#45573=CARTESIAN_POINT('Ctrl Pts',(-8.08087814877779,31.3918967161785,21.2950180122802));
#45574=CARTESIAN_POINT('Ctrl Pts',(-8.18714894688558,31.337342542798,21.2892075880416));
#45575=CARTESIAN_POINT('Ctrl Pts',(-8.29568826514029,31.2875147797709,21.283397163803));
#45576=CARTESIAN_POINT('Ctrl Pts',(-8.40833602134445,31.2358009327344,21.2773668029753));
#45577=CARTESIAN_POINT('Ctrl Pts',(-8.52342705878339,31.1891786297618,21.2713364421475));
#45578=CARTESIAN_POINT('Ctrl Pts',(-8.64045761121134,31.1478746784292,21.2653060813198));
#45579=CARTESIAN_POINT('Ctrl Pts',(-8.7530929569649,31.1081219408507,21.2595021970967));
#45580=CARTESIAN_POINT('Ctrl Pts',(-8.86752434410631,31.0732954343172,21.2536983128737));
#45581=CARTESIAN_POINT('Ctrl Pts',(-8.98328254517895,31.0435482288972,21.2478944286506));
#45582=CARTESIAN_POINT('Ctrl Pts',(-9.09902364752437,31.0138054174584,21.2420914017235));
#45583=CARTESIAN_POINT('Ctrl Pts',(-9.21609077866904,30.9891405166922,21.2362883747964));
#45584=CARTESIAN_POINT('Ctrl Pts',(-9.33400102960615,30.9696562961164,21.2304853478693));
#45585=CARTESIAN_POINT('Ctrl Pts',(-9.45192169078268,30.950170355288,21.2246818085957));
#45586=CARTESIAN_POINT('Ctrl Pts',(-9.57068521686028,30.9358660706478,21.2188782693221));
#45587=CARTESIAN_POINT('Ctrl Pts',(-9.68980066115883,30.9267947056179,21.2130747300485));
#45588=CARTESIAN_POINT('Ctrl Pts',(-9.80895473320445,30.9177203988502,21.2072693087549));
#45589=CARTESIAN_POINT('Ctrl Pts',(-9.92846054348736,30.9138824175841,21.2014638874613));
#45590=CARTESIAN_POINT('Ctrl Pts',(-10.0478248515278,30.9152799626442,21.1956584661677));
#45591=CARTESIAN_POINT('Ctrl Pts',(-10.1673213444887,30.9166790553559,21.1898466159075));
#45592=CARTESIAN_POINT('Ctrl Pts',(-10.2866756138682,30.9233252426369,21.1840347656473));
#45593=CARTESIAN_POINT('Ctrl Pts',(-10.4053970920624,30.9351656617093,21.1782229153871));
#45594=CARTESIAN_POINT('Ctrl Pts',(-10.5241965471592,30.9470138576323,21.1724072478726));
#45595=CARTESIAN_POINT('Ctrl Pts',(-10.6423619801288,30.964063021455,21.166591580358));
#45596=CARTESIAN_POINT('Ctrl Pts',(-10.7594122392473,30.9862090175395,21.1607759128434));
#45597=CARTESIAN_POINT('Ctrl Pts',(-10.8766301602221,31.0083867353719,21.1549519150132));
#45598=CARTESIAN_POINT('Ctrl Pts',(-10.992729322997,31.0356757640889,21.1491279171829));
#45599=CARTESIAN_POINT('Ctrl Pts',(-11.1072428327368,31.0679218841237,21.1433039193526));
#45600=CARTESIAN_POINT('Ctrl Pts',(-11.1376238930657,31.0764769561007,21.1417587808808));
#45601=CARTESIAN_POINT('Ctrl Pts',(-11.1678934506043,31.0853806790487,21.1402136424091));
#45602=CARTESIAN_POINT('Ctrl Pts',(-11.1980430315782,31.0946296085407,21.1386685039373));
#45603=CARTESIAN_POINT('Ctrl Pts',(-11.3116761558715,31.129488625502,21.1328449101644));
#45604=CARTESIAN_POINT('Ctrl Pts',(-11.4239698392315,31.1693674834581,21.1270213163916));
#45605=CARTESIAN_POINT('Ctrl Pts',(-11.5344483324783,31.2141456294577,21.1211977226187));
#45606=CARTESIAN_POINT('Ctrl Pts',(-11.6447874407038,31.2588672811781,21.115381476174));
#45607=CARTESIAN_POINT('Ctrl Pts',(-11.7533155387359,31.3084757746901,21.1095652297293));
#45608=CARTESIAN_POINT('Ctrl Pts',(-11.8595713467884,31.3628006095069,21.1037489832845));
#45609=CARTESIAN_POINT('Ctrl Pts',(-11.9657207921956,31.4170710648668,21.0979385589343));
#45610=CARTESIAN_POINT('Ctrl Pts',(-12.0696021111229,31.4760482847061,21.0921281345841));
#45611=CARTESIAN_POINT('Ctrl Pts',(-12.1707739167872,31.539513675479,21.0863177102339));
#45612=CARTESIAN_POINT('Ctrl Pts',(-12.2757752820505,31.6053813609906,21.0802873494479));
#45613=CARTESIAN_POINT('Ctrl Pts',(-12.3778575445559,31.6760835353256,21.0742569886618));
#45614=CARTESIAN_POINT('Ctrl Pts',(-12.4765548627097,31.7513231905915,21.0682266278758));
#45615=CARTESIAN_POINT('Ctrl Pts',(-12.5715455007581,31.8237371426009,21.0624227435409));
#45616=CARTESIAN_POINT('Ctrl Pts',(-12.6634005056374,31.9003536323609,21.056618859206));
#45617=CARTESIAN_POINT('Ctrl Pts',(-12.7517346405485,31.9808641189895,21.0508149748711));
#45618=CARTESIAN_POINT('Ctrl Pts',(-12.8400557275596,32.0613627133548,21.0450119478323));
#45619=CARTESIAN_POINT('Ctrl Pts',(-12.9248566771465,32.1457538857377,21.0392089207934));
#45620=CARTESIAN_POINT('Ctrl Pts',(-13.0057868227125,32.2336900794726,21.0334058937545));
#45621=CARTESIAN_POINT('Ctrl Pts',(-13.0867241135586,32.3216340370481,21.0276023543695));
#45622=CARTESIAN_POINT('Ctrl Pts',(-13.1637896443656,32.413123337798,21.0217988149844));
#45623=CARTESIAN_POINT('Ctrl Pts',(-13.2366714207888,32.5077754688132,21.0159952755993));
#45624=CARTESIAN_POINT('Ctrl Pts',(-13.3095768319158,32.6024582944024,21.0101898541946));
#45625=CARTESIAN_POINT('Ctrl Pts',(-13.3782955414098,32.7003056667091,21.0043844327899));
#45626=CARTESIAN_POINT('Ctrl Pts',(-13.4425578412034,32.8009046155364,20.9985790113851));
#45627=CARTESIAN_POINT('Ctrl Pts',(-13.5068913055313,32.9016149683654,20.9927671610149));
#45628=CARTESIAN_POINT('Ctrl Pts',(-13.5667582894038,33.0050826356966,20.9869553106446));
#45629=CARTESIAN_POINT('Ctrl Pts',(-13.6219340944211,33.1108683434789,20.9811434602744));
#45630=CARTESIAN_POINT('Ctrl Pts',(-13.6771461391971,33.2167235318701,20.9753277926502));
#45631=CARTESIAN_POINT('Ctrl Pts',(-13.7276606964746,33.324899423677,20.9695121250261));
#45632=CARTESIAN_POINT('Ctrl Pts',(-13.7733011124365,33.4349365141039,20.963696457402));
#45633=CARTESIAN_POINT('Ctrl Pts',(-13.8190069033523,33.5451312207478,20.9578724594637));
#45634=CARTESIAN_POINT('Ctrl Pts',(-13.8598244786433,33.6571920648184,20.9520484615254));
#45635=CARTESIAN_POINT('Ctrl Pts',(-13.8956268883525,33.7706440113843,20.9462244635872));
#45636=CARTESIAN_POINT('Ctrl Pts',(-13.9051254566996,33.8007434118807,20.9446793261811));
#45637=CARTESIAN_POINT('Ctrl Pts',(-13.9142713021519,33.8309406722877,20.943134188775));
#45638=CARTESIAN_POINT('Ctrl Pts',(-13.923062660518,33.8612268172943,20.9415890513689));
#45639=CARTESIAN_POINT('Ctrl Pts',(-13.9640196809555,34.0023233587344,20.9343905933279));
#45640=CARTESIAN_POINT('Ctrl Pts',(-13.9973850464633,34.1457148908331,20.927192135287));
#45641=CARTESIAN_POINT('Ctrl Pts',(-14.0229437095927,34.2906700982983,20.9199936772461));
#45642=CARTESIAN_POINT('Ctrl Pts',(-14.0481513699598,34.4336346039029,20.9128940772184));
#45643=CARTESIAN_POINT('Ctrl Pts',(-14.0657652702748,34.5781201849237,20.9057944771907));
#45644=CARTESIAN_POINT('Ctrl Pts',(-14.0756251114016,34.7234047156716,20.898694877163));
#45645=CARTESIAN_POINT('Ctrl Pts',(-14.0817866583163,34.8141949668195,20.8942582419187));
#45646=CARTESIAN_POINT('Ctrl Pts',(-14.0849210219501,34.9052968107325,20.8898216066744));
#45647=CARTESIAN_POINT('Ctrl Pts',(-14.084998525967,34.996529719382,20.8853849714301));
#45648=CARTESIAN_POINT('Ctrl Pts',(-14.0849985259674,34.9965297199084,20.8853849714045));
#45649=CARTESIAN_POINT('Ctrl Pts',(-14.0851010661903,35.1172337115238,20.8795151642127));
#45650=CARTESIAN_POINT('Ctrl Pts',(-14.0798491529871,35.2380430359988,20.8736453570208));
#45651=CARTESIAN_POINT('Ctrl Pts',(-14.0692436282635,35.3584428738826,20.867775549829));
#45652=CARTESIAN_POINT('Ctrl Pts',(-14.0588381189791,35.4765720248277,20.862016444568));
#45653=CARTESIAN_POINT('Ctrl Pts',(-14.0432792039204,35.594306568102,20.8562573393069));
#45654=CARTESIAN_POINT('Ctrl Pts',(-14.0226202175485,35.7111621371884,20.8504982340459));
#45655=CARTESIAN_POINT('Ctrl Pts',(-14.0019643520335,35.8280000534476,20.8447399987861));
#45656=CARTESIAN_POINT('Ctrl Pts',(-13.9762100192018,35.9439588506284,20.8389817635263));
#45657=CARTESIAN_POINT('Ctrl Pts',(-13.9454620141955,36.058562466055,20.8332235282666));
#45658=CARTESIAN_POINT('Ctrl Pts',(-13.9147111095653,36.1731768889268,20.8274647499889));
#45659=CARTESIAN_POINT('Ctrl Pts',(-13.8789657046316,36.2864354749415,20.8217059717112));
#45660=CARTESIAN_POINT('Ctrl Pts',(-13.8383807969595,36.3978761953523,20.8159471934336));
#45661=CARTESIAN_POINT('Ctrl Pts',(-13.79642617796,36.5130779596051,20.8099940605475));
#45662=CARTESIAN_POINT('Ctrl Pts',(-13.7492997768768,36.6263365341239,20.8040409276614));
#45663=CARTESIAN_POINT('Ctrl Pts',(-13.6972267955671,36.7371640746171,20.7980877947753));
#45664=CARTESIAN_POINT('Ctrl Pts',(-13.6467793219885,36.8445320278283,20.7923204946049));
#45665=CARTESIAN_POINT('Ctrl Pts',(-13.5916897459076,36.9496181183724,20.7865531944344));
#45666=CARTESIAN_POINT('Ctrl Pts',(-13.5322089943319,37.0520050244482,20.780785894264));
#45667=CARTESIAN_POINT('Ctrl Pts',(-13.4698533786252,37.1593405640898,20.7747398450201));
#45668=CARTESIAN_POINT('Ctrl Pts',(-13.4026717823633,37.2637090316623,20.7686937957761));
#45669=CARTESIAN_POINT('Ctrl Pts',(-13.3310026043533,37.3646662871939,20.7626477465322));
#45670=CARTESIAN_POINT('Ctrl Pts',(-13.2593334263433,37.4656235427255,20.7566016972883));
#45671=CARTESIAN_POINT('Ctrl Pts',(-13.1831770448823,37.563169225137,20.7505556480444));
#45672=CARTESIAN_POINT('Ctrl Pts',(-13.102917086446,37.6569024360412,20.7445095988004));
#45673=CARTESIAN_POINT('Ctrl Pts',(-13.0256101762298,37.7471868700332,20.7386860051284));
#45674=CARTESIAN_POINT('Ctrl Pts',(-12.9442348728705,37.8342400379334,20.7328624114565));
#45675=CARTESIAN_POINT('Ctrl Pts',(-12.8590915555362,37.9176738126566,20.7270388177845));
#45676=CARTESIAN_POINT('Ctrl Pts',(-12.7740556591683,38.0010023232557,20.7212225714426));
#45677=CARTESIAN_POINT('Ctrl Pts',(-12.6852614933218,38.0807202398707,20.7154063251008));
#45678=CARTESIAN_POINT('Ctrl Pts',(-12.5930494621087,38.1564726336621,20.7095900787589));
#45679=CARTESIAN_POINT('Ctrl Pts',(-12.5009297356738,38.2321491988679,20.7037796545134));
#45680=CARTESIAN_POINT('Ctrl Pts',(-12.4053992638386,38.3038678803899,20.6979692302679));
#45681=CARTESIAN_POINT('Ctrl Pts',(-12.3068346110207,38.3713111807421,20.6921588060223));
#45682=CARTESIAN_POINT('Ctrl Pts',(-12.2045390821698,38.4413073495485,20.6861284451977));
#45683=CARTESIAN_POINT('Ctrl Pts',(-12.0989754539081,38.5066977643392,20.6800980843731));
#45684=CARTESIAN_POINT('Ctrl Pts',(-11.9906019499406,38.567173794041,20.6740677235485));
#45685=CARTESIAN_POINT('Ctrl Pts',(-11.8862985278857,38.6253785822895,20.6682638393222));
#45686=CARTESIAN_POINT('Ctrl Pts',(-11.7793928683705,38.6790312416888,20.6624599550958));
#45687=CARTESIAN_POINT('Ctrl Pts',(-11.6703216060842,38.727901652706,20.6566560708695));
#45688=CARTESIAN_POINT('Ctrl Pts',(-11.5612664548177,38.7767648450285,20.6508530439404));
#45689=CARTESIAN_POINT('Ctrl Pts',(-11.4500467094675,38.820847026836,20.6450500170113));
#45690=CARTESIAN_POINT('Ctrl Pts',(-11.3371209850514,38.8599653458723,20.6392469900822));
#45691=CARTESIAN_POINT('Ctrl Pts',(-11.2241852905032,38.8990871186373,20.6334434508079));
#45692=CARTESIAN_POINT('Ctrl Pts',(-11.1095437032821,38.933244023607,20.6276399115337));
#45693=CARTESIAN_POINT('Ctrl Pts',(-10.9936714595392,38.9623026172287,20.6218363722595));
#45694=CARTESIAN_POINT('Ctrl Pts',(-10.8777616398077,38.9913706342062,20.6160309509666));
#45695=CARTESIAN_POINT('Ctrl Pts',(-10.7606207657281,39.0153369524756,20.6102255296737));
#45696=CARTESIAN_POINT('Ctrl Pts',(-10.6427351272116,39.0341190557851,20.6044201083808));
#45697=CARTESIAN_POINT('Ctrl Pts',(-10.5247189413039,39.0529219585288,20.5986082581232));
#45698=CARTESIAN_POINT('Ctrl Pts',(-10.4059567481628,39.0665291224263,20.5927964078656));
#45699=CARTESIAN_POINT('Ctrl Pts',(-10.2869409963013,39.0749097983442,20.586984557608));
#45700=CARTESIAN_POINT('Ctrl Pts',(-10.1678470742798,39.0832959787333,20.5811688900972));
#45701=CARTESIAN_POINT('Ctrl Pts',(-10.0484996691281,39.0864488239077,20.5753532225864));
#45702=CARTESIAN_POINT('Ctrl Pts',(-9.92939060827338,39.0843897113033,20.5695375550756));
#45703=CARTESIAN_POINT('Ctrl Pts',(-9.81011093658415,39.0823276492429,20.5637135572507));
#45704=CARTESIAN_POINT('Ctrl Pts',(-9.69107069673944,39.0750387534088,20.5578895594258));
#45705=CARTESIAN_POINT('Ctrl Pts',(-9.57275612281357,39.0625961735578,20.5520655616009));
#45706=CARTESIAN_POINT('Ctrl Pts',(-9.54136661965563,39.0592950891135,20.5505204231446));
#45707=CARTESIAN_POINT('Ctrl Pts',(-9.51002813346101,39.0556315303432,20.5489752846882));
#45708=CARTESIAN_POINT('Ctrl Pts',(-9.47874959800879,39.0516074610485,20.5474301462319));
#45709=CARTESIAN_POINT('Ctrl Pts',(-9.36086616727409,39.0364414346629,20.541606784634));
#45710=CARTESIAN_POINT('Ctrl Pts',(-9.2434550920497,39.016101871959,20.5357834230361));
#45711=CARTESIAN_POINT('Ctrl Pts',(-9.12700558900731,38.9906272387152,20.5299600614382));
#45712=CARTESIAN_POINT('Ctrl Pts',(-9.01069687684402,38.9651834050533,20.5241437404559));
#45713=CARTESIAN_POINT('Ctrl Pts',(-8.8953478203895,38.9346169330401,20.5183274194737));
#45714=CARTESIAN_POINT('Ctrl Pts',(-8.78144188777357,38.8990179695825,20.5125110984915));
#45715=CARTESIAN_POINT('Ctrl Pts',(-8.66746502923026,38.8633968396807,20.5066911558545));
#45716=CARTESIAN_POINT('Ctrl Pts',(-8.55493349871637,38.822737008394,20.5008712132176));
#45717=CARTESIAN_POINT('Ctrl Pts',(-8.44432157315873,38.7771801164706,20.4950512705806));
#45718=CARTESIAN_POINT('Ctrl Pts',(-8.33397535865273,38.7317326609357,20.4892453085617));
#45719=CARTESIAN_POINT('Ctrl Pts',(-8.22553992374258,38.6814117788916,20.4834393465427));
#45720=CARTESIAN_POINT('Ctrl Pts',(-8.11947015931623,38.626407660247,20.4776333845238));
#45721=CARTESIAN_POINT('Ctrl Pts',(-8.01301727469707,38.5712048686944,20.4718064515778));
#45722=CARTESIAN_POINT('Ctrl Pts',(-7.90894757308101,38.5112850853853,20.4659795186319));
#45723=CARTESIAN_POINT('Ctrl Pts',(-7.80769890231647,38.4468885820542,20.4601525856859));
#45724=CARTESIAN_POINT('Ctrl Pts',(-7.70645023155192,38.3824920787231,20.45432565274));
#45725=CARTESIAN_POINT('Ctrl Pts',(-7.60802294883767,38.3136190698864,20.448498719794));
#45726=CARTESIAN_POINT('Ctrl Pts',(-7.51282733495086,38.2405550657615,20.4426717868481));
#45727=CARTESIAN_POINT('',(-14.0849985032409,35.0034969300359,20.9896150285484));
#45728=CARTESIAN_POINT('Ctrl Pts',(-14.0849985032409,35.0034969300359,20.9896150285484));
#45729=CARTESIAN_POINT('Ctrl Pts',(-14.0848731076928,35.149979879647,20.982490506098));
#45730=CARTESIAN_POINT('Ctrl Pts',(-14.0768649533832,35.2961228114989,20.9753659836477));
#45731=CARTESIAN_POINT('Ctrl Pts',(-14.0611057921048,35.4411856132435,20.9682414611973));
#45732=CARTESIAN_POINT('Ctrl Pts',(-14.0451084213706,35.5884411288293,20.9610092471899));
#45733=CARTESIAN_POINT('Ctrl Pts',(-14.0211239958759,35.7345836848413,20.9537770331826));
#45734=CARTESIAN_POINT('Ctrl Pts',(-13.9893392113713,35.8788615685165,20.9465448191752));
#45735=CARTESIAN_POINT('Ctrl Pts',(-13.9714671903015,35.9599864657635,20.9424782734007));
#45736=CARTESIAN_POINT('Ctrl Pts',(-13.9511298671922,36.0405222226871,20.9384117276261));
#45737=CARTESIAN_POINT('Ctrl Pts',(-13.9283670284786,36.120338113947,20.9343451818516));
#45738=CARTESIAN_POINT('Ctrl Pts',(-13.8957689635322,36.2346403606827,20.9285215881894));
#45739=CARTESIAN_POINT('Ctrl Pts',(-13.8581254755738,36.3477030066093,20.9226979945273));
#45740=CARTESIAN_POINT('Ctrl Pts',(-13.8155476565826,36.4590480048124,20.9168744008651));
#45741=CARTESIAN_POINT('Ctrl Pts',(-13.7730235558362,36.5702525247569,20.9110581545316));
#45742=CARTESIAN_POINT('Ctrl Pts',(-13.7255776507761,36.6797433291843,20.9052419081981));
#45743=CARTESIAN_POINT('Ctrl Pts',(-13.6733712581126,36.7870558469371,20.8994256618646));
#45744=CARTESIAN_POINT('Ctrl Pts',(-13.6212171243382,36.8942609442635,20.8936152376259));
#45745=CARTESIAN_POINT('Ctrl Pts',(-13.5643121604916,36.9992917276244,20.8878048133873));
#45746=CARTESIAN_POINT('Ctrl Pts',(-13.5028661614887,37.1017025609485,20.8819943891487));
#45747=CARTESIAN_POINT('Ctrl Pts',(-13.439094304187,37.2079898563765,20.875964028321));
#45748=CARTESIAN_POINT('Ctrl Pts',(-13.3704310041989,37.3114545231373,20.8699336674932));
#45749=CARTESIAN_POINT('Ctrl Pts',(-13.29716397028,37.4116249196522,20.8639033066655));
#45750=CARTESIAN_POINT('Ctrl Pts',(-13.2266485576238,37.5080333105528,20.8580994224424));
#45751=CARTESIAN_POINT('Ctrl Pts',(-13.151869234024,37.6013900493696,20.8522955382194));
#45752=CARTESIAN_POINT('Ctrl Pts',(-13.0731268378601,37.6913038547187,20.8464916539963));
#45753=CARTESIAN_POINT('Ctrl Pts',(-12.9943960727923,37.781204378835,20.8406886270691));
#45754=CARTESIAN_POINT('Ctrl Pts',(-12.9117036682631,37.8676626737381,20.834885600142));
#45755=CARTESIAN_POINT('Ctrl Pts',(-12.8253901565136,37.9503212475044,20.8290825732148));
#45756=CARTESIAN_POINT('Ctrl Pts',(-12.7390690241855,38.0329871191566,20.8232790339412));
#45757=CARTESIAN_POINT('Ctrl Pts',(-12.6491264439136,38.1118523202253,20.8174754946676));
#45758=CARTESIAN_POINT('Ctrl Pts',(-12.5559386644293,38.1865973300176,20.811671955394));
#45759=CARTESIAN_POINT('Ctrl Pts',(-12.4627206652368,38.2613665787434,20.8058665341004));
#45760=CARTESIAN_POINT('Ctrl Pts',(-12.3662556922538,38.3320127235715,20.8000611128068));
#45761=CARTESIAN_POINT('Ctrl Pts',(-12.2669512843216,38.3982579175973,20.7942556915132));
#45762=CARTESIAN_POINT('Ctrl Pts',(-12.1675369059512,38.4645764720424,20.7884438412529));
#45763=CARTESIAN_POINT('Ctrl Pts',(-12.0652771560088,38.5264841207323,20.7826319909927));
#45764=CARTESIAN_POINT('Ctrl Pts',(-11.9606067648518,38.5837474957951,20.7768201407325));
#45765=CARTESIAN_POINT('Ctrl Pts',(-11.8558676256214,38.6410484817492,20.7710044732179));
#45766=CARTESIAN_POINT('Ctrl Pts',(-11.7487150575937,38.6936989394978,20.7651888057033));
#45767=CARTESIAN_POINT('Ctrl Pts',(-11.6396049709297,38.74151313499,20.7593731381887));
#45768=CARTESIAN_POINT('Ctrl Pts',(-11.5303385958489,38.7893958191539,20.7535491403584));
#45769=CARTESIAN_POINT('Ctrl Pts',(-11.4191094851098,38.8324282674881,20.7477251425281));
#45770=CARTESIAN_POINT('Ctrl Pts',(-11.3063900619071,38.8704741319573,20.7419011446978));
#45771=CARTESIAN_POINT('Ctrl Pts',(-11.2764849825518,38.8805679078458,20.7403560062263));
#45772=CARTESIAN_POINT('Ctrl Pts',(-11.2464750655801,38.8903109709657,20.7388108677547));
#45773=CARTESIAN_POINT('Ctrl Pts',(-11.2163692495601,38.8997013794295,20.7372657292832));
#45774=CARTESIAN_POINT('Ctrl Pts',(-11.1028985208678,38.9350944240956,20.7314420044528));
#45775=CARTESIAN_POINT('Ctrl Pts',(-10.9876987634882,38.965587897618,20.7256182796223));
#45776=CARTESIAN_POINT('Ctrl Pts',(-10.8712307299976,38.991012655343,20.7197945547919));
#45777=CARTESIAN_POINT('Ctrl Pts',(-10.7549102795949,39.016405195951,20.7139782095253));
#45778=CARTESIAN_POINT('Ctrl Pts',(-10.6373251451083,39.0367417096102,20.7081618642587));
#45779=CARTESIAN_POINT('Ctrl Pts',(-10.5189523331906,39.0519024514265,20.7023455189922));
#45780=CARTESIAN_POINT('Ctrl Pts',(-10.4006986643615,39.0670479338469,20.6965350279191));
#45781=CARTESIAN_POINT('Ctrl Pts',(-10.28165929806,39.0770279566943,20.6907245368459));
#45782=CARTESIAN_POINT('Ctrl Pts',(-10.1623219706014,39.0817737048813,20.6849140457728));
#45783=CARTESIAN_POINT('Ctrl Pts',(-10.0430738621129,39.086515905052,20.6791078987389));
#45784=CARTESIAN_POINT('Ctrl Pts',(-9.92352864238431,39.0860316015774,20.673301751705));
#45785=CARTESIAN_POINT('Ctrl Pts',(-9.80417911357673,39.0803038098211,20.6674956046711));
#45786=CARTESIAN_POINT('Ctrl Pts',(-9.6848774062533,39.074578313101,20.6616917840692));
#45787=CARTESIAN_POINT('Ctrl Pts',(-9.56577164113457,39.0636135255086,20.6558879634673));
#45788=CARTESIAN_POINT('Ctrl Pts',(-9.44735408749383,39.0474445635969,20.6500841428655));
#45789=CARTESIAN_POINT('Ctrl Pts',(-9.32895603525967,39.031278264445,20.6442812780565));
#45790=CARTESIAN_POINT('Ctrl Pts',(-9.21124637345403,39.0099095510758,20.6384784132476));
#45791=CARTESIAN_POINT('Ctrl Pts',(-9.09471107987942,38.9834252812256,20.6326755484387));
#45792=CARTESIAN_POINT('Ctrl Pts',(-8.97816747571492,38.956939122678,20.6268722698047));
#45793=CARTESIAN_POINT('Ctrl Pts',(-8.86279880429894,38.9253367733678,20.6210689911707));
#45794=CARTESIAN_POINT('Ctrl Pts',(-8.74907907106665,38.8887558202536,20.6152657125367));
#45795=CARTESIAN_POINT('Ctrl Pts',(-8.6352596005273,38.8521427840028,20.609457344167));
#45796=CARTESIAN_POINT('Ctrl Pts',(-8.52309234671557,38.810542545988,20.6036489757974));
#45797=CARTESIAN_POINT('Ctrl Pts',(-8.41303458850368,38.7641421044794,20.5978406074277));
#45798=CARTESIAN_POINT('Ctrl Pts',(-8.3029290834294,38.7177215328542,20.5920297191869));
#45799=CARTESIAN_POINT('Ctrl Pts',(-8.1949352672077,38.6664967819516,20.5862188309461));
#45800=CARTESIAN_POINT('Ctrl Pts',(-8.0894874175106,38.6107016869508,20.5804079427053));
#45801=CARTESIAN_POINT('Ctrl Pts',(-7.98388384687261,38.554824196105,20.5745884731896));
#45802=CARTESIAN_POINT('Ctrl Pts',(-7.88083410901292,38.4943630802427,20.568769003674));
#45803=CARTESIAN_POINT('Ctrl Pts',(-7.78074545011815,38.429596804703,20.5629495341583));
#45804=CARTESIAN_POINT('Ctrl Pts',(-7.6888464767986,38.3701299850496,20.5576062387274));
#45805=CARTESIAN_POINT('Ctrl Pts',(-7.59944368418054,38.3070343607522,20.5522629432965));
#45806=CARTESIAN_POINT('Ctrl Pts',(-7.51282733495085,38.2405550657615,20.5469196478657));
#45807=CARTESIAN_POINT('Ctrl Pts',(-7.51282733495087,38.2405550657615,21.796951697066));
#45808=CARTESIAN_POINT('Ctrl Pts',(-7.4180311178499,38.1677976044195,21.7911462584032));
#45809=CARTESIAN_POINT('Ctrl Pts',(-7.32646749484719,38.0909057833876,21.7853408197403));
#45810=CARTESIAN_POINT('Ctrl Pts',(-7.23850323443017,38.0102093969934,21.7795353810774));
#45811=CARTESIAN_POINT('Ctrl Pts',(-7.15044149746005,37.9294235878546,21.7737235091864));
#45812=CARTESIAN_POINT('Ctrl Pts',(-7.06598738566451,37.8448250741453,21.7679116372954));
#45813=CARTESIAN_POINT('Ctrl Pts',(-6.98547092660869,37.7567806343049,21.7620997654045));
#45814=CARTESIAN_POINT('Ctrl Pts',(-6.90490146889063,37.6686782406302,21.7562840679425));
#45815=CARTESIAN_POINT('Ctrl Pts',(-6.82827508719332,37.5771257160173,21.7504683704804));
#45816=CARTESIAN_POINT('Ctrl Pts',(-6.75588057567389,37.4825217341868,21.7446526730184));
#45817=CARTESIAN_POINT('Ctrl Pts',(-6.68338249601108,37.3877824111744,21.738828655575));
#45818=CARTESIAN_POINT('Ctrl Pts',(-6.61512860297032,37.2899832515262,21.7330046381316));
#45819=CARTESIAN_POINT('Ctrl Pts',(-6.55136364389892,37.1895507035412,21.7271806206882));
#45820=CARTESIAN_POINT('Ctrl Pts',(-6.53487637640687,37.1635825494382,21.7256747445006));
#45821=CARTESIAN_POINT('Ctrl Pts',(-6.51868897258072,37.1374384598219,21.724168868313));
#45822=CARTESIAN_POINT('Ctrl Pts',(-6.50280514828385,37.1111260429283,21.7226629921254));
#45823=CARTESIAN_POINT('Ctrl Pts',(-6.44137849223954,37.0093694538341,21.7168393984561));
#45824=CARTESIAN_POINT('Ctrl Pts',(-6.38429762830083,36.9047655862678,21.7110158047867));
#45825=CARTESIAN_POINT('Ctrl Pts',(-6.33183666579976,36.7977215450756,21.7051922111174));
#45826=CARTESIAN_POINT('Ctrl Pts',(-6.27944189059542,36.6908125558416,21.6993759647765));
#45827=CARTESIAN_POINT('Ctrl Pts',(-6.23165560181378,36.5814698797651,21.6935597184356));
#45828=CARTESIAN_POINT('Ctrl Pts',(-6.18870781714492,36.4701281906377,21.6877434720948));
#45829=CARTESIAN_POINT('Ctrl Pts',(-6.14580302344537,36.3588979551552,21.6819330478485));
#45830=CARTESIAN_POINT('Ctrl Pts',(-6.10772724468464,36.2456730661968,21.6761226236023));
#45831=CARTESIAN_POINT('Ctrl Pts',(-6.07466360223744,36.1309107676561,21.6703121993561));
#45832=CARTESIAN_POINT('Ctrl Pts',(-6.04034843251919,36.0118044786872,21.6642818385311));
#45833=CARTESIAN_POINT('Ctrl Pts',(-6.01143253294929,35.8910424947053,21.6582514777062));
#45834=CARTESIAN_POINT('Ctrl Pts',(-5.98806495335441,35.7691567990318,21.6522211168812));
#45835=CARTESIAN_POINT('Ctrl Pts',(-5.9655749679841,35.6518486498751,21.64641723265));
#45836=CARTESIAN_POINT('Ctrl Pts',(-5.94822415578516,35.5335001083631,21.6406133484189));
#45837=CARTESIAN_POINT('Ctrl Pts',(-5.93609381245957,35.4145979967035,21.6348094641877));
#45838=CARTESIAN_POINT('Ctrl Pts',(-5.92396526091538,35.2957134481571,21.6290064372523));
#45839=CARTESIAN_POINT('Ctrl Pts',(-5.91705568616431,35.1762758981931,21.6232034103169));
#45840=CARTESIAN_POINT('Ctrl Pts',(-5.91539460443507,35.0567781870249,21.6174003833815));
#45841=CARTESIAN_POINT('Ctrl Pts',(-5.91373337604967,34.9372699254579,21.6115968440995));
#45842=CARTESIAN_POINT('Ctrl Pts',(-5.91732156768735,34.8177019004437,21.6057933048175));
#45843=CARTESIAN_POINT('Ctrl Pts',(-5.92613656673833,34.6985672095915,21.5999897655354));
#45844=CARTESIAN_POINT('Ctrl Pts',(-5.93495442439076,34.5793938847476,21.5941843442333));
#45845=CARTESIAN_POINT('Ctrl Pts',(-5.94900243029866,34.460654580553,21.5883789229311));
#45846=CARTESIAN_POINT('Ctrl Pts',(-5.96820615034577,34.3428368894328,21.5825735016289));
#45847=CARTESIAN_POINT('Ctrl Pts',(-5.98743113673544,34.2248887261243,21.57676165136));
#45848=CARTESIAN_POINT('Ctrl Pts',(-6.01182316813872,34.1078646163548,21.5709498010911));
#45849=CARTESIAN_POINT('Ctrl Pts',(-6.0412567294953,33.9922417362116,21.5651379508221));
#45850=CARTESIAN_POINT('Ctrl Pts',(-6.07070962297316,33.8765429143393,21.5593222832987));
#45851=CARTESIAN_POINT('Ctrl Pts',(-6.10521052322021,33.7622475449808,21.5535066157753));
#45852=CARTESIAN_POINT('Ctrl Pts',(-6.1445846228837,33.649815838526,21.5476909482518));
#45853=CARTESIAN_POINT('Ctrl Pts',(-6.18401512169361,33.5372230857914,21.5418669504126));
#45854=CARTESIAN_POINT('Ctrl Pts',(-6.22833260108606,33.4264997018816,21.5360429525734));
#45855=CARTESIAN_POINT('Ctrl Pts',(-6.2773148598132,33.3180843222586,21.5302189547342));
#45856=CARTESIAN_POINT('Ctrl Pts',(-6.29031012021587,33.2893211307181,21.5286738163418));
#45857=CARTESIAN_POINT('Ctrl Pts',(-6.30363347546003,33.2607202478935,21.5271286779494));
#45858=CARTESIAN_POINT('Ctrl Pts',(-6.31728025454018,33.2322895383009,21.525583539557));
#45859=CARTESIAN_POINT('Ctrl Pts',(-6.36871467403732,33.1251347997945,21.5197599458878));
#45860=CARTESIAN_POINT('Ctrl Pts',(-6.42491268003554,33.0200539820572,21.5139363522187));
#45861=CARTESIAN_POINT('Ctrl Pts',(-6.48568403854052,32.9174995022735,21.5081127585496));
#45862=CARTESIAN_POINT('Ctrl Pts',(-6.54637872494952,32.8150744101999,21.5022965122089));
#45863=CARTESIAN_POINT('Ctrl Pts',(-6.61163508121126,32.7151696647093,21.4964802658682));
#45864=CARTESIAN_POINT('Ctrl Pts',(-6.68121564602866,32.6182159183009,21.4906640195275));
#45865=CARTESIAN_POINT('Ctrl Pts',(-6.75072656031655,32.521359223128,21.4848535952816));
#45866=CARTESIAN_POINT('Ctrl Pts',(-6.82455283531785,32.4274479803262,21.4790431710356));
#45867=CARTESIAN_POINT('Ctrl Pts',(-6.90241242590131,32.3368859917778,21.4732327467896));
#45868=CARTESIAN_POINT('Ctrl Pts',(-6.98321916307439,32.2428960445964,21.4672023859646));
#45869=CARTESIAN_POINT('Ctrl Pts',(-7.06837035901901,32.1525142994728,21.4611720251395));
#45870=CARTESIAN_POINT('Ctrl Pts',(-7.15750278192142,32.0661570312616,21.4551416643145));
#45871=CARTESIAN_POINT('Ctrl Pts',(-7.24328774218274,31.9830430018149,21.4493377800837));
#45872=CARTESIAN_POINT('Ctrl Pts',(-7.33275996413731,31.9036569233247,21.4435338958528));
#45873=CARTESIAN_POINT('Ctrl Pts',(-7.42555684708045,31.8283336473731,21.437730011622));
#45874=CARTESIAN_POINT('Ctrl Pts',(-7.51834002293136,31.7530214974751,21.431926984687));
#45875=CARTESIAN_POINT('Ctrl Pts',(-7.61444656619753,31.6817712139399,21.4261239577519));
#45876=CARTESIAN_POINT('Ctrl Pts',(-7.71348045926666,31.6148776403438,21.4203209308169));
#45877=CARTESIAN_POINT('Ctrl Pts',(-7.81252309599266,31.5479781607448,21.4145173915353));
#45878=CARTESIAN_POINT('Ctrl Pts',(-7.91449325799753,31.4854363844379,21.4087138522537));
#45879=CARTESIAN_POINT('Ctrl Pts',(-8.01896613726001,31.427503697038,21.4029103129721));
#45880=CARTESIAN_POINT('Ctrl Pts',(-8.12347289585904,31.369552222743,21.3971048916703));
#45881=CARTESIAN_POINT('Ctrl Pts',(-8.2304836288856,31.3162130078463,21.3912994703686));
#45882=CARTESIAN_POINT('Ctrl Pts',(-8.33954972603321,31.2676910782086,21.3854940490669));
#45883=CARTESIAN_POINT('Ctrl Pts',(-8.44873660378823,31.2191154150251,21.3796821987984));
#45884=CARTESIAN_POINT('Ctrl Pts',(-8.55998301570261,31.1753678516908,21.3738703485299));
#45885=CARTESIAN_POINT('Ctrl Pts',(-8.6728210626815,31.1366049815819,21.3680584982614));
#45886=CARTESIAN_POINT('Ctrl Pts',(-8.78573322229546,31.0978166518117,21.3622428307385));
#45887=CARTESIAN_POINT('Ctrl Pts',(-8.90023870816946,31.0640196507947,21.3564271632156));
#45888=CARTESIAN_POINT('Ctrl Pts',(-9.01585679058879,31.0353200452786,21.3506114956926));
#45889=CARTESIAN_POINT('Ctrl Pts',(-9.13164048342669,31.0065793306766,21.344787497854));
#45890=CARTESIAN_POINT('Ctrl Pts',(-9.24853955487536,30.9829506655232,21.3389635000153));
#45891=CARTESIAN_POINT('Ctrl Pts',(-9.36606534026051,30.9644886510901,21.3331395021766));
#45892=CARTESIAN_POINT('Ctrl Pts',(-9.39724557221665,30.9595905779522,21.3315943637806));
#45893=CARTESIAN_POINT('Ctrl Pts',(-9.42846990348814,30.9550558856007,21.3300492253845));
#45894=CARTESIAN_POINT('Ctrl Pts',(-9.45972919594568,30.9508849783827,21.3285040869885));
#45895=CARTESIAN_POINT('Ctrl Pts',(-9.57754480302819,30.9351649179674,21.3226804933035));
#45896=CARTESIAN_POINT('Ctrl Pts',(-9.69623706723345,30.9245658317069,21.3168568996184));
#45897=CARTESIAN_POINT('Ctrl Pts',(-9.81532332053317,30.9191766119984,21.3110333059334));
#45898=CARTESIAN_POINT('Ctrl Pts',(-9.93425932883662,30.913794191591,21.3052170595767));
#45899=CARTESIAN_POINT('Ctrl Pts',(-10.0535879332387,30.9136085824498,21.2994008132201));
#45900=CARTESIAN_POINT('Ctrl Pts',(-10.1728187807789,30.9186572468108,21.2935845668634));
#45901=CARTESIAN_POINT('Ctrl Pts',(-10.2919302775845,30.923700857431,21.2877741426014));
#45902=CARTESIAN_POINT('Ctrl Pts',(-10.4109438065726,30.9339683009686,21.2819637183394));
#45903=CARTESIAN_POINT('Ctrl Pts',(-10.5293670326301,30.9494450324969,21.2761532940774));
#45904=CARTESIAN_POINT('Ctrl Pts',(-10.6522728223415,30.9655075902734,21.2701229332583));
#45905=CARTESIAN_POINT('Ctrl Pts',(-10.7745422900183,30.9871816129408,21.2640925724392));
#45906=CARTESIAN_POINT('Ctrl Pts',(-10.8956281649368,31.0143914906037,21.2580622116202));
#45907=CARTESIAN_POINT('Ctrl Pts',(-11.0121665318834,31.0405794725611,21.2522583273734));
#45908=CARTESIAN_POINT('Ctrl Pts',(-11.1276081707663,31.0718949007598,21.2464544431266));
#45909=CARTESIAN_POINT('Ctrl Pts',(-11.2414742568829,31.1082180598732,21.2406505588797));
#45910=CARTESIAN_POINT('Ctrl Pts',(-11.3553235237601,31.1445358536673,21.2348475319287));
#45911=CARTESIAN_POINT('Ctrl Pts',(-11.4675973117717,31.185859783291,21.2290445049777));
#45912=CARTESIAN_POINT('Ctrl Pts',(-11.5778319398252,31.2320202535487,21.2232414780267));
#45913=CARTESIAN_POINT('Ctrl Pts',(-11.6880763004424,31.2781847992926,21.2174379387292));
#45914=CARTESIAN_POINT('Ctrl Pts',(-11.7962807664794,31.3291865769534,21.2116343994316));
#45915=CARTESIAN_POINT('Ctrl Pts',(-11.9020022219751,31.3848080897964,21.2058308601341));
#45916=CARTESIAN_POINT('Ctrl Pts',(-12.007757961704,31.4404476400463,21.2000254388166));
#45917=CARTESIAN_POINT('Ctrl Pts',(-12.1110287283191,31.5007097148868,21.194220017499));
#45918=CARTESIAN_POINT('Ctrl Pts',(-12.2113971322741,31.5653314973101,21.1884145961814));
#45919=CARTESIAN_POINT('Ctrl Pts',(-12.3118766849435,31.6300248423742,21.1826027458973));
#45920=CARTESIAN_POINT('Ctrl Pts',(-12.4094471158047,31.699087310885,21.1767908956131));
#45921=CARTESIAN_POINT('Ctrl Pts',(-12.5037209694331,31.7722134043247,21.170979045329));
#45922=CARTESIAN_POINT('Ctrl Pts',(-12.5980567426327,31.8453875273736,21.1651633777905));
#45923=CARTESIAN_POINT('Ctrl Pts',(-12.6890913158874,31.9226303271731,21.159347710252));
#45924=CARTESIAN_POINT('Ctrl Pts',(-12.7764724595077,32.0035978771875,21.1535320427135));
#45925=CARTESIAN_POINT('Ctrl Pts',(-12.8639787671778,32.0846814044716,21.1477080448594));
#45926=CARTESIAN_POINT('Ctrl Pts',(-12.9478209141016,32.1695000415701,21.1418840470054));
#45927=CARTESIAN_POINT('Ctrl Pts',(-13.0276853651733,32.2576750138768,21.1360600491513));
#45928=CARTESIAN_POINT('Ctrl Pts',(-13.0488738375526,32.2810683126499,21.1345149109076));
#45929=CARTESIAN_POINT('Ctrl Pts',(-13.0697825624206,32.3046976868828,21.1329697726638));
#45930=CARTESIAN_POINT('Ctrl Pts',(-13.0904061924051,32.3285557153585,21.1314246344201));
#45931=CARTESIAN_POINT('Ctrl Pts',(-13.1692726209863,32.4197907452863,21.125515900844));
#45932=CARTESIAN_POINT('Ctrl Pts',(-13.2442376687111,32.5146859736304,21.119607167268));
#45933=CARTESIAN_POINT('Ctrl Pts',(-13.3149406608934,32.6128692087036,21.113698433692));
#45934=CARTESIAN_POINT('Ctrl Pts',(-13.3839459164557,32.7086948452011,21.1079315819948));
#45935=CARTESIAN_POINT('Ctrl Pts',(-13.4488911827402,32.8076520351367,21.1021647302976));
#45936=CARTESIAN_POINT('Ctrl Pts',(-13.5094788137178,32.9093581234305,21.0963978786004));
#45937=CARTESIAN_POINT('Ctrl Pts',(-13.5700104610616,33.0109702341862,21.0906363555373));
#45938=CARTESIAN_POINT('Ctrl Pts',(-13.6261922654222,33.1153258395129,21.0848748324742));
#45939=CARTESIAN_POINT('Ctrl Pts',(-13.6777687647287,33.2220118354765,21.079113309411));
#45940=CARTESIAN_POINT('Ctrl Pts',(-13.7293102997805,33.3286255078743,21.0733556921454));
#45941=CARTESIAN_POINT('Ctrl Pts',(-13.7762525571435,33.4375660566901,21.0675980748797));
#45942=CARTESIAN_POINT('Ctrl Pts',(-13.8183854556803,33.5483948498821,21.061840457614));
#45943=CARTESIAN_POINT('Ctrl Pts',(-13.8624295242045,33.6642508942395,21.0558216718625));
#45944=CARTESIAN_POINT('Ctrl Pts',(-13.9012174237266,33.7821701041747,21.0498028861109));
#45945=CARTESIAN_POINT('Ctrl Pts',(-13.9345650358086,33.901627122061,21.0437841003594));
#45946=CARTESIAN_POINT('Ctrl Pts',(-13.9664521067653,34.0158522244831,21.0380289222117));
#45947=CARTESIAN_POINT('Ctrl Pts',(-13.9933652579045,34.1314828387702,21.032273744064));
#45948=CARTESIAN_POINT('Ctrl Pts',(-14.0151946311385,34.2480444999362,21.0265185659163));
#45949=CARTESIAN_POINT('Ctrl Pts',(-14.0370247942147,34.364610378599,21.0207631795317));
#45950=CARTESIAN_POINT('Ctrl Pts',(-14.0537707443973,34.4821069611363,21.015007793147));
#45951=CARTESIAN_POINT('Ctrl Pts',(-14.0653740111759,34.6000510666906,21.0092524067624));
#45952=CARTESIAN_POINT('Ctrl Pts',(-14.0769833472086,34.7180568645902,21.0034940099409));
#45953=CARTESIAN_POINT('Ctrl Pts',(-14.0834446009016,34.8365102381816,20.9977356131194));
#45954=CARTESIAN_POINT('Ctrl Pts',(-14.0847513050874,34.9549247785714,20.9919772162979));
#45955=CARTESIAN_POINT('Ctrl Pts',(-14.0849299821656,34.9711166331078,20.9911898203971));
#45956=CARTESIAN_POINT('Ctrl Pts',(-14.0850123618426,34.9873077634264,20.9904024244963));
#45957=CARTESIAN_POINT('Ctrl Pts',(-14.0849985032417,35.0034969290672,20.9896150285955));
#45958=CARTESIAN_POINT('Origin',(-10.,35.,32.7603849714045));
#45959=CARTESIAN_POINT('',(-7.51282733495086,38.2405550657615,23.0467784846721));
#45960=CARTESIAN_POINT('',(-7.51282733495087,38.2405550657615,22.942760002634));
#45961=CARTESIAN_POINT('',(-7.51282733495086,38.2405550657615,32.7603849714045));
#45962=CARTESIAN_POINT('',(-14.084999774902,35.0013561158978,22.1353849714381));
#45963=CARTESIAN_POINT('Ctrl Pts',(-7.51282733495087,38.2405550657615,22.942760002634));
#45964=CARTESIAN_POINT('Ctrl Pts',(-7.41810510545334,38.1678543909703,22.9369372088697));
#45965=CARTESIAN_POINT('Ctrl Pts',(-7.32667850440273,38.0910780862914,22.9311144151054));
#45966=CARTESIAN_POINT('Ctrl Pts',(-7.23889853618177,38.0105719899217,22.9252916213411));
#45967=CARTESIAN_POINT('Ctrl Pts',(-7.17403461442627,37.9510830057991,22.9209889399118));
#45968=CARTESIAN_POINT('Ctrl Pts',(-7.11116111779867,37.8895582518679,22.9166862584826));
#45969=CARTESIAN_POINT('Ctrl Pts',(-7.05040557842172,37.8261489253389,22.9123835770533));
#45970=CARTESIAN_POINT('Ctrl Pts',(-6.968174165185,37.7403256640143,22.9065599833816));
#45971=CARTESIAN_POINT('Ctrl Pts',(-6.88955900838778,37.6507720416984,22.9007363897099));
#45972=CARTESIAN_POINT('Ctrl Pts',(-6.8149167632981,37.5578252042078,22.8949127960382));
#45973=CARTESIAN_POINT('Ctrl Pts',(-6.74036869048772,37.4649956329587,22.889096549695));
#45974=CARTESIAN_POINT('Ctrl Pts',(-6.66978381322939,37.3687816770076,22.8832803033517));
#45975=CARTESIAN_POINT('Ctrl Pts',(-6.60348180785171,37.2695570427741,22.8774640570085));
#45976=CARTESIAN_POINT('Ctrl Pts',(-6.53724617114725,37.1704317329471,22.8716536327599));
#45977=CARTESIAN_POINT('Ctrl Pts',(-6.47528510307411,37.0683020777964,22.8658432085113));
#45978=CARTESIAN_POINT('Ctrl Pts',(-6.41787746912869,36.9635740815727,22.8600327842627));
#45979=CARTESIAN_POINT('Ctrl Pts',(-6.35829683750226,36.8548819140831,22.8540024234387));
#45980=CARTESIAN_POINT('Ctrl Pts',(-6.30362144545678,36.7433911632484,22.8479720626146));
#45981=CARTESIAN_POINT('Ctrl Pts',(-6.25411329246119,36.6295882223077,22.8419417017905));
#45982=CARTESIAN_POINT('Ctrl Pts',(-6.20646447061094,36.5200592714014,22.836137817557));
#45983=CARTESIAN_POINT('Ctrl Pts',(-6.16360194235753,36.4083890800178,22.8303339333236));
#45984=CARTESIAN_POINT('Ctrl Pts',(-6.12571170368778,36.2950348246507,22.8245300490901));
#45985=CARTESIAN_POINT('Ctrl Pts',(-6.08782706181148,36.1816973129194,22.8187270221524));
#45986=CARTESIAN_POINT('Ctrl Pts',(-6.05491337832601,36.0666766190678,22.8129239952147));
#45987=CARTESIAN_POINT('Ctrl Pts',(-6.02710744688957,35.9504471376356,22.807120968277));
#45988=CARTESIAN_POINT('Ctrl Pts',(-5.99929906048016,35.8342073943556,22.8013174289927));
#45989=CARTESIAN_POINT('Ctrl Pts',(-5.97659941775083,35.7167590484535,22.7955138897084));
#45990=CARTESIAN_POINT('Ctrl Pts',(-5.95909450684949,35.5985881684648,22.7897103504241));
#45991=CARTESIAN_POINT('Ctrl Pts',(-5.94158391930968,35.4803789670377,22.7839049291197));
#45992=CARTESIAN_POINT('Ctrl Pts',(-5.92927147367316,35.361447169257,22.7780995078153));
#45993=CARTESIAN_POINT('Ctrl Pts',(-5.92219138970121,35.2422848277813,22.7722940865109));
#45994=CARTESIAN_POINT('Ctrl Pts',(-5.9151034651916,35.1229905250422,22.7664822362397));
#45995=CARTESIAN_POINT('Ctrl Pts',(-5.91325949261094,35.0034655768557,22.7606703859686));
#45996=CARTESIAN_POINT('Ctrl Pts',(-5.91664156972959,34.8842030659318,22.7548585356974));
#45997=CARTESIAN_POINT('Ctrl Pts',(-5.92002586821465,34.7648622227506,22.7490428681718));
#45998=CARTESIAN_POINT('Ctrl Pts',(-5.92864302289951,34.6457845664473,22.7432272006462));
#45999=CARTESIAN_POINT('Ctrl Pts',(-5.94242331960044,34.5274574276558,22.7374115331206));
#46000=CARTESIAN_POINT('Ctrl Pts',(-5.95622335508837,34.4089607980151,22.7315875352793));
#46001=CARTESIAN_POINT('Ctrl Pts',(-5.97520122914806,34.2912172333013,22.7257635374379));
#46002=CARTESIAN_POINT('Ctrl Pts',(-5.99923625789207,34.1747033988713,22.7199395395966));
#46003=CARTESIAN_POINT('Ctrl Pts',(-6.00561288201908,34.1437916435466,22.718394401226));
#46004=CARTESIAN_POINT('Ctrl Pts',(-6.01234519332935,34.1129663576641,22.7168492628554));
#46005=CARTESIAN_POINT('Ctrl Pts',(-6.01943035767116,34.0822362381473,22.7153041244848));
#46006=CARTESIAN_POINT('Ctrl Pts',(-6.04613419145458,33.9664150709686,22.7094805308136));
#46007=CARTESIAN_POINT('Ctrl Pts',(-6.07794029159737,33.8515735883069,22.7036569371423));
#46008=CARTESIAN_POINT('Ctrl Pts',(-6.11476218449409,33.7381948973939,22.697833343471));
#46009=CARTESIAN_POINT('Ctrl Pts',(-6.15153762110351,33.6249592505404,22.6920170971282));
#46010=CARTESIAN_POINT('Ctrl Pts',(-6.19331613887171,33.513183109667,22.6862008507854));
#46011=CARTESIAN_POINT('Ctrl Pts',(-6.23996041545217,33.4033386950786,22.6803846044426));
#46012=CARTESIAN_POINT('Ctrl Pts',(-6.28655800085442,33.2936042353552,22.6745741801944));
#46013=CARTESIAN_POINT('Ctrl Pts',(-6.33801149682608,33.1857980288159,22.6687637559463));
#46014=CARTESIAN_POINT('Ctrl Pts',(-6.39413419703502,33.0803758672574,22.6629533316981));
#46015=CARTESIAN_POINT('Ctrl Pts',(-6.45238125753126,32.9709632588284,22.6569229708739));
#46016=CARTESIAN_POINT('Ctrl Pts',(-6.51565784605973,32.8641191697906,22.6508926100497));
#46017=CARTESIAN_POINT('Ctrl Pts',(-6.58370077591595,32.7603293519978,22.6448622492254));
#46018=CARTESIAN_POINT('Ctrl Pts',(-6.64918828143558,32.6604374707993,22.6390583649924));
#46019=CARTESIAN_POINT('Ctrl Pts',(-6.71909033052302,32.5633749574202,22.6332544807593));
#46020=CARTESIAN_POINT('Ctrl Pts',(-6.79312651017594,32.469547981039,22.6274505965263));
#46021=CARTESIAN_POINT('Ctrl Pts',(-6.86715175389342,32.3757348639056,22.621647569589));
#46022=CARTESIAN_POINT('Ctrl Pts',(-6.94530966090001,32.2851566538041,22.6158445426517));
#46023=CARTESIAN_POINT('Ctrl Pts',(-7.02727844659217,32.1981878068107,22.6100415157144));
#46024=CARTESIAN_POINT('Ctrl Pts',(-7.10925446927096,32.1112112813775,22.6042379764306));
#46025=CARTESIAN_POINT('Ctrl Pts',(-7.19504175951734,32.0278450498116,22.5984344371467));
#46026=CARTESIAN_POINT('Ctrl Pts',(-7.28428091920428,31.9484274751856,22.5926308978628));
#46027=CARTESIAN_POINT('Ctrl Pts',(-7.37354901811011,31.8689841463663,22.5868254765588));
#46028=CARTESIAN_POINT('Ctrl Pts',(-7.46627090781391,31.7934922924429,22.5810200552548));
#46029=CARTESIAN_POINT('Ctrl Pts',(-7.56205380769659,31.7222502591819,22.5752146339508));
#46030=CARTESIAN_POINT('Ctrl Pts',(-7.65794277827528,31.6509293319631,22.5694027836801));
#46031=CARTESIAN_POINT('Ctrl Pts',(-7.75689919749645,31.5838678633924,22.5635909334093));
#46032=CARTESIAN_POINT('Ctrl Pts',(-7.85850085185887,31.5213211705432,22.5577790831386));
#46033=CARTESIAN_POINT('Ctrl Pts',(-7.96016923873341,31.4587333966904,22.5519634156134));
#46034=CARTESIAN_POINT('Ctrl Pts',(-8.06448596486822,31.4006665022316,22.5461477480882));
#46035=CARTESIAN_POINT('Ctrl Pts',(-8.17100522620662,31.3473293171384,22.540332080563));
#46036=CARTESIAN_POINT('Ctrl Pts',(-8.27767706488483,31.293915732287,22.534508082722));
#46037=CARTESIAN_POINT('Ctrl Pts',(-8.38655736429865,31.2452455449764,22.5286840848811));
#46038=CARTESIAN_POINT('Ctrl Pts',(-8.49718130078616,31.2014791092725,22.5228600870401));
#46039=CARTESIAN_POINT('Ctrl Pts',(-8.52653043416175,31.1898676353037,22.5213149486655));
#46040=CARTESIAN_POINT('Ctrl Pts',(-8.55600222175017,31.1786010472323,22.519769810291));
#46041=CARTESIAN_POINT('Ctrl Pts',(-8.58558783611666,31.1676817419923,22.5182246719164));
#46042=CARTESIAN_POINT('Ctrl Pts',(-8.69709538742306,31.1265271127798,22.5124010782454));
#46043=CARTESIAN_POINT('Ctrl Pts',(-8.81058043544496,31.0901768992956,22.5065774845743));
#46044=CARTESIAN_POINT('Ctrl Pts',(-8.92559152155267,31.0588235992993,22.5007538909033));
#46045=CARTESIAN_POINT('Ctrl Pts',(-9.04045750409172,31.027509856148,22.4949376445607));
#46046=CARTESIAN_POINT('Ctrl Pts',(-9.15684530480516,31.0011805937347,22.4891213982181));
#46047=CARTESIAN_POINT('Ctrl Pts',(-9.27428469714716,30.9799798135824,22.4833051518755));
#46048=CARTESIAN_POINT('Ctrl Pts',(-9.39160653200931,30.9588002555279,22.4774947276276));
#46049=CARTESIAN_POINT('Ctrl Pts',(-9.50997746485329,30.9427390391209,22.4716843033797));
#46050=CARTESIAN_POINT('Ctrl Pts',(-9.62891393896111,30.931889857034,22.4658738791318));
#46051=CARTESIAN_POINT('Ctrl Pts',(-9.7523524046294,30.920630010964,22.4598435183075));
#46052=CARTESIAN_POINT('Ctrl Pts',(-9.87639963886789,30.9149846857926,22.4538131574832));
#46053=CARTESIAN_POINT('Ctrl Pts',(-10.000505103477,30.9150000312276,22.4477827966588));
#46054=CARTESIAN_POINT('Ctrl Pts',(-10.1199496558401,30.9150148003486,22.441978912426));
#46055=CARTESIAN_POINT('Ctrl Pts',(-10.239447698591,30.9202727227138,22.4361750281932));
#46056=CARTESIAN_POINT('Ctrl Pts',(-10.3585058113543,30.9307619161291,22.4303711439604));
#46057=CARTESIAN_POINT('Ctrl Pts',(-10.4775463379612,30.9412495601784,22.4245681170234));
#46058=CARTESIAN_POINT('Ctrl Pts',(-10.5961466571583,30.9569669027656,22.4187650900864));
#46059=CARTESIAN_POINT('Ctrl Pts',(-10.7138171940892,30.9778500757154,22.4129620631493));
#46060=CARTESIAN_POINT('Ctrl Pts',(-10.8314981200979,30.998735092431,22.4071585238657));
#46061=CARTESIAN_POINT('Ctrl Pts',(-10.9482486985512,31.0247867749672,22.4013549845821));
#46062=CARTESIAN_POINT('Ctrl Pts',(-11.0635889233756,31.0558900114129,22.3955514452984));
#46063=CARTESIAN_POINT('Ctrl Pts',(-11.1789665516898,31.0870033342754,22.3897460239947));
#46064=CARTESIAN_POINT('Ctrl Pts',(-11.2929325227361,31.1231713627163,22.383940602691));
#46065=CARTESIAN_POINT('Ctrl Pts',(-11.4050220006952,31.1642291286415,22.3781351813872));
#46066=CARTESIAN_POINT('Ctrl Pts',(-11.5172356073763,31.2053323622422,22.3723233311168));
#46067=CARTESIAN_POINT('Ctrl Pts',(-11.6275681893683,31.2513360014652,22.3665114808463));
#46068=CARTESIAN_POINT('Ctrl Pts',(-11.7355747647748,31.3020268746411,22.3606996305758));
#46069=CARTESIAN_POINT('Ctrl Pts',(-11.8436522794798,31.3527510418545,22.3548839630509));
#46070=CARTESIAN_POINT('Ctrl Pts',(-11.9494003842287,31.4081683850273,22.3490682955259));
#46071=CARTESIAN_POINT('Ctrl Pts',(-12.052400046113,31.468020519494,22.343252628001));
#46072=CARTESIAN_POINT('Ctrl Pts',(-12.1555472438912,31.5279583856806,22.3374286301603));
#46073=CARTESIAN_POINT('Ctrl Pts',(-12.2559377985707,31.5923435024643,22.3316046323196));
#46074=CARTESIAN_POINT('Ctrl Pts',(-12.3531827952367,31.6608750050048,22.3257806344789));
#46075=CARTESIAN_POINT('Ctrl Pts',(-12.3789824229886,31.679056786232,22.3242354961019));
#46076=CARTESIAN_POINT('Ctrl Pts',(-12.4045608326988,31.6975302057917,22.3226903577249));
#46077=CARTESIAN_POINT('Ctrl Pts',(-12.4299111807625,31.716289194584,22.321145219348));
#46078=CARTESIAN_POINT('Ctrl Pts',(-12.5246533662665,31.7863974073616,22.3153705535969));
#46079=CARTESIAN_POINT('Ctrl Pts',(-12.6165244936635,31.860731942538,22.3095958878458));
#46080=CARTESIAN_POINT('Ctrl Pts',(-12.7051198634262,31.9390276831541,22.3038212220947));
#46081=CARTESIAN_POINT('Ctrl Pts',(-12.7936030129364,32.0172242496507,22.2980538708845));
#46082=CARTESIAN_POINT('Ctrl Pts',(-12.878818345861,32.099371772537,22.2922865196742));
#46083=CARTESIAN_POINT('Ctrl Pts',(-12.9603911014528,32.185162611013,22.286519168464));
#46084=CARTESIAN_POINT('Ctrl Pts',(-13.0418827354367,32.2708681331269,22.280757552708));
#46085=CARTESIAN_POINT('Ctrl Pts',(-13.1197387110857,32.3602094656816,22.2749959369519));
#46086=CARTESIAN_POINT('Ctrl Pts',(-13.1936188085977,32.4528400314524,22.2692343211959));
#46087=CARTESIAN_POINT('Ctrl Pts',(-13.2674469120447,32.5454054072761,22.2634767602507));
#46088=CARTESIAN_POINT('Ctrl Pts',(-13.3373044441081,32.6412550879758,22.2577191993055));
#46089=CARTESIAN_POINT('Ctrl Pts',(-13.402889872101,32.740007628696,22.2519616383604));
#46090=CARTESIAN_POINT('Ctrl Pts',(-13.4684512490792,32.8387239555972,22.2462061887864));
#46091=CARTESIAN_POINT('Ctrl Pts',(-13.5297434061291,32.9403406804837,22.2404507392124));
#46092=CARTESIAN_POINT('Ctrl Pts',(-13.5865071222819,33.0444459450527,22.2346952896385));
#46093=CARTESIAN_POINT('Ctrl Pts',(-13.6432640019236,33.1485386713869,22.2289405332396));
#46094=CARTESIAN_POINT('Ctrl Pts',(-13.6954933261924,33.2551189761469,22.2231857768408));
#46095=CARTESIAN_POINT('Ctrl Pts',(-13.7429813543268,33.3637495359323,22.2174310204419));
#46096=CARTESIAN_POINT('Ctrl Pts',(-13.7904753584471,33.4723937659988,22.2116755398533));
#46097=CARTESIAN_POINT('Ctrl Pts',(-13.8332267144456,33.5830883824799,22.2059200592647));
#46098=CARTESIAN_POINT('Ctrl Pts',(-13.8710697362886,33.6953758791166,22.2001645786761));
#46099=CARTESIAN_POINT('Ctrl Pts',(-13.9089487815488,33.8077702641347,22.1944036193474));
#46100=CARTESIAN_POINT('Ctrl Pts',(-13.9419100289843,33.9217601624649,22.1886426600188));
#46101=CARTESIAN_POINT('Ctrl Pts',(-13.9698376062264,34.0368726043817,22.1828817006901));
#46102=CARTESIAN_POINT('Ctrl Pts',(-13.9977791248236,34.1520425100522,22.1771178655095));
#46103=CARTESIAN_POINT('Ctrl Pts',(-14.0206818886159,34.2683356672832,22.1713540303288));
#46104=CARTESIAN_POINT('Ctrl Pts',(-14.0384814547986,34.3852703527179,22.1655901951481));
#46105=CARTESIAN_POINT('Ctrl Pts',(-14.0563077963079,34.5023809393155,22.1598176896118));
#46106=CARTESIAN_POINT('Ctrl Pts',(-14.0690155630161,34.6201345681094,22.1540451840755));
#46107=CARTESIAN_POINT('Ctrl Pts',(-14.0765923082487,34.7380455147783,22.1482726785391));
#46108=CARTESIAN_POINT('Ctrl Pts',(-14.0822309269687,34.8257949178241,22.1439767761721));
#46109=CARTESIAN_POINT('Ctrl Pts',(-14.085028897281,34.9136313781386,22.1396808738051));
#46110=CARTESIAN_POINT('Ctrl Pts',(-14.084999774902,35.0013561158978,22.1353849714381));
#46111=CARTESIAN_POINT('Ctrl Pts',(-14.0849997749018,35.0013561165845,22.1353849714045));
#46112=CARTESIAN_POINT('Ctrl Pts',(-14.0849741968583,35.0784042873399,22.1316119031962));
#46113=CARTESIAN_POINT('Ctrl Pts',(-14.0827689216963,35.1554131039001,22.1278388349879));
#46114=CARTESIAN_POINT('Ctrl Pts',(-14.0783897720535,35.2322969375804,22.1240657667795));
#46115=CARTESIAN_POINT('Ctrl Pts',(-14.0716307137146,35.3509643409699,22.1182421731102));
#46116=CARTESIAN_POINT('Ctrl Pts',(-14.0596772245188,35.4695278607971,22.1124185794409));
#46117=CARTESIAN_POINT('Ctrl Pts',(-14.0425329433293,35.5874967251799,22.1065949857716));
#46118=CARTESIAN_POINT('Ctrl Pts',(-14.0254102921972,35.7053167543175,22.1007787394307));
#46119=CARTESIAN_POINT('Ctrl Pts',(-14.0031099329979,35.8225432197027,22.0949624930898));
#46120=CARTESIAN_POINT('Ctrl Pts',(-13.9756874615848,35.9386874920855,22.0891462467489));
#46121=CARTESIAN_POINT('Ctrl Pts',(-13.9482924402167,36.054715503411,22.0833358225027));
#46122=CARTESIAN_POINT('Ctrl Pts',(-13.9157855999806,36.1696630816619,22.0775253982564));
#46123=CARTESIAN_POINT('Ctrl Pts',(-13.8782739859291,36.2830494495792,22.0717149740102));
#46124=CARTESIAN_POINT('Ctrl Pts',(-13.8393424796791,36.400727726104,22.0656846131852));
#46125=CARTESIAN_POINT('Ctrl Pts',(-13.7950198958781,36.5167238234022,22.0596542523603));
#46126=CARTESIAN_POINT('Ctrl Pts',(-13.7454836013012,36.6305145176857,22.0536238915353));
#46127=CARTESIAN_POINT('Ctrl Pts',(-13.6978076947825,36.7400316818114,22.0478200073042));
#46128=CARTESIAN_POINT('Ctrl Pts',(-13.6453028057693,36.8475057000283,22.042016123073));
#46129=CARTESIAN_POINT('Ctrl Pts',(-13.5881767206809,36.9524888786274,22.0362122388418));
#46130=CARTESIAN_POINT('Ctrl Pts',(-13.5310590737261,37.0574565500886,22.0304092119064));
#46131=CARTESIAN_POINT('Ctrl Pts',(-13.4693217832903,37.1599337550384,22.024606184971));
#46132=CARTESIAN_POINT('Ctrl Pts',(-13.4032187691411,37.259497070006,22.0188031580356));
#46133=CARTESIAN_POINT('Ctrl Pts',(-13.3371099187868,37.3590691753735,22.0129996187536));
#46134=CARTESIAN_POINT('Ctrl Pts',(-13.2666348042263,37.4557265390491,22.0071960794716));
#46135=CARTESIAN_POINT('Ctrl Pts',(-13.1920905142096,37.5490749594888,22.0013925401896));
#46136=CARTESIAN_POINT('Ctrl Pts',(-13.1175220503485,37.6424536517333,21.9955871188874));
#46137=CARTESIAN_POINT('Ctrl Pts',(-13.0388820413468,37.7325209477668,21.9897816975852));
#46138=CARTESIAN_POINT('Ctrl Pts',(-12.9565072374651,37.8189164504852,21.9839762762831));
#46139=CARTESIAN_POINT('Ctrl Pts',(-12.8740412111122,37.9054076282268,21.9781644260141));
#46140=CARTESIAN_POINT('Ctrl Pts',(-12.7878324161358,37.9882186005192,21.9723525757452));
#46141=CARTESIAN_POINT('Ctrl Pts',(-12.6982538800312,38.0670264098792,21.9665407254763));
#46142=CARTESIAN_POINT('Ctrl Pts',(-12.6086165082629,38.1458859806317,21.9607250579528));
#46143=CARTESIAN_POINT('Ctrl Pts',(-12.5156053049828,38.2207368967183,21.9549093904294));
#46144=CARTESIAN_POINT('Ctrl Pts',(-12.4196244006156,38.2912980357217,21.949093722906));
#46145=CARTESIAN_POINT('Ctrl Pts',(-12.3235060139662,38.361960245938,21.9432697250668));
#46146=CARTESIAN_POINT('Ctrl Pts',(-12.2244097740082,38.4283201883,21.9374457272276));
#46147=CARTESIAN_POINT('Ctrl Pts',(-12.1227667446997,38.4901413076833,21.9316217293883));
#46148=CARTESIAN_POINT('Ctrl Pts',(-12.0958002946353,38.5065427878449,21.9300765909959));
#46149=CARTESIAN_POINT('Ctrl Pts',(-12.0686547041497,38.5226250516946,21.9285314526035));
#46150=CARTESIAN_POINT('Ctrl Pts',(-12.0413382690484,38.5383842458555,21.9269863142111));
#46151=CARTESIAN_POINT('Ctrl Pts',(-11.9383832073534,38.5977803127684,21.9211627205419));
#46152=CARTESIAN_POINT('Ctrl Pts',(-11.8326676330745,38.6527749624113,21.9153391268728));
#46153=CARTESIAN_POINT('Ctrl Pts',(-11.7246040083451,38.7031022149544,21.9095155332037));
#46154=CARTESIAN_POINT('Ctrl Pts',(-11.6166767219304,38.7533659721925,21.903699286863));
#46155=CARTESIAN_POINT('Ctrl Pts',(-11.5064076441376,38.7989738737752,21.8978830405223));
#46156=CARTESIAN_POINT('Ctrl Pts',(-11.3942359259936,38.8397045697122,21.8920667941817));
#46157=CARTESIAN_POINT('Ctrl Pts',(-11.2821764923588,38.8803944939977,21.8862563699357));
#46158=CARTESIAN_POINT('Ctrl Pts',(-11.1682185888573,38.9162167864233,21.8804459456898));
#46159=CARTESIAN_POINT('Ctrl Pts',(-11.052823001915,38.9469974318004,21.8746355214438));
#46160=CARTESIAN_POINT('Ctrl Pts',(-10.9330594532611,38.978943188288,21.8686051606187));
#46161=CARTESIAN_POINT('Ctrl Pts',(-10.8117476384202,39.0054578936876,21.8625747997937));
#46162=CARTESIAN_POINT('Ctrl Pts',(-10.689422392677,39.0264030802287,21.8565444389686));
#46163=CARTESIAN_POINT('Ctrl Pts',(-10.5716912012283,39.046561648083,21.8507405547378));
#46164=CARTESIAN_POINT('Ctrl Pts',(-10.4530217657467,39.0615614161482,21.844936670507));
#46165=CARTESIAN_POINT('Ctrl Pts',(-10.3339024252795,39.0713307616052,21.8391327862762));
#46166=CARTESIAN_POINT('Ctrl Pts',(-10.2148006800129,39.0810986640253,21.8333297593412));
#46167=CARTESIAN_POINT('Ctrl Pts',(-10.0952495687809,39.0856376469056,21.8275267324061));
#46168=CARTESIAN_POINT('Ctrl Pts',(-9.97574242032439,39.0849279760882,21.8217237054711));
#46169=CARTESIAN_POINT('Ctrl Pts',(-9.85622472063662,39.0842182426144,21.8159201661895));
#46170=CARTESIAN_POINT('Ctrl Pts',(-9.73675139979158,39.0782589365143,21.8101166269079));
#46171=CARTESIAN_POINT('Ctrl Pts',(-9.6178150098177,39.0670824473177,21.8043130876263));
#46172=CARTESIAN_POINT('Ctrl Pts',(-9.49884005015977,39.0559023337159,21.7985076663245));
#46173=CARTESIAN_POINT('Ctrl Pts',(-9.38040277399597,39.0395017104503,21.7927022450228));
#46174=CARTESIAN_POINT('Ctrl Pts',(-9.26298920129247,39.0179646691563,21.7868968237211));
#46175=CARTESIAN_POINT('Ctrl Pts',(-9.14544560392483,38.9964037775826,21.7810849734526));
#46176=CARTESIAN_POINT('Ctrl Pts',(-9.02892837476783,38.969695187746,21.7752731231842));
#46177=CARTESIAN_POINT('Ctrl Pts',(-8.913912106228,38.9379738555508,21.7694612729157));
#46178=CARTESIAN_POINT('Ctrl Pts',(-8.79882029438557,38.9062316886144,21.7636456053928));
#46179=CARTESIAN_POINT('Ctrl Pts',(-8.68523179408831,38.8694703478723,21.7578299378699));
#46180=CARTESIAN_POINT('Ctrl Pts',(-8.57360325759354,38.8278737352808,21.7520142703469));
#46181=CARTESIAN_POINT('Ctrl Pts',(-8.46181482527368,38.7862175400332,21.7461902725083));
#46182=CARTESIAN_POINT('Ctrl Pts',(-8.35199233492593,38.7397124076678,21.7403662746696));
#46183=CARTESIAN_POINT('Ctrl Pts',(-8.24456992799178,38.6885891967376,21.7345422768309));
#46184=CARTESIAN_POINT('Ctrl Pts',(-8.21607017745062,38.6750259300044,21.7329971384348));
#46185=CARTESIAN_POINT('Ctrl Pts',(-8.1877392119687,38.6611378526349,21.7314520000387));
#46186=CARTESIAN_POINT('Ctrl Pts',(-8.15958480185777,38.6469297907208,21.7299068616426));
#46187=CARTESIAN_POINT('Ctrl Pts',(-8.0534531648498,38.5933706906114,21.7240822655408));
#46188=CARTESIAN_POINT('Ctrl Pts',(-7.9494902807754,38.535088453809,21.718257669439));
#46189=CARTESIAN_POINT('Ctrl Pts',(-7.84814493426046,38.4722823583417,21.7124330733371));
#46190=CARTESIAN_POINT('Ctrl Pts',(-7.74693946608145,38.40956294877,21.7066165164284));
#46191=CARTESIAN_POINT('Ctrl Pts',(-7.64834469092929,38.3423323182262,21.7007999595197));
#46192=CARTESIAN_POINT('Ctrl Pts',(-7.55278652960942,38.2708364725768,21.694983402611));
#46193=CARTESIAN_POINT('Ctrl Pts',(-7.53940692985026,38.2608259639398,21.6941689959466));
#46194=CARTESIAN_POINT('Ctrl Pts',(-7.52608682171778,38.2507319127429,21.6933545892822));
#46195=CARTESIAN_POINT('Ctrl Pts',(-7.51282733495086,38.2405550657615,21.6925401826178));
#46196=CARTESIAN_POINT('',(-14.0849992774348,34.997570317556,22.2396150286382));
#46197=CARTESIAN_POINT('Ctrl Pts',(-14.0849992774354,34.9975703184362,22.2396150285955));
#46198=CARTESIAN_POINT('Ctrl Pts',(-14.085070989627,35.1181393078928,22.233766442302));
#46199=CARTESIAN_POINT('Ctrl Pts',(-14.0798004648248,35.2387276668954,22.2279178560085));
#46200=CARTESIAN_POINT('Ctrl Pts',(-14.0692091476505,35.3588341018879,22.2220692697149));
#46201=CARTESIAN_POINT('Ctrl Pts',(-14.0586166826973,35.4789535527894,22.2162200496113));
#46202=CARTESIAN_POINT('Ctrl Pts',(-14.0427023124911,35.5985905779619,22.2103708295077));
#46203=CARTESIAN_POINT('Ctrl Pts',(-14.0215393834305,35.7172489020677,22.2045216094042));
#46204=CARTESIAN_POINT('Ctrl Pts',(-14.0003694708714,35.8359463819171,22.198670459132));
#46205=CARTESIAN_POINT('Ctrl Pts',(-13.9739476224999,35.9536641249992,22.1928193088599));
#46206=CARTESIAN_POINT('Ctrl Pts',(-13.9423982256983,36.0699164593606,22.1869681585878));
#46207=CARTESIAN_POINT('Ctrl Pts',(-13.9108091820569,36.186314883288,22.1811096554138));
#46208=CARTESIAN_POINT('Ctrl Pts',(-13.8740798226734,36.3012438337504,22.1752511522399));
#46209=CARTESIAN_POINT('Ctrl Pts',(-13.8323844851566,36.4142327099637,22.1693926490659));
#46210=CARTESIAN_POINT('Ctrl Pts',(-13.7906628672968,36.527292802447,22.1635304533095));
#46211=CARTESIAN_POINT('Ctrl Pts',(-13.7439691883516,36.6384100158729,22.157668257553));
#46212=CARTESIAN_POINT('Ctrl Pts',(-13.6925253126223,36.7471353169242,22.1518060617966));
#46213=CARTESIAN_POINT('Ctrl Pts',(-13.6409886366947,36.8560567487948,22.1459332911579));
#46214=CARTESIAN_POINT('Ctrl Pts',(-13.5846848248008,36.9625772912325,22.1400605205192));
#46215=CARTESIAN_POINT('Ctrl Pts',(-13.5238813533298,37.0662732654841,22.1341877498805));
#46216=CARTESIAN_POINT('Ctrl Pts',(-13.4639491572563,37.1684833418256,22.1283991323411));
#46217=CARTESIAN_POINT('Ctrl Pts',(-13.3996456789963,37.2679490084678,22.1226105148017));
#46218=CARTESIAN_POINT('Ctrl Pts',(-13.3312658119027,37.364295474438,22.1168218972623));
#46219=CARTESIAN_POINT('Ctrl Pts',(-13.2624727782426,37.4612240874675,22.1109983035913));
#46220=CARTESIAN_POINT('Ctrl Pts',(-13.1893348551766,37.5553040447086,22.1051747099203));
#46221=CARTESIAN_POINT('Ctrl Pts',(-13.1121159531809,37.6461215569125,22.0993511162492));
#46222=CARTESIAN_POINT('Ctrl Pts',(-13.0349944743,37.736824489335,22.0935348699066));
#46223=CARTESIAN_POINT('Ctrl Pts',(-12.9538025194293,37.8242728551197,22.087718623564));
#46224=CARTESIAN_POINT('Ctrl Pts',(-12.8688468720517,37.9080822933197,22.0819023772214));
#46225=CARTESIAN_POINT('Ctrl Pts',(-12.7839762657457,37.9918078378097,22.0760919529735));
#46226=CARTESIAN_POINT('Ctrl Pts',(-12.6953497508831,38.0719014160679,22.0702815287256));
#46227=CARTESIAN_POINT('Ctrl Pts',(-12.6033135194903,38.1480126618613,22.0644711044777));
#46228=CARTESIAN_POINT('Ctrl Pts',(-12.5077935263661,38.227004875741,22.0584407436534));
#46229=CARTESIAN_POINT('Ctrl Pts',(-12.4086008771728,38.3017069798914,22.052410382829));
#46230=CARTESIAN_POINT('Ctrl Pts',(-12.3061638909231,38.3717700259956,22.0463800220047));
#46231=CARTESIAN_POINT('Ctrl Pts',(-12.2075740342511,38.439201780153,22.0405761377719));
#46232=CARTESIAN_POINT('Ctrl Pts',(-12.1059795022868,38.50233639066,22.0347722535391));
#46233=CARTESIAN_POINT('Ctrl Pts',(-12.0017942403325,38.5609050562142,22.0289683693063));
#46234=CARTESIAN_POINT('Ctrl Pts',(-11.8976243676556,38.6194650705501,22.0231653423693));
#46235=CARTESIAN_POINT('Ctrl Pts',(-11.7908648818676,38.6734602811338,22.0173623154322));
#46236=CARTESIAN_POINT('Ctrl Pts',(-11.6819559081379,38.7226669637613,22.0115592884952));
#46237=CARTESIAN_POINT('Ctrl Pts',(-11.5730373188848,38.7718779908243,22.0057557492116));
#46238=CARTESIAN_POINT('Ctrl Pts',(-11.4619692365034,38.8162994812118,21.9999522099279));
#46239=CARTESIAN_POINT('Ctrl Pts',(-11.3492128233253,38.8557554068398,21.9941486706443));
#46240=CARTESIAN_POINT('Ctrl Pts',(-11.2364198445577,38.8952241275643,21.9883432493406));
#46241=CARTESIAN_POINT('Ctrl Pts',(-11.121937831351,38.9297239462582,21.9825378280369));
#46242=CARTESIAN_POINT('Ctrl Pts',(-11.0062435766446,38.9591285486154,21.9767324067331));
#46243=CARTESIAN_POINT('Ctrl Pts',(-10.8904212012593,38.9885657138481,21.9709205564627));
#46244=CARTESIAN_POINT('Ctrl Pts',(-10.773384300728,39.012896299226,21.9651087061922));
#46245=CARTESIAN_POINT('Ctrl Pts',(-10.6556204998727,39.0320449848863,21.9592968559217));
#46246=CARTESIAN_POINT('Ctrl Pts',(-10.5377793511207,39.0512062475061,21.9534811883967));
#46247=CARTESIAN_POINT('Ctrl Pts',(-10.4192107558254,39.0651787845738,21.9476655208718));
#46248=CARTESIAN_POINT('Ctrl Pts',(-10.3004064516139,39.0739392440031,21.9418498533468));
#46249=CARTESIAN_POINT('Ctrl Pts',(-10.1814319730652,39.0827122518446,21.9360258555061));
#46250=CARTESIAN_POINT('Ctrl Pts',(-10.0622215184218,39.086258268742,21.9302018576654));
#46251=CARTESIAN_POINT('Ctrl Pts',(-9.94326595422021,39.0846060089132,21.9243778598247));
#46252=CARTESIAN_POINT('Ctrl Pts',(-9.91170639454557,39.0841676553732,21.9228327214478));
#46253=CARTESIAN_POINT('Ctrl Pts',(-9.88016474084429,39.083363693142,21.9212875830708));
#46254=CARTESIAN_POINT('Ctrl Pts',(-9.8486500682641,39.0821952670302,21.9197424446939));
#46255=CARTESIAN_POINT('Ctrl Pts',(-9.72988906658912,39.077792128934,21.9139196908352));
#46256=CARTESIAN_POINT('Ctrl Pts',(-9.61112888814208,39.0681950209669,21.9080969369765));
#46257=CARTESIAN_POINT('Ctrl Pts',(-9.49286006791139,39.0533978449298,21.9022741831178));
#46258=CARTESIAN_POINT('Ctrl Pts',(-9.37473174465413,39.0386182471389,21.8964583463763));
#46259=CARTESIAN_POINT('Ctrl Pts',(-9.25709402035442,39.0186509142913,21.8906425096348));
#46260=CARTESIAN_POINT('Ctrl Pts',(-9.14043642794768,38.9935417195267,21.8848266728934));
#46261=CARTESIAN_POINT('Ctrl Pts',(-9.02388987407472,38.9684564245197,21.8790163718566));
#46262=CARTESIAN_POINT('Ctrl Pts',(-8.90832199345271,38.9382390867825,21.8732060708199));
#46263=CARTESIAN_POINT('Ctrl Pts',(-8.7942155633382,38.9029871755239,21.8673957697831));
#46264=CARTESIAN_POINT('Ctrl Pts',(-8.6789300613533,38.8673710031373,21.86152543039));
#46265=CARTESIAN_POINT('Ctrl Pts',(-8.56513680480514,38.8266156664125,21.8556550909969));
#46266=CARTESIAN_POINT('Ctrl Pts',(-8.4533218289518,38.7808744537743,21.8497847516038));
#46267=CARTESIAN_POINT('Ctrl Pts',(-8.34277846018579,38.7356534295073,21.8439811721874));
#46268=CARTESIAN_POINT('Ctrl Pts',(-8.23416899235596,38.6855595136954,21.838177592771));
#46269=CARTESIAN_POINT('Ctrl Pts',(-8.12794564672773,38.6307902030267,21.8323740133545));
#46270=CARTESIAN_POINT('Ctrl Pts',(-8.01988943187385,38.5750758554318,21.8264702939731));
#46271=CARTESIAN_POINT('Ctrl Pts',(-7.91430285340421,38.5145234231377,21.8205665745917));
#46272=CARTESIAN_POINT('Ctrl Pts',(-7.81163749354091,38.4493904592441,21.8146628552103));
#46273=CARTESIAN_POINT('Ctrl Pts',(-7.7089721336776,38.3842574953504,21.8087591358289));
#46274=CARTESIAN_POINT('Ctrl Pts',(-7.60922836451667,38.3145442437736,21.8028554164475));
#46275=CARTESIAN_POINT('Ctrl Pts',(-7.51282733495087,38.2405550657615,21.796951697066));
#46276=CARTESIAN_POINT('Ctrl Pts',(-7.51282733495086,38.2405550657615,23.0467784846721));
#46277=CARTESIAN_POINT('Ctrl Pts',(-7.41657395968785,38.1666792145524,23.0408768689581));
#46278=CARTESIAN_POINT('Ctrl Pts',(-7.3235466771998,38.0884588542002,23.0349752532441));
#46279=CARTESIAN_POINT('Ctrl Pts',(-7.23415348605168,38.0062132428156,23.0290736375301));
#46280=CARTESIAN_POINT('Ctrl Pts',(-7.14624403414103,37.9253327358551,23.0232699762429));
#46281=CARTESIAN_POINT('Ctrl Pts',(-7.06184926695299,37.8405598681496,23.0174663149557));
#46282=CARTESIAN_POINT('Ctrl Pts',(-6.98132337274585,37.7522384380844,23.0116626536685));
#46283=CARTESIAN_POINT('Ctrl Pts',(-6.9008064225061,37.6639268178326,23.0058596369908));
#46284=CARTESIAN_POINT('Ctrl Pts',(-6.82415776570052,37.5720677207802,23.0000566203132));
#46285=CARTESIAN_POINT('Ctrl Pts',(-6.75169343838683,37.4770404683373,22.9942536036355));
#46286=CARTESIAN_POINT('Ctrl Pts',(-6.67922005806772,37.3820013440913,22.988449861984));
#46287=CARTESIAN_POINT('Ctrl Pts',(-6.61093229428784,37.2837936021546,22.9826461203324));
#46288=CARTESIAN_POINT('Ctrl Pts',(-6.54710433902782,37.1828276511075,22.9768423786809));
#46289=CARTESIAN_POINT('Ctrl Pts',(-6.48139048348633,37.0788784975636,22.9708671560855));
#46290=CARTESIAN_POINT('Ctrl Pts',(-6.42040433136491,36.9720059953963,22.9648919334901));
#46291=CARTESIAN_POINT('Ctrl Pts',(-6.36439496966692,36.8626865177525,22.9589167108947));
#46292=CARTESIAN_POINT('Ctrl Pts',(-6.30991126876428,36.7563448358941,22.9531042497124));
#46293=CARTESIAN_POINT('Ctrl Pts',(-6.26013684913735,36.6476881651299,22.9472917885301));
#46294=CARTESIAN_POINT('Ctrl Pts',(-6.21525214167994,36.5371755426566,22.9414793273478));
#46295=CARTESIAN_POINT('Ctrl Pts',(-6.16848213171892,36.4220210335447,22.9354227240459));
#46296=CARTESIAN_POINT('Ctrl Pts',(-6.12702172979419,36.3048517336437,22.9293661207439));
#46297=CARTESIAN_POINT('Ctrl Pts',(-6.09101723354879,36.1862034950157,22.923309517442));
#46298=CARTESIAN_POINT('Ctrl Pts',(-6.05501273730338,36.0675552563876,22.91725291414));
#46299=CARTESIAN_POINT('Ctrl Pts',(-6.02446420208395,35.9474285749655,22.911196310838));
#46300=CARTESIAN_POINT('Ctrl Pts',(-5.99945759808047,35.8263688585879,22.9051397075361));
#46301=CARTESIAN_POINT('Ctrl Pts',(-5.97541304809779,35.7099665513844,22.8993161138646));
#46302=CARTESIAN_POINT('Ctrl Pts',(-5.95641431380094,35.592326242637,22.8934925201932));
#46303=CARTESIAN_POINT('Ctrl Pts',(-5.94258432963635,35.4739230716978,22.8876689265217));
#46304=CARTESIAN_POINT('Ctrl Pts',(-5.92877179405107,35.3556692839461,22.8818526801787));
#46305=CARTESIAN_POINT('Ctrl Pts',(-5.92011508514747,35.2366549503255,22.8760364338357));
#46306=CARTESIAN_POINT('Ctrl Pts',(-5.91668638256212,35.1173665269419,22.8702201874927));
#46307=CARTESIAN_POINT('Ctrl Pts',(-5.91326111212698,34.9981975119284,22.8644097632444));
#46308=CARTESIAN_POINT('Ctrl Pts',(-5.91505344874562,34.8787553587903,22.8585993389961));
#46309=CARTESIAN_POINT('Ctrl Pts',(-5.92208383683801,34.7595321929608,22.8527889147477));
#46310=CARTESIAN_POINT('Ctrl Pts',(-5.92938033966108,34.6357961837083,22.8467585539236));
#46311=CARTESIAN_POINT('Ctrl Pts',(-5.94231932317017,34.512296512764,22.8407281930994));
#46312=CARTESIAN_POINT('Ctrl Pts',(-5.96086422097439,34.3895844377842,22.8346978322752));
#46313=CARTESIAN_POINT('Ctrl Pts',(-5.97871264549011,34.2714809448146,22.828893948042));
#46314=CARTESIAN_POINT('Ctrl Pts',(-6.00175343918375,34.1541073967008,22.8230900638088));
#46315=CARTESIAN_POINT('Ctrl Pts',(-6.02990118229129,34.0379499089819,22.8172861795755));
#46316=CARTESIAN_POINT('Ctrl Pts',(-6.05804476767612,33.9218095789663,22.8114831526381));
#46317=CARTESIAN_POINT('Ctrl Pts',(-6.09129370616824,33.8068853488722,22.8056801257006));
#46318=CARTESIAN_POINT('Ctrl Pts',(-6.12951174889358,33.6936517699912,22.7998770987632));
#46319=CARTESIAN_POINT('Ctrl Pts',(-6.16773316587247,33.5804081937692,22.7940735594791));
#46320=CARTESIAN_POINT('Ctrl Pts',(-6.21092442877671,33.4688559524523,22.7882700201951));
#46321=CARTESIAN_POINT('Ctrl Pts',(-6.25890004806708,33.3594524847943,22.782466480911));
#46322=CARTESIAN_POINT('Ctrl Pts',(-6.30689122529137,33.2500135388675,22.7766610596068));
#46323=CARTESIAN_POINT('Ctrl Pts',(-6.35966968060203,33.14272512619,22.7708556383027));
#46324=CARTESIAN_POINT('Ctrl Pts',(-6.41700289212914,33.0380222414642,22.7650502169985));
#46325=CARTESIAN_POINT('Ctrl Pts',(-6.47439959488128,32.9332034079848,22.7592383667276));
#46326=CARTESIAN_POINT('Ctrl Pts',(-6.53636092581199,32.8309761760842,22.7534265164567));
#46327=CARTESIAN_POINT('Ctrl Pts',(-6.60260966410514,32.731748711988,22.7476146661858));
#46328=CARTESIAN_POINT('Ctrl Pts',(-6.66890191492497,32.6324560747611,22.7417989986604));
#46329=CARTESIAN_POINT('Ctrl Pts',(-6.73948694036518,32.5361674577396,22.7359833311351));
#46330=CARTESIAN_POINT('Ctrl Pts',(-6.81404668775278,32.4432586184401,22.7301676636097));
#46331=CARTESIAN_POINT('Ctrl Pts',(-6.88871323392784,32.3502166972602,22.7243436657686));
#46332=CARTESIAN_POINT('Ctrl Pts',(-6.96736559735073,32.2605645223719,22.7185196679275));
#46333=CARTESIAN_POINT('Ctrl Pts',(-7.0496482181394,32.1746417283339,22.7126956700863));
#46334=CARTESIAN_POINT('Ctrl Pts',(-7.07147824594366,32.1518459427246,22.7111505317134));
#46335=CARTESIAN_POINT('Ctrl Pts',(-7.09356361386295,32.1293124389546,22.7096053933405));
#46336=CARTESIAN_POINT('Ctrl Pts',(-7.11589729903296,32.1070470777639,22.7080602549676));
#46337=CARTESIAN_POINT('Ctrl Pts',(-7.20007248353149,32.0231294048904,22.7022366612962));
#46338=CARTESIAN_POINT('Ctrl Pts',(-7.28804902917342,31.9427532793078,22.6964130676248));
#46339=CARTESIAN_POINT('Ctrl Pts',(-7.37949693130055,31.8662819739267,22.6905894739534));
#46340=CARTESIAN_POINT('Ctrl Pts',(-7.47082945831563,31.7899071484562,22.6847732276105));
#46341=CARTESIAN_POINT('Ctrl Pts',(-7.56562432034542,31.7174276041097,22.6789569812675));
#46342=CARTESIAN_POINT('Ctrl Pts',(-7.66351422578696,31.6491703673717,22.6731407349246));
#46343=CARTESIAN_POINT('Ctrl Pts',(-7.7613061428933,31.580981456504,22.6673303106763));
#46344=CARTESIAN_POINT('Ctrl Pts',(-7.86218660699066,31.5170066772535,22.661519886428));
#46345=CARTESIAN_POINT('Ctrl Pts',(-7.96575522545295,31.4575328939808,22.6557094621797));
#46346=CARTESIAN_POINT('Ctrl Pts',(-8.07324413034226,31.3958079049975,22.6496791013556));
#46347=CARTESIAN_POINT('Ctrl Pts',(-8.18362837108477,31.3389316761016,22.6436487405314));
#46348=CARTESIAN_POINT('Ctrl Pts',(-8.29642684731927,31.2871758035876,22.6376183797072));
#46349=CARTESIAN_POINT('Ctrl Pts',(-8.40498905724828,31.2373636777106,22.631814495474));
#46350=CARTESIAN_POINT('Ctrl Pts',(-8.51578703002254,31.192294428774,22.6260106112408));
#46351=CARTESIAN_POINT('Ctrl Pts',(-8.62836736862838,31.1521630849844,22.6202067270077));
#46352=CARTESIAN_POINT('Ctrl Pts',(-8.74093107791437,31.1120376690235,22.6144037000702));
#46353=CARTESIAN_POINT('Ctrl Pts',(-8.8552762449359,31.0768488447719,22.6086006731328));
#46354=CARTESIAN_POINT('Ctrl Pts',(-8.97093128201541,31.0467427893362,22.6027976461954));
#46355=CARTESIAN_POINT('Ctrl Pts',(-9.08659653022548,31.0166340758505,22.5969941069114));
#46356=CARTESIAN_POINT('Ctrl Pts',(-9.20357148324194,30.9916091262857,22.5911905676274));
#46357=CARTESIAN_POINT('Ctrl Pts',(-9.32137187388096,30.9717635538067,22.5853870283434));
#46358=CARTESIAN_POINT('Ctrl Pts',(-9.43921046581253,30.95191154564,22.5795816070393));
#46359=CARTESIAN_POINT('Ctrl Pts',(-9.55787462526565,30.9372423227284,22.5737761857352));
#46360=CARTESIAN_POINT('Ctrl Pts',(-9.67687307520295,30.9277998587408,22.5679707644311));
#46361=CARTESIAN_POINT('Ctrl Pts',(-9.79600330490938,30.9183469380984,22.5621589141602));
#46362=CARTESIAN_POINT('Ctrl Pts',(-9.91546815674363,30.9141323623456,22.5563470638893));
#46363=CARTESIAN_POINT('Ctrl Pts',(-10.0347742898978,30.915148013849,22.5505352136185));
#46364=CARTESIAN_POINT('Ctrl Pts',(-10.1541587839607,30.9161643324377,22.5447195460931));
#46365=CARTESIAN_POINT('Ctrl Pts',(-10.2733839448934,30.9224176983138,22.5389038785678));
#46366=CARTESIAN_POINT('Ctrl Pts',(-10.3919611550605,30.9338480779829,22.5330882110425));
#46367=CARTESIAN_POINT('Ctrl Pts',(-10.5107082142768,30.9452948304366,22.5272642132014));
#46368=CARTESIAN_POINT('Ctrl Pts',(-10.6288050673429,30.9619333408792,22.5214402153604));
#46369=CARTESIAN_POINT('Ctrl Pts',(-10.7457727487375,30.9836524045794,22.5156162175193));
#46370=CARTESIAN_POINT('Ctrl Pts',(-10.7768049121928,30.989414590568,22.5140710791459));
#46371=CARTESIAN_POINT('Ctrl Pts',(-10.8077576788365,30.9955341090123,22.5125259407726));
#46372=CARTESIAN_POINT('Ctrl Pts',(-10.8386222972362,31.0020082988357,22.5109808023992));
#46373=CARTESIAN_POINT('Ctrl Pts',(-10.9549503876449,31.0264093826057,22.5051572087275));
#46374=CARTESIAN_POINT('Ctrl Pts',(-11.0704001978096,31.0559311623806,22.4993336150558));
#46375=CARTESIAN_POINT('Ctrl Pts',(-11.1844870002163,31.0904967647643,22.4935100213841));
#46376=CARTESIAN_POINT('Ctrl Pts',(-11.2984298651754,31.1250187575062,22.4876937750409));
#46377=CARTESIAN_POINT('Ctrl Pts',(-11.411012755344,31.1645717985846,22.4818775286976));
#46378=CARTESIAN_POINT('Ctrl Pts',(-11.5217608193279,31.2090279599081,22.4760612823544));
#46379=CARTESIAN_POINT('Ctrl Pts',(-11.6323980238884,31.2534396203687,22.4702508581059));
#46380=CARTESIAN_POINT('Ctrl Pts',(-11.7412036793263,31.3027444858749,22.4644404338573));
#46381=CARTESIAN_POINT('Ctrl Pts',(-11.8477183799133,31.3567649281812,22.4586300096088));
#46382=CARTESIAN_POINT('Ctrl Pts',(-11.9582648822224,31.4128301559596,22.4525996487847));
#46383=CARTESIAN_POINT('Ctrl Pts',(-12.0663431391599,31.4739748727744,22.4465692879606));
#46384=CARTESIAN_POINT('Ctrl Pts',(-12.1714622737273,31.5399455793616,22.4405389271365));
#46385=CARTESIAN_POINT('Ctrl Pts',(-12.2726335478101,31.6034386861594,22.434735042903));
#46386=CARTESIAN_POINT('Ctrl Pts',(-12.3710635802309,31.6714015928774,22.4289311586696));
#46387=CARTESIAN_POINT('Ctrl Pts',(-12.4663407192963,31.7435619986953,22.4231272744361));
#46388=CARTESIAN_POINT('Ctrl Pts',(-12.5616037849094,31.8157117456497,22.4173242474984));
#46389=CARTESIAN_POINT('Ctrl Pts',(-12.6537145579033,31.8920575122198,22.4115212205607));
#46390=CARTESIAN_POINT('Ctrl Pts',(-12.7422922727758,31.9722850050452,22.405718193623));
#46391=CARTESIAN_POINT('Ctrl Pts',(-12.830877808134,32.052519581119,22.3999146543387));
#46392=CARTESIAN_POINT('Ctrl Pts',(-12.9159293625088,32.1366362907165,22.3941111150544));
#46393=CARTESIAN_POINT('Ctrl Pts',(-12.9971015101764,32.2242825183931,22.3883075757702));
#46394=CARTESIAN_POINT('Ctrl Pts',(-13.0782999810246,32.3119571687189,22.3825021544658));
#46395=CARTESIAN_POINT('Ctrl Pts',(-13.1556162658772,32.4031633140018,22.3766967331614));
#46396=CARTESIAN_POINT('Ctrl Pts',(-13.228744286248,32.4975141690669,22.370891311857));
#46397=CARTESIAN_POINT('Ctrl Pts',(-13.3019532891329,32.5919695089712,22.3650794615859));
#46398=CARTESIAN_POINT('Ctrl Pts',(-13.3709645191639,32.6895761870393,22.3592676113147));
#46399=CARTESIAN_POINT('Ctrl Pts',(-13.4355143342332,32.7899171374634,22.3534557610436));
#46400=CARTESIAN_POINT('Ctrl Pts',(-13.5001065459675,32.8903239923622,22.347640093518));
#46401=CARTESIAN_POINT('Ctrl Pts',(-13.5602313018439,32.9934683442013,22.3418244259924));
#46402=CARTESIAN_POINT('Ctrl Pts',(-13.615670969754,33.0989086191143,22.3360087584668));
#46403=CARTESIAN_POINT('Ctrl Pts',(-13.6711900490022,33.2044999258359,22.3301847606255));
#46404=CARTESIAN_POINT('Ctrl Pts',(-13.7220104723443,33.3123933515242,22.3243607627841));
#46405=CARTESIAN_POINT('Ctrl Pts',(-13.7679626967556,33.4221273448537,22.3185367649427));
#46406=CARTESIAN_POINT('Ctrl Pts',(-13.7801540723517,33.4512403713825,22.3169916265721));
#46407=CARTESIAN_POINT('Ctrl Pts',(-13.7920030629533,33.4804828693455,22.3154464882014));
#46408=CARTESIAN_POINT('Ctrl Pts',(-13.8035070969918,33.5098460605921,22.3139013498308));
#46409=CARTESIAN_POINT('Ctrl Pts',(-13.8524065999432,33.6346584048717,22.3073335234437));
#46410=CARTESIAN_POINT('Ctrl Pts',(-13.8952013288733,33.7619885269329,22.3007656970566));
#46411=CARTESIAN_POINT('Ctrl Pts',(-13.9316569522712,33.8912626056376,22.2941978706695));
#46412=CARTESIAN_POINT('Ctrl Pts',(-13.9679980306452,34.020130500027,22.2876506806551));
#46413=CARTESIAN_POINT('Ctrl Pts',(-13.998039658383,34.1509299686843,22.2811034906407));
#46414=CARTESIAN_POINT('Ctrl Pts',(-14.0215963303964,34.2830704669619,22.2745563006263));
#46415=CARTESIAN_POINT('Ctrl Pts',(-14.045014957528,34.4144366063038,22.2680474779191));
#46416=CARTESIAN_POINT('Ctrl Pts',(-14.0620243166781,34.5471279040333,22.2615386552119));
#46417=CARTESIAN_POINT('Ctrl Pts',(-14.0724898512343,34.6805451337141,22.2550298325047));
#46418=CARTESIAN_POINT('Ctrl Pts',(-14.0807516711158,34.7858688622623,22.2498915645492));
#46419=CARTESIAN_POINT('Ctrl Pts',(-14.0849362747585,34.8916445871562,22.2447532965937));
#46420=CARTESIAN_POINT('Ctrl Pts',(-14.0849992774348,34.997570317556,22.2396150286382));
#46421=CARTESIAN_POINT('Origin',(-10.,35.,32.7603849714045));
#46422=CARTESIAN_POINT('',(-7.51282733495087,38.2405550657615,24.2969436900965));
#46423=CARTESIAN_POINT('',(-7.51282733495086,38.2405550657615,24.1926554110861));
#46424=CARTESIAN_POINT('',(-7.51282733495086,38.2405550657615,32.7603849714045));
#46425=CARTESIAN_POINT('',(-14.0849994926668,35.0020359057622,23.3853849713652));
#46426=CARTESIAN_POINT('Ctrl Pts',(-7.51282733495086,38.2405550657615,24.1926554110861));
#46427=CARTESIAN_POINT('Ctrl Pts',(-7.41801595757955,38.1677859686938,24.1868522021358));
#46428=CARTESIAN_POINT('Ctrl Pts',(-7.32640211884168,38.090853475721,24.1810489931854));
#46429=CARTESIAN_POINT('Ctrl Pts',(-7.23836078677592,38.0100787125893,24.175245784235));
#46430=CARTESIAN_POINT('Ctrl Pts',(-7.15029803900647,37.9292843013178,24.1694411636772));
#46431=CARTESIAN_POINT('Ctrl Pts',(-7.06580982687109,37.8446460372456,24.1636365431193));
#46432=CARTESIAN_POINT('Ctrl Pts',(-6.98523496836354,37.7565225926921,24.1578319225615));
#46433=CARTESIAN_POINT('Ctrl Pts',(-6.90457399469106,37.6683049653488,24.1520210982589));
#46434=CARTESIAN_POINT('Ctrl Pts',(-6.82783500204308,37.5765950215359,24.1462102739563));
#46435=CARTESIAN_POINT('Ctrl Pts',(-6.75531726620277,37.4817854373411,24.1403994496536));
#46436=CARTESIAN_POINT('Ctrl Pts',(-6.68275717128929,37.3869204729545,24.1345852311313));
#46437=CARTESIAN_POINT('Ctrl Pts',(-6.61442347813049,37.2889525962203,24.1287710126089));
#46438=CARTESIAN_POINT('Ctrl Pts',(-6.55057180331045,37.1883030219517,24.1229567940865));
#46439=CARTESIAN_POINT('Ctrl Pts',(-6.48662268280583,37.087499843777,24.1171337023356));
#46440=CARTESIAN_POINT('Ctrl Pts',(-6.42716944479547,36.9840071480697,24.1113106105847));
#46441=CARTESIAN_POINT('Ctrl Pts',(-6.3724216621271,36.8782705882261,24.1054875188338));
#46442=CARTESIAN_POINT('Ctrl Pts',(-6.3391164979892,36.8139470063507,24.1019451100438));
#46443=CARTESIAN_POINT('Ctrl Pts',(-6.30755177516101,36.7487934398425,24.0984027012539));
#46444=CARTESIAN_POINT('Ctrl Pts',(-6.27776578209767,36.6829133747989,24.0948602924639));
#46445=CARTESIAN_POINT('Ctrl Pts',(-6.22879867214834,36.5746088982081,24.0890366987924));
#46446=CARTESIAN_POINT('Ctrl Pts',(-6.18448346565953,36.4639908317763,24.0832131051209));
#46447=CARTESIAN_POINT('Ctrl Pts',(-6.14504422535157,36.3514958288891,24.0773895114494));
#46448=CARTESIAN_POINT('Ctrl Pts',(-6.1056547435035,36.2391427551579,24.0715732651064));
#46449=CARTESIAN_POINT('Ctrl Pts',(-6.07112912604364,36.1249178368807,24.0657570187633));
#46450=CARTESIAN_POINT('Ctrl Pts',(-6.04164439422485,36.0092798909264,24.0599407724203));
#46451=CARTESIAN_POINT('Ctrl Pts',(-6.01218917678531,35.8937576991942,24.0541303481719));
#46452=CARTESIAN_POINT('Ctrl Pts',(-5.98776490699338,35.7768256870582,24.0483199239235));
#46453=CARTESIAN_POINT('Ctrl Pts',(-5.96849937054938,35.6589595395312,24.0425094996752));
#46454=CARTESIAN_POINT('Ctrl Pts',(-5.94850459370311,35.536631914532,24.036479138851));
#46455=CARTESIAN_POINT('Ctrl Pts',(-5.93406695235358,35.413298461934,24.0304487780269));
#46456=CARTESIAN_POINT('Ctrl Pts',(-5.92527156445519,35.2895050544681,24.0244184172027));
#46457=CARTESIAN_POINT('Ctrl Pts',(-5.91680649666945,35.1703608395985,24.0186145329694));
#46458=CARTESIAN_POINT('Ctrl Pts',(-5.91356755497438,35.0507910389473,24.0128106487362));
#46459=CARTESIAN_POINT('Ctrl Pts',(-5.91557791684954,34.9312886714371,24.0070067645029));
#46460=CARTESIAN_POINT('Ctrl Pts',(-5.91758798177276,34.8118039557044,24.0012037375654));
#46461=CARTESIAN_POINT('Ctrl Pts',(-5.92484580141719,34.6923870614731,23.9954007106279));
#46462=CARTESIAN_POINT('Ctrl Pts',(-5.93732242544661,34.5735308625223,23.9895976836904));
#46463=CARTESIAN_POINT('Ctrl Pts',(-5.94980015103141,34.4546641698125,23.9837941444063));
#46464=CARTESIAN_POINT('Ctrl Pts',(-5.96749755448297,34.3363586769337,23.9779906051222));
#46465=CARTESIAN_POINT('Ctrl Pts',(-5.99033389170669,34.2191013510039,23.9721870658381));
#46466=CARTESIAN_POINT('Ctrl Pts',(-6.01317763448839,34.10180599989,23.9663816445339));
#46467=CARTESIAN_POINT('Ctrl Pts',(-6.04116354730872,33.9855598923264,23.9605762232297));
#46468=CARTESIAN_POINT('Ctrl Pts',(-6.07416007869768,33.870838402925,23.9547708019254));
#46469=CARTESIAN_POINT('Ctrl Pts',(-6.10719315069095,33.7559898700929,23.9489589516545));
#46470=CARTESIAN_POINT('Ctrl Pts',(-6.14524780418735,33.642669718221,23.9431471013835));
#46471=CARTESIAN_POINT('Ctrl Pts',(-6.18814299626849,33.5313369402402,23.9373352511126));
#46472=CARTESIAN_POINT('Ctrl Pts',(-6.231066362142,33.4199310382933,23.9315195835871));
#46473=CARTESIAN_POINT('Ctrl Pts',(-6.27883643523125,33.3105154831759,23.9257039160617));
#46474=CARTESIAN_POINT('Ctrl Pts',(-6.33122523149234,33.2035265941402,23.9198882485363));
#46475=CARTESIAN_POINT('Ctrl Pts',(-6.38368906904711,33.0963844550736,23.9140642506952));
#46476=CARTESIAN_POINT('Ctrl Pts',(-6.44078463980339,32.9916762771008,23.908240252854));
#46477=CARTESIAN_POINT('Ctrl Pts',(-6.50223944854455,32.8898113532951,23.9024162550128));
#46478=CARTESIAN_POINT('Ctrl Pts',(-6.51854374427875,32.8627860337687,23.9008711166404));
#46479=CARTESIAN_POINT('Ctrl Pts',(-6.53515464753998,32.8359606696416,23.8993259782679));
#46480=CARTESIAN_POINT('Ctrl Pts',(-6.5520665903944,32.809342518118,23.8977808398955));
#46481=CARTESIAN_POINT('Ctrl Pts',(-6.6158073434137,32.7090192710078,23.891957246224));
#46482=CARTESIAN_POINT('Ctrl Pts',(-6.68403312025836,32.6113185160413,23.8861336525526));
#46483=CARTESIAN_POINT('Ctrl Pts',(-6.75650153965819,32.5166670102944,23.8803100588811));
#46484=CARTESIAN_POINT('Ctrl Pts',(-6.82887852938271,32.4221349214811,23.8744938125381));
#46485=CARTESIAN_POINT('Ctrl Pts',(-6.90548726917439,32.3306447514965,23.8686775661951));
#46486=CARTESIAN_POINT('Ctrl Pts',(-6.98604105444614,32.2425960625045,23.862861319852));
#46487=CARTESIAN_POINT('Ctrl Pts',(-7.06651420493434,32.1546355107359,23.8570508956037));
#46488=CARTESIAN_POINT('Ctrl Pts',(-7.15092427078563,32.0701098862195,23.8512404713553));
#46489=CARTESIAN_POINT('Ctrl Pts',(-7.2389434502476,31.9893868184256,23.845430047107));
#46490=CARTESIAN_POINT('Ctrl Pts',(-7.33029433770718,31.9056082155517,23.8393996862828));
#46491=CARTESIAN_POINT('Ctrl Pts',(-7.42553268961834,31.825926082405,23.8333693254587));
#46492=CARTESIAN_POINT('Ctrl Pts',(-7.52424861234205,31.7507108367353,23.8273389646345));
#46493=CARTESIAN_POINT('Ctrl Pts',(-7.61925715398179,31.6783203793198,23.8215350804013));
#46494=CARTESIAN_POINT('Ctrl Pts',(-7.71748641525967,31.6100676123452,23.815731196168));
#46495=CARTESIAN_POINT('Ctrl Pts',(-7.81853675442483,31.5462421758026,23.8099273119348));
#46496=CARTESIAN_POINT('Ctrl Pts',(-7.91957216737421,31.4824261669596,23.8041242849973));
#46497=CARTESIAN_POINT('Ctrl Pts',(-8.0234274843748,31.423036406021,23.7983212580599));
#46498=CARTESIAN_POINT('Ctrl Pts',(-8.12967461049948,31.3683188552146,23.7925182311224));
#46499=CARTESIAN_POINT('Ctrl Pts',(-8.2359311171346,31.3135964734205,23.7867146918383));
#46500=CARTESIAN_POINT('Ctrl Pts',(-8.34457948971319,31.2635473088899,23.7809111525543));
#46501=CARTESIAN_POINT('Ctrl Pts',(-8.45516818201734,31.218370767229,23.7751076132702));
#46502=CARTESIAN_POINT('Ctrl Pts',(-8.5657927369445,31.1731795753425,23.769302191966));
#46503=CARTESIAN_POINT('Ctrl Pts',(-8.67835848516235,31.1328643031991,23.7634967706618));
#46504=CARTESIAN_POINT('Ctrl Pts',(-8.79239572533773,31.0975755079928,23.7576913493577));
#46505=CARTESIAN_POINT('Ctrl Pts',(-8.90655925120153,31.0622476337121,23.7518794990867));
#46506=CARTESIAN_POINT('Ctrl Pts',(-9.02219713140855,31.0319574680794,23.7460676488158));
#46507=CARTESIAN_POINT('Ctrl Pts',(-9.13882623638185,31.0068051952283,23.7402557985449));
#46508=CARTESIAN_POINT('Ctrl Pts',(-9.25553194397738,30.9816364022293,23.7344401310195));
#46509=CARTESIAN_POINT('Ctrl Pts',(-9.37322977127797,30.9616122909336,23.7286244634941));
#46510=CARTESIAN_POINT('Ctrl Pts',(-9.49142982090204,30.946781356387,23.7228087959687));
#46511=CARTESIAN_POINT('Ctrl Pts',(-9.60979917933367,30.9319291781281,23.7169847981276));
#46512=CARTESIAN_POINT('Ctrl Pts',(-9.72867179037554,30.9222850566915,23.7111608002865));
#46513=CARTESIAN_POINT('Ctrl Pts',(-9.8475559611583,30.9178454444961,23.7053368024454));
#46514=CARTESIAN_POINT('Ctrl Pts',(-9.87909657968253,30.9166675911811,23.7037916640726));
#46515=CARTESIAN_POINT('Ctrl Pts',(-9.91063803235893,30.9158557838219,23.7022465256998));
#46516=CARTESIAN_POINT('Ctrl Pts',(-9.94217119733301,30.915409343694,23.700701387327));
#46517=CARTESIAN_POINT('Ctrl Pts',(-10.0610190256046,30.9137267203452,23.6948777936556));
#46518=CARTESIAN_POINT('Ctrl Pts',(-10.1801320038198,30.9172327961846,23.6890541999841));
#46519=CARTESIAN_POINT('Ctrl Pts',(-10.2990203400902,30.9259587831967,23.6832306063126));
#46520=CARTESIAN_POINT('Ctrl Pts',(-10.4177586810649,30.93467376108,23.6774143599696));
#46521=CARTESIAN_POINT('Ctrl Pts',(-10.5362725401572,30.9485955217199,23.6715981136266));
#46522=CARTESIAN_POINT('Ctrl Pts',(-10.6540705740902,30.9677032990975,23.6657818672836));
#46523=CARTESIAN_POINT('Ctrl Pts',(-10.7717506915413,30.9867919494845,23.6599714430352));
#46524=CARTESIAN_POINT('Ctrl Pts',(-10.8887160085587,31.0110562242921,23.6541610187869));
#46525=CARTESIAN_POINT('Ctrl Pts',(-11.0044793614797,31.0404234806786,23.6483505945386));
#46526=CARTESIAN_POINT('Ctrl Pts',(-11.1246245967487,31.0709023484613,23.6423202337144));
#46527=CARTESIAN_POINT('Ctrl Pts',(-11.2434746293577,31.1068781148384,23.6362898728902));
#46528=CARTESIAN_POINT('Ctrl Pts',(-11.3604949638257,31.1482110061161,23.6302595120661));
#46529=CARTESIAN_POINT('Ctrl Pts',(-11.4731204756299,31.1879915968627,23.6244556278328));
#46530=CARTESIAN_POINT('Ctrl Pts',(-11.5840508237368,31.2327340357742,23.6186517435996));
#46531=CARTESIAN_POINT('Ctrl Pts',(-11.6928246925636,31.2822628441151,23.6128478593664));
#46532=CARTESIAN_POINT('Ctrl Pts',(-11.8015824943266,31.3317843365213,23.6070448324289));
#46533=CARTESIAN_POINT('Ctrl Pts',(-11.9081840787502,31.3860906231921,23.6012418054915));
#46534=CARTESIAN_POINT('Ctrl Pts',(-12.0121890640777,31.4449584854174,23.595438778554));
#46535=CARTESIAN_POINT('Ctrl Pts',(-12.1162032319578,31.5038315450593,23.58963523927));
#46536=CARTESIAN_POINT('Ctrl Pts',(-12.2176199895527,31.5672667798505,23.5838316999859));
#46537=CARTESIAN_POINT('Ctrl Pts',(-12.3160250385771,31.6349958364537,23.5780281607019));
#46538=CARTESIAN_POINT('Ctrl Pts',(-12.4144619992115,31.7027468568003,23.5722227393977));
#46539=CARTESIAN_POINT('Ctrl Pts',(-12.5098849727222,31.7747942368095,23.5664173180935));
#46540=CARTESIAN_POINT('Ctrl Pts',(-12.6019105642536,31.8508276618093,23.5606118967894));
#46541=CARTESIAN_POINT('Ctrl Pts',(-12.6940380656099,31.9269452867898,23.5548000465184));
#46542=CARTESIAN_POINT('Ctrl Pts',(-12.7827603601636,32.0070575075925,23.5489881962475));
#46543=CARTESIAN_POINT('Ctrl Pts',(-12.8677288227591,32.0908151658727,23.5431763459766));
#46544=CARTESIAN_POINT('Ctrl Pts',(-12.9527530930976,32.174627836633,23.5373606784512));
#46545=CARTESIAN_POINT('Ctrl Pts',(-13.0340183439925,32.2620904148114,23.5315450109258));
#46546=CARTESIAN_POINT('Ctrl Pts',(-13.1112154716859,32.3528197475914,23.5257293434004));
#46547=CARTESIAN_POINT('Ctrl Pts',(-13.1885231759283,32.4436790403428,23.5199053455592));
#46548=CARTESIAN_POINT('Ctrl Pts',(-13.2617508764709,32.5378141061121,23.5140813477181));
#46549=CARTESIAN_POINT('Ctrl Pts',(-13.3306320122865,32.6348117625161,23.508257349877));
#46550=CARTESIAN_POINT('Ctrl Pts',(-13.3489065530772,32.6605457694769,23.5067122115042));
#46551=CARTESIAN_POINT('Ctrl Pts',(-13.3668754008443,32.6864811271589,23.5051670731314));
#46552=CARTESIAN_POINT('Ctrl Pts',(-13.384534122985,32.7126098342542,23.5036219347586));
#46553=CARTESIAN_POINT('Ctrl Pts',(-13.4520539487645,32.8125154637139,23.4977139492936));
#46554=CARTESIAN_POINT('Ctrl Pts',(-13.5152498617656,32.9155658287591,23.4918059638286));
#46555=CARTESIAN_POINT('Ctrl Pts',(-13.5738211458682,33.0213571779258,23.4858979783635));
#46556=CARTESIAN_POINT('Ctrl Pts',(-13.632313063434,33.1270051753951,23.4799979984656));
#46557=CARTESIAN_POINT('Ctrl Pts',(-13.6861926320066,33.2353864267388,23.4740980185677));
#46558=CARTESIAN_POINT('Ctrl Pts',(-13.7352017518379,33.3460674520807,23.4681980386698));
#46559=CARTESIAN_POINT('Ctrl Pts',(-13.7841547944733,33.456621834023,23.4623048096446));
#46560=CARTESIAN_POINT('Ctrl Pts',(-13.8282483207179,33.5694703964324,23.4564115806194));
#46561=CARTESIAN_POINT('Ctrl Pts',(-13.8672698330022,33.6841546296196,23.4505183515942));
#46562=CARTESIAN_POINT('Ctrl Pts',(-13.9062483904797,33.7987126186204,23.4446316098243));
#46563=CARTESIAN_POINT('Ctrl Pts',(-13.9401659294038,33.9151018831737,23.4387448680545));
#46564=CARTESIAN_POINT('Ctrl Pts',(-13.9688580865625,34.0328441238729,23.4328581262846));
#46565=CARTESIAN_POINT('Ctrl Pts',(-13.9975315945566,34.150509835142,23.4269752107456));
#46566=CARTESIAN_POINT('Ctrl Pts',(-14.020986387276,34.2695263920299,23.4210922952066));
#46567=CARTESIAN_POINT('Ctrl Pts',(-14.0391079923919,34.3894006012155,23.4152093796675));
#46568=CARTESIAN_POINT('Ctrl Pts',(-14.0572220478135,34.5092248692604,23.409328915027));
#46569=CARTESIAN_POINT('Ctrl Pts',(-14.0700072787421,34.6299056907764,23.4034484503864));
#46570=CARTESIAN_POINT('Ctrl Pts',(-14.0774004327816,34.7509403469993,23.3975679857458));
#46571=CARTESIAN_POINT('Ctrl Pts',(-14.0825060895164,34.8345259728912,23.3935069809654));
#46572=CARTESIAN_POINT('Ctrl Pts',(-14.0850412353373,34.9182801351345,23.3894459761849));
#46573=CARTESIAN_POINT('Ctrl Pts',(-14.0849994926672,35.0020359049511,23.3853849714045));
#46574=CARTESIAN_POINT('Ctrl Pts',(-14.0849994926668,35.0020359057622,23.3853849713652));
#46575=CARTESIAN_POINT('Ctrl Pts',(-14.0849319581215,35.1375424641162,23.3788147639339));
#46576=CARTESIAN_POINT('Ctrl Pts',(-14.0781173618785,35.2728211146141,23.3722445565027));
#46577=CARTESIAN_POINT('Ctrl Pts',(-14.0646509392799,35.4072318035354,23.3656743490714));
#46578=CARTESIAN_POINT('Ctrl Pts',(-14.0514755036666,35.5387381011188,23.3592461128904));
#46579=CARTESIAN_POINT('Ctrl Pts',(-14.0319329338456,35.6694133588879,23.3528178767094));
#46580=CARTESIAN_POINT('Ctrl Pts',(-14.0061633244727,35.7986741623779,23.3463896405284));
#46581=CARTESIAN_POINT('Ctrl Pts',(-13.9795400103919,35.9322171633543,23.339748447472));
#46582=CARTESIAN_POINT('Ctrl Pts',(-13.9462701124894,36.0642500789004,23.3331072544156));
#46583=CARTESIAN_POINT('Ctrl Pts',(-13.9065621511343,36.1941512296711,23.3264660613593));
#46584=CARTESIAN_POINT('Ctrl Pts',(-13.8668541897792,36.3240523804417,23.3198248683029));
#46585=CARTESIAN_POINT('Ctrl Pts',(-13.8207083428048,36.451821524871,23.3131836752465));
#46586=CARTESIAN_POINT('Ctrl Pts',(-13.7683854637982,36.5768627068437,23.3065424821901));
#46587=CARTESIAN_POINT('Ctrl Pts',(-13.7225040710322,36.6865100292187,23.3007188885187));
#46588=CARTESIAN_POINT('Ctrl Pts',(-13.671759167446,36.7943300130207,23.2948952948473));
#46589=CARTESIAN_POINT('Ctrl Pts',(-13.6163175769508,36.8998610956163,23.2890717011758));
#46590=CARTESIAN_POINT('Ctrl Pts',(-13.5609459342572,37.005259035076,23.2832554548328));
#46591=CARTESIAN_POINT('Ctrl Pts',(-13.5008895787069,37.1083734587724,23.2774392084898));
#46592=CARTESIAN_POINT('Ctrl Pts',(-13.4363636137901,37.2087621225066,23.2716229621468));
#46593=CARTESIAN_POINT('Ctrl Pts',(-13.3719022397201,37.3090502966344,23.2658125378984));
#46594=CARTESIAN_POINT('Ctrl Pts',(-13.3029803764777,37.4066177972895,23.2600021136501));
#46595=CARTESIAN_POINT('Ctrl Pts',(-13.2298590274942,37.5010469132974,23.2541916894018));
#46596=CARTESIAN_POINT('Ctrl Pts',(-13.1539698842106,37.5990503666593,23.2481613285776));
#46597=CARTESIAN_POINT('Ctrl Pts',(-13.0735572636367,37.6936727555006,23.2421309677534));
#46598=CARTESIAN_POINT('Ctrl Pts',(-12.9889626109015,37.784479755831,23.2361006069293));
#46599=CARTESIAN_POINT('Ctrl Pts',(-12.9075449999921,37.8718764030386,23.230296722696));
#46600=CARTESIAN_POINT('Ctrl Pts',(-12.8222541168128,37.9557387498776,23.2244928384628));
#46601=CARTESIAN_POINT('Ctrl Pts',(-12.7334349445222,38.0357138211737,23.2186889542296));
#46602=CARTESIAN_POINT('Ctrl Pts',(-12.6446288917731,38.1156770792965,23.2128859272921));
#46603=CARTESIAN_POINT('Ctrl Pts',(-12.5522958897155,38.1917539306026,23.2070829003546));
#46604=CARTESIAN_POINT('Ctrl Pts',(-12.4568163427329,38.2636296447484,23.2012798734172));
#46605=CARTESIAN_POINT('Ctrl Pts',(-12.3613283659046,38.3355117047682,23.1954763341331));
#46606=CARTESIAN_POINT('Ctrl Pts',(-12.2626936180526,38.4031916445604,23.1896727948491));
#46607=CARTESIAN_POINT('Ctrl Pts',(-12.1613234809667,38.466396660889,23.183869255565));
#46608=CARTESIAN_POINT('Ctrl Pts',(-12.0599204707275,38.5296221738672,23.1780638342609));
#46609=CARTESIAN_POINT('Ctrl Pts',(-11.9557806534257,38.5883696614061,23.1722584129567));
#46610=CARTESIAN_POINT('Ctrl Pts',(-11.8493415552261,38.6424114007226,23.1664529916525));
#46611=CARTESIAN_POINT('Ctrl Pts',(-11.7427845855772,38.6965129862633,23.1606411413816));
#46612=CARTESIAN_POINT('Ctrl Pts',(-11.6339236168275,38.7458982366489,23.1548292911107));
#46613=CARTESIAN_POINT('Ctrl Pts',(-11.5232179180482,38.790386810622,23.1490174408398));
#46614=CARTESIAN_POINT('Ctrl Pts',(-11.4124395071716,38.8349046049292,23.1432017733144));
#46615=CARTESIAN_POINT('Ctrl Pts',(-11.299814337594,38.8745191825742,23.1373861057891));
#46616=CARTESIAN_POINT('Ctrl Pts',(-11.1858170787976,38.9091000058366,23.1315704382637));
#46617=CARTESIAN_POINT('Ctrl Pts',(-11.0716565312375,38.9437303623943,23.1257464404226));
#46618=CARTESIAN_POINT('Ctrl Pts',(-10.95612036586,38.9733124722587,23.1199224425815));
#46619=CARTESIAN_POINT('Ctrl Pts',(-10.8396938113804,38.9977667894875,23.1140984447403));
#46620=CARTESIAN_POINT('Ctrl Pts',(-10.8088052118554,39.0042546531447,23.1125533063675));
#46621=CARTESIAN_POINT('Ctrl Pts',(-10.7778539682479,39.0103818700821,23.1110081679946));
#46622=CARTESIAN_POINT('Ctrl Pts',(-10.7468491860047,39.0161475686738,23.1094630296217));
#46623=CARTESIAN_POINT('Ctrl Pts',(-10.6299803966617,39.0378806745165,23.1036388167764));
#46624=CARTESIAN_POINT('Ctrl Pts',(-10.5119736989003,39.0545433208812,23.0978146039311));
#46625=CARTESIAN_POINT('Ctrl Pts',(-10.3933067302697,39.0660219891098,23.0919903910859));
#46626=CARTESIAN_POINT('Ctrl Pts',(-10.27479242528,39.0774858901685,23.086173671021));
#46627=CARTESIAN_POINT('Ctrl Pts',(-10.1556199421426,39.0837790401271,23.0803569509561));
#46628=CARTESIAN_POINT('Ctrl Pts',(-10.0362771935645,39.0848389154564,23.0745402308913));
#46629=CARTESIAN_POINT('Ctrl Pts',(-9.91707555091006,39.085897537633,23.0687303882753));
#46630=CARTESIAN_POINT('Ctrl Pts',(-9.79770444963335,39.0817352006476,23.0629205456594));
#46631=CARTESIAN_POINT('Ctrl Pts',(-9.67865617647097,39.0723412365714,23.0571107030434));
#46632=CARTESIAN_POINT('Ctrl Pts',(-9.55968699036968,39.0629535131653,23.0513047200666));
#46633=CARTESIAN_POINT('Ctrl Pts',(-9.4410406114256,39.0483411063072,23.0454987370898));
#46634=CARTESIAN_POINT('Ctrl Pts',(-9.32320835254928,39.0285454032369,23.039692754113));
#46635=CARTESIAN_POINT('Ctrl Pts',(-9.20542656317161,39.0087581789925,23.0338892579345));
#46636=CARTESIAN_POINT('Ctrl Pts',(-9.08845860213525,38.9837921425446,23.0280857617559));
#46637=CARTESIAN_POINT('Ctrl Pts',(-8.97278905484733,38.953740339749,23.0222822655773));
#46638=CARTESIAN_POINT('Ctrl Pts',(-8.85714175273698,38.9236943164149,23.0164798855076));
#46639=CARTESIAN_POINT('Ctrl Pts',(-8.74279276211062,38.8885645766798,23.0106775054378));
#46640=CARTESIAN_POINT('Ctrl Pts',(-8.63021426868508,38.8484947772195,23.0048751253681));
#46641=CARTESIAN_POINT('Ctrl Pts',(-8.51759076243004,38.8084089564483,22.9990704253033));
#46642=CARTESIAN_POINT('Ctrl Pts',(-8.40673955369542,38.7633792637949,22.9932657252385));
#46643=CARTESIAN_POINT('Ctrl Pts',(-8.29811539405272,38.7135984958043,22.9874610251737));
#46644=CARTESIAN_POINT('Ctrl Pts',(-8.18946829494124,38.6638072150108,22.9816550992607));
#46645=CARTESIAN_POINT('Ctrl Pts',(-8.08304954841149,38.6092630402489,22.9758491733477));
#46646=CARTESIAN_POINT('Ctrl Pts',(-7.9792905795812,38.5502054078927,22.9700432474347));
#46647=CARTESIAN_POINT('Ctrl Pts',(-7.87543494651362,38.4910927560905,22.9642319125878));
#46648=CARTESIAN_POINT('Ctrl Pts',(-7.77424438905138,38.4274584610306,22.9584205777409));
#46649=CARTESIAN_POINT('Ctrl Pts',(-7.67612259923038,38.3595861093582,22.952609242894));
#46650=CARTESIAN_POINT('Ctrl Pts',(-7.62068926029576,38.3212420159472,22.9493261628073));
#46651=CARTESIAN_POINT('Ctrl Pts',(-7.56623480188463,38.2815460655043,22.9460430827206));
#46652=CARTESIAN_POINT('Ctrl Pts',(-7.51282733495087,38.2405550657615,22.942760002634));
#46653=CARTESIAN_POINT('',(-14.0849999165586,34.9991743389247,23.4896150285502));
#46654=CARTESIAN_POINT('Ctrl Pts',(-14.0849999165586,34.9991743389247,23.4896150285502));
#46655=CARTESIAN_POINT('Ctrl Pts',(-14.0850238118884,35.1173976913746,23.4838237303793));
#46656=CARTESIAN_POINT('Ctrl Pts',(-14.0799112176567,35.2358210967393,23.4780324322084));
#46657=CARTESIAN_POINT('Ctrl Pts',(-14.0696361080072,35.3539589642939,23.4722411340375));
#46658=CARTESIAN_POINT('Ctrl Pts',(-14.0593738341097,35.4719492530461,23.4664570704042));
#46659=CARTESIAN_POINT('Ctrl Pts',(-14.0439619044241,35.5896543051682,23.4606730067709));
#46660=CARTESIAN_POINT('Ctrl Pts',(-14.0234262888692,35.706587502038,23.4548889431377));
#46661=CARTESIAN_POINT('Ctrl Pts',(-14.0029108151614,35.8234060078938,23.4491105526591));
#46662=CARTESIAN_POINT('Ctrl Pts',(-13.9772817220657,35.9394537594224,23.4433321621806));
#46663=CARTESIAN_POINT('Ctrl Pts',(-13.9466168096246,36.054248907037,23.4375537717021));
#46664=CARTESIAN_POINT('Ctrl Pts',(-13.9159728587046,36.1689655844809,23.4317793311404));
#46665=CARTESIAN_POINT('Ctrl Pts',(-13.8803000416626,36.2824309629973,23.4260048905788));
#46666=CARTESIAN_POINT('Ctrl Pts',(-13.8397271776588,36.3941736624783,23.4202304500171));
#46667=CARTESIAN_POINT('Ctrl Pts',(-13.799168923569,36.5058761244445,23.4144580887782));
#46668=CARTESIAN_POINT('Ctrl Pts',(-13.753714270898,36.6158567524158,23.4086857275393));
#46669=CARTESIAN_POINT('Ctrl Pts',(-13.7035416294543,36.7236601750053,23.4029133663004));
#46670=CARTESIAN_POINT('Ctrl Pts',(-13.653374866864,36.8314509659989,23.3971416814234));
#46671=CARTESIAN_POINT('Ctrl Pts',(-13.598491389195,36.937064684168,23.3913699965464));
#46672=CARTESIAN_POINT('Ctrl Pts',(-13.5391171100778,37.0400674207375,23.3855983116695));
#46673=CARTESIAN_POINT('Ctrl Pts',(-13.4797353646703,37.1430831098572,23.3798259010056));
#46674=CARTESIAN_POINT('Ctrl Pts',(-13.4158619018823,37.243486806659,23.3740534903417));
#46675=CARTESIAN_POINT('Ctrl Pts',(-13.3477674386442,37.3408712430959,23.3682810796779));
#46676=CARTESIAN_POINT('Ctrl Pts',(-13.2796050587144,37.4383528097317,23.3625029116731));
#46677=CARTESIAN_POINT('Ctrl Pts',(-13.2072135061452,37.5328087612768,23.3567247436684));
#46678=CARTESIAN_POINT('Ctrl Pts',(-13.130905624707,37.6238626048591,23.3509465756636));
#46679=CARTESIAN_POINT('Ctrl Pts',(-13.0545602420002,37.7149611965668,23.3451655679964));
#46680=CARTESIAN_POINT('Ctrl Pts',(-12.9742949756232,37.8026540447818,23.3393845603291));
#46681=CARTESIAN_POINT('Ctrl Pts',(-12.8904603476387,37.8866007653862,23.3336035526619));
#46682=CARTESIAN_POINT('Ctrl Pts',(-12.8064891229373,37.9706842653466,23.327813125657));
#46683=CARTESIAN_POINT('Ctrl Pts',(-12.7189372206986,38.0510091615247,23.3220226986521));
#46684=CARTESIAN_POINT('Ctrl Pts',(-12.6281895523726,38.1272743206824,23.3162322716471));
#46685=CARTESIAN_POINT('Ctrl Pts',(-12.5397280240124,38.201618187188,23.3105877186557));
#46686=CARTESIAN_POINT('Ctrl Pts',(-12.4482301579863,38.2721042776266,23.3049431656643));
#46687=CARTESIAN_POINT('Ctrl Pts',(-12.3540776653063,38.3384941733821,23.2992986126729));
#46688=CARTESIAN_POINT('Ctrl Pts',(-12.2569387313004,38.4069899032228,23.2934750190015));
#46689=CARTESIAN_POINT('Ctrl Pts',(-12.1566511796999,38.4713529449552,23.28765142533));
#46690=CARTESIAN_POINT('Ctrl Pts',(-12.0536016281218,38.5312809790465,23.2818278316586));
#46691=CARTESIAN_POINT('Ctrl Pts',(-11.9506820888599,38.591133405021,23.2760115853155));
#46692=CARTESIAN_POINT('Ctrl Pts',(-11.8450078304294,38.6465617490465,23.2701953389725));
#46693=CARTESIAN_POINT('Ctrl Pts',(-11.7369961000549,38.6973057147596,23.2643790926295));
#46694=CARTESIAN_POINT('Ctrl Pts',(-11.6290924900184,38.7479988854831,23.2585686683812));
#46695=CARTESIAN_POINT('Ctrl Pts',(-11.5188564302833,38.7940168336229,23.2527582441328));
#46696=CARTESIAN_POINT('Ctrl Pts',(-11.4067310105654,38.8351444384682,23.2469478198845));
#46697=CARTESIAN_POINT('Ctrl Pts',(-11.290361411796,38.8778288082234,23.2409174590603));
#46698=CARTESIAN_POINT('Ctrl Pts',(-11.1719569820487,38.915245075191,23.2348870982362));
#46699=CARTESIAN_POINT('Ctrl Pts',(-11.0520377807438,38.9472067982166,23.228856737412));
#46700=CARTESIAN_POINT('Ctrl Pts',(-10.9366222721185,38.9779681648652,23.2230528531788));
#46701=CARTESIAN_POINT('Ctrl Pts',(-10.8198041478439,39.0036771868587,23.2172489689455));
#46702=CARTESIAN_POINT('Ctrl Pts',(-10.702063230289,39.0242182123583,23.2114450847123));
#46703=CARTESIAN_POINT('Ctrl Pts',(-10.5843397043267,39.0447562037287,23.2056420577748));
#46704=CARTESIAN_POINT('Ctrl Pts',(-10.465694058307,39.0601276465443,23.1998390308373));
#46705=CARTESIAN_POINT('Ctrl Pts',(-10.3466157934312,39.070268110548,23.1940360038999));
#46706=CARTESIAN_POINT('Ctrl Pts',(-10.2275270151899,39.0804094698486,23.1882324646158));
#46707=CARTESIAN_POINT('Ctrl Pts',(-10.1080059490346,39.0853188974369,23.1824289253317));
#46708=CARTESIAN_POINT('Ctrl Pts',(-9.98854605372726,39.0849839420878,23.1766253860477));
#46709=CARTESIAN_POINT('Ctrl Pts',(-9.86904741896912,39.0846488781165,23.1708199647435));
#46710=CARTESIAN_POINT('Ctrl Pts',(-9.74961040263544,39.0790660500592,23.1650145434394));
#46711=CARTESIAN_POINT('Ctrl Pts',(-9.63072665119051,39.0682750882726,23.1592091221352));
#46712=CARTESIAN_POINT('Ctrl Pts',(-9.51171124699446,39.0574721764945,23.1533972718643));
#46713=CARTESIAN_POINT('Ctrl Pts',(-9.39325073757442,39.0414496554457,23.1475854215933));
#46714=CARTESIAN_POINT('Ctrl Pts',(-9.2758300057599,39.0202988470314,23.1417735713224));
#46715=CARTESIAN_POINT('Ctrl Pts',(-9.15833215137831,38.9991341466526,23.135957903797));
#46716=CARTESIAN_POINT('Ctrl Pts',(-9.04187583206838,38.9728345406241,23.1301422362717));
#46717=CARTESIAN_POINT('Ctrl Pts',(-8.92693250720861,38.9415417232238,23.1243265687463));
#46718=CARTESIAN_POINT('Ctrl Pts',(-8.81182453844765,38.9102040822417,23.1185025709051));
#46719=CARTESIAN_POINT('Ctrl Pts',(-8.69823427728596,38.8738590784108,23.112678573064));
#46720=CARTESIAN_POINT('Ctrl Pts',(-8.58661502727579,38.8326972120006,23.1068545752229));
#46721=CARTESIAN_POINT('Ctrl Pts',(-8.55700183183216,38.8217767444763,23.1053094368501));
#46722=CARTESIAN_POINT('Ctrl Pts',(-8.52752724292257,38.8105174870963,23.1037642984773));
#46723=CARTESIAN_POINT('Ctrl Pts',(-8.49819943683015,38.7989235407498,23.1022191601045));
#46724=CARTESIAN_POINT('Ctrl Pts',(-8.38767210568014,38.7552295820833,23.0963960167005));
#46725=CARTESIAN_POINT('Ctrl Pts',(-8.27887501036345,38.7066375795626,23.0905728732964));
#46726=CARTESIAN_POINT('Ctrl Pts',(-8.1722728246637,38.6533051299525,23.0847497298924));
#46727=CARTESIAN_POINT('Ctrl Pts',(-8.06578901655625,38.600031903959,23.0789330528632));
#46728=CARTESIAN_POINT('Ctrl Pts',(-7.96149563552509,38.542028874668,23.0731163758341));
#46729=CARTESIAN_POINT('Ctrl Pts',(-7.85983920561452,38.4795023745035,23.0672996988049));
#46730=CARTESIAN_POINT('Ctrl Pts',(-7.75829239064119,38.4170432959314,23.0614892938305));
#46731=CARTESIAN_POINT('Ctrl Pts',(-7.65937721402651,38.3500706661944,23.055678888856));
#46732=CARTESIAN_POINT('Ctrl Pts',(-7.56351647808874,38.2788371486634,23.0498684838815));
#46733=CARTESIAN_POINT('Ctrl Pts',(-7.54652342283912,38.266209714843,23.048838484145));
#46734=CARTESIAN_POINT('Ctrl Pts',(-7.52962628560435,38.2534485022311,23.0478084844086));
#46735=CARTESIAN_POINT('Ctrl Pts',(-7.51282733495086,38.2405550657615,23.0467784846721));
#46736=CARTESIAN_POINT('Ctrl Pts',(-7.51282733495087,38.2405550657615,24.2969436900965));
#46737=CARTESIAN_POINT('Ctrl Pts',(-7.44658649974838,38.1897142711191,24.2928610852361));
#46738=CARTESIAN_POINT('Ctrl Pts',(-7.38197057038218,38.1368917967566,24.2887784803756));
#46739=CARTESIAN_POINT('Ctrl Pts',(-7.31909951636829,38.0822066116442,24.2846958755152));
#46740=CARTESIAN_POINT('Ctrl Pts',(-7.22941768704517,38.0042014387603,24.2788722818435));
#46741=CARTESIAN_POINT('Ctrl Pts',(-7.14299859653684,37.9221530692216,24.2730486881718));
#46742=CARTESIAN_POINT('Ctrl Pts',(-7.0602280293539,37.8363648849546,24.2672250945001));
#46743=CARTESIAN_POINT('Ctrl Pts',(-6.97756188953597,37.7506849352248,24.2614088481569));
#46744=CARTESIAN_POINT('Ctrl Pts',(-6.8985353985021,37.6612748466875,24.2555926018137));
#46745=CARTESIAN_POINT('Ctrl Pts',(-6.82350083292964,37.5684777673948,24.2497763554704));
#46746=CARTESIAN_POINT('Ctrl Pts',(-6.74854137737129,37.4757735784904,24.2439659312219));
#46747=CARTESIAN_POINT('Ctrl Pts',(-6.67756615311727,37.3796894593027,24.2381555069733));
#46748=CARTESIAN_POINT('Ctrl Pts',(-6.61088972602059,37.2806044266394,24.2323450827247));
#46749=CARTESIAN_POINT('Ctrl Pts',(-6.54168945825131,37.177768820552,24.2263147219006));
#46750=CARTESIAN_POINT('Ctrl Pts',(-6.47712016569852,37.0717009532391,24.2202843610766));
#46751=CARTESIAN_POINT('Ctrl Pts',(-6.41748691440689,36.9628614295345,24.2142540002525));
#46752=CARTESIAN_POINT('Ctrl Pts',(-6.36009325305589,36.8581094894707,24.208450116019));
#46753=CARTESIAN_POINT('Ctrl Pts',(-6.30727177640937,36.7507907139614,24.2026462317855));
#46754=CARTESIAN_POINT('Ctrl Pts',(-6.25924920886273,36.6413435102397,24.1968423475521));
#46755=CARTESIAN_POINT('Ctrl Pts',(-6.21123373476286,36.5319124730403,24.1910393206144));
#46756=CARTESIAN_POINT('Ctrl Pts',(-6.16801592410824,36.420354006679,24.1852362936767));
#46757=CARTESIAN_POINT('Ctrl Pts',(-6.12977506487738,36.3071281312691,24.179433266739));
#46758=CARTESIAN_POINT('Ctrl Pts',(-6.09153082937854,36.1938922591985,24.1736297274547));
#46759=CARTESIAN_POINT('Ctrl Pts',(-6.05826454962927,36.0789890722679,24.1678261881704));
#46760=CARTESIAN_POINT('Ctrl Pts',(-6.03010597741497,35.9628948278206,24.1620226488861));
#46761=CARTESIAN_POINT('Ctrl Pts',(-6.00193827370406,35.8467629353636,24.1562172275817));
#46762=CARTESIAN_POINT('Ctrl Pts',(-5.97888166787568,35.7294396138604,24.1504118062773));
#46763=CARTESIAN_POINT('Ctrl Pts',(-5.96101490017239,35.6114117788942,24.1446063849729));
#46764=CARTESIAN_POINT('Ctrl Pts',(-5.9431283466776,35.4932532390254,24.1387945347017));
#46765=CARTESIAN_POINT('Ctrl Pts',(-5.93044316449469,35.3743890323574,24.1329826844306));
#46766=CARTESIAN_POINT('Ctrl Pts',(-5.92298628051653,35.2553118311861,24.1271708341594));
#46767=CARTESIAN_POINT('Ctrl Pts',(-5.91552449881694,35.1361564194698,24.1213551666338));
#46768=CARTESIAN_POINT('Ctrl Pts',(-5.91329786176667,35.0167881419714,24.1155394991082));
#46769=CARTESIAN_POINT('Ctrl Pts',(-5.91628117607831,34.8976986454261,24.1097238315826));
#46770=CARTESIAN_POINT('Ctrl Pts',(-5.91926876366556,34.7784385660364,24.1038998337412));
#46771=CARTESIAN_POINT('Ctrl Pts',(-5.92748116972554,34.6594584705499,24.0980758358998));
#46772=CARTESIAN_POINT('Ctrl Pts',(-5.94084147361198,34.5412440107732,24.0922518380585));
#46773=CARTESIAN_POINT('Ctrl Pts',(-5.9443860350524,34.5098810702753,24.0907066996879));
#46774=CARTESIAN_POINT('Ctrl Pts',(-5.94829266398167,34.4785719579324,24.0891615613173));
#46775=CARTESIAN_POINT('Ctrl Pts',(-5.95255932733317,34.4473255920143,24.0876164229467));
#46776=CARTESIAN_POINT('Ctrl Pts',(-5.96864029080211,34.3295587031203,24.0817928292753));
#46777=CARTESIAN_POINT('Ctrl Pts',(-5.9898913818671,34.2123043416862,24.0759692356039));
#46778=CARTESIAN_POINT('Ctrl Pts',(-6.01627033365602,34.0960514696672,24.0701456419325));
#46779=CARTESIAN_POINT('Ctrl Pts',(-6.042616004479,33.9799452679141,24.0643293955896));
#46780=CARTESIAN_POINT('Ctrl Pts',(-6.07407657866468,33.864838437153,24.0585131492466));
#46781=CARTESIAN_POINT('Ctrl Pts',(-6.11055816232705,33.7512137126957,24.0526969029037));
#46782=CARTESIAN_POINT('Ctrl Pts',(-6.14700322772288,33.6377027272145,24.0468864786554));
#46783=CARTESIAN_POINT('Ctrl Pts',(-6.18845917976376,33.5256712831598,24.0410760544071));
#46784=CARTESIAN_POINT('Ctrl Pts',(-6.23478145327104,33.4155902375432,24.0352656301588));
#46785=CARTESIAN_POINT('Ctrl Pts',(-6.28285712064224,33.3013423966617,24.0292352693346));
#46786=CARTESIAN_POINT('Ctrl Pts',(-6.33617468997625,33.1891959619523,24.0232049085104));
#46787=CARTESIAN_POINT('Ctrl Pts',(-6.39451615077475,33.0796585686457,24.0171745476863));
#46788=CARTESIAN_POINT('Ctrl Pts',(-6.45066653618959,32.9742349682195,24.0113706634531));
#46789=CARTESIAN_POINT('Ctrl Pts',(-6.51147005382735,32.8712283654531,24.0055667792199));
#46790=CARTESIAN_POINT('Ctrl Pts',(-6.57668431458382,32.7710687049656,23.9997628949867));
#46791=CARTESIAN_POINT('Ctrl Pts',(-6.64188894249656,32.6709238391312,23.9939598680493));
#46792=CARTESIAN_POINT('Ctrl Pts',(-6.7115027951286,32.5736254213892,23.9881568411119));
#46793=CARTESIAN_POINT('Ctrl Pts',(-6.78523940407018,32.4795755693025,23.9823538141745));
#46794=CARTESIAN_POINT('Ctrl Pts',(-6.85898252318327,32.3855174135973,23.9765502748905));
#46795=CARTESIAN_POINT('Ctrl Pts',(-6.93684887036415,32.2947087151672,23.9707467356065));
#46796=CARTESIAN_POINT('Ctrl Pts',(-7.01851124291598,32.2075190615903,23.9649431963225));
#46797=CARTESIAN_POINT('Ctrl Pts',(-7.1002000976229,32.1203011334255,23.9591377750184));
#46798=CARTESIAN_POINT('Ctrl Pts',(-7.18568714690232,32.0367048820438,23.9533323537143));
#46799=CARTESIAN_POINT('Ctrl Pts',(-7.2746083111431,31.9570630728998,23.9475269324102));
#46800=CARTESIAN_POINT('Ctrl Pts',(-7.36362794734278,31.8773330678238,23.9417150821393));
#46801=CARTESIAN_POINT('Ctrl Pts',(-7.45608898519393,31.8015665187932,23.9359032318685));
#46802=CARTESIAN_POINT('Ctrl Pts',(-7.55159412814597,31.7300560116921,23.9300913815976));
#46803=CARTESIAN_POINT('Ctrl Pts',(-7.64716199938857,31.6584985361061,23.9242757140723));
#46804=CARTESIAN_POINT('Ctrl Pts',(-7.74577762104491,31.5912028991786,23.918460046547));
#46805=CARTESIAN_POINT('Ctrl Pts',(-7.84701598392935,31.5284175328038,23.9126443790217));
#46806=CARTESIAN_POINT('Ctrl Pts',(-7.94839935983682,31.4655422331712,23.9068203811806));
#46807=CARTESIAN_POINT('Ctrl Pts',(-8.05241262046835,31.4071902979273,23.9009963833395));
#46808=CARTESIAN_POINT('Ctrl Pts',(-8.15860741556952,31.3535636094943,23.8951723854985));
#46809=CARTESIAN_POINT('Ctrl Pts',(-8.18678147356946,31.3393361567381,23.8936272471251));
#46810=CARTESIAN_POINT('Ctrl Pts',(-8.21510898346396,31.3254410334175,23.8920821087517));
#46811=CARTESIAN_POINT('Ctrl Pts',(-8.2435813718164,31.311881427805,23.8905369703783));
#46812=CARTESIAN_POINT('Ctrl Pts',(-8.35089319804208,31.2607755626009,23.8847133767068));
#46813=CARTESIAN_POINT('Ctrl Pts',(-8.46061043672434,31.2142747918228,23.8788897830354));
#46814=CARTESIAN_POINT('Ctrl Pts',(-8.57230096503299,31.1726117958124,23.8730661893639));
#46815=CARTESIAN_POINT('Ctrl Pts',(-8.68385057914995,31.13100136386,23.8672499430209));
#46816=CARTESIAN_POINT('Ctrl Pts',(-8.79736815192766,31.09421670827,23.8614336966779));
#46817=CARTESIAN_POINT('Ctrl Pts',(-8.91239846827199,31.0624439168206,23.8556174503349));
#46818=CARTESIAN_POINT('Ctrl Pts',(-9.02731363863492,31.0307029301108,23.8498070260866));
#46819=CARTESIAN_POINT('Ctrl Pts',(-9.14373814878634,31.0039639351248,23.8439966018382));
#46820=CARTESIAN_POINT('Ctrl Pts',(-9.26119894214244,30.9823641283824,23.8381861775899));
#46821=CARTESIAN_POINT('Ctrl Pts',(-9.38310586947809,30.9599467242787,23.8321558167657));
#46822=CARTESIAN_POINT('Ctrl Pts',(-9.50612866105522,30.943065410048,23.8261254559415));
#46823=CARTESIAN_POINT('Ctrl Pts',(-9.62972324000001,30.9318161151438,23.8200950951174));
#46824=CARTESIAN_POINT('Ctrl Pts',(-9.74867609356314,30.9209892994302,23.8142912108841));
#46825=CARTESIAN_POINT('Ctrl Pts',(-9.86815811762731,30.9153791393267,23.8084873266509));
#46826=CARTESIAN_POINT('Ctrl Pts',(-9.98767685004044,30.9150185875606,23.8026834424177));
#46827=CARTESIAN_POINT('Ctrl Pts',(-10.1071779282586,30.9146580890519,23.7968804154802));
#46828=CARTESIAN_POINT('Ctrl Pts',(-10.2267152958179,30.9195456580402,23.7910773885428));
#46829=CARTESIAN_POINT('Ctrl Pts',(-10.3457956016436,30.929662126815,23.7852743616053));
#46830=CARTESIAN_POINT('Ctrl Pts',(-10.4648864210149,30.9397794887682,23.7794708223212));
#46831=CARTESIAN_POINT('Ctrl Pts',(-10.5835196915282,30.9551266338264,23.7736672830372));
#46832=CARTESIAN_POINT('Ctrl Pts',(-10.7012069401966,30.9756324935438,23.7678637437531));
#46833=CARTESIAN_POINT('Ctrl Pts',(-10.8189323534675,30.9961450030725,23.762058322449));
#46834=CARTESIAN_POINT('Ctrl Pts',(-10.9357107327005,31.0218194842462,23.7562529011448));
#46835=CARTESIAN_POINT('Ctrl Pts',(-11.0510641872895,31.0525338412853,23.7504474798406));
#46836=CARTESIAN_POINT('Ctrl Pts',(-11.1665453851523,31.0832822116319,23.7446356295697));
#46837=CARTESIAN_POINT('Ctrl Pts',(-11.2805981137804,31.1190814932624,23.7388237792988));
#46838=CARTESIAN_POINT('Ctrl Pts',(-11.3927598792845,31.1597597837303,23.7330119290279));
#46839=CARTESIAN_POINT('Ctrl Pts',(-11.5049953132384,31.2004647919177,23.7271962615025));
#46840=CARTESIAN_POINT('Ctrl Pts',(-11.6153369340792,31.2460550353328,23.7213805939771));
#46841=CARTESIAN_POINT('Ctrl Pts',(-11.7233439859837,31.2963112298718,23.7155649264518));
#46842=CARTESIAN_POINT('Ctrl Pts',(-11.8315057463272,31.3466394109827,23.7097409286107));
#46843=CARTESIAN_POINT('Ctrl Pts',(-11.9373259022321,31.4016466953953,23.7039169307695));
#46844=CARTESIAN_POINT('Ctrl Pts',(-12.0403898357864,31.4610687604844,23.6980929329284));
#46845=CARTESIAN_POINT('Ctrl Pts',(-12.0677332591423,31.4768337582521,23.6965477945556));
#46846=CARTESIAN_POINT('Ctrl Pts',(-12.094882848487,31.4929092696485,23.6950026561827));
#46847=CARTESIAN_POINT('Ctrl Pts',(-12.1218312375957,31.5092898717935,23.6934575178098));
#46848=CARTESIAN_POINT('Ctrl Pts',(-12.2233991431153,31.5710280129606,23.6876339241383));
#46849=CARTESIAN_POINT('Ctrl Pts',(-12.3224340400303,31.6373023167315,23.6818103304668));
#46850=CARTESIAN_POINT('Ctrl Pts',(-12.4185044472204,31.707878914928,23.6759867367953));
#46851=CARTESIAN_POINT('Ctrl Pts',(-12.5144536473217,31.7783664702627,23.6701704904523));
#46852=CARTESIAN_POINT('Ctrl Pts',(-12.607445470577,31.8531452842684,23.6643542441092));
#46853=CARTESIAN_POINT('Ctrl Pts',(-12.6970747462039,31.9319366347174,23.6585379977661));
#46854=CARTESIAN_POINT('Ctrl Pts',(-12.7866143024314,32.0106491145899,23.6527275735178));
#46855=CARTESIAN_POINT('Ctrl Pts',(-12.8727977022077,32.0933658723848,23.6469171492694));
#46856=CARTESIAN_POINT('Ctrl Pts',(-12.9552508859335,32.17976646336,23.641106725021));
#46857=CARTESIAN_POINT('Ctrl Pts',(-13.0408250932051,32.2694374954099,23.6350763641969));
#46858=CARTESIAN_POINT('Ctrl Pts',(-13.1223807507816,32.3630764869399,23.6290460033727));
#46859=CARTESIAN_POINT('Ctrl Pts',(-13.1995393829108,32.4602809727841,23.6230156425486));
#46860=CARTESIAN_POINT('Ctrl Pts',(-13.2738002408486,32.5538348411587,23.6172117583153));
#46861=CARTESIAN_POINT('Ctrl Pts',(-13.3439881105525,32.6506908730695,23.611407874082));
#46862=CARTESIAN_POINT('Ctrl Pts',(-13.4098054814972,32.7504552508671,23.6056039898487));
#46863=CARTESIAN_POINT('Ctrl Pts',(-13.4756131305124,32.8502048923992,23.5998009629112));
#46864=CARTESIAN_POINT('Ctrl Pts',(-13.5370513397982,32.9528616847393,23.5939979359737));
#46865=CARTESIAN_POINT('Ctrl Pts',(-13.5938657035848,33.0580024962433,23.5881949090362));
#46866=CARTESIAN_POINT('Ctrl Pts',(-13.6506850834856,33.1631525905815,23.5823913697521));
#46867=CARTESIAN_POINT('Ctrl Pts',(-13.7028796120812,33.2707867808696,23.576587830468));
#46868=CARTESIAN_POINT('Ctrl Pts',(-13.7502409658695,33.380457565263,23.5707842911839));
#46869=CARTESIAN_POINT('Ctrl Pts',(-13.7976176783924,33.4901639146125,23.5649788698797));
#46870=CARTESIAN_POINT('Ctrl Pts',(-13.8401579372118,33.601907796859,23.5591734485755));
#46871=CARTESIAN_POINT('Ctrl Pts',(-13.8777018974906,33.7152225896296,23.5533680272713));
#46872=CARTESIAN_POINT('Ctrl Pts',(-13.9152874342304,33.828662868045,23.5475561770004));
#46873=CARTESIAN_POINT('Ctrl Pts',(-13.9478654997087,33.9436771416056,23.5417443267294));
#46874=CARTESIAN_POINT('Ctrl Pts',(-13.9753263458668,34.0597843631074,23.5359324764584));
#46875=CARTESIAN_POINT('Ctrl Pts',(-14.0028052284561,34.1759678444556,23.530116808933));
#46876=CARTESIAN_POINT('Ctrl Pts',(-14.0251601218919,34.2932453031767,23.5243011414076));
#46877=CARTESIAN_POINT('Ctrl Pts',(-14.0423328227828,34.4111279002593,23.5184854738822));
#46878=CARTESIAN_POINT('Ctrl Pts',(-14.0595301217133,34.529179351433,23.512661476041));
#46879=CARTESIAN_POINT('Ctrl Pts',(-14.0715303713907,34.6478372662219,23.5068374781999));
#46880=CARTESIAN_POINT('Ctrl Pts',(-14.0783273651943,34.7666099781324,23.5010134803587));
#46881=CARTESIAN_POINT('Ctrl Pts',(-14.0801306446991,34.7981210260031,23.4994683419863));
#46882=CARTESIAN_POINT('Ctrl Pts',(-14.0815679668199,34.8296401689612,23.4979232036138));
#46883=CARTESIAN_POINT('Ctrl Pts',(-14.0826398292009,34.8611582734834,23.4963780652414));
#46884=CARTESIAN_POINT('Ctrl Pts',(-14.0842036685506,34.9071429567314,23.4941237196927));
#46885=CARTESIAN_POINT('Ctrl Pts',(-14.0849906149495,34.953154209098,23.4918693741441));
#46886=CARTESIAN_POINT('Ctrl Pts',(-14.0849999165584,34.9991743380006,23.4896150285955));
#46887=CARTESIAN_POINT('Origin',(-10.,35.,32.7603849714045));
#46888=CARTESIAN_POINT('',(-7.51282733495086,38.2405550657615,25.5469376052728));
#46889=CARTESIAN_POINT('',(-7.51282733495087,38.2405550657615,25.4425445275748));
#46890=CARTESIAN_POINT('',(-7.51282733495086,38.2405550657615,32.7603849714045));
#46891=CARTESIAN_POINT('',(-14.0849984277889,34.9964160131029,24.6353849714293));
#46892=CARTESIAN_POINT('Ctrl Pts',(-7.51282733495087,38.2405550657615,25.4425445275748));
#46893=CARTESIAN_POINT('Ctrl Pts',(-7.41827383907103,38.167983896451,25.4367331956948));
#46894=CARTESIAN_POINT('Ctrl Pts',(-7.32679683731213,38.0911923601983,25.4309218638148));
#46895=CARTESIAN_POINT('Ctrl Pts',(-7.23879170183744,38.0104740048966,25.4251105319348));
#46896=CARTESIAN_POINT('Ctrl Pts',(-7.15085573664087,37.9298190926094,25.4193037676456));
#46897=CARTESIAN_POINT('Ctrl Pts',(-7.06638650781902,37.8452437774452,25.4134970033563));
#46898=CARTESIAN_POINT('Ctrl Pts',(-6.98574662823781,37.7570820827136,25.4076902390671));
#46899=CARTESIAN_POINT('Ctrl Pts',(-6.90514174153435,37.668958644877,25.4018859945658));
#46900=CARTESIAN_POINT('Ctrl Pts',(-6.8283631753088,37.5772522224484,25.3960817500644));
#46901=CARTESIAN_POINT('Ctrl Pts',(-6.75573660684465,37.4823335867349,25.3902775055631));
#46902=CARTESIAN_POINT('Ctrl Pts',(-6.683124423063,37.3874337509518,25.3844744106716));
#46903=CARTESIAN_POINT('Ctrl Pts',(-6.61466284974465,37.2893232912073,25.37867131578));
#46904=CARTESIAN_POINT('Ctrl Pts',(-6.55063677423441,37.1884054324407,25.3728682208885));
#46905=CARTESIAN_POINT('Ctrl Pts',(-6.48660826976873,37.0874837451561,25.3670649058451));
#46906=CARTESIAN_POINT('Ctrl Pts',(-6.42701581633417,36.9837547919758,25.3612615908017));
#46907=CARTESIAN_POINT('Ctrl Pts',(-6.37210016940302,36.8776495464155,25.3554582757583));
#46908=CARTESIAN_POINT('Ctrl Pts',(-6.31716947910029,36.7715152348107,25.3496533709781));
#46909=CARTESIAN_POINT('Ctrl Pts',(-6.26691833075206,36.6630036988033,25.3438484661979));
#46910=CARTESIAN_POINT('Ctrl Pts',(-6.22154056228396,36.5525686063857,25.3380435614177));
#46911=CARTESIAN_POINT('Ctrl Pts',(-6.17611361638147,36.4420138316944,25.3322323656644));
#46912=CARTESIAN_POINT('Ctrl Pts',(-6.13557075027135,36.3295317166733,25.326421169911));
#46913=CARTESIAN_POINT('Ctrl Pts',(-6.10005692608878,36.2155941017675,25.3206099741577));
#46914=CARTESIAN_POINT('Ctrl Pts',(-6.06452138003439,36.1015867974288,25.3147952240124));
#46915=CARTESIAN_POINT('Ctrl Pts',(-6.03402110671144,35.9861226142386,25.3089804738671));
#46916=CARTESIAN_POINT('Ctrl Pts',(-6.00865023460705,35.8696850293627,25.3031657237219));
#46917=CARTESIAN_POINT('Ctrl Pts',(-5.98324156117036,35.7530739583009,25.2973423098893));
#46918=CARTESIAN_POINT('Ctrl Pts',(-5.96297761825259,35.635486991259,25.2915188960568));
#46919=CARTESIAN_POINT('Ctrl Pts',(-5.94790088227622,35.5174144761621,25.2856954822242));
#46920=CARTESIAN_POINT('Ctrl Pts',(-5.94068755835331,35.4609237808869,25.2829093241077));
#46921=CARTESIAN_POINT('Ctrl Pts',(-5.93466084598134,35.4043219717969,25.2801231659911));
#46922=CARTESIAN_POINT('Ctrl Pts',(-5.92982117855721,35.347662712235,25.2773370078746));
#46923=CARTESIAN_POINT('Ctrl Pts',(-5.91970536480494,35.2292342197704,25.2715134142015));
#46924=CARTESIAN_POINT('Ctrl Pts',(-5.91474633401455,35.1101728819247,25.2656898205283));
#46925=CARTESIAN_POINT('Ctrl Pts',(-5.91500999150824,34.9909650388779,25.2598662268552));
#46926=CARTESIAN_POINT('Ctrl Pts',(-5.91527331635883,34.8719075942315,25.2540499805105));
#46927=CARTESIAN_POINT('Ctrl Pts',(-5.92074622284017,34.7527044167591,25.2482337341658));
#46928=CARTESIAN_POINT('Ctrl Pts',(-5.93144287956206,34.6338470842206,25.2424174878211));
#46929=CARTESIAN_POINT('Ctrl Pts',(-5.9421288288716,34.5151087285273,25.236607063571));
#46930=CARTESIAN_POINT('Ctrl Pts',(-5.95802808957789,34.3967159334161,25.2307966393209));
#46931=CARTESIAN_POINT('Ctrl Pts',(-5.9791027876393,34.2791597905014,25.2249862150709));
#46932=CARTESIAN_POINT('Ctrl Pts',(-6.00097520660355,34.1571539044783,25.2189558542474));
#46933=CARTESIAN_POINT('Ctrl Pts',(-6.02842260533313,34.0360497083627,25.2129254934238));
#46934=CARTESIAN_POINT('Ctrl Pts',(-6.06134350857744,33.9163902720191,25.2068951326003));
#46935=CARTESIAN_POINT('Ctrl Pts',(-6.09302803242813,33.8012247725595,25.2010912483653));
#46936=CARTESIAN_POINT('Ctrl Pts',(-6.1297822303506,33.6873979000119,25.1952873641303));
#46937=CARTESIAN_POINT('Ctrl Pts',(-6.17146381683957,33.5753822638226,25.1894834798953));
#46938=CARTESIAN_POINT('Ctrl Pts',(-6.21313924651255,33.4633831735404,25.1836804529561));
#46939=CARTESIAN_POINT('Ctrl Pts',(-6.25974047496561,33.3531951701633,25.1778774260168));
#46940=CARTESIAN_POINT('Ctrl Pts',(-6.31107611101002,33.2452733713655,25.1720743990776));
#46941=CARTESIAN_POINT('Ctrl Pts',(-6.36241627945433,33.1373420442012,25.1662708597918));
#46942=CARTESIAN_POINT('Ctrl Pts',(-6.41849151116107,33.0316776881912,25.1604673205059));
#46943=CARTESIAN_POINT('Ctrl Pts',(-6.47906354243962,32.9287126076225,25.1546637812201));
#46944=CARTESIAN_POINT('Ctrl Pts',(-6.53965521652162,32.8257141366787,25.1488583599141));
#46945=CARTESIAN_POINT('Ctrl Pts',(-6.60474638338519,32.7254170338091,25.1430529386082));
#46946=CARTESIAN_POINT('Ctrl Pts',(-6.67405472993697,32.6282257568341,25.1372475173022));
#46947=CARTESIAN_POINT('Ctrl Pts',(-6.74343982906742,32.5309268495158,25.1314356670295));
#46948=CARTESIAN_POINT('Ctrl Pts',(-6.81705119265443,32.4367409661172,25.1256238167568));
#46949=CARTESIAN_POINT('Ctrl Pts',(-6.8945652935171,32.3460406401432,25.1198119664841));
#46950=CARTESIAN_POINT('Ctrl Pts',(-6.97213030605738,32.2552807417081,25.1139962989569));
#46951=CARTESIAN_POINT('Ctrl Pts',(-7.05360288281349,32.1680112577565,25.1081806314297));
#46952=CARTESIAN_POINT('Ctrl Pts',(-7.13862278214205,32.0845677135074,25.1023649639026));
#46953=CARTESIAN_POINT('Ctrl Pts',(-7.22376446329569,32.0010046453916,25.0965409660596));
#46954=CARTESIAN_POINT('Ctrl Pts',(-7.31246330612202,31.9212787272494,25.0907169682167));
#46955=CARTESIAN_POINT('Ctrl Pts',(-7.40432609492042,31.8456851808215,25.0848929703738));
#46956=CARTESIAN_POINT('Ctrl Pts',(-7.42869779324151,31.8256298011334,25.0833478320179));
#46957=CARTESIAN_POINT('Ctrl Pts',(-7.45329203647522,31.8058650485147,25.0818026936621));
#46958=CARTESIAN_POINT('Ctrl Pts',(-7.47810115818958,31.7863959124255,25.0802575553062));
#46959=CARTESIAN_POINT('Ctrl Pts',(-7.57160621141033,31.7130171516962,25.0744339616352));
#46960=CARTESIAN_POINT('Ctrl Pts',(-7.66846731883891,31.6436044726484,25.0686103679641));
#46961=CARTESIAN_POINT('Ctrl Pts',(-7.7683138464795,31.5784795905643,25.0627867742931));
#46962=CARTESIAN_POINT('Ctrl Pts',(-7.86803440289447,31.5134368731926,25.0569705279505));
#46963=CARTESIAN_POINT('Ctrl Pts',(-7.9707325489391,31.4526714141459,25.0511542816079));
#46964=CARTESIAN_POINT('Ctrl Pts',(-8.07600490987562,31.3964645286639,25.0453380352653));
#46965=CARTESIAN_POINT('Ctrl Pts',(-8.18117189259796,31.3403139065845,25.0395276110174));
#46966=CARTESIAN_POINT('Ctrl Pts',(-8.28890760584183,31.2887129714506,25.0337171867695));
#46967=CARTESIAN_POINT('Ctrl Pts',(-8.39878055358142,31.2418992450427,25.0279067625216));
#46968=CARTESIAN_POINT('Ctrl Pts',(-8.51281241966084,31.1933135222578,25.0218764016973));
#46969=CARTESIAN_POINT('Ctrl Pts',(-8.62914613917008,31.1498848252515,25.0158460408729));
#46970=CARTESIAN_POINT('Ctrl Pts',(-8.74727187910778,31.1118259741717,25.0098156800486));
#46971=CARTESIAN_POINT('Ctrl Pts',(-8.86096128169651,31.0751964635777,25.0040117958158));
#46972=CARTESIAN_POINT('Ctrl Pts',(-8.97631010603354,31.0435408686069,24.998207911583));
#46973=CARTESIAN_POINT('Ctrl Pts',(-9.09284507948373,31.0169992530527,24.9924040273502));
#46974=CARTESIAN_POINT('Ctrl Pts',(-9.20936283947211,30.9904615579789,24.9866010004132));
#46975=CARTESIAN_POINT('Ctrl Pts',(-9.3270660021089,30.9690364307456,24.9807979734761));
#46976=CARTESIAN_POINT('Ctrl Pts',(-9.44546900642545,30.952813276217,24.9749949465391));
#46977=CARTESIAN_POINT('Ctrl Pts',(-9.56388246448913,30.9365886893536,24.9691914072555));
#46978=CARTESIAN_POINT('Ctrl Pts',(-9.68299548250637,30.9255670437877,24.9633878679718));
#46979=CARTESIAN_POINT('Ctrl Pts',(-9.80231588616876,30.9197860361081,24.9575843286882));
#46980=CARTESIAN_POINT('Ctrl Pts',(-9.92167498404659,30.914003153715,24.9517789073845));
#46981=CARTESIAN_POINT('Ctrl Pts',(-10.0412411936714,30.9134643088361,24.9459734860807));
#46982=CARTESIAN_POINT('Ctrl Pts',(-10.1605214844378,30.9181550919916,24.940168064777));
#46983=CARTESIAN_POINT('Ctrl Pts',(-10.2799338670858,30.9228510697553,24.9343562145065));
#46984=CARTESIAN_POINT('Ctrl Pts',(-10.3990592905939,30.9327882194868,24.928544364236));
#46985=CARTESIAN_POINT('Ctrl Pts',(-10.5174088328717,30.9479001616858,24.9227325139655));
#46986=CARTESIAN_POINT('Ctrl Pts',(-10.6358361077642,30.9630220294894,24.9169168464406));
#46987=CARTESIAN_POINT('Ctrl Pts',(-10.7534860850753,30.9833253893368,24.9111011789156));
#46988=CARTESIAN_POINT('Ctrl Pts',(-10.8698806698456,31.0086928682161,24.9052855113907));
#46989=CARTESIAN_POINT('Ctrl Pts',(-10.9864419772903,31.0340966832697,24.89946151355));
#46990=CARTESIAN_POINT('Ctrl Pts',(-11.1017439096834,31.0645789915572,24.8936375157093));
#46991=CARTESIAN_POINT('Ctrl Pts',(-11.2153240055548,31.099972748618,24.8878135178686));
#46992=CARTESIAN_POINT('Ctrl Pts',(-11.2454574241771,31.1093629053171,24.8862683794916));
#46993=CARTESIAN_POINT('Ctrl Pts',(-11.2754697617164,31.119098503343,24.8847232411147));
#46994=CARTESIAN_POINT('Ctrl Pts',(-11.3053526426732,31.1291758657534,24.8831781027377));
#46995=CARTESIAN_POINT('Ctrl Pts',(-11.4179805852676,31.1671572302912,24.8773545090664));
#46996=CARTESIAN_POINT('Ctrl Pts',(-11.529131078261,31.2101195632519,24.8715309153951));
#46997=CARTESIAN_POINT('Ctrl Pts',(-11.6383318802172,31.2579292296559,24.8657073217238));
#46998=CARTESIAN_POINT('Ctrl Pts',(-11.7473949091412,31.3056785770641,24.859891075381));
#46999=CARTESIAN_POINT('Ctrl Pts',(-11.8545127688013,31.3582629317444,24.8540748290382));
#47000=CARTESIAN_POINT('Ctrl Pts',(-11.9592290599093,31.4154991294733,24.8482585826953));
#47001=CARTESIAN_POINT('Ctrl Pts',(-12.0638405294322,31.4726780334524,24.8424481584472));
#47002=CARTESIAN_POINT('Ctrl Pts',(-12.1660548565827,31.5344993221901,24.836637734199));
#47003=CARTESIAN_POINT('Ctrl Pts',(-12.2654368545924,31.6007323056496,24.8308273099508));
#47004=CARTESIAN_POINT('Ctrl Pts',(-12.3685806667885,31.6694723445293,24.8247969491266));
#47005=CARTESIAN_POINT('Ctrl Pts',(-12.4686730836359,31.7429644808949,24.8187665883024));
#47006=CARTESIAN_POINT('Ctrl Pts',(-12.5652566366221,31.8208989653888,24.8127362274781));
#47007=CARTESIAN_POINT('Ctrl Pts',(-12.6582128919254,31.8959065377296,24.8069323432451));
#47008=CARTESIAN_POINT('Ctrl Pts',(-12.7479187422818,31.9750285219178,24.8011284590121));
#47009=CARTESIAN_POINT('Ctrl Pts',(-12.8339976115554,32.0579458642475,24.795324574779));
#47010=CARTESIAN_POINT('Ctrl Pts',(-12.9200637660593,32.1408509587989,24.7895215478417));
#47011=CARTESIAN_POINT('Ctrl Pts',(-13.0025037108972,32.2275500133955,24.7837185209045));
#47012=CARTESIAN_POINT('Ctrl Pts',(-13.080976503583,32.3176859273438,24.7779154939672));
#47013=CARTESIAN_POINT('Ctrl Pts',(-13.1594562245957,32.4078297993508,24.7721119546833));
#47014=CARTESIAN_POINT('Ctrl Pts',(-13.2339678289211,32.5014108260291,24.7663084153994));
#47015=CARTESIAN_POINT('Ctrl Pts',(-13.3042099961909,32.5980380308856,24.7605048761156));
#47016=CARTESIAN_POINT('Ctrl Pts',(-13.3744749421764,32.6946965708177,24.7546994548116));
#47017=CARTESIAN_POINT('Ctrl Pts',(-13.4404674576145,32.7944029233995,24.7488940335076));
#47018=CARTESIAN_POINT('Ctrl Pts',(-13.5019293327583,32.896736833307,24.7430886122036));
#47019=CARTESIAN_POINT('Ctrl Pts',(-13.5634592712398,32.9991840685478,24.7372767619329));
#47020=CARTESIAN_POINT('Ctrl Pts',(-13.6204483441698,33.1042643190166,24.7314649116622));
#47021=CARTESIAN_POINT('Ctrl Pts',(-13.6726840601651,33.2115322775602,24.7256530613915));
#47022=CARTESIAN_POINT('Ctrl Pts',(-13.7249540848591,33.3188706902747,24.7198373938663));
#47023=CARTESIAN_POINT('Ctrl Pts',(-13.7724643728939,33.4283992989325,24.7140217263411));
#47024=CARTESIAN_POINT('Ctrl Pts',(-13.815051017427,33.5396538990948,24.7082060588159));
#47025=CARTESIAN_POINT('Ctrl Pts',(-13.8576986627298,33.6510678594582,24.702382060975));
#47026=CARTESIAN_POINT('Ctrl Pts',(-13.8954084592957,33.7642123598829,24.6965580631341));
#47027=CARTESIAN_POINT('Ctrl Pts',(-13.928066613758,33.8786090432503,24.6907340652932));
#47028=CARTESIAN_POINT('Ctrl Pts',(-13.936731000161,33.90895910694,24.6891889269185));
#47029=CARTESIAN_POINT('Ctrl Pts',(-13.9450400971673,33.9393972602586,24.6876437885439));
#47030=CARTESIAN_POINT('Ctrl Pts',(-13.9529923889216,33.9699144826142,24.6860986501693));
#47031=CARTESIAN_POINT('Ctrl Pts',(-13.9915465443551,34.1178675218693,24.6786075385625));
#47032=CARTESIAN_POINT('Ctrl Pts',(-14.0218101378451,34.2680627700932,24.6711164269557));
#47033=CARTESIAN_POINT('Ctrl Pts',(-14.0435706506767,34.4196885379504,24.6636253153489));
#47034=CARTESIAN_POINT('Ctrl Pts',(-14.0649246235171,34.5684815629024,24.6562741561629));
#47035=CARTESIAN_POINT('Ctrl Pts',(-14.0780902876873,34.7186523616395,24.6489229969768));
#47036=CARTESIAN_POINT('Ctrl Pts',(-14.0829121862387,34.8694125600844,24.6415718377907));
#47037=CARTESIAN_POINT('Ctrl Pts',(-14.084264918109,34.911706715187,24.6395095490036));
#47038=CARTESIAN_POINT('Ctrl Pts',(-14.0849612552969,34.9540471161242,24.6374472602165));
#47039=CARTESIAN_POINT('Ctrl Pts',(-14.0849984277889,34.9964160131029,24.6353849714293));
#47040=CARTESIAN_POINT('Ctrl Pts',(-14.0849984277894,34.9964160136128,24.6353849714045));
#47041=CARTESIAN_POINT('Ctrl Pts',(-14.0851020062225,35.1144738661964,24.6296385535608));
#47042=CARTESIAN_POINT('Ctrl Pts',(-14.0800834836686,35.2326545958956,24.6238921357172));
#47043=CARTESIAN_POINT('Ctrl Pts',(-14.0699376947858,35.3504741938599,24.6181457178735));
#47044=CARTESIAN_POINT('Ctrl Pts',(-14.0597976023172,35.4682276413016,24.6124025263907));
#47045=CARTESIAN_POINT('Ctrl Pts',(-14.0445360024406,35.5856199446743,24.606659334908));
#47046=CARTESIAN_POINT('Ctrl Pts',(-14.024199795063,35.7021687898326,24.6009161434252));
#47047=CARTESIAN_POINT('Ctrl Pts',(-14.003869129897,35.8186858720201,24.5951745171302));
#47048=CARTESIAN_POINT('Ctrl Pts',(-13.9784666777729,35.934359541358,24.5894328908351));
#47049=CARTESIAN_POINT('Ctrl Pts',(-13.9480909112641,36.0487150024645,24.5836912645401));
#47050=CARTESIAN_POINT('Ctrl Pts',(-13.9177158689797,36.1630677370876,24.577949775138));
#47051=CARTESIAN_POINT('Ctrl Pts',(-13.8823678558293,36.276101922028,24.5722082857358));
#47052=CARTESIAN_POINT('Ctrl Pts',(-13.842195744884,36.3873560674878,24.5664667963337));
#47053=CARTESIAN_POINT('Ctrl Pts',(-13.8020146008845,36.4986352294257,24.5607240159069));
#47054=CARTESIAN_POINT('Ctrl Pts',(-13.7570073454804,36.6081331633929,24.5549812354801));
#47055=CARTESIAN_POINT('Ctrl Pts',(-13.7073714148722,36.7154072962969,24.5492384550533));
#47056=CARTESIAN_POINT('Ctrl Pts',(-13.657683486109,36.8227938086187,24.5434896585413));
#47057=CARTESIAN_POINT('Ctrl Pts',(-13.6033573785645,36.9279514897564,24.5377408620293));
#47058=CARTESIAN_POINT('Ctrl Pts',(-13.5446370465652,37.03046132889,24.5319920655174));
#47059=CARTESIAN_POINT('Ctrl Pts',(-13.4858820406439,37.1330316993258,24.5262398743836));
#47060=CARTESIAN_POINT('Ctrl Pts',(-13.4227278681908,37.2329507627263,24.5204876832497));
#47061=CARTESIAN_POINT('Ctrl Pts',(-13.355461467923,37.3298290360634,24.5147354921159));
#47062=CARTESIAN_POINT('Ctrl Pts',(-13.288094569961,37.4268520479781,24.5089747070638));
#47063=CARTESIAN_POINT('Ctrl Pts',(-13.2166034327953,37.5208248695699,24.5032139220118));
#47064=CARTESIAN_POINT('Ctrl Pts',(-13.141314941821,37.6113914751128,24.4974531369597));
#47065=CARTESIAN_POINT('Ctrl Pts',(-13.1045735045831,37.6555887649024,24.4946418238401));
#47066=CARTESIAN_POINT('Ctrl Pts',(-13.0669282755439,37.6989754169976,24.4918305107205));
#47067=CARTESIAN_POINT('Ctrl Pts',(-13.0284202510578,37.7415134110529,24.4890191976008));
#47068=CARTESIAN_POINT('Ctrl Pts',(-12.9486514461779,37.8296302384692,24.4831956039294));
#47069=CARTESIAN_POINT('Ctrl Pts',(-12.8649049617742,37.9144047658744,24.477372010258));
#47070=CARTESIAN_POINT('Ctrl Pts',(-12.7774917727232,37.9954573027261,24.4715484165866));
#47071=CARTESIAN_POINT('Ctrl Pts',(-12.6901888683943,38.0764075797631,24.4657321702437));
#47072=CARTESIAN_POINT('Ctrl Pts',(-12.5992287573944,38.1536449309788,24.4599159239007));
#47073=CARTESIAN_POINT('Ctrl Pts',(-12.5049615082202,38.2268239558946,24.4540996775578));
#47074=CARTESIAN_POINT('Ctrl Pts',(-12.4107886210825,38.2999297282026,24.4482892533095));
#47075=CARTESIAN_POINT('Ctrl Pts',(-12.3133155022275,38.3689850069095,24.4424788290612));
#47076=CARTESIAN_POINT('Ctrl Pts',(-12.2129273337961,38.433682806454,24.4366684048129));
#47077=CARTESIAN_POINT('Ctrl Pts',(-12.1087392655496,38.5008295515304,24.4306380439888));
#47078=CARTESIAN_POINT('Ctrl Pts',(-12.0014114347734,38.5632821155977,24.4246076831646));
#47079=CARTESIAN_POINT('Ctrl Pts',(-11.8914104071374,38.6207446294612,24.4185773223404));
#47080=CARTESIAN_POINT('Ctrl Pts',(-11.7855405846603,38.6760490777246,24.4127734381072));
#47081=CARTESIAN_POINT('Ctrl Pts',(-11.6771951282994,38.7267313236942,24.406969553874));
#47082=CARTESIAN_POINT('Ctrl Pts',(-11.5668168564609,38.7725733840854,24.4011656696409));
#47083=CARTESIAN_POINT('Ctrl Pts',(-11.4564548886736,38.8184086731141,24.3953626427035));
#47084=CARTESIAN_POINT('Ctrl Pts',(-11.3440610795531,38.8594050417916,24.3895596157661));
#47085=CARTESIAN_POINT('Ctrl Pts',(-11.2300989151574,38.8953923626419,24.3837565888287));
#47086=CARTESIAN_POINT('Ctrl Pts',(-11.1161266890942,38.9313828607963,24.3779530495447));
#47087=CARTESIAN_POINT('Ctrl Pts',(-11.0005862218483,38.9623633088637,24.3721495102607));
#47088=CARTESIAN_POINT('Ctrl Pts',(-10.8839562508837,38.9882134279052,24.3663459709767));
#47089=CARTESIAN_POINT('Ctrl Pts',(-10.7672884581794,39.014071929839,24.3605405496725));
#47090=CARTESIAN_POINT('Ctrl Pts',(-10.6495308575529,39.0347967056966,24.3547351283684));
#47091=CARTESIAN_POINT('Ctrl Pts',(-10.531171830717,39.0503186894679,24.3489297070643));
#47092=CARTESIAN_POINT('Ctrl Pts',(-10.4126817322146,39.0658578623994,24.3431178567934));
#47093=CARTESIAN_POINT('Ctrl Pts',(-10.2935892831723,39.0761826894489,24.3373060065226));
#47094=CARTESIAN_POINT('Ctrl Pts',(-10.1743875930832,39.0812760219542,24.3314941562517));
#47095=CARTESIAN_POINT('Ctrl Pts',(-10.0551076106835,39.0863726997878,24.3256784887264));
#47096=CARTESIAN_POINT('Ctrl Pts',(-9.93571865174297,39.0862310405332,24.319862821201));
#47097=CARTESIAN_POINT('Ctrl Pts',(-9.81671176650951,39.0808859851096,24.3140471536757));
#47098=CARTESIAN_POINT('Ctrl Pts',(-9.69753441676378,39.0755332734713,24.3082231558346));
#47099=CARTESIAN_POINT('Ctrl Pts',(-9.57874063835108,39.064962325341,24.3023991579936));
#47100=CARTESIAN_POINT('Ctrl Pts',(-9.46081446167668,39.0492596798999,24.2965751601525));
#47101=CARTESIAN_POINT('Ctrl Pts',(-9.4295280041992,39.0450936824706,24.2950300217791));
#47102=CARTESIAN_POINT('Ctrl Pts',(-9.39830254646565,39.0405667565594,24.2934848834058));
#47103=CARTESIAN_POINT('Ctrl Pts',(-9.36714696466197,39.035681111741,24.2919397450324));
#47104=CARTESIAN_POINT('Ctrl Pts',(-9.24972281423343,39.0172673104611,24.2861161798706));
#47105=CARTESIAN_POINT('Ctrl Pts',(-9.1329136420351,38.9936946162266,24.2802926147089));
#47106=CARTESIAN_POINT('Ctrl Pts',(-9.01720746822139,38.9650149860348,24.2744690495471));
#47107=CARTESIAN_POINT('Ctrl Pts',(-8.90164192703478,38.9363702138941,24.2686525625147));
#47108=CARTESIAN_POINT('Ctrl Pts',(-8.78717711116186,38.9026309465696,24.2628360754823));
#47109=CARTESIAN_POINT('Ctrl Pts',(-8.67429385793938,38.8639006489431,24.2570195884499));
#47110=CARTESIAN_POINT('Ctrl Pts',(-8.56153930383042,38.8252145080434,24.2512097328416));
#47111=CARTESIAN_POINT('Ctrl Pts',(-8.45036310699467,38.7815487958191,24.2453998772333));
#47112=CARTESIAN_POINT('Ctrl Pts',(-8.34123302696642,38.7330573434081,24.239590021625));
#47113=CARTESIAN_POINT('Ctrl Pts',(-8.23217569907244,38.6845982180755,24.2337840391871));
#47114=CARTESIAN_POINT('Ctrl Pts',(-8.12516214703689,38.6313199156194,24.2279780567491));
#47115=CARTESIAN_POINT('Ctrl Pts',(-8.02064187898784,38.5734250277266,24.2221720743112));
#47116=CARTESIAN_POINT('Ctrl Pts',(-7.91616129548763,38.5155521215275,24.216368296305));
#47117=CARTESIAN_POINT('Ctrl Pts',(-7.81417247075485,38.4530663117817,24.2105645182988));
#47118=CARTESIAN_POINT('Ctrl Pts',(-7.71510143288208,38.3862166997968,24.2047607402926));
#47119=CARTESIAN_POINT('Ctrl Pts',(-7.6462217291788,38.3397391260772,24.2007256305571));
#47120=CARTESIAN_POINT('Ctrl Pts',(-7.57875194927019,38.2911531563236,24.1966905208216));
#47121=CARTESIAN_POINT('Ctrl Pts',(-7.51282733495086,38.2405550657615,24.1926554110861));
#47122=CARTESIAN_POINT('',(-14.084998667809,35.0032990905415,24.7396150285614));
#47123=CARTESIAN_POINT('Ctrl Pts',(-14.084998667809,35.0032990905415,24.7396150285614));
#47124=CARTESIAN_POINT('Ctrl Pts',(-14.0848838734084,35.145439770813,24.7327077308575));
#47125=CARTESIAN_POINT('Ctrl Pts',(-14.0773464015934,35.2872683007845,24.7258004331536));
#47126=CARTESIAN_POINT('Ctrl Pts',(-14.0625068059482,35.4280928072564,24.7188931354498));
#47127=CARTESIAN_POINT('Ctrl Pts',(-14.0474942948949,35.5705582430094,24.7119053518465));
#47128=CARTESIAN_POINT('Ctrl Pts',(-14.0250085659473,35.7119960749589,24.7049175682433));
#47129=CARTESIAN_POINT('Ctrl Pts',(-13.9952238380689,35.8517109155848,24.6979297846401));
#47130=CARTESIAN_POINT('Ctrl Pts',(-13.9681220732688,35.9788404554339,24.6915714499774));
#47131=CARTESIAN_POINT('Ctrl Pts',(-13.9349776994647,36.1045436836478,24.6852131153147));
#47132=CARTESIAN_POINT('Ctrl Pts',(-13.8959562242754,36.2283118897615,24.6788547806521));
#47133=CARTESIAN_POINT('Ctrl Pts',(-13.8602164861204,36.341671091508,24.673031186981));
#47134=CARTESIAN_POINT('Ctrl Pts',(-13.8194674520747,36.4536519397332,24.66720759331));
#47135=CARTESIAN_POINT('Ctrl Pts',(-13.7738333631693,36.5637796350606,24.661383999639));
#47136=CARTESIAN_POINT('Ctrl Pts',(-13.7282568484454,36.6737683879422,24.6555677532964));
#47137=CARTESIAN_POINT('Ctrl Pts',(-13.677807692304,36.7819082643004,24.6497515069538));
#47138=CARTESIAN_POINT('Ctrl Pts',(-13.6226599695283,36.8877393212987,24.6439352606112));
#47139=CARTESIAN_POINT('Ctrl Pts',(-13.5675674499273,36.9934644408251,24.6381248363633));
#47140=CARTESIAN_POINT('Ctrl Pts',(-13.5077859079211,37.0968849786803,24.6323144121154));
#47141=CARTESIAN_POINT('Ctrl Pts',(-13.4435373555386,37.1975612576241,24.6265039878675));
#47142=CARTESIAN_POINT('Ctrl Pts',(-13.3768568625528,37.3020483419707,24.6204736270431));
#47143=CARTESIAN_POINT('Ctrl Pts',(-13.3053646778811,37.4035788967282,24.6144432662188));
#47144=CARTESIAN_POINT('Ctrl Pts',(-13.2293614153235,37.5016893990301,24.6084129053945));
#47145=CARTESIAN_POINT('Ctrl Pts',(-13.1562125358369,37.596115257444,24.6026090211617));
#47146=CARTESIAN_POINT('Ctrl Pts',(-13.0788855771601,37.6873729663277,24.5968051369289));
#47147=CARTESIAN_POINT('Ctrl Pts',(-12.9976920602387,37.7750796947082,24.5910012526961));
#47148=CARTESIAN_POINT('Ctrl Pts',(-12.9165105364681,37.862773467867,24.585198225759));
#47149=CARTESIAN_POINT('Ctrl Pts',(-12.8314638675764,37.9469170040542,24.579395198822));
#47150=CARTESIAN_POINT('Ctrl Pts',(-12.7429023208599,38.0271623442131,24.573592171885));
#47151=CARTESIAN_POINT('Ctrl Pts',(-12.6543329550849,38.1074147691964,24.5677886326014));
#47152=CARTESIAN_POINT('Ctrl Pts',(-12.5622483970906,38.1837680396641,24.5619850933177));
#47153=CARTESIAN_POINT('Ctrl Pts',(-12.4670335692749,38.2559131389014,24.5561815540341));
#47154=CARTESIAN_POINT('Ctrl Pts',(-12.3717878644008,38.3280816339531,24.5503761327304));
#47155=CARTESIAN_POINT('Ctrl Pts',(-12.2734101961747,38.3960389972939,24.5445707114266));
#47156=CARTESIAN_POINT('Ctrl Pts',(-12.1723156152314,38.4595187335555,24.5387652901229));
#47157=CARTESIAN_POINT('Ctrl Pts',(-12.071109081397,38.5230687677495,24.5329534398524));
#47158=CARTESIAN_POINT('Ctrl Pts',(-11.9671799751829,38.5821310598852,24.5271415895819));
#47159=CARTESIAN_POINT('Ctrl Pts',(-11.8609693010198,38.63648432702,24.5213297393114));
#47160=CARTESIAN_POINT('Ctrl Pts',(-11.7546888671159,38.6908732936724,24.5155140717865));
#47161=CARTESIAN_POINT('Ctrl Pts',(-11.6461242513323,38.7405469062056,24.5096984042615));
#47162=CARTESIAN_POINT('Ctrl Pts',(-11.5357363154178,38.7853320818004,24.5038827367366));
#47163=CARTESIAN_POINT('Ctrl Pts',(-11.4251902607046,38.8301814073233,24.4980587388959));
#47164=CARTESIAN_POINT('Ctrl Pts',(-11.3128160564156,38.8701281836955,24.4922347410552));
#47165=CARTESIAN_POINT('Ctrl Pts',(-11.1990897082746,38.9050491509724,24.4864107432145));
#47166=CARTESIAN_POINT('Ctrl Pts',(-11.168917488128,38.9143138739643,24.4848656048375));
#47167=CARTESIAN_POINT('Ctrl Pts',(-11.1386501479591,38.9232251248635,24.4833204664606));
#47168=CARTESIAN_POINT('Ctrl Pts',(-11.1082966765157,38.9317812091753,24.4817753280836));
#47169=CARTESIAN_POINT('Ctrl Pts',(-10.993890353726,38.9640302435378,24.4759514933952));
#47170=CARTESIAN_POINT('Ctrl Pts',(-10.8778908004984,38.9913336744909,24.4701276587067));
#47171=CARTESIAN_POINT('Ctrl Pts',(-10.7607632878954,39.0135351275142,24.4643038240182));
#47172=CARTESIAN_POINT('Ctrl Pts',(-10.643784722252,39.0357083477265,24.4584873952966));
#47173=CARTESIAN_POINT('Ctrl Pts',(-10.5256814480422,39.0527924196243,24.4526709665749));
#47174=CARTESIAN_POINT('Ctrl Pts',(-10.406933615581,39.0646808032747,24.4468545378532));
#47175=CARTESIAN_POINT('Ctrl Pts',(-10.2883058386793,39.076557167619,24.4410439896145));
#47176=CARTESIAN_POINT('Ctrl Pts',(-10.1690352040094,39.0832482538052,24.4352334413758));
#47177=CARTESIAN_POINT('Ctrl Pts',(-10.0496111758125,39.0846987320039,24.4294228931371));
#47178=CARTESIAN_POINT('Ctrl Pts',(-9.93027871603207,39.086148098048,24.4236168001383));
#47179=CARTESIAN_POINT('Ctrl Pts',(-9.81079350372809,39.0823648482954,24.4178107071396));
#47180=CARTESIAN_POINT('Ctrl Pts',(-9.69164860839685,39.073345605187,24.4120046141408));
#47181=CARTESIAN_POINT('Ctrl Pts',(-9.5725522194164,39.064330033999,24.4062008849226));
#47182=CARTESIAN_POINT('Ctrl Pts',(-9.45379627835535,39.0500827395527,24.4003971557043));
#47183=CARTESIAN_POINT('Ctrl Pts',(-9.33587187472176,39.0306524078881,24.3945934264861));
#47184=CARTESIAN_POINT('Ctrl Pts',(-9.21796765035945,39.0112254011498,24.3887906904043));
#47185=CARTESIAN_POINT('Ctrl Pts',(-9.10089508299161,38.9866171882742,24.3829879543226));
#47186=CARTESIAN_POINT('Ctrl Pts',(-8.98513753636281,38.956927997816,24.3771852182408));
#47187=CARTESIAN_POINT('Ctrl Pts',(-8.86937247998411,38.927236881277,24.3713821057076));
#47188=CARTESIAN_POINT('Ctrl Pts',(-8.75492300913772,38.8924642342029,24.3655789931744));
#47189=CARTESIAN_POINT('Ctrl Pts',(-8.64225911211109,38.8527606571593,24.3597758806412));
#47190=CARTESIAN_POINT('Ctrl Pts',(-8.52950544821218,38.8130254456168,24.3539681443795));
#47191=CARTESIAN_POINT('Ctrl Pts',(-8.41854058513476,38.7683515933072,24.3481604081179));
#47192=CARTESIAN_POINT('Ctrl Pts',(-8.30981632197193,38.7189385763316,24.3423526718563));
#47193=CARTESIAN_POINT('Ctrl Pts',(-8.20104516969539,38.6695042491857,24.3365424309136));
#47194=CARTESIAN_POINT('Ctrl Pts',(-8.09451690726418,38.6153268687497,24.3307321899709));
#47195=CARTESIAN_POINT('Ctrl Pts',(-7.9906590570246,38.5566520739148,24.3249219490281));
#47196=CARTESIAN_POINT('Ctrl Pts',(-7.88666743955713,38.4979017068952,24.3191042245893));
#47197=CARTESIAN_POINT('Ctrl Pts',(-7.78535345100347,38.4346425708196,24.3132865001504));
#47198=CARTESIAN_POINT('Ctrl Pts',(-7.68711615239853,38.367163985835,24.3074687757115));
#47199=CARTESIAN_POINT('Ctrl Pts',(-7.62787443402184,38.3264712206136,24.3039604138398));
#47200=CARTESIAN_POINT('Ctrl Pts',(-7.56975099729801,38.2842447961043,24.3004520519682));
#47201=CARTESIAN_POINT('Ctrl Pts',(-7.51282733495087,38.2405550657615,24.2969436900965));
#47202=CARTESIAN_POINT('Ctrl Pts',(-7.51282733495086,38.2405550657615,25.5469376052728));
#47203=CARTESIAN_POINT('Ctrl Pts',(-7.41802255720225,38.1677910339992,25.5411329091515));
#47204=CARTESIAN_POINT('Ctrl Pts',(-7.3264425387479,38.0908854305494,25.5353282130303));
#47205=CARTESIAN_POINT('Ctrl Pts',(-7.23845601126725,38.0101660748693,25.529523516909));
#47206=CARTESIAN_POINT('Ctrl Pts',(-7.15037508265753,37.9293601150404,25.5237125929039));
#47207=CARTESIAN_POINT('Ctrl Pts',(-7.06589564461184,37.8447325091728,25.5179016688989));
#47208=CARTESIAN_POINT('Ctrl Pts',(-6.98534998547147,37.7566483798089,25.5120907448938));
#47209=CARTESIAN_POINT('Ctrl Pts',(-6.90475667042894,37.6685121343075,25.5062763827789));
#47210=CARTESIAN_POINT('Ctrl Pts',(-6.82810203213645,37.5769156044792,25.5004620206639));
#47211=CARTESIAN_POINT('Ctrl Pts',(-6.75567734419892,37.4822561320411,25.494647658549));
#47212=CARTESIAN_POINT('Ctrl Pts',(-6.68314285103467,37.3874531435573,25.4888244811065));
#47213=CARTESIAN_POINT('Ctrl Pts',(-6.61485134901944,37.2895782729125,25.483001303664));
#47214=CARTESIAN_POINT('Ctrl Pts',(-6.55105035391789,37.1890571803382,25.4771781262214));
#47215=CARTESIAN_POINT('Ctrl Pts',(-6.51450884287949,37.1314845263686,25.4738429477896));
#47216=CARTESIAN_POINT('Ctrl Pts',(-6.47943952189608,37.0730442819452,25.4705077693577));
#47217=CARTESIAN_POINT('Ctrl Pts',(-6.44588189144363,37.013819622119,25.4671725909258));
#47218=CARTESIAN_POINT('Ctrl Pts',(-6.38728652428229,36.9104067577203,25.4613489972415));
#47219=CARTESIAN_POINT('Ctrl Pts',(-6.33311386295598,36.8042676180022,25.4555254035571));
#47220=CARTESIAN_POINT('Ctrl Pts',(-6.28362667865849,36.6958167166357,25.4497018098728));
#47221=CARTESIAN_POINT('Ctrl Pts',(-6.23420192979309,36.5875026421868,25.4438855635167));
#47222=CARTESIAN_POINT('Ctrl Pts',(-6.18945106829059,36.4768829754139,25.4380693171607));
#47223=CARTESIAN_POINT('Ctrl Pts',(-6.14959202974776,36.364398571759,25.4322530708046));
#47224=CARTESIAN_POINT('Ctrl Pts',(-6.10977289032142,36.2520267656099,25.4264426465431));
#47225=CARTESIAN_POINT('Ctrl Pts',(-6.07483596799513,36.1377943186469,25.4206322222815));
#47226=CARTESIAN_POINT('Ctrl Pts',(-6.04495169710269,36.0221633537498,25.41482179802));
#47227=CARTESIAN_POINT('Ctrl Pts',(-6.01393624484118,35.9021555180351,25.4087914372007));
#47228=CARTESIAN_POINT('Ctrl Pts',(-5.98836369439253,35.7806416066818,25.4027610763815));
#47229=CARTESIAN_POINT('Ctrl Pts',(-5.96836835913579,35.6581575133526,25.3967307155622));
#47230=CARTESIAN_POINT('Ctrl Pts',(-5.94912396982272,35.5402734395715,25.3909268313155));
#47231=CARTESIAN_POINT('Ctrl Pts',(-5.93504550560123,35.4214911813111,25.3851229470688));
#47232=CARTESIAN_POINT('Ctrl Pts',(-5.92620079771532,35.3022996186976,25.379319062822));
#47233=CARTESIAN_POINT('Ctrl Pts',(-5.91735739628723,35.1831256619508,25.373516035871));
#47234=CARTESIAN_POINT('Ctrl Pts',(-5.91374624398912,35.0635429281912,25.36771300892));
#47235=CARTESIAN_POINT('Ctrl Pts',(-5.9153832462466,34.9440448844426,25.3619099819689));
#47236=CARTESIAN_POINT('Ctrl Pts',(-5.91702039303428,34.8245362902649,25.3561064426712));
#47237=CARTESIAN_POINT('Ctrl Pts',(-5.9239066100501,34.7051128092835,25.3503029033735));
#47238=CARTESIAN_POINT('Ctrl Pts',(-5.93600568662888,34.5862667273627,25.3444993640758));
#47239=CARTESIAN_POINT('Ctrl Pts',(-5.94810868679719,34.4673821050426,25.338693942758));
#47240=CARTESIAN_POINT('Ctrl Pts',(-5.96542786715539,34.349075660197,25.3328885214401));
#47241=CARTESIAN_POINT('Ctrl Pts',(-5.98787536717668,34.2318327456261,25.3270831001222));
#47242=CARTESIAN_POINT('Ctrl Pts',(-6.0103477257265,34.1144599953793,25.3212712498376));
#47243=CARTESIAN_POINT('Ctrl Pts',(-6.03795966315626,33.9981535276099,25.315459399553));
#47244=CARTESIAN_POINT('Ctrl Pts',(-6.0705725448776,33.8833868732053,25.3096475492684));
#47245=CARTESIAN_POINT('Ctrl Pts',(-6.10320684691488,33.7685448394454,25.3038318817293));
#47246=CARTESIAN_POINT('Ctrl Pts',(-6.14084850625437,33.6552450198145,25.2980162141902));
#47247=CARTESIAN_POINT('Ctrl Pts',(-6.18331008294142,33.543942625779,25.292200546651));
#47248=CARTESIAN_POINT('Ctrl Pts',(-6.22583248125123,33.4324808030847,25.2863765487963));
#47249=CARTESIAN_POINT('Ctrl Pts',(-6.27318841537602,33.3230224900152,25.2805525509415));
#47250=CARTESIAN_POINT('Ctrl Pts',(-6.32514366485763,33.2160000235247,25.2747285530867));
#47251=CARTESIAN_POINT('Ctrl Pts',(-6.33892767455449,33.1876063822544,25.2731834148436));
#47252=CARTESIAN_POINT('Ctrl Pts',(-6.35303517530403,33.1593840413966,25.2716382766005));
#47253=CARTESIAN_POINT('Ctrl Pts',(-6.36746128086535,33.1313407335772,25.2700931383574));
#47254=CARTESIAN_POINT('Ctrl Pts',(-6.42183297051189,33.0256460938884,25.2642695446884));
#47255=CARTESIAN_POINT('Ctrl Pts',(-6.48090920439752,32.9221560328926,25.2584459510193));
#47256=CARTESIAN_POINT('Ctrl Pts',(-6.54448733684888,32.8213175461297,25.2526223573503));
#47257=CARTESIAN_POINT('Ctrl Pts',(-6.60798525604231,32.7206062820963,25.2468061110097));
#47258=CARTESIAN_POINT('Ctrl Pts',(-6.67597356092362,32.6225402808324,25.2409898646691));
#47259=CARTESIAN_POINT('Ctrl Pts',(-6.74820299708105,32.5275434782777,25.2351736183285));
#47260=CARTESIAN_POINT('Ctrl Pts',(-6.82036013117396,32.4326417680469,25.2293631940827));
#47261=CARTESIAN_POINT('Ctrl Pts',(-6.89674970512732,32.3408034677767,25.2235527698368));
#47262=CARTESIAN_POINT('Ctrl Pts',(-6.97707863859544,32.2524244427561,25.2177423455909));
#47263=CARTESIAN_POINT('Ctrl Pts',(-7.0604481883922,32.1607000887864,25.2117119847658));
#47264=CARTESIAN_POINT('Ctrl Pts',(-7.14806097693785,32.0727024450321,25.2056816239407));
#47265=CARTESIAN_POINT('Ctrl Pts',(-7.23954242393711,31.9888376047186,25.1996512631157));
#47266=CARTESIAN_POINT('Ctrl Pts',(-7.32758818820413,31.908122397398,25.1938473788848));
#47267=CARTESIAN_POINT('Ctrl Pts',(-7.41921694001576,31.8312354687225,25.188043494654));
#47268=CARTESIAN_POINT('Ctrl Pts',(-7.51405697676075,31.7585015370653,25.1822396104232));
#47269=CARTESIAN_POINT('Ctrl Pts',(-7.60888300461805,31.6857783489877,25.1764365834882));
#47270=CARTESIAN_POINT('Ctrl Pts',(-7.70691905016106,31.6172071864138,25.1706335565532));
#47271=CARTESIAN_POINT('Ctrl Pts',(-7.80776111058734,31.5530718528309,25.1648305296181));
#47272=CARTESIAN_POINT('Ctrl Pts',(-7.90861207431313,31.4889308567686,25.1590269903365));
#47273=CARTESIAN_POINT('Ctrl Pts',(-8.01226920092046,31.4292266875141,25.1532234510548));
#47274=CARTESIAN_POINT('Ctrl Pts',(-8.11830090735156,31.3741989126917,25.1474199117732));
#47275=CARTESIAN_POINT('Ctrl Pts',(-8.22436699862915,31.3191532930033,25.1416144904714));
#47276=CARTESIAN_POINT('Ctrl Pts',(-8.33280883893436,31.2687872717215,25.1358090691696));
#47277=CARTESIAN_POINT('Ctrl Pts',(-8.44317233125128,31.2232934175636,25.1300036478679));
#47278=CARTESIAN_POINT('Ctrl Pts',(-8.55365804092114,31.1777491831729,25.1241917975993));
#47279=CARTESIAN_POINT('Ctrl Pts',(-8.66606927263243,31.1370880414473,25.1183799473308));
#47280=CARTESIAN_POINT('Ctrl Pts',(-8.77993398438469,31.101453614802,25.1125680970622));
#47281=CARTESIAN_POINT('Ctrl Pts',(-8.89387348309082,31.0657957832739,25.1067524295392));
#47282=CARTESIAN_POINT('Ctrl Pts',(-9.00926796928695,31.0351713464946,25.1009367620162));
#47283=CARTESIAN_POINT('Ctrl Pts',(-9.12563396948364,31.0096730654395,25.0951210944932));
#47284=CARTESIAN_POINT('Ctrl Pts',(-9.24216665141152,30.9841382608499,25.0892970966544));
#47285=CARTESIAN_POINT('Ctrl Pts',(-9.35967322398113,30.9637443371213,25.0834730988156));
#47286=CARTESIAN_POINT('Ctrl Pts',(-9.47766370191699,30.9485323903917,25.0776491009768));
#47287=CARTESIAN_POINT('Ctrl Pts',(-9.50896721933983,30.9444965779447,25.0761039625809));
#47288=CARTESIAN_POINT('Ctrl Pts',(-9.5403047920601,30.9408252247989,25.0745588241849));
#47289=CARTESIAN_POINT('Ctrl Pts',(-9.57166727427056,30.9375184829874,25.0730136857889));
#47290=CARTESIAN_POINT('Ctrl Pts',(-9.68987180102311,30.9250554436048,25.0671900921193));
#47291=CARTESIAN_POINT('Ctrl Pts',(-9.80881134156637,30.9177356190189,25.0613664984498));
#47292=CARTESIAN_POINT('Ctrl Pts',(-9.9280009587515,30.9156345489098,25.0555429047802));
#47293=CARTESIAN_POINT('Ctrl Pts',(-10.0470402005297,30.9135361296127,25.0497266584391));
#47294=CARTESIAN_POINT('Ctrl Pts',(-10.1663284867354,30.9166433760391,25.043910412098));
#47295=CARTESIAN_POINT('Ctrl Pts',(-10.2853746173911,30.9249802052323,25.0380941657569));
#47296=CARTESIAN_POINT('Ctrl Pts',(-10.4043015822122,30.9333086892133,25.0322837415105));
#47297=CARTESIAN_POINT('Ctrl Pts',(-10.5229864687082,30.9468563135307,25.0264733172642));
#47298=CARTESIAN_POINT('Ctrl Pts',(-10.640937530603,30.9655949531728,25.0206628930178));
#47299=CARTESIAN_POINT('Ctrl Pts',(-10.7633532842114,30.9850428890925,25.0146325321929));
#47300=CARTESIAN_POINT('Ctrl Pts',(-10.884978113858,31.0100825942663,25.008602171368));
#47301=CARTESIAN_POINT('Ctrl Pts',(-11.0052670436125,31.0406233860585,25.0025718105431));
#47302=CARTESIAN_POINT('Ctrl Pts',(-11.121038395089,31.0700171860381,24.9967679263119));
#47303=CARTESIAN_POINT('Ctrl Pts',(-11.235571948038,31.1045062163305,24.9909640420807));
#47304=CARTESIAN_POINT('Ctrl Pts',(-11.3483923635487,31.1439575943821,24.9851601578495));
#47305=CARTESIAN_POINT('Ctrl Pts',(-11.4611961142771,31.1834031450431,24.9793571309141));
#47306=CARTESIAN_POINT('Ctrl Pts',(-11.572286845455,31.227809451025,24.9735541039787));
#47307=CARTESIAN_POINT('Ctrl Pts',(-11.6812057324133,31.2769941867759,24.9677510770433));
#47308=CARTESIAN_POINT('Ctrl Pts',(-11.7901342357698,31.3261832650243,24.9619475377614));
#47309=CARTESIAN_POINT('Ctrl Pts',(-11.8968901414889,31.38015144379,24.9561439984794));
#47310=CARTESIAN_POINT('Ctrl Pts',(-12.0010365040093,31.4386690817024,24.9503404591974));
#47311=CARTESIAN_POINT('Ctrl Pts',(-12.1052166399804,31.4972056962023,24.9445350378953));
#47312=CARTESIAN_POINT('Ctrl Pts',(-12.2067851939559,31.5602945040393,24.9387296165933));
#47313=CARTESIAN_POINT('Ctrl Pts',(-12.3053321875728,31.627661270729,24.9329241952912));
#47314=CARTESIAN_POINT('Ctrl Pts',(-12.4039883128633,31.6951026398772,24.9271123450224));
#47315=CARTESIAN_POINT('Ctrl Pts',(-12.4996158613971,31.766831193643,24.9213004947536));
#47316=CARTESIAN_POINT('Ctrl Pts',(-12.5918359552986,31.8425308582947,24.9154886444848));
#47317=CARTESIAN_POINT('Ctrl Pts',(-12.6841166198525,31.9182802428921,24.9096729769616));
#47318=CARTESIAN_POINT('Ctrl Pts',(-12.7729850694209,31.9980056607131,24.9038573094384));
#47319=CARTESIAN_POINT('Ctrl Pts',(-12.858098698843,32.0813535966698,24.8980416419151));
#47320=CARTESIAN_POINT('Ctrl Pts',(-12.9433342443486,32.1648209195448,24.8922176440762));
#47321=CARTESIAN_POINT('Ctrl Pts',(-13.0248039568165,32.2519208200932,24.8863936462372));
#47322=CARTESIAN_POINT('Ctrl Pts',(-13.1022048725415,32.3422660161747,24.8805696483982));
#47323=CARTESIAN_POINT('Ctrl Pts',(-13.122739757652,32.366235089466,24.8790245100056));
#47324=CARTESIAN_POINT('Ctrl Pts',(-13.1429884873942,32.3904324289387,24.8774793716131));
#47325=CARTESIAN_POINT('Ctrl Pts',(-13.1629459212136,32.4148504686424,24.8759342332205));
#47326=CARTESIAN_POINT('Ctrl Pts',(-13.2378042578985,32.5064400915305,24.8701385737653));
#47327=CARTESIAN_POINT('Ctrl Pts',(-13.3088098080701,32.6014415259609,24.8643429143101));
#47328=CARTESIAN_POINT('Ctrl Pts',(-13.3756340199531,32.6994957154278,24.8585472548549));
#47329=CARTESIAN_POINT('Ctrl Pts',(-13.4423779072391,32.7974320409792,24.8527585619467));
#47330=CARTESIAN_POINT('Ctrl Pts',(-13.5049502169777,32.8984134904676,24.8469698690384));
#47331=CARTESIAN_POINT('Ctrl Pts',(-13.5630617794873,33.0020471087743,24.8411811761302));
#47332=CARTESIAN_POINT('Ctrl Pts',(-13.6211175348197,33.1055812030029,24.8353980423671));
#47333=CARTESIAN_POINT('Ctrl Pts',(-13.6747208597774,33.2117620448675,24.829614908604));
#47334=CARTESIAN_POINT('Ctrl Pts',(-13.723625557915,33.3201673582043,24.8238317748409));
#47335=CARTESIAN_POINT('Ctrl Pts',(-13.7724951073978,33.4284947587621,24.8180527975164));
#47336=CARTESIAN_POINT('Ctrl Pts',(-13.8166725773334,33.53904307673,24.8122738201918));
#47337=CARTESIAN_POINT('Ctrl Pts',(-13.8559577878752,33.6513656766476,24.8064948428672));
#47338=CARTESIAN_POINT('Ctrl Pts',(-13.8952293775642,33.763649332403,24.8007178692127));
#47339=CARTESIAN_POINT('Ctrl Pts',(-13.9296119399903,33.8777056600116,24.7949408955582));
#47340=CARTESIAN_POINT('Ctrl Pts',(-13.9589537101833,33.9930687607258,24.7891639219037));
#47341=CARTESIAN_POINT('Ctrl Pts',(-13.9882886312207,34.1084049326007,24.7833882967497));
#47342=CARTESIAN_POINT('Ctrl Pts',(-14.0125850024546,34.2250468704272,24.7776126715957));
#47343=CARTESIAN_POINT('Ctrl Pts',(-14.0317413883321,34.3425151122573,24.7718370464416));
#47344=CARTESIAN_POINT('Ctrl Pts',(-14.0509049499058,34.4600273559376,24.7660592578246));
#47345=CARTESIAN_POINT('Ctrl Pts',(-14.0649246106828,34.5783661150095,24.7602814692076));
#47346=CARTESIAN_POINT('Ctrl Pts',(-14.0737504068469,34.6970435300002,24.7545036805906));
#47347=CARTESIAN_POINT('Ctrl Pts',(-14.0813314046056,34.7989825732682,24.7495407965922));
#47348=CARTESIAN_POINT('Ctrl Pts',(-14.0850811474127,34.9011712045389,24.7445779125939));
#47349=CARTESIAN_POINT('Ctrl Pts',(-14.0849986678096,35.0032990898398,24.7396150285955));
#47350=CARTESIAN_POINT('Origin',(-10.,35.,32.7603849714045));
#47351=CARTESIAN_POINT('',(-7.51282733495086,38.2405550657615,26.7967727135811));
#47352=CARTESIAN_POINT('',(-7.51282733495086,38.2405550657615,26.6927653349501));
#47353=CARTESIAN_POINT('',(-7.51282733495086,38.2405550657615,32.7603849714045));
#47354=CARTESIAN_POINT('',(-14.0849995364304,35.0019461149621,25.8853849714457));
#47355=CARTESIAN_POINT('Ctrl Pts',(-7.51282733495086,38.2405550657615,26.6927653349501));
#47356=CARTESIAN_POINT('Ctrl Pts',(-7.41550399904621,38.1658580043565,26.6867866417674));
#47357=CARTESIAN_POINT('Ctrl Pts',(-7.32165086959052,38.08685124892,26.6808079485846));
#47358=CARTESIAN_POINT('Ctrl Pts',(-7.23165012498627,38.0039081160234,26.6748292554019));
#47359=CARTESIAN_POINT('Ctrl Pts',(-7.14164938038203,37.9209649831269,26.6688505622192));
#47360=CARTESIAN_POINT('Ctrl Pts',(-7.05550130075222,37.8340858473106,26.6628718690364));
#47361=CARTESIAN_POINT('Ctrl Pts',(-6.9735432720381,37.7436808622313,26.6568931758537));
#47362=CARTESIAN_POINT('Ctrl Pts',(-6.89371140427812,37.6556211696432,26.6510695823506));
#47363=CARTESIAN_POINT('Ctrl Pts',(-6.8175973521335,37.5639323246363,26.6452459888476));
#47364=CARTESIAN_POINT('Ctrl Pts',(-6.74554833177251,37.4689611862424,26.6394223953446));
#47365=CARTESIAN_POINT('Ctrl Pts',(-6.67359021199008,37.3741098680955,26.6336061491728));
#47366=CARTESIAN_POINT('Ctrl Pts',(-6.60568716786191,37.2759848155647,26.627789903001));
#47367=CARTESIAN_POINT('Ctrl Pts',(-6.542148441838,37.1749684139584,26.6219736568292));
#47368=CARTESIAN_POINT('Ctrl Pts',(-6.47867331845955,37.0740531303754,26.6161632327546));
#47369=CARTESIAN_POINT('Ctrl Pts',(-6.41955403834108,36.9702525991447,26.6103528086801));
#47370=CARTESIAN_POINT('Ctrl Pts',(-6.36505815740818,36.863980364965,26.6045423846056));
#47371=CARTESIAN_POINT('Ctrl Pts',(-6.30849949237123,36.7536855024396,26.5985120237172));
#47372=CARTESIAN_POINT('Ctrl Pts',(-6.25692142392517,36.6407284785424,26.5924816628289));
#47373=CARTESIAN_POINT('Ctrl Pts',(-6.21057243014792,36.5256027310034,26.5864513019405));
#47374=CARTESIAN_POINT('Ctrl Pts',(-6.16596412379834,36.4148006575079,26.5806474178865));
#47375=CARTESIAN_POINT('Ctrl Pts',(-6.12619937408759,36.3019902331726,26.5748435338324));
#47376=CARTESIAN_POINT('Ctrl Pts',(-6.09145149073612,36.1876335927933,26.5690396497783));
#47377=CARTESIAN_POINT('Ctrl Pts',(-6.05670874002877,36.0732938441461,26.5632366230217));
#47378=CARTESIAN_POINT('Ctrl Pts',(-6.0269815006576,35.95740872425,26.5574335962651));
#47379=CARTESIAN_POINT('Ctrl Pts',(-6.00239342363177,35.84045622169,26.5516305695084));
#47380=CARTESIAN_POINT('Ctrl Pts',(-5.97780317574206,35.7234933934766,26.5458270304067));
#47381=CARTESIAN_POINT('Ctrl Pts',(-5.95835307634472,35.6054633948514,26.5400234913049));
#47382=CARTESIAN_POINT('Ctrl Pts',(-5.94411566815009,35.4868544820112,26.5342199522032));
#47383=CARTESIAN_POINT('Ctrl Pts',(-5.92987364293303,35.3682071057088,26.5284145310826));
#47384=CARTESIAN_POINT('Ctrl Pts',(-5.92084771941127,35.2489808470468,26.5226091099621));
#47385=CARTESIAN_POINT('Ctrl Pts',(-5.91705852649427,35.1296685155574,26.5168036888415));
#47386=CARTESIAN_POINT('Ctrl Pts',(-5.91326513739736,35.0102240567207,26.5109918387552));
#47387=CARTESIAN_POINT('Ctrl Pts',(-5.91472006756182,34.8906937431675,26.5051799886689));
#47388=CARTESIAN_POINT('Ctrl Pts',(-5.92139181533038,34.771569975822,26.4993681385826));
#47389=CARTESIAN_POINT('Ctrl Pts',(-5.92806794513791,34.6523679673605,26.4935524712426));
#47390=CARTESIAN_POINT('Ctrl Pts',(-5.93996767577151,34.5335734422569,26.4877368039026));
#47391=CARTESIAN_POINT('Ctrl Pts',(-5.95700787207372,34.4156716218374,26.4819211365627));
#47392=CARTESIAN_POINT('Ctrl Pts',(-5.97407247661856,34.2976009197813,26.4760971389067));
#47393=CARTESIAN_POINT('Ctrl Pts',(-5.9962921674974,34.1804258743947,26.4702731412508));
#47394=CARTESIAN_POINT('Ctrl Pts',(-6.02353315355834,34.0646196393176,26.4644491435948));
#47395=CARTESIAN_POINT('Ctrl Pts',(-6.03076034396942,34.0338955785284,26.4629040034916));
#47396=CARTESIAN_POINT('Ctrl Pts',(-6.03834070085544,34.003267769391,26.4613588633884));
#47397=CARTESIAN_POINT('Ctrl Pts',(-6.0462711511481,33.9727448273402,26.4598137232852));
#47398=CARTESIAN_POINT('Ctrl Pts',(-6.07616081669262,33.8577046347074,26.453990129517));
#47399=CARTESIAN_POINT('Ctrl Pts',(-6.11112377218076,33.7437845469228,26.4481665357487));
#47400=CARTESIAN_POINT('Ctrl Pts',(-6.1510602459293,33.6314651010902,26.4423429419805));
#47401=CARTESIAN_POINT('Ctrl Pts',(-6.190946333893,33.5192873628972,26.4365266955395));
#47402=CARTESIAN_POINT('Ctrl Pts',(-6.23579332403263,33.4087066313721,26.4307104490985));
#47403=CARTESIAN_POINT('Ctrl Pts',(-6.28545091570393,33.3001911577018,26.4248942026575));
#47404=CARTESIAN_POINT('Ctrl Pts',(-6.33505879986176,33.191784308598,26.4190837783101));
#47405=CARTESIAN_POINT('Ctrl Pts',(-6.38946753689784,33.0854389738162,26.4132733539628));
#47406=CARTESIAN_POINT('Ctrl Pts',(-6.44847791432055,32.981605619575,26.4074629296154));
#47407=CARTESIAN_POINT('Ctrl Pts',(-6.50972195516655,32.8738419606042,26.401432568828));
#47408=CARTESIAN_POINT('Ctrl Pts',(-6.57592273232874,32.7687846290923,26.3954022080405));
#47409=CARTESIAN_POINT('Ctrl Pts',(-6.64680375535941,32.6669119294531,26.3893718472531));
#47410=CARTESIAN_POINT('Ctrl Pts',(-6.71502276806236,32.5688651646968,26.3835679629188));
#47411=CARTESIAN_POINT('Ctrl Pts',(-6.78757656909231,32.4737685065685,26.3777640785846));
#47412=CARTESIAN_POINT('Ctrl Pts',(-6.86417364427234,32.3820202317963,26.3719601942504));
#47413=CARTESIAN_POINT('Ctrl Pts',(-6.94075940525276,32.2902855092165,26.3661571672114));
#47414=CARTESIAN_POINT('Ctrl Pts',(-7.02138699104981,32.2018984997788,26.3603541401724));
#47415=CARTESIAN_POINT('Ctrl Pts',(-7.10572440673968,32.1172246375658,26.3545511131333));
#47416=CARTESIAN_POINT('Ctrl Pts',(-7.19006926854778,32.0325432995298,26.3487475737473));
#47417=CARTESIAN_POINT('Ctrl Pts',(-7.2781243232996,31.9515760498547,26.3429440343612));
#47418=CARTESIAN_POINT('Ctrl Pts',(-7.36952097283118,31.8746512054452,26.3371404949752));
#47419=CARTESIAN_POINT('Ctrl Pts',(-7.46094726123517,31.7977014152018,26.3313350735686));
#47420=CARTESIAN_POINT('Ctrl Pts',(-7.55571698728567,31.724796900126,26.3255296521621));
#47421=CARTESIAN_POINT('Ctrl Pts',(-7.65342928728698,31.6562250538893,26.3197242307556));
#47422=CARTESIAN_POINT('Ctrl Pts',(-7.75124979461412,31.5875772706814,26.3139123803824));
#47423=CARTESIAN_POINT('Ctrl Pts',(-7.85201904595084,31.523271968293,26.3081005300091));
#47424=CARTESIAN_POINT('Ctrl Pts',(-7.95530794327248,31.4635527159089,26.3022886796359));
#47425=CARTESIAN_POINT('Ctrl Pts',(-8.05866468129722,31.4037942395987,26.2964730120081));
#47426=CARTESIAN_POINT('Ctrl Pts',(-8.16454399981762,31.3486280002973,26.2906573443803));
#47427=CARTESIAN_POINT('Ctrl Pts',(-8.27249450201417,31.2982504468253,26.2848416767525));
#47428=CARTESIAN_POINT('Ctrl Pts',(-8.38059963163431,31.2478007329545,26.2790176788095));
#47429=CARTESIAN_POINT('Ctrl Pts',(-8.49078149049063,31.202153551386,26.2731936808666));
#47430=CARTESIAN_POINT('Ctrl Pts',(-8.60257100705781,31.1614563686621,26.2673696829236));
#47431=CARTESIAN_POINT('Ctrl Pts',(-8.63222935600017,31.1506591912231,26.2658245455214));
#47432=CARTESIAN_POINT('Ctrl Pts',(-8.66200079543199,31.1402101524658,26.2642794081191));
#47433=CARTESIAN_POINT('Ctrl Pts',(-8.69187643515535,31.1301114048208,26.2627342707168));
#47434=CARTESIAN_POINT('Ctrl Pts',(-8.80447715651746,31.0920494158489,26.2569106770561));
#47435=CARTESIAN_POINT('Ctrl Pts',(-8.9189220472593,31.0588445806593,26.2510870833955));
#47436=CARTESIAN_POINT('Ctrl Pts',(-9.0347545088317,31.0306768660414,26.2452634897348));
#47437=CARTESIAN_POINT('Ctrl Pts',(-9.15044083054925,31.0025446891792,26.2394472434025));
#47438=CARTESIAN_POINT('Ctrl Pts',(-9.26751084786546,30.9794370884277,26.2336309970703));
#47439=CARTESIAN_POINT('Ctrl Pts',(-9.38549053967956,30.9614850349198,26.227814750738));
#47440=CARTESIAN_POINT('Ctrl Pts',(-9.50335213317253,30.9435509515163,26.2220043265003));
#47441=CARTESIAN_POINT('Ctrl Pts',(-9.62212118828901,30.9307622097943,26.2161939022626));
#47442=CARTESIAN_POINT('Ctrl Pts',(-9.74131174706777,30.9231991233573,26.210383478025));
#47443=CARTESIAN_POINT('Ctrl Pts',(-9.86501391533451,30.9153497584358,26.2043531171968));
#47444=CARTESIAN_POINT('Ctrl Pts',(-9.98916969179079,30.9131295749646,26.1983227563686));
#47445=CARTESIAN_POINT('Ctrl Pts',(-10.1132274744092,30.9165695133823,26.1922923955404));
#47446=CARTESIAN_POINT('Ctrl Pts',(-10.2326261352478,30.9198802612593,26.1864885113176));
#47447=CARTESIAN_POINT('Ctrl Pts',(-10.3519335851551,30.9284336418294,26.1806846270947));
#47448=CARTESIAN_POINT('Ctrl Pts',(-10.4706569195293,30.942204161851,26.1748807428719));
#47449=CARTESIAN_POINT('Ctrl Pts',(-10.5893627171996,30.9559726478198,26.1690777159447));
#47450=CARTESIAN_POINT('Ctrl Pts',(-10.7074841654126,30.9749566936718,26.1632746890175));
#47451=CARTESIAN_POINT('Ctrl Pts',(-10.8245336381355,30.9990789460947,26.1574716620903));
#47452=CARTESIAN_POINT('Ctrl Pts',(-10.9415934451055,31.0232033282607,26.1516681228164));
#47453=CARTESIAN_POINT('Ctrl Pts',(-11.0575806884576,31.0524667365388,26.1458645835425));
#47454=CARTESIAN_POINT('Ctrl Pts',(-11.1720187213321,31.0867408574377,26.1400610442686));
#47455=CARTESIAN_POINT('Ctrl Pts',(-11.2864938651288,31.1210260930353,26.1342556229745));
#47456=CARTESIAN_POINT('Ctrl Pts',(-11.3994184083371,31.1603251557496,26.1284502016803));
#47457=CARTESIAN_POINT('Ctrl Pts',(-11.5103322443192,31.2044603135035,26.1226447803862));
#47458=CARTESIAN_POINT('Ctrl Pts',(-11.6213689071137,31.2486443468616,26.116832930125));
#47459=CARTESIAN_POINT('Ctrl Pts',(-11.730390038426,31.2976750142891,26.1110210798638));
#47460=CARTESIAN_POINT('Ctrl Pts',(-11.8369567081233,31.3513269463433,26.1052092296027));
#47461=CARTESIAN_POINT('Ctrl Pts',(-11.9435933713841,31.4050141172758,26.0993935620869));
#47462=CARTESIAN_POINT('Ctrl Pts',(-12.0477720069898,31.4633283986657,26.0935778945711));
#47463=CARTESIAN_POINT('Ctrl Pts',(-12.1490808715335,31.5259999413344,26.0877622270554));
#47464=CARTESIAN_POINT('Ctrl Pts',(-12.2505348500914,31.5887612542238,26.0819382292236));
#47465=CARTESIAN_POINT('Ctrl Pts',(-12.3491105166702,31.6558920566716,26.0761142313918));
#47466=CARTESIAN_POINT('Ctrl Pts',(-12.4444274065974,31.7270808665848,26.07029023356));
#47467=CARTESIAN_POINT('Ctrl Pts',(-12.4697154986905,31.7459676471171,26.0687450950895));
#47468=CARTESIAN_POINT('Ctrl Pts',(-12.4947744094078,31.7651398506132,26.0671999566189));
#47469=CARTESIAN_POINT('Ctrl Pts',(-12.5195974652219,31.7845912214389,26.0656548181484));
#47470=CARTESIAN_POINT('Ctrl Pts',(-12.6121091278205,31.8570834507757,26.0598963277382));
#47471=CARTESIAN_POINT('Ctrl Pts',(-12.7016553977115,31.9337015217862,26.054137837328));
#47472=CARTESIAN_POINT('Ctrl Pts',(-12.7878402403027,32.014171506173,26.0483793469178));
#47473=CARTESIAN_POINT('Ctrl Pts',(-12.8739158143967,32.0945394675823,26.0426281573459));
#47474=CARTESIAN_POINT('Ctrl Pts',(-12.9566381307581,32.1787493506631,26.0368769677739));
#47475=CARTESIAN_POINT('Ctrl Pts',(-13.0356421573526,32.2664854687594,26.031125778202));
#47476=CARTESIAN_POINT('Ctrl Pts',(-13.1145677909222,32.3541345292716,26.025380295341));
#47477=CARTESIAN_POINT('Ctrl Pts',(-13.1897821930166,32.4453025579342,26.0196348124801));
#47478=CARTESIAN_POINT('Ctrl Pts',(-13.260955868785,32.5396358355242,26.0138893296191));
#47479=CARTESIAN_POINT('Ctrl Pts',(-13.3320794864054,32.6339027662645,26.0081478876936));
#47480=CARTESIAN_POINT('Ctrl Pts',(-13.3991677787573,32.7313301853019,26.0024064457681));
#47481=CARTESIAN_POINT('Ctrl Pts',(-13.4619308537017,32.8315305480159,25.9966650038427));
#47482=CARTESIAN_POINT('Ctrl Pts',(-13.5246713353043,32.931694840779,25.9909256287114));
#47483=CARTESIAN_POINT('Ctrl Pts',(-13.5830894723143,33.0346297389846,25.9851862535801));
#47484=CARTESIAN_POINT('Ctrl Pts',(-13.6369384953871,33.139918447817,25.9794468784488));
#47485=CARTESIAN_POINT('Ctrl Pts',(-13.6907815551914,33.2451954969237,25.9737081388989));
#47486=CARTESIAN_POINT('Ctrl Pts',(-13.7400563170462,33.3528254656153,25.967969399349));
#47487=CARTESIAN_POINT('Ctrl Pts',(-13.784562181292,33.4623673728961,25.962230659799));
#47488=CARTESIAN_POINT('Ctrl Pts',(-13.8290742097634,33.5719244521334,25.9564911254126));
#47489=CARTESIAN_POINT('Ctrl Pts',(-13.8688158713915,33.6833936081926,25.9507515910262));
#47490=CARTESIAN_POINT('Ctrl Pts',(-13.903635172702,33.7963150584794,25.9450120566397));
#47491=CARTESIAN_POINT('Ctrl Pts',(-13.9384862376441,33.9093395204637,25.9392672864086));
#47492=CARTESIAN_POINT('Ctrl Pts',(-13.9684058548559,34.0238185210516,25.9335225161774));
#47493=CARTESIAN_POINT('Ctrl Pts',(-13.9932922830984,34.1392783598938,25.9277777459462));
#47494=CARTESIAN_POINT('Ctrl Pts',(-14.0181915929126,34.2547979624027,25.9220300021397));
#47495=CARTESIAN_POINT('Ctrl Pts',(-14.0380524566273,34.3712990019251,25.9162822583331));
#47496=CARTESIAN_POINT('Ctrl Pts',(-14.0528247789693,34.4883005657883,25.9105345145266));
#47497=CARTESIAN_POINT('Ctrl Pts',(-14.0676173085825,34.6054621777655,25.904778908299));
#47498=CARTESIAN_POINT('Ctrl Pts',(-14.0773073680087,34.7231252646438,25.8990233020715));
#47499=CARTESIAN_POINT('Ctrl Pts',(-14.0818969247286,34.8408067341535,25.8932676958439));
#47500=CARTESIAN_POINT('Ctrl Pts',(-14.0839921694519,34.8945311988609,25.8906401210445));
#47501=CARTESIAN_POINT('Ctrl Pts',(-14.0850251129975,34.948259530738,25.8880125462451));
#47502=CARTESIAN_POINT('Ctrl Pts',(-14.0849995364304,35.0019461149621,25.8853849714457));
#47503=CARTESIAN_POINT('Ctrl Pts',(-14.08499953643,35.0019461158033,25.8853849714045));
#47504=CARTESIAN_POINT('Ctrl Pts',(-14.0849449953633,35.1164306865273,25.879781769463));
#47505=CARTESIAN_POINT('Ctrl Pts',(-14.080078085778,35.2307950929958,25.8741785675215));
#47506=CARTESIAN_POINT('Ctrl Pts',(-14.0704266820106,35.3447486423126,25.8685753655799));
#47507=CARTESIAN_POINT('Ctrl Pts',(-14.0603956578548,35.4631843469393,25.8627517718956));
#47508=CARTESIAN_POINT('Ctrl Pts',(-14.0451750474133,35.5813728710574,25.8569281782112));
#47509=CARTESIAN_POINT('Ctrl Pts',(-14.0247820306547,35.6988237300772,25.8511045845269));
#47510=CARTESIAN_POINT('Ctrl Pts',(-14.0044147427152,35.8161264073961,25.8452883381708));
#47511=CARTESIAN_POINT('Ctrl Pts',(-13.9788880972782,35.9326928719345,25.8394720918147));
#47512=CARTESIAN_POINT('Ctrl Pts',(-13.9482711523926,36.048036214634,25.8336558454586));
#47513=CARTESIAN_POINT('Ctrl Pts',(-13.9176848552369,36.1632640980144,25.827845421197));
#47514=CARTESIAN_POINT('Ctrl Pts',(-13.8820184994948,36.2772709028511,25.8220349969355));
#47515=CARTESIAN_POINT('Ctrl Pts',(-13.8413923561535,36.3895789887896,25.8162245726739));
#47516=CARTESIAN_POINT('Ctrl Pts',(-13.7992284293876,36.5061381677141,25.8101942118546));
#47517=CARTESIAN_POINT('Ctrl Pts',(-13.7517218964731,36.6208670451566,25.8041638510354));
#47518=CARTESIAN_POINT('Ctrl Pts',(-13.6990644946204,36.733247490879,25.7981334902161));
#47519=CARTESIAN_POINT('Ctrl Pts',(-13.6483846971346,36.841407370216,25.7923296059694));
#47520=CARTESIAN_POINT('Ctrl Pts',(-13.5929341350882,36.9473916294299,25.7865257217226));
#47521=CARTESIAN_POINT('Ctrl Pts',(-13.5329328695572,37.0507584790028,25.7807218374759));
#47522=CARTESIAN_POINT('Ctrl Pts',(-13.472940466854,37.154110060188,25.7749188105248));
#47523=CARTESIAN_POINT('Ctrl Pts',(-13.4083989023735,37.2548446475391,25.7691157835738));
#47524=CARTESIAN_POINT('Ctrl Pts',(-13.3395736832524,37.3525459855501,25.7633127566227));
#47525=CARTESIAN_POINT('Ctrl Pts',(-13.2707423875834,37.4502559495688,25.757509217325));
#47526=CARTESIAN_POINT('Ctrl Pts',(-13.1976269204893,37.5449317979474,25.7517056780273));
#47527=CARTESIAN_POINT('Ctrl Pts',(-13.1205351352935,37.6361876771957,25.7459021387296));
#47528=CARTESIAN_POINT('Ctrl Pts',(-13.0434183501301,37.7274731496623,25.7400967174117));
#47529=CARTESIAN_POINT('Ctrl Pts',(-12.9623229457708,37.8153361355679,25.7342912960938));
#47530=CARTESIAN_POINT('Ctrl Pts',(-12.8775954891384,37.8994256674194,25.7284858747759));
#47531=CARTESIAN_POINT('Ctrl Pts',(-12.7927742046902,37.983608320644,25.7226740244913));
#47532=CARTESIAN_POINT('Ctrl Pts',(-12.7043131293883,38.0640088908545,25.7168621742066));
#47533=CARTESIAN_POINT('Ctrl Pts',(-12.6125940604571,38.1403148369653,25.711050323922));
#47534=CARTESIAN_POINT('Ctrl Pts',(-12.5208147499488,38.2166709012313,25.7052346563829));
#47535=CARTESIAN_POINT('Ctrl Pts',(-12.4257735085254,38.2889267388844,25.6994189888437));
#47536=CARTESIAN_POINT('Ctrl Pts',(-12.3278820700889,38.3568124862373,25.6936033213046));
#47537=CARTESIAN_POINT('Ctrl Pts',(-12.2298504127388,38.4247954725918,25.6877793234498));
#47538=CARTESIAN_POINT('Ctrl Pts',(-12.1289607539321,38.488395657677,25.681955325595));
#47539=CARTESIAN_POINT('Ctrl Pts',(-12.0256505210465,38.5473884713383,25.6761313277402));
#47540=CARTESIAN_POINT('Ctrl Pts',(-11.9982417555052,38.5630395850093,25.6745861894973));
#47541=CARTESIAN_POINT('Ctrl Pts',(-11.9706627263306,38.5783666607387,25.6730410512544));
#47542=CARTESIAN_POINT('Ctrl Pts',(-11.942921832498,38.5933660755346,25.6714959130115));
#47543=CARTESIAN_POINT('Ctrl Pts',(-11.8383669847759,38.6498985556834,25.6656723193424));
#47544=CARTESIAN_POINT('Ctrl Pts',(-11.7311741295247,38.7019551202848,25.6598487256734));
#47545=CARTESIAN_POINT('Ctrl Pts',(-11.6217629113322,38.7492812723811,25.6540251320044));
#47546=CARTESIAN_POINT('Ctrl Pts',(-11.5124897316433,38.7965477155066,25.6482088856638));
#47547=CARTESIAN_POINT('Ctrl Pts',(-11.4010041272243,38.8390954558911,25.6423926393232));
#47548=CARTESIAN_POINT('Ctrl Pts',(-11.287751189866,38.8767153458822,25.6365763929827));
#47549=CARTESIAN_POINT('Ctrl Pts',(-11.1746116193231,38.9142975781558,25.6307659687368));
#47550=CARTESIAN_POINT('Ctrl Pts',(-11.0597086205557,38.9469616452577,25.6249555444909));
#47551=CARTESIAN_POINT('Ctrl Pts',(-10.9435076063458,38.9745463133253,25.619145120245));
#47552=CARTESIAN_POINT('Ctrl Pts',(-10.8229081433339,39.0031751181505,25.6131147594199));
#47553=CARTESIAN_POINT('Ctrl Pts',(-10.7009108695603,39.026332216735,25.6070843985948));
#47554=CARTESIAN_POINT('Ctrl Pts',(-10.5780542375637,39.0438939524219,25.6010540377697));
#47555=CARTESIAN_POINT('Ctrl Pts',(-10.4598116166367,39.0607961385059,25.5952501535389));
#47556=CARTESIAN_POINT('Ctrl Pts',(-10.3407734622352,39.0725155990886,25.5894462693081));
#47557=CARTESIAN_POINT('Ctrl Pts',(-10.2214299038287,39.078994213981,25.5836423850773));
#47558=CARTESIAN_POINT('Ctrl Pts',(-10.1021039737419,39.0854718719127,25.5778393581423));
#47559=CARTESIAN_POINT('Ctrl Pts',(-9.98247313698898,39.0867102015237,25.5720363312073));
#47560=CARTESIAN_POINT('Ctrl Pts',(-9.86303107900381,39.0827030892144,25.5662333042722));
#47561=CARTESIAN_POINT('Ctrl Pts',(-9.74357847553385,39.0786956231191,25.5604297649906));
#47562=CARTESIAN_POINT('Ctrl Pts',(-9.62431509209752,39.0694418080057,25.554626225709));
#47563=CARTESIAN_POINT('Ctrl Pts',(-9.50573239939709,39.0549876126807,25.5488226864273));
#47564=CARTESIAN_POINT('Ctrl Pts',(-9.38711125171189,39.0405287300287,25.5430172651256));
#47565=CARTESIAN_POINT('Ctrl Pts',(-9.26917163889313,39.0208661626327,25.5372118438238));
#47566=CARTESIAN_POINT('Ctrl Pts',(-9.15239707538665,38.9960973814694,25.5314064225221));
#47567=CARTESIAN_POINT('Ctrl Pts',(-9.03549319485917,38.9713011711736,25.5255945722535));
#47568=CARTESIAN_POINT('Ctrl Pts',(-8.91975733864937,38.9413875447034,25.519782721985));
#47569=CARTESIAN_POINT('Ctrl Pts',(-8.80566019443292,38.9065045026005,25.5139708717165));
#47570=CARTESIAN_POINT('Ctrl Pts',(-8.69148811059923,38.8715985491282,25.5081552041935));
#47571=CARTESIAN_POINT('Ctrl Pts',(-8.57895726626273,38.8317168158974,25.5023395366704));
#47572=CARTESIAN_POINT('Ctrl Pts',(-8.46851906515115,38.7870557358183,25.4965238691474));
#47573=CARTESIAN_POINT('Ctrl Pts',(-8.357922673241,38.7423306835643,25.4906998713086));
#47574=CARTESIAN_POINT('Ctrl Pts',(-8.24942527753198,38.6928127893603,25.4848758734699));
#47575=CARTESIAN_POINT('Ctrl Pts',(-8.14345448377524,38.6387448036632,25.4790518756311));
#47576=CARTESIAN_POINT('Ctrl Pts',(-8.11533985413041,38.6244002721217,25.477506737235));
#47577=CARTESIAN_POINT('Ctrl Pts',(-8.0874029081827,38.6097357111295,25.475961598839));
#47578=CARTESIAN_POINT('Ctrl Pts',(-8.0596512801125,38.5947561593564,25.474416460443));
#47579=CARTESIAN_POINT('Ctrl Pts',(-7.95507361048059,38.5383080615151,25.4685938480793));
#47580=CARTESIAN_POINT('Ctrl Pts',(-7.85279263304946,38.477201648066,25.4627712357156));
#47581=CARTESIAN_POINT('Ctrl Pts',(-7.75325101345552,38.4116482807378,25.4569486233519));
#47582=CARTESIAN_POINT('Ctrl Pts',(-7.67116832542903,38.3575925337906,25.4521472580929));
#47583=CARTESIAN_POINT('Ctrl Pts',(-7.59094813059903,38.3005139010736,25.4473458928338));
#47584=CARTESIAN_POINT('Ctrl Pts',(-7.51282733495087,38.2405550657615,25.4425445275748));
#47585=CARTESIAN_POINT('',(-14.0849990113761,34.997157983738,25.9896150286377));
#47586=CARTESIAN_POINT('Ctrl Pts',(-14.0849990113767,34.9971579846073,25.9896150285955));
#47587=CARTESIAN_POINT('Ctrl Pts',(-14.0850823687406,35.1169725184056,25.9837992556083));
#47588=CARTESIAN_POINT('Ctrl Pts',(-14.0798901022421,35.2368329720402,25.9779834826211));
#47589=CARTESIAN_POINT('Ctrl Pts',(-14.0694367788927,35.3562433193698,25.9721677096339));
#47590=CARTESIAN_POINT('Ctrl Pts',(-14.0589841763782,35.4756454324611,25.9663523376878));
#47591=CARTESIAN_POINT('Ctrl Pts',(-14.0432712735987,35.5945970970668,25.9605369657417));
#47592=CARTESIAN_POINT('Ctrl Pts',(-14.0223646062367,35.7126064653753,25.9547215937957));
#47593=CARTESIAN_POINT('Ctrl Pts',(-14.0014545368501,35.8306350366852,25.9489052755468));
#47594=CARTESIAN_POINT('Ctrl Pts',(-13.9753490922683,35.9477206074002,25.9430889572979));
#47595=CARTESIAN_POINT('Ctrl Pts',(-13.9441660016536,36.0633811881917,25.937272639049));
#47596=CARTESIAN_POINT('Ctrl Pts',(-13.9129706122599,36.1790873861394,25.9314540268129));
#47597=CARTESIAN_POINT('Ctrl Pts',(-13.8766936982003,36.2933670848564,25.9256354145768));
#47598=CARTESIAN_POINT('Ctrl Pts',(-13.8355027712538,36.4057537094756,25.9198168023407));
#47599=CARTESIAN_POINT('Ctrl Pts',(-13.7942616422284,36.5182773070305,25.9139910985809));
#47600=CARTESIAN_POINT('Ctrl Pts',(-13.7480946838436,36.6289028436099,25.9081653948212));
#47601=CARTESIAN_POINT('Ctrl Pts',(-13.6972175586699,36.7371837334787,25.9023396910615));
#47602=CARTESIAN_POINT('Ctrl Pts',(-13.6463043683703,36.8455413801202,25.8965098576514));
#47603=CARTESIAN_POINT('Ctrl Pts',(-13.5906745491849,36.9515507116461,25.8906800242413));
#47604=CARTESIAN_POINT('Ctrl Pts',(-13.5305888844153,37.0547912617206,25.8848501908312));
#47605=CARTESIAN_POINT('Ctrl Pts',(-13.4704104787615,37.1581911612827,25.8790113592032));
#47606=CARTESIAN_POINT('Ctrl Pts',(-13.4057627161401,37.2588134079781,25.8731725275752));
#47607=CARTESIAN_POINT('Ctrl Pts',(-13.3369488313703,37.3562677048282,25.8673336959472));
#47608=CARTESIAN_POINT('Ctrl Pts',(-13.3133690744641,37.3896613816549,25.8653329626524));
#47609=CARTESIAN_POINT('Ctrl Pts',(-13.2893004869571,37.4226833896288,25.8633322293576));
#47610=CARTESIAN_POINT('Ctrl Pts',(-13.2647562933781,37.4553189904467,25.8613314960627));
#47611=CARTESIAN_POINT('Ctrl Pts',(-13.1933147821562,37.5503124003773,25.8555079024021));
#47612=CARTESIAN_POINT('Ctrl Pts',(-13.1176086426081,37.6423383452609,25.8496843087414));
#47613=CARTESIAN_POINT('Ctrl Pts',(-13.0379131029223,37.7309904758334,25.8438607150807));
#47614=CARTESIAN_POINT('Ctrl Pts',(-12.958318110997,37.8195307585757,25.8380444687484));
#47615=CARTESIAN_POINT('Ctrl Pts',(-12.8747440004759,37.9047053922272,25.8322282224161));
#47616=CARTESIAN_POINT('Ctrl Pts',(-12.7875080441765,37.986138627668,25.8264119760838));
#47617=CARTESIAN_POINT('Ctrl Pts',(-12.7003594115499,38.0674903479917,25.8206015518461));
#47618=CARTESIAN_POINT('Ctrl Pts',(-12.6095565220376,38.1451078435993,25.8147911276084));
#47619=CARTESIAN_POINT('Ctrl Pts',(-12.5154551039352,38.21865043459,25.8089807033707));
#47620=CARTESIAN_POINT('Ctrl Pts',(-12.4177917522782,38.2949767649528,25.8029503425425));
#47621=CARTESIAN_POINT('Ctrl Pts',(-12.3165755254885,38.3669132749912,25.7969199817143));
#47622=CARTESIAN_POINT('Ctrl Pts',(-12.2122442084511,38.4341229684119,25.7908896208861));
#47623=CARTESIAN_POINT('Ctrl Pts',(-12.1118311648279,38.4988085304176,25.7850857366633));
#47624=CARTESIAN_POINT('Ctrl Pts',(-12.0085331665974,38.5591156733134,25.7792818524404));
#47625=CARTESIAN_POINT('Ctrl Pts',(-11.9027714188067,38.6147871206715,25.7734779682176));
#47626=CARTESIAN_POINT('Ctrl Pts',(-11.7970252931551,38.6704503447625,25.7676749412904));
#47627=CARTESIAN_POINT('Ctrl Pts',(-11.6888165029063,38.7214790449011,25.7618719143631));
#47628=CARTESIAN_POINT('Ctrl Pts',(-11.5785911791359,38.7676617270071,25.7560688874359));
#47629=CARTESIAN_POINT('Ctrl Pts',(-11.4683561236196,38.813848486562,25.750265348162));
#47630=CARTESIAN_POINT('Ctrl Pts',(-11.3561045572319,38.8551882196057,25.7444618088881));
#47631=CARTESIAN_POINT('Ctrl Pts',(-11.2423023240607,38.8915176905204,25.7386582696141));
#47632=CARTESIAN_POINT('Ctrl Pts',(-11.1284631861493,38.9278589426599,25.7328528483199));
#47633=CARTESIAN_POINT('Ctrl Pts',(-11.0130727701695,38.9591865772534,25.7270474270257));
#47634=CARTESIAN_POINT('Ctrl Pts',(-10.8966111730493,38.9853874848455,25.7212420057315));
#47635=CARTESIAN_POINT('Ctrl Pts',(-10.7800206054849,39.0116174075187,25.7154301554704));
#47636=CARTESIAN_POINT('Ctrl Pts',(-10.6623568875714,39.0327091809837,25.7096183052092));
#47637=CARTESIAN_POINT('Ctrl Pts',(-10.5441095368408,39.0486009697078,25.703806454948));
#47638=CARTESIAN_POINT('Ctrl Pts',(-10.4257845206125,39.0645031962444,25.6979907874322));
#47639=CARTESIAN_POINT('Ctrl Pts',(-10.3068755139097,39.0751985997321,25.6921751199164));
#47640=CARTESIAN_POINT('Ctrl Pts',(-10.1878747114908,39.0806774061156,25.6863594524006));
#47641=CARTESIAN_POINT('Ctrl Pts',(-10.0687034532662,39.0861640602979,25.6805354545688));
#47642=CARTESIAN_POINT('Ctrl Pts',(-9.94944054377033,39.0864192023761,25.674711456737));
#47643=CARTESIAN_POINT('Ctrl Pts',(-9.83057587027134,39.0814850807354,25.6688874589052));
#47644=CARTESIAN_POINT('Ctrl Pts',(-9.79904042244212,39.0801760312844,25.6673423204349));
#47645=CARTESIAN_POINT('Ctrl Pts',(-9.76753296247365,39.0785020064223,25.6657971819646));
#47646=CARTESIAN_POINT('Ctrl Pts',(-9.73606253046936,39.0764644009457,25.6642520434943));
#47647=CARTESIAN_POINT('Ctrl Pts',(-9.61746471748885,39.0687855882367,25.6584291160142));
#47648=CARTESIAN_POINT('Ctrl Pts',(-9.49901105976693,39.0559144963217,25.652606188534));
#47649=CARTESIAN_POINT('Ctrl Pts',(-9.38119211768221,39.0378585667135,25.6467832610539));
#47650=CARTESIAN_POINT('Ctrl Pts',(-9.26351389264308,39.0198242022036,25.6409672881868));
#47651=CARTESIAN_POINT('Ctrl Pts',(-9.14646927575777,38.9966173744826,25.6351513153197));
#47652=CARTESIAN_POINT('Ctrl Pts',(-9.03054638182726,38.9682974538474,25.6293353424526));
#47653=CARTESIAN_POINT('Ctrl Pts',(-8.91473456847413,38.9400046701566,25.6235249426143));
#47654=CARTESIAN_POINT('Ctrl Pts',(-8.80004273458407,38.9066086345948,25.617714542776));
#47655=CARTESIAN_POINT('Ctrl Pts',(-8.68695080785641,38.8682201099486,25.6119041429377));
#47656=CARTESIAN_POINT('Ctrl Pts',(-8.57394311497465,38.8298601780868,25.6060980708383));
#47657=CARTESIAN_POINT('Ctrl Pts',(-8.46253334329489,38.7865152875142,25.6002919987388));
#47658=CARTESIAN_POINT('Ctrl Pts',(-8.35318755706752,38.7383463961761,25.5944859266393));
#47659=CARTESIAN_POINT('Ctrl Pts',(-8.24389061310108,38.6901990207797,25.5886824479795));
#47660=CARTESIAN_POINT('Ctrl Pts',(-8.13665619313469,38.6372320964834,25.5828789693196));
#47661=CARTESIAN_POINT('Ctrl Pts',(-8.03193111003031,38.5796549895672,25.5770754906597));
#47662=CARTESIAN_POINT('Ctrl Pts',(-7.92720867012837,38.522079335865,25.5712721584763));
#47663=CARTESIAN_POINT('Ctrl Pts',(-7.82499580309165,38.4598939198369,25.565468826293));
#47664=CARTESIAN_POINT('Ctrl Pts',(-7.72571506549868,38.3933542456838,25.5596654941096));
#47665=CARTESIAN_POINT('Ctrl Pts',(-7.6531341096041,38.3447092288151,25.5554228644974));
#47666=CARTESIAN_POINT('Ctrl Pts',(-7.58211977490954,38.2937380109861,25.5511802348851));
#47667=CARTESIAN_POINT('Ctrl Pts',(-7.51282733495086,38.2405550657615,25.5469376052728));
#47668=CARTESIAN_POINT('Ctrl Pts',(-7.51282733495086,38.2405550657615,26.7967727135811));
#47669=CARTESIAN_POINT('Ctrl Pts',(-7.41816743920586,38.1679022330228,26.7909660918651));
#47670=CARTESIAN_POINT('Ctrl Pts',(-7.3266191318822,38.0910411499093,26.7851594701491));
#47671=CARTESIAN_POINT('Ctrl Pts',(-7.23857267566336,38.0102730993063,26.7793528484331));
#47672=CARTESIAN_POINT('Ctrl Pts',(-7.15056331236747,37.9295390753206,26.7735486729777));
#47673=CARTESIAN_POINT('Ctrl Pts',(-7.06605316749299,37.8449016317536,26.7677444975222));
#47674=CARTESIAN_POINT('Ctrl Pts',(-6.98539889507687,37.7567018660342,26.7619403220667));
#47675=CARTESIAN_POINT('Ctrl Pts',(-6.90475988744046,37.6685187931688,26.7561372451205));
#47676=CARTESIAN_POINT('Ctrl Pts',(-6.82797557649666,37.5767750400944,26.7503341681742));
#47677=CARTESIAN_POINT('Ctrl Pts',(-6.75536479151172,37.4818475706292,26.744531091228));
#47678=CARTESIAN_POINT('Ctrl Pts',(-6.6827506127708,37.3869156643484,26.7387277430516));
#47679=CARTESIAN_POINT('Ctrl Pts',(-6.61431059584699,37.2888000702335,26.7329243948753));
#47680=CARTESIAN_POINT('Ctrl Pts',(-6.55032200867168,37.1879092202706,26.727121046699));
#47681=CARTESIAN_POINT('Ctrl Pts',(-6.48631532947053,37.0869898445979,26.7213160576938));
#47682=CARTESIAN_POINT('Ctrl Pts',(-6.42676280162494,36.9832939972967,26.7155110686885));
#47683=CARTESIAN_POINT('Ctrl Pts',(-6.3718969191612,36.8772567844618,26.7097060796833));
#47684=CARTESIAN_POINT('Ctrl Pts',(-6.31697134521963,36.7711042081688,26.7038947751253));
#47685=CARTESIAN_POINT('Ctrl Pts',(-6.26674278408351,36.6626055438139,26.6980834705674));
#47686=CARTESIAN_POINT('Ctrl Pts',(-6.22139661147764,36.5522182295822,26.6922721660094));
#47687=CARTESIAN_POINT('Ctrl Pts',(-6.17602234506711,36.4417625259041,26.6864572611111));
#47688=CARTESIAN_POINT('Ctrl Pts',(-6.13553663004733,36.3294162253693,26.6806423562128));
#47689=CARTESIAN_POINT('Ctrl Pts',(-6.10007521054347,36.2156527615164,26.6748274513145));
#47690=CARTESIAN_POINT('Ctrl Pts',(-6.06456131784517,36.1017209588761,26.6690039419486));
#47691=CARTESIAN_POINT('Ctrl Pts',(-6.03408666856618,35.9863681999291,26.6631804325827));
#47692=CARTESIAN_POINT('Ctrl Pts',(-6.00873614398522,35.8700792099976,26.6573569232168));
#47693=CARTESIAN_POINT('Ctrl Pts',(-5.99755204410615,35.8187750378067,26.65478771759));
#47694=CARTESIAN_POINT('Ctrl Pts',(-5.98736461721418,35.7672887225753,26.6522185119633));
#47695=CARTESIAN_POINT('Ctrl Pts',(-5.97817793785381,35.7156621412609,26.6496493063365));
#47696=CARTESIAN_POINT('Ctrl Pts',(-5.95735457763845,35.5986406520781,26.643825711963));
#47697=CARTESIAN_POINT('Ctrl Pts',(-5.94160927486657,35.4805208685255,26.6380021175896));
#47698=CARTESIAN_POINT('Ctrl Pts',(-5.93105180597031,35.3617811414413,26.6321785232162));
#47699=CARTESIAN_POINT('Ctrl Pts',(-5.92050765687337,35.2431912219815,26.6263622761633));
#47700=CARTESIAN_POINT('Ctrl Pts',(-5.91513835921745,35.123983317815,26.6205460291104));
#47701=CARTESIAN_POINT('Ctrl Pts',(-5.91500264167174,35.0046456916703,26.6147297820576));
#47702=CARTESIAN_POINT('Ctrl Pts',(-5.91486705997985,34.8854275229902,26.6089193570924));
#47703=CARTESIAN_POINT('Ctrl Pts',(-5.91995463684506,34.7660802966464,26.6031089321272));
#47704=CARTESIAN_POINT('Ctrl Pts',(-5.93027222897837,34.647096514929,26.5972985071621));
#47705=CARTESIAN_POINT('Ctrl Pts',(-5.94098036152084,34.523608971656,26.591268146604));
#47706=CARTESIAN_POINT('Ctrl Pts',(-5.95732230395538,34.4005133772377,26.5852377860459));
#47707=CARTESIAN_POINT('Ctrl Pts',(-5.97924629220264,34.2783597702222,26.5792074254878));
#47708=CARTESIAN_POINT('Ctrl Pts',(-6.00034690542287,34.1607937513929,26.5734035405249));
#47709=CARTESIAN_POINT('Ctrl Pts',(-6.02661776946005,34.0441006796139,26.567599655562));
#47710=CARTESIAN_POINT('Ctrl Pts',(-6.05796008300251,33.9287641283086,26.5617957705992));
#47711=CARTESIAN_POINT('Ctrl Pts',(-6.08929776696935,33.8134446133744,26.5559927429286));
#47712=CARTESIAN_POINT('Ctrl Pts',(-6.12570530365791,33.6994816143779,26.550189715258));
#47713=CARTESIAN_POINT('Ctrl Pts',(-6.16703340111029,33.5873457423007,26.5443866875875));
#47714=CARTESIAN_POINT('Ctrl Pts',(-6.20836514741999,33.4751999697485,26.5385831475676));
#47715=CARTESIAN_POINT('Ctrl Pts',(-6.25461817704179,33.3648820280153,26.5327796075478));
#47716=CARTESIAN_POINT('Ctrl Pts',(-6.30559444831266,33.2568440632973,26.526976067528));
#47717=CARTESIAN_POINT('Ctrl Pts',(-6.35658725060838,33.1487710630965,26.5211706454861));
#47718=CARTESIAN_POINT('Ctrl Pts',(-6.41230616658958,33.0429798794551,26.5153652234443));
#47719=CARTESIAN_POINT('Ctrl Pts',(-6.47250675950058,32.9398989252391,26.5095598014025));
#47720=CARTESIAN_POINT('Ctrl Pts',(-6.53277401897794,32.8367038184386,26.5037479503948));
#47721=CARTESIAN_POINT('Ctrl Pts',(-6.59753265599006,32.7362252847876,26.4979360993872));
#47722=CARTESIAN_POINT('Ctrl Pts',(-6.66649429216926,32.6388636854557,26.4921242483795));
#47723=CARTESIAN_POINT('Ctrl Pts',(-6.73550122271972,32.5414381385049,26.4863085801171));
#47724=CARTESIAN_POINT('Ctrl Pts',(-6.80871640031047,32.4471339247615,26.4804929118546));
#47725=CARTESIAN_POINT('Ctrl Pts',(-6.88581152455996,32.356317882302,26.4746772435922));
#47726=CARTESIAN_POINT('Ctrl Pts',(-6.96301707916817,32.2653717557645,26.4688532450191));
#47727=CARTESIAN_POINT('Ctrl Pts',(-7.04411339642909,32.1779240714469,26.463029246446));
#47728=CARTESIAN_POINT('Ctrl Pts',(-7.12873567982069,32.0943045232397,26.4572052478729));
#47729=CARTESIAN_POINT('Ctrl Pts',(-7.15118632826877,32.0721199046624,26.4556601165046));
#47730=CARTESIAN_POINT('Ctrl Pts',(-7.17388497986136,32.0502045115405,26.4541149851363));
#47731=CARTESIAN_POINT('Ctrl Pts',(-7.196824452785,32.0285640085144,26.452569853768));
#47732=CARTESIAN_POINT('Ctrl Pts',(-7.28328323015379,31.9470010432489,26.4467462601125));
#47733=CARTESIAN_POINT('Ctrl Pts',(-7.37344419471702,31.8690831724474,26.4409226664571));
#47734=CARTESIAN_POINT('Ctrl Pts',(-7.46696744322747,31.795164424447,26.4350990728016));
#47735=CARTESIAN_POINT('Ctrl Pts',(-7.56037269829168,31.7213389359083,26.429282826473));
#47736=CARTESIAN_POINT('Ctrl Pts',(-7.65713148249352,31.6515027857869,26.4234665801445));
#47737=CARTESIAN_POINT('Ctrl Pts',(-7.75686762003372,31.5859727408899,26.417650333816));
#47738=CARTESIAN_POINT('Ctrl Pts',(-7.85650392117553,31.5205082919126,26.4118399095807));
#47739=CARTESIAN_POINT('Ctrl Pts',(-7.95911130732079,31.4593415960198,26.4060294853453));
#47740=CARTESIAN_POINT('Ctrl Pts',(-8.06428162249677,31.4027483597896,26.40021906111));
#47741=CARTESIAN_POINT('Ctrl Pts',(-8.17343285197416,31.3440129523289,26.3941887002804));
#47742=CARTESIAN_POINT('Ctrl Pts',(-8.28534451679734,31.290204353265,26.3881583394508));
#47743=CARTESIAN_POINT('Ctrl Pts',(-8.39952820529889,31.2415807798536,26.3821279786212));
#47744=CARTESIAN_POINT('Ctrl Pts',(-8.50942360410989,31.1947833163823,26.3763240943971));
#47745=CARTESIAN_POINT('Ctrl Pts',(-8.62142303817242,31.1527886180174,26.370520210173));
#47746=CARTESIAN_POINT('Ctrl Pts',(-8.73506790146244,31.1157791275354,26.3647163259489));
#47747=CARTESIAN_POINT('Ctrl Pts',(-8.84869597821914,31.0787751037417,26.3589132990191));
#47748=CARTESIAN_POINT('Ctrl Pts',(-8.96396861269728,31.0467549498376,26.3531102720893));
#47749=CARTESIAN_POINT('Ctrl Pts',(-9.08041036314702,31.019851774143,26.3473072451596));
#47750=CARTESIAN_POINT('Ctrl Pts',(-9.19686239421507,30.9929462231726,26.3415037058817));
#47751=CARTESIAN_POINT('Ctrl Pts',(-9.31448334860745,30.9711586405803,26.3357001666039));
#47752=CARTESIAN_POINT('Ctrl Pts',(-9.43278650517214,30.9545712401174,26.3298966273261));
#47753=CARTESIAN_POINT('Ctrl Pts',(-9.551128026101,30.9379784605498,26.3240912060267));
#47754=CARTESIAN_POINT('Ctrl Pts',(-9.6701517850061,30.92658927357,26.3182857847272));
#47755=CARTESIAN_POINT('Ctrl Pts',(-9.78936547850621,30.9204340796655,26.3124803634278));
#47756=CARTESIAN_POINT('Ctrl Pts',(-9.90871119018325,30.914272069451,26.3066685131594));
#47757=CARTESIAN_POINT('Ctrl Pts',(-10.0282468482665,30.9133556430209,26.3008566628911));
#47758=CARTESIAN_POINT('Ctrl Pts',(-10.1474795238122,30.9176630724478,26.2950448126227));
#47759=CARTESIAN_POINT('Ctrl Pts',(-10.266790512046,30.9219733310185,26.2892291450985));
#47760=CARTESIAN_POINT('Ctrl Pts',(-10.3857977153321,30.9315142459272,26.2834134775744));
#47761=CARTESIAN_POINT('Ctrl Pts',(-10.5040143586819,30.9462123234878,26.2775978100502));
#47762=CARTESIAN_POINT('Ctrl Pts',(-10.6224003346473,30.9609314544622,26.2717738122084));
#47763=CARTESIAN_POINT('Ctrl Pts',(-10.7399930892949,30.9808224244376,26.2659498143666));
#47764=CARTESIAN_POINT('Ctrl Pts',(-10.8563169081083,31.0057608543193,26.2601258165248));
#47765=CARTESIAN_POINT('Ctrl Pts',(-10.8871782526725,31.0123771559962,26.2585806780831));
#47766=CARTESIAN_POINT('Ctrl Pts',(-10.9179503703238,31.0193484631904,26.2570355396413));
#47767=CARTESIAN_POINT('Ctrl Pts',(-10.9486245863916,31.0266718743485,26.2554904011996));
#47768=CARTESIAN_POINT('Ctrl Pts',(-11.0642350460018,31.0542736532507,26.2496668076964));
#47769=CARTESIAN_POINT('Ctrl Pts',(-11.1788262581777,31.0869699424238,26.2438432141931));
#47770=CARTESIAN_POINT('Ctrl Pts',(-11.2919158012722,31.1246705220816,26.2380196206899));
#47771=CARTESIAN_POINT('Ctrl Pts',(-11.4048626650515,31.1623235368387,26.2322033745179));
#47772=CARTESIAN_POINT('Ctrl Pts',(-11.5163112440597,31.2049681563606,26.2263871283459));
#47773=CARTESIAN_POINT('Ctrl Pts',(-11.6257903978218,31.2524633981307,26.2205708821739));
#47774=CARTESIAN_POINT('Ctrl Pts',(-11.7351599622947,31.299911096879,26.2147604580992));
#47775=CARTESIAN_POINT('Ctrl Pts',(-11.8425636509395,31.3521995968757,26.2089500340245));
#47776=CARTESIAN_POINT('Ctrl Pts',(-11.9475471345016,31.4091386605865,26.2031396099497));
#47777=CARTESIAN_POINT('Ctrl Pts',(-12.0565044644739,31.468232988023,26.1971092490615));
#47778=CARTESIAN_POINT('Ctrl Pts',(-12.1628543242716,31.5323367610234,26.1910788881732));
#47779=CARTESIAN_POINT('Ctrl Pts',(-12.2661130188982,31.6011830314681,26.1850485272849));
#47780=CARTESIAN_POINT('Ctrl Pts',(-12.3654937197075,31.6674437045248,26.1792446432306));
#47781=CARTESIAN_POINT('Ctrl Pts',(-12.4620108821194,31.7380968326876,26.1734407591764));
#47782=CARTESIAN_POINT('Ctrl Pts',(-12.5552605251456,31.812858859631,26.1676368751221));
#47783=CARTESIAN_POINT('Ctrl Pts',(-12.6484963941752,31.8876098434018,26.1618338483652));
#47784=CARTESIAN_POINT('Ctrl Pts',(-12.7384653851536,31.9664682636071,26.1560308216084));
#47785=CARTESIAN_POINT('Ctrl Pts',(-12.8247955502742,32.049109439652,26.1502277948515));
#47786=CARTESIAN_POINT('Ctrl Pts',(-12.9111333374235,32.1317579120274,26.1444242557496));
#47787=CARTESIAN_POINT('Ctrl Pts',(-12.9938313649679,32.2181895218882,26.1386207166476));
#47788=CARTESIAN_POINT('Ctrl Pts',(-13.0725540688902,32.3080422563223,26.1328171775457));
#47789=CARTESIAN_POINT('Ctrl Pts',(-13.1513023016507,32.3979241289314,26.1270117564249));
#47790=CARTESIAN_POINT('Ctrl Pts',(-13.2260723780103,32.4912290255449,26.1212063353041));
#47791=CARTESIAN_POINT('Ctrl Pts',(-13.2965690090939,32.5875618622892,26.1154009141833));
#47792=CARTESIAN_POINT('Ctrl Pts',(-13.3671437086616,32.6840013787204,26.1095890640968));
#47793=CARTESIAN_POINT('Ctrl Pts',(-13.4334352752984,32.7834751987622,26.1037772140103));
#47794=CARTESIAN_POINT('Ctrl Pts',(-13.4951916759194,32.8855591404383,26.0979653639237));
#47795=CARTESIAN_POINT('Ctrl Pts',(-13.5569886384688,32.9877101313838,26.0921496965835));
#47796=CARTESIAN_POINT('Ctrl Pts',(-13.6142443074278,33.0924743006253,26.0863340292433));
#47797=CARTESIAN_POINT('Ctrl Pts',(-13.6667533184719,33.1994042370718,26.0805183619031));
#47798=CARTESIAN_POINT('Ctrl Pts',(-13.7193375430087,33.3064873391147,26.0746943642469));
#47799=CARTESIAN_POINT('Ctrl Pts',(-13.7671613758866,33.4157420274988,26.0688703665907));
#47800=CARTESIAN_POINT('Ctrl Pts',(-13.8100680748157,33.5267022482641,26.0630463689346));
#47801=CARTESIAN_POINT('Ctrl Pts',(-13.8214514690128,33.5561406335206,26.0615012288334));
#47802=CARTESIAN_POINT('Ctrl Pts',(-13.8324890351497,33.5856989933228,26.0599560887323));
#47803=CARTESIAN_POINT('Ctrl Pts',(-13.843178444856,33.6153684818718,26.0584109486312));
#47804=CARTESIAN_POINT('Ctrl Pts',(-13.8896767283494,33.7444289564493,26.0516896829642));
#47805=CARTESIAN_POINT('Ctrl Pts',(-13.929706557768,33.8759349285887,26.0449684172972));
#47806=CARTESIAN_POINT('Ctrl Pts',(-13.9630405440442,34.0092756961385,26.0382471516302));
#47807=CARTESIAN_POINT('Ctrl Pts',(-13.9962417189321,34.1420851989211,26.0315526652574));
#47808=CARTESIAN_POINT('Ctrl Pts',(-14.0228002010074,34.2767147718557,26.0248581788846));
#47809=CARTESIAN_POINT('Ctrl Pts',(-14.0425382249071,34.412539618217,26.0181636925118));
#47810=CARTESIAN_POINT('Ctrl Pts',(-14.0621325522726,34.5473756340957,26.0115179432616));
#47811=CARTESIAN_POINT('Ctrl Pts',(-14.0750052824989,34.6833894343958,26.0048721940114));
#47812=CARTESIAN_POINT('Ctrl Pts',(-14.0810301740244,34.8199507881088,25.9982264447612));
#47813=CARTESIAN_POINT('Ctrl Pts',(-14.0836324814579,34.878935190466,25.9953559727201));
#47814=CARTESIAN_POINT('Ctrl Pts',(-14.0849578689422,34.9380215163847,25.9924855006789));
#47815=CARTESIAN_POINT('Ctrl Pts',(-14.0849990113761,34.997157983738,25.9896150286377));
#47816=CARTESIAN_POINT('Origin',(-10.,35.,32.7603849714045));
#47817=CARTESIAN_POINT('',(-7.51282733495085,38.2405550657615,28.0469627484298));
#47818=CARTESIAN_POINT('',(-7.51282733495086,38.2405550657615,27.9426390044296));
#47819=CARTESIAN_POINT('',(-7.51282733495086,38.2405550657615,32.7603849714045));
#47820=CARTESIAN_POINT('',(-14.0849997205636,35.0015109583762,27.1353849713726));
#47821=CARTESIAN_POINT('Ctrl Pts',(-7.51282733495086,38.2405550657615,27.9426390044296));
#47822=CARTESIAN_POINT('Ctrl Pts',(-7.41802037611531,38.1677893599836,27.9368359476833));
#47823=CARTESIAN_POINT('Ctrl Pts',(-7.32640226579339,38.0908542025866,27.9310328909369));
#47824=CARTESIAN_POINT('Ctrl Pts',(-7.2383497970762,38.0100686298972,27.9252298341906));
#47825=CARTESIAN_POINT('Ctrl Pts',(-7.15028244208156,37.9292693994822,27.9194257963712));
#47826=CARTESIAN_POINT('Ctrl Pts',(-7.06578222826958,37.8446187353752,27.9136217585517));
#47827=CARTESIAN_POINT('Ctrl Pts',(-6.98519006760836,37.7564734846453,27.9078177207322));
#47828=CARTESIAN_POINT('Ctrl Pts',(-6.90451482676891,37.6682373674703,27.9020076996944));
#47829=CARTESIAN_POINT('Ctrl Pts',(-6.8277559624221,37.5764997696668,27.8961976786565));
#47830=CARTESIAN_POINT('Ctrl Pts',(-6.75521511451344,37.4816518786724,27.8903876576187));
#47831=CARTESIAN_POINT('Ctrl Pts',(-6.6826367208746,37.3867548962567,27.8845746294271));
#47832=CARTESIAN_POINT('Ctrl Pts',(-6.61428092710793,37.288744748098,27.8787616012355));
#47833=CARTESIAN_POINT('Ctrl Pts',(-6.55040590798919,37.1880414987756,27.872948573044));
#47834=CARTESIAN_POINT('Ctrl Pts',(-6.48642760067838,37.0871754086947,27.8671261449777));
#47835=CARTESIAN_POINT('Ctrl Pts',(-6.42694474983516,36.983607869981,27.8613037169115));
#47836=CARTESIAN_POINT('Ctrl Pts',(-6.37216973770201,36.8777839566774,27.8554812888453));
#47837=CARTESIAN_POINT('Ctrl Pts',(-6.32164660039326,36.7801745560734,27.850110822985));
#47838=CARTESIAN_POINT('Ctrl Pts',(-6.27512835223445,36.6806459641039,27.8447403571246));
#47839=CARTESIAN_POINT('Ctrl Pts',(-6.2327445653037,36.5795605369061,27.8393698912643));
#47840=CARTESIAN_POINT('Ctrl Pts',(-6.18678478552992,36.4699463587314,27.8335463099825));
#47841=CARTESIAN_POINT('Ctrl Pts',(-6.14553895320145,36.3581478393045,27.8277227287006));
#47842=CARTESIAN_POINT('Ctrl Pts',(-6.10921899769923,36.2446076458609,27.8218991474188));
#47843=CARTESIAN_POINT('Ctrl Pts',(-6.07294486646626,36.1312107041455,27.8160829136503));
#47844=CARTESIAN_POINT('Ctrl Pts',(-6.04158437409596,36.0160768445666,27.8102666798818));
#47845=CARTESIAN_POINT('Ctrl Pts',(-6.01530181494215,35.8996695915705,27.8044504461132));
#47846=CARTESIAN_POINT('Ctrl Pts',(-5.98904556559313,35.7833788665002,27.7986400346078));
#47847=CARTESIAN_POINT('Ctrl Pts',(-5.96785722648496,35.6658176799201,27.7928296231025));
#47848=CARTESIAN_POINT('Ctrl Pts',(-5.95185140977864,35.5474650596055,27.7870192115971));
#47849=CARTESIAN_POINT('Ctrl Pts',(-5.93523969038897,35.4246321824225,27.7809888460595));
#47850=CARTESIAN_POINT('Ctrl Pts',(-5.92421075358353,35.3009471947128,27.774958480522));
#47851=CARTESIAN_POINT('Ctrl Pts',(-5.91883462399233,35.1769581127731,27.7689281149844));
#47852=CARTESIAN_POINT('Ctrl Pts',(-5.91366041635228,35.0576259344515,27.7631242438337));
#47853=CARTESIAN_POINT('Ctrl Pts',(-5.91372206606784,34.9380125375034,27.757320372683));
#47854=CARTESIAN_POINT('Ctrl Pts',(-5.91902913849428,34.8186113908173,27.7515165015323));
#47855=CARTESIAN_POINT('Ctrl Pts',(-5.92433542691345,34.6992278831154,27.7457134877804));
#47856=CARTESIAN_POINT('Ctrl Pts',(-5.93488557888585,34.5800569711454,27.7399104740284));
#47857=CARTESIAN_POINT('Ctrl Pts',(-5.95063705580308,34.4615905404203,27.7341074602764));
#47858=CARTESIAN_POINT('Ctrl Pts',(-5.9663899231729,34.3431136521391,27.7283039342668));
#47859=CARTESIAN_POINT('Ctrl Pts',(-5.98734497455411,34.2253417735434,27.7225004082571));
#47860=CARTESIAN_POINT('Ctrl Pts',(-6.01340806027706,34.1087594566358,27.7166968822474));
#47861=CARTESIAN_POINT('Ctrl Pts',(-6.03947959763761,33.9921393348611,27.7108914742926));
#47862=CARTESIAN_POINT('Ctrl Pts',(-6.0706623745295,33.876709940234,27.7050860663377));
#47863=CARTESIAN_POINT('Ctrl Pts',(-6.10681177311979,33.7629428347561,27.6992806583828));
#47864=CARTESIAN_POINT('Ctrl Pts',(-6.14300120363802,33.6490497433214,27.6934688215057));
#47865=CARTESIAN_POINT('Ctrl Pts',(-6.18416811069166,33.536823004872,27.6876569846286));
#47866=CARTESIAN_POINT('Ctrl Pts',(-6.23011885586395,33.4267164403429,27.6818451477515));
#47867=CARTESIAN_POINT('Ctrl Pts',(-6.27609978147261,33.3165375578534,27.6760294936616));
#47868=CARTESIAN_POINT('Ctrl Pts',(-6.32687062936867,33.2084819912689,27.6702138395717));
#47869=CARTESIAN_POINT('Ctrl Pts',(-6.38219146353194,33.1029796012012,27.6643981854818));
#47870=CARTESIAN_POINT('Ctrl Pts',(-6.43759153938857,32.9973260892611,27.6585742010352));
#47871=CARTESIAN_POINT('Ctrl Pts',(-6.49755440533462,32.8942334050838,27.6527502165887));
#47872=CARTESIAN_POINT('Ctrl Pts',(-6.56179637688084,32.794103165157,27.6469262321421));
#47873=CARTESIAN_POINT('Ctrl Pts',(-6.57884155236157,32.7675358374521,27.64538096766));
#47874=CARTESIAN_POINT('Ctrl Pts',(-6.59618775046187,32.7411768833744,27.643835703178));
#47875=CARTESIAN_POINT('Ctrl Pts',(-6.61382920367194,32.715033405475,27.6422904386959));
#47876=CARTESIAN_POINT('Ctrl Pts',(-6.68031409542711,32.6165071515693,27.6364668401181));
#47877=CARTESIAN_POINT('Ctrl Pts',(-6.75120994370549,32.5207261598631,27.6306432415404));
#47878=CARTESIAN_POINT('Ctrl Pts',(-6.82626268247139,32.4281103368678,27.6248196429626));
#47879=CARTESIAN_POINT('Ctrl Pts',(-6.9012207317816,32.3356113615987,27.6190033916635));
#47880=CARTESIAN_POINT('Ctrl Pts',(-6.9803249855821,32.2462699269102,27.6131871403643));
#47881=CARTESIAN_POINT('Ctrl Pts',(-7.06327782186871,32.1604775316135,27.6073708890651));
#47882=CARTESIAN_POINT('Ctrl Pts',(-7.14614762259942,32.0747710142632,27.6015604598171));
#47883=CARTESIAN_POINT('Ctrl Pts',(-7.23285805969597,31.9926067607567,27.5957500305691));
#47884=CARTESIAN_POINT('Ctrl Pts',(-7.32307131084594,31.9143432152645,27.5899396013212));
#47885=CARTESIAN_POINT('Ctrl Pts',(-7.41669921073822,31.8331173276134,27.5839092423548));
#47886=CARTESIAN_POINT('Ctrl Pts',(-7.51410005066375,31.7560936207688,27.5778788833884));
#47887=CARTESIAN_POINT('Ctrl Pts',(-7.61485387219103,31.6836310595777,27.571848524422));
#47888=CARTESIAN_POINT('Ctrl Pts',(-7.7118238918668,31.6138898241789,27.5660446351127));
#47889=CARTESIAN_POINT('Ctrl Pts',(-7.81189923141333,31.5483735852726,27.5602407458035));
#47890=CARTESIAN_POINT('Ctrl Pts',(-7.91467240806616,31.4873608448462,27.5544368564943));
#47891=CARTESIAN_POINT('Ctrl Pts',(-8.01743040437785,31.4263571164427,27.5486338244615));
#47892=CARTESIAN_POINT('Ctrl Pts',(-8.1228850942968,31.3698557720406,27.5428307924287));
#47893=CARTESIAN_POINT('Ctrl Pts',(-8.2306017580057,31.3180908673315,27.5370277603959));
#47894=CARTESIAN_POINT('Ctrl Pts',(-8.33832793221818,31.2663213922032,27.5312242160027));
#47895=CARTESIAN_POINT('Ctrl Pts',(-8.44831610923865,31.2192893651064,27.5254206716094));
#47896=CARTESIAN_POINT('Ctrl Pts',(-8.56010941160991,31.1771816557067,27.5196171272162));
#47897=CARTESIAN_POINT('Ctrl Pts',(-8.67193896737304,31.1350602912198,27.5138117007945));
#47898=CARTESIAN_POINT('Ctrl Pts',(-8.7855744307501,31.0978665641698,27.5080062743729));
#47899=CARTESIAN_POINT('Ctrl Pts',(-8.90054212403392,31.0657380134292,27.5022008479513));
#47900=CARTESIAN_POINT('Ctrl Pts',(-9.0156371330191,31.0335738833979,27.4963889925763));
#47901=CARTESIAN_POINT('Ctrl Pts',(-9.13206692326843,31.006486236081,27.4905771372013));
#47902=CARTESIAN_POINT('Ctrl Pts',(-9.24934578396128,30.9845618859279,27.4847652818263));
#47903=CARTESIAN_POINT('Ctrl Pts',(-9.36670167393422,30.9626231357635,27.4789496091988));
#47904=CARTESIAN_POINT('Ctrl Pts',(-9.484907341612,30.9458544937966,27.4731339365712));
#47905=CARTESIAN_POINT('Ctrl Pts',(-9.60347173726377,30.9342909183205,27.4673182639436));
#47906=CARTESIAN_POINT('Ctrl Pts',(-9.72220596261296,30.9227107793683,27.4614942610419));
#47907=CARTESIAN_POINT('Ctrl Pts',(-9.84129953521717,30.9163506096816,27.4556702581401));
#47908=CARTESIAN_POINT('Ctrl Pts',(-9.96026104661172,30.9151932951994,27.4498462552384));
#47909=CARTESIAN_POINT('Ctrl Pts',(-9.99182116247825,30.9148862632971,27.4483011655347));
#47910=CARTESIAN_POINT('Ctrl Pts',(-10.0233720118736,30.9149451379122,27.4467560758311));
#47911=CARTESIAN_POINT('Ctrl Pts',(-10.0549044960146,30.915368988964,27.4452109861274));
#47912=CARTESIAN_POINT('Ctrl Pts',(-10.1737535104193,30.9169665250009,27.4393873920324));
#47913=CARTESIAN_POINT('Ctrl Pts',(-10.2927243948804,30.9237581020526,27.4335637979374));
#47914=CARTESIAN_POINT('Ctrl Pts',(-10.4113266826636,30.9357614046258,27.4277402038423));
#47915=CARTESIAN_POINT('Ctrl Pts',(-10.529779336445,30.9477495632906,27.4219239570566));
#47916=CARTESIAN_POINT('Ctrl Pts',(-10.647863915818,30.9649363285096,27.4161077102708));
#47917=CARTESIAN_POINT('Ctrl Pts',(-10.7650898375638,30.9872873837693,27.4102914634851));
#47918=CARTESIAN_POINT('Ctrl Pts',(-10.8821984158978,31.0096160655724,27.4044810387755));
#47919=CARTESIAN_POINT('Ctrl Pts',(-10.9984496477042,31.0370986773648,27.3986706140659));
#47920=CARTESIAN_POINT('Ctrl Pts',(-11.1133585593071,31.0696491608996,27.3928601893562));
#47921=CARTESIAN_POINT('Ctrl Pts',(-11.2326169981372,31.1034317439505,27.386829828698));
#47922=CARTESIAN_POINT('Ctrl Pts',(-11.3504290441034,31.142673391791,27.3807994680398));
#47923=CARTESIAN_POINT('Ctrl Pts',(-11.4662642623488,31.1872196348388,27.3747691073816));
#47924=CARTESIAN_POINT('Ctrl Pts',(-11.5777491789926,31.2300929014343,27.3689652226434));
#47925=CARTESIAN_POINT('Ctrl Pts',(-11.6874026581099,31.2778793505669,27.3631613379053));
#47926=CARTESIAN_POINT('Ctrl Pts',(-11.7947684019703,31.3303908405269,27.3573574531672));
#47927=CARTESIAN_POINT('Ctrl Pts',(-11.9021182870467,31.3828945741174,27.3515544257095));
#47928=CARTESIAN_POINT('Ctrl Pts',(-12.0071807421609,31.4401217812231,27.3457513982518));
#47929=CARTESIAN_POINT('Ctrl Pts',(-12.1095217127996,31.5018371759984,27.3399483707941));
#47930=CARTESIAN_POINT('Ctrl Pts',(-12.2118717193363,31.5635580197547,27.334144830975));
#47931=CARTESIAN_POINT('Ctrl Pts',(-12.3114994139579,31.6297676281855,27.3283412911559));
#47932=CARTESIAN_POINT('Ctrl Pts',(-12.4079980611583,31.7001863177661,27.3225377513369));
#47933=CARTESIAN_POINT('Ctrl Pts',(-12.5045280019799,31.7706278434782,27.3167323294833));
#47934=CARTESIAN_POINT('Ctrl Pts',(-12.5979265476489,31.8452809243699,27.3109269076298));
#47935=CARTESIAN_POINT('Ctrl Pts',(-12.6878190122229,31.923824784325,27.3051214857763));
#47936=CARTESIAN_POINT('Ctrl Pts',(-12.7778110246595,32.0024556245785,27.2993096349375));
#47937=CARTESIAN_POINT('Ctrl Pts',(-12.8642888981799,32.0849855755752,27.2934977840986));
#47938=CARTESIAN_POINT('Ctrl Pts',(-12.9469137751714,32.1710559917692,27.2876859332597));
#47939=CARTESIAN_POINT('Ctrl Pts',(-13.0295929207846,32.2571829396402,27.2818702651549));
#47940=CARTESIAN_POINT('Ctrl Pts',(-13.1084137609984,32.3468546778158,27.27605459705));
#47941=CARTESIAN_POINT('Ctrl Pts',(-13.183077882607,32.4396796697956,27.2702389289451));
#47942=CARTESIAN_POINT('Ctrl Pts',(-13.2578489526581,32.5326376237402,27.2644149305119));
#47943=CARTESIAN_POINT('Ctrl Pts',(-13.3284511792542,32.6287575186502,27.2585909320788));
#47944=CARTESIAN_POINT('Ctrl Pts',(-13.3946295043692,32.7276189738369,27.2527669336456));
#47945=CARTESIAN_POINT('Ctrl Pts',(-13.4121869160277,32.7538473690533,27.2512218002834));
#47946=CARTESIAN_POINT('Ctrl Pts',(-13.4294331969676,32.7802686016505,27.2496766669212));
#47947=CARTESIAN_POINT('Ctrl Pts',(-13.4463641371064,32.8068745511333,27.248131533559));
#47948=CARTESIAN_POINT('Ctrl Pts',(-13.511628181384,32.9094330535468,27.242175476108));
#47949=CARTESIAN_POINT('Ctrl Pts',(-13.5724057738479,33.0150566328513,27.2362194186571));
#47950=CARTESIAN_POINT('Ctrl Pts',(-13.6284046854858,33.1233262301762,27.2302633612062));
#47951=CARTESIAN_POINT('Ctrl Pts',(-13.6843233504708,33.2314406767572,27.2243158388082));
#47952=CARTESIAN_POINT('Ctrl Pts',(-13.735476789618,33.3421932568942,27.2183683164102));
#47953=CARTESIAN_POINT('Ctrl Pts',(-13.7816163112617,33.4551365515363,27.2124207940122));
#47954=CARTESIAN_POINT('Ctrl Pts',(-13.8276986054601,33.5679397611495,27.2064806484032));
#47955=CARTESIAN_POINT('Ctrl Pts',(-13.8687792177871,33.6829279234472,27.2005405027941));
#47956=CARTESIAN_POINT('Ctrl Pts',(-13.9046557781041,33.7996299510075,27.194600357185));
#47957=CARTESIAN_POINT('Ctrl Pts',(-13.9404859561889,33.9161811028851,27.1886678911643));
#47958=CARTESIAN_POINT('Ctrl Pts',(-13.971125376415,34.0344413399889,27.1827354251435));
#47959=CARTESIAN_POINT('Ctrl Pts',(-13.9964203632244,34.1539212327418,27.1768029591227));
#47960=CARTESIAN_POINT('Ctrl Pts',(-14.021696079943,34.2733101039656,27.1708750125413));
#47961=CARTESIAN_POINT('Ctrl Pts',(-14.0416353884593,34.3939164074824,27.1649470659599));
#47962=CARTESIAN_POINT('Ctrl Pts',(-14.0561348460667,34.5152370573942,27.1590191193785));
#47963=CARTESIAN_POINT('Ctrl Pts',(-14.0706246909313,34.636477275043,27.153095102863));
#47964=CARTESIAN_POINT('Ctrl Pts',(-14.0796818242133,34.7584305156171,27.1471710863476));
#47965=CARTESIAN_POINT('Ctrl Pts',(-14.0832542386473,34.880585501012,27.1412470698321));
#47966=CARTESIAN_POINT('Ctrl Pts',(-14.0844325971131,34.9208782396713,27.1392930370229));
#47967=CARTESIAN_POINT('Ctrl Pts',(-14.0850146333955,34.9611928784735,27.1373390042137));
#47968=CARTESIAN_POINT('Ctrl Pts',(-14.0849997205639,35.0015109577178,27.1353849714045));
#47969=CARTESIAN_POINT('Ctrl Pts',(-14.0849997205636,35.0015109583762,27.1353849713726));
#47970=CARTESIAN_POINT('Ctrl Pts',(-14.0849517284655,35.1312615262673,27.1290965550734));
#47971=CARTESIAN_POINT('Ctrl Pts',(-14.0787177200379,35.260826007354,27.1228081387741));
#47972=CARTESIAN_POINT('Ctrl Pts',(-14.0663757192053,35.3896325323401,27.1165197224749));
#47973=CARTESIAN_POINT('Ctrl Pts',(-14.0539812321377,35.518986826657,27.1102045637293));
#47974=CARTESIAN_POINT('Ctrl Pts',(-14.0354267800673,35.6475764227977,27.1038894049837));
#47975=CARTESIAN_POINT('Ctrl Pts',(-14.0108419950697,35.7748364282771,27.0975742462381));
#47976=CARTESIAN_POINT('Ctrl Pts',(-13.9862032615903,35.902375691195,27.0912452296032));
#47977=CARTESIAN_POINT('Ctrl Pts',(-13.955507825809,36.0285792550034,27.0849162129684));
#47978=CARTESIAN_POINT('Ctrl Pts',(-13.918935263764,36.1528969591543,27.0785871963336));
#47979=CARTESIAN_POINT('Ctrl Pts',(-13.882247254912,36.2776070908842,27.0722382012035));
#47980=CARTESIAN_POINT('Ctrl Pts',(-13.8396450940903,36.4004191788262,27.0658892060733));
#47981=CARTESIAN_POINT('Ctrl Pts',(-13.7913574449856,36.5208003565073,27.0595402109431));
#47982=CARTESIAN_POINT('Ctrl Pts',(-13.7698384574765,36.5744472228773,27.0567108342923));
#47983=CARTESIAN_POINT('Ctrl Pts',(-13.7471909666541,36.6276116407118,27.0538814576414));
#47984=CARTESIAN_POINT('Ctrl Pts',(-13.723438111232,36.6802480863923,27.0510520809906));
#47985=CARTESIAN_POINT('Ctrl Pts',(-13.6745485456912,36.7885876066396,27.0452284866162));
#47986=CARTESIAN_POINT('Ctrl Pts',(-13.6208477443071,36.8949662781929,27.0394048922419));
#47987=CARTESIAN_POINT('Ctrl Pts',(-13.5625152040873,36.9989273174997,27.0335812978675));
#47988=CARTESIAN_POINT('Ctrl Pts',(-13.5042562589436,37.1027571946701,27.0277650508137));
#47989=CARTESIAN_POINT('Ctrl Pts',(-13.441377395838,37.2041751533971,27.0219488037599));
#47990=CARTESIAN_POINT('Ctrl Pts',(-13.3741058398894,37.3027450534577,27.0161325567061));
#47991=CARTESIAN_POINT('Ctrl Pts',(-13.3069016230506,37.4012162846349,27.01032213174));
#47992=CARTESIAN_POINT('Ctrl Pts',(-13.2353136897221,37.4968447933583,27.0045117067738));
#47993=CARTESIAN_POINT('Ctrl Pts',(-13.1596144705095,37.5892202296728,26.9987012818077));
#47994=CARTESIAN_POINT('Ctrl Pts',(-13.0810498924533,37.6850922512379,26.99267092125));
#47995=CARTESIAN_POINT('Ctrl Pts',(-12.9980568583433,37.7774596737138,26.9866405606923));
#47996=CARTESIAN_POINT('Ctrl Pts',(-12.9109886680953,37.8658977606015,26.9806102001345));
#47997=CARTESIAN_POINT('Ctrl Pts',(-12.8271904017444,37.9510144758964,26.9748063151707));
#47998=CARTESIAN_POINT('Ctrl Pts',(-12.7396178638162,38.0324913554615,26.9690024302068));
#47999=CARTESIAN_POINT('Ctrl Pts',(-12.6486256463042,38.1099850780574,26.963198545243));
#48000=CARTESIAN_POINT('Ctrl Pts',(-12.5576468692598,38.1874673540495,26.9573955175714));
#48001=CARTESIAN_POINT('Ctrl Pts',(-12.4632497279483,38.2609673784343,26.9515924898999));
#48002=CARTESIAN_POINT('Ctrl Pts',(-12.3658231667572,38.3301810376667,26.9457894622284));
#48003=CARTESIAN_POINT('Ctrl Pts',(-12.2683880037758,38.3994008077726,26.9399859222075));
#48004=CARTESIAN_POINT('Ctrl Pts',(-12.1679232220264,38.4643332237901,26.9341823821867));
#48005=CARTESIAN_POINT('Ctrl Pts',(-12.0648475745558,38.5247169381173,26.9283788421659));
#48006=CARTESIAN_POINT('Ctrl Pts',(-11.9617385008254,38.585120234196,26.9225734201231));
#48007=CARTESIAN_POINT('Ctrl Pts',(-11.8560172296798,38.6409716886629,26.9167679980803));
#48008=CARTESIAN_POINT('Ctrl Pts',(-11.7481274046206,38.6920557386386,26.9109625760375));
#48009=CARTESIAN_POINT('Ctrl Pts',(-11.6401181015986,38.7431963594561,26.9051507250288));
#48010=CARTESIAN_POINT('Ctrl Pts',(-11.5299358203959,38.7895588626861,26.8993388740202));
#48011=CARTESIAN_POINT('Ctrl Pts',(-11.4180446316806,38.8309756489127,26.8935270230115));
#48012=CARTESIAN_POINT('Ctrl Pts',(-11.3060799522349,38.8724196379056,26.8877113547481));
#48013=CARTESIAN_POINT('Ctrl Pts',(-11.192404517851,38.9089113161549,26.8818956864847));
#48014=CARTESIAN_POINT('Ctrl Pts',(-11.0774964194521,38.9403332937796,26.8760800182213));
#48015=CARTESIAN_POINT('Ctrl Pts',(-10.9624237277325,38.9718002799608,26.8702560196472));
#48016=CARTESIAN_POINT('Ctrl Pts',(-10.8461152446498,38.9981829813635,26.8644320210732));
#48017=CARTESIAN_POINT('Ctrl Pts',(-10.7290582092595,39.0194152718413,26.8586080224991));
#48018=CARTESIAN_POINT('Ctrl Pts',(-10.698002484593,39.0250482879597,26.8570628911401));
#48019=CARTESIAN_POINT('Ctrl Pts',(-10.6668940919761,39.0303190693622,26.8555177597811));
#48020=CARTESIAN_POINT('Ctrl Pts',(-10.6357421573143,39.0352269960206,26.8539726284221));
#48021=CARTESIAN_POINT('Ctrl Pts',(-10.5183157489126,39.0537272980548,26.8481482959058));
#48022=CARTESIAN_POINT('Ctrl Pts',(-10.399891739978,39.0671274618897,26.8423239633895));
#48023=CARTESIAN_POINT('Ctrl Pts',(-10.280950748406,39.0753271864931,26.8364996308732));
#48024=CARTESIAN_POINT('Ctrl Pts',(-10.1586484671851,39.0837586365015,26.8305107018764));
#48025=CARTESIAN_POINT('Ctrl Pts',(-10.0357999544713,39.08669119238,26.8245217728796));
#48026=CARTESIAN_POINT('Ctrl Pts',(-9.91293954859989,39.084072168535,26.8185328438828));
#48027=CARTESIAN_POINT('Ctrl Pts',(-9.79375530529611,39.0815315097039,26.812723112378));
#48028=CARTESIAN_POINT('Ctrl Pts',(-9.67456031682524,39.0737667410615,26.8069133808732));
#48029=CARTESIAN_POINT('Ctrl Pts',(-9.55584699425329,39.0607823270259,26.8011036493684));
#48030=CARTESIAN_POINT('Ctrl Pts',(-9.43721246835627,39.0478065314725,26.7952977741075));
#48031=CARTESIAN_POINT('Ctrl Pts',(-9.31905937694257,39.029618025078,26.7894918988466));
#48032=CARTESIAN_POINT('Ctrl Pts',(-9.2018775407792,39.0062732732662,26.7836860235857));
#48033=CARTESIAN_POINT('Ctrl Pts',(-9.08474582834405,38.9829385070122,26.7778826317482));
#48034=CARTESIAN_POINT('Ctrl Pts',(-8.96858494435268,38.9544519629652,26.7720792399107));
#48035=CARTESIAN_POINT('Ctrl Pts',(-8.85387638091336,38.9209215306828,26.7662758480732));
#48036=CARTESIAN_POINT('Ctrl Pts',(-8.73918981206799,38.8873975276347,26.760473568997));
#48037=CARTESIAN_POINT('Ctrl Pts',(-8.62595540081611,38.8488316768081,26.7546712899207));
#48038=CARTESIAN_POINT('Ctrl Pts',(-8.51464067433854,38.8053820667143,26.7488690108445));
#48039=CARTESIAN_POINT('Ctrl Pts',(-8.40328784783913,38.7619175849934,26.743064745805));
#48040=CARTESIAN_POINT('Ctrl Pts',(-8.29385639982131,38.7135661517273,26.7372604807654));
#48041=CARTESIAN_POINT('Ctrl Pts',(-8.18679482973066,38.6605343886526,26.7314562157259));
#48042=CARTESIAN_POINT('Ctrl Pts',(-8.07971025319162,38.6074912295886,26.7256507034086));
#48043=CARTESIAN_POINT('Ctrl Pts',(-7.97499692976636,38.549765928425,26.7198451910912));
#48044=CARTESIAN_POINT('Ctrl Pts',(-7.87307860825309,38.4876109865249,26.7140396787738));
#48045=CARTESIAN_POINT('Ctrl Pts',(-7.77108030047314,38.4254072649581,26.7082296102467));
#48046=CARTESIAN_POINT('Ctrl Pts',(-7.67188171481285,38.3587671863771,26.7024195417195));
#48047=CARTESIAN_POINT('Ctrl Pts',(-7.57587734912902,38.287986370643,26.6966094731923));
#48048=CARTESIAN_POINT('Ctrl Pts',(-7.55470410181315,38.2723760418201,26.6953280937783));
#48049=CARTESIAN_POINT('Ctrl Pts',(-7.5336860937674,38.2565644634426,26.6940467143642));
#48050=CARTESIAN_POINT('Ctrl Pts',(-7.51282733495086,38.2405550657615,26.6927653349501));
#48051=CARTESIAN_POINT('',(-14.0849999969886,34.9998431448262,27.2396150285597));
#48052=CARTESIAN_POINT('Ctrl Pts',(-14.0849999969886,34.9998431448262,27.2396150285597));
#48053=CARTESIAN_POINT('Ctrl Pts',(-14.0850045558039,35.1185689743034,27.2337980380796));
#48054=CARTESIAN_POINT('Ctrl Pts',(-14.0798288721455,35.2374885762744,27.2279810475995));
#48055=CARTESIAN_POINT('Ctrl Pts',(-14.0694482080588,35.3561127376648,27.2221640571194));
#48056=CARTESIAN_POINT('Ctrl Pts',(-14.0590806440589,35.474587198921,27.2163544075068));
#48057=CARTESIAN_POINT('Ctrl Pts',(-14.0435211990243,35.5927665569149,27.2105447578942));
#48058=CARTESIAN_POINT('Ctrl Pts',(-14.0227971293024,35.7101607258055,27.2047351082816));
#48059=CARTESIAN_POINT('Ctrl Pts',(-14.0020937762772,35.8274375422926,27.1989312662518));
#48060=CARTESIAN_POINT('Ctrl Pts',(-13.9762361395857,35.9439303302516,27.1931274242219));
#48061=CARTESIAN_POINT('Ctrl Pts',(-13.9453032926047,36.0591538742612,27.187323582192));
#48062=CARTESIAN_POINT('Ctrl Pts',(-13.9134326011801,36.1778708490754,27.1813437750787));
#48063=CARTESIAN_POINT('Ctrl Pts',(-13.8761740789372,36.2952399475765,27.1753639679655));
#48064=CARTESIAN_POINT('Ctrl Pts',(-13.8336711615995,36.4107410906047,27.1693841608522));
#48065=CARTESIAN_POINT('Ctrl Pts',(-13.7924649384881,36.5227184833897,27.1635867878363));
#48066=CARTESIAN_POINT('Ctrl Pts',(-13.7463298210225,36.6329398305309,27.1577894148203));
#48067=CARTESIAN_POINT('Ctrl Pts',(-13.6954469874095,36.7409470305687,27.1519920418044));
#48068=CARTESIAN_POINT('Ctrl Pts',(-13.6445714568429,36.8489387286871,27.1461955008664));
#48069=CARTESIAN_POINT('Ctrl Pts',(-13.5889497396612,36.9547165414042,27.1403989599284));
#48070=CARTESIAN_POINT('Ctrl Pts',(-13.5288104706594,37.0578439353275,27.1346024189904));
#48071=CARTESIAN_POINT('Ctrl Pts',(-13.4686655496186,37.1609810214215,27.128805333279));
#48072=CARTESIAN_POINT('Ctrl Pts',(-13.4040024389248,37.2614668398338,27.1230082475676));
#48073=CARTESIAN_POINT('Ctrl Pts',(-13.3350945484181,37.3588915517911,27.1172111618562));
#48074=CARTESIAN_POINT('Ctrl Pts',(-13.2661638155399,37.4563485592004,27.1114121544608));
#48075=CARTESIAN_POINT('Ctrl Pts',(-13.1929857408893,37.5507421081638,27.1056131470655));
#48076=CARTESIAN_POINT('Ctrl Pts',(-13.1158752615912,37.6416938418757,27.0998141396701));
#48077=CARTESIAN_POINT('Ctrl Pts',(-13.0386792540938,37.7327464560136,27.0940087002221));
#48078=CARTESIAN_POINT('Ctrl Pts',(-12.9575424012137,37.8203493229476,27.0882032607742));
#48079=CARTESIAN_POINT('Ctrl Pts',(-12.8728179773002,37.9041594083832,27.0823978213262));
#48080=CARTESIAN_POINT('Ctrl Pts',(-12.7880371252074,37.9880253130302,27.0765885153382));
#48081=CARTESIAN_POINT('Ctrl Pts',(-12.6996642465922,38.0680931317307,27.0707792093502));
#48082=CARTESIAN_POINT('Ctrl Pts',(-12.6080860325812,38.1440598350946,27.0649699033622));
#48083=CARTESIAN_POINT('Ctrl Pts',(-12.5163779071733,38.2201343036147,27.0591523563851));
#48084=CARTESIAN_POINT('Ctrl Pts',(-12.4214556969101,38.2920958001124,27.0533348094081));
#48085=CARTESIAN_POINT('Ctrl Pts',(-12.3237354569492,38.3596842896494,27.0475172624311));
#48086=CARTESIAN_POINT('Ctrl Pts',(-12.3029678636063,38.3740482562742,27.0462809121119));
#48087=CARTESIAN_POINT('Ctrl Pts',(-12.2820739852722,38.3882148807375,27.0450445617926));
#48088=CARTESIAN_POINT('Ctrl Pts',(-12.2610579524937,38.4021819374432,27.0438082114734));
#48089=CARTESIAN_POINT('Ctrl Pts',(-12.1620659091485,38.4679711136116,27.0379846173782));
#48090=CARTESIAN_POINT('Ctrl Pts',(-12.0600404855678,38.5295422904057,27.032161023283));
#48091=CARTESIAN_POINT('Ctrl Pts',(-11.955376494584,38.586603931915,27.0263374291879));
#48092=CARTESIAN_POINT('Ctrl Pts',(-11.8508445524174,38.6435935818808,27.020521182402));
#48093=CARTESIAN_POINT('Ctrl Pts',(-11.7436810193798,38.6960848189747,27.0147049356161));
#48094=CARTESIAN_POINT('Ctrl Pts',(-11.6343101666339,38.7438289596665,27.0088886888302));
#48095=CARTESIAN_POINT('Ctrl Pts',(-11.5250487943582,38.7915253083657,27.0030782641205));
#48096=CARTESIAN_POINT('Ctrl Pts',(-11.4135848700468,38.8344838514615,26.9972678394107));
#48097=CARTESIAN_POINT('Ctrl Pts',(-11.3003672509087,38.8725017769866,26.991457414701));
#48098=CARTESIAN_POINT('Ctrl Pts',(-11.1828641232769,38.9119587554081,26.9854270540428));
#48099=CARTESIAN_POINT('Ctrl Pts',(-11.0634723096386,38.9460934875123,26.9793966933847));
#48100=CARTESIAN_POINT('Ctrl Pts',(-10.9427168160288,38.9747339539618,26.9733663327265));
#48101=CARTESIAN_POINT('Ctrl Pts',(-10.8264964096308,39.0022988005015,26.9675624479883));
#48102=CARTESIAN_POINT('Ctrl Pts',(-10.7090133377308,39.0247745211941,26.96175856325));
#48103=CARTESIAN_POINT('Ctrl Pts',(-10.5907504314025,39.0420587486821,26.9559546785118));
#48104=CARTESIAN_POINT('Ctrl Pts',(-10.4725049934573,39.0593404231507,26.9501516510541));
#48105=CARTESIAN_POINT('Ctrl Pts',(-10.3534803540914,39.0714320703526,26.9443486235963));
#48106=CARTESIAN_POINT('Ctrl Pts',(-10.2341676060894,39.0782827920901,26.9385455961386));
#48107=CARTESIAN_POINT('Ctrl Pts',(-10.1148443237163,39.0851341186921,26.9327420563194));
#48108=CARTESIAN_POINT('Ctrl Pts',(-9.99523328981639,39.0867435763978,26.9269385165003));
#48109=CARTESIAN_POINT('Ctrl Pts',(-9.87582811889162,39.0831123354547,26.9211349766812));
#48110=CARTESIAN_POINT('Ctrl Pts',(-9.75638422597141,39.0794799169336,26.9153295548276));
#48111=CARTESIAN_POINT('Ctrl Pts',(-9.63714673673404,39.0706034322274,26.9095241329741));
#48112=CARTESIAN_POINT('Ctrl Pts',(-9.51860601690882,39.0565360633234,26.9037187111205));
#48113=CARTESIAN_POINT('Ctrl Pts',(-9.39993402384117,39.0424531160669,26.8979068602816));
#48114=CARTESIAN_POINT('Ctrl Pts',(-9.28196074611695,39.0231678583829,26.8920950094427));
#48115=CARTESIAN_POINT('Ctrl Pts',(-9.16516836200605,38.9987849574845,26.8862831586038));
#48116=CARTESIAN_POINT('Ctrl Pts',(-9.04829926780661,38.9743860417192,26.8804674904989));
#48117=CARTESIAN_POINT('Ctrl Pts',(-8.93261300664934,38.9448829154511,26.8746518223941));
#48118=CARTESIAN_POINT('Ctrl Pts',(-8.81857694846586,38.910430228671,26.8688361542892));
#48119=CARTESIAN_POINT('Ctrl Pts',(-8.70437754571248,38.8759281920677,26.863012155856));
#48120=CARTESIAN_POINT('Ctrl Pts',(-8.59183344779533,38.8364625788986,26.8571881574228));
#48121=CARTESIAN_POINT('Ctrl Pts',(-8.48139252895936,38.7922363255604,26.8513641589896));
#48122=CARTESIAN_POINT('Ctrl Pts',(-8.45209204920571,38.7805028987275,26.8498190256281));
#48123=CARTESIAN_POINT('Ctrl Pts',(-8.42293947092207,38.7684346380036,26.8482738922665));
#48124=CARTESIAN_POINT('Ctrl Pts',(-8.39394285403675,38.7560358682926,26.8467287589049));
#48125=CARTESIAN_POINT('Ctrl Pts',(-8.28465587827726,38.7093054496986,26.840905219114));
#48126=CARTESIAN_POINT('Ctrl Pts',(-8.1772338902608,38.6577259362034,26.8350816793232));
#48127=CARTESIAN_POINT('Ctrl Pts',(-8.07213713171789,38.6014677231789,26.8292581395323));
#48128=CARTESIAN_POINT('Ctrl Pts',(-7.96718840989531,38.5452887540954,26.823442802637));
#48129=CARTESIAN_POINT('Ctrl Pts',(-7.86455875644979,38.4844443913091,26.8176274657417));
#48130=CARTESIAN_POINT('Ctrl Pts',(-7.76468852857154,38.4191530567818,26.8118121288463));
#48131=CARTESIAN_POINT('Ctrl Pts',(-7.67859493062924,38.3628683558921,26.8067989904246));
#48132=CARTESIAN_POINT('Ctrl Pts',(-7.59455181840578,38.3032797833452,26.8017858520028));
#48133=CARTESIAN_POINT('Ctrl Pts',(-7.51282733495086,38.2405550657615,26.7967727135811));
#48134=CARTESIAN_POINT('Ctrl Pts',(-7.51282733495086,38.2405550657615,28.0469627484298));
#48135=CARTESIAN_POINT('Ctrl Pts',(-7.41670709116374,38.1667813948768,28.0410436570584));
#48136=CARTESIAN_POINT('Ctrl Pts',(-7.32400107801209,38.0888265544615,28.035124565687));
#48137=CARTESIAN_POINT('Ctrl Pts',(-7.23507125100175,38.0070573677539,28.0292054743156));
#48138=CARTESIAN_POINT('Ctrl Pts',(-7.14757772263507,37.9266088287515,28.0233819817235));
#48139=CARTESIAN_POINT('Ctrl Pts',(-7.06345707173295,37.8422087686331,28.0175584891315));
#48140=CARTESIAN_POINT('Ctrl Pts',(-6.98308656305463,37.7541710756557,28.0117349965394));
#48141=CARTESIAN_POINT('Ctrl Pts',(-6.90281747526042,37.6662444789101,28.0059188527097));
#48142=CARTESIAN_POINT('Ctrl Pts',(-6.82628939002253,37.5746896783972,28.0001027088799));
#48143=CARTESIAN_POINT('Ctrl Pts',(-6.75384498132295,37.4798593901102,27.9942865650502));
#48144=CARTESIAN_POINT('Ctrl Pts',(-6.68147310735251,37.3851240503417,27.9884762446156));
#48145=CARTESIAN_POINT('Ctrl Pts',(-6.6131770223021,37.2871200697274,27.982665924181));
#48146=CARTESIAN_POINT('Ctrl Pts',(-6.54926071521043,37.1862349801451,27.9768556037465));
#48147=CARTESIAN_POINT('Ctrl Pts',(-6.4829234357633,37.0815286433088,27.9708252044965));
#48148=CARTESIAN_POINT('Ctrl Pts',(-6.42130458400046,36.9737189565349,27.9647948052465));
#48149=CARTESIAN_POINT('Ctrl Pts',(-6.36469642355648,36.8632747803523,27.9587644059965));
#48150=CARTESIAN_POINT('Ctrl Pts',(-6.31021558851144,36.7569810782235,27.9529606281628));
#48151=CARTESIAN_POINT('Ctrl Pts',(-6.26037584188556,36.6482477169935,27.9471568503291));
#48152=CARTESIAN_POINT('Ctrl Pts',(-6.21539172638949,36.5375191755939,27.9413530724953));
#48153=CARTESIAN_POINT('Ctrl Pts',(-6.17041426163255,36.4268070050095,27.9355501527292));
#48154=CARTESIAN_POINT('Ctrl Pts',(-6.13029115401035,36.3141006191003,27.9297472329631));
#48155=CARTESIAN_POINT('Ctrl Pts',(-6.09518893192452,36.199864793481,27.9239443131969));
#48156=CARTESIAN_POINT('Ctrl Pts',(-6.06008361459922,36.085618894789,27.9181408817416));
#48157=CARTESIAN_POINT('Ctrl Pts',(-6.03000018301447,35.9698436786082,27.9123374502864));
#48158=CARTESIAN_POINT('Ctrl Pts',(-6.00505520043724,35.8530187855179,27.9065340188311));
#48159=CARTESIAN_POINT('Ctrl Pts',(-5.98010213067867,35.7361560177131,27.9007287058991));
#48160=CARTESIAN_POINT('Ctrl Pts',(-5.96029090822835,35.6182432953538,27.8949233929672));
#48161=CARTESIAN_POINT('Ctrl Pts',(-5.94568681023975,35.4997695062086,27.8891180800352));
#48162=CARTESIAN_POINT('Ctrl Pts',(-5.93106653992792,35.3811645212572,27.8833063384011));
#48163=CARTESIAN_POINT('Ctrl Pts',(-5.92166495405033,35.2619976348475,27.8774945967669));
#48164=CARTESIAN_POINT('Ctrl Pts',(-5.91749537731631,35.1427620599678,27.8716828551327));
#48165=CARTESIAN_POINT('Ctrl Pts',(-5.91332306213287,35.0234481748396,27.8658672965259));
#48166=CARTESIAN_POINT('Ctrl Pts',(-5.91438959577009,34.9040659187974,27.8600517379191));
#48167=CARTESIAN_POINT('Ctrl Pts',(-5.92065623087951,34.7851060416443,27.8542361793122));
#48168=CARTESIAN_POINT('Ctrl Pts',(-5.92693184288152,34.6659757556479,27.8484122899754));
#48169=CARTESIAN_POINT('Ctrl Pts',(-5.93842238513361,34.5472694612052,27.8425884006386));
#48170=CARTESIAN_POINT('Ctrl Pts',(-5.95503756801433,34.4294704882089,27.8367645113017));
#48171=CARTESIAN_POINT('Ctrl Pts',(-5.95944867244888,34.3981964675797,27.8352183481169));
#48172=CARTESIAN_POINT('Ctrl Pts',(-5.96422070095098,34.3669863273422,27.833672184932));
#48173=CARTESIAN_POINT('Ctrl Pts',(-5.96935137044259,34.3358489441046,27.8321260217471));
#48174=CARTESIAN_POINT('Ctrl Pts',(-5.98867604553686,34.2185699388332,27.8263023955636));
#48175=CARTESIAN_POINT('Ctrl Pts',(-6.0131547955719,34.1019459598726,27.8204787693801));
#48176=CARTESIAN_POINT('Ctrl Pts',(-6.04273187214429,33.9864646211121,27.8146551431966));
#48177=CARTESIAN_POINT('Ctrl Pts',(-6.07227163448797,33.8711289727844,27.8088388640583));
#48178=CARTESIAN_POINT('Ctrl Pts',(-6.10689682982483,33.7569334895309,27.80302258492));
#48179=CARTESIAN_POINT('Ctrl Pts',(-6.14650027428743,33.6443581358142,27.7972063057817));
#48180=CARTESIAN_POINT('Ctrl Pts',(-6.1860640773497,33.5318954653432,27.7913958484969));
#48181=CARTESIAN_POINT('Ctrl Pts',(-6.23059608170363,33.4210500812495,27.7855853912121));
#48182=CARTESIAN_POINT('Ctrl Pts',(-6.27993877937317,33.3122886755169,27.7797749339272));
#48183=CARTESIAN_POINT('Ctrl Pts',(-6.33114880464832,33.199411297514,27.7737445853961));
#48184=CARTESIAN_POINT('Ctrl Pts',(-6.38754071709162,33.0887791803389,27.7677142368649));
#48185=CARTESIAN_POINT('Ctrl Pts',(-6.44888258169824,32.980893741916,27.7616838883337));
#48186=CARTESIAN_POINT('Ctrl Pts',(-6.50792114793186,32.8770592458045,27.7558799706756));
#48187=CARTESIAN_POINT('Ctrl Pts',(-6.5715444214833,32.7757692666811,27.7500760530175));
#48188=CARTESIAN_POINT('Ctrl Pts',(-6.63949823731052,32.6774468998619,27.7442721353594));
#48189=CARTESIAN_POINT('Ctrl Pts',(-6.70744201668592,32.5791390547835,27.7384690749121));
#48190=CARTESIAN_POINT('Ctrl Pts',(-6.77971483427688,32.4837982861855,27.7326660144647));
#48191=CARTESIAN_POINT('Ctrl Pts',(-6.85601923051103,32.3918186564037,27.7268629540173));
#48192=CARTESIAN_POINT('Ctrl Pts',(-6.93233036422389,32.2998309050611,27.7210593811749));
#48193=CARTESIAN_POINT('Ctrl Pts',(-7.01267352362666,32.2112051968888,27.7152558083325));
#48194=CARTESIAN_POINT('Ctrl Pts',(-7.09671142810893,32.1263019524789,27.70945223549));
#48195=CARTESIAN_POINT('Ctrl Pts',(-7.18077658511862,32.0413711749217,27.7036467806156));
#48196=CARTESIAN_POINT('Ctrl Pts',(-7.2685385829815,31.9601655519409,27.6978413257411));
#48197=CARTESIAN_POINT('Ctrl Pts',(-7.35962429435116,31.883007678383,27.6920358708667));
#48198=CARTESIAN_POINT('Ctrl Pts',(-7.45081087175119,31.8057643621327,27.6862239871772));
#48199=CARTESIAN_POINT('Ctrl Pts',(-7.54532819768965,31.7325780065979,27.6804121034877));
#48200=CARTESIAN_POINT('Ctrl Pts',(-7.64277104928343,31.6637301257387,27.6746002197983));
#48201=CARTESIAN_POINT('Ctrl Pts',(-7.74027790067057,31.5948370260658,27.6687845189037));
#48202=CARTESIAN_POINT('Ctrl Pts',(-7.84071376164357,31.530288296142,27.6629688180091));
#48203=CARTESIAN_POINT('Ctrl Pts',(-7.94364692557595,31.4703205480799,27.6571531171144));
#48204=CARTESIAN_POINT('Ctrl Pts',(-8.04672752351718,31.4102669065589,27.6513290862311));
#48205=CARTESIAN_POINT('Ctrl Pts',(-8.15231220361358,31.3548075324376,27.6455050553477));
#48206=CARTESIAN_POINT('Ctrl Pts',(-8.25994721148222,31.3041318620422,27.6396810244644));
#48207=CARTESIAN_POINT('Ctrl Pts',(-8.28849729080766,31.2906901906167,27.6381362060358));
#48208=CARTESIAN_POINT('Ctrl Pts',(-8.3171915328134,31.2775848174412,27.6365913876072));
#48209=CARTESIAN_POINT('Ctrl Pts',(-8.3460212848029,31.2648186911912,27.6350465691787));
#48210=CARTESIAN_POINT('Ctrl Pts',(-8.45470265279246,31.2166934050185,27.6292229679152));
#48211=CARTESIAN_POINT('Ctrl Pts',(-8.56566144318004,31.1732378534696,27.6233993666517));
#48212=CARTESIAN_POINT('Ctrl Pts',(-8.67845927504702,31.1346727030831,27.6175757653883));
#48213=CARTESIAN_POINT('Ctrl Pts',(-8.79111479986565,31.0961562069361,27.6117595112475));
#48214=CARTESIAN_POINT('Ctrl Pts',(-8.90560436845581,31.0625179713262,27.6059432571067));
#48215=CARTESIAN_POINT('Ctrl Pts',(-9.02146780232413,31.033931450654,27.6001270029659));
#48216=CARTESIAN_POINT('Ctrl Pts',(-9.13721526030036,31.0053735442488,27.5943165707245));
#48217=CARTESIAN_POINT('Ctrl Pts',(-9.25433345359814,30.9818573905163,27.5885061384832));
#48218=CARTESIAN_POINT('Ctrl Pts',(-9.37234571834909,30.9635070788214,27.5826957062418));
#48219=CARTESIAN_POINT('Ctrl Pts',(-9.49482476356167,30.9444622053033,27.5766653483405));
#48220=CARTESIAN_POINT('Ctrl Pts',(-9.61826647477876,30.9309821007485,27.5706349904392));
#48221=CARTESIAN_POINT('Ctrl Pts',(-9.74212433676339,30.9231476428119,27.5646046325379));
#48222=CARTESIAN_POINT('Ctrl Pts',(-9.86133081644452,30.9156074016364,27.5588007398732));
#48223=CARTESIAN_POINT('Ctrl Pts',(-9.98092230995851,30.9132964462796,27.5529968472085));
#48224=CARTESIAN_POINT('Ctrl Pts',(-10.100405632154,30.9162341265651,27.5471929545439));
#48225=CARTESIAN_POINT('Ctrl Pts',(-10.2198713084547,30.9191713729992,27.5413899190271));
#48226=CARTESIAN_POINT('Ctrl Pts',(-10.3392284371046,30.9273557035237,27.5355868835104));
#48227=CARTESIAN_POINT('Ctrl Pts',(-10.4579843827478,30.9407543428416,27.5297838479936));
#48228=CARTESIAN_POINT('Ctrl Pts',(-10.576750816131,30.9541541654388,27.5239802999911));
#48229=CARTESIAN_POINT('Ctrl Pts',(-10.6949155551654,30.9727691666192,27.5181767519886));
#48230=CARTESIAN_POINT('Ctrl Pts',(-10.8119922730246,30.9965148247373,27.5123732039862));
#48231=CARTESIAN_POINT('Ctrl Pts',(-10.9291069600736,31.0202681838178,27.5065677738331));
#48232=CARTESIAN_POINT('Ctrl Pts',(-11.0451325242137,31.049155427883,27.50076234368));
#48233=CARTESIAN_POINT('Ctrl Pts',(-11.1595946251472,31.0830413194253,27.4949569135269));
#48234=CARTESIAN_POINT('Ctrl Pts',(-11.274183485032,31.1169647372757,27.4891450542568));
#48235=CARTESIAN_POINT('Ctrl Pts',(-11.38720503386,31.1558977362739,27.4833331949867));
#48236=CARTESIAN_POINT('Ctrl Pts',(-11.4982016966553,31.1996557161042,27.4775213357166));
#48237=CARTESIAN_POINT('Ctrl Pts',(-11.6092712644171,31.2434424371054,27.4717056590939));
#48238=CARTESIAN_POINT('Ctrl Pts',(-11.7183129253534,31.2920602844803,27.4658899824711));
#48239=CARTESIAN_POINT('Ctrl Pts',(-11.8248921418185,31.3452778941855,27.4600743058484));
#48240=CARTESIAN_POINT('Ctrl Pts',(-11.931624022648,31.3985717329421,27.4542502988344));
#48241=CARTESIAN_POINT('Ctrl Pts',(-12.0358860631754,31.4564782871829,27.4484262918204));
#48242=CARTESIAN_POINT('Ctrl Pts',(-12.1372710965806,31.5187218927926,27.4426022848063));
#48243=CARTESIAN_POINT('Ctrl Pts',(-12.1641676233916,31.5352345549763,27.441057228741));
#48244=CARTESIAN_POINT('Ctrl Pts',(-12.1908618429779,31.5520522309247,27.4395121726756));
#48245=CARTESIAN_POINT('Ctrl Pts',(-12.217346542732,31.5691692974683,27.4379671166102));
#48246=CARTESIAN_POINT('Ctrl Pts',(-12.3171719183238,31.6336864569078,27.4321435353173));
#48247=CARTESIAN_POINT('Ctrl Pts',(-12.4143400985931,31.7026681387707,27.4263199540244));
#48248=CARTESIAN_POINT('Ctrl Pts',(-12.5084262207643,31.7758686604014,27.4204963727315));
#48249=CARTESIAN_POINT('Ctrl Pts',(-12.6023936360806,31.8489768261829,27.4146801389518));
#48250=CARTESIAN_POINT('Ctrl Pts',(-12.6932864081474,31.9262929961999,27.4088639051721));
#48251=CARTESIAN_POINT('Ctrl Pts',(-12.7807072119933,32.0075273767052,27.4030476713923));
#48252=CARTESIAN_POINT('Ctrl Pts',(-12.8680405044135,32.0886804386212,27.3972372598756));
#48253=CARTESIAN_POINT('Ctrl Pts',(-12.951908445413,32.1737436317883,27.3914268483588));
#48254=CARTESIAN_POINT('Ctrl Pts',(-13.0319459604685,32.2623863141782,27.385616436842));
#48255=CARTESIAN_POINT('Ctrl Pts',(-13.1150133078971,32.3543845788666,27.3795860713087));
#48256=CARTESIAN_POINT('Ctrl Pts',(-13.1939541424458,32.450238416805,27.3735557057754));
#48257=CARTESIAN_POINT('Ctrl Pts',(-13.2684012350255,32.5495350712806,27.367525340242));
#48258=CARTESIAN_POINT('Ctrl Pts',(-13.3400521708365,32.6451022448201,27.3617214690796));
#48259=CARTESIAN_POINT('Ctrl Pts',(-13.4075405704582,32.7438579256658,27.3559175979173));
#48260=CARTESIAN_POINT('Ctrl Pts',(-13.4705799038275,32.8454002387569,27.3501137267549));
#48261=CARTESIAN_POINT('Ctrl Pts',(-13.533609924475,32.9469275511292,27.3443107129911));
#48262=CARTESIAN_POINT('Ctrl Pts',(-13.5921919706256,33.0512403302465,27.3385076992274));
#48263=CARTESIAN_POINT('Ctrl Pts',(-13.6460834093786,33.1579085875413,27.3327046854636));
#48264=CARTESIAN_POINT('Ctrl Pts',(-13.6999796053681,33.2645862609166,27.3269011594421));
#48265=CARTESIAN_POINT('Ctrl Pts',(-13.7491841865616,33.373619461399,27.3210976334205));
#48266=CARTESIAN_POINT('Ctrl Pts',(-13.7935012572056,33.4845551110054,27.315294107399));
#48267=CARTESIAN_POINT('Ctrl Pts',(-13.8378326988198,33.5955267344003,27.3094886994322));
#48268=CARTESIAN_POINT('Ctrl Pts',(-13.8772733264631,33.7084016548261,27.3036832914655));
#48269=CARTESIAN_POINT('Ctrl Pts',(-13.9116762321749,33.8227090187054,27.2978778834987));
#48270=CARTESIAN_POINT('Ctrl Pts',(-13.9461172357447,33.9371429668258,27.2920660466096));
#48271=CARTESIAN_POINT('Ctrl Pts',(-13.9755092638981,34.0530121335273,27.2862542097205));
#48272=CARTESIAN_POINT('Ctrl Pts',(-13.9997558844047,34.169832628219,27.2804423728314));
#48273=CARTESIAN_POINT('Ctrl Pts',(-14.0240184300848,34.2867298505785,27.2746267187295));
#48274=CARTESIAN_POINT('Ctrl Pts',(-14.0431287725431,34.4045792431493,27.2688110646276));
#48275=CARTESIAN_POINT('Ctrl Pts',(-14.0570422195955,34.5228905488052,27.2629954105257));
#48276=CARTESIAN_POINT('Ctrl Pts',(-14.0709755963022,34.6413713238538,27.2571714260672));
#48277=CARTESIAN_POINT('Ctrl Pts',(-14.0796971899385,34.7603149267955,27.2513474416087));
#48278=CARTESIAN_POINT('Ctrl Pts',(-14.0832143633154,34.8792297088905,27.2455234571501));
#48279=CARTESIAN_POINT('Ctrl Pts',(-14.0841475668188,34.9107810938712,27.2439781927807));
#48280=CARTESIAN_POINT('Ctrl Pts',(-14.0847146690769,34.9423304726006,27.2424329284112));
#48281=CARTESIAN_POINT('Ctrl Pts',(-14.0849164197748,34.9738687265078,27.2408876640418));
#48282=CARTESIAN_POINT('Ctrl Pts',(-14.0849718051389,34.9825267271777,27.2404634522263));
#48283=CARTESIAN_POINT('Ctrl Pts',(-14.0849996645293,34.9911849040951,27.2400392404109));
#48284=CARTESIAN_POINT('Ctrl Pts',(-14.0849999969885,34.9998431440964,27.2396150285955));
#48285=CARTESIAN_POINT('Origin',(-10.,35.,32.7603849714045));
#48286=CARTESIAN_POINT('',(-7.51282733495086,38.2405550657615,29.2969304734038));
#48287=CARTESIAN_POINT('',(-7.51282733495085,38.2405550657615,29.1925543226443));
#48288=CARTESIAN_POINT('',(-7.51282733495086,38.2405550657615,32.7603849714045));
#48289=CARTESIAN_POINT('',(-14.0823970704021,34.9955937245638,29.7396160303676));
#48290=CARTESIAN_POINT('Ctrl Pts',(-14.0849976427674,34.9956115396029,29.7396150285955));
#48291=CARTESIAN_POINT('Ctrl Pts',(-14.0851248516661,35.1140239221068,29.7338651219894));
#48292=CARTESIAN_POINT('Ctrl Pts',(-14.0800991461781,35.23251947308,29.7281152153833));
#48293=CARTESIAN_POINT('Ctrl Pts',(-14.069925823144,35.3506120278963,29.7223653087771));
#48294=CARTESIAN_POINT('Ctrl Pts',(-14.0597551855942,35.4686734094473,29.7166169199921));
#48295=CARTESIAN_POINT('Ctrl Pts',(-14.0444396668569,35.586331591759,29.710868531207));
#48296=CARTESIAN_POINT('Ctrl Pts',(-14.0240365959555,35.7031034592512,29.7051201424219));
#48297=CARTESIAN_POINT('Ctrl Pts',(-14.0036338790127,35.8198733009501,29.6993718533616));
#48298=CARTESIAN_POINT('Ctrl Pts',(-13.9781438571365,35.9357564482399,29.6936235643013));
#48299=CARTESIAN_POINT('Ctrl Pts',(-13.9476752271182,36.0502786778742,29.687875275241));
#48300=CARTESIAN_POINT('Ctrl Pts',(-13.9171996109861,36.1648271661664,29.6821256681627));
#48301=CARTESIAN_POINT('Ctrl Pts',(-13.8817432246565,36.2780137142396,29.6763760610845));
#48302=CARTESIAN_POINT('Ctrl Pts',(-13.8414647957863,36.389378718253,29.6706264540062));
#48303=CARTESIAN_POINT('Ctrl Pts',(-13.8011415409952,36.5008676605382,29.664870448182));
#48304=CARTESIAN_POINT('Ctrl Pts',(-13.7559856700422,36.6105306188601,29.6591144423578));
#48305=CARTESIAN_POINT('Ctrl Pts',(-13.7062043603838,36.7179273090186,29.6533584365337));
#48306=CARTESIAN_POINT('Ctrl Pts',(-13.656393756972,36.8253871966339,29.6475990435946));
#48307=CARTESIAN_POINT('Ctrl Pts',(-13.6019524871551,36.9305777917755,29.6418396506555));
#48308=CARTESIAN_POINT('Ctrl Pts',(-13.5431331597973,37.0330844576516,29.6360802577164));
#48309=CARTESIAN_POINT('Ctrl Pts',(-13.4842168562484,37.1357601276029,29.6303113691912));
#48310=CARTESIAN_POINT('Ctrl Pts',(-13.4209083020718,37.2357426795967,29.624542480666));
#48311=CARTESIAN_POINT('Ctrl Pts',(-13.3535030157968,37.3326471064098,29.6187735921407));
#48312=CARTESIAN_POINT('Ctrl Pts',(-13.303134059545,37.4050594512641,29.6144627597149));
#48313=CARTESIAN_POINT('Ctrl Pts',(-13.2504784154346,37.4757536320588,29.610151927289));
#48314=CARTESIAN_POINT('Ctrl Pts',(-13.1956731526218,37.5445821074613,29.6058410948631));
#48315=CARTESIAN_POINT('Ctrl Pts',(-13.1215708848067,37.6376451794332,29.6000124126795));
#48316=CARTESIAN_POINT('Ctrl Pts',(-13.0432813170809,37.7276176964846,29.5941837304958));
#48317=CARTESIAN_POINT('Ctrl Pts',(-12.9610914531482,37.8141006389418,29.5883550483122));
#48318=CARTESIAN_POINT('Ctrl Pts',(-12.8790055816135,37.9004741570961,29.5825337409873));
#48319=CARTESIAN_POINT('Ctrl Pts',(-12.7930295079769,37.9833665900373,29.5767124336624));
#48320=CARTESIAN_POINT('Ctrl Pts',(-12.7034913998388,38.0624106927383,29.5708911263375));
#48321=CARTESIAN_POINT('Ctrl Pts',(-12.6140433636273,38.1413752800824,29.565075675026));
#48322=CARTESIAN_POINT('Ctrl Pts',(-12.5210407253993,38.2164989707507,29.5592602237146));
#48323=CARTESIAN_POINT('Ctrl Pts',(-12.4248491102627,38.287450652475,29.5534447724031));
#48324=CARTESIAN_POINT('Ctrl Pts',(-12.3251341209551,38.3610012023275,29.5474163086486));
#48325=CARTESIAN_POINT('Ctrl Pts',(-12.2219923741619,38.4300679393296,29.5413878448941));
#48326=CARTESIAN_POINT('Ctrl Pts',(-12.115869891107,38.4943267740592,29.5353593811396));
#48327=CARTESIAN_POINT('Ctrl Pts',(-12.0136144202408,38.55624407201,29.5295505894295));
#48328=CARTESIAN_POINT('Ctrl Pts',(-11.9085920261414,38.6136975053864,29.5237417977195));
#48329=CARTESIAN_POINT('Ctrl Pts',(-11.8012314361141,38.666441096425,29.5179330060095));
#48330=CARTESIAN_POINT('Ctrl Pts',(-11.6938876777556,38.7191764184828,29.5121251249842));
#48331=CARTESIAN_POINT('Ctrl Pts',(-11.5842068181623,38.7672031871182,29.506317243959));
#48332=CARTESIAN_POINT('Ctrl Pts',(-11.4726412539763,38.8103218679118,29.5005093629338));
#48333=CARTESIAN_POINT('Ctrl Pts',(-11.3610669851957,38.8534439129213,29.4947010287647));
#48334=CARTESIAN_POINT('Ctrl Pts',(-11.247608099589,38.8916569618532,29.4888926945956));
#48335=CARTESIAN_POINT('Ctrl Pts',(-11.132735395391,38.9248102532515,29.4830843604265));
#48336=CARTESIAN_POINT('Ctrl Pts',(-11.0178267568282,38.9579739156295,29.4772742093001));
#48337=CARTESIAN_POINT('Ctrl Pts',(-10.9015038114156,38.986074559665,29.4714640581737));
#48338=CARTESIAN_POINT('Ctrl Pts',(-10.7842502614603,39.0090119141005,29.4656539070474));
#48339=CARTESIAN_POINT('Ctrl Pts',(-10.6668694190319,39.0319741697229,29.4598374483209));
#48340=CARTESIAN_POINT('Ctrl Pts',(-10.5485563555924,39.0497618685147,29.4540209895943));
#48341=CARTESIAN_POINT('Ctrl Pts',(-10.4298028153473,39.0623262473513,29.4482045308678));
#48342=CARTESIAN_POINT('Ctrl Pts',(-10.3109726770349,39.0748987304275,29.4423843204258));
#48343=CARTESIAN_POINT('Ctrl Pts',(-10.1917019019098,39.0822411583369,29.4365641099838));
#48344=CARTESIAN_POINT('Ctrl Pts',(-10.0724835403599,39.0843568816127,29.4307438995418));
#48345=CARTESIAN_POINT('Ctrl Pts',(-9.95309723424697,39.0864755853373,29.4249154900885));
#48346=CARTESIAN_POINT('Ctrl Pts',(-9.83376389507452,39.0833528986784,29.4190870806351));
#48347=CARTESIAN_POINT('Ctrl Pts',(-9.71497289432271,39.0750441162065,29.4132586711818));
#48348=CARTESIAN_POINT('Ctrl Pts',(-9.68442101642287,39.0729071790145,29.4117596615528));
#48349=CARTESIAN_POINT('Ctrl Pts',(-9.65390496521215,39.0704274626179,29.4102606519237));
#48350=CARTESIAN_POINT('Ctrl Pts',(-9.6234329543552,39.0676064534483,29.4087616422947));
#48351=CARTESIAN_POINT('Ctrl Pts',(-9.50487383801798,39.0566305990523,29.4029293636888));
#48352=CARTESIAN_POINT('Ctrl Pts',(-9.38661074311595,39.0404499089252,29.397097085083));
#48353=CARTESIAN_POINT('Ctrl Pts',(-9.26913529492874,39.0190871827918,29.3912648064771));
#48354=CARTESIAN_POINT('Ctrl Pts',(-9.15179756714227,38.9977495008973,29.3854393652467));
#48355=CARTESIAN_POINT('Ctrl Pts',(-9.0352460465635,38.9712419363312,29.3796139240163));
#48356=CARTESIAN_POINT('Ctrl Pts',(-8.9199682526141,38.9396391236557,29.3737884827859));
#48357=CARTESIAN_POINT('Ctrl Pts',(-8.8047986408493,38.9080659685682,29.3679685084276));
#48358=CARTESIAN_POINT('Ctrl Pts',(-8.69090076818878,38.8714071838209,29.3621485340693));
#48359=CARTESIAN_POINT('Ctrl Pts',(-8.5787523465093,38.8297885199378,29.356328559711));
#48360=CARTESIAN_POINT('Ctrl Pts',(-8.46668726322049,38.7882007832173,29.3505129102223));
#48361=CARTESIAN_POINT('Ctrl Pts',(-8.35636942347186,38.7416606445584,29.3446972607336));
#48362=CARTESIAN_POINT('Ctrl Pts',(-8.24826109381904,38.6903435889592,29.3388816112449));
#48363=CARTESIAN_POINT('Ctrl Pts',(-8.14019930221163,38.6390486241226,29.3330684652539));
#48364=CARTESIAN_POINT('Ctrl Pts',(-8.03434549466983,38.5829810088661,29.327255319263));
#48365=CARTESIAN_POINT('Ctrl Pts',(-7.93114120708155,38.5223640207912,29.321442173272));
#48366=CARTESIAN_POINT('Ctrl Pts',(-7.82794611936189,38.4617524362546,29.3156295454783));
#48367=CARTESIAN_POINT('Ctrl Pts',(-7.72740043409766,38.3965924885014,29.3098169176846));
#48368=CARTESIAN_POINT('Ctrl Pts',(-7.62991994784687,38.3271527687177,29.3040042898909));
#48369=CARTESIAN_POINT('Ctrl Pts',(-7.59037621104445,38.2989839925003,29.3016463510619));
#48370=CARTESIAN_POINT('Ctrl Pts',(-7.55133655523326,38.2701114467194,29.2992884122329));
#48371=CARTESIAN_POINT('Ctrl Pts',(-7.51282733495086,38.2405550657615,29.2969304734038));
#48372=CARTESIAN_POINT('',(-11.0579044229731,31.0543614925016,30.));
#48373=CARTESIAN_POINT('Ctrl Pts',(-11.057904422973,31.0543614925016,30.));
#48374=CARTESIAN_POINT('Ctrl Pts',(-12.3607928946041,31.403691892172,29.9343068491439));
#48375=CARTESIAN_POINT('Ctrl Pts',(-13.8213065450876,32.7806934417622,29.8475124055188));
#48376=CARTESIAN_POINT('Ctrl Pts',(-14.0838324696554,34.5614760231763,29.7607179618936));
#48377=CARTESIAN_POINT('Ctrl Pts',(-14.0807388749966,34.9955823652123,29.7396166691247));
#48378=CARTESIAN_POINT('',(-8.94137326277089,31.0545552302404,29.9999998972464));
#48379=CARTESIAN_POINT('Origin',(-10.,35.,30.));
#48380=CARTESIAN_POINT('',(-14.0849993157578,35.0023643727775,29.6353849714467));
#48381=CARTESIAN_POINT('Ctrl Pts',(-8.94137326277089,31.0545552302404,29.9999998972464));
#48382=CARTESIAN_POINT('Ctrl Pts',(-9.05557900702206,31.0239119792345,29.9942072258419));
#48383=CARTESIAN_POINT('Ctrl Pts',(-9.17130906545843,30.9981799216732,29.9884145544374));
#48384=CARTESIAN_POINT('Ctrl Pts',(-9.28810103205902,30.9775101169245,29.9826218830329));
#48385=CARTESIAN_POINT('Ctrl Pts',(-9.40474625781243,30.9568662823238,29.9768364897104));
#48386=CARTESIAN_POINT('Ctrl Pts',(-9.52245033541758,30.9412721240102,29.9710510963879));
#48387=CARTESIAN_POINT('Ctrl Pts',(-9.64073638462371,30.9308287508798,29.9652657030654));
#48388=CARTESIAN_POINT('Ctrl Pts',(-9.75890552637127,30.9203956994078,29.959486027709));
#48389=CARTESIAN_POINT('Ctrl Pts',(-9.87765508648077,30.9151033438613,29.9537063523527));
#48390=CARTESIAN_POINT('Ctrl Pts',(-9.99649934938507,30.9150014999458,29.9479266769964));
#48391=CARTESIAN_POINT('Ctrl Pts',(-10.115260739166,30.9148997270486,29.9421510319545));
#48392=CARTESIAN_POINT('Ctrl Pts',(-10.2341162885532,30.9199812664573,29.9363753869126));
#48393=CARTESIAN_POINT('Ctrl Pts',(-10.3525771683274,30.9302439458397,29.9305997418708));
#48394=CARTESIAN_POINT('Ctrl Pts',(-10.4709944600259,30.940502849035,29.9248262219967));
#48395=CARTESIAN_POINT('Ctrl Pts',(-10.5890169597165,30.955939066815,29.9190527021227));
#48396=CARTESIAN_POINT('Ctrl Pts',(-10.7061584327085,30.9764983822652,29.9132791822487));
#48397=CARTESIAN_POINT('Ctrl Pts',(-10.8232852272653,30.9970551215263,29.9075063858267));
#48398=CARTESIAN_POINT('Ctrl Pts',(-10.9395308077791,31.0227336104439,29.9017335894047));
#48399=CARTESIAN_POINT('Ctrl Pts',(-11.0544173397038,31.0534281871817,29.8959607929827));
#48400=CARTESIAN_POINT('Ctrl Pts',(-11.1693173531074,31.0841263658064,29.8901873191459));
#48401=CARTESIAN_POINT('Ctrl Pts',(-11.2828576018,31.1198416953922,29.8844138453092));
#48402=CARTESIAN_POINT('Ctrl Pts',(-11.3945743500606,31.1604183324022,29.8786403714724));
#48403=CARTESIAN_POINT('Ctrl Pts',(-11.5064001388795,31.2010345740303,29.8728612624662));
#48404=CARTESIAN_POINT('Ctrl Pts',(-11.6163984829982,31.2465214596229,29.86708215346));
#48405=CARTESIAN_POINT('Ctrl Pts',(-11.7241244467073,31.2966744820005,29.8613030444537));
#48406=CARTESIAN_POINT('Ctrl Pts',(-11.8319025585855,31.3468517825391,29.8555211378865));
#48407=CARTESIAN_POINT('Ctrl Pts',(-11.9374057320661,31.4016995289724,29.8497392313193));
#48408=CARTESIAN_POINT('Ctrl Pts',(-12.0402141148433,31.4609674534424,29.8439573247521));
#48409=CARTESIAN_POINT('Ctrl Pts',(-12.1431866646754,31.5203300184499,29.8381661854886));
#48410=CARTESIAN_POINT('Ctrl Pts',(-12.2434554767513,31.5841266426451,29.832375046225));
#48411=CARTESIAN_POINT('Ctrl Pts',(-12.34062969668,31.6520636769765,29.8265839069615));
#48412=CARTESIAN_POINT('Ctrl Pts',(-12.4324683408004,31.7162704709508,29.8211107436239));
#48413=CARTESIAN_POINT('Ctrl Pts',(-12.5215429394954,31.7841749336168,29.8156375802863));
#48414=CARTESIAN_POINT('Ctrl Pts',(-12.6075527664519,31.85549788199,29.8101644169487));
#48415=CARTESIAN_POINT('Ctrl Pts',(-12.6979865222769,31.9304893373405,29.804409740601));
#48416=CARTESIAN_POINT('Ctrl Pts',(-12.7853423440294,32.0095178940369,29.7986550642532));
#48417=CARTESIAN_POINT('Ctrl Pts',(-12.8692326967171,32.092298376365,29.7929003879054));
#48418=CARTESIAN_POINT('Ctrl Pts',(-12.9530188019921,32.1749759904749,29.7871528626793));
#48419=CARTESIAN_POINT('Ctrl Pts',(-13.0333477040205,32.2613959694969,29.7814053374532));
#48420=CARTESIAN_POINT('Ctrl Pts',(-13.1098641070867,32.351232317576,29.7756578122272));
#48421=CARTESIAN_POINT('Ctrl Pts',(-13.1876742137717,32.4425875766853,29.769813110528));
#48422=CARTESIAN_POINT('Ctrl Pts',(-13.2615413720246,32.5374755234182,29.7639684088288));
#48423=CARTESIAN_POINT('Ctrl Pts',(-13.3311299036824,32.6355130440637,29.7581237071296));
#48424=CARTESIAN_POINT('Ctrl Pts',(-13.3994485329896,32.7317615044294,29.7523856638158));
#48425=CARTESIAN_POINT('Ctrl Pts',(-13.4636431121346,32.8310452079152,29.746647620502));
#48426=CARTESIAN_POINT('Ctrl Pts',(-13.5234363744694,32.9329680420792,29.7409095771881));
#48427=CARTESIAN_POINT('Ctrl Pts',(-13.5832097718704,33.0348570147297,29.735173440207));
#48428=CARTESIAN_POINT('Ctrl Pts',(-13.6385845473066,33.1393830141318,29.7294373032259));
#48429=CARTESIAN_POINT('Ctrl Pts',(-13.689327483289,33.2461220906093,29.7237011662447));
#48430=CARTESIAN_POINT('Ctrl Pts',(-13.7400662411507,33.352852378302,29.7179655015712));
#48431=CARTESIAN_POINT('Ctrl Pts',(-13.7861737388538,33.4617950019341,29.7122298368976));
#48432=CARTESIAN_POINT('Ctrl Pts',(-13.8274636895596,33.5725033432253,29.7064941722241));
#48433=CARTESIAN_POINT('Ctrl Pts',(-13.8701221485458,33.6868809861062,29.7005684054926));
#48434=CARTESIAN_POINT('Ctrl Pts',(-13.9076379799982,33.8031429876553,29.6946426387612));
#48435=CARTESIAN_POINT('Ctrl Pts',(-13.939860989921,33.9207778819453,29.6887168720297));
#48436=CARTESIAN_POINT('Ctrl Pts',(-13.9710834695739,34.0347601915507,29.6829751014241));
#48437=CARTESIAN_POINT('Ctrl Pts',(-13.9973369048824,34.1500309688985,29.6772333308184));
#48438=CARTESIAN_POINT('Ctrl Pts',(-14.0185365826894,34.2661139505434,29.6714915602128));
#48439=CARTESIAN_POINT('Ctrl Pts',(-14.040755282028,34.3877767838648,29.6654737954184));
#48440=CARTESIAN_POINT('Ctrl Pts',(-14.0574222060512,34.5103313261811,29.6594560306241));
#48441=CARTESIAN_POINT('Ctrl Pts',(-14.0685010044489,34.6332240782187,29.6534382658297));
#48442=CARTESIAN_POINT('Ctrl Pts',(-14.0795798028465,34.7561168302564,29.6474205010354));
#48443=CARTESIAN_POINT('Ctrl Pts',(-14.0850705173113,34.8793472663617,29.6414027362411));
#48444=CARTESIAN_POINT('Ctrl Pts',(-14.0849993157578,35.0023643727775,29.6353849714467));
#48445=CARTESIAN_POINT('Ctrl Pts',(-14.0849993157573,35.0023643736406,29.6353849714045));
#48446=CARTESIAN_POINT('Ctrl Pts',(-14.0849113652874,35.1543190406916,29.6279516357298));
#48447=CARTESIAN_POINT('Ctrl Pts',(-14.0763451188053,35.3060182549354,29.6205183000551));
#48448=CARTESIAN_POINT('Ctrl Pts',(-14.0593832670936,35.4567630576578,29.6130849643803));
#48449=CARTESIAN_POINT('Ctrl Pts',(-14.0461086957647,35.5747379503874,29.6072675367608));
#48450=CARTESIAN_POINT('Ctrl Pts',(-14.0276650664714,35.6923278959856,29.6014501091414));
#48451=CARTESIAN_POINT('Ctrl Pts',(-14.0040820227916,35.8090439757872,29.5956326815219));
#48452=CARTESIAN_POINT('Ctrl Pts',(-13.9805290796663,35.9256110833537,29.5898226790592));
#48453=CARTESIAN_POINT('Ctrl Pts',(-13.9518498489588,36.0413061458505,29.5840126765965));
#48454=CARTESIAN_POINT('Ctrl Pts',(-13.9181257430916,36.1556451277631,29.5782026741339));
#48455=CARTESIAN_POINT('Ctrl Pts',(-13.8844358370561,36.2698681577824,29.5723985636319));
#48456=CARTESIAN_POINT('Ctrl Pts',(-13.8457113481323,36.3827374525738,29.5665944531299));
#48457=CARTESIAN_POINT('Ctrl Pts',(-13.8020846470484,36.4937795475501,29.5607903426279));
#48458=CARTESIAN_POINT('Ctrl Pts',(-13.756739739236,36.6091949568039,29.5547576413439));
#48459=CARTESIAN_POINT('Ctrl Pts',(-13.7060986387152,36.7226358434001,29.5487249400599));
#48460=CARTESIAN_POINT('Ctrl Pts',(-13.6503671389336,36.8335879447121,29.5426922387759));
#48461=CARTESIAN_POINT('Ctrl Pts',(-13.5968090770892,36.9402130943514,29.5368948030399));
#48462=CARTESIAN_POINT('Ctrl Pts',(-13.5385504059576,37.0445395351898,29.5310973673038));
#48463=CARTESIAN_POINT('Ctrl Pts',(-13.475822392104,37.1461322649241,29.5252999315678));
#48464=CARTESIAN_POINT('Ctrl Pts',(-13.4131040737471,37.2477092920733,29.5195033919069));
#48465=CARTESIAN_POINT('Ctrl Pts',(-13.3459180013724,37.346553100151,29.5137068522461));
#48466=CARTESIAN_POINT('Ctrl Pts',(-13.274540196362,37.4422554130167,29.5079103125853));
#48467=CARTESIAN_POINT('Ctrl Pts',(-13.2031564756587,37.5379656575567,29.5021132925153));
#48468=CARTESIAN_POINT('Ctrl Pts',(-13.1275805764068,37.6305335611139,29.4963162724454));
#48469=CARTESIAN_POINT('Ctrl Pts',(-13.0481300393714,37.7195823692401,29.4905192523754));
#48470=CARTESIAN_POINT('Ctrl Pts',(-12.9686540526691,37.80865970156,29.4847203753988));
#48471=CARTESIAN_POINT('Ctrl Pts',(-12.8853012324082,37.8942153914736,29.4789214984222));
#48472=CARTESIAN_POINT('Ctrl Pts',(-12.7984268784555,37.9759086017446,29.4731226214456));
#48473=CARTESIAN_POINT('Ctrl Pts',(-12.7114562804842,38.0576923160884,29.4673173201655));
#48474=CARTESIAN_POINT('Ctrl Pts',(-12.6209566598982,38.1356047289336,29.4615120188853));
#48475=CARTESIAN_POINT('Ctrl Pts',(-12.5273174902497,38.2093443728398,29.4557067176051));
#48476=CARTESIAN_POINT('Ctrl Pts',(-12.4336169181786,38.2831323703653,29.4498976095893));
#48477=CARTESIAN_POINT('Ctrl Pts',(-12.3367730289423,38.3527419116578,29.4440885015735));
#48478=CARTESIAN_POINT('Ctrl Pts',(-12.2372040492131,38.4179150138914,29.4382793935577));
#48479=CARTESIAN_POINT('Ctrl Pts',(-12.1374916958428,38.4831819616681,29.4324619207583));
#48480=CARTESIAN_POINT('Ctrl Pts',(-12.0350467707998,38.543999511847,29.4266444479589));
#48481=CARTESIAN_POINT('Ctrl Pts',(-11.9303119364292,38.6001556672009,29.4208269751595));
#48482=CARTESIAN_POINT('Ctrl Pts',(-11.9013775415724,38.6156695540793,29.4192198207103));
#48483=CARTESIAN_POINT('Ctrl Pts',(-11.8722684918198,38.6308279610645,29.4176126662611));
#48484=CARTESIAN_POINT('Ctrl Pts',(-11.8429943645596,38.6456270753057,29.4160055118119));
#48485=CARTESIAN_POINT('Ctrl Pts',(-11.7368983395956,38.6992623956694,29.4101808224181));
#48486=CARTESIAN_POINT('Ctrl Pts',(-11.6282883268288,38.7483487055701,29.4043561330244));
#48487=CARTESIAN_POINT('Ctrl Pts',(-11.5175910307645,38.792643202747,29.3985314436306));
#48488=CARTESIAN_POINT('Ctrl Pts',(-11.407033319077,38.8368818465291,29.3927140989116));
#48489=CARTESIAN_POINT('Ctrl Pts',(-11.2943939346871,38.8763405453162,29.3868967541926));
#48490=CARTESIAN_POINT('Ctrl Pts',(-11.1801237564454,38.9108225374559,29.3810794094736));
#48491=CARTESIAN_POINT('Ctrl Pts',(-11.0659679166969,38.9452700269888,29.3752678855772));
#48492=CARTESIAN_POINT('Ctrl Pts',(-10.9501849178431,38.9747505991847,29.3694563616807));
#48493=CARTESIAN_POINT('Ctrl Pts',(-10.8332446195773,38.9991159528008,29.3636448377843));
#48494=CARTESIAN_POINT('Ctrl Pts',(-10.7119091386374,39.0243970743912,29.3576148886784));
#48495=CARTESIAN_POINT('Ctrl Pts',(-10.589328073091,39.044170756343,29.3515849395726));
#48496=CARTESIAN_POINT('Ctrl Pts',(-10.466042848905,39.0583283582018,29.3455549904667));
#48497=CARTESIAN_POINT('Ctrl Pts',(-10.3473572312565,39.0719577589034,29.3397500106831));
#48498=CARTESIAN_POINT('Ctrl Pts',(-10.2280194980236,39.0803825800956,29.3339450308994));
#48499=CARTESIAN_POINT('Ctrl Pts',(-10.1085213539266,39.0835582664806,29.3281400511158));
#48500=CARTESIAN_POINT('Ctrl Pts',(-9.98904092901901,39.0867334819747,29.3223359320948));
#48501=CARTESIAN_POINT('Ctrl Pts',(-9.86940054845317,39.0846610997186,29.3165318130738));
#48502=CARTESIAN_POINT('Ctrl Pts',(-9.75009403409503,39.0773486493315,29.3107276940528));
#48503=CARTESIAN_POINT('Ctrl Pts',(-9.63077708468077,39.0700355593662,29.3049230673789));
#48504=CARTESIAN_POINT('Ctrl Pts',(-9.51179446694682,39.0574815149923,29.2991184407049));
#48505=CARTESIAN_POINT('Ctrl Pts',(-9.39363635173109,39.0397460472235,29.2933138140309));
#48506=CARTESIAN_POINT('Ctrl Pts',(-9.27544004699479,39.0220048472288,29.2875073112614));
#48507=CARTESIAN_POINT('Ctrl Pts',(-9.15806917818911,38.9990789538252,29.2817008084919));
#48508=CARTESIAN_POINT('Ctrl Pts',(-9.04200454416728,38.9710791614628,29.2758943057224));
#48509=CARTESIAN_POINT('Ctrl Pts',(-8.92581168937801,38.9430484367246,29.2700813883009));
#48510=CARTESIAN_POINT('Ctrl Pts',(-8.81092834683337,38.9099327200765,29.2642684708794));
#48511=CARTESIAN_POINT('Ctrl Pts',(-8.69782110222245,38.8718929631619,29.2584555534578));
#48512=CARTESIAN_POINT('Ctrl Pts',(-8.58463972000513,38.8338282725966,29.2526388258844));
#48513=CARTESIAN_POINT('Ctrl Pts',(-8.47323713413662,38.7908332606018,29.246822098311));
#48514=CARTESIAN_POINT('Ctrl Pts',(-8.36405932425061,38.7431167635312,29.2410053707375));
#48515=CARTESIAN_POINT('Ctrl Pts',(-8.25472550561882,38.6953320823593,29.2351803313984));
#48516=CARTESIAN_POINT('Ctrl Pts',(-8.14762317343606,38.6428126290242,29.2293552920593));
#48517=CARTESIAN_POINT('Ctrl Pts',(-8.04317324693783,38.5858128867106,29.2235302527202));
#48518=CARTESIAN_POINT('Ctrl Pts',(-8.01565368056036,38.5707950858879,29.2219955215613));
#48519=CARTESIAN_POINT('Ctrl Pts',(-7.98831807609793,38.5554665065085,29.2204607904023));
#48520=CARTESIAN_POINT('Ctrl Pts',(-7.96117377535177,38.5398322877909,29.2189260592434));
#48521=CARTESIAN_POINT('Ctrl Pts',(-7.85816140270912,38.4805005709941,29.2131017685561));
#48522=CARTESIAN_POINT('Ctrl Pts',(-7.75757564042123,38.4165731977983,29.2072774778688));
#48523=CARTESIAN_POINT('Ctrl Pts',(-7.65985336587902,38.3482739927927,29.2014531871815));
#48524=CARTESIAN_POINT('Ctrl Pts',(-7.61008379849843,38.3134894781927,29.1984868990024));
#48525=CARTESIAN_POINT('Ctrl Pts',(-7.56105664497159,38.2775717555271,29.1955206108233));
#48526=CARTESIAN_POINT('Ctrl Pts',(-7.51282733495086,38.2405550657615,29.1925543226443));
#48527=CARTESIAN_POINT('Origin',(-10.,35.,23.));
#48528=CARTESIAN_POINT('',(-13.1787500078856,36.1772652419347,17.9149433153638));
#48529=CARTESIAN_POINT('',(-13.1787500671536,36.1772650819042,17.5703580226472));
#48530=CARTESIAN_POINT('',(-13.1787500671536,36.1772650819043,23.));
#48531=CARTESIAN_POINT('',(-6.62123117139838,34.7273715616997,17.));
#48532=CARTESIAN_POINT('Ctrl Pts',(-13.1787500671536,36.1772650819042,17.5703580226472));
#48533=CARTESIAN_POINT('Ctrl Pts',(-13.1427559868796,36.2744532061821,17.5642606450182));
#48534=CARTESIAN_POINT('Ctrl Pts',(-13.1022540729216,36.3701148704846,17.5581632673893));
#48535=CARTESIAN_POINT('Ctrl Pts',(-13.0573974094917,36.4638053637467,17.5520658897603));
#48536=CARTESIAN_POINT('Ctrl Pts',(-13.0125843104849,36.5574048655711,17.5459744338544));
#48537=CARTESIAN_POINT('Ctrl Pts',(-12.9634250562128,36.6490366202576,17.5398829779485));
#48538=CARTESIAN_POINT('Ctrl Pts',(-12.9101211932366,36.7382749216321,17.5337915220426));
#48539=CARTESIAN_POINT('Ctrl Pts',(-12.8568511675345,36.8274565745633,17.5277039329908));
#48540=CARTESIAN_POINT('Ctrl Pts',(-12.7994419829177,36.9142474296897,17.521616343939));
#48541=CARTESIAN_POINT('Ctrl Pts',(-12.7381412063363,36.9982461801949,17.5155287548873));
#48542=CARTESIAN_POINT('Ctrl Pts',(-12.6768600667662,37.0822180226491,17.5094431159259));
#48543=CARTESIAN_POINT('Ctrl Pts',(-12.6116900644843,37.1633991936884,17.5033574769645));
#48544=CARTESIAN_POINT('Ctrl Pts',(-12.5429217250004,37.2414178912066,17.4972718380031));
#48545=CARTESIAN_POINT('Ctrl Pts',(-12.4741576889056,37.3194317064662,17.4911865798692));
#48546=CARTESIAN_POINT('Ctrl Pts',(-12.401796045861,37.3942831216331,17.4851013217353));
#48547=CARTESIAN_POINT('Ctrl Pts',(-12.3261665912132,37.4656346145412,17.4790160636014));
#48548=CARTESIAN_POINT('Ctrl Pts',(-12.2505223753453,37.5370000337045,17.4729296177578));
#48549=CARTESIAN_POINT('Ctrl Pts',(-12.1716093909688,37.604863880215,17.4668431719142));
#48550=CARTESIAN_POINT('Ctrl Pts',(-12.0897924734438,37.6689272152754,17.4607567260706));
#48551=CARTESIAN_POINT('Ctrl Pts',(-12.0078881301222,37.7330590054704,17.4546637765309));
#48552=CARTESIAN_POINT('Ctrl Pts',(-11.9230739945184,37.7933819118439,17.4485708269911));
#48553=CARTESIAN_POINT('Ctrl Pts',(-11.8357459700176,37.8496388887128,17.4424778774513));
#48554=CARTESIAN_POINT('Ctrl Pts',(-11.7483675492014,37.9059283310401,17.4363814117183));
#48555=CARTESIAN_POINT('Ctrl Pts',(-11.6584727190608,37.9581469561964,17.4302849459853));
#48556=CARTESIAN_POINT('Ctrl Pts',(-11.5664824782971,38.0060834498876,17.4241884802523));
#48557=CARTESIAN_POINT('Ctrl Pts',(-11.4743456381263,38.0540963371342,17.4180822989423));
#48558=CARTESIAN_POINT('Ctrl Pts',(-11.380107105204,38.0978132841681,17.4119761176324));
#48559=CARTESIAN_POINT('Ctrl Pts',(-11.2842084864572,38.1370708671962,17.4058699363224));
#48560=CARTESIAN_POINT('Ctrl Pts',(-11.2229005725148,38.1621682101333,17.4019662592606));
#48561=CARTESIAN_POINT('Ctrl Pts',(-11.1609145333314,38.1854439917115,17.3980625821987));
#48562=CARTESIAN_POINT('Ctrl Pts',(-11.0983685544785,38.2068663179236,17.3941589051368));
#48563=CARTESIAN_POINT('Ctrl Pts',(-11.0015155370981,38.2400389849919,17.3881140256857));
#48564=CARTESIAN_POINT('Ctrl Pts',(-10.902977197853,38.2688819196769,17.3820691462345));
#48565=CARTESIAN_POINT('Ctrl Pts',(-10.8031806010433,38.2932212170772,17.3760242667834));
#48566=CARTESIAN_POINT('Ctrl Pts',(-10.7035168525737,38.3175281142219,17.3699874342218));
#48567=CARTESIAN_POINT('Ctrl Pts',(-10.6025985948985,38.3373431845761,17.3639506016603));
#48568=CARTESIAN_POINT('Ctrl Pts',(-10.5008707652887,38.3525413552974,17.3579137690988));
#48569=CARTESIAN_POINT('Ctrl Pts',(-10.3992478574947,38.3677238506653,17.3518831629105));
#48570=CARTESIAN_POINT('Ctrl Pts',(-10.2968174665736,38.3782988468126,17.3458525567222));
#48571=CARTESIAN_POINT('Ctrl Pts',(-10.1940365532007,38.3841919092336,17.3398219505339));
#48572=CARTESIAN_POINT('Ctrl Pts',(-10.0913245511466,38.3900810205445,17.3337953876744));
#48573=CARTESIAN_POINT('Ctrl Pts',(-9.98826292812799,38.3912944108315,17.3277688248149));
#48574=CARTESIAN_POINT('Ctrl Pts',(-9.88531472849353,38.3878093734742,17.3217422619554));
#48575=CARTESIAN_POINT('Ctrl Pts',(-9.78240185029908,38.3843255318302,17.3157177668045));
#48576=CARTESIAN_POINT('Ctrl Pts',(-9.67960275408466,38.3761464790843,17.3096932716536));
#48577=CARTESIAN_POINT('Ctrl Pts',(-9.5773804931766,38.3633016241414,17.3036687765027));
#48578=CARTESIAN_POINT('Ctrl Pts',(-9.47516557914334,38.3504576923785,17.2976447143417));
#48579=CARTESIAN_POINT('Ctrl Pts',(-9.37352785126157,38.3329486791751,17.2916206521807));
#48580=CARTESIAN_POINT('Ctrl Pts',(-9.27292421516466,38.3108557603143,17.2855965900198));
#48581=CARTESIAN_POINT('Ctrl Pts',(-9.17230052182162,38.2887584368103,17.2795713268476));
#48582=CARTESIAN_POINT('Ctrl Pts',(-9.07271175622782,38.2620754860212,17.2735460636754));
#48583=CARTESIAN_POINT('Ctrl Pts',(-8.97460260719551,38.2309387566665,17.2675208005032));
#48584=CARTESIAN_POINT('Ctrl Pts',(-8.87637753594343,38.1997652372793,17.2614884180981));
#48585=CARTESIAN_POINT('Ctrl Pts',(-8.77963598915772,38.1641275636369,17.255456035693));
#48586=CARTESIAN_POINT('Ctrl Pts',(-8.68480545078267,38.1242068369762,17.2494236532879));
#48587=CARTESIAN_POINT('Ctrl Pts',(-8.58991797440138,38.0842621411742,17.2433876489291));
#48588=CARTESIAN_POINT('Ctrl Pts',(-8.49694418404904,38.0400294616795,17.2373516445702));
#48589=CARTESIAN_POINT('Ctrl Pts',(-8.40628759282379,37.9917362560414,17.2313156402113));
#48590=CARTESIAN_POINT('Ctrl Pts',(-8.31546419781163,37.9433541932174,17.2252685298934));
#48591=CARTESIAN_POINT('Ctrl Pts',(-8.22696689339884,37.8908969041228,17.2192214195756));
#48592=CARTESIAN_POINT('Ctrl Pts',(-8.14117103419852,37.8346357682068,17.2131743092577));
#48593=CARTESIAN_POINT('Ctrl Pts',(-8.06505357281228,37.7847212982015,17.2078093570279));
#48594=CARTESIAN_POINT('Ctrl Pts',(-7.99106216092855,37.731813522163,17.2024444047982));
#48595=CARTESIAN_POINT('Ctrl Pts',(-7.91943573511002,37.6761273142664,17.1970794525685));
#48596=CARTESIAN_POINT('Ctrl Pts',(-7.83581618354862,37.6111170100491,17.1908161929618));
#48597=CARTESIAN_POINT('Ctrl Pts',(-7.75512934647832,37.5420931533284,17.1845529333551));
#48598=CARTESIAN_POINT('Ctrl Pts',(-7.67777110567854,37.469343642525,17.1782896737485));
#48599=CARTESIAN_POINT('Ctrl Pts',(-7.60052564249751,37.3967001904493,17.1720355451083));
#48600=CARTESIAN_POINT('Ctrl Pts',(-7.52659940702115,37.3203421665363,17.1657814164681));
#48601=CARTESIAN_POINT('Ctrl Pts',(-7.45635611458709,37.2405983233729,17.1595272878279));
#48602=CARTESIAN_POINT('Ctrl Pts',(-7.38619919224281,37.1609525320328,17.1532808491697));
#48603=CARTESIAN_POINT('Ctrl Pts',(-7.31971646168714,37.077929507357,17.1470344105115));
#48604=CARTESIAN_POINT('Ctrl Pts',(-7.25723519115291,36.991895144291,17.1407879718533));
#48605=CARTESIAN_POINT('Ctrl Pts',(-7.1948270975312,36.9059615430854,17.1345488489089));
#48606=CARTESIAN_POINT('Ctrl Pts',(-7.13641136175374,36.817023952268,17.1283097259645));
#48607=CARTESIAN_POINT('Ctrl Pts',(-7.0822748183824,36.7254810422182,17.1220706030201));
#48608=CARTESIAN_POINT('Ctrl Pts',(-7.0281753355621,36.6340008002016,17.1158357512265));
#48609=CARTESIAN_POINT('Ctrl Pts',(-6.97834941786856,36.5399191321524,17.1096008994328));
#48610=CARTESIAN_POINT('Ctrl Pts',(-6.93304034137542,36.4436632276502,17.1033660476391));
#48611=CARTESIAN_POINT('Ctrl Pts',(-6.88775292182805,36.3474533317861,17.0971341759954));
#48612=CARTESIAN_POINT('Ctrl Pts',(-6.84697821549959,36.249071629913,17.0909023043518));
#48613=CARTESIAN_POINT('Ctrl Pts',(-6.8109130642717,36.1489689198873,17.0846704327082));
#48614=CARTESIAN_POINT('Ctrl Pts',(-6.77485770566963,36.048893390349,17.0784402531796));
#48615=CARTESIAN_POINT('Ctrl Pts',(-6.74350949055321,35.9470981596222,17.0722100736511));
#48616=CARTESIAN_POINT('Ctrl Pts',(-6.71701651636321,35.8440524324164,17.0659798941226));
#48617=CARTESIAN_POINT('Ctrl Pts',(-6.69051805353856,35.740985356896,17.0597484238677));
#48618=CARTESIAN_POINT('Ctrl Pts',(-6.66887694611004,35.6366676536819,17.0535169536129));
#48619=CARTESIAN_POINT('Ctrl Pts',(-6.65219090412263,35.5315819034361,17.047285483358));
#48620=CARTESIAN_POINT('Ctrl Pts',(-6.63550340623277,35.4264869841735,17.0410534693905));
#48621=CARTESIAN_POINT('Ctrl Pts',(-6.62377189134541,35.3206242807345,17.034821455423));
#48622=CARTESIAN_POINT('Ctrl Pts',(-6.61704244698939,35.2144836987476,17.0285894414554));
#48623=CARTESIAN_POINT('Ctrl Pts',(-6.61030846998724,35.1082716253162,17.0223532298881));
#48624=CARTESIAN_POINT('Ctrl Pts',(-6.60858331255194,35.0017816995389,17.0161170183208));
#48625=CARTESIAN_POINT('Ctrl Pts',(-6.61186097188341,34.8955060353267,17.0098808067535));
#48626=CARTESIAN_POINT('Ctrl Pts',(-6.61359203986214,34.8393774445761,17.0065872045023));
#48627=CARTESIAN_POINT('Ctrl Pts',(-6.61671768475108,34.7833086021908,17.0032936022512));
#48628=CARTESIAN_POINT('Ctrl Pts',(-6.62123117139838,34.7273715616998,17.));
#48629=CARTESIAN_POINT('',(-13.1787500671536,36.1772650819043,17.));
#48630=CARTESIAN_POINT('Origin',(-10.,35.,17.));
#48631=CARTESIAN_POINT('',(-13.1787500671536,36.1772650819043,16.));
#48632=CARTESIAN_POINT('',(-13.1787500671536,36.1772650819043,23.));
#48633=CARTESIAN_POINT('Origin',(-10.,35.,16.));
#48634=CARTESIAN_POINT('',(-10.7859693978642,31.6996294197336,16.9983166722812));
#48635=CARTESIAN_POINT('Origin',(-10.,35.,17.));
#48636=CARTESIAN_POINT('Ctrl Pts',(-10.7851701022683,31.7024383291583,16.996642740892));
#48637=CARTESIAN_POINT('Ctrl Pts',(-10.7411264267437,31.6919512539592,16.999386876595));
#48638=CARTESIAN_POINT('Ctrl Pts',(-10.6968789035782,31.6823480701864,17.0021729732053));
#48639=CARTESIAN_POINT('Ctrl Pts',(-10.4988382553133,31.6435031285275,17.0147342295983));
#48640=CARTESIAN_POINT('Ctrl Pts',(-10.3433284096488,31.6240511354772,17.0248328987275));
#48641=CARTESIAN_POINT('Ctrl Pts',(-10.021322125722,31.6062561466042,17.045626997098));
#48642=CARTESIAN_POINT('Ctrl Pts',(-9.85514091465291,31.6092808843973,17.0562905526885));
#48643=CARTESIAN_POINT('Ctrl Pts',(-9.59130494280269,31.6335234341404,17.0728388515459));
#48644=CARTESIAN_POINT('Ctrl Pts',(-9.49320747682181,31.6468879567694,17.0789100101203));
#48645=CARTESIAN_POINT('Ctrl Pts',(-9.35840574527622,31.6713053283894,17.0871363837311));
#48646=CARTESIAN_POINT('Ctrl Pts',(-9.32109954833055,31.678713237895,17.0894007906279));
#48647=CARTESIAN_POINT('Ctrl Pts',(-9.25714978418302,31.6925343532475,17.0932628810753));
#48648=CARTESIAN_POINT('Ctrl Pts',(-9.23044539200801,31.6986455480178,17.0948697313219));
#48649=CARTESIAN_POINT('Ctrl Pts',(-9.17591691225517,31.7118217782151,17.098139777934));
#48650=CARTESIAN_POINT('Ctrl Pts',(-9.14810257201344,31.7189178921617,17.0998018599688));
#48651=CARTESIAN_POINT('Ctrl Pts',(-9.07702610942875,31.7380159989879,17.1040358879454));
#48652=CARTESIAN_POINT('Ctrl Pts',(-9.03390552350392,31.7505258659306,17.1065918591574));
#48653=CARTESIAN_POINT('Ctrl Pts',(-8.81646979273867,31.818318018793,17.1194352130547));
#48654=CARTESIAN_POINT('Ctrl Pts',(-8.64657820423122,31.8867857793393,17.1293003925232));
#48655=CARTESIAN_POINT('Ctrl Pts',(-8.35934160216759,32.0305263578168,17.1464422259585));
#48656=CARTESIAN_POINT('Ctrl Pts',(-8.23956527355586,32.0999308126459,17.1537539082429));
#48657=CARTESIAN_POINT('Ctrl Pts',(-8.06417273695908,32.2164411131496,17.1651453164485));
#48658=CARTESIAN_POINT('Ctrl Pts',(-8.00527557065218,32.2583397943134,17.1690994156838));
#48659=CARTESIAN_POINT('Ctrl Pts',(-7.9096309651066,32.3310942205926,17.175815982098));
#48660=CARTESIAN_POINT('Ctrl Pts',(-7.8721176974738,32.3609059877608,17.1785303817331));
#48661=CARTESIAN_POINT('Ctrl Pts',(-7.81948420685802,32.4045856350584,17.1824749404527));
#48662=CARTESIAN_POINT('Ctrl Pts',(-7.80383698835832,32.4178123941095,17.1836653466823));
#48663=CARTESIAN_POINT('Ctrl Pts',(-7.77685357372822,32.4410444290983,17.1857511697483));
#48664=CARTESIAN_POINT('Ctrl Pts',(-7.76546280953573,32.4509850560138,17.186642134439));
#48665=CARTESIAN_POINT('Ctrl Pts',(-7.74059935982598,32.4729779299354,17.1886106717852));
#48666=CARTESIAN_POINT('Ctrl Pts',(-7.72715655682884,32.4850617410864,17.1896903936014));
#48667=CARTESIAN_POINT('Ctrl Pts',(-7.68771597842631,32.5210895826394,17.1929024025501));
#48668=CARTESIAN_POINT('Ctrl Pts',(-7.66199607375009,32.5453326733591,17.1950545426587));
#48669=CARTESIAN_POINT('Ctrl Pts',(-7.50555211679663,32.6974832505138,17.2084799205615));
#48670=CARTESIAN_POINT('Ctrl Pts',(-7.38498718494906,32.835386398258,17.2202835065605));
#48671=CARTESIAN_POINT('Ctrl Pts',(-7.18123271787017,33.1104549616444,17.2423263602993));
#48672=CARTESIAN_POINT('Ctrl Pts',(-7.09547533081672,33.2451286740339,17.2525469084595));
#48673=CARTESIAN_POINT('Ctrl Pts',(-6.97367055807644,33.469968232975,17.2684982720421));
#48674=CARTESIAN_POINT('Ctrl Pts',(-6.93144998863293,33.5565074950471,17.2743984365352));
#48675=CARTESIAN_POINT('Ctrl Pts',(-6.87798031957433,33.679090023124,17.2824270095669));
#48676=CARTESIAN_POINT('Ctrl Pts',(-6.86356451819029,33.7136941698809,17.284658445714));
#48677=CARTESIAN_POINT('Ctrl Pts',(-6.83970828396745,33.7737465691577,17.2884724309912));
#48678=CARTESIAN_POINT('Ctrl Pts',(-6.82999426406078,33.7990816411739,17.2900638451231));
#48679=CARTESIAN_POINT('Ctrl Pts',(-6.81069030079557,33.8512951102679,17.2933085782584));
#48680=CARTESIAN_POINT('Ctrl Pts',(-6.80113347061025,33.8781834908117,17.2949607148208));
#48681=CARTESIAN_POINT('Ctrl Pts',(-6.77744749324618,33.9475896671186,17.2991791018446));
#48682=CARTESIAN_POINT('Ctrl Pts',(-6.76381944918456,33.9902733672679,17.3017291516867));
#48683=CARTESIAN_POINT('Ctrl Pts',(-6.70058920045596,34.202763963745,17.3142250995888));
#48684=CARTESIAN_POINT('Ctrl Pts',(-6.66348371290786,34.3760085691405,17.3237717318427));
#48685=CARTESIAN_POINT('Ctrl Pts',(-6.61570910217244,34.7338105861568,17.3429884947556));
#48686=CARTESIAN_POINT('Ctrl Pts',(-6.60625019359733,34.9179185846505,17.3526186824546));
#48687=CARTESIAN_POINT('Ctrl Pts',(-6.61349238013712,35.1587867714413,17.3657576428875));
#48688=CARTESIAN_POINT('Ctrl Pts',(-6.61663722798599,35.2156451851466,17.3689000751842));
#48689=CARTESIAN_POINT('Ctrl Pts',(-6.62445738252534,35.3126465183482,17.3743701434751));
#48690=CARTESIAN_POINT('Ctrl Pts',(-6.62842133460257,35.3528353921515,17.3766686402334));
#48691=CARTESIAN_POINT('Ctrl Pts',(-6.63529971133893,35.4117723167526,17.380099017414));
#48692=CARTESIAN_POINT('Ctrl Pts',(-6.6376552271799,35.4305834016102,17.3812028673973));
#48693=CARTESIAN_POINT('Ctrl Pts',(-6.64194964881517,35.4626915286908,17.3831038201127));
#48694=CARTESIAN_POINT('Ctrl Pts',(-6.64381002726752,35.4759983936192,17.3838966491269));
#48695=CARTESIAN_POINT('Ctrl Pts',(-6.64833952165301,35.5070493591057,17.3857586777808));
#48696=CARTESIAN_POINT('Ctrl Pts',(-6.65107038291607,35.5247831959168,17.3868311454087));
#48697=CARTESIAN_POINT('Ctrl Pts',(-6.65943965434514,35.5764041635967,17.3899776426211));
#48698=CARTESIAN_POINT('Ctrl Pts',(-6.66545241734355,35.6102273395331,17.3920703653927));
#48699=CARTESIAN_POINT('Ctrl Pts',(-6.7083393281207,35.83187215234,17.4059632924908));
#48700=CARTESIAN_POINT('Ctrl Pts',(-6.76054939127837,36.0163615608002,17.4183557835258));
#48701=CARTESIAN_POINT('Ctrl Pts',(-6.88280270999425,36.3407449535208,17.4407017782544));
#48702=CARTESIAN_POINT('Ctrl Pts',(-6.94748646663371,36.4821215789602,17.4506519561146));
#48703=CARTESIAN_POINT('Ctrl Pts',(-7.06686039490361,36.7017830791203,17.4662438555088));
#48704=CARTESIAN_POINT('Ctrl Pts',(-7.11554988678168,36.7830658251065,17.4720479250566));
#48705=CARTESIAN_POINT('Ctrl Pts',(-7.18793324557844,36.8931607855543,17.4799555951851));
#48706=CARTESIAN_POINT('Ctrl Pts',(-7.20878951179149,36.9237778889776,17.4821601563955));
#48707=CARTESIAN_POINT('Ctrl Pts',(-7.24560880572158,36.9759691057734,17.4859290340767));
#48708=CARTESIAN_POINT('Ctrl Pts',(-7.26133352942859,36.9977063805835,17.4875021059801));
#48709=CARTESIAN_POINT('Ctrl Pts',(-7.29412165692374,37.0419166143423,17.4907094090485));
#48710=CARTESIAN_POINT('Ctrl Pts',(-7.31121094112717,37.0643678293169,17.4923424739859));
#48711=CARTESIAN_POINT('Ctrl Pts',(-7.35582814436308,37.1214900054473,17.4965104496895));
#48712=CARTESIAN_POINT('Ctrl Pts',(-7.38375895943528,37.1558403742924,17.4990293864204));
#48713=CARTESIAN_POINT('Ctrl Pts',(-7.51973144955706,37.3165285553142,17.5108904132821));
#48714=CARTESIAN_POINT('Ctrl Pts',(-7.63630078101025,37.435358478565,17.5198810883679));
#48715=CARTESIAN_POINT('Ctrl Pts',(-7.94683299614805,37.7085200222348,17.541911912794));
#48716=CARTESIAN_POINT('Ctrl Pts',(-8.14983486907573,37.8510416720303,17.5547004283059));
#48717=CARTESIAN_POINT('Ctrl Pts',(-8.40493313337227,37.9913358579405,17.5710015945399));
#48718=CARTESIAN_POINT('Ctrl Pts',(-8.4437668968697,38.0117215469657,17.5734903196969));
#48719=CARTESIAN_POINT('Ctrl Pts',(-8.50039306296983,38.0400597211273,17.577145143416));
#48720=CARTESIAN_POINT('Ctrl Pts',(-8.51787715361973,38.0486219677823,17.5782771145932));
#48721=CARTESIAN_POINT('Ctrl Pts',(-8.5487213565273,38.0633988398235,17.5802818418297));
#48722=CARTESIAN_POINT('Ctrl Pts',(-8.56204971772011,38.0696776903511,17.5811507330038));
#48723=CARTESIAN_POINT('Ctrl Pts',(-8.59184229922979,38.0834760480281,17.5830989460335));
#48724=CARTESIAN_POINT('Ctrl Pts',(-8.60832596063734,38.0909506603511,17.584180758451));
#48725=CARTESIAN_POINT('Ctrl Pts',(-8.65672487555514,38.1124318079675,17.5873668344585));
#48726=CARTESIAN_POINT('Ctrl Pts',(-8.68879634279656,38.1260781476977,17.5894903052495));
#48727=CARTESIAN_POINT('Ctrl Pts',(-8.88737486137295,38.2069795294698,17.6026882856611));
#48728=CARTESIAN_POINT('Ctrl Pts',(-9.05878728590457,38.2614048484046,17.6142793958227));
#48729=CARTESIAN_POINT('Ctrl Pts',(-9.39241175343074,38.338830877452,17.6363558036028));
#48730=CARTESIAN_POINT('Ctrl Pts',(-9.55359663419627,38.3641770308464,17.6468164142448));
#48731=CARTESIAN_POINT('Ctrl Pts',(-9.81317234771921,38.3860023173606,17.6630794146817));
#48732=CARTESIAN_POINT('Ctrl Pts',(-9.91066852454422,38.3899762481629,17.6690615626971));
#48733=CARTESIAN_POINT('Ctrl Pts',(-10.045797604665,38.3896490416361,17.6771748634721));
#48734=CARTESIAN_POINT('Ctrl Pts',(-10.0833841255746,38.3889327677104,17.679412796351));
#48735=CARTESIAN_POINT('Ctrl Pts',(-10.1480187572473,38.3866250229969,17.6832302743005));
#48736=CARTESIAN_POINT('Ctrl Pts',(-10.1750733932721,38.3853342477687,17.6848188640769));
#48737=CARTESIAN_POINT('Ctrl Pts',(-10.2304300624439,38.3820277825385,17.6880511882454));
#48738=CARTESIAN_POINT('Ctrl Pts',(-10.2587281194445,38.3799807346645,17.689693829833));
#48739=CARTESIAN_POINT('Ctrl Pts',(-10.3311383734469,38.3738279297547,17.6938740795105));
#48740=CARTESIAN_POINT('Ctrl Pts',(-10.3752025331188,38.369212198078,17.6963959332254));
#48741=CARTESIAN_POINT('Ctrl Pts',(-10.5814067108247,38.3435164725506,17.708111051368));
#48742=CARTESIAN_POINT('Ctrl Pts',(-10.7419810360386,38.3115869573673,17.7169691838201));
#48743=CARTESIAN_POINT('Ctrl Pts',(-11.085676112541,38.2169776767717,17.7359949379022));
#48744=CARTESIAN_POINT('Ctrl Pts',(-11.2669922509377,38.1499780525723,17.7460736057422));
#48745=CARTESIAN_POINT('Ctrl Pts',(-11.5191354814177,38.0314961386416,17.761251343863));
#48746=CARTESIAN_POINT('Ctrl Pts',(-11.5952419293796,37.9921467849032,17.7660006966031));
#48747=CARTESIAN_POINT('Ctrl Pts',(-11.6913588870011,37.9377415739088,17.7723209494345));
#48748=CARTESIAN_POINT('Ctrl Pts',(-11.7128117728121,37.9252856602422,17.7737530311017));
#48749=CARTESIAN_POINT('Ctrl Pts',(-11.7477043593022,37.9045110239774,17.7761207762636));
#48750=CARTESIAN_POINT('Ctrl Pts',(-11.7612263902153,37.8963315414164,17.7770479641744));
#48751=CARTESIAN_POINT('Ctrl Pts',(-11.7883066574618,37.8796909157193,17.7789252460971));
#48752=CARTESIAN_POINT('Ctrl Pts',(-11.8018632161967,37.8712278555233,17.7798754465478));
#48753=CARTESIAN_POINT('Ctrl Pts',(-11.8370991385832,37.8488830287239,17.7823714659029));
#48754=CARTESIAN_POINT('Ctrl Pts',(-11.858680703033,37.8348498572842,17.7839264790033));
#48755=CARTESIAN_POINT('Ctrl Pts',(-11.9531431078626,37.771884371514,17.7908420491013));
#48756=CARTESIAN_POINT('Ctrl Pts',(-12.0242622899506,37.7203806252843,17.7963383554722));
#48757=CARTESIAN_POINT('Ctrl Pts',(-12.2646849354758,37.5316176728037,17.8157459863821));
#48758=CARTESIAN_POINT('Ctrl Pts',(-12.422700858004,37.3808428703411,17.8299712066777));
#48759=CARTESIAN_POINT('Ctrl Pts',(-12.6570714645664,37.1095368911862,17.8527165106462));
#48760=CARTESIAN_POINT('Ctrl Pts',(-12.7422859494787,36.9975110474234,17.8614586231315));
#48761=CARTESIAN_POINT('Ctrl Pts',(-12.8435911066558,36.8455776319802,17.8724714955442));
#48762=CARTESIAN_POINT('Ctrl Pts',(-12.8662286105954,36.8102212479383,17.8749796047546));
#48763=CARTESIAN_POINT('Ctrl Pts',(-12.9027948517976,36.7507038531411,17.8791133768719));
#48764=CARTESIAN_POINT('Ctrl Pts',(-12.9170922270035,36.7267758804843,17.8807521934373));
#48765=CARTESIAN_POINT('Ctrl Pts',(-12.9446663129053,36.6793080578827,17.8839590674971));
#48766=CARTESIAN_POINT('Ctrl Pts',(-12.9579598466322,36.6557804368797,17.8855276397676));
#48767=CARTESIAN_POINT('Ctrl Pts',(-12.9867520941661,36.6033687299806,17.8889772226961));
#48768=CARTESIAN_POINT('Ctrl Pts',(-13.0021161604321,36.574413548406,17.8908534563623));
#48769=CARTESIAN_POINT('Ctrl Pts',(-13.0544872020102,36.4721598214295,17.8973813807106));
#48770=CARTESIAN_POINT('Ctrl Pts',(-13.0892503388676,36.3977411699346,17.9019575345575));
#48771=CARTESIAN_POINT('Ctrl Pts',(-13.1415553572831,36.2742596460579,17.9093185834347));
#48772=CARTESIAN_POINT('Ctrl Pts',(-13.1607162010614,36.2259585707977,17.9121421215577));
#48773=CARTESIAN_POINT('Ctrl Pts',(-13.1787500078856,36.1772652419345,17.9149433153638));
#48774=CARTESIAN_POINT('Origin',(-10.,35.,23.));
#48775=CARTESIAN_POINT('',(-13.1787500671498,36.1772650819144,19.1603162262584));
#48776=CARTESIAN_POINT('',(-13.1787500897853,36.1772650207959,18.8205585884996));
#48777=CARTESIAN_POINT('',(-13.1787500671536,36.1772650819043,23.));
#48778=CARTESIAN_POINT('',(-13.389748949659,35.0026684800589,17.6410178032058));
#48779=CARTESIAN_POINT('Ctrl Pts',(-13.1787500897853,36.1772650207959,18.8205585884996));
#48780=CARTESIAN_POINT('Ctrl Pts',(-13.1278282806594,36.3147597245981,18.8127838324376));
#48781=CARTESIAN_POINT('Ctrl Pts',(-13.0680280570975,36.4488359492941,18.8050415662166));
#48782=CARTESIAN_POINT('Ctrl Pts',(-12.9630886910638,36.6482401636516,18.7927316152069));
#48783=CARTESIAN_POINT('Ctrl Pts',(-12.924054066361,36.7165361208937,18.7883602818215));
#48784=CARTESIAN_POINT('Ctrl Pts',(-12.8696319512129,36.8045035021615,18.7824416265651));
#48785=CARTESIAN_POINT('Ctrl Pts',(-12.8563500412601,36.8254546802598,18.7810096908794));
#48786=CARTESIAN_POINT('Ctrl Pts',(-12.8350992651065,36.8581763082458,18.7787349125609));
#48787=CARTESIAN_POINT('Ctrl Pts',(-12.8272839994421,36.8700460438123,18.7779016731655));
#48788=CARTESIAN_POINT('Ctrl Pts',(-12.8107584435316,36.8948044803658,18.7761459289914));
#48789=CARTESIAN_POINT('Ctrl Pts',(-12.802033736237,36.9076828763056,18.7752224137424));
#48790=CARTESIAN_POINT('Ctrl Pts',(-12.7797674981871,36.9400674172989,18.7728750046548));
#48791=CARTESIAN_POINT('Ctrl Pts',(-12.7661092015947,36.9594919604339,18.7714437583405));
#48792=CARTESIAN_POINT('Ctrl Pts',(-12.7084912604756,37.0396320584636,18.7654468848372));
#48793=CARTESIAN_POINT('Ctrl Pts',(-12.6627304298567,37.0990209326818,18.7607810236025));
#48794=CARTESIAN_POINT('Ctrl Pts',(-12.5210168748795,37.2708403584923,18.746719921106));
#48795=CARTESIAN_POINT('Ctrl Pts',(-12.4196403145262,37.3785668372318,18.7371553329958));
#48796=CARTESIAN_POINT('Ctrl Pts',(-12.1614050163612,37.6193280921082,18.7144226847852));
#48797=CARTESIAN_POINT('Ctrl Pts',(-11.9988219908403,37.7454113249418,18.701368413872));
#48798=CARTESIAN_POINT('Ctrl Pts',(-11.7811821434201,37.8845451131068,18.6856402949913));
#48799=CARTESIAN_POINT('Ctrl Pts',(-11.7358926364506,37.91202465048,18.6824517258225));
#48800=CARTESIAN_POINT('Ctrl Pts',(-11.6636078735654,37.9535976613584,18.6774914018006));
#48801=CARTESIAN_POINT('Ctrl Pts',(-11.63703645124,37.9684073254537,18.675694594728));
#48802=CARTESIAN_POINT('Ctrl Pts',(-11.5869893954297,37.9954247737233,18.6723585764118));
#48803=CARTESIAN_POINT('Ctrl Pts',(-11.5635633846692,38.0077191552521,18.6708164266608));
#48804=CARTESIAN_POINT('Ctrl Pts',(-11.510525004539,38.0347674788116,18.6673670404646));
#48805=CARTESIAN_POINT('Ctrl Pts',(-11.4808355256115,38.0493648021045,18.6654652947617));
#48806=CARTESIAN_POINT('Ctrl Pts',(-11.3890990175868,38.0928127288703,18.6596738900431));
#48807=CARTESIAN_POINT('Ctrl Pts',(-11.3263865632731,38.1202221415413,18.655832464063));
#48808=CARTESIAN_POINT('Ctrl Pts',(-11.175488714436,38.1808018425857,18.6468274851246));
#48809=CARTESIAN_POINT('Ctrl Pts',(-11.0866653705874,38.2122319412057,18.6417150888241));
#48810=CARTESIAN_POINT('Ctrl Pts',(-10.7881266228143,38.3040665020567,18.6249528514246));
#48811=CARTESIAN_POINT('Ctrl Pts',(-10.5739159679095,38.3479264065704,18.6136248192712));
#48812=CARTESIAN_POINT('Ctrl Pts',(-10.2696063402654,38.3801536354768,18.5969865528056));
#48813=CARTESIAN_POINT('Ctrl Pts',(-10.1819048914782,38.3860056690546,18.5921241808017));
#48814=CARTESIAN_POINT('Ctrl Pts',(-10.0684420522953,38.3891560435511,18.5856374616524));
#48815=CARTESIAN_POINT('Ctrl Pts',(-10.0427951658551,38.3895768897431,18.5841582705194));
#48816=CARTESIAN_POINT('Ctrl Pts',(-10.0011954831906,38.3897873214299,18.5817344975548));
#48817=CARTESIAN_POINT('Ctrl Pts',(-9.98524414545605,38.38975541238,18.5807992627702));
#48818=CARTESIAN_POINT('Ctrl Pts',(-9.95354842323859,38.3894682852285,18.578928282167));
#48819=CARTESIAN_POINT('Ctrl Pts',(-9.93780446933173,38.3892159410399,18.5779927003318));
#48820=CARTESIAN_POINT('Ctrl Pts',(-9.89733806343113,38.3882852961738,18.5755729699747));
#48821=CARTESIAN_POINT('Ctrl Pts',(-9.87262060272855,38.3874461077077,18.574080549325));
#48822=CARTESIAN_POINT('Ctrl Pts',(-9.76257407699222,38.3825037790683,18.5673783106616));
#48823=CARTESIAN_POINT('Ctrl Pts',(-9.67741454847383,38.3754465238114,18.5620376944088));
#48824=CARTESIAN_POINT('Ctrl Pts',(-9.40233572272547,38.3421461775074,18.5444664096964));
#48825=CARTESIAN_POINT('Ctrl Pts',(-9.21434991361348,38.3030135644837,18.531980745581));
#48826=CARTESIAN_POINT('Ctrl Pts',(-8.87109217682399,38.2005792933359,18.5090907199521));
#48827=CARTESIAN_POINT('Ctrl Pts',(-8.71521672238509,38.1412553761799,18.4986556327387));
#48828=CARTESIAN_POINT('Ctrl Pts',(-8.52412634334786,38.0519125783087,18.4859060694986));
#48829=CARTESIAN_POINT('Ctrl Pts',(-8.48430723718972,38.0323339467858,18.4832506769565));
#48830=CARTESIAN_POINT('Ctrl Pts',(-8.41970730030144,37.9989802917374,18.4789431838222));
#48831=CARTESIAN_POINT('Ctrl Pts',(-8.39469551180887,37.9856666558795,18.4772754996969));
#48832=CARTESIAN_POINT('Ctrl Pts',(-8.34619143302035,37.9590624513042,18.4740406305722));
#48833=CARTESIAN_POINT('Ctrl Pts',(-8.32268521211471,37.9458018485712,18.4724725541925));
#48834=CARTESIAN_POINT('Ctrl Pts',(-8.26703045648805,37.9135230603468,18.4687575652132));
#48835=CARTESIAN_POINT('Ctrl Pts',(-8.23503261944236,37.8942512614012,18.4666198369451));
#48836=CARTESIAN_POINT('Ctrl Pts',(-8.12181685826711,37.8234871824903,18.4590422033253));
#48837=CARTESIAN_POINT('Ctrl Pts',(-8.04247637135539,37.769071185333,18.4537074721338));
#48838=CARTESIAN_POINT('Ctrl Pts',(-7.83823071677698,37.6158165567845,18.4397756986438));
#48839=CARTESIAN_POINT('Ctrl Pts',(-7.71779240633974,37.511428755291,18.4313562533397));
#48840=CARTESIAN_POINT('Ctrl Pts',(-7.4742206590898,37.2682728190713,18.4131084803104));
#48841=CARTESIAN_POINT('Ctrl Pts',(-7.354238683669,37.1271002551932,18.4033027723595));
#48842=CARTESIAN_POINT('Ctrl Pts',(-7.22612142652934,36.9486430538533,18.3908924263128));
#48843=CARTESIAN_POINT('Ctrl Pts',(-7.20629597877852,36.9201119076517,18.3889074823669));
#48844=CARTESIAN_POINT('Ctrl Pts',(-7.17683301593104,36.8762887997899,18.3858492750645));
#48845=CARTESIAN_POINT('Ctrl Pts',(-7.16687294609215,36.8612153407633,18.3847957162192));
#48846=CARTESIAN_POINT('Ctrl Pts',(-7.14890076295715,36.8335379027941,18.3828568142714));
#48847=CARTESIAN_POINT('Ctrl Pts',(-7.1408507715899,36.8209595722282,18.3819739153624));
#48848=CARTESIAN_POINT('Ctrl Pts',(-7.12235685123925,36.7916373485821,18.3799118583016));
#48849=CARTESIAN_POINT('Ctrl Pts',(-7.11197576631915,36.7748550545828,18.378728886131));
#48850=CARTESIAN_POINT('Ctrl Pts',(-7.07842754798129,36.7195465788642,18.3748236377314));
#48851=CARTESIAN_POINT('Ctrl Pts',(-7.05588111410464,36.6806515410949,18.3720669698688));
#48852=CARTESIAN_POINT('Ctrl Pts',(-7.00207898041549,36.5834305729399,18.3651722376466));
#48853=CARTESIAN_POINT('Ctrl Pts',(-6.97174536780424,36.5246166140466,18.3609977528751));
#48854=CARTESIAN_POINT('Ctrl Pts',(-6.8265729628989,36.2216930211849,18.3396049988428));
#48855=CARTESIAN_POINT('Ctrl Pts',(-6.73943060950019,35.9653441938233,18.3219512890962));
#48856=CARTESIAN_POINT('Ctrl Pts',(-6.66499312025702,35.6133717187204,18.2995522385174));
#48857=CARTESIAN_POINT('Ctrl Pts',(-6.64989085774551,35.5246586603036,18.2940447296492));
#48858=CARTESIAN_POINT('Ctrl Pts',(-6.63353339474193,35.3983774507571,18.2864006122948));
#48859=CARTESIAN_POINT('Ctrl Pts',(-6.62934539642089,35.3612335930106,18.2841757201296));
#48860=CARTESIAN_POINT('Ctrl Pts',(-6.62321559105519,35.2974013704534,18.2803910756214));
#48861=CARTESIAN_POINT('Ctrl Pts',(-6.62097392553736,35.2707459487775,18.2788222318819));
#48862=CARTESIAN_POINT('Ctrl Pts',(-6.61700987958879,35.2158335968354,18.275613110802));
#48863=CARTESIAN_POINT('Ctrl Pts',(-6.61532547781573,35.187575973454,18.2739741217276));
#48864=CARTESIAN_POINT('Ctrl Pts',(-6.61192136845952,35.1152198158909,18.2698072218175));
#48865=CARTESIAN_POINT('Ctrl Pts',(-6.61070845659356,35.0711020788213,18.2672949422737));
#48866=CARTESIAN_POINT('Ctrl Pts',(-6.60895982020982,34.8513442667541,18.2549044232832));
#48867=CARTESIAN_POINT('Ctrl Pts',(-6.62121350551241,34.6758656554659,18.2454216283818));
#48868=CARTESIAN_POINT('Ctrl Pts',(-6.68396046236489,34.2533018670943,18.2226743888106));
#48869=CARTESIAN_POINT('Ctrl Pts',(-6.74848100810393,34.0094093873721,18.209635051806));
#48870=CARTESIAN_POINT('Ctrl Pts',(-6.85151705257719,33.7435802144125,18.193508770649));
#48871=CARTESIAN_POINT('Ctrl Pts',(-6.86413372287889,33.7124138624643,18.1915858924437));
#48872=CARTESIAN_POINT('Ctrl Pts',(-6.88415465444445,33.6649975807396,18.1886034287414));
#48873=CARTESIAN_POINT('Ctrl Pts',(-6.89122754008479,33.6486090726427,18.1875620351187));
#48874=CARTESIAN_POINT('Ctrl Pts',(-6.90448492406748,33.6185454335661,18.1856308147937));
#48875=CARTESIAN_POINT('Ctrl Pts',(-6.91063127883601,33.6048544235058,18.1847431853012));
#48876=CARTESIAN_POINT('Ctrl Pts',(-6.92525000528413,33.5728615126812,18.1826501167789));
#48877=CARTESIAN_POINT('Ctrl Pts',(-6.93379503460657,33.5545938776892,18.1814405192206));
#48878=CARTESIAN_POINT('Ctrl Pts',(-6.96294610069723,33.4936963885261,18.177362180186));
#48879=CARTESIAN_POINT('Ctrl Pts',(-6.98428140872673,33.4514239242431,18.1744551609298));
#48880=CARTESIAN_POINT('Ctrl Pts',(-7.039899528721,33.346736612388,18.1670885310381));
#48881=CARTESIAN_POINT('Ctrl Pts',(-7.07527638456773,33.2849299224575,18.1625866505059));
#48882=CARTESIAN_POINT('Ctrl Pts',(-7.19900649314821,33.0837365051866,18.1475178717461));
#48883=CARTESIAN_POINT('Ctrl Pts',(-7.29558860097697,32.9496852513521,18.13680640595));
#48884=CARTESIAN_POINT('Ctrl Pts',(-7.50986707701628,32.6939007421099,18.1154839016283));
#48885=CARTESIAN_POINT('Ctrl Pts',(-7.62769486318381,32.572854102371,18.1049119870985));
#48886=CARTESIAN_POINT('Ctrl Pts',(-7.78735088589727,32.4316222197916,18.0920291876821));
#48887=CARTESIAN_POINT('Ctrl Pts',(-7.82121822514116,32.4028302361729,18.0893690830604));
#48888=CARTESIAN_POINT('Ctrl Pts',(-7.87763859666961,32.3567456220642,18.0850529184204));
#48889=CARTESIAN_POINT('Ctrl Pts',(-7.89985932065496,32.3390564017648,18.0833812792042));
#48890=CARTESIAN_POINT('Ctrl Pts',(-7.94368724137733,32.3050574113178,18.0801377833348));
#48891=CARTESIAN_POINT('Ctrl Pts',(-7.96527262173455,32.2887231281411,18.0785650460092));
#48892=CARTESIAN_POINT('Ctrl Pts',(-8.01721856005453,32.2503839211067,18.0748371619889));
#48893=CARTESIAN_POINT('Ctrl Pts',(-8.0477534391205,32.2286204981029,18.0726912674813));
#48894=CARTESIAN_POINT('Ctrl Pts',(-8.15838632296632,32.1525040892002,18.0650698788626));
#48895=CARTESIAN_POINT('Ctrl Pts',(-8.24044592110707,32.10107854891,18.0597008640835));
#48896=CARTESIAN_POINT('Ctrl Pts',(-8.4643861482978,31.9737561311255,18.0456486880187));
#48897=CARTESIAN_POINT('Ctrl Pts',(-8.60965559581636,31.9043243903016,18.0371469933706));
#48898=CARTESIAN_POINT('Ctrl Pts',(-8.92931242851481,31.7786019036434,18.0189325886959));
#48899=CARTESIAN_POINT('Ctrl Pts',(-9.10442734983922,31.7255972688611,18.0092408203109));
#48900=CARTESIAN_POINT('Ctrl Pts',(-9.31701251105216,31.6795860704288,17.9969547677973));
#48901=CARTESIAN_POINT('Ctrl Pts',(-9.35119808591971,31.6727373934834,17.9949630454292));
#48902=CARTESIAN_POINT('Ctrl Pts',(-9.40328345824383,31.6631358883837,17.9918959692929));
#48903=CARTESIAN_POINT('Ctrl Pts',(-9.42111068902769,31.6599970263153,17.990840455264));
#48904=CARTESIAN_POINT('Ctrl Pts',(-9.45349244477459,31.6545625634264,17.9889114062777));
#48905=CARTESIAN_POINT('Ctrl Pts',(-9.4680380059237,31.6522188593565,17.988040498488));
#48906=CARTESIAN_POINT('Ctrl Pts',(-9.50183579229274,31.6469988988546,17.9860066638246));
#48907=CARTESIAN_POINT('Ctrl Pts',(-9.52109777951664,31.6441936013375,17.9848400197797));
#48908=CARTESIAN_POINT('Ctrl Pts',(-9.5838179358729,31.6356100793622,17.9810191482581));
#48909=CARTESIAN_POINT('Ctrl Pts',(-9.62736262386855,31.6305092303872,17.9783320502771));
#48910=CARTESIAN_POINT('Ctrl Pts',(-9.9168360425269,31.6022797268836,17.9602941827535));
#48911=CARTESIAN_POINT('Ctrl Pts',(-10.1645559663494,31.6052485178992,17.9440864350204));
#48912=CARTESIAN_POINT('Ctrl Pts',(-10.5750465582232,31.6552347056375,17.9176488491895));
#48913=CARTESIAN_POINT('Ctrl Pts',(-10.7386528338555,31.6875178142305,17.9072123375417));
#48914=CARTESIAN_POINT('Ctrl Pts',(-10.9419323896949,31.7434483166295,17.8944687327603));
#48915=CARTESIAN_POINT('Ctrl Pts',(-10.9843899300566,31.7560298647002,17.8918186452865));
#48916=CARTESIAN_POINT('Ctrl Pts',(-11.0534808670315,31.7779852198053,17.88752345164));
#48917=CARTESIAN_POINT('Ctrl Pts',(-11.0802642196022,31.7868659428537,17.8858626945999));
#48918=CARTESIAN_POINT('Ctrl Pts',(-11.1322897339523,31.8048404319631,17.8826441643419));
#48919=CARTESIAN_POINT('Ctrl Pts',(-11.157540908227,31.8139014745961,17.8810854650393));
#48920=CARTESIAN_POINT('Ctrl Pts',(-11.2173913326308,31.8361834610762,17.8773979035282));
#48921=CARTESIAN_POINT('Ctrl Pts',(-11.2518870682638,31.8496737199851,17.8752780658735));
#48922=CARTESIAN_POINT('Ctrl Pts',(-11.3737357018973,31.899642688006,17.867803085788));
#48923=CARTESIAN_POINT('Ctrl Pts',(-11.4597771528815,31.9392128422422,17.8625500290831));
#48924=CARTESIAN_POINT('Ctrl Pts',(-11.682179435475,32.0530098960424,17.8489148092356));
#48925=CARTESIAN_POINT('Ctrl Pts',(-11.8152935379764,32.1330868631926,17.8407009522263));
#48926=CARTESIAN_POINT('Ctrl Pts',(-12.0994948645564,32.3318087180425,17.8223251054345));
#48927=CARTESIAN_POINT('Ctrl Pts',(-12.2469229880581,32.4547211164256,17.8121931739081));
#48928=CARTESIAN_POINT('Ctrl Pts',(-12.4075838113332,32.6135539896643,17.7994264046186));
#48929=CARTESIAN_POINT('Ctrl Pts',(-12.4316358390742,32.6380661896071,17.7974638258578));
#48930=CARTESIAN_POINT('Ctrl Pts',(-12.4676794551313,32.6759335135489,17.7944355565083));
#48931=CARTESIAN_POINT('Ctrl Pts',(-12.4799449135196,32.689026153061,17.7933891652836));
#48932=CARTESIAN_POINT('Ctrl Pts',(-12.5012142106865,32.7120941680484,17.7915453179189));
#48933=CARTESIAN_POINT('Ctrl Pts',(-12.5102635598188,32.7220266762317,17.7907512581966));
#48934=CARTESIAN_POINT('Ctrl Pts',(-12.5319400045785,32.7461046157187,17.7888261350229));
#48935=CARTESIAN_POINT('Ctrl Pts',(-12.54450763853,32.7603023796487,17.7876909037504));
#48936=CARTESIAN_POINT('Ctrl Pts',(-12.5834775496722,32.8050783819994,17.7841125453147));
#48937=CARTESIAN_POINT('Ctrl Pts',(-12.6094518021758,32.836022610098,17.7816422801798));
#48938=CARTESIAN_POINT('Ctrl Pts',(-12.6707076162852,32.9117060530137,17.775621798458));
#48939=CARTESIAN_POINT('Ctrl Pts',(-12.7054258833151,32.9568844992691,17.7720453366169));
#48940=CARTESIAN_POINT('Ctrl Pts',(-12.8475522043249,33.1518096133732,17.7567547109341));
#48941=CARTESIAN_POINT('Ctrl Pts',(-12.9437936577634,33.3093078219513,17.7447596745295));
#48942=CARTESIAN_POINT('Ctrl Pts',(-13.1062734859634,33.631547451641,17.7216514940857));
#48943=CARTESIAN_POINT('Ctrl Pts',(-13.1733516966057,33.7952380719363,17.7105578478115));
#48944=CARTESIAN_POINT('Ctrl Pts',(-13.2410702762761,34.0060809186809,17.6971678942629));
#48945=CARTESIAN_POINT('Ctrl Pts',(-13.2539221383331,34.0489991164086,17.6944858759613));
#48946=CARTESIAN_POINT('Ctrl Pts',(-13.2735617939049,34.1196521141618,17.690139719863));
#48947=CARTESIAN_POINT('Ctrl Pts',(-13.2808563328518,34.1472391801397,17.6884597196753));
#48948=CARTESIAN_POINT('Ctrl Pts',(-13.2944060712666,34.201232275468,17.6852036605684));
#48949=CARTESIAN_POINT('Ctrl Pts',(-13.3006942258176,34.2276277256105,17.6836266700366));
#48950=CARTESIAN_POINT('Ctrl Pts',(-13.3125727059751,34.2802862109926,17.6805087444614));
#48951=CARTESIAN_POINT('Ctrl Pts',(-13.3181692525206,34.3065457906286,17.6789677179711));
#48952=CARTESIAN_POINT('Ctrl Pts',(-13.3306122343721,34.3685331798546,17.6753607697588));
#48953=CARTESIAN_POINT('Ctrl Pts',(-13.3371967839182,34.4043105150398,17.6733028638893));
#48954=CARTESIAN_POINT('Ctrl Pts',(-13.374326420083,34.6260491159392,17.6606823226094));
#48955=CARTESIAN_POINT('Ctrl Pts',(-13.3898959837627,34.8141824997077,17.6505782097631));
#48956=CARTESIAN_POINT('Ctrl Pts',(-13.3897489686288,35.0026442731042,17.6405623182023));
#48957=CARTESIAN_POINT('Ctrl Pts',(-13.389748949659,35.0026684800589,17.6410178032058));
#48958=CARTESIAN_POINT('Ctrl Pts',(-13.3896451106924,35.1345742916728,17.633279295912));
#48959=CARTESIAN_POINT('Ctrl Pts',(-13.3818383067087,35.2661542793446,17.6255407886183));
#48960=CARTESIAN_POINT('Ctrl Pts',(-13.3664640668758,35.3966418396162,17.6178022813246));
#48961=CARTESIAN_POINT('Ctrl Pts',(-13.3507859989956,35.5297081147419,17.6099108444822));
#48962=CARTESIAN_POINT('Ctrl Pts',(-13.3272384397749,35.6616386106036,17.6020194076398));
#48963=CARTESIAN_POINT('Ctrl Pts',(-13.2960136305224,35.7916433603022,17.5941279707973));
#48964=CARTESIAN_POINT('Ctrl Pts',(-13.2922024269181,35.807511337801,17.5931647664334));
#48965=CARTESIAN_POINT('Ctrl Pts',(-13.2882769070792,35.8233506505285,17.5922015620694));
#48966=CARTESIAN_POINT('Ctrl Pts',(-13.2842374693377,35.8391598819644,17.5912383577054));
#48967=CARTESIAN_POINT('Ctrl Pts',(-13.2586267193139,35.9393932065711,17.5851314716073));
#48968=CARTESIAN_POINT('Ctrl Pts',(-13.228380821193,36.0386188205438,17.5790245855091));
#48969=CARTESIAN_POINT('Ctrl Pts',(-13.1935954601691,36.1363771817876,17.572917699411));
#48970=CARTESIAN_POINT('Ctrl Pts',(-13.18873541208,36.1500355231923,17.5720644738231));
#48971=CARTESIAN_POINT('Ctrl Pts',(-13.1837868341332,36.1636652362783,17.5712112482351));
#48972=CARTESIAN_POINT('Ctrl Pts',(-13.1787500671536,36.1772650819042,17.5703580226472));
#48973=CARTESIAN_POINT('Ctrl Pts',(-13.1787500078856,36.1772652419345,17.9149433153638));
#48974=CARTESIAN_POINT('Ctrl Pts',(-13.2574737368644,35.9647022228304,17.9271714835018));
#48975=CARTESIAN_POINT('Ctrl Pts',(-13.3147215403028,35.744662343441,17.938932006304));
#48976=CARTESIAN_POINT('Ctrl Pts',(-13.3598257005944,35.4543632313368,17.954834547551));
#48977=CARTESIAN_POINT('Ctrl Pts',(-13.3681327804114,35.3880146410483,17.9584979595338));
#48978=CARTESIAN_POINT('Ctrl Pts',(-13.3787671680747,35.276384512114,17.964771474124));
#48979=CARTESIAN_POINT('Ctrl Pts',(-13.3821578636708,35.2312222999742,17.9673395823382));
#48980=CARTESIAN_POINT('Ctrl Pts',(-13.3857286073074,35.1662482708981,17.9710943312934));
#48981=CARTESIAN_POINT('Ctrl Pts',(-13.3866414468256,35.1464798948084,17.9722446909789));
#48982=CARTESIAN_POINT('Ctrl Pts',(-13.387939505466,35.1117771359175,17.9742798447986));
#48983=CARTESIAN_POINT('Ctrl Pts',(-13.3883991762541,35.0968464327591,17.9751606377858));
#48984=CARTESIAN_POINT('Ctrl Pts',(-13.3891957309927,35.0638926544424,17.9771164546381));
#48985=CARTESIAN_POINT('Ctrl Pts',(-13.3894875568287,35.0458698624516,17.9781937406211));
#48986=CARTESIAN_POINT('Ctrl Pts',(-13.3899283128212,34.9922176524452,17.981421718358));
#48987=CARTESIAN_POINT('Ctrl Pts',(-13.3896592369081,34.956588344402,17.9835928974183));
#48988=CARTESIAN_POINT('Ctrl Pts',(-13.3847778707467,34.7472700987069,17.9964849456708));
#48989=CARTESIAN_POINT('Ctrl Pts',(-13.3673782870388,34.574150112671,18.0076869690477));
#48990=CARTESIAN_POINT('Ctrl Pts',(-13.307490239155,34.2393407127586,18.0296129566669));
#48991=CARTESIAN_POINT('Ctrl Pts',(-13.2661670724509,34.0779071717534,18.0403067371467));
#48992=CARTESIAN_POINT('Ctrl Pts',(-13.1817362310069,33.8266783060786,18.056862752586));
#48993=CARTESIAN_POINT('Ctrl Pts',(-13.1462564350678,33.7346136586263,18.0629141153332));
#48994=CARTESIAN_POINT('Ctrl Pts',(-13.0917428664217,33.6096942284475,18.0710987307272));
#48995=CARTESIAN_POINT('Ctrl Pts',(-13.0761012990294,33.5754210936235,18.0733417216152));
#48996=CARTESIAN_POINT('Ctrl Pts',(-13.0482554303218,33.5170046742794,18.0771617579532));
#48997=CARTESIAN_POINT('Ctrl Pts',(-13.0363277520216,33.4927342138675,18.0787479850568));
#48998=CARTESIAN_POINT('Ctrl Pts',(-13.011355193237,33.4434197286816,18.0819701373425));
#48999=CARTESIAN_POINT('Ctrl Pts',(-12.9982852481794,33.4183907304188,18.083605041529));
#49000=CARTESIAN_POINT('Ctrl Pts',(-12.9641061669834,33.354884344402,18.0877539442405));
#49001=CARTESIAN_POINT('Ctrl Pts',(-12.9425594343131,33.3166476561134,18.0902525271073));
#49002=CARTESIAN_POINT('Ctrl Pts',(-12.841974288071,33.1459859216965,18.1014228192928));
#49003=CARTESIAN_POINT('Ctrl Pts',(-12.7546946967595,33.01862417274,18.1097990609624));
#49004=CARTESIAN_POINT('Ctrl Pts',(-12.6379658746111,32.8709872291919,18.1198580992063));
#49005=CARTESIAN_POINT('Ctrl Pts',(-12.6164948149473,32.8446544932345,18.1216674037375));
#49006=CARTESIAN_POINT('Ctrl Pts',(-12.4712502278462,32.6718917774241,18.1336629451838));
#49007=CARTESIAN_POINT('Ctrl Pts',(-12.3356489064617,32.5358773968653,18.1436957400029));
#49008=CARTESIAN_POINT('Ctrl Pts',(-12.1380004880188,32.368674836656,18.1579332351119));
#49009=CARTESIAN_POINT('Ctrl Pts',(-12.0854361190351,32.326823384687,18.1616891628925));
#49010=CARTESIAN_POINT('Ctrl Pts',(-12.0128206541591,32.2724530486525,18.166889304276));
#49011=CARTESIAN_POINT('Ctrl Pts',(-11.9938285773464,32.2585392770875,18.1682503985757));
#49012=CARTESIAN_POINT('Ctrl Pts',(-11.9633395140369,32.2366871049758,18.1704397425555));
#49013=CARTESIAN_POINT('Ctrl Pts',(-11.9519353703066,32.2286197485778,18.171259589436));
#49014=CARTESIAN_POINT('Ctrl Pts',(-11.9275130570899,32.2115687829466,18.1730180660892));
#49015=CARTESIAN_POINT('Ctrl Pts',(-11.9144812785049,32.2026053819707,18.1739580397653));
#49016=CARTESIAN_POINT('Ctrl Pts',(-11.8806712345647,32.179697364679,18.1763999673659));
#49017=CARTESIAN_POINT('Ctrl Pts',(-11.8598007858599,32.1658912858409,18.1779104491723));
#49018=CARTESIAN_POINT('Ctrl Pts',(-11.7642843321946,32.1042152447318,18.1848305649245));
#49019=CARTESIAN_POINT('Ctrl Pts',(-11.6879353312886,32.05905791051,18.1903810266286));
#49020=CARTESIAN_POINT('Ctrl Pts',(-11.4264553756632,31.9179408479928,18.2092448853357));
#49021=CARTESIAN_POINT('Ctrl Pts',(-11.234257509621,31.8360663435837,18.2228446642719));
#49022=CARTESIAN_POINT('Ctrl Pts',(-10.8952326188486,31.7272729549394,18.2454917925623));
#49023=CARTESIAN_POINT('Ctrl Pts',(-10.7519069833692,31.6914007941183,18.2546930563343));
#49024=CARTESIAN_POINT('Ctrl Pts',(-10.5638749337427,31.657195287625,18.2662352166154));
#49025=CARTESIAN_POINT('Ctrl Pts',(-10.5209189285271,31.6502325424156,18.2688378313032));
#49026=CARTESIAN_POINT('Ctrl Pts',(-10.4499424724363,31.6401263653891,18.2730837208633));
#49027=CARTESIAN_POINT('Ctrl Pts',(-10.4219966768903,31.6365021264532,18.2747416764053));
#49028=CARTESIAN_POINT('Ctrl Pts',(-10.3670715493681,31.6300743234197,18.2779742172728));
#49029=CARTESIAN_POINT('Ctrl Pts',(-10.3400973946498,31.6272452782984,18.2795494756072));
#49030=CARTESIAN_POINT('Ctrl Pts',(-10.2752487927842,31.6212298738484,18.2833085758431));
#49031=CARTESIAN_POINT('Ctrl Pts',(-10.2373486060489,31.6183561294805,18.285482672281));
#49032=CARTESIAN_POINT('Ctrl Pts',(-10.0985023867817,31.6101741286913,18.293371603538));
#49033=CARTESIAN_POINT('Ctrl Pts',(-9.99737718196369,31.6087439217334,18.2989690461317));
#49034=CARTESIAN_POINT('Ctrl Pts',(-9.63158270987046,31.6199361273164,18.3188933922899));
#49035=CARTESIAN_POINT('Ctrl Pts',(-9.36871450613035,31.6590375405653,18.3325299046251));
#49036=CARTESIAN_POINT('Ctrl Pts',(-9.02690851700285,31.7516972245671,18.3517722572991));
#49037=CARTESIAN_POINT('Ctrl Pts',(-8.94169128184659,31.7784540800753,18.3567099340684));
#49038=CARTESIAN_POINT('Ctrl Pts',(-8.83334038820817,31.8172376219756,18.3632854085892));
#49039=CARTESIAN_POINT('Ctrl Pts',(-8.80914498459322,31.8262112150819,18.3647733239792));
#49040=CARTESIAN_POINT('Ctrl Pts',(-8.77012868800927,31.8411905313918,18.3672080561683));
#49041=CARTESIAN_POINT('Ctrl Pts',(-8.75524326046369,31.8470265875581,18.3681453780294));
#49042=CARTESIAN_POINT('Ctrl Pts',(-8.7257924319867,31.8588142841921,18.3700176763244));
#49043=CARTESIAN_POINT('Ctrl Pts',(-8.71122613660854,31.8647624444458,18.3709524520316));
#49044=CARTESIAN_POINT('Ctrl Pts',(-8.67396546723535,31.8802814045573,18.3733651266888));
#49045=CARTESIAN_POINT('Ctrl Pts',(-8.65133336133557,31.8899984055399,18.3748511897266));
#49046=CARTESIAN_POINT('Ctrl Pts',(-8.55186335758576,31.9339953614789,18.3814676058993));
#49047=CARTESIAN_POINT('Ctrl Pts',(-8.47621634746672,31.9708804295639,18.3867246618528));
#49048=CARTESIAN_POINT('Ctrl Pts',(-8.23843695988298,32.0979819872935,18.4038126259038));
#49049=CARTESIAN_POINT('Ctrl Pts',(-8.08230345588369,32.1987051232657,18.4158861790797));
#49050=CARTESIAN_POINT('Ctrl Pts',(-7.79745859456951,32.4174858910498,18.438868168231));
#49051=CARTESIAN_POINT('Ctrl Pts',(-7.66804239486149,32.5337162001579,18.4497687312902));
#49052=CARTESIAN_POINT('Ctrl Pts',(-7.51732984544045,32.6915939150976,18.4629626473845));
#49053=CARTESIAN_POINT('Ctrl Pts',(-7.48720530877304,32.7244225189734,18.4656293339936));
#49054=CARTESIAN_POINT('Ctrl Pts',(-7.43896051606056,32.779124608657,18.4699511327769));
#49055=CARTESIAN_POINT('Ctrl Pts',(-7.42045319735698,32.8006480253532,18.4716219949042));
#49056=CARTESIAN_POINT('Ctrl Pts',(-7.38487822813602,32.8430874516784,18.4748604004166));
#49057=CARTESIAN_POINT('Ctrl Pts',(-7.3677858166782,32.8639798274188,18.4764288706277));
#49058=CARTESIAN_POINT('Ctrl Pts',(-7.32768172759338,32.9142123136093,18.4801406798094));
#49059=CARTESIAN_POINT('Ctrl Pts',(-7.30490076097197,32.9437326367169,18.4822749089106));
#49060=CARTESIAN_POINT('Ctrl Pts',(-7.22549258662012,33.0502197240417,18.4898150291918));
#49061=CARTESIAN_POINT('Ctrl Pts',(-7.17163557473333,33.1292003437612,18.4951173132169));
#49062=CARTESIAN_POINT('Ctrl Pts',(-7.03809095549763,33.3440198283868,18.5089225950051));
#49063=CARTESIAN_POINT('Ctrl Pts',(-6.96440467901353,33.4833128932906,18.5172526612765));
#49064=CARTESIAN_POINT('Ctrl Pts',(-6.82458713481651,33.7989812725241,18.5355573459174));
#49065=CARTESIAN_POINT('Ctrl Pts',(-6.76292868593539,33.9767467743751,18.5455065568653));
#49066=CARTESIAN_POINT('Ctrl Pts',(-6.70772591617784,34.1922042228426,18.5580733603935));
#49067=CARTESIAN_POINT('Ctrl Pts',(-6.69965101103648,34.2258559447375,18.5600507823694));
#49068=CARTESIAN_POINT('Ctrl Pts',(-6.68815172819012,34.2772332962,18.5631000415621));
#49069=CARTESIAN_POINT('Ctrl Pts',(-6.68435118572477,34.2948733502009,18.5641523731711));
#49070=CARTESIAN_POINT('Ctrl Pts',(-6.67766161796203,34.3271731455828,18.5660904572285));
#49071=CARTESIAN_POINT('Ctrl Pts',(-6.67472841789347,34.3418228357329,18.5669737907543));
#49072=CARTESIAN_POINT('Ctrl Pts',(-6.66813730901591,34.3759108369394,18.5690390367213));
#49073=CARTESIAN_POINT('Ctrl Pts',(-6.66455259353223,34.3953622306618,18.5702247986471));
#49074=CARTESIAN_POINT('Ctrl Pts',(-6.65333058821598,34.4593941833802,18.5741496315848));
#49075=CARTESIAN_POINT('Ctrl Pts',(-6.64641561736558,34.504094595666,18.5769235469875));
#49076=CARTESIAN_POINT('Ctrl Pts',(-6.63151573486521,34.6150669633137,18.5838724460606));
#49077=CARTESIAN_POINT('Ctrl Pts',(-6.62459014109601,34.6814610339877,18.5880845230382));
#49078=CARTESIAN_POINT('Ctrl Pts',(-6.59899064905051,35.0248741805579,18.6100205052718));
#49079=CARTESIAN_POINT('Ctrl Pts',(-6.61244268644938,35.3032706506471,18.6281900922993));
#49080=CARTESIAN_POINT('Ctrl Pts',(-6.67380871640482,35.6585780828493,18.6505648944949));
#49081=CARTESIAN_POINT('Ctrl Pts',(-6.69090473181836,35.7397052143762,18.6556269678899));
#49082=CARTESIAN_POINT('Ctrl Pts',(-6.71891389856819,35.8520329631934,18.6625699168365));
#49083=CARTESIAN_POINT('Ctrl Pts',(-6.72733305303587,35.8838197462793,18.6645272979804));
#49084=CARTESIAN_POINT('Ctrl Pts',(-6.74351583598507,35.9415131472858,18.6680675330598));
#49085=CARTESIAN_POINT('Ctrl Pts',(-6.75112944201349,35.9674586697056,18.6696549991719));
#49086=CARTESIAN_POINT('Ctrl Pts',(-6.76720466728399,36.0199084677491,18.6728556531484));
#49087=CARTESIAN_POINT('Ctrl Pts',(-6.77568377932629,36.0464052380243,18.6744681374077));
#49088=CARTESIAN_POINT('Ctrl Pts',(-6.79770348406088,36.1124053628343,18.678475183605));
#49089=CARTESIAN_POINT('Ctrl Pts',(-6.81164982337988,36.151769088874,18.6808564782364));
#49090=CARTESIAN_POINT('Ctrl Pts',(-6.87478416354492,36.3200232092906,18.6910104763902));
#49091=CARTESIAN_POINT('Ctrl Pts',(-6.93108945298465,36.4461081662682,18.6985502284358));
#49092=CARTESIAN_POINT('Ctrl Pts',(-7.05801722143222,36.6892999880298,18.7132834687168));
#49093=CARTESIAN_POINT('Ctrl Pts',(-7.12834390326038,36.8062638320009,18.7204672411293));
#49094=CARTESIAN_POINT('Ctrl Pts',(-7.30011764709784,37.0564458450041,18.7365948897122));
#49095=CARTESIAN_POINT('Ctrl Pts',(-7.40476058402889,37.1870195002611,18.7455477509877));
#49096=CARTESIAN_POINT('Ctrl Pts',(-7.53809854519715,37.330293189993,18.7566882544843));
#49097=CARTESIAN_POINT('Ctrl Pts',(-7.55787202794012,37.3510074389266,18.7583343782505));
#49098=CARTESIAN_POINT('Ctrl Pts',(-7.58951273439657,37.3833236256132,18.7609638906814));
#49099=CARTESIAN_POINT('Ctrl Pts',(-7.60120722331595,37.395093641453,18.7619348118881));
#49100=CARTESIAN_POINT('Ctrl Pts',(-7.62386809544514,37.4175684226488,18.763815512673));
#49101=CARTESIAN_POINT('Ctrl Pts',(-7.63482139908449,37.4282854151188,18.7647243494528));
#49102=CARTESIAN_POINT('Ctrl Pts',(-7.66207750307962,37.4545941306971,18.7669846204552));
#49103=CARTESIAN_POINT('Ctrl Pts',(-7.67846386531112,37.4700979460759,18.76834235092));
#49104=CARTESIAN_POINT('Ctrl Pts',(-7.7423009904672,37.5293005692098,18.7736230666405));
#49105=CARTESIAN_POINT('Ctrl Pts',(-7.79083819078676,37.5718027125818,18.7776197936291));
#49106=CARTESIAN_POINT('Ctrl Pts',(-7.92840390429801,37.6854950034228,18.7888300672702));
#49107=CARTESIAN_POINT('Ctrl Pts',(-8.01985465427923,37.7536186715916,18.7961510145572));
#49108=CARTESIAN_POINT('Ctrl Pts',(-8.32923100282967,37.9606866546992,18.8201381309361));
#49109=CARTESIAN_POINT('Ctrl Pts',(-8.55966214074549,38.0793834557709,18.8367393744504));
#49110=CARTESIAN_POINT('Ctrl Pts',(-8.84841550554478,38.1885401013835,18.8554885685725));
#49111=CARTESIAN_POINT('Ctrl Pts',(-8.8958546019063,38.2052766139491,18.8585103434692));
#49112=CARTESIAN_POINT('Ctrl Pts',(-8.97174754735594,38.2301666066708,18.8632544358456));
#49113=CARTESIAN_POINT('Ctrl Pts',(-8.9999645191197,38.2390135123422,18.8649988508767));
#49114=CARTESIAN_POINT('Ctrl Pts',(-9.05375818275718,38.2551095137381,18.8682887301039));
#49115=CARTESIAN_POINT('Ctrl Pts',(-9.07931128525613,38.2624291368385,18.8698363540595));
#49116=CARTESIAN_POINT('Ctrl Pts',(-9.13816202739051,38.2785402534777,18.8733672540571));
#49117=CARTESIAN_POINT('Ctrl Pts',(-9.17151311934725,38.2871264802635,18.8753438874345));
#49118=CARTESIAN_POINT('Ctrl Pts',(-9.27921664916526,38.3131113315731,18.8816540075309));
#49119=CARTESIAN_POINT('Ctrl Pts',(-9.35403032508145,38.3285071268317,18.8859251773574));
#49120=CARTESIAN_POINT('Ctrl Pts',(-9.53807991223995,38.3599422924838,18.8962168845084));
#49121=CARTESIAN_POINT('Ctrl Pts',(-9.64770240680229,38.373198923697,18.9021621190918));
#49122=CARTESIAN_POINT('Ctrl Pts',(-9.97124758164976,38.3963775051253,18.9194654657229));
#49123=CARTESIAN_POINT('Ctrl Pts',(-10.1856666571974,38.3914189824154,18.9306019144693));
#49124=CARTESIAN_POINT('Ctrl Pts',(-10.4657257158652,38.3582930408322,18.9461040473908));
#49125=CARTESIAN_POINT('Ctrl Pts',(-10.5330205381347,38.348271267213,18.9499057276965));
#49126=CARTESIAN_POINT('Ctrl Pts',(-10.6232488906448,38.3320452606206,18.9551602437128));
#49127=CARTESIAN_POINT('Ctrl Pts',(-10.646488931375,38.3276142794452,18.9565278473308));
#49128=CARTESIAN_POINT('Ctrl Pts',(-10.6834014258582,38.3201752180674,18.9587253813454));
#49129=CARTESIAN_POINT('Ctrl Pts',(-10.6971053412979,38.3173249939127,18.959546812163));
#49130=CARTESIAN_POINT('Ctrl Pts',(-10.7262329422082,38.3110784041568,18.9613054144346));
#49131=CARTESIAN_POINT('Ctrl Pts',(-10.7416512321639,38.3076589772876,18.9622438986756));
#49132=CARTESIAN_POINT('Ctrl Pts',(-10.7813302888713,38.2985676883638,18.9646776954431));
#49133=CARTESIAN_POINT('Ctrl Pts',(-10.8055530423254,38.2927359492437,18.9661814368163));
#49134=CARTESIAN_POINT('Ctrl Pts',(-10.9144544496812,38.265243895829,18.9730165798034));
#49135=CARTESIAN_POINT('Ctrl Pts',(-10.9983348363186,38.240581704884,18.978484793347));
#49136=CARTESIAN_POINT('Ctrl Pts',(-11.272293649203,38.1483873099071,18.9968276151663));
#49137=CARTESIAN_POINT('Ctrl Pts',(-11.4573045305303,38.0671387423422,19.0099758697996));
#49138=CARTESIAN_POINT('Ctrl Pts',(-11.7699493716988,37.8951271926131,19.0327164826388));
#49139=CARTESIAN_POINT('Ctrl Pts',(-11.9006164884307,37.8110762423608,19.0424098985284));
#49140=CARTESIAN_POINT('Ctrl Pts',(-12.0602197371496,37.6921775530949,19.0544328831739));
#49141=CARTESIAN_POINT('Ctrl Pts',(-12.0948515084282,37.6653185119369,19.057054615581));
#49142=CARTESIAN_POINT('Ctrl Pts',(-12.1509258423316,37.620061128751,19.0613229001861));
#49143=CARTESIAN_POINT('Ctrl Pts',(-12.1726757357922,37.6020535191987,19.0629844555667));
#49144=CARTESIAN_POINT('Ctrl Pts',(-12.2148345538133,37.566251334666,19.0662179693834));
#49145=CARTESIAN_POINT('Ctrl Pts',(-12.2352602458271,37.5484798820384,19.0677906801247));
#49146=CARTESIAN_POINT('Ctrl Pts',(-12.2836641032722,37.5053362305936,19.0715337851037));
#49147=CARTESIAN_POINT('Ctrl Pts',(-12.31143575106,37.4797371423685,19.0736946403023));
#49148=CARTESIAN_POINT('Ctrl Pts',(-12.4106089966362,37.3852081056333,19.0814674795521));
#49149=CARTESIAN_POINT('Ctrl Pts',(-12.4794055762551,37.3136127210192,19.0869667195723));
#49150=CARTESIAN_POINT('Ctrl Pts',(-12.6561208494848,37.1127574764076,19.1015431875277));
#49151=CARTESIAN_POINT('Ctrl Pts',(-12.7577173892411,36.9783123975225,19.1104189085226));
#49152=CARTESIAN_POINT('Ctrl Pts',(-12.9417520109245,36.6928833302103,19.1284390167693));
#49153=CARTESIAN_POINT('Ctrl Pts',(-13.0235344597169,36.5420720942912,19.1375634827756));
#49154=CARTESIAN_POINT('Ctrl Pts',(-13.1080563742962,36.3533839020144,19.1492398646752));
#49155=CARTESIAN_POINT('Ctrl Pts',(-13.1220429590985,36.3207989877073,19.1512655420536));
#49156=CARTESIAN_POINT('Ctrl Pts',(-13.1423541552481,36.2713533634722,19.1543618390188));
#49157=CARTESIAN_POINT('Ctrl Pts',(-13.1490601993261,36.2546508842353,19.155411566517));
#49158=CARTESIAN_POINT('Ctrl Pts',(-13.1610912394212,36.2239814758689,19.1573474253524));
#49159=CARTESIAN_POINT('Ctrl Pts',(-13.1664573193219,36.2100316091788,19.158231182366));
#49160=CARTESIAN_POINT('Ctrl Pts',(-13.174089201427,36.1897930383037,19.1595179084281));
#49161=CARTESIAN_POINT('Ctrl Pts',(-13.1764289149267,36.1835324577998,19.1599165583278));
#49162=CARTESIAN_POINT('Ctrl Pts',(-13.1787500671498,36.1772650819144,19.1603162262584));
#49163=CARTESIAN_POINT('Origin',(-10.,35.,23.));
#49164=CARTESIAN_POINT('',(-13.1787500668679,36.1772650826756,20.4156323441327));
#49165=CARTESIAN_POINT('',(-13.1787500740781,36.1772650632072,20.0676095644498));
#49166=CARTESIAN_POINT('',(-13.1787500671536,36.1772650819043,23.));
#49167=CARTESIAN_POINT('Ctrl Pts',(-13.1787500740781,36.1772650632072,20.0676095644498));
#49168=CARTESIAN_POINT('Ctrl Pts',(-13.1746481889117,36.1883406214516,20.0668917208588));
#49169=CARTESIAN_POINT('Ctrl Pts',(-13.1704879689934,36.1993959560735,20.066175595704));
#49170=CARTESIAN_POINT('Ctrl Pts',(-13.1502072770507,36.2524466119533,20.0627410937961));
#49171=CARTESIAN_POINT('Ctrl Pts',(-13.1333097411937,36.2941401629776,20.0600477707336));
#49172=CARTESIAN_POINT('Ctrl Pts',(-13.104369160782,36.3616562938897,20.0556942975385));
#49173=CARTESIAN_POINT('Ctrl Pts',(-13.092822079692,36.3876841882828,20.0540179476221));
#49174=CARTESIAN_POINT('Ctrl Pts',(-13.0697111426167,36.4380558681641,20.050776518079));
#49175=CARTESIAN_POINT('Ctrl Pts',(-13.0581822547919,36.4624132579488,20.049210410293));
#49176=CARTESIAN_POINT('Ctrl Pts',(-13.030131040444,36.5198950407201,20.045516217134));
#49177=CARTESIAN_POINT('Ctrl Pts',(-13.0133540221758,36.5528917369351,20.0433970020786));
#49178=CARTESIAN_POINT('Ctrl Pts',(-12.9550659329678,36.6630283007685,20.0363216581615));
#49179=CARTESIAN_POINT('Ctrl Pts',(-12.9111049838055,36.73883503347,20.0314497067886));
#49180=CARTESIAN_POINT('Ctrl Pts',(-12.7185874906963,37.0430060999382,20.0117420460759));
#49181=CARTESIAN_POINT('Ctrl Pts',(-12.5457249798516,37.2547431657124,19.9977238366642));
#49182=CARTESIAN_POINT('Ctrl Pts',(-12.301572191913,37.4894923488405,19.9793837759671));
#49183=CARTESIAN_POINT('Ctrl Pts',(-12.2524099465646,37.534059048756,19.9757471210263));
#49184=CARTESIAN_POINT('Ctrl Pts',(-12.1677320496253,37.6064096683398,19.9695147238718));
#49185=CARTESIAN_POINT('Ctrl Pts',(-12.1329116527835,37.6349802803739,19.9669602621342));
#49186=CARTESIAN_POINT('Ctrl Pts',(-12.0820209617161,37.6750670572722,19.963221950236));
#49187=CARTESIAN_POINT('Ctrl Pts',(-12.0664016676778,37.6871507499599,19.9620739438972));
#49188=CARTESIAN_POINT('Ctrl Pts',(-12.038782313622,37.7081349551153,19.960041072472));
#49189=CARTESIAN_POINT('Ctrl Pts',(-12.0268276111752,37.7170936825634,19.959160167627));
#49190=CARTESIAN_POINT('Ctrl Pts',(-12.0002814568725,37.7367144008505,19.9572015004046));
#49191=CARTESIAN_POINT('Ctrl Pts',(-11.9856639066511,37.7473387916401,19.9561214381139));
#49192=CARTESIAN_POINT('Ctrl Pts',(-11.94181470817,37.778676705131,19.9528786920042));
#49193=CARTESIAN_POINT('Ctrl Pts',(-11.912339749599,37.7990435964089,19.9506952775332));
#49194=CARTESIAN_POINT('Ctrl Pts',(-11.7563138613436,37.9032410959823,19.9391411644117));
#49195=CARTESIAN_POINT('Ctrl Pts',(-11.624568263956,37.9789625652757,19.9294056030737));
#49196=CARTESIAN_POINT('Ctrl Pts',(-11.3683758866146,38.1041488289136,19.9110351726018));
#49197=CARTESIAN_POINT('Ctrl Pts',(-11.2451910205221,38.1555814743432,19.9024248664836));
#49198=CARTESIAN_POINT('Ctrl Pts',(-11.0288920205865,38.2312472263064,19.8878753173445));
#49199=CARTESIAN_POINT('Ctrl Pts',(-10.937186569662,38.2590276260626,19.8818722575603));
#49200=CARTESIAN_POINT('Ctrl Pts',(-10.7773697535569,38.3001355649519,19.8717198153037));
#49201=CARTESIAN_POINT('Ctrl Pts',(-10.7098018875377,38.3153251427303,19.8675197638821));
#49202=CARTESIAN_POINT('Ctrl Pts',(-10.6091932039276,38.3347252168402,19.8613993562556));
#49203=CARTESIAN_POINT('Ctrl Pts',(-10.5764825577093,38.3405353777558,19.8594299840065));
#49204=CARTESIAN_POINT('Ctrl Pts',(-10.5178134127196,38.3500689034386,19.8559332230054));
#49205=CARTESIAN_POINT('Ctrl Pts',(-10.4918875079849,38.3539736321139,19.8544003109999));
#49206=CARTESIAN_POINT('Ctrl Pts',(-10.4359887075654,38.361730498224,19.8511206308588));
#49207=CARTESIAN_POINT('Ctrl Pts',(-10.4060041946999,38.3654834385051,19.849377057284));
#49208=CARTESIAN_POINT('Ctrl Pts',(-10.324246597414,38.374607848468,19.8446629714049));
#49209=CARTESIAN_POINT('Ctrl Pts',(-10.2723925404282,38.3791887626699,19.8417167821468));
#49210=CARTESIAN_POINT('Ctrl Pts',(-9.98601941611297,38.3978524774416,19.8256514175369));
#49211=CARTESIAN_POINT('Ctrl Pts',(-9.75063268142627,38.3887201089399,19.8132607551762));
#49212=CARTESIAN_POINT('Ctrl Pts',(-9.33497104200979,38.3290174259411,19.7909831091838));
#49213=CARTESIAN_POINT('Ctrl Pts',(-9.15435588456849,38.2877790080985,19.7811409946492));
#49214=CARTESIAN_POINT('Ctrl Pts',(-8.95044428321495,38.2233018574705,19.768972268358));
#49215=CARTESIAN_POINT('Ctrl Pts',(-8.92297318446377,38.2142269969063,19.7673097128734));
#49216=CARTESIAN_POINT('Ctrl Pts',(-8.87987539986128,38.1993754645878,19.7646598753113));
#49217=CARTESIAN_POINT('Ctrl Pts',(-8.86416878390821,38.1938331055786,19.7636853845228));
#49218=CARTESIAN_POINT('Ctrl Pts',(-8.83428349181316,38.1830392218888,19.7618132767603));
#49219=CARTESIAN_POINT('Ctrl Pts',(-8.82009811659088,38.1778082348519,19.7609168055625));
#49220=CARTESIAN_POINT('Ctrl Pts',(-8.78845175370926,38.1658972532263,19.7588998727725));
#49221=CARTESIAN_POINT('Ctrl Pts',(-8.77101008686548,38.1591673475547,19.7577766439844));
#49222=CARTESIAN_POINT('Ctrl Pts',(-8.70998068782779,38.1350371429179,19.7538077436741));
#49223=CARTESIAN_POINT('Ctrl Pts',(-8.66670126424905,38.116876920112,19.7509235806817));
#49224=CARTESIAN_POINT('Ctrl Pts',(-8.43337429521405,38.0132232174265,19.7350453057583));
#49225=CARTESIAN_POINT('Ctrl Pts',(-8.25114908510957,37.9112445165442,19.7214711749323));
#49226=CARTESIAN_POINT('Ctrl Pts',(-8.04009636564505,37.7661278883454,19.7050222434688));
#49227=CARTESIAN_POINT('Ctrl Pts',(-8.00132003569355,37.7382410991211,19.7019654143914));
#49228=CARTESIAN_POINT('Ctrl Pts',(-7.88169184199549,37.6483125797003,19.6924382532026));
#49229=CARTESIAN_POINT('Ctrl Pts',(-7.80303617469414,37.5834360116449,19.6860335012907));
#49230=CARTESIAN_POINT('Ctrl Pts',(-7.67377195495666,37.4666365112751,19.6752958110445));
#49231=CARTESIAN_POINT('Ctrl Pts',(-7.62168775418397,37.4164570426838,19.6709037698695));
#49232=CARTESIAN_POINT('Ctrl Pts',(-7.54769891797832,37.3404623048075,19.6645637840062));
#49233=CARTESIAN_POINT('Ctrl Pts',(-7.52451447077213,37.3159265781363,19.6625615742977));
#49234=CARTESIAN_POINT('Ctrl Pts',(-7.4837856083522,37.2715133096524,19.6590147723866));
#49235=CARTESIAN_POINT('Ctrl Pts',(-7.46610086686064,37.2517688209343,19.6574643827435));
#49236=CARTESIAN_POINT('Ctrl Pts',(-7.42892518230136,37.2092706455652,19.6541819018539));
#49237=CARTESIAN_POINT('Ctrl Pts',(-7.40950055397257,37.1864618008938,19.6524525883054));
#49238=CARTESIAN_POINT('Ctrl Pts',(-7.35793194002284,37.1242566623269,19.6478203001039));
#49239=CARTESIAN_POINT('Ctrl Pts',(-7.32636712091726,37.0843890246193,19.6449402007254));
#49240=CARTESIAN_POINT('Ctrl Pts',(-7.14580335498472,36.8454757933509,19.6281597817043));
#49241=CARTESIAN_POINT('Ctrl Pts',(-7.01817291413066,36.6312380959689,19.6150946905916));
#49242=CARTESIAN_POINT('Ctrl Pts',(-6.86567257296838,36.2963901077095,19.5955562926053));
#49243=CARTESIAN_POINT('Ctrl Pts',(-6.82199734694118,36.1852981352074,19.5891901021845));
#49244=CARTESIAN_POINT('Ctrl Pts',(-6.76329638196891,36.0092334878109,19.5789694892443));
#49245=CARTESIAN_POINT('Ctrl Pts',(-6.74417400275514,35.9457264251997,19.5752567306465));
#49246=CARTESIAN_POINT('Ctrl Pts',(-6.72100311517982,35.8597111540797,19.5701438171519));
#49247=CARTESIAN_POINT('Ctrl Pts',(-6.71530068859649,35.8376599621526,19.5688256990064));
#49248=CARTESIAN_POINT('Ctrl Pts',(-6.70612460584923,35.8006409937981,19.5665980593921));
#49249=CARTESIAN_POINT('Ctrl Pts',(-6.70252960948114,35.7857035889831,19.5656951610231));
#49250=CARTESIAN_POINT('Ctrl Pts',(-6.69528111933497,35.7546594863426,19.5638094620014));
#49251=CARTESIAN_POINT('Ctrl Pts',(-6.69164361627216,35.738549817976,19.5628258901429));
#49252=CARTESIAN_POINT('Ctrl Pts',(-6.6820983079581,35.6947897978722,19.5601417160081));
#49253=CARTESIAN_POINT('Ctrl Pts',(-6.67641863314986,35.6670916621244,19.5584293590153));
#49254=CARTESIAN_POINT('Ctrl Pts',(-6.6440048582426,35.4983162076584,19.5479272858178));
#49255=CARTESIAN_POINT('Ctrl Pts',(-6.62591283485192,35.3557396668313,19.5387733092486));
#49256=CARTESIAN_POINT('Ctrl Pts',(-6.60455275586004,35.0156156354847,19.5168567475431));
#49257=CARTESIAN_POINT('Ctrl Pts',(-6.60939366282214,34.8180503603989,19.5040823821948));
#49258=CARTESIAN_POINT('Ctrl Pts',(-6.64341459676024,34.5148515074624,19.4849484694782));
#49259=CARTESIAN_POINT('Ctrl Pts',(-6.66054759682791,34.4083108671089,19.4783101271036));
#49260=CARTESIAN_POINT('Ctrl Pts',(-6.69071701979547,34.2647735857211,19.4694918551654));
#49261=CARTESIAN_POINT('Ctrl Pts',(-6.69935316299162,34.2269266732445,19.4671784081731));
#49262=CARTESIAN_POINT('Ctrl Pts',(-6.71515758638176,34.1627673951826,19.4632750764709));
#49263=CARTESIAN_POINT('Ctrl Pts',(-6.72199659912525,34.1363786214932,19.4616749996981));
#49264=CARTESIAN_POINT('Ctrl Pts',(-6.73563134885518,34.0862652333679,19.4586457208562));
#49265=CARTESIAN_POINT('Ctrl Pts',(-6.74236926027316,34.0625268404369,19.4572147959216));
#49266=CARTESIAN_POINT('Ctrl Pts',(-6.75880169764879,34.0069511230665,19.453873141394));
#49267=CARTESIAN_POINT('Ctrl Pts',(-6.76870714444392,33.975178503657,19.4519692488166));
#49268=CARTESIAN_POINT('Ctrl Pts',(-6.80619309705904,33.86089010105,19.4451393586131));
#49269=CARTESIAN_POINT('Ctrl Pts',(-6.8364807470101,33.7792946699934,19.44029949432));
#49270=CARTESIAN_POINT('Ctrl Pts',(-6.97200284650646,33.4532495636193,19.4209636923964));
#49271=CARTESIAN_POINT('Ctrl Pts',(-7.10269551438376,33.2204429127832,19.4072427031282));
#49272=CARTESIAN_POINT('Ctrl Pts',(-7.300758236245,32.9483002251139,19.3890639541454));
#49273=CARTESIAN_POINT('Ctrl Pts',(-7.34402222694572,32.8925942210297,19.3852088298101));
#49274=CARTESIAN_POINT('Ctrl Pts',(-7.41897360533566,32.8020649558604,19.3786433969239));
#49275=CARTESIAN_POINT('Ctrl Pts',(-7.44970645616594,32.7664785435094,19.3759803259579));
#49276=CARTESIAN_POINT('Ctrl Pts',(-7.49460319739658,32.7166264020737,19.3721114058172));
#49277=CARTESIAN_POINT('Ctrl Pts',(-7.50817047492936,32.7018281827625,19.3709449417286));
#49278=CARTESIAN_POINT('Ctrl Pts',(-7.53208044883887,32.676209523852,19.3688920674883));
#49279=CARTESIAN_POINT('Ctrl Pts',(-7.54236462911873,32.6653356854624,19.3680099072379));
#49280=CARTESIAN_POINT('Ctrl Pts',(-7.56506307204315,32.6416519782033,19.366064224167));
#49281=CARTESIAN_POINT('Ctrl Pts',(-7.57750645713788,32.6288719480635,19.3649986225416));
#49282=CARTESIAN_POINT('Ctrl Pts',(-7.61368819539718,32.5922934352367,19.3619047098435));
#49283=CARTESIAN_POINT('Ctrl Pts',(-7.63767978540804,32.5687497144543,19.3598587429436));
#49284=CARTESIAN_POINT('Ctrl Pts',(-7.80847053961603,32.4060620111369,19.3453577430601));
#49285=CARTESIAN_POINT('Ctrl Pts',(-7.96710660652606,32.2799541602845,19.33223913149));
#49286=CARTESIAN_POINT('Ctrl Pts',(-8.26023889405901,32.0869683071562,19.3096377418253));
#49287=CARTESIAN_POINT('Ctrl Pts',(-8.38971074011162,32.0134472314179,19.3001297483767));
#49288=CARTESIAN_POINT('Ctrl Pts',(-8.60679005159429,31.9084127982974,19.2851090027198));
#49289=CARTESIAN_POINT('Ctrl Pts',(-8.69159424775899,31.8715783239885,19.2794505214719));
#49290=CARTESIAN_POINT('Ctrl Pts',(-8.81218468804827,31.8249632312105,19.2716938098448));
#49291=CARTESIAN_POINT('Ctrl Pts',(-8.84678053863947,31.8122345234694,19.2695006731047));
#49292=CARTESIAN_POINT('Ctrl Pts',(-8.90699300037439,31.7911893824084,19.2657375593471));
#49293=CARTESIAN_POINT('Ctrl Pts',(-8.93251327023129,31.7826094385677,19.2641591333279));
#49294=CARTESIAN_POINT('Ctrl Pts',(-8.98527935284905,31.7655663806991,19.2609284559228));
#49295=CARTESIAN_POINT('Ctrl Pts',(-9.01253526895736,31.7571413372478,19.2592775386029));
#49296=CARTESIAN_POINT('Ctrl Pts',(-9.08328316424185,31.7362472454735,19.2550363550548));
#49297=CARTESIAN_POINT('Ctrl Pts',(-9.12692493479394,31.7243028221104,19.2524628938555));
#49298=CARTESIAN_POINT('Ctrl Pts',(-9.36522482443571,31.6641830225298,19.2386207620168));
#49299=CARTESIAN_POINT('Ctrl Pts',(-9.5636312785151,31.6324774247616,19.2278820128614));
#49300=CARTESIAN_POINT('Ctrl Pts',(-9.9266933244055,31.6071060370756,19.2085661712198));
#49301=CARTESIAN_POINT('Ctrl Pts',(-10.0902933164566,31.6075164136381,19.1999726962771));
#49302=CARTESIAN_POINT('Ctrl Pts',(-10.3320395342068,31.6256255621093,19.1867233754342));
#49303=CARTESIAN_POINT('Ctrl Pts',(-10.4106269333618,31.6342850999612,19.182327065726));
#49304=CARTESIAN_POINT('Ctrl Pts',(-10.5127328363551,31.6491652684983,19.1764173597361));
#49305=CARTESIAN_POINT('Ctrl Pts',(-10.5365932898354,31.6529033582388,19.1750221288207));
#49306=CARTESIAN_POINT('Ctrl Pts',(-10.5758293217941,31.659480570528,19.172701363434));
#49307=CARTESIAN_POINT('Ctrl Pts',(-10.5912293195967,31.6621717623279,19.1717837275779));
#49308=CARTESIAN_POINT('Ctrl Pts',(-10.6205078232576,31.6674972400463,19.1700253444571));
#49309=CARTESIAN_POINT('Ctrl Pts',(-10.6343894912911,31.6701119296227,19.1691857716318));
#49310=CARTESIAN_POINT('Ctrl Pts',(-10.6721683023672,31.6774725836025,19.1668856000318));
#49311=CARTESIAN_POINT('Ctrl Pts',(-10.6960308013067,31.6823894580117,19.1654160213758));
#49312=CARTESIAN_POINT('Ctrl Pts',(-10.7923723209155,31.7033257759096,19.1594207118596));
#49313=CARTESIAN_POINT('Ctrl Pts',(-10.8643649064742,31.7214657887102,19.1547981933379));
#49314=CARTESIAN_POINT('Ctrl Pts',(-11.1356775609669,31.7993857317645,19.1369723423511));
#49315=CARTESIAN_POINT('Ctrl Pts',(-11.3299418694936,31.8751078431174,19.1233948854259));
#49316=CARTESIAN_POINT('Ctrl Pts',(-11.6138236153652,32.0170599741632,19.1031332904401));
#49317=CARTESIAN_POINT('Ctrl Pts',(-11.7091919274473,32.0706615010458,19.096240130547));
#49318=CARTESIAN_POINT('Ctrl Pts',(-11.8660783264693,32.1691142894761,19.0848010239855));
#49319=CARTESIAN_POINT('Ctrl Pts',(-11.9289786386675,32.2115945419809,19.0801848533728));
#49320=CARTESIAN_POINT('Ctrl Pts',(-12.0182121526282,32.2763250965903,19.0735902758953));
#49321=CARTESIAN_POINT('Ctrl Pts',(-12.045712752512,32.2969193987151,19.0715511663265));
#49322=CARTESIAN_POINT('Ctrl Pts',(-12.0939168991972,32.3341750082714,19.0679635834466));
#49323=CARTESIAN_POINT('Ctrl Pts',(-12.1147461978105,32.3506681133217,19.0664088054572));
#49324=CARTESIAN_POINT('Ctrl Pts',(-12.1583737002382,32.3860557375712,19.0631415289015));
#49325=CARTESIAN_POINT('Ctrl Pts',(-12.1811226673032,32.4050075862408,19.0614314792296));
#49326=CARTESIAN_POINT('Ctrl Pts',(-12.2419873958665,32.457079051722,19.0568364870027));
#49327=CARTESIAN_POINT('Ctrl Pts',(-12.2796169646292,32.4907568277201,19.0539742479324));
#49328=CARTESIAN_POINT('Ctrl Pts',(-12.5039500931819,32.7007442959409,19.0367435136889));
#49329=CARTESIAN_POINT('Ctrl Pts',(-12.6708715753343,32.8969548691086,19.0232783395124));
#49330=CARTESIAN_POINT('Ctrl Pts',(-12.9075582767635,33.2493877737716,19.000718507335));
#49331=CARTESIAN_POINT('Ctrl Pts',(-12.9905972085184,33.3953647767369,18.991734581058));
#49332=CARTESIAN_POINT('Ctrl Pts',(-13.0747329638813,33.5726813072942,18.9805621173631));
#49333=CARTESIAN_POINT('Ctrl Pts',(-13.086654245125,33.5986481859257,18.9789195747798));
#49334=CARTESIAN_POINT('Ctrl Pts',(-13.1049713986649,33.6399145169202,18.9762944763266));
#49335=CARTESIAN_POINT('Ctrl Pts',(-13.1115859536996,33.6551160885171,18.9753243173024));
#49336=CARTESIAN_POINT('Ctrl Pts',(-13.1240326132902,33.6843043947198,18.9734544326089));
#49337=CARTESIAN_POINT('Ctrl Pts',(-13.1298828549991,33.6982826822769,18.9725557686771));
#49338=CARTESIAN_POINT('Ctrl Pts',(-13.1441674203176,33.7330665727496,18.9703123790643));
#49339=CARTESIAN_POINT('Ctrl Pts',(-13.1524890655588,33.7539174552925,18.9689613431577));
#49340=CARTESIAN_POINT('Ctrl Pts',(-13.1819053277365,33.8298045141081,18.964025611232));
#49341=CARTESIAN_POINT('Ctrl Pts',(-13.2017696931057,33.8853031942499,18.9603808025434));
#49342=CARTESIAN_POINT('Ctrl Pts',(-13.282114859431,34.1296808341905,18.9442618499703));
#49343=CARTESIAN_POINT('Ctrl Pts',(-13.3273998389391,34.323139501773,18.9313474947223));
#49344=CARTESIAN_POINT('Ctrl Pts',(-13.3782228220261,34.6780122634763,18.908343335226));
#49345=CARTESIAN_POINT('Ctrl Pts',(-13.3896658156566,34.8380079264556,18.8982113280507));
#49346=CARTESIAN_POINT('Ctrl Pts',(-13.3897786081615,35.0538627721316,18.8849937840186));
#49347=CARTESIAN_POINT('Ctrl Pts',(-13.3884380466477,35.1094913576134,18.8816262725728));
#49348=CARTESIAN_POINT('Ctrl Pts',(-13.3840803196029,35.1988752088003,18.8762763153671));
#49349=CARTESIAN_POINT('Ctrl Pts',(-13.3819255185102,35.2326604180868,18.8742681345242));
#49350=CARTESIAN_POINT('Ctrl Pts',(-13.3771810294872,35.2928419726195,18.8707147101195));
#49351=CARTESIAN_POINT('Ctrl Pts',(-13.3747870021675,35.3192504911896,18.8691635881286));
#49352=CARTESIAN_POINT('Ctrl Pts',(-13.3690346183339,35.3753728951024,18.8658835758968));
#49353=CARTESIAN_POINT('Ctrl Pts',(-13.3655924526277,35.4050760364955,18.8641574090822));
#49354=CARTESIAN_POINT('Ctrl Pts',(-13.3551001603312,35.4862126207624,18.8594666442448));
#49355=CARTESIAN_POINT('Ctrl Pts',(-13.3472607242299,35.5375368298244,18.8565264589389));
#49356=CARTESIAN_POINT('Ctrl Pts',(-13.3091780690012,35.7534996137863,18.8442430039122));
#49357=CARTESIAN_POINT('Ctrl Pts',(-13.2679409780853,35.9159642102598,18.8352348808651));
#49358=CARTESIAN_POINT('Ctrl Pts',(-13.2033727732961,36.1091086076841,18.8244023662525));
#49359=CARTESIAN_POINT('Ctrl Pts',(-13.1913324612675,36.1432911799257,18.8224796684973));
#49360=CARTESIAN_POINT('Ctrl Pts',(-13.1787500897853,36.1772650207959,18.8205585884996));
#49361=CARTESIAN_POINT('',(-13.3897486112447,35.0022154189341,19.236243357794));
#49362=CARTESIAN_POINT('Ctrl Pts',(-13.1787500671498,36.1772650819144,19.1603162262584));
#49363=CARTESIAN_POINT('Ctrl Pts',(-13.1833209132271,36.1649232758945,19.1611032580501));
#49364=CARTESIAN_POINT('Ctrl Pts',(-13.1878197822913,36.1525551186986,19.1618942373848));
#49365=CARTESIAN_POINT('Ctrl Pts',(-13.2075901839104,36.0972015494627,19.1654433738761));
#49366=CARTESIAN_POINT('Ctrl Pts',(-13.2220643860508,36.0539386562107,19.1682417168197));
#49367=CARTESIAN_POINT('Ctrl Pts',(-13.2557961376661,35.9459174962265,19.1752668961463));
#49368=CARTESIAN_POINT('Ctrl Pts',(-13.2739988194855,35.8808514098209,19.17953178583));
#49369=CARTESIAN_POINT('Ctrl Pts',(-13.3561519696634,35.5493074944838,19.2012975900872));
#49370=CARTESIAN_POINT('Ctrl Pts',(-13.3895698315011,35.2762817947677,19.2192236441355));
#49371=CARTESIAN_POINT('Ctrl Pts',(-13.3897492734148,35.0022194331732,19.2362442617547));
#49372=CARTESIAN_POINT('Ctrl Pts',(-13.3897492759939,35.0022154907005,19.2362445066015));
#49373=CARTESIAN_POINT('Ctrl Pts',(-13.3897859513971,34.9461013207655,19.2397294702646));
#49374=CARTESIAN_POINT('Ctrl Pts',(-13.3884292511353,34.8899920833807,19.2431782295167));
#49375=CARTESIAN_POINT('Ctrl Pts',(-13.3835973433518,34.7914781253556,19.2491688806532));
#49376=CARTESIAN_POINT('Ctrl Pts',(-13.3807160429095,34.7490585006874,19.2517273939982));
#49377=CARTESIAN_POINT('Ctrl Pts',(-13.3747937564741,34.6808690193758,19.2558074152118));
#49378=CARTESIAN_POINT('Ctrl Pts',(-13.3722536726454,34.6550613026596,19.2573440137728));
#49379=CARTESIAN_POINT('Ctrl Pts',(-13.3666222901008,34.603877871851,19.2603770776508));
#49380=CARTESIAN_POINT('Ctrl Pts',(-13.3635396053426,34.5785029524776,19.2618737031685));
#49381=CARTESIAN_POINT('Ctrl Pts',(-13.3563330893324,34.5243104450402,19.2650557919355));
#49382=CARTESIAN_POINT('Ctrl Pts',(-13.3521244500627,34.4955060881943,19.2667384995122));
#49383=CARTESIAN_POINT('Ctrl Pts',(-13.3399839648154,34.4192913716709,19.2711700603055));
#49384=CARTESIAN_POINT('Ctrl Pts',(-13.331413715781,34.3719885568378,19.2738990212357));
#49385=CARTESIAN_POINT('Ctrl Pts',(-13.276703108367,34.1027912260741,19.2893334004269));
#49386=CARTESIAN_POINT('Ctrl Pts',(-13.2094077981967,33.8857823812972,19.301350816821));
#49387=CARTESIAN_POINT('Ctrl Pts',(-13.0664686385234,33.5485648649071,19.3207686233031));
#49388=CARTESIAN_POINT('Ctrl Pts',(-13.0041014865471,33.4235280404811,19.3281642250464));
#49389=CARTESIAN_POINT('Ctrl Pts',(-12.8978338807741,33.239817879346,19.3398060197016));
#49390=CARTESIAN_POINT('Ctrl Pts',(-12.8594500708009,33.1781256557972,19.3438595595536));
#49391=CARTESIAN_POINT('Ctrl Pts',(-12.8060708022103,33.0981788411377,19.3493707187719));
#49392=CARTESIAN_POINT('Ctrl Pts',(-12.7928220670751,33.078775936306,19.3507291241371));
#49393=CARTESIAN_POINT('Ctrl Pts',(-12.7704993626501,33.0468029720778,19.3530051875142));
#49394=CARTESIAN_POINT('Ctrl Pts',(-12.7615386494156,33.0341542211689,19.3539155624273));
#49395=CARTESIAN_POINT('Ctrl Pts',(-12.7441683572752,33.0099878257811,19.3556749693573));
#49396=CARTESIAN_POINT('Ctrl Pts',(-12.7357723256925,32.9984610440331,19.356522997312));
#49397=CARTESIAN_POINT('Ctrl Pts',(-12.7124179384345,32.9668196491567,19.3588745475498));
#49398=CARTESIAN_POINT('Ctrl Pts',(-12.6973091128324,32.9468178647107,19.3603877159618));
#49399=CARTESIAN_POINT('Ctrl Pts',(-12.6321300198654,32.8624918262777,19.3668749505465));
#49400=CARTESIAN_POINT('Ctrl Pts',(-12.5799731120531,32.79982128501,19.3719662232217));
#49401=CARTESIAN_POINT('Ctrl Pts',(-12.3913289807048,32.5890904959606,19.3898815374649));
#49402=CARTESIAN_POINT('Ctrl Pts',(-12.2439493319577,32.4513470055959,19.4030089220356));
#49403=CARTESIAN_POINT('Ctrl Pts',(-11.9575449564879,32.2278806502156,19.4261891081191));
#49404=CARTESIAN_POINT('Ctrl Pts',(-11.8228877864242,32.1375325555115,19.4363173200672));
#49405=CARTESIAN_POINT('Ctrl Pts',(-11.6445808430822,32.0356040037148,19.4487200711556));
#49406=CARTESIAN_POINT('Ctrl Pts',(-11.6064794796322,32.0147841424693,19.4513166603101));
#49407=CARTESIAN_POINT('Ctrl Pts',(-11.5430275658565,31.9816786837632,19.4555550498077));
#49408=CARTESIAN_POINT('Ctrl Pts',(-11.517906023229,31.9689673355246,19.4572114402722));
#49409=CARTESIAN_POINT('Ctrl Pts',(-11.4685520455162,31.9447620293955,19.4604245764479));
#49410=CARTESIAN_POINT('Ctrl Pts',(-11.4443358755747,31.9332398029091,19.4619822017545));
#49411=CARTESIAN_POINT('Ctrl Pts',(-11.3856318006525,31.9061575852501,19.4657141376613));
#49412=CARTESIAN_POINT('Ctrl Pts',(-11.3510147644108,31.8908850707872,19.4678786573922));
#49413=CARTESIAN_POINT('Ctrl Pts',(-11.2307700840454,31.8402225544561,19.4752807359053));
#49414=CARTESIAN_POINT('Ctrl Pts',(-11.1439488643843,31.8077638749011,19.4804228455331));
#49415=CARTESIAN_POINT('Ctrl Pts',(-10.8030076912662,31.6960006957601,19.5000159423903));
#49416=CARTESIAN_POINT('Ctrl Pts',(-10.5412490019225,31.6431751690629,19.5137249585293));
#49417=CARTESIAN_POINT('Ctrl Pts',(-10.2103794336094,31.6161438562228,19.5317064137122));
#49418=CARTESIAN_POINT('Ctrl Pts',(-10.1446042300187,31.6126956646164,19.5353173718313));
#49419=CARTESIAN_POINT('Ctrl Pts',(-10.0339828742907,31.6101242586555,19.5415104164065));
#49420=CARTESIAN_POINT('Ctrl Pts',(-9.98917784940192,31.6099712593154,19.5440518981458));
#49421=CARTESIAN_POINT('Ctrl Pts',(-9.92467973627502,31.6110296060087,19.5477745778743));
#49422=CARTESIAN_POINT('Ctrl Pts',(-9.90497795183971,31.6115247908046,19.5489203448823));
#49423=CARTESIAN_POINT('Ctrl Pts',(-9.87035382763641,31.6126972320095,19.5509508208465));
#49424=CARTESIAN_POINT('Ctrl Pts',(-9.85542991136827,31.6133013642996,19.551831604835));
#49425=CARTESIAN_POINT('Ctrl Pts',(-9.82242917742865,31.6148557921981,19.5537919824455));
#49426=CARTESIAN_POINT('Ctrl Pts',(-9.80435589183241,31.6158522409432,19.5548739041302));
#49427=CARTESIAN_POINT('Ctrl Pts',(-9.75038309739215,31.6192617592164,19.5581279409394));
#49428=CARTESIAN_POINT('Ctrl Pts',(-9.71451419376199,31.6221016470966,19.5603209918448));
#49429=CARTESIAN_POINT('Ctrl Pts',(-9.52853492721746,31.6398096201221,19.5718274999163));
#49430=CARTESIAN_POINT('Ctrl Pts',(-9.37950415595507,31.6641138383263,19.5815003205184));
#49431=CARTESIAN_POINT('Ctrl Pts',(-9.10403298677183,31.7281395686387,19.5997200329444));
#49432=CARTESIAN_POINT('Ctrl Pts',(-8.97731579142982,31.7655066802657,19.6082423553762));
#49433=CARTESIAN_POINT('Ctrl Pts',(-8.71672277903737,31.859202815516,19.6258343873426));
#49434=CARTESIAN_POINT('Ctrl Pts',(-8.58362070499405,31.9169356582054,19.6348561736552));
#49435=CARTESIAN_POINT('Ctrl Pts',(-8.41696361149814,32.0023025669185,19.6461522068079));
#49436=CARTESIAN_POINT('Ctrl Pts',(-8.37968091993087,32.0222893980235,19.6486800011991));
#49437=CARTESIAN_POINT('Ctrl Pts',(-8.31841797384137,32.0566232111149,19.652836635119));
#49438=CARTESIAN_POINT('Ctrl Pts',(-8.29422433373469,32.0705777910784,19.6544789544498));
#49439=CARTESIAN_POINT('Ctrl Pts',(-8.24701869200418,32.0985885309955,19.6576859501265));
#49440=CARTESIAN_POINT('Ctrl Pts',(-8.22399652542444,32.1126233881965,19.6592512283196));
#49441=CARTESIAN_POINT('Ctrl Pts',(-8.17354492233872,32.1442116320417,19.6626854777171));
#49442=CARTESIAN_POINT('Ctrl Pts',(-8.14619586299924,32.1618887127506,19.6645498156955));
#49443=CARTESIAN_POINT('Ctrl Pts',(-8.05189841026667,32.2247826603346,19.6709919374897));
#49444=CARTESIAN_POINT('Ctrl Pts',(-7.98631255448871,32.2719979245523,19.675496838413));
#49445=CARTESIAN_POINT('Ctrl Pts',(-7.70095134512102,32.4933340632817,19.6953339550285));
#49446=CARTESIAN_POINT('Ctrl Pts',(-7.5016156007714,32.6919565368106,19.7097473743365));
#49447=CARTESIAN_POINT('Ctrl Pts',(-7.28779451961526,32.9655892205927,19.7285441706244));
#49448=CARTESIAN_POINT('Ctrl Pts',(-7.24815234748168,33.019540612387,19.7322119169322));
#49449=CARTESIAN_POINT('Ctrl Pts',(-7.1843913628039,33.1119302622325,19.738491877043));
#49450=CARTESIAN_POINT('Ctrl Pts',(-7.15939938875763,33.1497440470904,19.7410619858739));
#49451=CARTESIAN_POINT('Ctrl Pts',(-7.12459263146445,33.2047759458082,19.7448191366729));
#49452=CARTESIAN_POINT('Ctrl Pts',(-7.11415798676445,33.2215982530906,19.7459698343339));
#49453=CARTESIAN_POINT('Ctrl Pts',(-7.09610629491205,33.2512776917493,19.7480055885666));
#49454=CARTESIAN_POINT('Ctrl Pts',(-7.0884259896767,33.2640952986017,19.7488866424555));
#49455=CARTESIAN_POINT('Ctrl Pts',(-7.07166314076046,33.2924949309947,19.7508432691994));
#49456=CARTESIAN_POINT('Ctrl Pts',(-7.06262015615893,33.308098719567,19.7519211083327));
#49457=CARTESIAN_POINT('Ctrl Pts',(-7.03607660937178,33.3547542230724,19.7551504412399));
#49458=CARTESIAN_POINT('Ctrl Pts',(-7.01894136126975,33.3860096940951,19.7573224239395));
#49459=CARTESIAN_POINT('Ctrl Pts',(-6.93478191111249,33.5454340418753,19.7684223412914));
#49460=CARTESIAN_POINT('Ctrl Pts',(-6.87552155421854,33.6775205607052,19.7776814933723));
#49461=CARTESIAN_POINT('Ctrl Pts',(-6.78145685926589,33.929129914246,19.7949788906622));
#49462=CARTESIAN_POINT('Ctrl Pts',(-6.74443751229219,34.047583495572,19.802991267768));
#49463=CARTESIAN_POINT('Ctrl Pts',(-6.68810899949707,34.2700014601163,19.8176172217993));
#49464=CARTESIAN_POINT('Ctrl Pts',(-6.66700664612224,34.3733596589572,19.8242535637967));
#49465=CARTESIAN_POINT('Ctrl Pts',(-6.63934684936884,34.5506737391051,19.8353252439669));
#49466=CARTESIAN_POINT('Ctrl Pts',(-6.6303363811157,34.6241648655108,19.8398248364971));
#49467=CARTESIAN_POINT('Ctrl Pts',(-6.62070470724929,34.7318069576637,19.8462872715072));
#49468=CARTESIAN_POINT('Ctrl Pts',(-6.61818142459289,34.7657620153388,19.848307423722));
#49469=CARTESIAN_POINT('Ctrl Pts',(-6.61460250033738,34.826238860104,19.8518740462407));
#49470=CARTESIAN_POINT('Ctrl Pts',(-6.61334599840029,34.8527454675655,19.8534265593735));
#49471=CARTESIAN_POINT('Ctrl Pts',(-6.61134000417948,34.9090297737922,19.8567014727689));
#49472=CARTESIAN_POINT('Ctrl Pts',(-6.6106714828239,34.9388082220139,19.8584212579233));
#49473=CARTESIAN_POINT('Ctrl Pts',(-6.60991976005278,35.0199362365609,19.8630739525241));
#49474=CARTESIAN_POINT('Ctrl Pts',(-6.6106106493336,35.0712860793639,19.8659831357775));
#49475=CARTESIAN_POINT('Ctrl Pts',(-6.6214922543671,35.3719473195746,19.8828425627138));
#49476=CARTESIAN_POINT('Ctrl Pts',(-6.65801709166713,35.6195326687046,19.8959510611556));
#49477=CARTESIAN_POINT('Ctrl Pts',(-6.75155910422572,35.9757811740877,19.9155113669309));
#49478=CARTESIAN_POINT('Ctrl Pts',(-6.78774636918095,36.0890089950618,19.9218522234144));
#49479=CARTESIAN_POINT('Ctrl Pts',(-6.85321779018722,36.261959684961,19.9320373567151));
#49480=CARTESIAN_POINT('Ctrl Pts',(-6.87844063718257,36.3231199969566,19.9357411443414));
#49481=CARTESIAN_POINT('Ctrl Pts',(-6.91472265543276,36.4042744205853,19.9408435492707));
#49482=CARTESIAN_POINT('Ctrl Pts',(-6.92421942558523,36.4249549953694,19.9421605608939));
#49483=CARTESIAN_POINT('Ctrl Pts',(-6.94047376995444,36.4594314825958,19.9443868850372));
#49484=CARTESIAN_POINT('Ctrl Pts',(-6.94711839880611,36.4732803286641,19.9452895925584));
#49485=CARTESIAN_POINT('Ctrl Pts',(-6.96110536812461,36.5019312482451,19.9471755395472));
#49486=CARTESIAN_POINT('Ctrl Pts',(-6.96846211926132,36.51672545655,19.9481595579424));
#49487=CARTESIAN_POINT('Ctrl Pts',(-6.98871563213885,36.556718608566,19.9508461969604));
#49488=CARTESIAN_POINT('Ctrl Pts',(-7.00182009215659,36.5818101961619,19.9525606067622));
#49489=CARTESIAN_POINT('Ctrl Pts',(-7.08629060749199,36.7387275934138,19.9634510523104));
#49490=CARTESIAN_POINT('Ctrl Pts',(-7.16601568452584,36.8658512162986,19.9730242246334));
#49491=CARTESIAN_POINT('Ctrl Pts',(-7.40146450523306,37.1912073720351,19.9988694706518));
#49492=CARTESIAN_POINT('Ctrl Pts',(-7.57132958598149,37.3781022593344,20.0151344717468));
#49493=CARTESIAN_POINT('Ctrl Pts',(-7.80858444641188,37.5869350989711,20.0345205536798));
#49494=CARTESIAN_POINT('Ctrl Pts',(-7.85802584857969,37.6280188176932,20.0384103482283));
#49495=CARTESIAN_POINT('Ctrl Pts',(-7.93404264179854,37.6876141419592,20.0441730478829));
#49496=CARTESIAN_POINT('Ctrl Pts',(-7.95976165249794,37.7071899039101,20.0460869995352));
#49497=CARTESIAN_POINT('Ctrl Pts',(-8.00493617232509,37.7405645362262,20.0493884189096));
#49498=CARTESIAN_POINT('Ctrl Pts',(-8.02426428940801,37.7545311939911,20.0507822448012));
#49499=CARTESIAN_POINT('Ctrl Pts',(-8.06825554290844,37.7856183633018,20.0539135108066));
#49500=CARTESIAN_POINT('Ctrl Pts',(-8.09300215911319,37.802617639262,20.0556463197875));
#49501=CARTESIAN_POINT('Ctrl Pts',(-8.16050267116758,37.8476779289139,20.0602985979658));
#49502=CARTESIAN_POINT('Ctrl Pts',(-8.20367186002381,37.8751044513944,20.0631948420224));
#49503=CARTESIAN_POINT('Ctrl Pts',(-8.45781675896607,38.0286097414877,20.0798277144288));
#49504=CARTESIAN_POINT('Ctrl Pts',(-8.68138044176266,38.1324207425783,20.0927522951134));
#49505=CARTESIAN_POINT('Ctrl Pts',(-9.08118647019215,38.2676064883701,20.1151586074467));
#49506=CARTESIAN_POINT('Ctrl Pts',(-9.2522846978392,38.3109482404968,20.1245686240925));
#49507=CARTESIAN_POINT('Ctrl Pts',(-9.45422299637824,38.34564721471,20.136230884418));
#49508=CARTESIAN_POINT('Ctrl Pts',(-9.48255203168395,38.3501455651758,20.1378796420496));
#49509=CARTESIAN_POINT('Ctrl Pts',(-9.52736315677967,38.3566791835309,20.1405124568663));
#49510=CARTESIAN_POINT('Ctrl Pts',(-9.5438095815106,38.3589538555199,20.1414839965556));
#49511=CARTESIAN_POINT('Ctrl Pts',(-9.57528735065574,38.3630720417082,20.1433546400792));
#49512=CARTESIAN_POINT('Ctrl Pts',(-9.59031537983691,38.3649357899928,20.1442526561776));
#49513=CARTESIAN_POINT('Ctrl Pts',(-9.62759228764077,38.3693053961751,20.1464916925396));
#49514=CARTESIAN_POINT('Ctrl Pts',(-9.64985427099698,38.371691603106,20.1478389683194));
#49515=CARTESIAN_POINT('Ctrl Pts',(-9.73037933845661,38.3795168139083,20.1527448387466));
#49516=CARTESIAN_POINT('Ctrl Pts',(-9.7887544343873,38.3836671926511,20.1563626406687));
#49517=CARTESIAN_POINT('Ctrl Pts',(-10.0705888312135,38.396384062205,20.1740357449717));
#49518=CARTESIAN_POINT('Ctrl Pts',(-10.2944178722726,38.3843352061911,20.1886533522992));
#49519=CARTESIAN_POINT('Ctrl Pts',(-10.6811970049692,38.3248316346608,20.2136570634508));
#49520=CARTESIAN_POINT('Ctrl Pts',(-10.8448614882688,38.2870589952907,20.2241632800895));
#49521=CARTESIAN_POINT('Ctrl Pts',(-11.0468413028531,38.2243512316133,20.2369384049874));
#49522=CARTESIAN_POINT('Ctrl Pts',(-11.08835357324,38.2105769490652,20.2395546682865));
#49523=CARTESIAN_POINT('Ctrl Pts',(-11.1561937118057,38.1865996582169,20.2438164488122));
#49524=CARTESIAN_POINT('Ctrl Pts',(-11.1826803699991,38.1768645698736,20.2454768790858));
#49525=CARTESIAN_POINT('Ctrl Pts',(-11.2340602819566,38.1572483865664,20.248692009257));
#49526=CARTESIAN_POINT('Ctrl Pts',(-11.2589640144119,38.1474008045813,20.2502476657056));
#49527=CARTESIAN_POINT('Ctrl Pts',(-11.3185585680652,38.1230150434055,20.2539651822138));
#49528=CARTESIAN_POINT('Ctrl Pts',(-11.3531296118309,38.1081924123281,20.2561174499319));
#49529=CARTESIAN_POINT('Ctrl Pts',(-11.4706736034283,38.0554614535248,20.2634275851432));
#49530=CARTESIAN_POINT('Ctrl Pts',(-11.552362497242,38.0147799449385,20.2684932738229));
#49531=CARTESIAN_POINT('Ctrl Pts',(-11.8670839962399,37.841858091817,20.2881167815834));
#49532=CARTESIAN_POINT('Ctrl Pts',(-12.0857190100495,37.6855031020326,20.301911856918));
#49533=CARTESIAN_POINT('Ctrl Pts',(-12.3324347132558,37.4605910924204,20.3199932492261));
#49534=CARTESIAN_POINT('Ctrl Pts',(-12.3798933573563,37.4147188148722,20.3236114857764));
#49535=CARTESIAN_POINT('Ctrl Pts',(-12.4573189112764,37.3353805151204,20.3298156795104));
#49536=CARTESIAN_POINT('Ctrl Pts',(-12.4880151238788,37.3026503703234,20.3323608406852));
#49537=CARTESIAN_POINT('Ctrl Pts',(-12.5312525755986,37.2546738822414,20.336087948429));
#49538=CARTESIAN_POINT('Ctrl Pts',(-12.5443256166716,37.2399109429867,20.3372343468971));
#49539=CARTESIAN_POINT('Ctrl Pts',(-12.567073806651,37.2137660818011,20.3392654935164));
#49540=CARTESIAN_POINT('Ctrl Pts',(-12.5768036806673,37.202432966661,20.340146306676));
#49541=CARTESIAN_POINT('Ctrl Pts',(-12.5981528983106,37.1772307886925,20.3421061837542));
#49542=CARTESIAN_POINT('Ctrl Pts',(-12.6097361740289,37.163332951671,20.343187567674));
#49543=CARTESIAN_POINT('Ctrl Pts',(-12.6432925477366,37.1224096570335,20.3463718478109));
#49544=CARTESIAN_POINT('Ctrl Pts',(-12.6649603964635,37.0951382120961,20.3484939274892));
#49545=CARTESIAN_POINT('Ctrl Pts',(-12.7979282938112,36.9223826739345,20.3619118902352));
#49546=CARTESIAN_POINT('Ctrl Pts',(-12.8976955683043,36.7684198104552,20.3737452838208));
#49547=CARTESIAN_POINT('Ctrl Pts',(-13.0591714039707,36.4685568064207,20.3956963255708));
#49548=CARTESIAN_POINT('Ctrl Pts',(-13.124069307029,36.3249093741373,20.4057970344023));
#49549=CARTESIAN_POINT('Ctrl Pts',(-13.1787500668679,36.1772650826756,20.4156323441327));
#49550=CARTESIAN_POINT('Origin',(-10.,35.,23.));
#49551=CARTESIAN_POINT('',(-13.1787500358286,36.1772651664852,21.6644776847947));
#49552=CARTESIAN_POINT('',(-13.1787500764527,36.1772650567955,21.3230161660245));
#49553=CARTESIAN_POINT('',(-13.1787500671536,36.1772650819043,23.));
#49554=CARTESIAN_POINT('',(-13.3897498409689,34.9989616594858,20.1438254858951));
#49555=CARTESIAN_POINT('Ctrl Pts',(-13.1787500764527,36.1772650567955,21.3230161660245));
#49556=CARTESIAN_POINT('Ctrl Pts',(-13.1402670886756,36.2811735178786,21.3160961033474));
#49557=CARTESIAN_POINT('Ctrl Pts',(-13.0967087805464,36.3831420775156,21.3090033589191));
#49558=CARTESIAN_POINT('Ctrl Pts',(-12.9319072502346,36.7219284421956,21.2847566554013));
#49559=CARTESIAN_POINT('Ctrl Pts',(-12.787829044545,36.946578925495,21.2675899894107));
#49560=CARTESIAN_POINT('Ctrl Pts',(-12.5843279146492,37.1942261447432,21.2480503943131));
#49561=CARTESIAN_POINT('Ctrl Pts',(-12.5486913805438,37.2355205002278,21.24476435188));
#49562=CARTESIAN_POINT('Ctrl Pts',(-12.4914291974183,37.2987237562876,21.2396882918648));
#49563=CARTESIAN_POINT('Ctrl Pts',(-12.4704765363389,37.321227289646,21.2378712414739));
#49564=CARTESIAN_POINT('Ctrl Pts',(-12.4309565104849,37.3625311455461,21.2345167826778));
#49565=CARTESIAN_POINT('Ctrl Pts',(-12.4124700611279,37.3814053061226,21.2329761367735));
#49566=CARTESIAN_POINT('Ctrl Pts',(-12.3706686878054,37.4230969994869,21.2295541942591));
#49567=CARTESIAN_POINT('Ctrl Pts',(-12.3472410722571,37.4457981419276,21.2276780039746));
#49568=CARTESIAN_POINT('Ctrl Pts',(-12.2755071035913,37.5133274749273,21.2220534768247));
#49569=CARTESIAN_POINT('Ctrl Pts',(-12.226216491852,37.5570898480338,21.2183492704528));
#49570=CARTESIAN_POINT('Ctrl Pts',(-12.1071696258625,37.6567316170979,21.209738350357));
#49571=CARTESIAN_POINT('Ctrl Pts',(-12.0364173039599,37.7113451824053,21.204876513967));
#49572=CARTESIAN_POINT('Ctrl Pts',(-11.8490708954995,37.8444821088063,21.192514726961));
#49573=CARTESIAN_POINT('Ctrl Pts',(-11.7296049591917,37.9186656463085,21.185113627102));
#49574=CARTESIAN_POINT('Ctrl Pts',(-11.4575838212683,38.0649976550872,21.1687011831968));
#49575=CARTESIAN_POINT('Ctrl Pts',(-11.3035639542655,38.1336033100024,21.1596847172857));
#49576=CARTESIAN_POINT('Ctrl Pts',(-11.1180931056047,38.2001713284898,21.1484690616378));
#49577=CARTESIAN_POINT('Ctrl Pts',(-11.0909596614066,38.209522647731,21.146819427164));
#49578=CARTESIAN_POINT('Ctrl Pts',(-11.0479440506684,38.223739149603,21.1441855309555));
#49579=CARTESIAN_POINT('Ctrl Pts',(-11.0321386624572,38.2288342469343,21.1432138040647));
#49580=CARTESIAN_POINT('Ctrl Pts',(-11.0016831651396,38.2384055569475,21.1413326825629));
#49581=CARTESIAN_POINT('Ctrl Pts',(-10.9870391587164,38.2428989159647,21.1404242461049));
#49582=CARTESIAN_POINT('Ctrl Pts',(-10.9507887981037,38.2537536827921,21.1381665144));
#49583=CARTESIAN_POINT('Ctrl Pts',(-10.9291487169067,38.2599992283481,21.1368109541544));
#49584=CARTESIAN_POINT('Ctrl Pts',(-10.8455691681973,38.2832213618119,21.1315498158576));
#49585=CARTESIAN_POINT('Ctrl Pts',(-10.7832174746857,38.2986510930381,21.1275711614449));
#49586=CARTESIAN_POINT('Ctrl Pts',(-10.6099031652785,38.3363492778771,21.1164316171922));
#49587=CARTESIAN_POINT('Ctrl Pts',(-10.4982069549816,38.3548466145101,21.1091647365135));
#49588=CARTESIAN_POINT('Ctrl Pts',(-10.1276278474889,38.3972995616737,21.0851322998734));
#49589=CARTESIAN_POINT('Ctrl Pts',(-9.86686539711964,38.3970943769782,21.0684275607769));
#49590=CARTESIAN_POINT('Ctrl Pts',(-9.55889844332096,38.3613009783166,21.0495996918934));
#49591=CARTESIAN_POINT('Ctrl Pts',(-9.50926812009674,38.3544146245683,21.0465902282935));
#49592=CARTESIAN_POINT('Ctrl Pts',(-9.43065626371985,38.3417248028084,21.04186079421));
#49593=CARTESIAN_POINT('Ctrl Pts',(-9.40156798094662,38.3366384504322,21.0401189581931));
#49594=CARTESIAN_POINT('Ctrl Pts',(-9.34642145606504,38.3262511971017,21.0368312576107));
#49595=CARTESIAN_POINT('Ctrl Pts',(-9.3203520254786,38.321022527673,21.0352832722747));
#49596=CARTESIAN_POINT('Ctrl Pts',(-9.26059185481515,38.3083034365583,21.0317478201388));
#49597=CARTESIAN_POINT('Ctrl Pts',(-9.22694830050268,38.3006040701895,21.029767060457));
#49598=CARTESIAN_POINT('Ctrl Pts',(-9.11881703001145,38.2741139890942,21.0234270828467));
#49599=CARTESIAN_POINT('Ctrl Pts',(-9.04484631925979,38.2533042412468,21.0191310555369));
#49600=CARTESIAN_POINT('Ctrl Pts',(-8.86555302330443,38.1962213568535,21.0087623787634));
#49601=CARTESIAN_POINT('Ctrl Pts',(-8.76118760718904,38.1572372406447,21.0027666627582));
#49602=CARTESIAN_POINT('Ctrl Pts',(-8.45703801181351,38.0262179875849,20.9851062495034));
#49603=CARTESIAN_POINT('Ctrl Pts',(-8.26410524917939,37.9198257217929,20.9736757605094));
#49604=CARTESIAN_POINT('Ctrl Pts',(-8.03153522371403,37.7603301151047,20.9581149131681));
#49605=CARTESIAN_POINT('Ctrl Pts',(-7.98120728540772,37.7237384119442,20.9546267478011));
#49606=CARTESIAN_POINT('Ctrl Pts',(-7.91376695178496,37.671808662366,20.9497424166574));
#49607=CARTESIAN_POINT('Ctrl Pts',(-7.89575868129411,37.6576490119732,20.9484169032379));
#49608=CARTESIAN_POINT('Ctrl Pts',(-7.86601462959727,37.6337698546867,20.9461893013062));
#49609=CARTESIAN_POINT('Ctrl Pts',(-7.85419800871779,37.62415148478,20.945294066193));
#49610=CARTESIAN_POINT('Ctrl Pts',(-7.82978275251786,37.6040030252424,20.9434220423155));
#49611=CARTESIAN_POINT('Ctrl Pts',(-7.81719520779816,37.5934605975639,20.942444450851));
#49612=CARTESIAN_POINT('Ctrl Pts',(-7.7834828158011,37.5648062171452,20.9397936532997));
#49613=CARTESIAN_POINT('Ctrl Pts',(-7.76250402743272,37.5465252842937,20.9381091598229));
#49614=CARTESIAN_POINT('Ctrl Pts',(-7.63905645419594,37.4362498518559,20.9279992134172));
#49615=CARTESIAN_POINT('Ctrl Pts',(-7.54205407463878,37.3383461351494,20.9192368892726));
#49616=CARTESIAN_POINT('Ctrl Pts',(-7.26378710599566,37.0209953981113,20.8921162783271));
#49617=CARTESIAN_POINT('Ctrl Pts',(-7.10390926385604,36.784374998941,20.8736973182101));
#49618=CARTESIAN_POINT('Ctrl Pts',(-6.95198716001513,36.4841580751381,20.8532253379525));
#49619=CARTESIAN_POINT('Ctrl Pts',(-6.92958422965808,36.4372386403844,20.8500975192902));
#49620=CARTESIAN_POINT('Ctrl Pts',(-6.89588501118752,36.3622728857203,20.8452100005472));
#49621=CARTESIAN_POINT('Ctrl Pts',(-6.88387005089418,36.3345604173895,20.8434264313684));
#49622=CARTESIAN_POINT('Ctrl Pts',(-6.86304357668276,36.2847089074802,20.8402582346486));
#49623=CARTESIAN_POINT('Ctrl Pts',(-6.85409218511805,36.2626308414514,20.8388690243188));
#49624=CARTESIAN_POINT('Ctrl Pts',(-6.83363778395511,36.210613047384,20.8356275429106));
#49625=CARTESIAN_POINT('Ctrl Pts',(-6.82232535535287,36.1806005198627,20.8337816455484));
#49626=CARTESIAN_POINT('Ctrl Pts',(-6.79007856078249,36.0912246149537,20.8283528880154));
#49627=CARTESIAN_POINT('Ctrl Pts',(-6.77036920022641,36.0314322051005,20.8248095574175));
#49628=CARTESIAN_POINT('Ctrl Pts',(-6.70800966867564,35.8228871798355,20.812712914069));
#49629=CARTESIAN_POINT('Ctrl Pts',(-6.67388256622869,35.6717826933221,20.8044111253319));
#49630=CARTESIAN_POINT('Ctrl Pts',(-6.62072192194677,35.3285780473721,20.7859521737936));
#49631=CARTESIAN_POINT('Ctrl Pts',(-6.60751700831568,35.136136613001,20.7758747215507));
#49632=CARTESIAN_POINT('Ctrl Pts',(-6.61181674793735,34.8776111047162,20.7616435944293));
#49633=CARTESIAN_POINT('Ctrl Pts',(-6.61484342204103,34.8116423361436,20.7579495644333));
#49634=CARTESIAN_POINT('Ctrl Pts',(-6.62154953261965,34.7224653425152,20.7528218626585));
#49635=CARTESIAN_POINT('Ctrl Pts',(-6.62354664442012,34.6991416963975,20.7514682646804));
#49636=CARTESIAN_POINT('Ctrl Pts',(-6.62711932350132,34.6619531609368,20.7492874503246));
#49637=CARTESIAN_POINT('Ctrl Pts',(-6.62853925496047,34.6480736543568,20.7484684994737));
#49638=CARTESIAN_POINT('Ctrl Pts',(-6.63175583893251,34.6184403848103,20.7467085169525));
#49639=CARTESIAN_POINT('Ctrl Pts',(-6.63357741781179,34.6026897382002,20.745766101977));
#49640=CARTESIAN_POINT('Ctrl Pts',(-6.63858116388066,34.5619315464553,20.7433104000562));
#49641=CARTESIAN_POINT('Ctrl Pts',(-6.6419318659679,34.5369461297512,20.7417884103346));
#49642=CARTESIAN_POINT('Ctrl Pts',(-6.65865396292542,34.422000639533,20.7347169890567));
#49643=CARTESIAN_POINT('Ctrl Pts',(-6.67536293949245,34.3325703367701,20.7290193888631));
#49644=CARTESIAN_POINT('Ctrl Pts',(-6.74505854337428,34.0279711327977,20.7091653277677));
#49645=CARTESIAN_POINT('Ctrl Pts',(-6.81552330891013,33.8173758536015,20.6946985810215));
#49646=CARTESIAN_POINT('Ctrl Pts',(-6.960771753636,33.4928681796736,20.6721745097831));
#49647=CARTESIAN_POINT('Ctrl Pts',(-7.02271238128343,33.3739249693935,20.6638530143631));
#49648=CARTESIAN_POINT('Ctrl Pts',(-7.11335725474402,33.2225008438249,20.6532047237716));
#49649=CARTESIAN_POINT('Ctrl Pts',(-7.13585969464756,33.1864647381241,20.6506656764381));
#49650=CARTESIAN_POINT('Ctrl Pts',(-7.17428923733135,33.1274226957785,20.6464956784856));
#49651=CARTESIAN_POINT('Ctrl Pts',(-7.18983388803537,33.1041747001132,20.6448510683413));
#49652=CARTESIAN_POINT('Ctrl Pts',(-7.22108972324115,33.0586589123826,20.6416249091609));
#49653=CARTESIAN_POINT('Ctrl Pts',(-7.23678524282947,33.0363829767677,20.6400429445881));
#49654=CARTESIAN_POINT('Ctrl Pts',(-7.27545215822539,32.9828866450222,20.6362348821541));
#49655=CARTESIAN_POINT('Ctrl Pts',(-7.2986939950278,32.951865905135,20.6340192190981));
#49656=CARTESIAN_POINT('Ctrl Pts',(-7.38829184746641,32.8364592967501,20.6257390718982));
#49657=CARTESIAN_POINT('Ctrl Pts',(-7.4581140913868,32.7548392455734,20.6198087820014));
#49658=CARTESIAN_POINT('Ctrl Pts',(-7.66562670514252,32.5343786086058,20.6033703056137));
#49659=CARTESIAN_POINT('Ctrl Pts',(-7.81160649093395,32.4039409593276,20.593145506339));
#49660=CARTESIAN_POINT('Ctrl Pts',(-8.08489373022266,32.1992685009152,20.5749368864106));
#49661=CARTESIAN_POINT('Ctrl Pts',(-8.20729830180845,32.1193853493378,20.5670502833848));
#49662=CARTESIAN_POINT('Ctrl Pts',(-8.35909633188967,32.0337497459747,20.5571253165051));
#49663=CARTESIAN_POINT('Ctrl Pts',(-8.38390857876547,32.0201587584433,20.555498513415));
#49664=CARTESIAN_POINT('Ctrl Pts',(-8.42347326230401,31.9991265631009,20.552892784773));
#49665=CARTESIAN_POINT('Ctrl Pts',(-8.43811552169387,31.9914796343646,20.5519259460265));
#49666=CARTESIAN_POINT('Ctrl Pts',(-8.46648192394435,31.9769281536673,20.5500469685834));
#49667=CARTESIAN_POINT('Ctrl Pts',(-8.48019804154927,31.9700093976188,20.5491356886571));
#49668=CARTESIAN_POINT('Ctrl Pts',(-8.51435711778015,31.953068980097,20.5468602281064));
#49669=CARTESIAN_POINT('Ctrl Pts',(-8.53485474279792,31.9431596824384,20.545489565854));
#49670=CARTESIAN_POINT('Ctrl Pts',(-8.61536854905398,31.9052322009635,20.5400897409359));
#49671=CARTESIAN_POINT('Ctrl Pts',(-8.67609763291702,31.8787705415132,20.5359827085348));
#49672=CARTESIAN_POINT('Ctrl Pts',(-8.84804562636995,31.8097681132631,20.5243341378571));
#49673=CARTESIAN_POINT('Ctrl Pts',(-8.96078709549218,31.7712831686984,20.5166762908007));
#49674=CARTESIAN_POINT('Ctrl Pts',(-9.31488547436865,31.6708811573794,20.4929544557103));
#49675=CARTESIAN_POINT('Ctrl Pts',(-9.5612518294219,31.6295473465749,20.476977211535));
#49676=CARTESIAN_POINT('Ctrl Pts',(-9.86126606251305,31.6127002547486,20.4587111187294));
#49677=CARTESIAN_POINT('Ctrl Pts',(-9.91264263792916,31.6109860145143,20.4556212561396));
#49678=CARTESIAN_POINT('Ctrl Pts',(-9.9938332417984,31.6101246719796,20.4507964703319));
#49679=CARTESIAN_POINT('Ctrl Pts',(-10.0236295128718,31.6102014072492,20.4490381392533));
#49680=CARTESIAN_POINT('Ctrl Pts',(-10.0799514296053,31.6110891371298,20.445736744064));
#49681=CARTESIAN_POINT('Ctrl Pts',(-10.1064759378639,31.6118187768088,20.444191305581));
#49682=CARTESIAN_POINT('Ctrl Pts',(-10.1669916357057,31.6141948122974,20.4406854894196));
#49683=CARTESIAN_POINT('Ctrl Pts',(-10.2009723617675,31.6160417843793,20.4387314095428));
#49684=CARTESIAN_POINT('Ctrl Pts',(-10.3086552074759,31.623522533375,20.4325805174505));
#49685=CARTESIAN_POINT('Ctrl Pts',(-10.3822059413008,31.6310553852561,20.4284415074141));
#49686=CARTESIAN_POINT('Ctrl Pts',(-10.5597107176296,31.6551236244737,20.418554101261));
#49687=CARTESIAN_POINT('Ctrl Pts',(-10.6632556300735,31.6741064314767,20.4128728242203));
#49688=CARTESIAN_POINT('Ctrl Pts',(-10.8868065408144,31.7259473379431,20.4006108908022));
#49689=CARTESIAN_POINT('Ctrl Pts',(-11.0062228896755,31.7606540440783,20.3940639114528));
#49690=CARTESIAN_POINT('Ctrl Pts',(-11.2600069298808,31.8498044078353,20.3797477177074));
#49691=CARTESIAN_POINT('Ctrl Pts',(-11.3933258856956,31.9064607772689,20.3719694648174));
#49692=CARTESIAN_POINT('Ctrl Pts',(-11.5544680356929,31.9874751125343,20.3617858243671));
#49693=CARTESIAN_POINT('Ctrl Pts',(-11.586076725617,32.0039964150502,20.3597487195188));
#49694=CARTESIAN_POINT('Ctrl Pts',(-11.6332707830033,32.0296200537614,20.356638431783));
#49695=CARTESIAN_POINT('Ctrl Pts',(-11.6490546933376,32.0383536567832,20.3555864238806));
#49696=CARTESIAN_POINT('Ctrl Pts',(-11.6777844646556,32.0545513678361,20.3536485543875));
#49697=CARTESIAN_POINT('Ctrl Pts',(-11.6907517447967,32.0619756867108,20.3527651052668));
#49698=CARTESIAN_POINT('Ctrl Pts',(-11.72077859221,32.0794319470043,20.350699069882));
#49699=CARTESIAN_POINT('Ctrl Pts',(-11.7377998013694,32.0895277832822,20.3495126251859));
#49700=CARTESIAN_POINT('Ctrl Pts',(-11.7934809581228,32.1232166708795,20.3455834126762));
#49701=CARTESIAN_POINT('Ctrl Pts',(-11.8317550446842,32.1474346097968,20.3428057028407));
#49702=CARTESIAN_POINT('Ctrl Pts',(-11.9253085770032,32.2092898366946,20.3358450494066));
#49703=CARTESIAN_POINT('Ctrl Pts',(-11.9799805734388,32.2478095344636,20.3316248689289));
#49704=CARTESIAN_POINT('Ctrl Pts',(-12.2569543912757,32.4554800244865,20.3095721389797));
#49705=CARTESIAN_POINT('Ctrl Pts',(-12.4589041246991,32.650052979678,20.2912917732139));
#49706=CARTESIAN_POINT('Ctrl Pts',(-12.6859950186215,32.9305834338275,20.2689104909987));
#49707=CARTESIAN_POINT('Ctrl Pts',(-12.7349997054509,32.9957963060646,20.263932575384));
#49708=CARTESIAN_POINT('Ctrl Pts',(-12.8002843966378,33.0895340107787,20.2570834576977));
#49709=CARTESIAN_POINT('Ctrl Pts',(-12.8185726964726,33.116619776858,20.25513845529));
#49710=CARTESIAN_POINT('Ctrl Pts',(-12.851245136309,33.1665511471194,20.2516135245821));
#49711=CARTESIAN_POINT('Ctrl Pts',(-12.8657533698945,33.1893119514426,20.2500291264053));
#49712=CARTESIAN_POINT('Ctrl Pts',(-12.8946967509512,33.2359383426637,20.2468276930368));
#49713=CARTESIAN_POINT('Ctrl Pts',(-12.9091123117754,33.2598136777781,20.2452114493914));
#49714=CARTESIAN_POINT('Ctrl Pts',(-12.9445447384575,33.3201685938597,20.2411814734842));
#49715=CARTESIAN_POINT('Ctrl Pts',(-12.9651800502123,33.3568673941831,20.2387813403999));
#49716=CARTESIAN_POINT('Ctrl Pts',(-13.0525325701925,33.5192266685033,20.2283675269239));
#49717=CARTESIAN_POINT('Ctrl Pts',(-13.111987825755,33.6486368332558,20.2206030369261));
#49718=CARTESIAN_POINT('Ctrl Pts',(-13.2363893698021,33.9715509248681,20.2020406417496));
#49719=CARTESIAN_POINT('Ctrl Pts',(-13.2923435131101,34.1678987840244,20.1914318998722));
#49720=CARTESIAN_POINT('Ctrl Pts',(-13.3487488038878,34.465161910175,20.1750617541494));
#49721=CARTESIAN_POINT('Ctrl Pts',(-13.3629151548252,34.5630003003109,20.1696205142505));
#49722=CARTESIAN_POINT('Ctrl Pts',(-13.3754286230421,34.6876131109885,20.1624711018325));
#49723=CARTESIAN_POINT('Ctrl Pts',(-13.377762174746,34.7139465840842,20.1609479117543));
#49724=CARTESIAN_POINT('Ctrl Pts',(-13.3810224023721,34.7563764520376,20.158469985341));
#49725=CARTESIAN_POINT('Ctrl Pts',(-13.3821427003247,34.7724573671774,20.1575253854599));
#49726=CARTESIAN_POINT('Ctrl Pts',(-13.3840196626613,34.802487637254,20.1557501933554));
#49727=CARTESIAN_POINT('Ctrl Pts',(-13.3848048711002,34.816434825108,20.1549211865484));
#49728=CARTESIAN_POINT('Ctrl Pts',(-13.3862870526388,34.846019257766,20.1531536454526));
#49729=CARTESIAN_POINT('Ctrl Pts',(-13.3869619660537,34.8616573387686,20.1522139712181));
#49730=CARTESIAN_POINT('Ctrl Pts',(-13.3889969374834,34.9178389117,20.1488201544703));
#49731=CARTESIAN_POINT('Ctrl Pts',(-13.3897374160989,34.9583996272579,20.1463364607818));
#49732=CARTESIAN_POINT('Ctrl Pts',(-13.3897498409689,34.9989616594858,20.1438254858951));
#49733=CARTESIAN_POINT('Ctrl Pts',(-13.3897498397739,34.9989577654279,20.1438257269549));
#49734=CARTESIAN_POINT('Ctrl Pts',(-13.389815647109,35.212988665529,20.1305762467729));
#49735=CARTESIAN_POINT('Ctrl Pts',(-13.3696105698165,35.426542922744,20.1166329548135));
#49736=CARTESIAN_POINT('Ctrl Pts',(-13.2942105014199,35.8207824637724,20.0908445206738));
#49737=CARTESIAN_POINT('Ctrl Pts',(-13.2438204622287,36.0015675863871,20.0789970994992));
#49738=CARTESIAN_POINT('Ctrl Pts',(-13.1787500740781,36.1772650632072,20.0676095644498));
#49739=CARTESIAN_POINT('Ctrl Pts',(-13.1787500668679,36.1772650826756,20.4156323441327));
#49740=CARTESIAN_POINT('Ctrl Pts',(-13.1797425060653,36.1745853835903,20.4158108520197));
#49741=CARTESIAN_POINT('Ctrl Pts',(-13.1807315795116,36.1719043681469,20.4159892768759));
#49742=CARTESIAN_POINT('Ctrl Pts',(-13.2150217790527,36.0785929896502,20.4221933131743));
#49743=CARTESIAN_POINT('Ctrl Pts',(-13.2444410083631,35.9865764817198,20.4281141169251));
#49744=CARTESIAN_POINT('Ctrl Pts',(-13.2797552998974,35.8573274305439,20.4361577408318));
#49745=CARTESIAN_POINT('Ctrl Pts',(-13.2890192969764,35.8210708756514,20.4383851970052));
#49746=CARTESIAN_POINT('Ctrl Pts',(-13.3039345590445,35.7583872572105,20.442188056826));
#49747=CARTESIAN_POINT('Ctrl Pts',(-13.3098735122455,35.7320329215109,20.4437724006817));
#49748=CARTESIAN_POINT('Ctrl Pts',(-13.3213964926778,35.6778891089177,20.4469987021115));
#49749=CARTESIAN_POINT('Ctrl Pts',(-13.3269482994619,35.650094907814,20.4486395360157));
#49750=CARTESIAN_POINT('Ctrl Pts',(-13.3402905138677,35.5786454319229,20.4528201443975));
#49751=CARTESIAN_POINT('Ctrl Pts',(-13.3475742214937,35.5349003089246,20.4553440538966));
#49752=CARTESIAN_POINT('Ctrl Pts',(-13.3779360928064,35.3275096800624,20.4671587069783));
#49753=CARTESIAN_POINT('Ctrl Pts',(-13.3898865541809,35.1624564179043,20.4761051573321));
#49754=CARTESIAN_POINT('Ctrl Pts',(-13.3895661465026,34.7779583694554,20.496610089433));
#49755=CARTESIAN_POINT('Ctrl Pts',(-13.3681189643523,34.5592939174178,20.5080099220275));
#49756=CARTESIAN_POINT('Ctrl Pts',(-13.3135660143134,34.2826222305813,20.5235640353451));
#49757=CARTESIAN_POINT('Ctrl Pts',(-13.2997048073285,34.2213487326185,20.5270844963043));
#49758=CARTESIAN_POINT('Ctrl Pts',(-13.2784570013726,34.1382266811757,20.5320070886447));
#49759=CARTESIAN_POINT('Ctrl Pts',(-13.2725372796528,34.1160128654812,20.5333371291529));
#49760=CARTESIAN_POINT('Ctrl Pts',(-13.2623153214775,34.0791653746228,20.5355701438627));
#49761=CARTESIAN_POINT('Ctrl Pts',(-13.2581393070868,34.0644969739984,20.5364661906848));
#49762=CARTESIAN_POINT('Ctrl Pts',(-13.2492696500637,34.0341218917911,20.5383373894828));
#49763=CARTESIAN_POINT('Ctrl Pts',(-13.2445608562356,34.0184203525582,20.5393133146451));
#49764=CARTESIAN_POINT('Ctrl Pts',(-13.2315887840289,33.976278173755,20.5419548364519));
#49765=CARTESIAN_POINT('Ctrl Pts',(-13.2231151333839,33.9499042061093,20.5436315920241));
#49766=CARTESIAN_POINT('Ctrl Pts',(-13.1716750416938,33.7962896327822,20.553524437595));
#49767=CARTESIAN_POINT('Ctrl Pts',(-13.1215037817248,33.6715991700884,20.562061248656));
#49768=CARTESIAN_POINT('Ctrl Pts',(-12.9399346243912,33.2878556099403,20.589325940471));
#49769=CARTESIAN_POINT('Ctrl Pts',(-12.7825810086151,33.0424625581116,20.6081405644321));
#49770=CARTESIAN_POINT('Ctrl Pts',(-12.5628257386086,32.7807730967697,20.6289128143236));
#49771=CARTESIAN_POINT('Ctrl Pts',(-12.5289001868035,32.7421895358724,20.6320009565101));
#49772=CARTESIAN_POINT('Ctrl Pts',(-12.4739358009627,32.6824724206787,20.6368237023879));
#49773=CARTESIAN_POINT('Ctrl Pts',(-12.4534737785582,32.6608208852368,20.6385816805327));
#49774=CARTESIAN_POINT('Ctrl Pts',(-12.4142506512456,32.6203985808672,20.6418827742585));
#49775=CARTESIAN_POINT('Ctrl Pts',(-12.3955494715002,32.6015730343549,20.6434282588747));
#49776=CARTESIAN_POINT('Ctrl Pts',(-12.3523583605508,32.5591038974443,20.6469346693323));
#49777=CARTESIAN_POINT('Ctrl Pts',(-12.3277292768483,32.5356055158479,20.6488892890816));
#49778=CARTESIAN_POINT('Ctrl Pts',(-12.2484675891758,32.4622312552077,20.6550439668156));
#49779=CARTESIAN_POINT('Ctrl Pts',(-12.1925527628919,32.4137691199468,20.6591861171708));
#49780=CARTESIAN_POINT('Ctrl Pts',(-12.0532841989469,32.300829128104,20.6690830366963));
#49781=CARTESIAN_POINT('Ctrl Pts',(-11.9684232613417,32.2383317956253,20.6747705005376));
#49782=CARTESIAN_POINT('Ctrl Pts',(-11.7775198450321,32.1110148445428,20.6870309010475));
#49783=CARTESIAN_POINT('Ctrl Pts',(-11.670549371612,32.0478690963406,20.6935705798324));
#49784=CARTESIAN_POINT('Ctrl Pts',(-11.4319116761727,31.9241313661927,20.7078775084907));
#49785=CARTESIAN_POINT('Ctrl Pts',(-11.2993455873243,31.8658283131306,20.7156539419354));
#49786=CARTESIAN_POINT('Ctrl Pts',(-11.1299936393782,31.8039414663263,20.7258346380206));
#49787=CARTESIAN_POINT('Ctrl Pts',(-11.0963225879659,31.792235615245,20.7278707354697));
#49788=CARTESIAN_POINT('Ctrl Pts',(-11.045347826199,31.7754103720041,20.7309797901621));
#49789=CARTESIAN_POINT('Ctrl Pts',(-11.0281765984122,31.7698942436056,20.7320315974449));
#49790=CARTESIAN_POINT('Ctrl Pts',(-10.996699326441,31.7600588248876,20.7339692903609));
#49791=CARTESIAN_POINT('Ctrl Pts',(-10.9824075808536,31.7556967336545,20.7348527668899));
#49792=CARTESIAN_POINT('Ctrl Pts',(-10.9491168725208,31.7457759651913,20.7369191236008));
#49793=CARTESIAN_POINT('Ctrl Pts',(-10.9300976093357,31.7402890769505,20.7381058664843));
#49794=CARTESIAN_POINT('Ctrl Pts',(-10.8673803913281,31.7227892767996,20.7420371358552));
#49795=CARTESIAN_POINT('Ctrl Pts',(-10.8234912005484,31.7114865533703,20.7448166523558));
#49796=CARTESIAN_POINT('Ctrl Pts',(-10.7142567059567,31.6856793011802,20.7517829456565));
#49797=CARTESIAN_POINT('Ctrl Pts',(-10.6486841291773,31.6722241161883,20.756007030276));
#49798=CARTESIAN_POINT('Ctrl Pts',(-10.306785163656,31.6125570765483,20.7781167424471));
#49799=CARTESIAN_POINT('Ctrl Pts',(-10.0258548807651,31.5987863553112,20.7964512385192));
#49800=CARTESIAN_POINT('Ctrl Pts',(-9.66575819337621,31.6257990533152,20.8188361769607));
#49801=CARTESIAN_POINT('Ctrl Pts',(-9.58532443139292,31.6347369463962,20.8237735179649));
#49802=CARTESIAN_POINT('Ctrl Pts',(-9.47305112889551,31.6513000427277,20.8305772292584));
#49803=CARTESIAN_POINT('Ctrl Pts',(-9.44088943014509,31.6565194783803,20.8325161164076));
#49804=CARTESIAN_POINT('Ctrl Pts',(-9.38225464696641,31.6669049079264,20.8360334522105));
#49805=CARTESIAN_POINT('Ctrl Pts',(-9.35575869732726,31.6719246672362,20.8376163014039));
#49806=CARTESIAN_POINT('Ctrl Pts',(-9.30195502547475,31.6827846158784,20.8408180503895));
#49807=CARTESIAN_POINT('Ctrl Pts',(-9.27465389840548,31.6886471356912,20.8424361151924));
#49808=CARTESIAN_POINT('Ctrl Pts',(-9.20621603358119,31.7042302060499,20.8464774005731));
#49809=CARTESIAN_POINT('Ctrl Pts',(-9.16518226108181,31.7143842150928,20.848886855502));
#49810=CARTESIAN_POINT('Ctrl Pts',(-8.98474201328525,31.762633844568,20.8594352965703));
#49811=CARTESIAN_POINT('Ctrl Pts',(-8.84765884685266,31.808855319541,20.8673163995646));
#49812=CARTESIAN_POINT('Ctrl Pts',(-8.59151044541241,31.9138908563147,20.8821575270251));
#49813=CARTESIAN_POINT('Ctrl Pts',(-8.47213069762243,31.9712166995524,20.8891280360757));
#49814=CARTESIAN_POINT('Ctrl Pts',(-8.22435600619584,32.108583239846,20.904191122184));
#49815=CARTESIAN_POINT('Ctrl Pts',(-8.09735488610336,32.1905275547102,20.9122867878498));
#49816=CARTESIAN_POINT('Ctrl Pts',(-7.94737604290737,32.3021424236888,20.922839006702));
#49817=CARTESIAN_POINT('Ctrl Pts',(-7.91884622173413,32.324089062384,20.9248943191478));
#49818=CARTESIAN_POINT('Ctrl Pts',(-7.87650097398503,32.3577500714075,20.9280268777391));
#49819=CARTESIAN_POINT('Ctrl Pts',(-7.8624202848406,32.3691283330538,20.9290824939516));
#49820=CARTESIAN_POINT('Ctrl Pts',(-7.8368896505127,32.3900992772204,20.9310235583407));
#49821=CARTESIAN_POINT('Ctrl Pts',(-7.82541100869835,32.3996556266936,20.9319065336308));
#49822=CARTESIAN_POINT('Ctrl Pts',(-7.79893616242646,32.4219947026402,20.9339668693319));
#49823=CARTESIAN_POINT('Ctrl Pts',(-7.78398791222559,32.4348326144344,20.935148012226));
#49824=CARTESIAN_POINT('Ctrl Pts',(-7.73543558904368,32.4772716093215,20.9390407552629));
#49825=CARTESIAN_POINT('Ctrl Pts',(-7.70230735446399,32.5074072528284,20.9417864512292));
#49826=CARTESIAN_POINT('Ctrl Pts',(-7.62199190422747,32.5834293511702,20.9486474289154));
#49827=CARTESIAN_POINT('Ctrl Pts',(-7.57552621564693,32.6300501686825,20.9527987036615));
#49828=CARTESIAN_POINT('Ctrl Pts',(-7.34854216910096,32.8714569250744,20.9738968739488));
#49829=CARTESIAN_POINT('Ctrl Pts',(-7.18997344677847,33.0856589319398,20.9912726918922));
#49830=CARTESIAN_POINT('Ctrl Pts',(-7.01179353570882,33.3969735796828,21.0136402124513));
#49831=CARTESIAN_POINT('Ctrl Pts',(-6.96889511597271,33.4796456953558,21.0193472387506));
#49832=CARTESIAN_POINT('Ctrl Pts',(-6.91339543848853,33.5983174965646,21.0272161549342));
#49833=CARTESIAN_POINT('Ctrl Pts',(-6.89791568122033,33.6329174810132,21.0294733407504));
#49834=CARTESIAN_POINT('Ctrl Pts',(-6.87247524486415,33.6924397935413,21.0332949632924));
#49835=CARTESIAN_POINT('Ctrl Pts',(-6.86222452049364,33.71723350163,21.0348689683744));
#49836=CARTESIAN_POINT('Ctrl Pts',(-6.84182957145973,33.7682711069477,21.0380735674958));
#49837=CARTESIAN_POINT('Ctrl Pts',(-6.83171555580551,33.7945248771616,21.039703064246));
#49838=CARTESIAN_POINT('Ctrl Pts',(-6.80686219933836,33.8615131432614,21.0438147284361));
#49839=CARTESIAN_POINT('Ctrl Pts',(-6.79257443114171,33.9024104607707,21.0462820811328));
#49840=CARTESIAN_POINT('Ctrl Pts',(-6.72912246092845,34.0958680872891,21.0577690469058));
#49841=CARTESIAN_POINT('Ctrl Pts',(-6.69003258528172,34.2515230287149,21.0664650471424));
#49842=CARTESIAN_POINT('Ctrl Pts',(-6.62808213176658,34.6016333246794,21.0854512244782));
#49843=CARTESIAN_POINT('Ctrl Pts',(-6.61073871748351,34.7964625318229,21.095635732872));
#49844=CARTESIAN_POINT('Ctrl Pts',(-6.61004403236768,35.0798746583062,21.1110424746374));
#49845=CARTESIAN_POINT('Ctrl Pts',(-6.61326910226161,35.1680262790533,21.1159213023215));
#49846=CARTESIAN_POINT('Ctrl Pts',(-6.62186746255237,35.2815785732353,21.1224286776713));
#49847=CARTESIAN_POINT('Ctrl Pts',(-6.62409999441359,35.3071888683805,21.1239110626468));
#49848=CARTESIAN_POINT('Ctrl Pts',(-6.62819059256733,35.3486562737177,21.1263387175266));
#49849=CARTESIAN_POINT('Ctrl Pts',(-6.62986982515734,35.3645304639123,21.1272745824342));
#49850=CARTESIAN_POINT('Ctrl Pts',(-6.63342828175083,35.3960403082881,21.1291462701152));
#49851=CARTESIAN_POINT('Ctrl Pts',(-6.63530446779698,35.4116758548307,21.1300819190504));
#49852=CARTESIAN_POINT('Ctrl Pts',(-6.6404032897058,35.4518021558286,21.132499866595));
#49853=CARTESIAN_POINT('Ctrl Pts',(-6.64378476590792,35.4762714232378,21.1339903971671));
#49854=CARTESIAN_POINT('Ctrl Pts',(-6.65998278926792,35.5847293276504,21.1406619454116));
#49855=CARTESIAN_POINT('Ctrl Pts',(-6.67568611000042,35.6682501579278,21.1459721910308));
#49856=CARTESIAN_POINT('Ctrl Pts',(-6.73647559923416,35.9357816445134,21.1633658340175));
#49857=CARTESIAN_POINT('Ctrl Pts',(-6.79384818005745,36.1166333244834,21.1756994660848));
#49858=CARTESIAN_POINT('Ctrl Pts',(-6.93043900063315,36.4480233758005,21.1986138881485));
#49859=CARTESIAN_POINT('Ctrl Pts',(-7.00645753782626,36.5992789627376,21.2092111198128));
#49860=CARTESIAN_POINT('Ctrl Pts',(-7.11632520716456,36.7823580349376,21.2221167445271));
#49861=CARTESIAN_POINT('Ctrl Pts',(-7.13994346702926,36.8200157650581,21.2247770012469));
#49862=CARTESIAN_POINT('Ctrl Pts',(-7.17983596922893,36.8809264604542,21.2290911223918));
#49863=CARTESIAN_POINT('Ctrl Pts',(-7.19567308560185,36.9044579649717,21.2307606300248));
#49864=CARTESIAN_POINT('Ctrl Pts',(-7.22716059674186,36.9499989318475,21.233998247697));
#49865=CARTESIAN_POINT('Ctrl Pts',(-7.24278229734094,36.9720255557289,21.2355672601181));
#49866=CARTESIAN_POINT('Ctrl Pts',(-7.28063547956017,37.0240693456179,21.2392832881431));
#49867=CARTESIAN_POINT('Ctrl Pts',(-7.30310341070712,37.0539106733541,21.2414211354459));
#49868=CARTESIAN_POINT('Ctrl Pts',(-7.3850914081183,37.159139396174,21.2489926650137));
#49869=CARTESIAN_POINT('Ctrl Pts',(-7.44731851084905,37.2323640575236,21.2543215322003));
#49870=CARTESIAN_POINT('Ctrl Pts',(-7.62047122176675,37.4193948861021,21.2682290237367));
#49871=CARTESIAN_POINT('Ctrl Pts',(-7.73642765146448,37.5282152295015,21.2766310950034));
#49872=CARTESIAN_POINT('Ctrl Pts',(-8.00343276518211,37.7456393773768,21.2948886017388));
#49873=CARTESIAN_POINT('Ctrl Pts',(-8.15663440121449,37.8507551754478,21.3047209487584));
#49874=CARTESIAN_POINT('Ctrl Pts',(-8.34779037152248,37.9600361858194,21.3171602556404));
#49875=CARTESIAN_POINT('Ctrl Pts',(-8.37819848513812,37.9768054234377,21.3191442489981));
#49876=CARTESIAN_POINT('Ctrl Pts',(-8.42481328278357,38.0015859805632,21.3222016483387));
#49877=CARTESIAN_POINT('Ctrl Pts',(-8.44083616375052,38.0099401476889,21.3232553930993));
#49878=CARTESIAN_POINT('Ctrl Pts',(-8.47022682634529,38.0249664955053,21.3251947955204));
#49879=CARTESIAN_POINT('Ctrl Pts',(-8.48357300990874,38.0316789769413,21.3260780115949));
#49880=CARTESIAN_POINT('Ctrl Pts',(-8.51466427973469,38.0470597091706,21.3281412813292));
#49881=CARTESIAN_POINT('Ctrl Pts',(-8.53244115773614,38.0556613156932,21.3293251566281));
#49882=CARTESIAN_POINT('Ctrl Pts',(-8.59100797757151,38.0833707946534,21.3332366609151));
#49883=CARTESIAN_POINT('Ctrl Pts',(-8.63210215704156,38.1018202806324,21.335998819727));
#49884=CARTESIAN_POINT('Ctrl Pts',(-8.73461192320585,38.1454094918872,21.3429109901449));
#49885=CARTESIAN_POINT('Ctrl Pts',(-8.7964205866403,38.1695746663377,21.3470976310758));
#49886=CARTESIAN_POINT('Ctrl Pts',(-9.11543363832712,38.2836215597325,21.368674145764));
#49887=CARTESIAN_POINT('Ctrl Pts',(-9.38213575284987,38.3440847577589,21.3865026970966));
#49888=CARTESIAN_POINT('Ctrl Pts',(-9.74023510837264,38.3809143995264,21.4088888187047));
#49889=CARTESIAN_POINT('Ctrl Pts',(-9.827587495936,38.3864931647787,21.4142409768036));
#49890=CARTESIAN_POINT('Ctrl Pts',(-9.95205552033723,38.3896129003117,21.4217121324108));
#49891=CARTESIAN_POINT('Ctrl Pts',(-9.98906068059602,38.3899343328772,21.4239140865079));
#49892=CARTESIAN_POINT('Ctrl Pts',(-10.0530088835909,38.3894426011005,21.4276873534833));
#49893=CARTESIAN_POINT('Ctrl Pts',(-10.0799500732001,38.3889141529525,21.4292672418271));
#49894=CARTESIAN_POINT('Ctrl Pts',(-10.1353445886381,38.387166631661,21.4324965665023));
#49895=CARTESIAN_POINT('Ctrl Pts',(-10.1637946459336,38.3859101190277,21.4341447244349));
#49896=CARTESIAN_POINT('Ctrl Pts',(-10.2371523686184,38.3817434400452,21.4383695440258));
#49897=CARTESIAN_POINT('Ctrl Pts',(-10.2820247112337,38.3782972440925,21.4409296549925));
#49898=CARTESIAN_POINT('Ctrl Pts',(-10.5256891312304,38.354694821158,21.4547205458477));
#49899=CARTESIAN_POINT('Ctrl Pts',(-10.7224763350515,38.3178857516672,21.4654249146074));
#49900=CARTESIAN_POINT('Ctrl Pts',(-11.1225155014591,38.2057539380884,21.4874766703825));
#49901=CARTESIAN_POINT('Ctrl Pts',(-11.3240902377039,38.1278850788692,21.4987635220807));
#49902=CARTESIAN_POINT('Ctrl Pts',(-11.5530583861937,38.0133123274318,21.5131507330899));
#49903=CARTESIAN_POINT('Ctrl Pts',(-11.5889067402504,37.9945645101524,21.5154526623596));
#49904=CARTESIAN_POINT('Ctrl Pts',(-11.6410367674659,37.9661022029266,21.518885668097));
#49905=CARTESIAN_POINT('Ctrl Pts',(-11.6575873778843,37.9568848470562,21.519988513745));
#49906=CARTESIAN_POINT('Ctrl Pts',(-11.6870198376183,37.9401685810241,21.5219744707776));
#49907=CARTESIAN_POINT('Ctrl Pts',(-11.6999307728334,37.9327227224269,21.5228543382273));
#49908=CARTESIAN_POINT('Ctrl Pts',(-11.7289774575403,37.9157149688938,21.5248537058461));
#49909=CARTESIAN_POINT('Ctrl Pts',(-11.7450831514072,37.9061041941658,21.5259761376055));
#49910=CARTESIAN_POINT('Ctrl Pts',(-11.7947931052927,37.8758784714215,21.5294816164314));
#49911=CARTESIAN_POINT('Ctrl Pts',(-11.8281169645073,37.8548112635178,21.5318904087556));
#49912=CARTESIAN_POINT('Ctrl Pts',(-11.9071561586478,37.8028916520861,21.5377324749079));
#49913=CARTESIAN_POINT('Ctrl Pts',(-11.9525002551562,37.7714956984792,21.5411901997962));
#49914=CARTESIAN_POINT('Ctrl Pts',(-12.136514583697,37.6373278664343,21.5556071252993));
#49915=CARTESIAN_POINT('Ctrl Pts',(-12.268001015821,37.5251461274097,21.5668228749371));
#49916=CARTESIAN_POINT('Ctrl Pts',(-12.5240270088587,37.2705124309373,21.5899908266797));
#49917=CARTESIAN_POINT('Ctrl Pts',(-12.6463770424732,37.1266512374872,21.6018687630537));
#49918=CARTESIAN_POINT('Ctrl Pts',(-12.7825202299871,36.9365018174192,21.6160149011046));
#49919=CARTESIAN_POINT('Ctrl Pts',(-12.808157399601,36.8991341279968,21.6187285328247));
#49920=CARTESIAN_POINT('Ctrl Pts',(-12.8487096072503,36.8374093653372,21.6231061785001));
#49921=CARTESIAN_POINT('Ctrl Pts',(-12.86407905636,36.8133589924949,21.6247867373711));
#49922=CARTESIAN_POINT('Ctrl Pts',(-12.8933487524465,36.7662566186755,21.628030633002));
#49923=CARTESIAN_POINT('Ctrl Pts',(-12.9072817377776,36.7432275826075,21.6295950738596));
#49924=CARTESIAN_POINT('Ctrl Pts',(-12.9396201242865,36.6883109745446,21.6332764619072));
#49925=CARTESIAN_POINT('Ctrl Pts',(-12.9577834163658,36.6562843457432,21.6353847132555));
#49926=CARTESIAN_POINT('Ctrl Pts',(-13.0195448673777,36.5431254308602,21.6427062204683));
#49927=CARTESIAN_POINT('Ctrl Pts',(-13.0603570280963,36.4605150202644,21.6478240567444));
#49928=CARTESIAN_POINT('Ctrl Pts',(-13.1268588912888,36.3108378906477,21.6567778185595));
#49929=CARTESIAN_POINT('Ctrl Pts',(-13.1538692920563,36.2444460084989,21.6606432273797));
#49930=CARTESIAN_POINT('Ctrl Pts',(-13.1787500358286,36.1772651664852,21.6644776847947));
#49931=CARTESIAN_POINT('Origin',(-10.,35.,23.));
#49932=CARTESIAN_POINT('',(-13.1787500671534,36.1772650819049,22.9104832616759));
#49933=CARTESIAN_POINT('',(-13.1787500907405,36.1772650182168,22.5700365663484));
#49934=CARTESIAN_POINT('',(-13.1787500671536,36.1772650819043,23.));
#49935=CARTESIAN_POINT('Ctrl Pts',(-13.1787500907405,36.1772650182168,22.5700365663484));
#49936=CARTESIAN_POINT('Ctrl Pts',(-13.1240748334016,36.3248944614926,22.5616683248361));
#49937=CARTESIAN_POINT('Ctrl Pts',(-13.0591692600091,36.4685690213728,22.5533981955439));
#49938=CARTESIAN_POINT('Ctrl Pts',(-12.953278579165,36.6651978966316,22.5413012604624));
#49939=CARTESIAN_POINT('Ctrl Pts',(-12.9203862141367,36.722231662174,22.5376917011256));
#49940=CARTESIAN_POINT('Ctrl Pts',(-12.862359117909,36.8164006997973,22.5315008009975));
#49941=CARTESIAN_POINT('Ctrl Pts',(-12.8381097881809,36.854061395087,22.5289600288544));
#49942=CARTESIAN_POINT('Ctrl Pts',(-12.8021282474947,36.9075824146467,22.5252382085787));
#49943=CARTESIAN_POINT('Ctrl Pts',(-12.7909917220288,36.9238395336274,22.5240925693446));
#49944=CARTESIAN_POINT('Ctrl Pts',(-12.7711659513161,36.9522467660789,22.522062233656));
#49945=CARTESIAN_POINT('Ctrl Pts',(-12.7625371644089,36.9644379776868,22.5211814602275));
#49946=CARTESIAN_POINT('Ctrl Pts',(-12.7432722266394,36.9912785471148,22.5192209971691));
#49947=CARTESIAN_POINT('Ctrl Pts',(-12.7325992555222,37.0058998075448,22.5181389779323));
#49948=CARTESIAN_POINT('Ctrl Pts',(-12.7003592927021,37.049331579848,22.5148843473055));
#49949=CARTESIAN_POINT('Ctrl Pts',(-12.6784506995931,37.0778839863913,22.512690789305));
#49950=CARTESIAN_POINT('Ctrl Pts',(-12.5622988252026,37.2243694035762,22.501176388498));
#49951=CARTESIAN_POINT('Ctrl Pts',(-12.4607148884698,37.3362511881488,22.4914956445948));
#49952=CARTESIAN_POINT('Ctrl Pts',(-12.2567899647403,37.5327443441236,22.4732517459289));
#49953=CARTESIAN_POINT('Ctrl Pts',(-12.1562644065705,37.6188587491143,22.4647131265315));
#49954=CARTESIAN_POINT('Ctrl Pts',(-11.9358421855869,37.7863642726116,22.447127787365));
#49955=CARTESIAN_POINT('Ctrl Pts',(-11.815233037322,37.8663999118682,22.438127609866));
#49956=CARTESIAN_POINT('Ctrl Pts',(-11.6532220051078,37.9595690612221,22.4268534458134));
#49957=CARTESIAN_POINT('Ctrl Pts',(-11.6161847975068,37.9799562025201,22.4243271679779));
#49958=CARTESIAN_POINT('Ctrl Pts',(-11.5540650684416,38.0126510786662,22.4201723334279));
#49959=CARTESIAN_POINT('Ctrl Pts',(-11.5291952260054,38.0253506886248,22.4185303210996));
#49960=CARTESIAN_POINT('Ctrl Pts',(-11.4800059931705,38.0497072693643,22.415323439542));
#49961=CARTESIAN_POINT('Ctrl Pts',(-11.4556988504484,38.0613841782599,22.4137579747704));
#49962=CARTESIAN_POINT('Ctrl Pts',(-11.4017242153313,38.0865248280804,22.4103227341902));
#49963=CARTESIAN_POINT('Ctrl Pts',(-11.3719965608593,38.0998535177034,22.408457601695));
#49964=CARTESIAN_POINT('Ctrl Pts',(-11.2678131543279,38.1447727838095,22.4020095182351));
#49965=CARTESIAN_POINT('Ctrl Pts',(-11.1924201109888,38.1741269200825,22.3974996356972));
#49966=CARTESIAN_POINT('Ctrl Pts',(-10.8514430469606,38.2930193095256,22.3776650327892));
#49967=CARTESIAN_POINT('Ctrl Pts',(-10.576441979743,38.3521092583466,22.3632575660505));
#49968=CARTESIAN_POINT('Ctrl Pts',(-10.2306418796184,38.3825565690339,22.3444676418831));
#49969=CARTESIAN_POINT('Ctrl Pts',(-10.1638143312928,38.386450735793,22.3408003520829));
#49970=CARTESIAN_POINT('Ctrl Pts',(-10.051617552822,38.3896599509054,22.3345210897479));
#49971=CARTESIAN_POINT('Ctrl Pts',(-10.0062969927845,38.3900470341661,22.3319512098715));
#49972=CARTESIAN_POINT('Ctrl Pts',(-9.94119071108923,38.3892976234969,22.3281943332827));
#49973=CARTESIAN_POINT('Ctrl Pts',(-9.92139969834953,38.388896408077,22.3270436734235));
#49974=CARTESIAN_POINT('Ctrl Pts',(-9.88667697117286,38.3878881699818,22.3250079580833));
#49975=CARTESIAN_POINT('Ctrl Pts',(-9.87174398862509,38.3873557157185,22.3241269046615));
#49976=CARTESIAN_POINT('Ctrl Pts',(-9.83879511612483,38.3859626885178,22.3221702433607));
#49977=CARTESIAN_POINT('Ctrl Pts',(-9.82078249799305,38.385057074477,22.3210923686942));
#49978=CARTESIAN_POINT('Ctrl Pts',(-9.76719231671656,38.3819338132044,22.3178628266232));
#49979=CARTESIAN_POINT('Ctrl Pts',(-9.73164263613224,38.3792987205387,22.315690666583));
#49980=CARTESIAN_POINT('Ctrl Pts',(-9.52762696058861,38.3609368272521,22.3030781511606));
#49981=CARTESIAN_POINT('Ctrl Pts',(-9.36049586365792,38.3331754301121,22.2921819110593));
#49982=CARTESIAN_POINT('Ctrl Pts',(-9.03469859496188,38.2536468917318,22.2705642625866));
#49983=CARTESIAN_POINT('Ctrl Pts',(-8.87635205915459,38.2024128624622,22.2598737825077));
#49984=CARTESIAN_POINT('Ctrl Pts',(-8.65816652165064,38.1136307064377,22.245136206382));
#49985=CARTESIAN_POINT('Ctrl Pts',(-8.59475315223077,38.0855300236096,22.2408496240776));
#49986=CARTESIAN_POINT('Ctrl Pts',(-8.48292021989554,38.0318093784302,22.2332891459944));
#49987=CARTESIAN_POINT('Ctrl Pts',(-8.4341762795063,38.0069246355187,22.2299933809457));
#49988=CARTESIAN_POINT('Ctrl Pts',(-8.35926028906029,37.966362523062,22.2249251786272));
#49989=CARTESIAN_POINT('Ctrl Pts',(-8.33266280069066,37.9514945657911,22.2231251927658));
#49990=CARTESIAN_POINT('Ctrl Pts',(-8.28336520002296,37.9230581828056,22.2197867477784));
#49991=CARTESIAN_POINT('Ctrl Pts',(-8.26061657955208,37.9095789303039,22.2182452969182));
#49992=CARTESIAN_POINT('Ctrl Pts',(-8.20984725963833,37.8786883038778,22.2148019413831));
#49993=CARTESIAN_POINT('Ctrl Pts',(-8.18191811509319,37.8611311668697,22.2129054537828));
#49994=CARTESIAN_POINT('Ctrl Pts',(-8.09727621906227,37.8061826628612,22.2071471304879));
#49995=CARTESIAN_POINT('Ctrl Pts',(-8.04142568974309,37.767491002517,22.2033327186608));
#49996=CARTESIAN_POINT('Ctrl Pts',(-7.78494965597834,37.5781558283928,22.1856728776683));
#49997=CARTESIAN_POINT('Ctrl Pts',(-7.60029304008272,37.4072280026226,22.1726005173881));
#49998=CARTESIAN_POINT('Ctrl Pts',(-7.37136608705129,37.1425465210397,22.1539345267788));
#49999=CARTESIAN_POINT('Ctrl Pts',(-7.30987100487107,37.0648064418633,22.1486010838034));
#50000=CARTESIAN_POINT('Ctrl Pts',(-7.22811837760224,36.9515951551464,22.1408731518037));
#50001=CARTESIAN_POINT('Ctrl Pts',(-7.20495776541068,36.9182778810178,22.1386032305441));
#50002=CARTESIAN_POINT('Ctrl Pts',(-7.16496794475606,36.8584890737967,22.1345224653878));
#50003=CARTESIAN_POINT('Ctrl Pts',(-7.14789738789962,36.8321841976466,22.1327246341959));
#50004=CARTESIAN_POINT('Ctrl Pts',(-7.1220499668426,36.7911179193518,22.1299080658624));
#50005=CARTESIAN_POINT('Ctrl Pts',(-7.11301579520889,36.7765196221734,22.1289049352438));
#50006=CARTESIAN_POINT('Ctrl Pts',(-7.09624203462262,36.748949086996,22.1270056462231));
#50007=CARTESIAN_POINT('Ctrl Pts',(-7.08847770369093,36.7359928326479,22.1261110472179));
#50008=CARTESIAN_POINT('Ctrl Pts',(-7.07001483287942,36.7047117752317,22.1239467244453));
#50009=CARTESIAN_POINT('Ctrl Pts',(-7.05940139866072,36.6863377868322,22.1226718851205));
#50010=CARTESIAN_POINT('Ctrl Pts',(-7.02428562987325,36.6242057010499,22.118352224853));
#50011=CARTESIAN_POINT('Ctrl Pts',(-7.00058306537671,36.5800055927959,22.1152648488027));
#50012=CARTESIAN_POINT('Ctrl Pts',(-6.88474934629017,36.3519949274575,22.099325458337));
#50013=CARTESIAN_POINT('Ctrl Pts',(-6.80850146248942,36.1606070220361,22.0859336384872));
#50014=CARTESIAN_POINT('Ctrl Pts',(-6.70408338379959,35.8083990017249,22.062346420005));
#50015=CARTESIAN_POINT('Ctrl Pts',(-6.66925905913548,35.6501926389613,22.0521019447303));
#50016=CARTESIAN_POINT('Ctrl Pts',(-6.63669862728671,35.4273510782366,22.0382965542551));
#50017=CARTESIAN_POINT('Ctrl Pts',(-6.62929335743372,35.3643660270074,22.0344606193522));
#50018=CARTESIAN_POINT('Ctrl Pts',(-6.620801378988,35.2691762886354,22.0287603734784));
#50019=CARTESIAN_POINT('Ctrl Pts',(-6.61839976213907,35.2371057417626,22.0268563351426));
#50020=CARTESIAN_POINT('Ctrl Pts',(-6.61501361606447,35.1812184367081,22.0235657910832));
#50021=CARTESIAN_POINT('Ctrl Pts',(-6.61382326067023,35.1574168803638,22.0221730578377));
#50022=CARTESIAN_POINT('Ctrl Pts',(-6.61169611075612,35.103489693268,22.0190363317463));
#50023=CARTESIAN_POINT('Ctrl Pts',(-6.61090989077505,35.0733599246977,22.0172970754516));
#50024=CARTESIAN_POINT('Ctrl Pts',(-6.60986657974326,34.9915451606357,22.0126077806275));
#50025=CARTESIAN_POINT('Ctrl Pts',(-6.61038950006398,34.9398572932841,22.009681622323));
#50026=CARTESIAN_POINT('Ctrl Pts',(-6.62000305866061,34.6485360722685,21.9933597521017));
#50027=CARTESIAN_POINT('Ctrl Pts',(-6.65331888001949,34.410387545852,21.9807292090286));
#50028=CARTESIAN_POINT('Ctrl Pts',(-6.75543340137381,34.0019990613022,21.9583899477608));
#50029=CARTESIAN_POINT('Ctrl Pts',(-6.81338542707709,33.8300893896225,21.9487366449005));
#50030=CARTESIAN_POINT('Ctrl Pts',(-6.89610746265219,33.6372522247897,21.9367942635273));
#50031=CARTESIAN_POINT('Ctrl Pts',(-6.90776787490348,33.6109964899008,21.9351430178509));
#50032=CARTESIAN_POINT('Ctrl Pts',(-6.92669539641054,33.5697972673561,21.9325071339685));
#50033=CARTESIAN_POINT('Ctrl Pts',(-6.93374134454911,33.5547530053815,21.9315350624761));
#50034=CARTESIAN_POINT('Ctrl Pts',(-6.94741911519368,33.5260989854699,21.9296641597028));
#50035=CARTESIAN_POINT('Ctrl Pts',(-6.95403197758398,33.5124809137856,21.928766426658));
#50036=CARTESIAN_POINT('Ctrl Pts',(-6.97063926822555,33.478856094825,21.9265292187996));
#50037=CARTESIAN_POINT('Ctrl Pts',(-6.98074081353265,33.4589032705041,21.9251835109177));
#50038=CARTESIAN_POINT('Ctrl Pts',(-7.01790422861383,33.3872651962381,21.9202899813154));
#50039=CARTESIAN_POINT('Ctrl Pts',(-7.0461006201939,33.3361831949844,21.9166833221699));
#50040=CARTESIAN_POINT('Ctrl Pts',(-7.1761218337607,33.1143614177892,21.9005780598949));
#50041=CARTESIAN_POINT('Ctrl Pts',(-7.29153158692936,32.952045916123,21.8876329515913));
#50042=CARTESIAN_POINT('Ctrl Pts',(-7.44846752083327,32.7679726580888,21.8721105511825));
#50043=CARTESIAN_POINT('Ctrl Pts',(-7.47706437847027,32.735698778186,21.8693527459737));
#50044=CARTESIAN_POINT('Ctrl Pts',(-7.57490202988622,32.6294363836983,21.8601597966048));
#50045=CARTESIAN_POINT('Ctrl Pts',(-7.6468462254978,32.5580045040303,21.8537928138538));
#50046=CARTESIAN_POINT('Ctrl Pts',(-7.77521704371321,32.4414979959072,21.8431098197026));
#50047=CARTESIAN_POINT('Ctrl Pts',(-7.83007809760845,32.3948067609101,21.8387355263668));
#50048=CARTESIAN_POINT('Ctrl Pts',(-7.9127393274734,32.3288796334042,21.8324157722934));
#50049=CARTESIAN_POINT('Ctrl Pts',(-7.93940298999155,32.3082568448392,21.8304165424675));
#50050=CARTESIAN_POINT('Ctrl Pts',(-7.98757233747021,32.2721359549518,21.8268730029141));
#50051=CARTESIAN_POINT('Ctrl Pts',(-8.00896026393256,32.2564861630127,21.8253229367178));
#50052=CARTESIAN_POINT('Ctrl Pts',(-8.05493692332513,32.2236653744321,21.8220390784082));
#50053=CARTESIAN_POINT('Ctrl Pts',(-8.07957453643129,32.2065665485705,21.8203080919864));
#50054=CARTESIAN_POINT('Ctrl Pts',(-8.1467024904504,32.1612868003273,21.8156662648115));
#50055=CARTESIAN_POINT('Ctrl Pts',(-8.18960781887453,32.1337332958274,21.8127784657201));
#50056=CARTESIAN_POINT('Ctrl Pts',(-8.44415620060174,31.9782611691288,21.7960670437488));
#50057=CARTESIAN_POINT('Ctrl Pts',(-8.66866182100946,31.8728439018321,21.7830677304709));
#50058=CARTESIAN_POINT('Ctrl Pts',(-9.01623991895204,31.7539202875529,21.7635622020818));
#50059=CARTESIAN_POINT('Ctrl Pts',(-9.13180493708184,31.7211203909402,21.7571573977968));
#50060=CARTESIAN_POINT('Ctrl Pts',(-9.31376983133033,31.6797704506472,21.7468827496576));
#50061=CARTESIAN_POINT('Ctrl Pts',(-9.37909728951348,31.6669361288875,21.7431563619037));
#50062=CARTESIAN_POINT('Ctrl Pts',(-9.4672545123361,31.6522981821704,21.7380274703794));
#50063=CARTESIAN_POINT('Ctrl Pts',(-9.48978981083185,31.6487896637498,21.7367076573531));
#50064=CARTESIAN_POINT('Ctrl Pts',(-9.52756791276552,31.6432978667114,21.7344779852149));
#50065=CARTESIAN_POINT('Ctrl Pts',(-9.5427923625267,31.6411903212946,21.7335747765295));
#50066=CARTESIAN_POINT('Ctrl Pts',(-9.57439489128271,31.6370343778509,21.7316893902204));
#50067=CARTESIAN_POINT('Ctrl Pts',(-9.59077432647982,31.6350019602782,21.7307064528448));
#50068=CARTESIAN_POINT('Ctrl Pts',(-9.63520371504883,31.6298181861203,21.7280258497445));
#50069=CARTESIAN_POINT('Ctrl Pts',(-9.6632786462595,31.6268975104417,21.7263164799453));
#50070=CARTESIAN_POINT('Ctrl Pts',(-9.83078740627791,31.61158334856,21.7160381847619));
#50071=CARTESIAN_POINT('Ctrl Pts',(-9.97083258109448,31.6074872991042,21.7071230645722));
#50072=CARTESIAN_POINT('Ctrl Pts',(-10.3106000012477,31.618590645801,21.6852706723473));
#50073=CARTESIAN_POINT('Ctrl Pts',(-10.5095317489432,31.642800216435,21.6723092961866));
#50074=CARTESIAN_POINT('Ctrl Pts',(-10.8113716252329,31.7069969791034,21.6529507523898));
#50075=CARTESIAN_POINT('Ctrl Pts',(-10.9164288150099,31.7346738502891,21.6462658129306));
#50076=CARTESIAN_POINT('Ctrl Pts',(-11.0570826479788,31.7790537778506,21.6373977359519));
#50077=CARTESIAN_POINT('Ctrl Pts',(-11.0939768985247,31.7913970290446,21.6350790906563));
#50078=CARTESIAN_POINT('Ctrl Pts',(-11.1563641943484,31.8134704131955,21.6311696554965));
#50079=CARTESIAN_POINT('Ctrl Pts',(-11.1819664934257,31.8228779956116,21.6295685967896));
#50080=CARTESIAN_POINT('Ctrl Pts',(-11.2304957023538,31.8413779088336,21.6265391418273));
#50081=CARTESIAN_POINT('Ctrl Pts',(-11.2534422592592,31.8504134020597,21.6251090013564));
#50082=CARTESIAN_POINT('Ctrl Pts',(-11.3070591832291,31.8722045179716,21.6217716846679));
#50083=CARTESIAN_POINT('Ctrl Pts',(-11.3376449986924,31.8851622428578,21.6198712984982));
#50084=CARTESIAN_POINT('Ctrl Pts',(-11.4468686778143,31.9333406120716,21.6130920692451));
#50085=CARTESIAN_POINT('Ctrl Pts',(-11.5243504206456,31.9711080911887,21.6082974731666));
#50086=CARTESIAN_POINT('Ctrl Pts',(-11.8417918393518,32.1411114185032,21.5885705416975));
#50087=CARTESIAN_POINT('Ctrl Pts',(-12.0666879679872,32.299216324603,21.5744752797977));
#50088=CARTESIAN_POINT('Ctrl Pts',(-12.3194610678473,32.527163003976,21.5560460291012));
#50089=CARTESIAN_POINT('Ctrl Pts',(-12.3674970106603,32.5731132133238,21.5524031605411));
#50090=CARTESIAN_POINT('Ctrl Pts',(-12.445805707116,32.6525602928082,21.5461612535621));
#50091=CARTESIAN_POINT('Ctrl Pts',(-12.4768170330812,32.6853044006922,21.5436036597938));
#50092=CARTESIAN_POINT('Ctrl Pts',(-12.5204614908523,32.7332690282505,21.5398615764893));
#50093=CARTESIAN_POINT('Ctrl Pts',(-12.5336302373429,32.7479979563091,21.5387130307118));
#50094=CARTESIAN_POINT('Ctrl Pts',(-12.5565294316919,32.7740652431572,21.5366795845223));
#50095=CARTESIAN_POINT('Ctrl Pts',(-12.5663148466432,32.7853541202747,21.5357986529009));
#50096=CARTESIAN_POINT('Ctrl Pts',(-12.5877666462179,32.8104349434227,21.533840407924));
#50097=CARTESIAN_POINT('Ctrl Pts',(-12.5993974742058,32.8242555087767,21.5327608015043));
#50098=CARTESIAN_POINT('Ctrl Pts',(-12.6330425918723,32.8648898460294,21.5295867470802));
#50099=CARTESIAN_POINT('Ctrl Pts',(-12.6547557452605,32.8919486740716,21.5274732911627));
#50100=CARTESIAN_POINT('Ctrl Pts',(-12.7903104244531,33.0662924111964,21.5138823619218));
#50101=CARTESIAN_POINT('Ctrl Pts',(-12.8922641625607,33.2224017677656,21.5018489434669));
#50102=CARTESIAN_POINT('Ctrl Pts',(-13.0562996617983,33.5253717271096,21.4796451306051));
#50103=CARTESIAN_POINT('Ctrl Pts',(-13.1218667113147,33.6697925283375,21.4694888105455));
#50104=CARTESIAN_POINT('Ctrl Pts',(-13.2105289880325,33.9081640681836,21.4536217906998));
#50105=CARTESIAN_POINT('Ctrl Pts',(-13.240134312842,33.9994329603985,21.4477424264719));
#50106=CARTESIAN_POINT('Ctrl Pts',(-13.2758327438995,34.1278082103715,21.4397439961777));
#50107=CARTESIAN_POINT('Ctrl Pts',(-13.2852397255235,34.1639385208381,21.4375218599814));
#50108=CARTESIAN_POINT('Ctrl Pts',(-13.3004184563616,34.2264548939642,21.4337251817474));
#50109=CARTESIAN_POINT('Ctrl Pts',(-13.3064751189927,34.2527675271827,21.4321417758316));
#50110=CARTESIAN_POINT('Ctrl Pts',(-13.3182496956387,34.3068702776582,21.4289148941704));
#50111=CARTESIAN_POINT('Ctrl Pts',(-13.3239344023853,34.3346654868932,21.4272725738821));
#50112=CARTESIAN_POINT('Ctrl Pts',(-13.3376335907142,34.4062112064827,21.4230829777617));
#50113=CARTESIAN_POINT('Ctrl Pts',(-13.3451372988414,34.4500547052136,21.4205517055033));
#50114=CARTESIAN_POINT('Ctrl Pts',(-13.3771969725709,34.6624345785642,21.4084462577946));
#50115=CARTESIAN_POINT('Ctrl Pts',(-13.3898921005314,34.8325187363542,21.3992403245363));
#50116=CARTESIAN_POINT('Ctrl Pts',(-13.389547595615,35.2420129420187,21.3774222643481));
#50117=CARTESIAN_POINT('Ctrl Pts',(-13.3640366786116,35.4804553378116,21.3650138727178));
#50118=CARTESIAN_POINT('Ctrl Pts',(-13.3041286241496,35.7584090300179,21.3491057155548));
#50119=CARTESIAN_POINT('Ctrl Pts',(-13.2937170393995,35.8024200146644,21.3465411345039));
#50120=CARTESIAN_POINT('Ctrl Pts',(-13.2775434416502,35.8651572202666,21.3428027266053));
#50121=CARTESIAN_POINT('Ctrl Pts',(-13.272494286683,35.8840639862052,21.3416652449651));
#50122=CARTESIAN_POINT('Ctrl Pts',(-13.2632990017694,35.9173375929995,21.3396425222441));
#50123=CARTESIAN_POINT('Ctrl Pts',(-13.2592210829668,35.9317223597353,21.338761064133));
#50124=CARTESIAN_POINT('Ctrl Pts',(-13.2500375059252,35.9633190315991,21.3368090748593));
#50125=CARTESIAN_POINT('Ctrl Pts',(-13.2448902763815,35.9805174190649,21.3357363553798));
#50126=CARTESIAN_POINT('Ctrl Pts',(-13.2292397832685,36.0313370858835,21.332537864918));
#50127=CARTESIAN_POINT('Ctrl Pts',(-13.2183491101846,36.0648354603712,21.3303921567018));
#50128=CARTESIAN_POINT('Ctrl Pts',(-13.1978681340611,36.1246459099784,21.3265010764352));
#50129=CARTESIAN_POINT('Ctrl Pts',(-13.1884710276968,36.1510173784738,21.3247642005658));
#50130=CARTESIAN_POINT('Ctrl Pts',(-13.1787500764527,36.1772650567955,21.3230161660245));
#50131=CARTESIAN_POINT('',(-13.3897506916886,35.0009530681513,21.7311315226218));
#50132=CARTESIAN_POINT('Ctrl Pts',(-13.1787500358286,36.1772651664852,21.6644776847947));
#50133=CARTESIAN_POINT('Ctrl Pts',(-13.2052005884591,36.1058456617591,21.6685540708782));
#50134=CARTESIAN_POINT('Ctrl Pts',(-13.229244265339,36.0335344957176,21.6725954405618));
#50135=CARTESIAN_POINT('Ctrl Pts',(-13.2853773975532,35.8435413485962,21.6830989269644));
#50136=CARTESIAN_POINT('Ctrl Pts',(-13.3135856461982,35.7248549705581,21.689546781913));
#50137=CARTESIAN_POINT('Ctrl Pts',(-13.3523689842039,35.5110130260137,21.7013224548051));
#50138=CARTESIAN_POINT('Ctrl Pts',(-13.3654247099463,35.4164440716398,21.7065851171462));
#50139=CARTESIAN_POINT('Ctrl Pts',(-13.3769574710367,35.2953803598093,21.713529728992));
#50140=CARTESIAN_POINT('Ctrl Pts',(-13.3791392803472,35.2692748645804,21.7150394842961));
#50141=CARTESIAN_POINT('Ctrl Pts',(-13.3821708195026,35.2271206727215,21.7175008534419));
#50142=CARTESIAN_POINT('Ctrl Pts',(-13.3832094035605,35.2110861454004,21.7184425739285));
#50143=CARTESIAN_POINT('Ctrl Pts',(-13.3849363276215,35.1811231303917,21.7202135320163));
#50144=CARTESIAN_POINT('Ctrl Pts',(-13.3856527877675,35.1671966216966,21.7210412028214));
#50145=CARTESIAN_POINT('Ctrl Pts',(-13.3869928539982,35.1375890736215,21.7228099230972));
#50146=CARTESIAN_POINT('Ctrl Pts',(-13.3875935323677,35.1219072807308,21.7237521568866));
#50147=CARTESIAN_POINT('Ctrl Pts',(-13.3891851612891,35.071140361859,21.7268187924234));
#50148=CARTESIAN_POINT('Ctrl Pts',(-13.3897400387479,35.0360451300958,21.7289639786243));
#50149=CARTESIAN_POINT('Ctrl Pts',(-13.3897498670814,35.0009492742509,21.7311303263703));
#50150=CARTESIAN_POINT('Ctrl Pts',(-13.3897498660416,35.0009529799439,21.7311300976305));
#50151=CARTESIAN_POINT('Ctrl Pts',(-13.3897871967006,34.8681678178271,21.7393264681746));
#50152=CARTESIAN_POINT('Ctrl Pts',(-13.3820221592067,34.7355012784614,21.7478135385921));
#50153=CARTESIAN_POINT('Ctrl Pts',(-13.3370444115537,34.3534811525516,21.7725674067684));
#50154=CARTESIAN_POINT('Ctrl Pts',(-13.2797947392605,34.107345296519,21.7888426133663));
#50155=CARTESIAN_POINT('Ctrl Pts',(-13.1743644891748,33.8092252777544,21.8082373372983));
#50156=CARTESIAN_POINT('Ctrl Pts',(-13.1512200789771,33.7492613384332,21.812126653608));
#50157=CARTESIAN_POINT('Ctrl Pts',(-13.1138941227878,33.6601817731483,21.8178887982532));
#50158=CARTESIAN_POINT('Ctrl Pts',(-13.1009786533478,33.6305544958312,21.8198026613793));
#50159=CARTESIAN_POINT('Ctrl Pts',(-13.077800747378,33.5793958307059,21.8231039824557));
#50160=CARTESIAN_POINT('Ctrl Pts',(-13.0677312919129,33.5577800410288,21.8244977974237));
#50161=CARTESIAN_POINT('Ctrl Pts',(-13.0444706661095,33.5091932600773,21.8276291075011));
#50162=CARTESIAN_POINT('Ctrl Pts',(-13.0311474861603,33.4822874536548,21.8293619705711));
#50163=CARTESIAN_POINT('Ctrl Pts',(-12.9941673416453,33.4100369769172,21.8340145630055));
#50164=CARTESIAN_POINT('Ctrl Pts',(-12.9698383377374,33.3650440019246,21.8369110616529));
#50165=CARTESIAN_POINT('Ctrl Pts',(-12.8227627523316,33.1071730957554,21.853541525632));
#50166=CARTESIAN_POINT('Ctrl Pts',(-12.6781801189912,32.9075981196782,21.8664638158916));
#50167=CARTESIAN_POINT('Ctrl Pts',(-12.4321209232357,32.6357196241759,21.8859314784994));
#50168=CARTESIAN_POINT('Ctrl Pts',(-12.3462237179379,32.5504561934043,21.8923819588513));
#50169=CARTESIAN_POINT('Ctrl Pts',(-12.2060547807196,32.4254712953345,21.9027204457817));
#50170=CARTESIAN_POINT('Ctrl Pts',(-12.1548471869276,32.3824614284095,21.9064628609247));
#50171=CARTESIAN_POINT('Ctrl Pts',(-12.0844870797371,32.3268295159777,21.9116105286617));
#50172=CARTESIAN_POINT('Ctrl Pts',(-12.0664269862487,32.312844204056,21.9129323165402));
#50173=CARTESIAN_POINT('Ctrl Pts',(-12.0359757077302,32.2897519657831,21.915164349922));
#50174=CARTESIAN_POINT('Ctrl Pts',(-12.0236610282268,32.2805446271314,21.9160679129245));
#50175=CARTESIAN_POINT('Ctrl Pts',(-11.9980080842283,32.2616353824461,21.9179529107245));
#50176=CARTESIAN_POINT('Ctrl Pts',(-11.9846610627102,32.2519465936043,21.9189350918329));
#50177=CARTESIAN_POINT('Ctrl Pts',(-11.94832746727,32.2259742839834,21.9216114751428));
#50178=CARTESIAN_POINT('Ctrl Pts',(-11.9252082416032,32.2098796250075,21.92331732207));
#50179=CARTESIAN_POINT('Ctrl Pts',(-11.788424375324,32.1171657477977,21.9334139011426));
#50180=CARTESIAN_POINT('Ctrl Pts',(-11.6704058533844,32.0472161404183,21.9421366455033));
#50181=CARTESIAN_POINT('Ctrl Pts',(-11.3685700309193,31.8922147832037,21.9639392891909));
#50182=CARTESIAN_POINT('Ctrl Pts',(-11.1807258807694,31.8161013081737,21.9770543761855));
#50183=CARTESIAN_POINT('Ctrl Pts',(-10.8827796239532,31.7253975200335,21.9965967614637));
#50184=CARTESIAN_POINT('Ctrl Pts',(-10.7768680187487,31.6986667489452,22.0033193268099));
#50185=CARTESIAN_POINT('Ctrl Pts',(-10.6316422157301,31.6693916961895,22.0122275768809));
#50186=CARTESIAN_POINT('Ctrl Pts',(-10.5933116178055,31.6623503664467,22.0145503874427));
#50187=CARTESIAN_POINT('Ctrl Pts',(-10.5279481342339,31.651504755951,22.0184647135941));
#50188=CARTESIAN_POINT('Ctrl Pts',(-10.5009758692781,31.6473632950838,22.0200665596888));
#50189=CARTESIAN_POINT('Ctrl Pts',(-10.4495495423893,31.6401015162877,22.0230961623548));
#50190=CARTESIAN_POINT('Ctrl Pts',(-10.4251058324832,31.6369213970013,22.0245256801874));
#50191=CARTESIAN_POINT('Ctrl Pts',(-10.3614124523037,31.6293404448622,22.0282245237038));
#50192=CARTESIAN_POINT('Ctrl Pts',(-10.3221161121198,31.6253583610429,22.0304808456655));
#50193=CARTESIAN_POINT('Ctrl Pts',(-10.17830453932,31.6133202809862,22.0386533215906));
#50194=CARTESIAN_POINT('Ctrl Pts',(-10.0734964515061,31.6094258547114,22.0444436988178));
#50195=CARTESIAN_POINT('Ctrl Pts',(-9.71660611565063,31.6127246681469,22.0638272162417));
#50196=CARTESIAN_POINT('Ctrl Pts',(-9.46560577388935,31.6431621920133,22.0768390208613));
#50197=CARTESIAN_POINT('Ctrl Pts',(-9.15738022643535,31.7160118582454,22.0940076768971));
#50198=CARTESIAN_POINT('Ctrl Pts',(-9.0948937655809,31.732681822105,22.0975560429474));
#50199=CARTESIAN_POINT('Ctrl Pts',(-8.99053895859396,31.7637445592702,22.1036530666487));
#50200=CARTESIAN_POINT('Ctrl Pts',(-8.94840541126325,31.7771892220145,22.1061627413326));
#50201=CARTESIAN_POINT('Ctrl Pts',(-8.88798770104519,31.7977791696906,22.1098470753705));
#50202=CARTESIAN_POINT('Ctrl Pts',(-8.86948207477235,31.8042655335771,22.110987304417));
#50203=CARTESIAN_POINT('Ctrl Pts',(-8.83711662853796,31.8159261676621,22.1130038592239));
#50204=CARTESIAN_POINT('Ctrl Pts',(-8.82323278726384,31.8210311703321,22.1138762480749));
#50205=CARTESIAN_POINT('Ctrl Pts',(-8.79242670489897,31.8325878457828,22.1158286510366));
#50206=CARTESIAN_POINT('Ctrl Pts',(-8.77552267719398,31.8390842669947,22.116911108101));
#50207=CARTESIAN_POINT('Ctrl Pts',(-8.72514961835843,31.8589079368591,22.1201683968653));
#50208=CARTESIAN_POINT('Ctrl Pts',(-8.69184114462838,31.8726332114071,22.1223642235575));
#50209=CARTESIAN_POINT('Ctrl Pts',(-8.51964182168825,31.9468228370251,22.1339131329145));
#50210=CARTESIAN_POINT('Ctrl Pts',(-8.38470903366246,32.0160128949617,22.1436284602083));
#50211=CARTESIAN_POINT('Ctrl Pts',(-8.14053051457069,32.1626481525991,22.1619784413374));
#50212=CARTESIAN_POINT('Ctrl Pts',(-8.03034162285736,32.238000588316,22.1705886982985));
#50213=CARTESIAN_POINT('Ctrl Pts',(-7.84914557794703,32.3782824252039,22.1851383292965));
#50214=CARTESIAN_POINT('Ctrl Pts',(-7.77592928735999,32.4400996975595,22.191141514427));
#50215=CARTESIAN_POINT('Ctrl Pts',(-7.65446323979724,32.5518055802909,22.2012941381525));
#50216=CARTESIAN_POINT('Ctrl Pts',(-7.60494707278587,32.6002247757725,22.2054942486877));
#50217=CARTESIAN_POINT('Ctrl Pts',(-7.53391680625709,32.6740717301949,22.211614716734));
#50218=CARTESIAN_POINT('Ctrl Pts',(-7.51124033835845,32.6983518732947,22.213584092283));
#50219=CARTESIAN_POINT('Ctrl Pts',(-7.47131293553962,32.7423830903402,22.2170808483868));
#50220=CARTESIAN_POINT('Ctrl Pts',(-7.45392758289421,32.7620081133185,22.2186137523732));
#50221=CARTESIAN_POINT('Ctrl Pts',(-7.4169986531111,32.8046817735381,22.2218934033547));
#50222=CARTESIAN_POINT('Ctrl Pts',(-7.39753196867647,32.8277941385416,22.2236369559785));
#50223=CARTESIAN_POINT('Ctrl Pts',(-7.34538328570631,32.8914165980645,22.2283509535885));
#50224=CARTESIAN_POINT('Ctrl Pts',(-7.31332041030026,32.9324248386212,22.2312970767807));
#50225=CARTESIAN_POINT('Ctrl Pts',(-7.14180156178449,33.1625273605921,22.2473632307134));
#50226=CARTESIAN_POINT('Ctrl Pts',(-7.02135205553594,33.3649857624503,22.2597546337074));
#50227=CARTESIAN_POINT('Ctrl Pts',(-6.84536550365538,33.7458966409345,22.2820149374201));
#50228=CARTESIAN_POINT('Ctrl Pts',(-6.78175997293218,33.9195327300596,22.2918389028713));
#50229=CARTESIAN_POINT('Ctrl Pts',(-6.72486051399581,34.1255207552602,22.3039957312443));
#50230=CARTESIAN_POINT('Ctrl Pts',(-6.71747123191749,34.1536801024915,22.3056684144008));
#50231=CARTESIAN_POINT('Ctrl Pts',(-6.70641680112374,34.1981312548462,22.3083307426546));
#50232=CARTESIAN_POINT('Ctrl Pts',(-6.70250762009858,34.2143615645847,22.3093073938329));
#50233=CARTESIAN_POINT('Ctrl Pts',(-6.69529062534935,34.2453284753201,22.3111806270871));
#50234=CARTESIAN_POINT('Ctrl Pts',(-6.69196116566526,34.2600593280704,22.3120760213429));
#50235=CARTESIAN_POINT('Ctrl Pts',(-6.68399119241162,34.2964508742514,22.3142979522997));
#50236=CARTESIAN_POINT('Ctrl Pts',(-6.67946440979049,34.3181355550316,22.3156305343772));
#50237=CARTESIAN_POINT('Ctrl Pts',(-6.6640779178295,34.3956311686845,22.3204196891367));
#50238=CARTESIAN_POINT('Ctrl Pts',(-6.65441075713335,34.4516664648283,22.3239319989747));
#50239=CARTESIAN_POINT('Ctrl Pts',(-6.61344575588223,34.7308663815522,22.3415921554194));
#50240=CARTESIAN_POINT('Ctrl Pts',(-6.60304682726792,34.9565187894291,22.3563253559259));
#50241=CARTESIAN_POINT('Ctrl Pts',(-6.62411897839837,35.3494355253839,22.3814689111761));
#50242=CARTESIAN_POINT('Ctrl Pts',(-6.64560491559087,35.516453853132,22.392003007808));
#50243=CARTESIAN_POINT('Ctrl Pts',(-6.68819631154312,35.7240689634728,22.4048054868156));
#50244=CARTESIAN_POINT('Ctrl Pts',(-6.69781864164055,35.7667581624873,22.4074231291862));
#50245=CARTESIAN_POINT('Ctrl Pts',(-6.71500267386269,35.83665650359,22.4116865502195));
#50246=CARTESIAN_POINT('Ctrl Pts',(-6.72208235676282,35.8639777392101,22.4133472646366));
#50247=CARTESIAN_POINT('Ctrl Pts',(-6.73654233511079,35.9170420311705,22.4165625403042));
#50248=CARTESIAN_POINT('Ctrl Pts',(-6.74388808026892,35.9427922591487,22.4181180634545));
#50249=CARTESIAN_POINT('Ctrl Pts',(-6.76227949196456,36.0044821682919,22.4218345917871));
#50250=CARTESIAN_POINT('Ctrl Pts',(-6.77361959960515,36.0403308060633,22.4239860182427));
#50251=CARTESIAN_POINT('Ctrl Pts',(-6.81447741735757,36.1623913525112,22.4312898845888));
#50252=CARTESIAN_POINT('Ctrl Pts',(-6.84687438983762,36.2476011219593,22.4363503663778));
#50253=CARTESIAN_POINT('Ctrl Pts',(-6.9879272825928,36.5778597812969,22.4559759662225));
#50254=CARTESIAN_POINT('Ctrl Pts',(-7.12203266361379,36.8109440050839,22.4697769151542));
#50255=CARTESIAN_POINT('Ctrl Pts',(-7.32162444066562,37.0787173494879,22.4878651231777));
#50256=CARTESIAN_POINT('Ctrl Pts',(-7.36260474475307,37.1304710405901,22.4914838524526));
#50257=CARTESIAN_POINT('Ctrl Pts',(-7.43394002675994,37.2153453461314,22.497688800945));
#50258=CARTESIAN_POINT('Ctrl Pts',(-7.4634905847049,37.2491194671204,22.5002342112493));
#50259=CARTESIAN_POINT('Ctrl Pts',(-7.50697878240321,37.2968759556688,22.5039616193136));
#50260=CARTESIAN_POINT('Ctrl Pts',(-7.52038286599269,37.3113400388686,22.505108061081));
#50261=CARTESIAN_POINT('Ctrl Pts',(-7.54416065250997,37.3365532938056,22.5071392542106));
#50262=CARTESIAN_POINT('Ctrl Pts',(-7.55448038674853,37.3473521261819,22.5080200699032));
#50263=CARTESIAN_POINT('Ctrl Pts',(-7.57745693619613,37.3710793899617,22.5099799145479));
#50264=CARTESIAN_POINT('Ctrl Pts',(-7.59014593088893,37.3839747697212,22.5110612629601));
#50265=CARTESIAN_POINT('Ctrl Pts',(-7.62756282720698,37.4213962736053,22.5142453382233));
#50266=CARTESIAN_POINT('Ctrl Pts',(-7.65256553169329,37.4456429148682,22.516367245006));
#50267=CARTESIAN_POINT('Ctrl Pts',(-7.81040413290899,37.5940581561363,22.5297023582383));
#50268=CARTESIAN_POINT('Ctrl Pts',(-7.95266982387728,37.7077476531749,22.5414453349241));
#50269=CARTESIAN_POINT('Ctrl Pts',(-8.29801832697801,37.9408890909804,22.568302210783));
#50270=CARTESIAN_POINT('Ctrl Pts',(-8.50584439936249,38.0517374492212,22.5832951254527));
#50271=CARTESIAN_POINT('Ctrl Pts',(-8.76843260760859,38.1584807113425,22.6004868945263));
#50272=CARTESIAN_POINT('Ctrl Pts',(-8.81376362727027,38.1757837267063,22.603398381087));
#50273=CARTESIAN_POINT('Ctrl Pts',(-8.88695075780059,38.2019336577603,22.6080114324668));
#50274=CARTESIAN_POINT('Ctrl Pts',(-8.91457565630795,38.2114034063355,22.6097330393229));
#50275=CARTESIAN_POINT('Ctrl Pts',(-8.96765906593314,38.2288370308799,22.6130048958773));
#50276=CARTESIAN_POINT('Ctrl Pts',(-8.99309583709367,38.236859657542,22.6145569457201));
#50277=CARTESIAN_POINT('Ctrl Pts',(-9.05171559621727,38.2545901280128,22.6180988632354));
#50278=CARTESIAN_POINT('Ctrl Pts',(-9.08495799973722,38.2640922895552,22.6200820313661));
#50279=CARTESIAN_POINT('Ctrl Pts',(-9.19200487203,38.292927125482,22.626392044211));
#50280=CARTESIAN_POINT('Ctrl Pts',(-9.26632101758552,38.3102781610593,22.6306569510443));
#50281=CARTESIAN_POINT('Ctrl Pts',(-9.57740228938219,38.3719157862724,22.6481279932382));
#50282=CARTESIAN_POINT('Ctrl Pts',(-9.81795078746105,38.3934150874859,22.660674800165));
#50283=CARTESIAN_POINT('Ctrl Pts',(-10.200571702129,38.3867823715123,22.681103085593));
#50284=CARTESIAN_POINT('Ctrl Pts',(-10.3420831469256,38.3754251200986,22.6887776084487));
#50285=CARTESIAN_POINT('Ctrl Pts',(-10.5101320608057,38.351261317329,22.6984497930879));
#50286=CARTESIAN_POINT('Ctrl Pts',(-10.5377616887143,38.3469388096134,22.7000584480233));
#50287=CARTESIAN_POINT('Ctrl Pts',(-10.5815525963573,38.339531736401,22.7026417857048));
#50288=CARTESIAN_POINT('Ctrl Pts',(-10.5977509274284,38.3366704129808,22.7036047330348));
#50289=CARTESIAN_POINT('Ctrl Pts',(-10.6288961664269,38.3309347541883,22.705471533659));
#50290=CARTESIAN_POINT('Ctrl Pts',(-10.64384558234,38.3280774567546,22.7063744717012));
#50291=CARTESIAN_POINT('Ctrl Pts',(-10.6811594660227,38.3206848068373,22.7086446819186));
#50292=CARTESIAN_POINT('Ctrl Pts',(-10.7034981331256,38.3160241433137,22.7100185920139));
#50293=CARTESIAN_POINT('Ctrl Pts',(-10.7859265184943,38.2979561943271,22.7151388463239));
#50294=CARTESIAN_POINT('Ctrl Pts',(-10.8456917047292,38.2831387625296,22.7189510136887));
#50295=CARTESIAN_POINT('Ctrl Pts',(-11.1174819575795,38.2078412579838,22.7366488834324));
#50296=CARTESIAN_POINT('Ctrl Pts',(-11.3236941565528,38.1283933409034,22.7510560544434));
#50297=CARTESIAN_POINT('Ctrl Pts',(-11.6203304299284,37.9794889124857,22.7722596522514));
#50298=CARTESIAN_POINT('Ctrl Pts',(-11.7174102892579,37.9246076939456,22.7792921829856));
#50299=CARTESIAN_POINT('Ctrl Pts',(-11.8765850910188,37.8239585697418,22.7909295381597));
#50300=CARTESIAN_POINT('Ctrl Pts',(-11.9401410101294,37.7806775938133,22.7956079225141));
#50301=CARTESIAN_POINT('Ctrl Pts',(-12.030028303397,37.7148815250112,22.8022729919868));
#50302=CARTESIAN_POINT('Ctrl Pts',(-12.0575699910443,37.6940680154032,22.804322216628));
#50303=CARTESIAN_POINT('Ctrl Pts',(-12.1057546284907,37.6564844128666,22.8079212169355));
#50304=CARTESIAN_POINT('Ctrl Pts',(-12.1265268242327,37.6398855499504,22.809477434317));
#50305=CARTESIAN_POINT('Ctrl Pts',(-12.1699476299181,37.6043432897772,22.812741481674));
#50306=CARTESIAN_POINT('Ctrl Pts',(-12.1925484534373,37.5853448602842,22.8144469456281));
#50307=CARTESIAN_POINT('Ctrl Pts',(-12.2528068087566,37.533332627246,22.8190140901353));
#50308=CARTESIAN_POINT('Ctrl Pts',(-12.2899864433215,37.499775023734,22.8218535611006));
#50309=CARTESIAN_POINT('Ctrl Pts',(-12.5155550441293,37.2869235113488,22.8392506164396));
#50310=CARTESIAN_POINT('Ctrl Pts',(-12.6835313330988,37.0872725588065,22.8528762465068));
#50311=CARTESIAN_POINT('Ctrl Pts',(-12.8894240682693,36.7760681177932,22.8727119541689));
#50312=CARTESIAN_POINT('Ctrl Pts',(-12.9470511194547,36.6787126695618,22.8787610932485));
#50313=CARTESIAN_POINT('Ctrl Pts',(-13.0295991552326,36.5218590229713,22.8885358050778));
#50314=CARTESIAN_POINT('Ctrl Pts',(-13.0578738109652,36.4642174124952,22.8921340885628));
#50315=CARTESIAN_POINT('Ctrl Pts',(-13.0938327008631,36.3853199706915,22.8971127072279));
#50316=CARTESIAN_POINT('Ctrl Pts',(-13.1029674863365,36.3647362097376,22.898416407167));
#50317=CARTESIAN_POINT('Ctrl Pts',(-13.1179696486694,36.3300018609973,22.9006268686073));
#50318=CARTESIAN_POINT('Ctrl Pts',(-13.1239475977154,36.3158993428972,22.9015272402178));
#50319=CARTESIAN_POINT('Ctrl Pts',(-13.13620761629,36.2864224305801,22.9034160612439));
#50320=CARTESIAN_POINT('Ctrl Pts',(-13.1424725488627,36.2710417524475,22.904405382709));
#50321=CARTESIAN_POINT('Ctrl Pts',(-13.1589894394447,36.2296234539651,22.9070783602887));
#50322=CARTESIAN_POINT('Ctrl Pts',(-13.1690321917515,36.2035044544652,22.908773312553));
#50323=CARTESIAN_POINT('Ctrl Pts',(-13.1787500671531,36.1772650819055,22.9104832616759));
#50324=CARTESIAN_POINT('Origin',(-10.,35.,23.));
#50325=CARTESIAN_POINT('',(-13.178750056895,36.1772651096035,24.1659535227378));
#50326=CARTESIAN_POINT('',(-13.1787500981843,36.1772649981177,23.8178418924018));
#50327=CARTESIAN_POINT('',(-13.1787500671536,36.1772650819043,23.));
#50328=CARTESIAN_POINT('',(-13.3897493118688,34.997840096011,22.6386987365911));
#50329=CARTESIAN_POINT('Ctrl Pts',(-13.1787500981843,36.1772649981177,23.8178418924018));
#50330=CARTESIAN_POINT('Ctrl Pts',(-13.1694440470449,36.2023924002069,23.8161924048054));
#50331=CARTESIAN_POINT('Ctrl Pts',(-13.1598380975955,36.227414744048,23.8145512589474));
#50332=CARTESIAN_POINT('Ctrl Pts',(-13.1303459993096,36.3015952007151,23.8096904199983));
#50333=CARTESIAN_POINT('Ctrl Pts',(-13.1096041701896,36.3503993931377,23.8064984235902));
#50334=CARTESIAN_POINT('Ctrl Pts',(-13.0751712850199,36.426412371984,23.8015343405411));
#50335=CARTESIAN_POINT('Ctrl Pts',(-13.0622446906755,36.4539560626101,23.7997371210261));
#50336=CARTESIAN_POINT('Ctrl Pts',(-13.037392130686,36.5051091176036,23.7964012308428));
#50337=CARTESIAN_POINT('Ctrl Pts',(-13.0255573687388,36.5287599806311,23.7948596086142));
#50338=CARTESIAN_POINT('Ctrl Pts',(-12.9983125749134,36.5816507236623,23.7914125762159));
#50339=CARTESIAN_POINT('Ctrl Pts',(-12.9827491305477,36.6108088163751,23.7895126359239));
#50340=CARTESIAN_POINT('Ctrl Pts',(-12.9337347569534,36.6994901666946,23.78373133017));
#50341=CARTESIAN_POINT('Ctrl Pts',(-12.8989090301473,36.7582359773237,23.779897966608));
#50342=CARTESIAN_POINT('Ctrl Pts',(-12.7279490069987,37.027714544724,23.7622230032025));
#50343=CARTESIAN_POINT('Ctrl Pts',(-12.5704739595874,37.2239604773315,23.749152693907));
#50344=CARTESIAN_POINT('Ctrl Pts',(-12.2903365481919,37.5031344233068,23.7280551178306));
#50345=CARTESIAN_POINT('Ctrl Pts',(-12.181471230538,37.5985569296795,23.7202397615594));
#50346=CARTESIAN_POINT('Ctrl Pts',(-12.0444421099716,37.7039714192192,23.7103945622788));
#50347=CARTESIAN_POINT('Ctrl Pts',(-12.0218109287665,37.7209346619372,23.7087681940128));
#50348=CARTESIAN_POINT('Ctrl Pts',(-11.9856313184478,37.7473525712948,23.7061630018856));
#50349=CARTESIAN_POINT('Ctrl Pts',(-11.972220989971,37.7569951442803,23.7051962563634));
#50350=CARTESIAN_POINT('Ctrl Pts',(-11.9462020140114,37.7754168740919,23.7033173185527));
#50351=CARTESIAN_POINT('Ctrl Pts',(-11.9336033012458,37.7842089259797,23.70240598313));
#50352=CARTESIAN_POINT('Ctrl Pts',(-11.9021830721159,37.8058195219928,23.7001301771527));
#50353=CARTESIAN_POINT('Ctrl Pts',(-11.883291479793,37.8185345075371,23.6987592207321));
#50354=CARTESIAN_POINT('Ctrl Pts',(-11.8089231531161,37.8675066344641,23.6933566481783));
#50355=CARTESIAN_POINT('Ctrl Pts',(-11.7525190574556,37.9023220098992,23.6892470656246));
#50356=CARTESIAN_POINT('Ctrl Pts',(-11.5919348887097,37.9950542825703,23.6775882311117));
#50357=CARTESIAN_POINT('Ctrl Pts',(-11.4856684540666,38.0491627629834,23.6699224584744));
#50358=CARTESIAN_POINT('Ctrl Pts',(-11.1494210048519,38.1986153519764,23.6462064435097));
#50359=CARTESIAN_POINT('Ctrl Pts',(-10.9115914089616,38.2743467580589,23.6302433837918));
#50360=CARTESIAN_POINT('Ctrl Pts',(-10.6177625164372,38.3333702471048,23.6120248941159));
#50361=CARTESIAN_POINT('Ctrl Pts',(-10.5677172143813,38.3422575175997,23.6089692491099));
#50362=CARTESIAN_POINT('Ctrl Pts',(-10.4878872640331,38.3545891320663,23.6041679680593));
#50363=CARTESIAN_POINT('Ctrl Pts',(-10.4582256612732,38.3587693515591,23.6023998525243));
#50364=CARTESIAN_POINT('Ctrl Pts',(-10.4022183564581,38.365906717322,23.599090050561));
#50365=CARTESIAN_POINT('Ctrl Pts',(-10.3758859713122,38.3689490099072,23.5975458420579));
#50366=CARTESIAN_POINT('Ctrl Pts',(-10.3159376064496,38.3751634613507,23.5940561779519));
#50367=CARTESIAN_POINT('Ctrl Pts',(-10.2823042112321,38.3781428938766,23.5921167952211));
#50368=CARTESIAN_POINT('Ctrl Pts',(-10.1764762535761,38.3859261165218,23.5860680207337));
#50369=CARTESIAN_POINT('Ctrl Pts',(-10.104166980661,38.3889216267094,23.582013627439));
#50370=CARTESIAN_POINT('Ctrl Pts',(-9.92981838308282,38.3905579954587,23.57238083607));
#50371=CARTESIAN_POINT('Ctrl Pts',(-9.8278278545131,38.3869112206398,23.5668646894312));
#50372=CARTESIAN_POINT('Ctrl Pts',(-9.6783393914639,38.3747949007638,23.5588416264451));
#50373=CARTESIAN_POINT('Ctrl Pts',(-9.63061350507016,38.3699050256527,23.5562891447993));
#50374=CARTESIAN_POINT('Ctrl Pts',(-9.37552963722338,38.3382855064769,23.5426418228869));
#50375=CARTESIAN_POINT('Ctrl Pts',(-9.1708961320108,38.2934304167805,23.5317000523753));
#50376=CARTESIAN_POINT('Ctrl Pts',(-8.92768901535505,38.2160051841248,23.5174466710071));
#50377=CARTESIAN_POINT('Ctrl Pts',(-8.88395227236528,38.2010900073663,23.5148310170969));
#50378=CARTESIAN_POINT('Ctrl Pts',(-8.82307951324614,38.1789319507984,23.5110989805216));
#50379=CARTESIAN_POINT('Ctrl Pts',(-8.80567568239572,38.1724343288568,23.5100213329413));
#50380=CARTESIAN_POINT('Ctrl Pts',(-8.77423159431035,38.1603994445343,23.5080534799556));
#50381=CARTESIAN_POINT('Ctrl Pts',(-8.76017301405214,38.1549107551086,23.507166026257));
#50382=CARTESIAN_POINT('Ctrl Pts',(-8.73061806457926,38.1431439832503,23.5052834440944));
#50383=CARTESIAN_POINT('Ctrl Pts',(-8.71513092735981,38.1368449176771,23.5042871921066));
#50384=CARTESIAN_POINT('Ctrl Pts',(-8.67269888365236,38.1192196323019,23.5015320029517));
#50385=CARTESIAN_POINT('Ctrl Pts',(-8.64585349441067,38.1076593257293,23.4997602926481));
#50386=CARTESIAN_POINT('Ctrl Pts',(-8.58537585143135,38.080683720785,23.4957092544685));
#50387=CARTESIAN_POINT('Ctrl Pts',(-8.55183997815384,38.0650621545962,23.4934204316772));
#50388=CARTESIAN_POINT('Ctrl Pts',(-8.44181771393183,38.0116032794516,23.4857853553859));
#50389=CARTESIAN_POINT('Ctrl Pts',(-8.36650693795593,37.9714281500254,23.480355326714));
#50390=CARTESIAN_POINT('Ctrl Pts',(-8.05246275588005,37.7883496970749,23.4570436344576));
#50391=CARTESIAN_POINT('Ctrl Pts',(-7.83024639287046,37.6191618495753,23.4389595248882));
#50392=CARTESIAN_POINT('Ctrl Pts',(-7.58602075993207,37.3805668005,23.418022523368));
#50393=CARTESIAN_POINT('Ctrl Pts',(-7.54208347470578,37.3351747711789,23.4141997906668));
#50394=CARTESIAN_POINT('Ctrl Pts',(-7.47748959503964,37.2645977908168,23.4084903912907));
#50395=CARTESIAN_POINT('Ctrl Pts',(-7.45588682222745,37.240301351695,23.4065647516059));
#50396=CARTESIAN_POINT('Ctrl Pts',(-7.41737208023839,37.1957084724819,23.4031006310243));
#50397=CARTESIAN_POINT('Ctrl Pts',(-7.40034169456701,37.1755181960916,23.4015573999201));
#50398=CARTESIAN_POINT('Ctrl Pts',(-7.36394537603487,37.1313309896768,23.3982330277994));
#50399=CARTESIAN_POINT('Ctrl Pts',(-7.34466728025906,37.1072645789736,23.3964554564036));
#50400=CARTESIAN_POINT('Ctrl Pts',(-7.29097505295884,37.0383292244939,23.3914535547448));
#50401=CARTESIAN_POINT('Ctrl Pts',(-7.25735066109879,36.9928565692545,23.3882595940673));
#50402=CARTESIAN_POINT('Ctrl Pts',(-7.18326972081692,36.8872428654232,23.3810586019873));
#50403=CARTESIAN_POINT('Ctrl Pts',(-7.14357238987514,36.8266026573691,23.3770777801798));
#50404=CARTESIAN_POINT('Ctrl Pts',(-7.0045879838954,36.5986691191853,23.3625813834011));
#50405=CARTESIAN_POINT('Ctrl Pts',(-6.91781022090188,36.4241992602515,23.3524011966253));
#50406=CARTESIAN_POINT('Ctrl Pts',(-6.79247288801839,36.1062782847982,23.3341807746097));
#50407=CARTESIAN_POINT('Ctrl Pts',(-6.74746016543556,35.9659489878006,23.3262327773586));
#50408=CARTESIAN_POINT('Ctrl Pts',(-6.70484339488062,35.7957063970745,23.3162390737919));
#50409=CARTESIAN_POINT('Ctrl Pts',(-6.69831630727073,35.7681734210844,23.3146119696541));
#50410=CARTESIAN_POINT('Ctrl Pts',(-6.68852571355139,35.7244418729553,23.3120058696344));
#50411=CARTESIAN_POINT('Ctrl Pts',(-6.68503452159498,35.708295015611,23.3110389664242));
#50412=CARTESIAN_POINT('Ctrl Pts',(-6.6785249078087,35.6770851279166,23.3091599630209));
#50413=CARTESIAN_POINT('Ctrl Pts',(-6.67549063766089,35.6620260749826,23.3082487229304));
#50414=CARTESIAN_POINT('Ctrl Pts',(-6.66821432190783,35.624601838705,23.3059735057705));
#50415=CARTESIAN_POINT('Ctrl Pts',(-6.664095055223,35.6022137488682,23.304603050029));
#50416=CARTESIAN_POINT('Ctrl Pts',(-6.64887776011335,35.5145561510175,23.2992051424694));
#50417=CARTESIAN_POINT('Ctrl Pts',(-6.6394680226325,35.4490121989421,23.2950998881306));
#50418=CARTESIAN_POINT('Ctrl Pts',(-6.61853351234081,35.2650338455354,23.283458469059));
#50419=CARTESIAN_POINT('Ctrl Pts',(-6.61131597000853,35.146207252024,23.2758061427764));
#50420=CARTESIAN_POINT('Ctrl Pts',(-6.60835629606417,34.7780968254941,23.2520801987147));
#50421=CARTESIAN_POINT('Ctrl Pts',(-6.63383047159029,34.5294389852347,23.2360930170618));
#50422=CARTESIAN_POINT('Ctrl Pts',(-6.6971695240008,34.2355682775101,23.2178191134987));
#50423=CARTESIAN_POINT('Ctrl Pts',(-6.70913613335116,34.1855919602214,23.2147302498774));
#50424=CARTESIAN_POINT('Ctrl Pts',(-6.72982897005069,34.1070979865729,23.209906648742));
#50425=CARTESIAN_POINT('Ctrl Pts',(-6.73780273619619,34.078391803655,23.2081485227569));
#50426=CARTESIAN_POINT('Ctrl Pts',(-6.75359194803223,34.024323896758,23.2048473030709));
#50427=CARTESIAN_POINT('Ctrl Pts',(-6.76132874644872,33.9989417256242,23.2033018380946));
#50428=CARTESIAN_POINT('Ctrl Pts',(-6.77966767816542,33.9412162177968,23.1997956777938));
#50429=CARTESIAN_POINT('Ctrl Pts',(-6.79046058297763,33.9089362021686,23.1978412850797));
#50430=CARTESIAN_POINT('Ctrl Pts',(-6.82623977061605,33.8070544435604,23.1916881984726));
#50431=CARTESIAN_POINT('Ctrl Pts',(-6.8530189159206,33.7381029237299,23.1875473679018));
#50432=CARTESIAN_POINT('Ctrl Pts',(-6.92333828605412,33.5732409311739,23.1776544468405));
#50433=CARTESIAN_POINT('Ctrl Pts',(-6.96913370522978,33.4783757844422,23.1719695833861));
#50434=CARTESIAN_POINT('Ctrl Pts',(-7.07840889812364,33.2765929052141,23.1597085400523));
#50435=CARTESIAN_POINT('Ctrl Pts',(-7.14350115414826,33.1707266542365,23.1531657939876));
#50436=CARTESIAN_POINT('Ctrl Pts',(-7.2967056248336,32.9497448973863,23.1388544187194));
#50437=CARTESIAN_POINT('Ctrl Pts',(-7.38667947823775,32.8362314058612,23.1310766571475));
#50438=CARTESIAN_POINT('Ctrl Pts',(-7.50750469824291,32.7023614232893,23.1208944326394));
#50439=CARTESIAN_POINT('Ctrl Pts',(-7.53180444153565,32.6762774836675,23.1188582708401));
#50440=CARTESIAN_POINT('Ctrl Pts',(-7.56901054606389,32.6375816141312,23.11574913724));
#50441=CARTESIAN_POINT('Ctrl Pts',(-7.58161436727421,32.6246808099203,23.1146973169989));
#50442=CARTESIAN_POINT('Ctrl Pts',(-7.60484796358133,32.6012763628509,23.112759612337));
#50443=CARTESIAN_POINT('Ctrl Pts',(-7.61544509433741,32.5907415580135,23.1118761372337));
#50444=CARTESIAN_POINT('Ctrl Pts',(-7.64024170948591,32.5664146398687,23.1098098000257));
#50445=CARTESIAN_POINT('Ctrl Pts',(-7.65449268376823,32.5526765063624,23.108623075485));
#50446=CARTESIAN_POINT('Ctrl Pts',(-7.70176270925975,32.5078996688428,23.1046919343801));
#50447=CARTESIAN_POINT('Ctrl Pts',(-7.73528264588995,32.477399439137,23.1019125308104));
#50448=CARTESIAN_POINT('Ctrl Pts',(-7.81979433282978,32.40354335991,23.0949465905495));
#50449=CARTESIAN_POINT('Ctrl Pts',(-7.87147726008746,32.3610089282996,23.0907227504941));
#50450=CARTESIAN_POINT('Ctrl Pts',(-8.1458269260407,32.1485267275507,23.0686166221264));
#50451=CARTESIAN_POINT('Ctrl Pts',(-8.38771595592868,32.0050987041101,23.0502855313726));
#50452=CARTESIAN_POINT('Ctrl Pts',(-8.71868527498482,31.8607025106908,23.0279008285589));
#50453=CARTESIAN_POINT('Ctrl Pts',(-8.79401063808962,31.83100213861,23.0229609415297));
#50454=CARTESIAN_POINT('Ctrl Pts',(-8.90105552995791,31.7931654272864,23.0161543785634));
#50455=CARTESIAN_POINT('Ctrl Pts',(-8.93193473242825,31.7827490585224,23.014215105562));
#50456=CARTESIAN_POINT('Ctrl Pts',(-8.98863444207013,31.7645290906823,23.0106972902869));
#50457=CARTESIAN_POINT('Ctrl Pts',(-9.01440678523066,31.7565853835132,23.0091143431091));
#50458=CARTESIAN_POINT('Ctrl Pts',(-9.0670490480128,31.7410450918367,23.0059126139253));
#50459=CARTESIAN_POINT('Ctrl Pts',(-9.0939235462556,31.7334712460837,23.0042946641622));
#50460=CARTESIAN_POINT('Ctrl Pts',(-9.16169917519376,31.7152713441513,23.0002540950105));
#50461=CARTESIAN_POINT('Ctrl Pts',(-9.2027117367464,31.7050762886332,22.9978452306953));
#50462=CARTESIAN_POINT('Ctrl Pts',(-9.38463472994689,31.6634490439883,22.9873054408207));
#50463=CARTESIAN_POINT('Ctrl Pts',(-9.52728472119763,31.6402689021603,22.9794318342961));
#50464=CARTESIAN_POINT('Ctrl Pts',(-9.80279090209768,31.61340138008,22.964591953365));
#50465=CARTESIAN_POINT('Ctrl Pts',(-9.93523275854053,31.6082825495473,22.9576156553733));
#50466=CARTESIAN_POINT('Ctrl Pts',(-10.2186429965412,31.6139383961391,22.9425441038466));
#50467=CARTESIAN_POINT('Ctrl Pts',(-10.3692683777537,31.6270413314131,22.9344458532902));
#50468=CARTESIAN_POINT('Ctrl Pts',(-10.5540757490596,31.6556464104576,22.9238905821411));
#50469=CARTESIAN_POINT('Ctrl Pts',(-10.5895579876908,31.6617187011541,22.9218350723981));
#50470=CARTESIAN_POINT('Ctrl Pts',(-10.6427291402081,31.6716923104537,22.918702272269));
#50471=CARTESIAN_POINT('Ctrl Pts',(-10.6604955359162,31.6751724196638,22.9176466167639));
#50472=CARTESIAN_POINT('Ctrl Pts',(-10.6927275976253,31.6817546202959,22.9157138968354));
#50473=CARTESIAN_POINT('Ctrl Pts',(-10.7072020536281,31.6848093335655,22.9148394107943));
#50474=CARTESIAN_POINT('Ctrl Pts',(-10.7408229476522,31.6921349433345,22.9127930259245));
#50475=CARTESIAN_POINT('Ctrl Pts',(-10.7599527147625,31.6964773795904,22.9116173217179));
#50476=CARTESIAN_POINT('Ctrl Pts',(-10.8221236798561,31.711158693517,22.907761716833));
#50477=CARTESIAN_POINT('Ctrl Pts',(-10.8649986353705,31.7221742801175,22.9050485713767));
#50478=CARTESIAN_POINT('Ctrl Pts',(-10.9700246437505,31.7513619429165,22.8982884150339));
#50479=CARTESIAN_POINT('Ctrl Pts',(-11.0318934371808,31.770481130059,22.894206648712));
#50480=CARTESIAN_POINT('Ctrl Pts',(-11.3326357937338,31.8729430700979,22.8739873588518));
#50481=CARTESIAN_POINT('Ctrl Pts',(-11.5622427693034,31.9810894878182,22.8574401783296));
#50482=CARTESIAN_POINT('Ctrl Pts',(-11.8661939716176,32.168298586302,22.8350714814403));
#50483=CARTESIAN_POINT('Ctrl Pts',(-11.9521627892503,32.2268651951213,22.8286739422701));
#50484=CARTESIAN_POINT('Ctrl Pts',(-12.066813975298,32.3129501226264,22.820049079161));
#50485=CARTESIAN_POINT('Ctrl Pts',(-12.0979036647445,32.3371523772841,22.8176999712436));
#50486=CARTESIAN_POINT('Ctrl Pts',(-12.1477355377951,32.3773593728496,22.8139162615041));
#50487=CARTESIAN_POINT('Ctrl Pts',(-12.1667368720697,32.3930356399658,22.8124689844635));
#50488=CARTESIAN_POINT('Ctrl Pts',(-12.2064373081224,32.426522778753,22.8094347744225));
#50489=CARTESIAN_POINT('Ctrl Pts',(-12.2270955442067,32.4443795071023,22.8078498350675));
#50490=CARTESIAN_POINT('Ctrl Pts',(-12.2767796559105,32.4883858712774,22.8040215391787));
#50491=CARTESIAN_POINT('Ctrl Pts',(-12.3055739584146,32.5147917524815,22.801788898798));
#50492=CARTESIAN_POINT('Ctrl Pts',(-12.4136911549082,32.6174376465673,22.7933426946227));
#50493=CARTESIAN_POINT('Ctrl Pts',(-12.4897454112563,32.6970281644076,22.7872708146075));
#50494=CARTESIAN_POINT('Ctrl Pts',(-12.6964471328915,32.9355740600739,22.7701517313383));
#50495=CARTESIAN_POINT('Ctrl Pts',(-12.8166747149855,33.1028903693201,22.7594226545617));
#50496=CARTESIAN_POINT('Ctrl Pts',(-12.9884260337641,33.3945798929774,22.7413164429681));
#50497=CARTESIAN_POINT('Ctrl Pts',(-13.0490531827442,33.5129453193569,22.7341029229709));
#50498=CARTESIAN_POINT('Ctrl Pts',(-13.113870881966,33.660223889843,22.7249368637606));
#50499=CARTESIAN_POINT('Ctrl Pts',(-13.1248506179628,33.6860363771903,22.7233234641984));
#50500=CARTESIAN_POINT('Ctrl Pts',(-13.1417656050304,33.7272136376652,22.7207342724987));
#50501=CARTESIAN_POINT('Ctrl Pts',(-13.1479116117321,33.7424910731574,22.719770307238));
#50502=CARTESIAN_POINT('Ctrl Pts',(-13.1595858714477,33.7721323139816,22.7178924862814));
#50503=CARTESIAN_POINT('Ctrl Pts',(-13.1651280048847,33.7864899620716,22.7169794300388));
#50504=CARTESIAN_POINT('Ctrl Pts',(-13.1786788532794,33.822319652334,22.7146930548227));
#50505=CARTESIAN_POINT('Ctrl Pts',(-13.1865678774194,33.8438359315183,22.7133131208587));
#50506=CARTESIAN_POINT('Ctrl Pts',(-13.216830825245,33.9290374133678,22.707826128039));
#50507=CARTESIAN_POINT('Ctrl Pts',(-13.2375172912439,33.9933014483144,22.7036381059386));
#50508=CARTESIAN_POINT('Ctrl Pts',(-13.2904172436133,34.1761903180638,22.6916605835383));
#50509=CARTESIAN_POINT('Ctrl Pts',(-13.3181174214828,34.2960097984519,22.6837479201958));
#50510=CARTESIAN_POINT('Ctrl Pts',(-13.3727273443506,34.6088327219239,22.6632787510039));
#50511=CARTESIAN_POINT('Ctrl Pts',(-13.3896252539285,34.8031437948669,22.6507666687411));
#50512=CARTESIAN_POINT('Ctrl Pts',(-13.3897493118688,34.997840096011,22.6386987365911));
#50513=CARTESIAN_POINT('Ctrl Pts',(-13.3897493143602,34.9978440095506,22.6386984940168));
#50514=CARTESIAN_POINT('Ctrl Pts',(-13.3897813532124,35.0482169959177,22.6355762082653));
#50515=CARTESIAN_POINT('Ctrl Pts',(-13.388690550124,35.0985867233104,22.6324834989972));
#50516=CARTESIAN_POINT('Ctrl Pts',(-13.3847480802509,35.1882419257925,22.6270318747773));
#50517=CARTESIAN_POINT('Ctrl Pts',(-13.3823338315342,35.2275360092128,22.6246607571154));
#50518=CARTESIAN_POINT('Ctrl Pts',(-13.3771512899539,35.2931818710239,22.620729142537));
#50519=CARTESIAN_POINT('Ctrl Pts',(-13.3747575965931,35.3195585528621,22.6191574267673));
#50520=CARTESIAN_POINT('Ctrl Pts',(-13.3694901232354,35.3709085110181,22.6161126305208));
#50521=CARTESIAN_POINT('Ctrl Pts',(-13.3666472033063,35.3958831560609,22.6146387018143));
#50522=CARTESIAN_POINT('Ctrl Pts',(-13.360026985118,35.4487966316066,22.6115298301513));
#50523=CARTESIAN_POINT('Ctrl Pts',(-13.3561783869392,35.47672472364,22.6098972152488));
#50524=CARTESIAN_POINT('Ctrl Pts',(-13.345491508273,35.547715740626,22.6057665190862));
#50525=CARTESIAN_POINT('Ctrl Pts',(-13.3381698751238,35.5907013570226,22.6032835401932));
#50526=CARTESIAN_POINT('Ctrl Pts',(-13.3010067506192,35.7860401113829,22.5920677815193));
#50527=CARTESIAN_POINT('Ctrl Pts',(-13.2615494772013,35.9363795930766,22.5836353822097));
#50528=CARTESIAN_POINT('Ctrl Pts',(-13.2013205570211,36.1149222559032,22.5735644268251));
#50529=CARTESIAN_POINT('Ctrl Pts',(-13.190262087422,36.1461813115495,22.5717985181564));
#50530=CARTESIAN_POINT('Ctrl Pts',(-13.1787500907405,36.1772650182168,22.5700365663484));
#50531=CARTESIAN_POINT('Ctrl Pts',(-13.1787500671531,36.1772650819055,22.9104832616759));
#50532=CARTESIAN_POINT('Ctrl Pts',(-13.1790010362648,36.1765874366642,22.9105274219881));
#50533=CARTESIAN_POINT('Ctrl Pts',(-13.1792517886975,36.1759097111395,22.9105715923064));
#50534=CARTESIAN_POINT('Ctrl Pts',(-13.237959351312,36.017080776246,22.9209242746198));
#50535=CARTESIAN_POINT('Ctrl Pts',(-13.2845300025084,35.8548021059035,22.9317479373225));
#50536=CARTESIAN_POINT('Ctrl Pts',(-13.3479888675779,35.5494604665671,22.9518446707695));
#50537=CARTESIAN_POINT('Ctrl Pts',(-13.3682219563147,35.4074566325111,22.9610883679741));
#50538=CARTESIAN_POINT('Ctrl Pts',(-13.3862516561372,35.177179987411,22.9756973013826));
#50539=CARTESIAN_POINT('Ctrl Pts',(-13.3897019621106,35.0895291320123,22.981172033509));
#50540=CARTESIAN_POINT('Ctrl Pts',(-13.3897847495307,34.9368201348819,22.9905428193598));
#50541=CARTESIAN_POINT('Ctrl Pts',(-13.3879493868519,34.8718120078073,22.9944794268219));
#50542=CARTESIAN_POINT('Ctrl Pts',(-13.3823960459844,34.7744882129693,23.0002963219772));
#50543=CARTESIAN_POINT('Ctrl Pts',(-13.3800816063056,34.7421104449772,23.002218818337));
#50544=CARTESIAN_POINT('Ctrl Pts',(-13.3750412188899,34.6834572553323,23.0056796193798));
#50545=CARTESIAN_POINT('Ctrl Pts',(-13.3724725428528,34.6571712605943,23.0072226311836));
#50546=CARTESIAN_POINT('Ctrl Pts',(-13.3662351554364,34.6002260632992,23.0105491027415));
#50547=CARTESIAN_POINT('Ctrl Pts',(-13.3624541975311,34.5695813871893,23.0123289563566));
#50548=CARTESIAN_POINT('Ctrl Pts',(-13.3505367053427,34.4827673434493,23.0173448377495));
#50549=CARTESIAN_POINT('Ctrl Pts',(-13.3414073772441,34.4267434342593,23.020550214379));
#50550=CARTESIAN_POINT('Ctrl Pts',(-13.3173627889314,34.2994206011118,23.0277818538587));
#50551=CARTESIAN_POINT('Ctrl Pts',(-13.301547801169,34.2283197839812,23.0317815621783));
#50552=CARTESIAN_POINT('Ctrl Pts',(-13.2346136479775,33.9673721187257,23.0464065155067));
#50553=CARTESIAN_POINT('Ctrl Pts',(-13.1693041380711,33.7815755641973,23.0566891604838));
#50554=CARTESIAN_POINT('Ctrl Pts',(-13.0286977226376,33.470860464845,23.074882961935));
#50555=CARTESIAN_POINT('Ctrl Pts',(-12.960786560075,33.3431922308508,23.0826902191492));
#50556=CARTESIAN_POINT('Ctrl Pts',(-12.8700995584479,33.1961891904062,23.0925263426979));
#50557=CARTESIAN_POINT('Ctrl Pts',(-12.8549505523261,33.1723068788148,23.0941526470204));
#50558=CARTESIAN_POINT('Ctrl Pts',(-12.8304839003608,33.1347818451024,23.0967577600203));
#50559=CARTESIAN_POINT('Ctrl Pts',(-12.8213619693701,33.1210123767248,23.0977244916006));
#50560=CARTESIAN_POINT('Ctrl Pts',(-12.8035615170438,33.0945646355133,23.0996034230145));
#50561=CARTESIAN_POINT('Ctrl Pts',(-12.7948968514952,33.0818778288787,23.1005147662609));
#50562=CARTESIAN_POINT('Ctrl Pts',(-12.7731755057489,33.050533079188,23.1027906218577));
#50563=CARTESIAN_POINT('Ctrl Pts',(-12.7600165841288,33.0319471413214,23.1041616206865));
#50564=CARTESIAN_POINT('Ctrl Pts',(-12.707829826336,32.9597902875326,23.1095645912291));
#50565=CARTESIAN_POINT('Ctrl Pts',(-12.6674235593339,32.9072390443733,23.113674543376));
#50566=CARTESIAN_POINT('Ctrl Pts',(-12.550116570713,32.7635929584303,23.1253348666963));
#50567=CARTESIAN_POINT('Ctrl Pts',(-12.4699139823224,32.6753208039544,23.1330017892973));
#50568=CARTESIAN_POINT('Ctrl Pts',(-12.2084708573829,32.4164075385744,23.1567169592011));
#50569=CARTESIAN_POINT('Ctrl Pts',(-12.0129460402042,32.2613181029668,23.1726779604988));
#50570=CARTESIAN_POINT('Ctrl Pts',(-11.7591365899137,32.1019961142846,23.1908948273533));
#50571=CARTESIAN_POINT('Ctrl Pts',(-11.7154874732903,32.075946099827,23.1939506750723));
#50572=CARTESIAN_POINT('Ctrl Pts',(-11.6452074716319,32.0361183147008,23.1987521980932));
#50573=CARTESIAN_POINT('Ctrl Pts',(-11.6189525312298,32.0216959428165,23.2005203567485));
#50574=CARTESIAN_POINT('Ctrl Pts',(-11.5691104855404,31.9951705683002,23.2038301954978));
#50575=CARTESIAN_POINT('Ctrl Pts',(-11.5455660218386,31.9829926482725,23.2053743983222));
#50576=CARTESIAN_POINT('Ctrl Pts',(-11.4917133231471,31.9559342575447,23.2088639909069));
#50577=CARTESIAN_POINT('Ctrl Pts',(-11.4613205080669,31.9412277998095,23.2108033087802));
#50578=CARTESIAN_POINT('Ctrl Pts',(-11.3651288806111,31.8964437026354,23.2168516383603));
#50579=CARTESIAN_POINT('Ctrl Pts',(-11.29858204463,31.8680159256617,23.2209056636385));
#50580=CARTESIAN_POINT('Ctrl Pts',(-11.136151867512,31.804696400042,23.2305373551007));
#50581=CARTESIAN_POINT('Ctrl Pts',(-11.0395035859398,31.7719602944652,23.2360527903826));
#50582=CARTESIAN_POINT('Ctrl Pts',(-10.8954845330859,31.7303197202495,23.2440726517501));
#50583=CARTESIAN_POINT('Ctrl Pts',(-10.8491696145934,31.717986480605,23.2466226662982));
#50584=CARTESIAN_POINT('Ctrl Pts',(-10.5996093179044,31.657167400373,23.2602609581185));
#50585=CARTESIAN_POINT('Ctrl Pts',(-10.3924902656419,31.62657498258,23.2711961614971));
#50586=CARTESIAN_POINT('Ctrl Pts',(-10.1376220864304,31.6127278166058,23.285448443925));
#50587=CARTESIAN_POINT('Ctrl Pts',(-10.0913035027647,31.6111630426429,23.2880714943449));
#50588=CARTESIAN_POINT('Ctrl Pts',(-10.0263719791877,31.610301559026,23.2918124098229));
#50589=CARTESIAN_POINT('Ctrl Pts',(-10.0077729005632,31.610207889779,23.2928912982889));
#50590=CARTESIAN_POINT('Ctrl Pts',(-9.97407740020386,31.610315500748,23.2948606776596));
#50591=CARTESIAN_POINT('Ctrl Pts',(-9.9589810600504,31.6104645706882,23.2957484012477));
#50592=CARTESIAN_POINT('Ctrl Pts',(-9.92718124961997,31.6109910558264,23.2976305159197));
#50593=CARTESIAN_POINT('Ctrl Pts',(-9.91047896593155,31.6113911183827,23.2986260179514));
#50594=CARTESIAN_POINT('Ctrl Pts',(-9.86462320596399,31.612828734458,23.3013769920706));
#50595=CARTESIAN_POINT('Ctrl Pts',(-9.83547975630948,31.614119165717,23.3031451758726));
#50596=CARTESIAN_POINT('Ctrl Pts',(-9.6251088743864,31.6261564363506,23.3160347380531));
#50597=CARTESIAN_POINT('Ctrl Pts',(-9.44500128685725,31.6510704660152,23.3277302093005));
#50598=CARTESIAN_POINT('Ctrl Pts',(-9.03504994591969,31.7417662843148,23.3547950441538));
#50599=CARTESIAN_POINT('Ctrl Pts',(-8.80837231914258,31.8176625754771,23.3700577075697));
#50600=CARTESIAN_POINT('Ctrl Pts',(-8.54439843685343,31.938250187376,23.3877128278553));
#50601=CARTESIAN_POINT('Ctrl Pts',(-8.49778369292848,31.9608497182314,23.3908289163907));
#50602=CARTESIAN_POINT('Ctrl Pts',(-8.42487103274369,31.9982865615605,23.3957024282971));
#50603=CARTESIAN_POINT('Ctrl Pts',(-8.39822333882072,32.0124213071822,23.3974834926456));
#50604=CARTESIAN_POINT('Ctrl Pts',(-8.35086869849873,32.0383553973183,23.4006494198237));
#50605=CARTESIAN_POINT('Ctrl Pts',(-8.33009108193094,32.0500208390009,23.4020388292089));
#50606=CARTESIAN_POINT('Ctrl Pts',(-8.28159297876372,32.0779263524652,23.4052835299536));
#50607=CARTESIAN_POINT('Ctrl Pts',(-8.25397667995462,32.0943434890479,23.4071324037281));
#50608=CARTESIAN_POINT('Ctrl Pts',(-8.17271133678789,32.1442305518428,23.4125802022864));
#50609=CARTESIAN_POINT('Ctrl Pts',(-8.11975940755048,32.1788124816991,23.4161391612297));
#50610=CARTESIAN_POINT('Ctrl Pts',(-7.93675195973932,32.3057741395555,23.4285150176036));
#50611=CARTESIAN_POINT('Ctrl Pts',(-7.81227382540192,32.40583241055,23.4370614599859));
#50612=CARTESIAN_POINT('Ctrl Pts',(-7.54770180353582,32.6511383752549,23.4562265243886));
#50613=CARTESIAN_POINT('Ctrl Pts',(-7.41259936293109,32.8008496255516,23.4667596128032));
#50614=CARTESIAN_POINT('Ctrl Pts',(-7.25827255709008,33.0059075604897,23.4809902501718));
#50615=CARTESIAN_POINT('Ctrl Pts',(-7.22605193391819,33.0509783340861,23.4841086724474));
#50616=CARTESIAN_POINT('Ctrl Pts',(-7.18264621140156,33.1149527645479,23.4885522307905));
#50617=CARTESIAN_POINT('Ctrl Pts',(-7.17051698050485,33.1332083035395,23.4898221336829));
#50618=CARTESIAN_POINT('Ctrl Pts',(-7.15027025870247,33.1643320273062,23.4919926734218));
#50619=CARTESIAN_POINT('Ctrl Pts',(-7.14206061492794,33.1771398928868,23.4928874607243));
#50620=CARTESIAN_POINT('Ctrl Pts',(-7.12494242745946,33.2042458972411,23.4947852347788));
#50621=CARTESIAN_POINT('Ctrl Pts',(-7.11605392912648,33.2185556767856,23.4957893461617));
#50622=CARTESIAN_POINT('Ctrl Pts',(-7.09172521015697,33.2583822717003,23.4985888414825));
#50623=CARTESIAN_POINT('Ctrl Pts',(-7.07651489579452,33.284036923941,23.5003976516913));
#50624=CARTESIAN_POINT('Ctrl Pts',(-7.04270596196799,33.3428156470571,23.5045485258767));
#50625=CARTESIAN_POINT('Ctrl Pts',(-7.02432182693637,33.3760581310844,23.506900737016));
#50626=CARTESIAN_POINT('Ctrl Pts',(-6.96473670443895,33.4882111376033,23.5148353098581));
#50627=CARTESIAN_POINT('Ctrl Pts',(-6.92608723196081,33.5684318075203,23.5205078409061));
#50628=CARTESIAN_POINT('Ctrl Pts',(-6.77279864837253,33.9215102555887,23.5452157101113));
#50629=CARTESIAN_POINT('Ctrl Pts',(-6.69098154746527,34.2072672839233,23.5644121033627));
#50630=CARTESIAN_POINT('Ctrl Pts',(-6.63992642826559,34.549638822686,23.585434055818));
#50631=CARTESIAN_POINT('Ctrl Pts',(-6.63363163752506,34.599395396823,23.58844645004));
#50632=CARTESIAN_POINT('Ctrl Pts',(-6.62538676749286,34.6786543079254,23.593179361793));
#50633=CARTESIAN_POINT('Ctrl Pts',(-6.62271470197707,34.7080725753672,23.5949218003576));
#50634=CARTESIAN_POINT('Ctrl Pts',(-6.61836888853687,34.7640278650643,23.5982099887422));
#50635=CARTESIAN_POINT('Ctrl Pts',(-6.61662218436591,34.7905568372708,23.5997578687227));
#50636=CARTESIAN_POINT('Ctrl Pts',(-6.6133266858152,34.8515458972155,23.6032921769436));
#50637=CARTESIAN_POINT('Ctrl Pts',(-6.61199140036092,34.8860148651668,23.6052719137775));
#50638=CARTESIAN_POINT('Ctrl Pts',(-6.60938345397695,34.9971816450453,23.611604554602));
#50639=CARTESIAN_POINT('Ctrl Pts',(-6.61018768586979,35.0739065300959,23.6158944818222));
#50640=CARTESIAN_POINT('Ctrl Pts',(-6.61852832529547,35.2615268822037,23.626244239358));
#50641=CARTESIAN_POINT('Ctrl Pts',(-6.62891537096276,35.3722064551309,23.6322275374187));
#50642=CARTESIAN_POINT('Ctrl Pts',(-6.67578277287569,35.6983356425664,23.6497991201291));
#50643=CARTESIAN_POINT('Ctrl Pts',(-6.72765817888526,35.9109655475504,23.6611563387769));
#50644=CARTESIAN_POINT('Ctrl Pts',(-6.82059014850658,36.1772039111982,23.6767013508439));
#50645=CARTESIAN_POINT('Ctrl Pts',(-6.84325253315092,36.2366893158103,23.6802668779848));
#50646=CARTESIAN_POINT('Ctrl Pts',(-6.87640281495692,36.3168444539819,23.6852428101942));
#50647=CARTESIAN_POINT('Ctrl Pts',(-6.88544906112173,36.3380998006529,23.6865790925589));
#50648=CARTESIAN_POINT('Ctrl Pts',(-6.90083553885204,36.373250866194,23.6888195826673));
#50649=CARTESIAN_POINT('Ctrl Pts',(-6.90705391012291,36.3871996162766,23.6897167607591));
#50650=CARTESIAN_POINT('Ctrl Pts',(-6.92012699800989,36.4159996070253,23.6915868804811));
#50651=CARTESIAN_POINT('Ctrl Pts',(-6.92699525970748,36.4308439597377,23.6925605551736));
#50652=CARTESIAN_POINT('Ctrl Pts',(-6.9457129090319,36.4705419181782,23.6951895581798));
#50653=CARTESIAN_POINT('Ctrl Pts',(-6.95775788990161,36.4953013092134,23.6968558729484));
#50654=CARTESIAN_POINT('Ctrl Pts',(-7.02841392737375,36.6361520751646,23.7064769317425));
#50655=CARTESIAN_POINT('Ctrl Pts',(-7.0933612405727,36.74893177814,23.7147327644));
#50656=CARTESIAN_POINT('Ctrl Pts',(-7.32786337109546,37.1068508177878,23.7421945215145));
#50657=CARTESIAN_POINT('Ctrl Pts',(-7.52327651724279,37.3334601426814,23.7615235411329));
#50658=CARTESIAN_POINT('Ctrl Pts',(-7.7829469991365,37.5646739473172,23.7826314286395));
#50659=CARTESIAN_POINT('Ctrl Pts',(-7.82079914019173,37.5969136430714,23.7856170967689));
#50660=CARTESIAN_POINT('Ctrl Pts',(-7.8821818061923,37.6469073226659,23.7903182818475));
#50661=CARTESIAN_POINT('Ctrl Pts',(-7.90525717897291,37.6652063470725,23.7920552158234));
#50662=CARTESIAN_POINT('Ctrl Pts',(-7.94962858653411,37.6994610539502,23.795338973765));
#50663=CARTESIAN_POINT('Ctrl Pts',(-7.9708796360039,37.7154711419472,23.7968878418707));
#50664=CARTESIAN_POINT('Ctrl Pts',(-8.02024647532204,37.7517599030373,23.800432742459));
#50665=CARTESIAN_POINT('Ctrl Pts',(-8.0484894770182,37.7718609971389,23.8024219380572));
#50666=CARTESIAN_POINT('Ctrl Pts',(-8.14106819544522,37.8356345368181,23.8088227462943));
#50667=CARTESIAN_POINT('Ctrl Pts',(-8.20660133201395,37.877528998706,23.8131693798985));
#50668=CARTESIAN_POINT('Ctrl Pts',(-8.37107695936773,37.9748723647408,23.8236957393256));
#50669=CARTESIAN_POINT('Ctrl Pts',(-8.47147183575167,38.027682251715,23.8297951377052));
#50670=CARTESIAN_POINT('Ctrl Pts',(-8.78507571381331,38.1730621215018,23.8482176561924));
#50671=CARTESIAN_POINT('Ctrl Pts',(-9.00528612859248,38.248828864041,23.8602789028901));
#50672=CARTESIAN_POINT('Ctrl Pts',(-9.28041509113971,38.3128728074358,23.8760028044217));
#50673=CARTESIAN_POINT('Ctrl Pts',(-9.32958717842764,38.3231723987147,23.8788392182005));
#50674=CARTESIAN_POINT('Ctrl Pts',(-9.39983482402353,38.3362639888771,23.8829513012432));
#50675=CARTESIAN_POINT('Ctrl Pts',(-9.42073788771664,38.3399567358594,23.8841824021774));
#50676=CARTESIAN_POINT('Ctrl Pts',(-9.45657338143525,38.3459409386346,23.8863078733471));
#50677=CARTESIAN_POINT('Ctrl Pts',(-9.47148878515081,38.348329306437,23.8871969790942));
#50678=CARTESIAN_POINT('Ctrl Pts',(-9.50338598360247,38.3532184808963,23.8891085218536));
#50679=CARTESIAN_POINT('Ctrl Pts',(-9.52037084487927,38.3556900195747,23.8901323806456));
#50680=CARTESIAN_POINT('Ctrl Pts',(-9.56841966752616,38.3623095705297,23.8930442927407));
#50681=CARTESIAN_POINT('Ctrl Pts',(-9.59952264710387,38.3661558148426,23.8949474910764));
#50682=CARTESIAN_POINT('Ctrl Pts',(-9.81157920205511,38.3893985893415,23.908027323243));
#50683=CARTESIAN_POINT('Ctrl Pts',(-9.99377378532583,38.3946245500903,23.9197636325374));
#50684=CARTESIAN_POINT('Ctrl Pts',(-10.4086339630798,38.3731180695714,23.9465417353679));
#50685=CARTESIAN_POINT('Ctrl Pts',(-10.6399393699847,38.3369769890681,23.9614767965651));
#50686=CARTESIAN_POINT('Ctrl Pts',(-10.9161280140314,38.264020993372,23.9788596037172));
#50687=CARTESIAN_POINT('Ctrl Pts',(-10.966226371067,38.2495431424341,23.9819970189684));
#50688=CARTESIAN_POINT('Ctrl Pts',(-11.0448189971437,38.2248523292749,23.986895993547));
#50689=CARTESIAN_POINT('Ctrl Pts',(-11.0735431648861,38.2154042427478,23.988681609264));
#50690=CARTESIAN_POINT('Ctrl Pts',(-11.1269277328669,38.1970495984058,23.9919921397577));
#50691=CARTESIAN_POINT('Ctrl Pts',(-11.1516184652904,38.1882388895907,23.9935200190865));
#50692=CARTESIAN_POINT('Ctrl Pts',(-11.2073334278124,38.1676257148147,23.9969614169578));
#50693=CARTESIAN_POINT('Ctrl Pts',(-11.2382917465465,38.1556521254748,23.9988691756973));
#50694=CARTESIAN_POINT('Ctrl Pts',(-11.3331159425852,38.1173670753526,24.0047027745979));
#50695=CARTESIAN_POINT('Ctrl Pts',(-11.3963592499947,38.0895561717351,24.0085792840567));
#50696=CARTESIAN_POINT('Ctrl Pts',(-11.5448704951598,38.0187564736,24.0176868664591));
#50697=CARTESIAN_POINT('Ctrl Pts',(-11.6292594306088,37.9740596565543,24.0228650414919));
#50698=CARTESIAN_POINT('Ctrl Pts',(-11.8271671203197,37.8582819067838,24.0351629231767));
#50699=CARTESIAN_POINT('Ctrl Pts',(-11.9385790619074,37.7839229222697,24.042212872294));
#50700=CARTESIAN_POINT('Ctrl Pts',(-12.1661883104333,37.6117068324503,24.0573869994672));
#50701=CARTESIAN_POINT('Ctrl Pts',(-12.2807913119895,37.5122433523538,24.0655129903433));
#50702=CARTESIAN_POINT('Ctrl Pts',(-12.4139150553755,37.380066759976,24.0761010639822));
#50703=CARTESIAN_POINT('Ctrl Pts',(-12.4390797937873,37.3542712713051,24.0781587346993));
#50704=CARTESIAN_POINT('Ctrl Pts',(-12.4762666280471,37.314916129411,24.081294177059));
#50705=CARTESIAN_POINT('Ctrl Pts',(-12.4885997937082,37.3016524789963,24.0823502595232));
#50706=CARTESIAN_POINT('Ctrl Pts',(-12.5108121476394,37.27737705764,24.0842833595824));
#50707=CARTESIAN_POINT('Ctrl Pts',(-12.5207263914183,37.2663985391161,24.0851577916669));
#50708=CARTESIAN_POINT('Ctrl Pts',(-12.5436136882859,37.2407183868211,24.0872035185065));
#50709=CARTESIAN_POINT('Ctrl Pts',(-12.5565313253448,37.2259687837473,24.0883786099033));
#50710=CARTESIAN_POINT('Ctrl Pts',(-12.5981561094729,37.1776005579619,24.0922300490401));
#50711=CARTESIAN_POINT('Ctrl Pts',(-12.6263326172292,37.1435335195029,24.0949395467786));
#50712=CARTESIAN_POINT('Ctrl Pts',(-12.6940406788553,37.0583309904781,24.1016884379336));
#50713=CARTESIAN_POINT('Ctrl Pts',(-12.7327908405863,37.0065978751163,24.1057624498016));
#50714=CARTESIAN_POINT('Ctrl Pts',(-12.9150806390208,36.7481519840138,24.1258881737976));
#50715=CARTESIAN_POINT('Ctrl Pts',(-13.0367913981084,36.5269734099696,24.1423473991613));
#50716=CARTESIAN_POINT('Ctrl Pts',(-13.1489048712689,36.2556117805636,24.1607545473902));
#50717=CARTESIAN_POINT('Ctrl Pts',(-13.1641921164709,36.2165732090061,24.1633644668778));
#50718=CARTESIAN_POINT('Ctrl Pts',(-13.178750056895,36.1772651096035,24.1659535227378));
#50719=CARTESIAN_POINT('Origin',(-10.,35.,23.));
#50720=CARTESIAN_POINT('',(-13.1787500473324,36.1772651354237,25.4139790685233));
#50721=CARTESIAN_POINT('',(-13.1787500684596,36.1772650783778,25.0733222522952));
#50722=CARTESIAN_POINT('',(-13.1787500671536,36.1772650819043,23.));
#50723=CARTESIAN_POINT('Ctrl Pts',(-13.1787500684596,36.1772650783778,25.0733222522952));
#50724=CARTESIAN_POINT('Ctrl Pts',(-13.1307659665353,36.3068276298187,25.064834390241));
#50725=CARTESIAN_POINT('Ctrl Pts',(-13.0749065290861,36.4333323936619,25.0560136504007));
#50726=CARTESIAN_POINT('Ctrl Pts',(-12.8969145979482,36.7778027413596,25.0310689985252));
#50727=CARTESIAN_POINT('Ctrl Pts',(-12.7581866467696,36.9862364570538,25.0149288008823));
#50728=CARTESIAN_POINT('Ctrl Pts',(-12.5543852563375,37.2293701933785,24.9954297643669));
#50729=CARTESIAN_POINT('Ctrl Pts',(-12.5094137971869,37.2798725539082,24.9913315841711));
#50730=CARTESIAN_POINT('Ctrl Pts',(-12.4403347371283,37.3529249384142,24.985328245993));
#50731=CARTESIAN_POINT('Ctrl Pts',(-12.4173620284244,37.376520636002,24.9833767580414));
#50732=CARTESIAN_POINT('Ctrl Pts',(-12.3753325337511,37.418449776571,24.9798850971513));
#50733=CARTESIAN_POINT('Ctrl Pts',(-12.3563983875437,37.4369018580045,24.9783398202262));
#50734=CARTESIAN_POINT('Ctrl Pts',(-12.3151515604359,37.4761682535823,24.9750314798694));
#50735=CARTESIAN_POINT('Ctrl Pts',(-12.2927696955729,37.4969067220169,24.973271698899));
#50736=CARTESIAN_POINT('Ctrl Pts',(-12.2304337736215,37.553120575905,24.9684641070128));
#50737=CARTESIAN_POINT('Ctrl Pts',(-12.189915463833,37.5879586914813,24.9654423232322));
#50738=CARTESIAN_POINT('Ctrl Pts',(-11.9992991484955,37.7441689558281,24.9516606629629));
#50739=CARTESIAN_POINT('Ctrl Pts',(-11.8398284350779,37.853541832687,24.9413606289992));
#50740=CARTESIAN_POINT('Ctrl Pts',(-11.5357026069175,38.0259769091778,24.9228168968916));
#50741=CARTESIAN_POINT('Ctrl Pts',(-11.3943239200313,38.0936668160623,24.9145663846892));
#50742=CARTESIAN_POINT('Ctrl Pts',(-11.1769089501328,38.1798219152437,24.9017726056846));
#50743=CARTESIAN_POINT('Ctrl Pts',(-11.104086921635,38.2058341240274,24.8974689607672));
#50744=CARTESIAN_POINT('Ctrl Pts',(-11.0075998701456,38.2366220979135,24.8916668246521));
#50745=CARTESIAN_POINT('Ctrl Pts',(-10.9846786870032,38.2436688974761,24.8902812101687));
#50746=CARTESIAN_POINT('Ctrl Pts',(-10.9467279707565,38.2548970059149,24.8879721549258));
#50747=CARTESIAN_POINT('Ctrl Pts',(-10.9317404144614,38.2592189489255,24.8870564508939));
#50748=CARTESIAN_POINT('Ctrl Pts',(-10.9030914715806,38.2672666496007,24.8852979081742));
#50749=CARTESIAN_POINT('Ctrl Pts',(-10.8894356113586,38.2710105231959,24.8844562004594));
#50750=CARTESIAN_POINT('Ctrl Pts',(-10.852049907661,38.2810087227404,24.8821431294106));
#50751=CARTESIAN_POINT('Ctrl Pts',(-10.8282754354986,38.287090964748,24.8806626214447));
#50752=CARTESIAN_POINT('Ctrl Pts',(-10.7306792828961,38.3109330769719,24.8745517855972));
#50753=CARTESIAN_POINT('Ctrl Pts',(-10.656341284176,38.3264672717401,24.8698200864907));
#50754=CARTESIAN_POINT('Ctrl Pts',(-10.3781507279653,38.3749123085134,24.8519748735418));
#50755=CARTESIAN_POINT('Ctrl Pts',(-10.1719425600578,38.3916763004284,24.8385046514535));
#50756=CARTESIAN_POINT('Ctrl Pts',(-9.80218809235398,38.3879116881612,24.8149018098583));
#50757=CARTESIAN_POINT('Ctrl Pts',(-9.63920413326415,38.374450116284,24.8046838239203));
#50758=CARTESIAN_POINT('Ctrl Pts',(-9.43483469850828,38.3425865386903,24.7921923868279));
#50759=CARTESIAN_POINT('Ctrl Pts',(-9.39199372105874,38.3350600017291,24.7895909629063));
#50760=CARTESIAN_POINT('Ctrl Pts',(-9.32166326175944,38.3213036289955,24.7853468304464));
#50761=CARTESIAN_POINT('Ctrl Pts',(-9.29408649567778,38.315551948378,24.7836894525287));
#50762=CARTESIAN_POINT('Ctrl Pts',(-9.24041235176783,38.3036571040734,24.7804758483898));
#50763=CARTESIAN_POINT('Ctrl Pts',(-9.21430990540812,38.2975467839535,24.7789187235205));
#50764=CARTESIAN_POINT('Ctrl Pts',(-9.15160397585775,38.2820811034703,24.7751904030704));
#50765=CARTESIAN_POINT('Ctrl Pts',(-9.11507863307438,38.2724221181932,24.7730289487159));
#50766=CARTESIAN_POINT('Ctrl Pts',(-8.98990788496932,38.2370721218985,24.7656499730415));
#50767=CARTESIAN_POINT('Ctrl Pts',(-8.90215147728608,38.2083722635716,24.7605270737406));
#50768=CARTESIAN_POINT('Ctrl Pts',(-8.56589816880191,38.082988402781,24.7409263409843));
#50769=CARTESIAN_POINT('Ctrl Pts',(-8.32800097456888,37.9607221207794,24.7271956836636));
#50770=CARTESIAN_POINT('Ctrl Pts',(-8.05223278435334,37.7750584524099,24.7091890787451));
#50771=CARTESIAN_POINT('Ctrl Pts',(-7.99866315804326,37.7366761811603,24.7055762790202));
#50772=CARTESIAN_POINT('Ctrl Pts',(-7.91059169059765,37.6696042425872,24.699380413987));
#50773=CARTESIAN_POINT('Ctrl Pts',(-7.87547837994948,37.6417458971431,24.6968380021484));
#50774=CARTESIAN_POINT('Ctrl Pts',(-7.82573407681131,37.6006463193765,24.6931142062832));
#50775=CARTESIAN_POINT('Ctrl Pts',(-7.81064886358121,37.5879596488668,24.6919682831208));
#50776=CARTESIAN_POINT('Ctrl Pts',(-7.78432814066581,37.5654290845402,24.6899376440576));
#50777=CARTESIAN_POINT('Ctrl Pts',(-7.77304572412354,37.5556413709203,24.6890568556549));
#50778=CARTESIAN_POINT('Ctrl Pts',(-7.74823554114634,37.5338290085789,24.6870966113779));
#50779=CARTESIAN_POINT('Ctrl Pts',(-7.73473931850067,37.5217705358107,24.6860148294879));
#50780=CARTESIAN_POINT('Ctrl Pts',(-7.69471106539412,37.4854258687375,24.6827616386347));
#50781=CARTESIAN_POINT('Ctrl Pts',(-7.66846914396718,37.4608255659265,24.6805693092405));
#50782=CARTESIAN_POINT('Ctrl Pts',(-7.53435401944144,37.3310292268565,24.6690741202448));
#50783=CARTESIAN_POINT('Ctrl Pts',(-7.43319833019352,37.2191506102405,24.6594126680355));
#50784=CARTESIAN_POINT('Ctrl Pts',(-7.25824653656227,36.9976283101894,24.6412277388753));
#50785=CARTESIAN_POINT('Ctrl Pts',(-7.18274818527904,36.8896628136849,24.6327288820794));
#50786=CARTESIAN_POINT('Ctrl Pts',(-7.0374692814943,36.6537710593604,24.615127176128));
#50787=CARTESIAN_POINT('Ctrl Pts',(-6.96925844379516,36.5251758384331,24.6060742301639));
#50788=CARTESIAN_POINT('Ctrl Pts',(-6.89212047061677,36.3539874192748,24.5947466750237));
#50789=CARTESIAN_POINT('Ctrl Pts',(-6.87545333140142,36.3150686141046,24.5922167013959));
#50790=CARTESIAN_POINT('Ctrl Pts',(-6.8490047142653,36.2499656544263,24.5880574786862));
#50791=CARTESIAN_POINT('Ctrl Pts',(-6.838810531346,36.2239553263872,24.5864147150729));
#50792=CARTESIAN_POINT('Ctrl Pts',(-6.81941333302961,36.1726040106012,24.5832075458548));
#50793=CARTESIAN_POINT('Ctrl Pts',(-6.81018880495963,36.1472734256455,24.5816425293851));
#50794=CARTESIAN_POINT('Ctrl Pts',(-6.7904975800991,36.0911270500908,24.5782096847999));
#50795=CARTESIAN_POINT('Ctrl Pts',(-6.78017044304921,36.0602649436259,24.5763464755342));
#50796=CARTESIAN_POINT('Ctrl Pts',(-6.74579996919094,35.9524137721716,24.5699128281044));
#50797=CARTESIAN_POINT('Ctrl Pts',(-6.72406007349754,35.8747164062729,24.5654150091625));
#50798=CARTESIAN_POINT('Ctrl Pts',(-6.63921363116226,35.5236489979135,24.5455744501793));
#50799=CARTESIAN_POINT('Ctrl Pts',(-6.60741895386023,35.243880156947,24.5311526757082));
#50800=CARTESIAN_POINT('Ctrl Pts',(-6.61117049327251,34.8964530030295,24.512346249462));
#50801=CARTESIAN_POINT('Ctrl Pts',(-6.61387656327999,34.8295459633342,24.5086778690344));
#50802=CARTESIAN_POINT('Ctrl Pts',(-6.62173408140458,34.7175478064566,24.5023969392579));
#50803=CARTESIAN_POINT('Ctrl Pts',(-6.6258130805747,34.6723995079999,24.4998265116199));
#50804=CARTESIAN_POINT('Ctrl Pts',(-6.6329722735689,34.6076719882143,24.4960689756137));
#50805=CARTESIAN_POINT('Ctrl Pts',(-6.6353209161597,34.5880150474372,24.4949182216722));
#50806=CARTESIAN_POINT('Ctrl Pts',(-6.6397442826629,34.553558649893,24.4928824052194));
#50807=CARTESIAN_POINT('Ctrl Pts',(-6.64174489819024,34.5387505834577,24.4920013462472));
#50808=CARTESIAN_POINT('Ctrl Pts',(-6.64637609662239,34.5061001997566,24.4900447548531));
#50809=CARTESIAN_POINT('Ctrl Pts',(-6.6490511581528,34.4882655716222,24.4889669568071));
#50810=CARTESIAN_POINT('Ctrl Pts',(-6.65743603863847,34.4352509858389,24.4857378774868));
#50811=CARTESIAN_POINT('Ctrl Pts',(-6.66355835072107,34.4001398588864,24.4835661119076));
#50812=CARTESIAN_POINT('Ctrl Pts',(-6.69730641142036,34.2231370476805,24.4724713568811));
#50813=CARTESIAN_POINT('Ctrl Pts',(-6.73343327716103,34.0830287871982,24.4632175107088));
#50814=CARTESIAN_POINT('Ctrl Pts',(-6.81690276305331,33.8279801492812,24.445936833305));
#50815=CARTESIAN_POINT('Ctrl Pts',(-6.86183874362242,33.7124891902504,24.4379359133095));
#50816=CARTESIAN_POINT('Ctrl Pts',(-6.95660901619957,33.5035630070515,24.4233106537873));
#50817=CARTESIAN_POINT('Ctrl Pts',(-7.00469479561024,33.4094962923371,24.4166641890884));
#50818=CARTESIAN_POINT('Ctrl Pts',(-7.09386509502281,33.2534964684357,24.4055779659803));
#50819=CARTESIAN_POINT('Ctrl Pts',(-7.13273453349769,33.1903910131828,24.4010737232964));
#50820=CARTESIAN_POINT('Ctrl Pts',(-7.19244624234888,33.1002087130594,24.3946060018994));
#50821=CARTESIAN_POINT('Ctrl Pts',(-7.21167640617214,33.0720952567253,24.3925850801741));
#50822=CARTESIAN_POINT('Ctrl Pts',(-7.24663772007443,33.0226013572735,24.3890176030153));
#50823=CARTESIAN_POINT('Ctrl Pts',(-7.26220218565181,33.0011072004863,24.3874649942433));
#50824=CARTESIAN_POINT('Ctrl Pts',(-7.29576401053198,32.9558866379838,24.3841903847806));
#50825=CARTESIAN_POINT('Ctrl Pts',(-7.31382492081051,32.9322100568245,24.382470992412));
#50826=CARTESIAN_POINT('Ctrl Pts',(-7.36385105411483,32.8683910711449,24.3778206556649));
#50827=CARTESIAN_POINT('Ctrl Pts',(-7.39642012803601,32.8287307562785,24.3749133950319));
#50828=CARTESIAN_POINT('Ctrl Pts',(-7.59276946009868,32.600404329679,24.3580376394101));
#50829=CARTESIAN_POINT('Ctrl Pts',(-7.77609952918974,32.4295727911918,24.3449135142832));
#50830=CARTESIAN_POINT('Ctrl Pts',(-8.11316344057911,32.1787861934753,24.3226016356645));
#50831=CARTESIAN_POINT('Ctrl Pts',(-8.2572263576797,32.0875908660576,24.313500107718));
#50832=CARTESIAN_POINT('Ctrl Pts',(-8.43415976623623,31.9934304034561,24.3021134264023));
#50833=CARTESIAN_POINT('Ctrl Pts',(-8.4609962638033,31.9796053662315,24.3003807724348));
#50834=CARTESIAN_POINT('Ctrl Pts',(-8.50315869420564,31.9585928353277,24.2976444958469));
#50835=CARTESIAN_POINT('Ctrl Pts',(-8.51836052225759,31.9511582744559,24.2966550937034));
#50836=CARTESIAN_POINT('Ctrl Pts',(-8.54730742930555,31.9372692031222,24.2947645765025));
#50837=CARTESIAN_POINT('Ctrl Pts',(-8.56104115305781,31.930792766629,24.2938647649355));
#50838=CARTESIAN_POINT('Ctrl Pts',(-8.59454285991083,31.9152685814993,24.2916634499116));
#50839=CARTESIAN_POINT('Ctrl Pts',(-8.61435507503563,31.9063184093079,24.2903563731094));
#50840=CARTESIAN_POINT('Ctrl Pts',(-8.68394411310862,31.8756840957899,24.285750508426));
#50841=CARTESIAN_POINT('Ctrl Pts',(-8.73415241136013,31.8550068100978,24.2824011031133));
#50842=CARTESIAN_POINT('Ctrl Pts',(-8.97360946777982,31.7630540204179,24.26637388975));
#50843=CARTESIAN_POINT('Ctrl Pts',(-9.16848723102129,31.7076028752931,24.2532037402413));
#50844=CARTESIAN_POINT('Ctrl Pts',(-9.55640992597417,31.6338819656676,24.2278574991085));
#50845=CARTESIAN_POINT('Ctrl Pts',(-9.74842605747257,31.6141098051895,24.2157107681617));
#50846=CARTESIAN_POINT('Ctrl Pts',(-9.9858867655,31.6099835110576,24.201351341659));
#50847=CARTESIAN_POINT('Ctrl Pts',(-10.0306799890562,31.6100929209268,24.198669995993));
#50848=CARTESIAN_POINT('Ctrl Pts',(-10.1038852804712,31.6117229550522,24.1943307772204));
#50849=CARTESIAN_POINT('Ctrl Pts',(-10.1323025345119,31.6127135347298,24.192656906725));
#50850=CARTESIAN_POINT('Ctrl Pts',(-10.1876405912292,31.6153400094382,24.1894168859055));
#50851=CARTESIAN_POINT('Ctrl Pts',(-10.214560890434,31.6169398573052,24.1878497526763));
#50852=CARTESIAN_POINT('Ctrl Pts',(-10.2784989357181,31.6215059126574,24.1841477910255));
#50853=CARTESIAN_POINT('Ctrl Pts',(-10.3154930659426,31.6247595293507,24.1820219388386));
#50854=CARTESIAN_POINT('Ctrl Pts',(-10.4405514020079,31.6378325089201,24.1748833829223));
#50855=CARTESIAN_POINT('Ctrl Pts',(-10.5282846130177,31.6504966188538,24.1699571137163));
#50856=CARTESIAN_POINT('Ctrl Pts',(-10.8821332536775,31.7158253221721,24.1502669074199));
#50857=CARTESIAN_POINT('Ctrl Pts',(-11.1419485056802,31.7968911083043,24.1363061019223));
#50858=CARTESIAN_POINT('Ctrl Pts',(-11.4497556915204,31.9351993029143,24.1180325298672));
#50859=CARTESIAN_POINT('Ctrl Pts',(-11.5093786412316,31.9641195480346,24.114400552371));
#50860=CARTESIAN_POINT('Ctrl Pts',(-11.6080048980004,32.015582137231,24.1081753158729));
#50861=CARTESIAN_POINT('Ctrl Pts',(-11.6474766874405,32.0371888525677,24.1056232141005));
#50862=CARTESIAN_POINT('Ctrl Pts',(-11.7036287547125,32.069395314039,24.1018877452565));
#50863=CARTESIAN_POINT('Ctrl Pts',(-11.7206662167474,32.0793660809494,24.1007401468952));
#50864=CARTESIAN_POINT('Ctrl Pts',(-11.7504422374339,32.0971427500939,24.0987077157912));
#50865=CARTESIAN_POINT('Ctrl Pts',(-11.7632177909871,32.1048849333368,24.0978268369253));
#50866=CARTESIAN_POINT('Ctrl Pts',(-11.7913388541426,32.1221819170472,24.0958678741783));
#50867=CARTESIAN_POINT('Ctrl Pts',(-11.8066591878827,32.1317750514576,24.094787485375));
#50868=CARTESIAN_POINT('Ctrl Pts',(-11.8512086648229,32.1601691334563,24.0916089328252));
#50869=CARTESIAN_POINT('Ctrl Pts',(-11.8802254548769,32.1792970896094,24.0894916840431));
#50870=CARTESIAN_POINT('Ctrl Pts',(-12.0617399108782,32.3029972225237,24.0759728494951));
#50871=CARTESIAN_POINT('Ctrl Pts',(-12.2057505547567,32.4194477007096,24.0640230841181));
#50872=CARTESIAN_POINT('Ctrl Pts',(-12.4547290570156,32.6569143889609,24.0418481997046));
#50873=CARTESIAN_POINT('Ctrl Pts',(-12.5620477518626,32.7747665669644,24.0316393548772));
#50874=CARTESIAN_POINT('Ctrl Pts',(-12.7202811607275,32.9752222657937,24.0157044531034));
#50875=CARTESIAN_POINT('Ctrl Pts',(-12.7766340598312,33.0532179199692,24.0098078003098));
#50876=CARTESIAN_POINT('Ctrl Pts',(-12.8501732572456,33.1647033509829,24.001790508696));
#50877=CARTESIAN_POINT('Ctrl Pts',(-12.8702321752451,33.1962348229104,23.9995661478259));
#50878=CARTESIAN_POINT('Ctrl Pts',(-12.903882554509,33.2511145105134,23.9957668848981));
#50879=CARTESIAN_POINT('Ctrl Pts',(-12.9177235470911,33.2743048614257,23.994183087062));
#50880=CARTESIAN_POINT('Ctrl Pts',(-12.9455273948703,33.3221807098169,23.9909564505232));
#50881=CARTESIAN_POINT('Ctrl Pts',(-12.9594605809514,33.3468810250783,23.9893147539574));
#50882=CARTESIAN_POINT('Ctrl Pts',(-12.9944190202137,33.4107130952642,23.9851289293572));
#50883=CARTESIAN_POINT('Ctrl Pts',(-13.01498835829,33.4500891668177,23.9826007466813));
#50884=CARTESIAN_POINT('Ctrl Pts',(-13.109637786221,33.6402966663951,23.9706260368517));
#50885=CARTESIAN_POINT('Ctrl Pts',(-13.1732114456117,33.7960989146199,23.9615368528855));
#50886=CARTESIAN_POINT('Ctrl Pts',(-13.2835713952204,34.1370027642995,23.9424376319687));
#50887=CARTESIAN_POINT('Ctrl Pts',(-13.3268235370846,34.3226200225679,23.9324995132982));
#50888=CARTESIAN_POINT('Ctrl Pts',(-13.3665599552516,34.5951205098924,23.9174973927582));
#50889=CARTESIAN_POINT('Ctrl Pts',(-13.3756656442352,34.6797929363055,23.9127763696353));
#50890=CARTESIAN_POINT('Ctrl Pts',(-13.3832899180907,34.7893691713031,23.9064907039485));
#50891=CARTESIAN_POINT('Ctrl Pts',(-13.3847357966339,34.8140442882095,23.9050637577592));
#50892=CARTESIAN_POINT('Ctrl Pts',(-13.3866610208941,34.8544655043237,23.9027042457129));
#50893=CARTESIAN_POINT('Ctrl Pts',(-13.3873006974258,34.8702035171999,23.901780119111));
#50894=CARTESIAN_POINT('Ctrl Pts',(-13.3883026537344,34.8999651424344,23.900021288718));
#50895=CARTESIAN_POINT('Ctrl Pts',(-13.3886876087989,34.9139876731016,23.8991878951735));
#50896=CARTESIAN_POINT('Ctrl Pts',(-13.3894915959102,34.9518369977503,23.896926466669));
#50897=CARTESIAN_POINT('Ctrl Pts',(-13.389746412554,34.97566603434,23.8954899494278));
#50898=CARTESIAN_POINT('Ctrl Pts',(-13.3897612597053,35.0753306280261,23.8894337867824));
#50899=CARTESIAN_POINT('Ctrl Pts',(-13.387227647782,35.151139962788,23.8847114418519));
#50900=CARTESIAN_POINT('Ctrl Pts',(-13.3720525334123,35.3774441921629,23.8703858501299));
#50901=CARTESIAN_POINT('Ctrl Pts',(-13.3518967387176,35.5272458346233,23.8606069283636));
#50902=CARTESIAN_POINT('Ctrl Pts',(-13.2871051319953,35.8460051064849,23.8396685724383));
#50903=CARTESIAN_POINT('Ctrl Pts',(-13.2392693847419,36.0138560049049,23.8285688711194));
#50904=CARTESIAN_POINT('Ctrl Pts',(-13.1787500981843,36.1772649981177,23.8178418924018));
#50905=CARTESIAN_POINT('',(-13.3897487153608,34.997048862956,24.2344129021999));
#50906=CARTESIAN_POINT('Ctrl Pts',(-13.178750056895,36.1772651096035,24.1659535227378));
#50907=CARTESIAN_POINT('Ctrl Pts',(-13.2007132313444,36.1179620338044,24.1698595619065));
#50908=CARTESIAN_POINT('Ctrl Pts',(-13.2210164453761,36.0580454759536,24.1737179086272));
#50909=CARTESIAN_POINT('Ctrl Pts',(-13.2512687078543,35.9598019389304,24.1799026900532));
#50910=CARTESIAN_POINT('Ctrl Pts',(-13.2622417301508,35.9218172623397,24.182260312743));
#50911=CARTESIAN_POINT('Ctrl Pts',(-13.2789753117563,35.8598452481243,24.1860538843696));
#50912=CARTESIAN_POINT('Ctrl Pts',(-13.2851427481617,35.8359725581357,24.1875026395995));
#50913=CARTESIAN_POINT('Ctrl Pts',(-13.2975842852012,35.7855489298977,24.1905369669661));
#50914=CARTESIAN_POINT('Ctrl Pts',(-13.303799450826,35.7589851722001,24.1921205795992));
#50915=CARTESIAN_POINT('Ctrl Pts',(-13.3155724314958,35.7057797025507,24.1952639922042));
#50916=CARTESIAN_POINT('Ctrl Pts',(-13.3211314305274,35.6791403530215,24.1968237246703));
#50917=CARTESIAN_POINT('Ctrl Pts',(-13.3336011557114,35.6155649456605,24.2005142969583));
#50918=CARTESIAN_POINT('Ctrl Pts',(-13.3402197721034,35.5785748800576,24.2026361865005));
#50919=CARTESIAN_POINT('Ctrl Pts',(-13.3753506445415,35.3614747083645,24.2149560550524));
#50920=CARTESIAN_POINT('Ctrl Pts',(-13.3899074801705,35.1794100348603,24.2247295043398));
#50921=CARTESIAN_POINT('Ctrl Pts',(-13.3897487153608,34.997048862956,24.2344129021999));
#50922=CARTESIAN_POINT('Ctrl Pts',(-13.3897487163589,34.9970500096102,24.2344128413124));
#50923=CARTESIAN_POINT('Ctrl Pts',(-13.3895571294199,34.776902993936,24.2461026719699));
#50924=CARTESIAN_POINT('Ctrl Pts',(-13.3679200225697,34.557313328916,24.2576093550979));
#50925=CARTESIAN_POINT('Ctrl Pts',(-13.3196008701561,34.3133621496472,24.2715832846215));
#50926=CARTESIAN_POINT('Ctrl Pts',(-13.3136953173194,34.2854059074429,24.2732031673232));
#50927=CARTESIAN_POINT('Ctrl Pts',(-13.3021887967361,34.2341485902329,24.2762127610933));
#50928=CARTESIAN_POINT('Ctrl Pts',(-13.2966927381551,34.2108256519966,24.2775973559733));
#50929=CARTESIAN_POINT('Ctrl Pts',(-13.287212423525,34.1724235763176,24.2799051712831));
#50930=CARTESIAN_POINT('Ctrl Pts',(-13.2833704138438,34.1573096848357,24.2808206721075));
#50931=CARTESIAN_POINT('Ctrl Pts',(-13.2753374520107,34.1265983334656,24.2826966460185));
#50932=CARTESIAN_POINT('Ctrl Pts',(-13.2711390869676,34.1110034051284,24.2836574706757));
#50933=CARTESIAN_POINT('Ctrl Pts',(-13.2597374138959,34.0698261488127,24.2862151579761));
#50934=CARTESIAN_POINT('Ctrl Pts',(-13.2523445416499,34.0442980129955,24.2878220441492));
#50935=CARTESIAN_POINT('Ctrl Pts',(-13.2156248932012,33.9228652515296,24.2955587624173));
#50936=CARTESIAN_POINT('Ctrl Pts',(-13.1823537217997,33.8282132618164,24.3018665739979));
#50937=CARTESIAN_POINT('Ctrl Pts',(-13.0668205335138,33.5409423662535,24.3216069462704));
#50938=CARTESIAN_POINT('Ctrl Pts',(-12.9708678509696,33.3543424825361,24.3352544126521));
#50939=CARTESIAN_POINT('Ctrl Pts',(-12.7852138530299,33.0631262000625,24.3571349096755));
#50940=CARTESIAN_POINT('Ctrl Pts',(-12.7052748078133,32.9529553537417,24.3655785682729));
#50941=CARTESIAN_POINT('Ctrl Pts',(-12.5925136060476,32.8157361353924,24.3762859235845));
#50942=CARTESIAN_POINT('Ctrl Pts',(-12.5655134067423,32.7840856021571,24.3787706258087));
#50943=CARTESIAN_POINT('Ctrl Pts',(-12.5195152074529,32.7321330698409,24.3828761294415));
#50944=CARTESIAN_POINT('Ctrl Pts',(-12.5008383397385,32.7115540293398,24.3845097291301));
#50945=CARTESIAN_POINT('Ctrl Pts',(-12.4634754324667,32.6713895982252,24.3877137161917));
#50946=CARTESIAN_POINT('Ctrl Pts',(-12.4448037123579,32.6517937740114,24.389284523467));
#50947=CARTESIAN_POINT('Ctrl Pts',(-12.4028608287367,32.6088176824744,24.3927479275085));
#50948=CARTESIAN_POINT('Ctrl Pts',(-12.3794789060723,32.5855490725045,24.3946355931771));
#50949=CARTESIAN_POINT('Ctrl Pts',(-12.2956055900131,32.5044842252876,24.4012616117989));
#50950=CARTESIAN_POINT('Ctrl Pts',(-12.2333161656908,32.4485877611927,24.405921185441));
#50951=CARTESIAN_POINT('Ctrl Pts',(-11.9563650478823,32.2179836515277,24.4256870232476));
#50952=CARTESIAN_POINT('Ctrl Pts',(-11.7228465203349,32.0676341469896,24.4399207379714));
#50953=CARTESIAN_POINT('Ctrl Pts',(-11.4136172364634,31.9183548791206,24.4585100745465));
#50954=CARTESIAN_POINT('Ctrl Pts',(-11.3527353409404,31.8911486768247,24.4621639210147));
#50955=CARTESIAN_POINT('Ctrl Pts',(-11.2493040403035,31.8485420462282,24.4684226242142));
#50956=CARTESIAN_POINT('Ctrl Pts',(-11.2071758782604,31.8321657535569,24.4709857455939));
#50957=CARTESIAN_POINT('Ctrl Pts',(-11.1461645194306,31.8098427955497,24.4747344849037));
#50958=CARTESIAN_POINT('Ctrl Pts',(-11.1275353565801,31.803210974512,24.475883982469));
#50959=CARTESIAN_POINT('Ctrl Pts',(-11.0947301526005,31.7918550208442,24.477918449241));
#50960=CARTESIAN_POINT('Ctrl Pts',(-11.0805792422273,31.7870610333325,24.4787994346731));
#50961=CARTESIAN_POINT('Ctrl Pts',(-11.0492623178913,31.7766819139516,24.4807569623977));
#50962=CARTESIAN_POINT('Ctrl Pts',(-11.0320833147195,31.7711403104398,24.4818357858848));
#50963=CARTESIAN_POINT('Ctrl Pts',(-10.9807753348092,31.7550406697284,24.4850710629145));
#50964=CARTESIAN_POINT('Ctrl Pts',(-10.9465238432179,31.7448849930582,24.4872481124605));
#50965=CARTESIAN_POINT('Ctrl Pts',(-10.6997374703552,31.6759362797509,24.5030263860203));
#50966=CARTESIAN_POINT('Ctrl Pts',(-10.4820847485064,31.637468725765,24.517392662528));
#50967=CARTESIAN_POINT('Ctrl Pts',(-10.1276831287408,31.6099675451656,24.5402396129539));
#50968=CARTESIAN_POINT('Ctrl Pts',(-9.99260102881325,31.6075711343711,24.5488308960645));
#50969=CARTESIAN_POINT('Ctrl Pts',(-9.79807649492301,31.6157428671968,24.5609265277053));
#50970=CARTESIAN_POINT('Ctrl Pts',(-9.73850081803834,31.6198242265351,24.5645946045661));
#50971=CARTESIAN_POINT('Ctrl Pts',(-9.63041023668735,31.6301043339381,24.571181857579));
#50972=CARTESIAN_POINT('Ctrl Pts',(-9.58186320276847,31.6357830948378,24.5741154059996));
#50973=CARTESIAN_POINT('Ctrl Pts',(-9.50445784953081,31.6465390938552,24.5787546789085));
#50974=CARTESIAN_POINT('Ctrl Pts',(-9.47551449149635,31.6509438488195,24.5804808506917));
#50975=CARTESIAN_POINT('Ctrl Pts',(-9.42033877975739,31.6600736315029,24.583756181418));
#50976=CARTESIAN_POINT('Ctrl Pts',(-9.39409811921259,31.6647341563619,24.5853072139116));
#50977=CARTESIAN_POINT('Ctrl Pts',(-9.33409786985865,31.6761221169906,24.5888396646425));
#50978=CARTESIAN_POINT('Ctrl Pts',(-9.30038004095852,31.6830553419444,24.5908145091278));
#50979=CARTESIAN_POINT('Ctrl Pts',(-9.19006831700129,31.70749516327,24.5972466329625));
#50980=CARTESIAN_POINT('Ctrl Pts',(-9.11397440444536,31.72715149279,24.6016370341393));
#50981=CARTESIAN_POINT('Ctrl Pts',(-8.80896738192478,31.8173589582658,24.6191471244879));
#50982=CARTESIAN_POINT('Ctrl Pts',(-8.58715702218629,31.9094272066104,24.6316240759671));
#50983=CARTESIAN_POINT('Ctrl Pts',(-8.29249733212567,32.0701395710731,24.649543263346));
#50984=CARTESIAN_POINT('Ctrl Pts',(-8.21009829635418,32.119740058332,24.6547255568649));
#50985=CARTESIAN_POINT('Ctrl Pts',(-8.09669859159546,32.1947485535841,24.6622559083283));
#50986=CARTESIAN_POINT('Ctrl Pts',(-8.06386495577287,32.2173083578861,24.6644860738599));
#50987=CARTESIAN_POINT('Ctrl Pts',(-8.00626338212422,32.2583990774589,24.6685022946936));
#50988=CARTESIAN_POINT('Ctrl Pts',(-7.98133681224192,32.2767005099841,24.6702759227249));
#50989=CARTESIAN_POINT('Ctrl Pts',(-7.94303937728579,32.3056337137126,24.6730626860955));
#50990=CARTESIAN_POINT('Ctrl Pts',(-7.92949201014461,32.3160303048044,24.6740607360829));
#50991=CARTESIAN_POINT('Ctrl Pts',(-7.9040892151567,32.3358318302873,24.6759566466741));
#50992=CARTESIAN_POINT('Ctrl Pts',(-7.89221736981219,32.3452144334309,24.6768530415));
#50993=CARTESIAN_POINT('Ctrl Pts',(-7.86370539158185,32.3680599266628,24.6790304474461));
#50994=CARTESIAN_POINT('Ctrl Pts',(-7.84712937311779,32.3816014024637,24.6803167366112));
#50995=CARTESIAN_POINT('Ctrl Pts',(-7.79069412837696,32.4286033057907,24.6847633795506));
#50996=CARTESIAN_POINT('Ctrl Pts',(-7.75147953748288,32.4628227273603,24.6879699769514));
#50997=CARTESIAN_POINT('Ctrl Pts',(-7.56239648637438,32.6356474182684,24.7039532512296));
#50998=CARTESIAN_POINT('Ctrl Pts',(-7.42447636238676,32.7866886688679,24.7172487192416));
#50999=CARTESIAN_POINT('Ctrl Pts',(-7.18378494213049,33.1034594890089,24.7427898806746));
#51000=CARTESIAN_POINT('Ctrl Pts',(-7.08000827381709,33.2674871264373,24.7550068616978));
#51001=CARTESIAN_POINT('Ctrl Pts',(-6.9701702869206,33.4792942672342,24.7694330112034));
#51002=CARTESIAN_POINT('Ctrl Pts',(-6.95032697822871,33.5194903699591,24.7721164481372));
#51003=CARTESIAN_POINT('Ctrl Pts',(-6.91920508131765,33.5858159424972,24.7764581553831));
#51004=CARTESIAN_POINT('Ctrl Pts',(-6.9074484187723,33.6117137648897,24.778132458361));
#51005=CARTESIAN_POINT('Ctrl Pts',(-6.88518322858662,33.662446810321,24.7813727219609));
#51006=CARTESIAN_POINT('Ctrl Pts',(-6.87464240460729,33.687265442976,24.782939673417));
#51007=CARTESIAN_POINT('Ctrl Pts',(-6.85029934367223,33.746537530876,24.7866402655671));
#51008=CARTESIAN_POINT('Ctrl Pts',(-6.8367644525545,33.7810974562904,24.788764948696));
#51009=CARTESIAN_POINT('Ctrl Pts',(-6.79290373373962,33.8987457486543,24.7958933691082));
#51010=CARTESIAN_POINT('Ctrl Pts',(-6.76526173564407,33.9827991857603,24.8008110292986));
#51011=CARTESIAN_POINT('Ctrl Pts',(-6.66630371271383,34.3287819850475,24.8205042823905));
#51012=CARTESIAN_POINT('Ctrl Pts',(-6.62328163017125,34.5977212700414,24.8344744210542));
#51013=CARTESIAN_POINT('Ctrl Pts',(-6.61022302245382,34.9351243512093,24.852758806131));
#51014=CARTESIAN_POINT('Ctrl Pts',(-6.6096026836829,35.0014027238726,24.8563915467869));
#51015=CARTESIAN_POINT('Ctrl Pts',(-6.61182336643764,35.1126475112598,24.8626179514774));
#51016=CARTESIAN_POINT('Ctrl Pts',(-6.61361745513232,35.1576173247334,24.8651704381664));
#51017=CARTESIAN_POINT('Ctrl Pts',(-6.61748568384727,35.2222424504657,24.868906370373));
#51018=CARTESIAN_POINT('Ctrl Pts',(-6.61883735722829,35.2419379015168,24.87005403492));
#51019=CARTESIAN_POINT('Ctrl Pts',(-6.62151395632357,35.2765145475507,24.8720865365758));
#51020=CARTESIAN_POINT('Ctrl Pts',(-6.62276533855362,35.2914005346689,24.8729674187618));
#51021=CARTESIAN_POINT('Ctrl Pts',(-6.62574829502362,35.3242795212311,24.8749263300077));
#51022=CARTESIAN_POINT('Ctrl Pts',(-6.62752538518625,35.3422670251966,24.8760066631514));
#51023=CARTESIAN_POINT('Ctrl Pts',(-6.63325599820558,35.3958851487253,24.8792510750172));
#51024=CARTESIAN_POINT('Ctrl Pts',(-6.63763087478682,35.4314671134746,24.8814359148847));
#51025=CARTESIAN_POINT('Ctrl Pts',(-6.66306125046046,35.6143064176287,24.8928042609559));
#51026=CARTESIAN_POINT('Ctrl Pts',(-6.69322803313417,35.7601215597907,24.9023376545813));
#51027=CARTESIAN_POINT('Ctrl Pts',(-6.76689822811388,36.0265275527062,24.9201419967892));
#51028=CARTESIAN_POINT('Ctrl Pts',(-6.807853772502,36.1475671557489,24.9283876597907));
#51029=CARTESIAN_POINT('Ctrl Pts',(-6.91181702503027,36.4057863683384,24.9460993640372));
#51030=CARTESIAN_POINT('Ctrl Pts',(-6.97735543101067,36.5416675614485,24.9554947061437));
#51031=CARTESIAN_POINT('Ctrl Pts',(-7.07280155197289,36.7098941663039,24.9671672477218));
#51032=CARTESIAN_POINT('Ctrl Pts',(-7.09457623989875,36.7466372943779,24.9697202037764));
#51033=CARTESIAN_POINT('Ctrl Pts',(-7.13177294527595,36.8067825466747,24.9739067234383));
#51034=CARTESIAN_POINT('Ctrl Pts',(-7.14680069096711,36.8304216404095,24.9755541697578));
#51035=CARTESIAN_POINT('Ctrl Pts',(-7.17683475990685,36.8763973432739,24.9787632310184));
#51036=CARTESIAN_POINT('Ctrl Pts',(-7.19181742038286,36.8987468560434,24.9803255511098));
#51037=CARTESIAN_POINT('Ctrl Pts',(-7.22538586335744,36.9475540279545,24.9837438659799));
#51038=CARTESIAN_POINT('Ctrl Pts',(-7.24408739419775,36.9739291046112,24.9855953902285));
#51039=CARTESIAN_POINT('Ctrl Pts',(-7.31045474192111,37.0647458723186,24.991990265523));
#51040=CARTESIAN_POINT('Ctrl Pts',(-7.36002806416642,37.1277637859511,24.9964618445592));
#51041=CARTESIAN_POINT('Ctrl Pts',(-7.59357434012739,37.4039059122624,25.016337395564));
#51042=CARTESIAN_POINT('Ctrl Pts',(-7.80140770260872,37.5953478339783,25.0308081024945));
#51043=CARTESIAN_POINT('Ctrl Pts',(-8.08505388986765,37.7978345718395,25.049670948102));
#51044=CARTESIAN_POINT('Ctrl Pts',(-8.14074216325374,37.8351466084457,25.0533430396186));
#51045=CARTESIAN_POINT('Ctrl Pts',(-8.23591532942056,37.8949038341931,25.059629642526));
#51046=CARTESIAN_POINT('Ctrl Pts',(-8.27481240491492,37.9182512376974,25.0622019332675));
#51047=CARTESIAN_POINT('Ctrl Pts',(-8.33134417493411,37.9506583912907,25.0659617118118));
#51048=CARTESIAN_POINT('Ctrl Pts',(-8.34860961260138,37.9603558826564,25.0671127853782));
#51049=CARTESIAN_POINT('Ctrl Pts',(-8.3790514016389,37.9771049728383,25.0691489450983));
#51050=CARTESIAN_POINT('Ctrl Pts',(-8.39219096032385,37.9842215832456,25.0700300226802));
#51051=CARTESIAN_POINT('Ctrl Pts',(-8.42128802356145,37.9997330950391,25.071986375748));
#51052=CARTESIAN_POINT('Ctrl Pts',(-8.43726551186566,38.00808760403,25.0730639129007));
#51053=CARTESIAN_POINT('Ctrl Pts',(-8.48403694018498,38.0320708398913,25.0762260874992));
#51054=CARTESIAN_POINT('Ctrl Pts',(-8.51500312988847,38.0473565060075,25.0783295298762));
#51055=CARTESIAN_POINT('Ctrl Pts',(-8.71707494132392,38.1432927835117,25.0920936307588));
#51056=CARTESIAN_POINT('Ctrl Pts',(-8.89443232965063,38.2099682747959,25.104329315168));
#51057=CARTESIAN_POINT('Ctrl Pts',(-9.22701757636996,38.3041496762514,25.1266041489797));
#51058=CARTESIAN_POINT('Ctrl Pts',(-9.38041031092342,38.3363187591695,25.1366350503712));
#51059=CARTESIAN_POINT('Ctrl Pts',(-9.62983306750515,38.3708237769615,25.152339574112));
#51060=CARTESIAN_POINT('Ctrl Pts',(-9.72469282572834,38.3798942411668,25.1581772941412));
#51061=CARTESIAN_POINT('Ctrl Pts',(-9.85700697659508,38.3869374285528,25.1661302544727));
#51062=CARTESIAN_POINT('Ctrl Pts',(-9.89422909683124,38.3883041232661,25.1683470025551));
#51063=CARTESIAN_POINT('Ctrl Pts',(-9.95844636072211,38.3896027087542,25.1721374235817));
#51064=CARTESIAN_POINT('Ctrl Pts',(-9.98543149969333,38.3898261090519,25.1737198832375));
#51065=CARTESIAN_POINT('Ctrl Pts',(-10.0408137242746,38.3896232365558,25.176947376927));
#51066=CARTESIAN_POINT('Ctrl Pts',(-10.0692085970337,38.3891623872687,25.178591223061));
#51067=CARTESIAN_POINT('Ctrl Pts',(-10.1421888457753,38.3870603269161,25.182790040654));
#51068=CARTESIAN_POINT('Ctrl Pts',(-10.1867543786129,38.3848956244716,25.1853288658937));
#51069=CARTESIAN_POINT('Ctrl Pts',(-10.4075522289393,38.3697965083944,25.197800676584));
#51070=CARTESIAN_POINT('Ctrl Pts',(-10.5826343583623,38.3439757491143,25.207333802329));
#51071=CARTESIAN_POINT('Ctrl Pts',(-10.9104044182862,38.2690986122176,25.2252288143845));
#51072=CARTESIAN_POINT('Ctrl Pts',(-11.0631822115104,38.2226514571052,25.2335967952355));
#51073=CARTESIAN_POINT('Ctrl Pts',(-11.2778418210958,38.1404583070954,25.2460122291844));
#51074=CARTESIAN_POINT('Ctrl Pts',(-11.3427634081787,38.1132528833275,25.249859945877));
#51075=CARTESIAN_POINT('Ctrl Pts',(-11.4495046871387,38.0645628796317,25.2564141280826));
#51076=CARTESIAN_POINT('Ctrl Pts',(-11.4918100652356,38.0441931213978,25.2590735633989));
#51077=CARTESIAN_POINT('Ctrl Pts',(-11.5515707743348,38.0138738889166,25.2629381110689));
#51078=CARTESIAN_POINT('Ctrl Pts',(-11.5693835782578,38.0046368878415,25.2641039588151));
#51079=CARTESIAN_POINT('Ctrl Pts',(-11.6003370923788,37.9882353045052,25.2661561336867));
#51080=CARTESIAN_POINT('Ctrl Pts',(-11.6135140243236,37.9811409774366,25.2670382201213));
#51081=CARTESIAN_POINT('Ctrl Pts',(-11.6422987305008,37.9653968250983,25.2689842001476));
#51082=CARTESIAN_POINT('Ctrl Pts',(-11.6578852319457,37.9567110066799,25.2700501788637));
#51083=CARTESIAN_POINT('Ctrl Pts',(-11.7026614991945,37.9312933781259,25.2731464020084));
#51084=CARTESIAN_POINT('Ctrl Pts',(-11.7316708777227,37.9142499612563,25.2751943427611));
#51085=CARTESIAN_POINT('Ctrl Pts',(-11.975306720037,37.766188390602,25.2927220602243));
#51086=CARTESIAN_POINT('Ctrl Pts',(-12.1749849035422,37.6121003403513,25.3092035926164));
#51087=CARTESIAN_POINT('Ctrl Pts',(-12.4401587470516,37.3558016131274,25.3328070381349));
#51088=CARTESIAN_POINT('Ctrl Pts',(-12.520250813079,37.2699153350808,25.3402293868745));
#51089=CARTESIAN_POINT('Ctrl Pts',(-12.6469040594358,37.1191118326437,25.3524164956147));
#51090=CARTESIAN_POINT('Ctrl Pts',(-12.6959178312605,37.0563960387051,25.3572645763915));
#51091=CARTESIAN_POINT('Ctrl Pts',(-12.7632229329192,36.9637275434503,25.3641209390319));
#51092=CARTESIAN_POINT('Ctrl Pts',(-12.7833257353138,36.9351291508179,25.3661969174104));
#51093=CARTESIAN_POINT('Ctrl Pts',(-12.8179653236338,36.884193805346,25.3698259824461));
#51094=CARTESIAN_POINT('Ctrl Pts',(-12.8326875270972,36.8619871898949,25.3713858794255));
#51095=CARTESIAN_POINT('Ctrl Pts',(-12.8630497633172,36.8149958189048,25.3746413425437));
#51096=CARTESIAN_POINT('Ctrl Pts',(-12.8786333281256,36.7901770890239,25.3763347577147));
#51097=CARTESIAN_POINT('Ctrl Pts',(-12.9194152057811,36.7233171511918,25.3808300696828));
#51098=CARTESIAN_POINT('Ctrl Pts',(-12.9440273257785,36.6809255167799,25.3836109977847));
#51099=CARTESIAN_POINT('Ctrl Pts',(-13.0495231215506,36.4897908377745,25.3958677956707));
#51100=CARTESIAN_POINT('Ctrl Pts',(-13.1200460176431,36.3357727065211,25.4049838019441));
#51101=CARTESIAN_POINT('Ctrl Pts',(-13.1787500473324,36.1772651354238,25.4139790685232));
#51102=CARTESIAN_POINT('Origin',(-10.,35.,23.));
#51103=CARTESIAN_POINT('',(-13.178750052031,36.1772651227369,26.6607620761902));
#51104=CARTESIAN_POINT('',(-13.1787501361565,36.1772648955886,26.3195304627418));
#51105=CARTESIAN_POINT('',(-13.1787500671536,36.1772650819043,23.));
#51106=CARTESIAN_POINT('',(-13.3897489515612,35.0026660626174,25.139683636804));
#51107=CARTESIAN_POINT('Ctrl Pts',(-13.1787501361565,36.1772648955886,26.3195304627418));
#51108=CARTESIAN_POINT('Ctrl Pts',(-13.1275293037145,36.3155670132421,26.3116510922332));
#51109=CARTESIAN_POINT('Ctrl Pts',(-13.0673160770592,36.4504360067458,26.3039018533949));
#51110=CARTESIAN_POINT('Ctrl Pts',(-12.9360697556378,36.6993528101704,26.2888533953585));
#51111=CARTESIAN_POINT('Ctrl Pts',(-12.8667215596882,36.8138925045017,26.2815932999696));
#51112=CARTESIAN_POINT('Ctrl Pts',(-12.7748582381106,36.9471402705108,26.2723743592933));
#51113=CARTESIAN_POINT('Ctrl Pts',(-12.7586346998618,36.9700578567182,26.2707593878122));
#51114=CARTESIAN_POINT('Ctrl Pts',(-12.732444421697,37.0060966882031,26.2681682566491));
#51115=CARTESIAN_POINT('Ctrl Pts',(-12.7226631404088,37.0193518364037,26.2672039542068));
#51116=CARTESIAN_POINT('Ctrl Pts',(-12.7035594609724,37.0448491562393,26.2653260017636));
#51117=CARTESIAN_POINT('Ctrl Pts',(-12.6942496972644,37.0570999892027,26.2644131582124));
#51118=CARTESIAN_POINT('Ctrl Pts',(-12.6708782214884,37.0874240017261,26.262128083507));
#51119=CARTESIAN_POINT('Ctrl Pts',(-12.6567162805108,37.1054187182352,26.2607492532518));
#51120=CARTESIAN_POINT('Ctrl Pts',(-12.6001877712615,37.1757675558729,26.2552727190622));
#51121=CARTESIAN_POINT('Ctrl Pts',(-12.5564494902722,37.2269947640009,26.2510944263239));
#51122=CARTESIAN_POINT('Ctrl Pts',(-12.4289837806037,37.3675792125859,26.2391567536474));
#51123=CARTESIAN_POINT('Ctrl Pts',(-12.341900084493,37.4537511963823,26.2312750484712));
#51124=CARTESIAN_POINT('Ctrl Pts',(-12.0685105409671,37.6964405626681,26.2077111659704));
#51125=CARTESIAN_POINT('Ctrl Pts',(-11.8698015821148,37.8378520034734,26.1921269069638));
#51126=CARTESIAN_POINT('Ctrl Pts',(-11.6128238807767,37.9819196123726,26.1742101421693));
#51127=CARTESIAN_POINT('Ctrl Pts',(-11.5674350984947,38.0060261291993,26.1711195098881));
#51128=CARTESIAN_POINT('Ctrl Pts',(-11.4946394343588,38.0425914087537,26.1662764067341));
#51129=CARTESIAN_POINT('Ctrl Pts',(-11.4675859575751,38.0557324921846,26.1645007869129));
#51130=CARTESIAN_POINT('Ctrl Pts',(-11.4187814457073,38.0786413446195,26.161339755989));
#51131=CARTESIAN_POINT('Ctrl Pts',(-11.3970957423347,38.0885428358814,26.1599498773572));
#51132=CARTESIAN_POINT('Ctrl Pts',(-11.3458353109171,38.1112974963614,26.1566979982741));
#51133=CARTESIAN_POINT('Ctrl Pts',(-11.31617778294,38.1239591772765,26.1548425128361));
#51134=CARTESIAN_POINT('Ctrl Pts',(-11.2272517195581,38.160433124529,26.149352274682));
#51135=CARTESIAN_POINT('Ctrl Pts',(-11.1674845477299,38.1829962091945,26.1457584688189));
#51136=CARTESIAN_POINT('Ctrl Pts',(-10.9515859052322,38.2576013036794,26.133071779718));
#51137=CARTESIAN_POINT('Ctrl Pts',(-10.7923438257267,38.2999514203855,26.1242691563581));
#51138=CARTESIAN_POINT('Ctrl Pts',(-10.4225482046364,38.3699727235213,26.1042887597988));
#51139=CARTESIAN_POINT('Ctrl Pts',(-10.2112343148089,38.389782548502,26.0932033489857));
#51140=CARTESIAN_POINT('Ctrl Pts',(-9.95505955389538,38.3897431239352,26.0788606215348));
#51141=CARTESIAN_POINT('Ctrl Pts',(-9.91064735909992,38.3888632030355,26.076340266163));
#51142=CARTESIAN_POINT('Ctrl Pts',(-9.84684763951365,38.3863442141167,26.0726550445531));
#51143=CARTESIAN_POINT('Ctrl Pts',(-9.82743521529211,38.3854104829736,26.0715251189875));
#51144=CARTESIAN_POINT('Ctrl Pts',(-9.79311507733015,38.383463747946,26.0695105551651));
#51145=CARTESIAN_POINT('Ctrl Pts',(-9.7782043870701,38.3825190315678,26.0686295832056));
#51146=CARTESIAN_POINT('Ctrl Pts',(-9.74528999012911,38.3802150555544,26.0666718741739));
#51147=CARTESIAN_POINT('Ctrl Pts',(-9.72729081810735,38.3788105423087,26.0655928529111));
#51148=CARTESIAN_POINT('Ctrl Pts',(-9.67369492241274,38.3741973078412,26.0623563811923));
#51149=CARTESIAN_POINT('Ctrl Pts',(-9.63813786584196,38.3705693959921,26.060178313178));
#51150=CARTESIAN_POINT('Ctrl Pts',(-9.45997914560893,38.3495402762919,26.0491315355943));
#51151=CARTESIAN_POINT('Ctrl Pts',(-9.31853753500384,38.3236493436193,26.0399366963367));
#51152=CARTESIAN_POINT('Ctrl Pts',(-8.91465693344667,38.2228504292406,26.0131331119742));
#51153=CARTESIAN_POINT('Ctrl Pts',(-8.65901756661329,38.1251478362792,25.9955696647063));
#51154=CARTESIAN_POINT('Ctrl Pts',(-8.3750743612192,37.9752913099574,25.976099755814));
#51155=CARTESIAN_POINT('Ctrl Pts',(-8.33281000526718,37.9518163210347,25.9731990792327));
#51156=CARTESIAN_POINT('Ctrl Pts',(-8.26587317576551,37.9127409452949,25.9685988784394));
#51157=CARTESIAN_POINT('Ctrl Pts',(-8.24087608367216,37.8977126813187,25.9668795096363));
#51158=CARTESIAN_POINT('Ctrl Pts',(-8.19338814528815,37.8683219039009,25.9636093324775));
#51159=CARTESIAN_POINT('Ctrl Pts',(-8.17086694621227,37.8540128362286,25.9620567602209));
#51160=CARTESIAN_POINT('Ctrl Pts',(-8.1189902405869,37.8201861331183,25.958475246064));
#51161=CARTESIAN_POINT('Ctrl Pts',(-8.08976528343335,37.800473352958,25.9564536415056));
#51162=CARTESIAN_POINT('Ctrl Pts',(-7.99405206312668,37.733717409021,25.9498141826609));
#51163=CARTESIAN_POINT('Ctrl Pts',(-7.92894950392359,37.6847326214061,25.9452685852849));
#51164=CARTESIAN_POINT('Ctrl Pts',(-7.77122064623841,37.5568981807403,25.9341091572406));
#51165=CARTESIAN_POINT('Ctrl Pts',(-7.6809530164362,37.475320059597,25.927590194822));
#51166=CARTESIAN_POINT('Ctrl Pts',(-7.4657713371864,37.2587265325699,25.9113514605366));
#51167=CARTESIAN_POINT('Ctrl Pts',(-7.34710101386797,37.1180840911621,25.9017337902083));
#51168=CARTESIAN_POINT('Ctrl Pts',(-7.19535360780638,36.9053569488521,25.8874505685673));
#51169=CARTESIAN_POINT('Ctrl Pts',(-7.15247585933609,36.8406604867681,25.8831352834082));
#51170=CARTESIAN_POINT('Ctrl Pts',(-7.09892555608304,36.7535057648641,25.877281531557));
#51171=CARTESIAN_POINT('Ctrl Pts',(-7.08622326977071,36.732316508884,25.8758552874268));
#51172=CARTESIAN_POINT('Ctrl Pts',(-7.06659106432234,36.6987402591333,25.87358743745));
#51173=CARTESIAN_POINT('Ctrl Pts',(-7.05950515217262,36.6864449252258,25.8727553373451));
#51174=CARTESIAN_POINT('Ctrl Pts',(-7.04480873252465,36.6605697705818,25.8710000266439));
#51175=CARTESIAN_POINT('Ctrl Pts',(-7.03721426087042,36.6469814884838,25.8700757835793));
#51176=CARTESIAN_POINT('Ctrl Pts',(-7.01823479764693,36.6124667064079,25.8677229102746));
#51177=CARTESIAN_POINT('Ctrl Pts',(-7.00697644950711,36.591471821073,25.8662868511381));
#51178=CARTESIAN_POINT('Ctrl Pts',(-6.96084190222991,36.503217626561,25.8602355795365));
#51179=CARTESIAN_POINT('Ctrl Pts',(-6.92800649605403,36.4349213974346,25.8555178657469));
#51180=CARTESIAN_POINT('Ctrl Pts',(-6.83676988804999,36.2276388294385,25.8412141486208));
#51181=CARTESIAN_POINT('Ctrl Pts',(-6.78532081259013,36.0857978917837,25.831452983835));
#51182=CARTESIAN_POINT('Ctrl Pts',(-6.6875560973918,35.7474668904436,25.8087826760018));
#51183=CARTESIAN_POINT('Ctrl Pts',(-6.64898825076266,35.5493013221105,25.7959825536002));
#51184=CARTESIAN_POINT('Ctrl Pts',(-6.62279325577151,35.2961256535132,25.7804840904007));
#51185=CARTESIAN_POINT('Ctrl Pts',(-6.61857471691793,35.2432680108596,25.7772922963834));
#51186=CARTESIAN_POINT('Ctrl Pts',(-6.61388941396592,35.1599554438428,25.7723284545866));
#51187=CARTESIAN_POINT('Ctrl Pts',(-6.61259014418947,35.1295577247001,25.7705312779608));
#51188=CARTESIAN_POINT('Ctrl Pts',(-6.61092676477455,35.0727119073951,25.7671954272703));
#51189=CARTESIAN_POINT('Ctrl Pts',(-6.61046262321786,35.0462692668806,25.7656538022693));
#51190=CARTESIAN_POINT('Ctrl Pts',(-6.61011468628387,34.9867737796948,25.7622067123146));
#51191=CARTESIAN_POINT('Ctrl Pts',(-6.61040476393469,34.9537223719902,25.7603067180634));
#51192=CARTESIAN_POINT('Ctrl Pts',(-6.61277593008491,34.8524185078345,25.7545250526883));
#51193=CARTESIAN_POINT('Ctrl Pts',(-6.61643584820695,34.7842184120162,25.7506913925367));
#51194=CARTESIAN_POINT('Ctrl Pts',(-6.64315860307748,34.4661899715361,25.73301560677));
#51195=CARTESIAN_POINT('Ctrl Pts',(-6.69184675734686,34.2193182773196,25.7199448208357));
#51196=CARTESIAN_POINT('Ctrl Pts',(-6.81084275816068,33.842159700656,25.6988475975735));
#51197=CARTESIAN_POINT('Ctrl Pts',(-6.86313146312335,33.7071870752379,25.6910331903002));
#51198=CARTESIAN_POINT('Ctrl Pts',(-6.93575182762144,33.5503144797316,25.6811890543293));
#51199=CARTESIAN_POINT('Ctrl Pts',(-6.94795358343876,33.5247991560503,25.6795626933458));
#51200=CARTESIAN_POINT('Ctrl Pts',(-6.9677845409416,33.4846296516265,25.6769575101952));
#51201=CARTESIAN_POINT('Ctrl Pts',(-6.97520432366668,33.4698728894683,25.6759907662249));
#51202=CARTESIAN_POINT('Ctrl Pts',(-6.9897332507737,33.4414958443124,25.674111829048));
#51203=CARTESIAN_POINT('Ctrl Pts',(-6.9968276186201,33.4278687337668,25.6732004926753));
#51204=CARTESIAN_POINT('Ctrl Pts',(-7.01466685717736,33.3941638751519,25.6709246808398));
#51205=CARTESIAN_POINT('Ctrl Pts',(-7.02552179740678,33.3741454573063,25.6695537194397));
#51206=CARTESIAN_POINT('Ctrl Pts',(-7.06875424686307,33.2962994110933,25.6641511004625));
#51207=CARTESIAN_POINT('Ctrl Pts',(-7.10262141876041,33.239320147732,25.6600414748331));
#51208=CARTESIAN_POINT('Ctrl Pts',(-7.20200129245492,33.0827596500587,25.6483824669053));
#51209=CARTESIAN_POINT('Ctrl Pts',(-7.27112703209098,32.9855876497149,25.6407165603508));
#51210=CARTESIAN_POINT('Ctrl Pts',(-7.49992591407496,32.6974065492212,25.6170006440483));
#51211=CARTESIAN_POINT('Ctrl Pts',(-7.67563750068054,32.5201446055275,25.6010378242968));
#51212=CARTESIAN_POINT('Ctrl Pts',(-7.908718515938,32.33175534775,25.5828195237582));
#51213=CARTESIAN_POINT('Ctrl Pts',(-7.94895775156781,32.3007012237518,25.5797638550779));
#51214=CARTESIAN_POINT('Ctrl Pts',(-8.01399985670856,32.2528003961934,25.5749625457225));
#51215=CARTESIAN_POINT('Ctrl Pts',(-8.03835286149508,32.2353584640058,25.5731944251065));
#51216=CARTESIAN_POINT('Ctrl Pts',(-8.08468636664157,32.203094331023,25.5698846187334));
#51217=CARTESIAN_POINT('Ctrl Pts',(-8.10661562962621,32.1882028309092,25.5683404108251));
#51218=CARTESIAN_POINT('Ctrl Pts',(-8.15686931485316,32.1549315947795,25.5648507548753));
#51219=CARTESIAN_POINT('Ctrl Pts',(-8.18529842637698,32.1367146022925,25.562911379592));
#51220=CARTESIAN_POINT('Ctrl Pts',(-8.2754877120701,32.0808054553026,25.5568626564743));
#51221=CARTESIAN_POINT('Ctrl Pts',(-8.33818698640275,32.044662803327,25.5528083057104));
#51222=CARTESIAN_POINT('Ctrl Pts',(-8.49195106430681,31.9624685908534,25.5431756415221));
#51223=CARTESIAN_POINT('Ctrl Pts',(-8.58403203672346,31.9184670592111,25.5376595771576));
#51224=CARTESIAN_POINT('Ctrl Pts',(-8.7221275872218,31.8599764721752,25.5296368796231));
#51225=CARTESIAN_POINT('Ctrl Pts',(-8.76668633368025,31.8422091338516,25.5270846785267));
#51226=CARTESIAN_POINT('Ctrl Pts',(-9.00739032764444,31.752103231928,25.5134383882406));
#51227=CARTESIAN_POINT('Ctrl Pts',(-9.2095145713375,31.697088564832,25.5024973692784));
#51228=CARTESIAN_POINT('Ctrl Pts',(-9.46092523955007,31.6530700603128,25.4882441144485));
#51229=CARTESIAN_POINT('Ctrl Pts',(-9.50661157815093,31.6460308503453,25.485627614754));
#51230=CARTESIAN_POINT('Ctrl Pts',(-9.57084239733155,31.6374750519693,25.4818945626879));
#51231=CARTESIAN_POINT('Ctrl Pts',(-9.58927900799401,31.6351733317521,25.4808167729782));
#51232=CARTESIAN_POINT('Ctrl Pts',(-9.62272441959315,31.6312768016293,25.4788487452096));
#51233=CARTESIAN_POINT('Ctrl Pts',(-9.63772696093006,31.6296304222895,25.4779612606449));
#51234=CARTESIAN_POINT('Ctrl Pts',(-9.66936998301466,31.6263716353199,25.4760787322545));
#51235=CARTESIAN_POINT('Ctrl Pts',(-9.6860119969392,31.6247820723671,25.4750825663478));
#51236=CARTESIAN_POINT('Ctrl Pts',(-9.73177405669042,31.620752475635,25.4723278612193));
#51237=CARTESIAN_POINT('Ctrl Pts',(-9.76091430141407,31.6185658528079,25.4705565559212));
#51238=CARTESIAN_POINT('Ctrl Pts',(-9.82699099950323,31.6144659568371,25.4665066047314));
#51239=CARTESIAN_POINT('Ctrl Pts',(-9.86393755295473,31.6127799490557,25.464218470908));
#51240=CARTESIAN_POINT('Ctrl Pts',(-9.98615724706017,31.6092054067664,25.4565866189869));
#51241=CARTESIAN_POINT('Ctrl Pts',(-10.0714711667598,31.6099306859455,25.451159193638));
#51242=CARTESIAN_POINT('Ctrl Pts',(-10.4342489180101,31.6267149018692,25.4278699980286));
#51243=CARTESIAN_POINT('Ctrl Pts',(-10.7092551647009,31.6736468145872,25.4098054879696));
#51244=CARTESIAN_POINT('Ctrl Pts',(-11.0361669224451,31.7718765194759,25.3888701735249));
#51245=CARTESIAN_POINT('Ctrl Pts',(-11.0963527678074,31.7918175694263,25.3850331258267));
#51246=CARTESIAN_POINT('Ctrl Pts',(-11.1865500028866,31.8245372101359,25.3793069739075));
#51247=CARTESIAN_POINT('Ctrl Pts',(-11.2169921272335,31.836079155179,25.3773785525555));
#51248=CARTESIAN_POINT('Ctrl Pts',(-11.2718254583321,31.8577774121937,25.3739114891858));
#51249=CARTESIAN_POINT('Ctrl Pts',(-11.296272888264,31.8677836209125,25.3723680588408));
#51250=CARTESIAN_POINT('Ctrl Pts',(-11.3489653591365,31.8900729921109,25.3690455176644));
#51251=CARTESIAN_POINT('Ctrl Pts',(-11.377165145625,31.9024574601535,25.3672699444308));
#51252=CARTESIAN_POINT('Ctrl Pts',(-11.4564828926092,31.9385886951742,25.3622802668674));
#51253=CARTESIAN_POINT('Ctrl Pts',(-11.5071840482756,31.9632289608131,25.359096286936));
#51254=CARTESIAN_POINT('Ctrl Pts',(-11.6213290531763,32.0222656589352,25.3519220577914));
#51255=CARTESIAN_POINT('Ctrl Pts',(-11.6843367330153,32.057446631537,25.347957719094));
#51256=CARTESIAN_POINT('Ctrl Pts',(-11.911358391023,32.1938896874611,25.3335722052934));
#51257=CARTESIAN_POINT('Ctrl Pts',(-12.0677716748163,32.3070707873441,25.323480277421));
#51258=CARTESIAN_POINT('Ctrl Pts',(-12.3270273149047,32.5306409346461,25.3052358954368));
#51259=CARTESIAN_POINT('Ctrl Pts',(-12.4337280804593,32.63573508668,25.2971662840273));
#51260=CARTESIAN_POINT('Ctrl Pts',(-12.551936842087,32.7686719969475,25.2870362578449));
#51261=CARTESIAN_POINT('Ctrl Pts',(-12.5704798986837,32.7900589866139,25.2854085809478));
#51262=CARTESIAN_POINT('Ctrl Pts',(-12.5994186357054,32.8242930330407,25.2828017742787));
#51263=CARTESIAN_POINT('Ctrl Pts',(-12.6099923323982,32.8369886617042,25.281834748339));
#51264=CARTESIAN_POINT('Ctrl Pts',(-12.6302165842051,32.8616357319033,25.2799556937193));
#51265=CARTESIAN_POINT('Ctrl Pts',(-12.6398793801173,32.8735762776283,25.2790445276599));
#51266=CARTESIAN_POINT('Ctrl Pts',(-12.6636559223769,32.9033693451576,25.2767697680011));
#51267=CARTESIAN_POINT('Ctrl Pts',(-12.6776715465503,32.9212989626353,25.2753997013193));
#51268=CARTESIAN_POINT('Ctrl Pts',(-12.7317198872348,32.9918944756329,25.2700054156625));
#51269=CARTESIAN_POINT('Ctrl Pts',(-12.7703857646075,33.0455837486532,25.2659035212957));
#51270=CARTESIAN_POINT('Ctrl Pts',(-12.8788185821629,33.2058357150553,25.2537390742254));
#51271=CARTESIAN_POINT('Ctrl Pts',(-12.9441804209429,33.3152386766303,25.2455359813105));
#51272=CARTESIAN_POINT('Ctrl Pts',(-13.1084485820639,33.6290757093731,25.2227021709515));
#51273=CARTESIAN_POINT('Ctrl Pts',(-13.1932325883007,33.8401817121344,25.2081577404558));
#51274=CARTESIAN_POINT('Ctrl Pts',(-13.2711801538501,34.1096864905325,25.1910044784193));
#51275=CARTESIAN_POINT('Ctrl Pts',(-13.2848488903701,34.1615216174511,25.1877640333986));
#51276=CARTESIAN_POINT('Ctrl Pts',(-13.3050041541777,34.2460368784401,25.1825736372484));
#51277=CARTESIAN_POINT('Ctrl Pts',(-13.3122480302675,34.278525154762,25.1806003659227));
#51278=CARTESIAN_POINT('Ctrl Pts',(-13.3243904396943,34.3370267211086,25.177085183281));
#51279=CARTESIAN_POINT('Ctrl Pts',(-13.3294649444423,34.3630003087431,25.1755378702808));
#51280=CARTESIAN_POINT('Ctrl Pts',(-13.3387175006471,34.4134942070377,25.1725547367493));
#51281=CARTESIAN_POINT('Ctrl Pts',(-13.3429308486618,34.438006242891,25.1711179063616));
#51282=CARTESIAN_POINT('Ctrl Pts',(-13.3516007075619,34.4919975417983,25.1679767972371));
#51283=CARTESIAN_POINT('Ctrl Pts',(-13.3559388788068,34.5214938654338,25.1662762338235));
#51284=CARTESIAN_POINT('Ctrl Pts',(-13.3674687876274,34.6077812026211,25.161343445804));
#51285=CARTESIAN_POINT('Ctrl Pts',(-13.3736120216804,34.6647030477051,25.1581424529301));
#51286=CARTESIAN_POINT('Ctrl Pts',(-13.3860065433332,34.8151913438201,25.149793627205));
#51287=CARTESIAN_POINT('Ctrl Pts',(-13.3898226925466,34.9089085392964,25.1447108366345));
#51288=CARTESIAN_POINT('Ctrl Pts',(-13.3897489515612,35.0026660626174,25.139683636804));
#51289=CARTESIAN_POINT('Ctrl Pts',(-13.3897489540441,35.0026629038459,25.1396838061747));
#51290=CARTESIAN_POINT('Ctrl Pts',(-13.3895586151162,35.2449552355166,25.1266922911326));
#51291=CARTESIAN_POINT('Ctrl Pts',(-13.3633917304235,35.486518723814,25.114168333125));
#51292=CARTESIAN_POINT('Ctrl Pts',(-13.2975733377464,35.7879081937708,25.0971784745588));
#51293=CARTESIAN_POINT('Ctrl Pts',(-13.2815550038618,35.8521648037139,25.0934711323419));
#51294=CARTESIAN_POINT('Ctrl Pts',(-13.2575155904463,35.9378248654316,25.0883645600871));
#51295=CARTESIAN_POINT('Ctrl Pts',(-13.2511440960134,35.9596797938305,25.0870471058161));
#51296=CARTESIAN_POINT('Ctrl Pts',(-13.2401052720513,35.9961721115334,25.0848202522941));
#51297=CARTESIAN_POINT('Ctrl Pts',(-13.235557549218,36.01084538306,25.0839174652042));
#51298=CARTESIAN_POINT('Ctrl Pts',(-13.2259125759084,36.0412329325706,25.0820316066258));
#51299=CARTESIAN_POINT('Ctrl Pts',(-13.2207999761956,36.0569415572434,25.0810477592457));
#51300=CARTESIAN_POINT('Ctrl Pts',(-13.2066196900164,36.0994525038195,25.0783620751255));
#51301=CARTESIAN_POINT('Ctrl Pts',(-13.1973311007903,36.1261790988632,25.0766484626819));
#51302=CARTESIAN_POINT('Ctrl Pts',(-13.1847541388108,36.1609572133311,25.074388478803));
#51303=CARTESIAN_POINT('Ctrl Pts',(-13.1817676762443,36.1691171929711,25.07385603406));
#51304=CARTESIAN_POINT('Ctrl Pts',(-13.1787500684596,36.1772650783778,25.0733222522952));
#51305=CARTESIAN_POINT('Ctrl Pts',(-13.1787500473324,36.1772651354238,25.4139790685232));
#51306=CARTESIAN_POINT('Ctrl Pts',(-13.2129579337196,36.0848999432503,25.4192207709888));
#51307=CARTESIAN_POINT('Ctrl Pts',(-13.2431524082573,35.9910104588357,25.4244252688241));
#51308=CARTESIAN_POINT('Ctrl Pts',(-13.3114026221524,35.7419465658512,25.4381644453243));
#51309=CARTESIAN_POINT('Ctrl Pts',(-13.3426522696491,35.5852664646178,25.4467389538416));
#51310=CARTESIAN_POINT('Ctrl Pts',(-13.3663308409915,35.3987855749979,25.4574416608772));
#51311=CARTESIAN_POINT('Ctrl Pts',(-13.3695568188617,35.3705401434797,25.4590761898304));
#51312=CARTESIAN_POINT('Ctrl Pts',(-13.3740979390716,35.3257944389112,25.4616914500143));
#51313=CARTESIAN_POINT('Ctrl Pts',(-13.3756482038414,35.3093187639212,25.4626599435699));
#51314=CARTESIAN_POINT('Ctrl Pts',(-13.3783882017451,35.2777198903346,25.4645291472995));
#51315=CARTESIAN_POINT('Ctrl Pts',(-13.379597151546,35.2625990083102,25.4654288302341));
#51316=CARTESIAN_POINT('Ctrl Pts',(-13.3823498930941,35.2249937680228,25.4676785497845));
#51317=CARTESIAN_POINT('Ctrl Pts',(-13.383770993291,35.2025013577761,25.4690349730233));
#51318=CARTESIAN_POINT('Ctrl Pts',(-13.3881296066075,35.1205346874929,25.4740133933695));
#51319=CARTESIAN_POINT('Ctrl Pts',(-13.3897239751888,35.0610028093467,25.4776967957614));
#51320=CARTESIAN_POINT('Ctrl Pts',(-13.389794204842,34.898358979822,25.4878914648462));
#51321=CARTESIAN_POINT('Ctrl Pts',(-13.3851345436779,34.7953108227253,25.4944935619505));
#51322=CARTESIAN_POINT('Ctrl Pts',(-13.3515711501112,34.4266772184745,25.5183173666823));
#51323=CARTESIAN_POINT('Ctrl Pts',(-13.2960042092167,34.164459520482,25.5355549120409));
#51324=CARTESIAN_POINT('Ctrl Pts',(-13.1929876577644,33.8606521634231,25.5550979313356));
#51325=CARTESIAN_POINT('Ctrl Pts',(-13.174553782942,33.8102553022593,25.5583292040501));
#51326=CARTESIAN_POINT('Ctrl Pts',(-13.1437546594498,33.7318732161826,25.5633400842122));
#51327=CARTESIAN_POINT('Ctrl Pts',(-13.132194492935,33.7035831501014,25.5651456110598));
#51328=CARTESIAN_POINT('Ctrl Pts',(-13.1099245406714,33.651121543416,25.5684892082005));
#51329=CARTESIAN_POINT('Ctrl Pts',(-13.0993115773421,33.6269116764551,25.5700303504126));
#51330=CARTESIAN_POINT('Ctrl Pts',(-13.0748705108757,33.5728852696599,25.5734665162781));
#51331=CARTESIAN_POINT('Ctrl Pts',(-13.0608896749292,33.5431404945895,25.5753562265366));
#51332=CARTESIAN_POINT('Ctrl Pts',(-13.0169918116406,33.4531686515352,25.5810696311151));
#51333=CARTESIAN_POINT('Ctrl Pts',(-12.9857125403696,33.3936226256971,25.5848470208367));
#51334=CARTESIAN_POINT('Ctrl Pts',(-12.830387160293,33.1181641750318,25.6023726157613));
#51335=CARTESIAN_POINT('Ctrl Pts',(-12.6845745934833,32.9154228338062,25.6153580405207));
#51336=CARTESIAN_POINT('Ctrl Pts',(-12.4187424083374,32.6205022365624,25.6365240637188));
#51337=CARTESIAN_POINT('Ctrl Pts',(-12.3125292888982,32.5171541309261,25.6445139537417));
#51338=CARTESIAN_POINT('Ctrl Pts',(-12.1783851522986,32.4027237243424,25.6545545900013));
#51339=CARTESIAN_POINT('Ctrl Pts',(-12.1566265858284,32.3846285957447,25.6561818926817));
#51340=CARTESIAN_POINT('Ctrl Pts',(-12.121811194821,32.3564048616195,25.6587882374092));
#51341=CARTESIAN_POINT('Ctrl Pts',(-12.1089020140346,32.3460952782005,25.6597551829125));
#51342=CARTESIAN_POINT('Ctrl Pts',(-12.0838449647861,32.3263823742694,25.6616342032859));
#51343=CARTESIAN_POINT('Ctrl Pts',(-12.0717077185813,32.3169666158632,25.6625454171772));
#51344=CARTESIAN_POINT('Ctrl Pts',(-12.041428341085,32.2938046098369,25.6648204739112));
#51345=CARTESIAN_POINT('Ctrl Pts',(-12.023211104007,32.2801581059877,25.6661907934732));
#51346=CARTESIAN_POINT('Ctrl Pts',(-11.9514883757159,32.2275500026887,25.6715874359183));
#51347=CARTESIAN_POINT('Ctrl Pts',(-11.8969867100227,32.1899775592534,25.6756915169324));
#51348=CARTESIAN_POINT('Ctrl Pts',(-11.741586563053,32.0894293128611,25.6873282187567));
#51349=CARTESIAN_POINT('Ctrl Pts',(-11.638423302349,32.0301326571558,25.694976903951));
#51350=CARTESIAN_POINT('Ctrl Pts',(-11.3100242659808,31.8637007264316,25.7187055492107));
#51351=CARTESIAN_POINT('Ctrl Pts',(-11.0758988969106,31.7758698465472,25.7346992769268));
#51352=CARTESIAN_POINT('Ctrl Pts',(-10.7844414725703,31.7018648464897,25.7529783223421));
#51353=CARTESIAN_POINT('Ctrl Pts',(-10.7343688324649,31.690355492673,25.7560665249389));
#51354=CARTESIAN_POINT('Ctrl Pts',(-10.6548757687406,31.6739768239713,25.7608893422627));
#51355=CARTESIAN_POINT('Ctrl Pts',(-10.625621100955,31.6683501440244,25.7626473326219));
#51356=CARTESIAN_POINT('Ctrl Pts',(-10.5701750566453,31.6584420514336,25.7659484364741));
#51357=CARTESIAN_POINT('Ctrl Pts',(-10.5440003376274,31.6540811709684,25.7674939191911));
#51358=CARTESIAN_POINT('Ctrl Pts',(-10.484138444133,31.6448288295742,25.771000307956));
#51359=CARTESIAN_POINT('Ctrl Pts',(-10.4504231103753,31.6401364971965,25.7729549082072));
#51360=CARTESIAN_POINT('Ctrl Pts',(-10.3432343308713,31.6268610184773,25.779109450332));
#51361=CARTESIAN_POINT('Ctrl Pts',(-10.2695456274935,31.6201741715645,25.7832514883377));
#51362=CARTESIAN_POINT('Ctrl Pts',(-10.0905435619604,31.6098229612272,25.7931480676126));
#51363=CARTESIAN_POINT('Ctrl Pts',(-9.98516328836684,31.6086462331143,25.7988353102028));
#51364=CARTESIAN_POINT('Ctrl Pts',(-9.75584269178043,31.6167766142942,25.8110957658923));
#51365=CARTESIAN_POINT('Ctrl Pts',(-9.63212658365565,31.6279853995241,25.8176357061282));
#51366=CARTESIAN_POINT('Ctrl Pts',(-9.36614051087889,31.6668990869816,25.831943014208));
#51367=CARTESIAN_POINT('Ctrl Pts',(-9.22447753827665,31.6969867277509,25.8397195612678));
#51368=CARTESIAN_POINT('Ctrl Pts',(-9.05086008350839,31.7456476525079,25.8499003880931));
#51369=CARTESIAN_POINT('Ctrl Pts',(-9.01669091796208,31.7558084487553,25.8519364909765));
#51370=CARTESIAN_POINT('Ctrl Pts',(-8.96548551177221,31.7719185076869,25.8550455522482));
#51371=CARTESIAN_POINT('Ctrl Pts',(-8.94832512955932,31.7774683426617,25.8560973605369));
#51372=CARTESIAN_POINT('Ctrl Pts',(-8.91702917831271,31.7878663532101,25.8580350543435));
#51373=CARTESIAN_POINT('Ctrl Pts',(-8.90288022146633,31.7926714339753,25.85891853074));
#51374=CARTESIAN_POINT('Ctrl Pts',(-8.87006237815579,31.8040591563383,25.8609848857952));
#51375=CARTESIAN_POINT('Ctrl Pts',(-8.85141893561129,31.8107119286145,25.8621716271334));
#51376=CARTESIAN_POINT('Ctrl Pts',(-8.79028772894628,31.8331316613072,25.866102885363));
#51377=CARTESIAN_POINT('Ctrl Pts',(-8.7480594590841,31.8495868026729,25.8688823919999));
#51378=CARTESIAN_POINT('Ctrl Pts',(-8.64431589011256,31.8924278146832,25.8758486544061));
#51379=CARTESIAN_POINT('Ctrl Pts',(-8.58322888800214,31.9197982201372,25.8800727175986));
#51380=CARTESIAN_POINT('Ctrl Pts',(-8.27084611525887,32.0710221917836,25.9021821167578));
#51381=CARTESIAN_POINT('Ctrl Pts',(-8.03475747257198,32.2238980568496,25.9205163153555));
#51382=CARTESIAN_POINT('Ctrl Pts',(-7.75821702137178,32.4561133559638,25.9429012316555));
#51383=CARTESIAN_POINT('Ctrl Pts',(-7.69814022995364,32.5103427116435,25.9478387935537));
#51384=CARTESIAN_POINT('Ctrl Pts',(-7.61666981971402,32.5893561432938,25.9546427523748));
#51385=CARTESIAN_POINT('Ctrl Pts',(-7.5936096050873,32.6123752533962,25.9565816731046));
#51386=CARTESIAN_POINT('Ctrl Pts',(-7.55207611508749,32.6550477883394,25.9600990507351));
#51387=CARTESIAN_POINT('Ctrl Pts',(-7.53349887165762,32.6745958485019,25.9616819085535));
#51388=CARTESIAN_POINT('Ctrl Pts',(-7.4961647475416,32.7148317984209,25.9648836561149));
#51389=CARTESIAN_POINT('Ctrl Pts',(-7.47742625546472,32.7355339586796,25.9665017111061));
#51390=CARTESIAN_POINT('Ctrl Pts',(-7.43097144619379,32.7881492519174,25.9705429348604));
#51391=CARTESIAN_POINT('Ctrl Pts',(-7.40359182095877,32.8203541037486,25.9729523388893));
#51392=CARTESIAN_POINT('Ctrl Pts',(-7.2853011931341,32.9648844789227,25.9835000321336));
#51393=CARTESIAN_POINT('Ctrl Pts',(-7.20102027088682,33.0824485999414,25.9913804870382));
#51394=CARTESIAN_POINT('Ctrl Pts',(-7.0544243131109,33.3172941839943,26.0062215062889));
#51395=CARTESIAN_POINT('Ctrl Pts',(-6.99098718101669,33.4335526628433,26.0131925154303));
#51396=CARTESIAN_POINT('Ctrl Pts',(-6.87006374622918,33.6897699226011,26.0282563326832));
#51397=CARTESIAN_POINT('Ctrl Pts',(-6.81482011967634,33.8304597850349,26.0363522214827));
#51398=CARTESIAN_POINT('Ctrl Pts',(-6.75825135522711,34.0086542694434,26.0469047037303));
#51399=CARTESIAN_POINT('Ctrl Pts',(-6.74790804294664,34.0431309808567,26.0489600331863));
#51400=CARTESIAN_POINT('Ctrl Pts',(-6.73319074922079,34.0951850355616,26.0520926126476));
#51401=CARTESIAN_POINT('Ctrl Pts',(-6.72840514697019,34.1126444419263,26.0531482322971));
#51402=CARTESIAN_POINT('Ctrl Pts',(-6.71996337684894,34.1444395539839,26.0550809198817));
#51403=CARTESIAN_POINT('Ctrl Pts',(-6.71626087657103,34.1587620608372,26.0559554100279));
#51404=CARTESIAN_POINT('Ctrl Pts',(-6.70786679777396,34.1921331275623,26.058001848591));
#51405=CARTESIAN_POINT('Ctrl Pts',(-6.70324672044636,34.2111985814637,26.0591776031071));
#51406=CARTESIAN_POINT('Ctrl Pts',(-6.68874025775819,34.2734163312111,26.0630335521217));
#51407=CARTESIAN_POINT('Ctrl Pts',(-6.6795340658647,34.3167207793455,26.0657469992499));
#51408=CARTESIAN_POINT('Ctrl Pts',(-6.65895655273479,34.4237821639482,26.0725080880666));
#51409=CARTESIAN_POINT('Ctrl Pts',(-6.64855941210567,34.4877076438142,26.076590496555));
#51410=CARTESIAN_POINT('Ctrl Pts',(-6.60654240728267,34.8027565724484,26.0968175771035));
#51411=CARTESIAN_POINT('Ctrl Pts',(-6.60128346208668,35.0566153876587,26.1133720840391));
#51412=CARTESIAN_POINT('Ctrl Pts',(-6.63379318920325,35.4121208727315,26.1357404985384));
#51413=CARTESIAN_POINT('Ctrl Pts',(-6.64800037936982,35.5150667980796,26.1421316293458));
#51414=CARTESIAN_POINT('Ctrl Pts',(-6.67408507685431,35.6559314352732,26.1507496210035));
#51415=CARTESIAN_POINT('Ctrl Pts',(-6.6819305894342,35.6945298457562,26.153098003867));
#51416=CARTESIAN_POINT('Ctrl Pts',(-6.69630519163327,35.7594337216339,26.1570262752042));
#51417=CARTESIAN_POINT('Ctrl Pts',(-6.7024801308566,35.785812789735,26.1586170789532));
#51418=CARTESIAN_POINT('Ctrl Pts',(-6.71562102871583,35.8390651589678,26.1618177213325));
#51419=CARTESIAN_POINT('Ctrl Pts',(-6.72260219383413,35.8659325926269,26.1634269411565));
#51420=CARTESIAN_POINT('Ctrl Pts',(-6.74082624985918,35.9326890201371,26.1674129572905));
#51421=CARTESIAN_POINT('Ctrl Pts',(-6.75247223380295,35.9724638608133,26.1697767964274));
#51422=CARTESIAN_POINT('Ctrl Pts',(-6.80488256715277,36.1400061541793,26.1796987879973));
#51423=CARTESIAN_POINT('Ctrl Pts',(-6.85248213256192,36.2655140600372,26.1870379992449));
#51424=CARTESIAN_POINT('Ctrl Pts',(-6.96430389757298,36.5146853749286,26.201723588649));
#51425=CARTESIAN_POINT('Ctrl Pts',(-7.02895615940997,36.6378711519729,26.2090467066191));
#51426=CARTESIAN_POINT('Ctrl Pts',(-7.18221366117368,36.8907801638766,26.2247588664028));
#51427=CARTESIAN_POINT('Ctrl Pts',(-7.27263037198655,37.0190133497008,26.2331464385165));
#51428=CARTESIAN_POINT('Ctrl Pts',(-7.39421745692432,37.1683144089255,26.2440160394932));
#51429=CARTESIAN_POINT('Ctrl Pts',(-7.4172919551955,37.195747931581,26.2460631948066));
#51430=CARTESIAN_POINT('Ctrl Pts',(-7.45264856404106,37.236455324781,26.2491857770703));
#51431=CARTESIAN_POINT('Ctrl Pts',(-7.46460962529923,37.2500060831041,26.2502397784419));
#51432=CARTESIAN_POINT('Ctrl Pts',(-7.48665377646385,37.2745810622936,26.2521794078705));
#51433=CARTESIAN_POINT('Ctrl Pts',(-7.4967021865019,37.2856352025265,26.2530625900414));
#51434=CARTESIAN_POINT('Ctrl Pts',(-7.52019932325557,37.3111433178607,26.2551254537146));
#51435=CARTESIAN_POINT('Ctrl Pts',(-7.53370156374956,37.3255465624326,26.2563089514506));
#51436=CARTESIAN_POINT('Ctrl Pts',(-7.57839552027932,37.3723959333416,26.260217860343));
#51437=CARTESIAN_POINT('Ctrl Pts',(-7.61010650921456,37.4043376239366,26.2629777411421));
#51438=CARTESIAN_POINT('Ctrl Pts',(-7.69006533416638,37.481733210946,26.2698828199203));
#51439=CARTESIAN_POINT('Ctrl Pts',(-7.73902777517446,37.5264207101726,26.2740645587824));
#51440=CARTESIAN_POINT('Ctrl Pts',(-7.99505183746927,37.7466852990106,26.2955733697877));
#51441=CARTESIAN_POINT('Ctrl Pts',(-8.22139470643331,37.8983945138822,26.313337773136));
#51442=CARTESIAN_POINT('Ctrl Pts',(-8.54216823478973,38.0615253975093,26.3357254568321));
#51443=CARTESIAN_POINT('Ctrl Pts',(-8.62246219390565,38.0984839708911,26.3411317933336));
#51444=CARTESIAN_POINT('Ctrl Pts',(-8.73839695488934,38.1464486775011,26.3486612393622));
#51445=CARTESIAN_POINT('Ctrl Pts',(-8.77291099435185,38.1600687112666,26.3508691982686));
#51446=CARTESIAN_POINT('Ctrl Pts',(-8.83288062143889,38.1826033852236,26.354649423319));
#51447=CARTESIAN_POINT('Ctrl Pts',(-8.8582312656269,38.191785733906,26.3562303505633));
#51448=CARTESIAN_POINT('Ctrl Pts',(-8.91054623081791,38.2100318661549,26.3594589051295));
#51449=CARTESIAN_POINT('Ctrl Pts',(-8.93752054364175,38.2190606663059,26.3611052910412));
#51450=CARTESIAN_POINT('Ctrl Pts',(-9.00730300704421,38.2414454142642,26.3653194339785));
#51451=CARTESIAN_POINT('Ctrl Pts',(-9.05026896558488,38.2542936130639,26.3678708067969));
#51452=CARTESIAN_POINT('Ctrl Pts',(-9.28072868080194,38.3182551428436,26.3813462136432));
#51453=CARTESIAN_POINT('Ctrl Pts',(-9.47210794703533,38.3540288363337,26.3917753520011));
#51454=CARTESIAN_POINT('Ctrl Pts',(-9.86973041572493,38.3934567282657,26.412995158163));
#51455=CARTESIAN_POINT('Ctrl Pts',(-10.07534386208,38.3951181844919,26.4237347825941));
#51456=CARTESIAN_POINT('Ctrl Pts',(-10.330320705509,38.3739977296586,26.4379718293838));
#51457=CARTESIAN_POINT('Ctrl Pts',(-10.3807143463015,38.3686834943876,26.4408320903622));
#51458=CARTESIAN_POINT('Ctrl Pts',(-10.4520586662249,38.3595386863507,26.4449709989678));
#51459=CARTESIAN_POINT('Ctrl Pts',(-10.473123681416,38.3566368815892,26.4462041897912));
#51460=CARTESIAN_POINT('Ctrl Pts',(-10.5091094067904,38.3513342163538,26.4483320651295));
#51461=CARTESIAN_POINT('Ctrl Pts',(-10.524043731852,38.3490314389279,26.4492214522734));
#51462=CARTESIAN_POINT('Ctrl Pts',(-10.5558900069774,38.3439027089257,26.4511321462089));
#51463=CARTESIAN_POINT('Ctrl Pts',(-10.5727959563151,38.3410483072142,26.4521548561418));
#51464=CARTESIAN_POINT('Ctrl Pts',(-10.6204532656969,38.3326295037993,26.4550601781411));
#51465=CARTESIAN_POINT('Ctrl Pts',(-10.6511496003247,38.3267680580755,26.4569578319867));
#51466=CARTESIAN_POINT('Ctrl Pts',(-10.7213255682068,38.3123595776737,26.4613499278876));
#51467=CARTESIAN_POINT('Ctrl Pts',(-10.7607419275674,38.3035296281939,26.463856181457));
#51468=CARTESIAN_POINT('Ctrl Pts',(-10.8955562134225,38.2707882572896,26.4725431510995));
#51469=CARTESIAN_POINT('Ctrl Pts',(-10.9900630250911,38.243431824829,26.478830806825));
#51470=CARTESIAN_POINT('Ctrl Pts',(-11.3181996510314,38.1327685586388,26.5011022942915));
#51471=CARTESIAN_POINT('Ctrl Pts',(-11.5437887770378,38.0279755606158,26.5171499893163));
#51472=CARTESIAN_POINT('Ctrl Pts',(-11.8162686423876,37.8629613558772,26.5367632981696));
#51473=CARTESIAN_POINT('Ctrl Pts',(-11.8754458527532,37.8245501338669,26.5410443860709));
#51474=CARTESIAN_POINT('Ctrl Pts',(-11.96085853744,37.7652409659417,26.5472576389746));
#51475=CARTESIAN_POINT('Ctrl Pts',(-11.9880490017677,37.7457576532585,26.5492410059997));
#51476=CARTESIAN_POINT('Ctrl Pts',(-12.0362389623791,37.7101359715483,26.5527671777657));
#51477=CARTESIAN_POINT('Ctrl Pts',(-12.057345830883,37.6941481561563,26.5543155221304));
#51478=CARTESIAN_POINT('Ctrl Pts',(-12.1020838324438,37.6594280899437,26.5576068484293));
#51479=CARTESIAN_POINT('Ctrl Pts',(-12.1256568148076,37.6406244326859,26.5593468731566));
#51480=CARTESIAN_POINT('Ctrl Pts',(-12.1900805896896,37.5878131685234,26.564120984843));
#51481=CARTESIAN_POINT('Ctrl Pts',(-12.2303881051556,37.5531547766629,26.5671291195338));
#51482=CARTESIAN_POINT('Ctrl Pts',(-12.401246492321,37.3991066755484,26.5800027459003));
#51483=CARTESIAN_POINT('Ctrl Pts',(-12.5231588145027,37.2705451671547,26.5894906968189));
#51484=CARTESIAN_POINT('Ctrl Pts',(-12.761688705398,36.9759408040542,26.6096249915204));
#51485=CARTESIAN_POINT('Ctrl Pts',(-12.8745708830499,36.8077874637358,26.6202034269639));
#51486=CARTESIAN_POINT('Ctrl Pts',(-12.9979583017571,36.5829117761982,26.6344372282672));
#51487=CARTESIAN_POINT('Ctrl Pts',(-13.02297040449,36.5346051403349,26.6375009887625));
#51488=CARTESIAN_POINT('Ctrl Pts',(-13.0563437455481,36.4661655087397,26.6418786968314));
#51489=CARTESIAN_POINT('Ctrl Pts',(-13.0656906446513,36.4465196880605,26.643139522253));
#51490=CARTESIAN_POINT('Ctrl Pts',(-13.0812398412988,36.4130098169372,26.6452994370896));
#51491=CARTESIAN_POINT('Ctrl Pts',(-13.087539397919,36.3991912532366,26.6461928208042));
#51492=CARTESIAN_POINT('Ctrl Pts',(-13.1006589900603,36.369892340669,26.648093450725));
#51493=CARTESIAN_POINT('Ctrl Pts',(-13.1074562483596,36.354402759637,26.6491018937862));
#51494=CARTESIAN_POINT('Ctrl Pts',(-13.1260474341217,36.3111604802397,26.6519259102269));
#51495=CARTESIAN_POINT('Ctrl Pts',(-13.1375871096232,36.2833009619197,26.6537552772376));
#51496=CARTESIAN_POINT('Ctrl Pts',(-13.1590745903235,36.2294021419145,26.6573084803199));
#51497=CARTESIAN_POINT('Ctrl Pts',(-13.1690741828736,36.203391072613,26.6590294020481));
#51498=CARTESIAN_POINT('Ctrl Pts',(-13.178750052031,36.1772651227369,26.6607620761902));
#51499=CARTESIAN_POINT('Origin',(-10.,35.,23.));
#51500=CARTESIAN_POINT('',(-13.1787500671536,36.1772650819043,27.9134187897562));
#51501=CARTESIAN_POINT('',(-13.1787501041618,36.1772649819778,27.5681446579994));
#51502=CARTESIAN_POINT('',(-13.1787500671536,36.1772650819043,23.));
#51503=CARTESIAN_POINT('Ctrl Pts',(-13.1787501041618,36.1772649819778,27.5681446579994));
#51504=CARTESIAN_POINT('Ctrl Pts',(-13.1644020558965,36.2160063533906,27.5655716628728));
#51505=CARTESIAN_POINT('Ctrl Pts',(-13.1493430220709,36.2544928168724,27.5630170421175));
#51506=CARTESIAN_POINT('Ctrl Pts',(-13.1093020225905,36.3515541614008,27.556579647575));
#51507=CARTESIAN_POINT('Ctrl Pts',(-13.0833705559431,36.4097108027348,27.5527276911668));
#51508=CARTESIAN_POINT('Ctrl Pts',(-13.0418761164669,36.4961390268219,27.5470088494505));
#51509=CARTESIAN_POINT('Ctrl Pts',(-13.0275237023559,36.5249729946894,27.5451018466481));
#51510=CARTESIAN_POINT('Ctrl Pts',(-13.0018381810593,36.5747827436353,27.5418080492359));
#51511=CARTESIAN_POINT('Ctrl Pts',(-12.9906908813596,36.595851261887,27.5404149881501));
#51512=CARTESIAN_POINT('Ctrl Pts',(-12.9649640131329,36.6432588482702,27.5372799027834));
#51513=CARTESIAN_POINT('Ctrl Pts',(-12.9502538263333,36.669524988143,27.5355425833204));
#51514=CARTESIAN_POINT('Ctrl Pts',(-12.9094257063638,36.7402014748802,27.5308644442906));
#51515=CARTESIAN_POINT('Ctrl Pts',(-12.8826415826952,36.7842188798417,27.5279473063303));
#51516=CARTESIAN_POINT('Ctrl Pts',(-12.7245416510446,37.0311827472875,27.5115250320381));
#51517=CARTESIAN_POINT('Ctrl Pts',(-12.5728206912721,37.2202331862985,27.4987999017403));
#51518=CARTESIAN_POINT('Ctrl Pts',(-12.2768441758102,37.5175365248139,27.4765345234232));
#51519=CARTESIAN_POINT('Ctrl Pts',(-12.141715186843,37.6334485909179,27.4670550970074));
#51520=CARTESIAN_POINT('Ctrl Pts',(-11.9741515042845,37.7557236460611,27.4552633861233));
#51521=CARTESIAN_POINT('Ctrl Pts',(-11.949934296921,37.7729123834219,27.4535581017219));
#51522=CARTESIAN_POINT('Ctrl Pts',(-11.9116532624196,37.7993338030989,27.4508555624415));
#51523=CARTESIAN_POINT('Ctrl Pts',(-11.8977406619426,37.808784130316,27.4498719623093));
#51524=CARTESIAN_POINT('Ctrl Pts',(-11.871101514872,37.826590873707,27.4479847820681));
#51525=CARTESIAN_POINT('Ctrl Pts',(-11.8583881346318,37.8349656704456,27.4470823941857));
#51526=CARTESIAN_POINT('Ctrl Pts',(-11.8301034720192,37.8533258692491,27.4450715141246));
#51527=CARTESIAN_POINT('Ctrl Pts',(-11.8145060099757,37.8632700083236,27.4439605018109));
#51528=CARTESIAN_POINT('Ctrl Pts',(-11.7600716163884,37.8973511802993,27.4400779309422));
#51529=CARTESIAN_POINT('Ctrl Pts',(-11.7208298036602,37.920828703608,27.4372699301773));
#51530=CARTESIAN_POINT('Ctrl Pts',(-11.4992048062422,38.0474056708746,27.4214112109975));
#51531=CARTESIAN_POINT('Ctrl Pts',(-11.3080503659179,38.1342134899517,27.4077641496928));
#51532=CARTESIAN_POINT('Ctrl Pts',(-11.0645838020527,38.2186004079409,27.3912144752835));
#51533=CARTESIAN_POINT('Ctrl Pts',(-11.0187199333602,38.2334095201176,27.3881296922592));
#51534=CARTESIAN_POINT('Ctrl Pts',(-10.8748282411207,38.2765054320731,27.3785672738993));
#51535=CARTESIAN_POINT('Ctrl Pts',(-10.7758241659961,38.3013500076338,27.3721550159289));
#51536=CARTESIAN_POINT('Ctrl Pts',(-10.6049382725524,38.3361190669073,27.3614064551439));
#51537=CARTESIAN_POINT('Ctrl Pts',(-10.5335856677132,38.3482724294034,27.357010886608));
#51538=CARTESIAN_POINT('Ctrl Pts',(-10.4284455187394,38.3627339321608,27.3506668669819));
#51539=CARTESIAN_POINT('Ctrl Pts',(-10.3949288408948,38.3668347739969,27.3486640528557));
#51540=CARTESIAN_POINT('Ctrl Pts',(-10.3350003600284,38.3732599071995,27.3451165732695));
#51541=CARTESIAN_POINT('Ctrl Pts',(-10.308612400127,38.3757763682488,27.3435661023063));
#51542=CARTESIAN_POINT('Ctrl Pts',(-10.2523492683192,38.3804765962723,27.3402838494633));
#51543=CARTESIAN_POINT('Ctrl Pts',(-10.2224690707656,38.3825744288559,27.3385548398914));
#51544=CARTESIAN_POINT('Ctrl Pts',(-10.1418306003378,38.3871627334773,27.3339243424286));
#51545=CARTESIAN_POINT('Ctrl Pts',(-10.0910367157713,38.3889083780982,27.3310456980157));
#51546=CARTESIAN_POINT('Ctrl Pts',(-9.79136243130594,38.3924643930525,27.3142523352531));
#51547=CARTESIAN_POINT('Ctrl Pts',(-9.54293663192563,38.3680036328702,27.3011748964854));
#51548=CARTESIAN_POINT('Ctrl Pts',(-9.18283425269056,38.2919359188974,27.281630270654));
#51549=CARTESIAN_POINT('Ctrl Pts',(-9.06764192911394,38.2611818699293,27.2752712826042));
#51550=CARTESIAN_POINT('Ctrl Pts',(-8.89128049273529,38.2039877261241,27.2650607504209));
#51551=CARTESIAN_POINT('Ctrl Pts',(-8.82886298743505,38.1817028847309,27.2613505344467));
#51552=CARTESIAN_POINT('Ctrl Pts',(-8.74593118652872,38.1493229430602,27.2562405951232));
#51553=CARTESIAN_POINT('Ctrl Pts',(-8.72480409780817,38.1408277474417,27.254922785503));
#51554=CARTESIAN_POINT('Ctrl Pts',(-8.68956942559027,38.1262457988304,27.2526955086954));
#51555=CARTESIAN_POINT('Ctrl Pts',(-8.67541431211795,38.1202746407128,27.2517926594589));
#51556=CARTESIAN_POINT('Ctrl Pts',(-8.64612540167611,38.1076842607834,27.2499068766235));
#51557=CARTESIAN_POINT('Ctrl Pts',(-8.63099872219983,38.1010503654269,27.2489231695905));
#51558=CARTESIAN_POINT('Ctrl Pts',(-8.59010257490957,38.082757580974,27.2462382656024));
#51559=CARTESIAN_POINT('Ctrl Pts',(-8.56443012585635,38.0708865291867,27.2445253039196));
#51560=CARTESIAN_POINT('Ctrl Pts',(-8.40825395622129,37.9962836885627,27.2339485776098));
#51561=CARTESIAN_POINT('Ctrl Pts',(-8.28174240922741,37.925569108145,27.2247143727789));
#51562=CARTESIAN_POINT('Ctrl Pts',(-7.94957210869555,37.7109064032872,27.199276412934));
#51563=CARTESIAN_POINT('Ctrl Pts',(-7.754709114995,37.5518560222649,27.18305415216));
#51564=CARTESIAN_POINT('Ctrl Pts',(-7.53140634715714,37.3240277613018,27.1634394493117));
#51565=CARTESIAN_POINT('Ctrl Pts',(-7.48513013212041,37.2738711930842,27.1593025439933));
#51566=CARTESIAN_POINT('Ctrl Pts',(-7.41873522160689,37.1974004792366,27.1532546627517));
#51567=CARTESIAN_POINT('Ctrl Pts',(-7.39743910987483,37.172135735042,27.1512963435665));
#51568=CARTESIAN_POINT('Ctrl Pts',(-7.35976917236088,37.1260963179081,27.1477973367732));
#51569=CARTESIAN_POINT('Ctrl Pts',(-7.34326287312982,37.1054339870156,27.1462514517745));
#51570=CARTESIAN_POINT('Ctrl Pts',(-7.30828608078966,37.0605842001141,27.1429470045155));
#51571=CARTESIAN_POINT('Ctrl Pts',(-7.28989601099042,37.0363367904838,27.1411916524712));
#51572=CARTESIAN_POINT('Ctrl Pts',(-7.24034935172679,36.9691489487084,27.1364096485186));
#51573=CARTESIAN_POINT('Ctrl Pts',(-7.20986971395812,36.925718747619,27.1334085524622));
#51574=CARTESIAN_POINT('Ctrl Pts',(-7.07251277690084,36.7198880915861,27.11956664319));
#51575=CARTESIAN_POINT('Ctrl Pts',(-6.97871098069999,36.5491993506769,27.1091945254157));
#51576=CARTESIAN_POINT('Ctrl Pts',(-6.83692802185636,36.2287087902784,27.0906067793392));
#51577=CARTESIAN_POINT('Ctrl Pts',(-6.78373414418195,36.0818402906496,27.0823834686507));
#51578=CARTESIAN_POINT('Ctrl Pts',(-6.71963273670488,35.857642677158,27.0696259765021));
#51579=CARTESIAN_POINT('Ctrl Pts',(-6.70096005667042,35.7827477730105,27.0653298627126));
#51580=CARTESIAN_POINT('Ctrl Pts',(-6.6798598236318,35.6838484005066,27.0595364743564));
#51581=CARTESIAN_POINT('Ctrl Pts',(-6.67510809459823,35.6603583672449,27.0581516520363));
#51582=CARTESIAN_POINT('Ctrl Pts',(-6.66767612221192,35.6215028990293,27.055843560445));
#51583=CARTESIAN_POINT('Ctrl Pts',(-6.66485204885391,35.6061653332914,27.0549280146077));
#51584=CARTESIAN_POINT('Ctrl Pts',(-6.6596654951604,35.5768631031551,27.0531694597432));
#51585=CARTESIAN_POINT('Ctrl Pts',(-6.65728451619725,35.5629021427547,27.0523275780995));
#51586=CARTESIAN_POINT('Ctrl Pts',(-6.65101480283981,35.5246962456425,27.0500134413177));
#51587=CARTESIAN_POINT('Ctrl Pts',(-6.64730199089043,35.5004238046987,27.048532027761));
#51588=CARTESIAN_POINT('Ctrl Pts',(-6.63316837427889,35.4007953650909,27.0424113529431));
#51589=CARTESIAN_POINT('Ctrl Pts',(-6.62502265743839,35.3251436393476,27.0376703232025));
#51590=CARTESIAN_POINT('Ctrl Pts',(-6.60425543679456,35.0435211784401,27.0198233656105));
#51591=CARTESIAN_POINT('Ctrl Pts',(-6.60789997071299,34.8368009088116,27.0063621847826));
#51592=CARTESIAN_POINT('Ctrl Pts',(-6.64805835080242,34.4693865817426,26.9827704669739));
#51593=CARTESIAN_POINT('Ctrl Pts',(-6.67750363943818,34.3085569921706,26.9725548286115));
#51594=CARTESIAN_POINT('Ctrl Pts',(-6.72933214669909,34.108356458548,26.9600657074071));
#51595=CARTESIAN_POINT('Ctrl Pts',(-6.74104113193493,34.0664670484797,26.9574644075734));
#51596=CARTESIAN_POINT('Ctrl Pts',(-6.7616570037712,33.9978357704238,26.9532204217887));
#51597=CARTESIAN_POINT('Ctrl Pts',(-6.77009672206383,33.970959966283,26.9515630685122));
#51598=CARTESIAN_POINT('Ctrl Pts',(-6.78722021490882,33.9187184810189,26.9483494745553));
#51599=CARTESIAN_POINT('Ctrl Pts',(-6.79587182008135,33.8933445261088,26.9467923357216));
#51600=CARTESIAN_POINT('Ctrl Pts',(-6.81743898512195,33.8324651265856,26.9430639190352));
#51601=CARTESIAN_POINT('Ctrl Pts',(-6.83064903740939,33.797067361924,26.9409023837029));
#51602=CARTESIAN_POINT('Ctrl Pts',(-6.87815973904472,33.6759769178717,26.9335228035249));
#51603=CARTESIAN_POINT('Ctrl Pts',(-6.91536770855719,33.5914655413139,26.9283994021722));
#51604=CARTESIAN_POINT('Ctrl Pts',(-7.07326268086494,33.2692001819934,26.908798880377));
#51605=CARTESIAN_POINT('Ctrl Pts',(-7.21836034386465,33.044512635551,26.8950687975203));
#51606=CARTESIAN_POINT('Ctrl Pts',(-7.43027435690701,32.7883814668859,26.8770628614091));
#51607=CARTESIAN_POINT('Ctrl Pts',(-7.47374557193833,32.738853362478,26.8734501106726));
#51608=CARTESIAN_POINT('Ctrl Pts',(-7.54916476029074,32.6578171542213,26.8672543205111));
#51609=CARTESIAN_POINT('Ctrl Pts',(-7.58034570596083,32.6256187003126,26.8647119332045));
#51610=CARTESIAN_POINT('Ctrl Pts',(-7.62614447078359,32.5801645702481,26.8609881662972));
#51611=CARTESIAN_POINT('Ctrl Pts',(-7.64025517303491,32.5664022740476,26.8598422467316));
#51612=CARTESIAN_POINT('Ctrl Pts',(-7.66526850837877,32.5424286300922,26.8578116110175));
#51613=CARTESIAN_POINT('Ctrl Pts',(-7.67611985515543,32.5321650711385,26.8569308223012));
#51614=CARTESIAN_POINT('Ctrl Pts',(-7.7002698022037,32.509623794949,26.8549705735495));
#51615=CARTESIAN_POINT('Ctrl Pts',(-7.7135989559906,32.4973808002714,26.8538887874433));
#51616=CARTESIAN_POINT('Ctrl Pts',(-7.75370965331564,32.4611265245754,26.8506355712557));
#51617=CARTESIAN_POINT('Ctrl Pts',(-7.78077521148381,32.4374348864085,26.8484432202856));
#51618=CARTESIAN_POINT('Ctrl Pts',(-7.92315383763938,32.3167521704878,26.8369476919827));
#51619=CARTESIAN_POINT('Ctrl Pts',(-8.04445579568718,32.2271046456035,26.8272858989504));
#51620=CARTESIAN_POINT('Ctrl Pts',(-8.28214658929394,32.0748139401915,26.8090999242139));
#51621=CARTESIAN_POINT('Ctrl Pts',(-8.39703335282622,32.0103120277561,26.8006003611032));
#51622=CARTESIAN_POINT('Ctrl Pts',(-8.64608555148325,31.8889779129413,26.7829989476883));
#51623=CARTESIAN_POINT('Ctrl Pts',(-8.78076070155903,31.8337708493311,26.7739469410946));
#51624=CARTESIAN_POINT('Ctrl Pts',(-8.95869955993819,31.7738737774273,26.7626203361656));
#51625=CARTESIAN_POINT('Ctrl Pts',(-8.99906970610587,31.7611212124363,26.7600904282288));
#51626=CARTESIAN_POINT('Ctrl Pts',(-9.066459874619,31.7412136844828,26.755931283695));
#51627=CARTESIAN_POINT('Ctrl Pts',(-9.09334757402283,31.7336309357148,26.754288533611));
#51628=CARTESIAN_POINT('Ctrl Pts',(-9.14635961059223,31.7193857579464,26.7510813700159));
#51629=CARTESIAN_POINT('Ctrl Pts',(-9.17247571667746,31.7127009047677,26.7495163459103));
#51630=CARTESIAN_POINT('Ctrl Pts',(-9.23028925957285,31.6986352157932,26.7460834597176));
#51631=CARTESIAN_POINT('Ctrl Pts',(-9.2620190447602,31.6913978365864,26.74422021691));
#51632=CARTESIAN_POINT('Ctrl Pts',(-9.37273548814627,31.6678160766798,26.7377863170969));
#51633=CARTESIAN_POINT('Ctrl Pts',(-9.45220018262722,31.6538339571314,26.7332882871803));
#51634=CARTESIAN_POINT('Ctrl Pts',(-9.80991657497855,31.6039789706991,26.7134478247527));
#51635=CARTESIAN_POINT('Ctrl Pts',(-10.0914517082179,31.5998944838945,26.6990262943814));
#51636=CARTESIAN_POINT('Ctrl Pts',(-10.4368149127558,31.6378459149163,26.6802201487411));
#51637=CARTESIAN_POINT('Ctrl Pts',(-10.5031297741189,31.6471285602743,26.6765517865612));
#51638=CARTESIAN_POINT('Ctrl Pts',(-10.6138089800698,31.6659786474563,26.6702708847003));
#51639=CARTESIAN_POINT('Ctrl Pts',(-10.6583358528913,31.6744845002267,26.6677004662677));
#51640=CARTESIAN_POINT('Ctrl Pts',(-10.7220433493207,31.6879839402809,26.663942941532));
#51641=CARTESIAN_POINT('Ctrl Pts',(-10.7413733646851,31.6922571939079,26.6627921893773));
#51642=CARTESIAN_POINT('Ctrl Pts',(-10.7752265327717,31.7000526992554,26.6607563750533));
#51643=CARTESIAN_POINT('Ctrl Pts',(-10.789765552222,31.7035020513524,26.6598753163988));
#51644=CARTESIAN_POINT('Ctrl Pts',(-10.8218010626107,31.7113265117992,26.6579187244417));
#51645=CARTESIAN_POINT('Ctrl Pts',(-10.8392855209772,31.7157451255028,26.6568409254977));
#51646=CARTESIAN_POINT('Ctrl Pts',(-10.8912166009179,31.7293107361177,26.6536118402494));
#51647=CARTESIAN_POINT('Ctrl Pts',(-10.9255540988702,31.7388614436303,26.6514400695276));
#51648=CARTESIAN_POINT('Ctrl Pts',(-11.0983743354471,31.7898792294697,26.6403451902187));
#51649=CARTESIAN_POINT('Ctrl Pts',(-11.2342449603887,31.8396306714422,26.6310912161772));
#51650=CARTESIAN_POINT('Ctrl Pts',(-11.479837990415,31.9478173169895,26.613810137012));
#51651=CARTESIAN_POINT('Ctrl Pts',(-11.5903452339949,32.0039120087511,26.6058089420885));
#51652=CARTESIAN_POINT('Ctrl Pts',(-11.7889214257883,32.1188003005747,26.5911836653386));
#51653=CARTESIAN_POINT('Ctrl Pts',(-11.8777914198948,32.1759153843919,26.5845374430253));
#51654=CARTESIAN_POINT('Ctrl Pts',(-12.0242455723205,32.2800139207113,26.5734515681327));
#51655=CARTESIAN_POINT('Ctrl Pts',(-12.0832144217084,32.32490872108,26.5689474367798));
#51656=CARTESIAN_POINT('Ctrl Pts',(-12.1670755064744,32.39321102412,26.562479842034));
#51657=CARTESIAN_POINT('Ctrl Pts',(-12.1931580262123,32.4151164408063,26.5604589388141));
#51658=CARTESIAN_POINT('Ctrl Pts',(-12.238967626392,32.454782287719,26.5568914823136));
#51659=CARTESIAN_POINT('Ctrl Pts',(-12.2588242792995,32.4723880500339,26.5553388759454));
#51660=CARTESIAN_POINT('Ctrl Pts',(-12.3005195117641,32.5102406322092,26.5520642595093));
#51661=CARTESIAN_POINT('Ctrl Pts',(-12.3223022462479,32.5305457906186,26.5503448579249));
#51662=CARTESIAN_POINT('Ctrl Pts',(-12.3808844902312,32.5866150286782,26.5456944654271));
#51663=CARTESIAN_POINT('Ctrl Pts',(-12.4171447564691,32.6229325651388,26.542787159267));
#51664=CARTESIAN_POINT('Ctrl Pts',(-12.6250174268864,32.840810802125,26.525911791026));
#51665=CARTESIAN_POINT('Ctrl Pts',(-12.7769577450057,33.0400685591439,26.5127880365558));
#51666=CARTESIAN_POINT('Ctrl Pts',(-12.9667207683926,33.3559064274085,26.4932199779168));
#51667=CARTESIAN_POINT('Ctrl Pts',(-13.0224293008694,33.4607164814866,26.4868879854454));
#51668=CARTESIAN_POINT('Ctrl Pts',(-13.1004418297251,33.6281278219799,26.4767152722671));
#51669=CARTESIAN_POINT('Ctrl Pts',(-13.1265970956252,33.6888317132664,26.4730146313256));
#51670=CARTESIAN_POINT('Ctrl Pts',(-13.159347324168,33.7714044156547,26.4679159140815));
#51671=CARTESIAN_POINT('Ctrl Pts',(-13.1675215079674,33.7926350755546,26.4665992928365));
#51672=CARTESIAN_POINT('Ctrl Pts',(-13.1808552114007,33.8283340536788,26.4643734342631));
#51673=CARTESIAN_POINT('Ctrl Pts',(-13.1861313654338,33.8427585036431,26.4634707955934));
#51674=CARTESIAN_POINT('Ctrl Pts',(-13.1968803537048,33.8727759126454,26.4615847677718));
#51675=CARTESIAN_POINT('Ctrl Pts',(-13.2023374458677,33.8883737154046,26.4606005970039));
#51676=CARTESIAN_POINT('Ctrl Pts',(-13.2168363153487,33.9308081847432,26.4579131069085));
#51677=CARTESIAN_POINT('Ctrl Pts',(-13.2256559906663,33.957718687971,26.456197986378));
#51678=CARTESIAN_POINT('Ctrl Pts',(-13.2797922067914,34.1301702577487,26.4451521429408));
#51679=CARTESIAN_POINT('Ctrl Pts',(-13.3155812426581,34.2785062403407,26.4354107616784));
#51680=CARTESIAN_POINT('Ctrl Pts',(-13.3733889843741,34.6166149298027,26.4133312549766));
#51681=CARTESIAN_POINT('Ctrl Pts',(-13.3896100389236,34.8068893592864,26.4010053753037));
#51682=CARTESIAN_POINT('Ctrl Pts',(-13.3898250631782,35.1016684315265,26.3825327747888));
#51683=CARTESIAN_POINT('Ctrl Pts',(-13.3851018672738,35.2057648191004,26.3761237399455));
#51684=CARTESIAN_POINT('Ctrl Pts',(-13.3719934711717,35.3487387793943,26.3674865606486));
#51685=CARTESIAN_POINT('Ctrl Pts',(-13.3677102660867,35.3879258514924,26.3651361613135));
#51686=CARTESIAN_POINT('Ctrl Pts',(-13.3596408924418,35.4514698737382,26.3613509560353));
#51687=CARTESIAN_POINT('Ctrl Pts',(-13.3562709876614,35.4758750658002,26.3599034550229));
#51688=CARTESIAN_POINT('Ctrl Pts',(-13.3486063500042,35.5272436884008,26.3568692292508));
#51689=CARTESIAN_POINT('Ctrl Pts',(-13.3442513026037,35.5541964300205,26.3552844929365));
#51690=CARTESIAN_POINT('Ctrl Pts',(-13.3328778060978,35.6195603568914,26.3514575704157));
#51691=CARTESIAN_POINT('Ctrl Pts',(-13.3255203152845,35.6579090489232,26.3492260812221));
#51692=CARTESIAN_POINT('Ctrl Pts',(-13.2949466182526,35.8036135565192,26.3407912840509));
#51693=CARTESIAN_POINT('Ctrl Pts',(-13.2671795835836,35.9099498061325,26.3347291378396));
#51694=CARTESIAN_POINT('Ctrl Pts',(-13.2171490333955,36.069410151205,26.3256643244751));
#51695=CARTESIAN_POINT('Ctrl Pts',(-13.1986266460729,36.1235960409069,26.3225880933694));
#51696=CARTESIAN_POINT('Ctrl Pts',(-13.1787501361565,36.1772648955886,26.3195304627418));
#51697=CARTESIAN_POINT('',(-13.3897497681227,35.0012537990022,26.7339821967504));
#51698=CARTESIAN_POINT('Ctrl Pts',(-13.178750052031,36.1772651227369,26.6607620761902));
#51699=CARTESIAN_POINT('Ctrl Pts',(-13.2278569142916,36.0446709959331,26.6695557244977));
#51700=CARTESIAN_POINT('Ctrl Pts',(-13.2686255387752,35.9091174585747,26.6786460656091));
#51701=CARTESIAN_POINT('Ctrl Pts',(-13.3456145540687,35.5796817978736,26.7004496954122));
#51702=CARTESIAN_POINT('Ctrl Pts',(-13.3736350392072,35.3844071259962,26.7131248457753));
#51703=CARTESIAN_POINT('Ctrl Pts',(-13.3879876626213,35.125729936053,26.7292118644511));
#51704=CARTESIAN_POINT('Ctrl Pts',(-13.3897235886384,35.0635844579724,26.7330266693701));
#51705=CARTESIAN_POINT('Ctrl Pts',(-13.3897497009126,35.0014239601829,26.7367916060834));
#51706=CARTESIAN_POINT('Ctrl Pts',(-13.3897497681227,35.0012537990022,26.7339821967504));
#51707=CARTESIAN_POINT('Ctrl Pts',(-13.3897890807757,34.8949687755281,26.7401898647473));
#51708=CARTESIAN_POINT('Ctrl Pts',(-13.3848252223009,34.7887128798793,26.7463975327442));
#51709=CARTESIAN_POINT('Ctrl Pts',(-13.3748927040089,34.6829758701176,26.7526052007411));
#51710=CARTESIAN_POINT('Ctrl Pts',(-13.3649548482759,34.5771820404203,26.7588162045549));
#51711=CARTESIAN_POINT('Ctrl Pts',(-13.3500430541169,34.4719080519769,26.7650272083686));
#51712=CARTESIAN_POINT('Ctrl Pts',(-13.3302435188436,34.3676368387545,26.7712382121823));
#51713=CARTESIAN_POINT('Ctrl Pts',(-13.3101893565392,34.2620246713595,26.7775290910759));
#51714=CARTESIAN_POINT('Ctrl Pts',(-13.2851209399016,34.1574416688483,26.7838199699694));
#51715=CARTESIAN_POINT('Ctrl Pts',(-13.255180393362,34.0543755136568,26.790110848863));
#51716=CARTESIAN_POINT('Ctrl Pts',(-13.2255498660534,33.9523765564249,26.7963365888842));
#51717=CARTESIAN_POINT('Ctrl Pts',(-13.1911478357508,33.851863538394,26.8025623289055));
#51718=CARTESIAN_POINT('Ctrl Pts',(-13.1521609227585,33.7532896970288,26.8087880689268));
#51719=CARTESIAN_POINT('Ctrl Pts',(-13.1125621394815,33.6531688133423,26.8151115172565));
#51720=CARTESIAN_POINT('Ctrl Pts',(-13.0682335274196,33.555048882714,26.8214349655862));
#51721=CARTESIAN_POINT('Ctrl Pts',(-13.0194189846875,33.4593786781273,26.8277584139158));
#51722=CARTESIAN_POINT('Ctrl Pts',(-12.9706044419554,33.3637084735407,26.8340818622455));
#51723=CARTESIAN_POINT('Ctrl Pts',(-12.917304237297,33.270488333665,26.8404053105752));
#51724=CARTESIAN_POINT('Ctrl Pts',(-12.8598073032452,33.1801353756927,26.8467287589049));
#51725=CARTESIAN_POINT('Ctrl Pts',(-12.8043271157467,33.0929516130794,26.8528304077103));
#51726=CARTESIAN_POINT('Ctrl Pts',(-12.7447627250487,33.0081598725026,26.8589320565156));
#51727=CARTESIAN_POINT('Ctrl Pts',(-12.6813468174437,32.9261667600589,26.865033705321));
#51728=CARTESIAN_POINT('Ctrl Pts',(-12.6180143250755,32.8442814987073,26.8711273282146));
#51729=CARTESIAN_POINT('Ctrl Pts',(-12.5508406470161,32.7651878825775,26.8772209511081));
#51730=CARTESIAN_POINT('Ctrl Pts',(-12.4801026278488,32.6892650481206,26.8833145740017));
#51731=CARTESIAN_POINT('Ctrl Pts',(-12.4094374149311,32.6134203563214,26.8894019251077));
#51732=CARTESIAN_POINT('Ctrl Pts',(-12.3352154458944,32.5407402680369,26.8954892762138));
#51733=CARTESIAN_POINT('Ctrl Pts',(-12.2577542980673,32.4715715173139,26.9015766273198));
#51734=CARTESIAN_POINT('Ctrl Pts',(-12.1803482539564,32.4024519713253,26.9076596480527));
#51735=CARTESIAN_POINT('Ctrl Pts',(-12.0997079314063,32.3368390797548,26.9137426687857));
#51736=CARTESIAN_POINT('Ctrl Pts',(-12.0161876933347,32.2750427071703,26.9198256895186));
#51737=CARTESIAN_POINT('Ctrl Pts',(-11.9326983778282,32.2132692140986,26.9259064580717));
#51738=CARTESIAN_POINT('Ctrl Pts',(-11.8463316094188,32.1553096858483,26.9319872266247));
#51739=CARTESIAN_POINT('Ctrl Pts',(-11.7574741265875,32.101433154665,26.9380679951777));
#51740=CARTESIAN_POINT('Ctrl Pts',(-11.6686265213304,32.0475626125038,26.9441480877804));
#51741=CARTESIAN_POINT('Ctrl Pts',(-11.5772891179794,31.9977743866539,26.9502281803831));
#51742=CARTESIAN_POINT('Ctrl Pts',(-11.4838760926028,31.9522931892484,26.9563082729858));
#51743=CARTESIAN_POINT('Ctrl Pts',(-11.3904492502357,31.9068052645875,26.9623892649126));
#51744=CARTESIAN_POINT('Ctrl Pts',(-11.2949465605175,31.865625821324,26.9684702568394));
#51745=CARTESIAN_POINT('Ctrl Pts',(-11.1978043188601,31.8289323759623,26.9745512487661));
#51746=CARTESIAN_POINT('Ctrl Pts',(-11.1005612478569,31.7922008444289,26.9806385524933));
#51747=CARTESIAN_POINT('Ctrl Pts',(-11.0016756272462,31.759964761198,26.9867258562204));
#51748=CARTESIAN_POINT('Ctrl Pts',(-10.9016011111557,31.7323524518604,26.9928131599476));
#51749=CARTESIAN_POINT('Ctrl Pts',(-10.8014728282463,31.704725307317,26.9989037341872));
#51750=CARTESIAN_POINT('Ctrl Pts',(-10.7001547947215,31.6817269797083,27.0049943084269));
#51751=CARTESIAN_POINT('Ctrl Pts',(-10.598111160826,31.6634346849199,27.0110848826666));
#51752=CARTESIAN_POINT('Ctrl Pts',(-10.4959009341694,31.64511252679,27.0171854001583));
#51753=CARTESIAN_POINT('Ctrl Pts',(-10.3929631650667,31.6315118056855,27.0232859176501));
#51754=CARTESIAN_POINT('Ctrl Pts',(-10.2897676713137,31.6226578853836,27.0293864351419));
#51755=CARTESIAN_POINT('Ctrl Pts',(-10.208448759635,31.6156809221767,27.034193693919));
#51756=CARTESIAN_POINT('Ctrl Pts',(-10.1269699497371,31.6116504791971,27.0390009526962));
#51757=CARTESIAN_POINT('Ctrl Pts',(-10.0455599792816,31.6105561885779,27.0438082114734));
#51758=CARTESIAN_POINT('Ctrl Pts',(-9.94222969237447,31.6091672510434,27.0499098649429));
#51759=CARTESIAN_POINT('Ctrl Pts',(-9.83866121416243,31.6125054504178,27.0560115184124));
#51760=CARTESIAN_POINT('Ctrl Pts',(-9.73532216908929,31.6205990607322,27.0621131718819));
#51761=CARTESIAN_POINT('Ctrl Pts',(-9.63211905207604,31.6286820250342,27.0682067994797));
#51762=CARTESIAN_POINT('Ctrl Pts',(-9.52914519108828,31.6415079318196,27.0743004270775));
#51763=CARTESIAN_POINT('Ctrl Pts',(-9.42686944164642,31.6590530645367,27.0803940546753));
#51764=CARTESIAN_POINT('Ctrl Pts',(-9.32469895763911,31.6765801392486,27.0864814105189));
#51765=CARTESIAN_POINT('Ctrl Pts',(-9.2232255757606,31.6988167094296,27.0925687663625));
#51766=CARTESIAN_POINT('Ctrl Pts',(-9.1229133792418,31.7256872290224,27.0986561222062));
#51767=CARTESIAN_POINT('Ctrl Pts',(-9.0226725414854,31.7525386338207,27.1047391477072));
#51768=CARTESIAN_POINT('Ctrl Pts',(-8.92359165844345,31.7840173224317,27.1108221732082));
#51769=CARTESIAN_POINT('Ctrl Pts',(-8.82612414125007,31.8199967718972,27.1169051987092));
#51770=CARTESIAN_POINT('Ctrl Pts',(-8.72869271016785,31.8559629004282,27.1229859720472));
#51771=CARTESIAN_POINT('Ctrl Pts',(-8.63287385862828,31.8964263300735,27.1290667453853));
#51772=CARTESIAN_POINT('Ctrl Pts',(-8.53910459385463,31.9412110771086,27.1351475187233));
#51773=CARTESIAN_POINT('Ctrl Pts',(-8.4453457524782,31.9859908458684,27.1412276161222));
#51774=CARTESIAN_POINT('Ctrl Pts',(-8.35363643080694,32.0350907924778,27.1473077135211));
#51775=CARTESIAN_POINT('Ctrl Pts',(-8.26439160825895,32.0882876905474,27.15338781092));
#51776=CARTESIAN_POINT('Ctrl Pts',(-8.17513358518265,32.1414924571648,27.1594688076484));
#51777=CARTESIAN_POINT('Ctrl Pts',(-8.08834115292697,32.1987951601621,27.1655498043767));
#51778=CARTESIAN_POINT('Ctrl Pts',(-8.00440194284902,32.2599282022554,27.1716308011051));
#51779=CARTESIAN_POINT('Ctrl Pts',(-7.920375607953,32.3211246974736,27.1777181096123));
#51780=CARTESIAN_POINT('Ctrl Pts',(-7.8392087560508,32.3861592192928,27.1838054181196));
#51781=CARTESIAN_POINT('Ctrl Pts',(-7.76125739204368,32.4547226874423,27.1898927266268));
#51782=CARTESIAN_POINT('Ctrl Pts',(-7.68326414736911,32.5233229924559,27.1959833056418));
#51783=CARTESIAN_POINT('Ctrl Pts',(-7.60849013968793,32.5954557234185,27.2020738846569));
#51784=CARTESIAN_POINT('Ctrl Pts',(-7.53725438080866,32.6707750049311,27.2081644636719));
#51785=CARTESIAN_POINT('Ctrl Pts',(-7.46590232575739,32.7462172491839,27.2142649858817));
#51786=CARTESIAN_POINT('Ctrl Pts',(-7.39810033851056,32.8248561122507,27.2203655080915));
#51787=CARTESIAN_POINT('Ctrl Pts',(-7.33412717001587,32.906312555119,27.2264660303013));
#51788=CARTESIAN_POINT('Ctrl Pts',(-7.28371631591037,32.9705002287016,27.2312732415481));
#51789=CARTESIAN_POINT('Ctrl Pts',(-7.23568214943518,33.0364367761876,27.236080452795));
#51790=CARTESIAN_POINT('Ctrl Pts',(-7.19014138143131,33.1039252108223,27.2408876640418));
#51791=CARTESIAN_POINT('Ctrl Pts',(-7.13233799108828,33.1895860483931,27.2469892982554));
#51792=CARTESIAN_POINT('Ctrl Pts',(-7.07835764615036,33.278037335163,27.253090932469));
#51793=CARTESIAN_POINT('Ctrl Pts',(-7.0284803286951,33.3689034652884,27.2591925666825));
#51794=CARTESIAN_POINT('Ctrl Pts',(-6.97866861832966,33.4596500729001,27.265286174994));
#51795=CARTESIAN_POINT('Ctrl Pts',(-6.93294941010423,33.5528048372231,27.2713797833055));
#51796=CARTESIAN_POINT('Ctrl Pts',(-6.89155987761914,33.6479626232708,27.277473391617));
#51797=CARTESIAN_POINT('Ctrl Pts',(-6.85021294471852,33.7430224695278,27.2835607281693));
#51798=CARTESIAN_POINT('Ctrl Pts',(-6.81318699597916,33.8400808478651,27.2896480647216));
#51799=CARTESIAN_POINT('Ctrl Pts',(-6.78067324037895,33.9387082035143,27.2957354012739));
#51800=CARTESIAN_POINT('Ctrl Pts',(-6.74818261367836,34.0372653998673,27.3018184075545));
#51801=CARTESIAN_POINT('Ctrl Pts',(-6.7201979307338,34.1373889490011,27.3079014138351));
#51802=CARTESIAN_POINT('Ctrl Pts',(-6.69686191490677,34.2386302781784,27.3139844201157));
#51803=CARTESIAN_POINT('Ctrl Pts',(-6.67353453877915,34.3398341247513,27.3200651742832));
#51804=CARTESIAN_POINT('Ctrl Pts',(-6.65485250520525,34.4421545125211,27.3261459284507));
#51805=CARTESIAN_POINT('Ctrl Pts',(-6.64090817798173,34.5451294758395,27.3322266826183));
#51806=CARTESIAN_POINT('Ctrl Pts',(-6.62696540064945,34.648092993644,27.338306760919));
#51807=CARTESIAN_POINT('Ctrl Pts',(-6.61775933994476,34.7517105184419,27.3443868392198));
#51808=CARTESIAN_POINT('Ctrl Pts',(-6.61333077242632,34.855512611258,27.3504669175205));
#51809=CARTESIAN_POINT('Ctrl Pts',(-6.60890154979115,34.9593300594879,27.3565478952455));
#51810=CARTESIAN_POINT('Ctrl Pts',(-6.6092512426745,35.063331702573,27.3626288729705));
#51811=CARTESIAN_POINT('Ctrl Pts',(-6.61436852588733,35.1670466521595,27.3687098506955));
#51812=CARTESIAN_POINT('Ctrl Pts',(-6.61949112082979,35.2708692576538,27.3747971404631));
#51813=CARTESIAN_POINT('Ctrl Pts',(-6.62939116804803,35.3744041472782,27.3808844302306));
#51814=CARTESIAN_POINT('Ctrl Pts',(-6.64400531070665,35.4771841446809,27.3869717199982));
#51815=CARTESIAN_POINT('Ctrl Pts',(-6.65862730536355,35.5800193645063,27.3930622803914));
#51816=CARTESIAN_POINT('Ctrl Pts',(-6.67796836100029,35.682098463848,27.3991528407845));
#51817=CARTESIAN_POINT('Ctrl Pts',(-6.70191406814667,35.7829650366467,27.4052434011777));
#51818=CARTESIAN_POINT('Ctrl Pts',(-6.72589886957236,35.8839962863934,27.4113439051514));
#51819=CARTESIAN_POINT('Ctrl Pts',(-6.75450322260136,35.9838106434497,27.4174444091252));
#51820=CARTESIAN_POINT('Ctrl Pts',(-6.78756291115494,36.0819671957655,27.4235449130989));
#51821=CARTESIAN_POINT('Ctrl Pts',(-6.81361505145846,36.159317841961,27.4283523142694));
#51822=CARTESIAN_POINT('Ctrl Pts',(-6.84243293212115,36.2356392854295,27.4331597154398));
#51823=CARTESIAN_POINT('Ctrl Pts',(-6.87391576260421,36.3107259069712,27.4379671166102));
#51824=CARTESIAN_POINT('Ctrl Pts',(-6.91387445338392,36.4060274743921,27.444068774367));
#51825=CARTESIAN_POINT('Ctrl Pts',(-6.95826267810669,36.4996611620125,27.4501704321238));
#51826=CARTESIAN_POINT('Ctrl Pts',(-7.00691976467638,36.5911869052425,27.4562720898807));
#51827=CARTESIAN_POINT('Ctrl Pts',(-7.05551284871861,36.6825922573988,27.4623657216428));
#51828=CARTESIAN_POINT('Ctrl Pts',(-7.10836343232686,36.7718948029809,27.4684593534049));
#51829=CARTESIAN_POINT('Ctrl Pts',(-7.1652626800912,36.8586740945137,27.474552985167));
#51830=CARTESIAN_POINT('Ctrl Pts',(-7.22210336421032,36.9453640683166,27.4806403450485));
#51831=CARTESIAN_POINT('Ctrl Pts',(-7.28298419289195,37.0295355965252,27.4867277049301));
#51832=CARTESIAN_POINT('Ctrl Pts',(-7.34765071064495,37.1107932892062,27.4928150648116));
#51833=CARTESIAN_POINT('Ctrl Pts',(-7.41227122464338,37.1919931751722,27.4988980941459));
#51834=CARTESIAN_POINT('Ctrl Pts',(-7.4806718065959,37.2702830140263,27.5049811234801));
#51835=CARTESIAN_POINT('Ctrl Pts',(-7.55255551693585,37.3452975429183,27.5110641528144));
#51836=CARTESIAN_POINT('Ctrl Pts',(-7.62441261176841,37.4202842970929,27.5171449298594));
#51837=CARTESIAN_POINT('Ctrl Pts',(-7.69974997624432,37.4919978429857,27.5232257069043));
#51838=CARTESIAN_POINT('Ctrl Pts',(-7.77823186408501,37.5601076955341,27.5293064839493));
#51839=CARTESIAN_POINT('Ctrl Pts',(-7.85670502620347,37.6282099755372,27.5353865849253));
#51840=CARTESIAN_POINT('Ctrl Pts',(-7.93832169342656,37.6927090785546,27.5414666859013));
#51841=CARTESIAN_POINT('Ctrl Pts',(-8.02271159073161,37.7533135689697,27.5475467868772));
#51842=CARTESIAN_POINT('Ctrl Pts',(-8.1071139685944,37.8139270222806,27.5536277870491));
#51843=CARTESIAN_POINT('Ctrl Pts',(-8.19429004390403,37.8706444691265,27.559708787221));
#51844=CARTESIAN_POINT('Ctrl Pts',(-8.28383976907246,37.9232172557446,27.5657897873929));
#51845=CARTESIAN_POINT('Ctrl Pts',(-8.37348243910881,37.9758446083672,27.5718770991169));
#51846=CARTESIAN_POINT('Ctrl Pts',(-8.46550330951064,38.0243184927264,27.5779644108409));
#51847=CARTESIAN_POINT('Ctrl Pts',(-8.55947691538168,38.0684358075706,27.5840517225649));
#51848=CARTESIAN_POINT('Ctrl Pts',(-8.65350100824729,38.1125768242897,27.5901423046761));
#51849=CARTESIAN_POINT('Ctrl Pts',(-8.74947953108165,38.1523564454947,27.5962328867873));
#51850=CARTESIAN_POINT('Ctrl Pts',(-8.84696804158223,38.1876201726942,27.6023234688984));
#51851=CARTESIAN_POINT('Ctrl Pts',(-8.9446157035233,38.2229414684519,27.6084239939753));
#51852=CARTESIAN_POINT('Ctrl Pts',(-9.04377786880567,38.253732015688,27.6145245190522));
#51853=CARTESIAN_POINT('Ctrl Pts',(-9.14399575154938,38.2798874659254,27.6206250441291));
#51854=CARTESIAN_POINT('Ctrl Pts',(-9.22296680667401,38.3004977946009,27.6254322191456));
#51855=CARTESIAN_POINT('Ctrl Pts',(-9.30259308127847,38.3182310356037,27.6302393941621));
#51856=CARTESIAN_POINT('Ctrl Pts',(-9.38264738477849,38.3330587770064,27.6350465691787));
#51857=CARTESIAN_POINT('Ctrl Pts',(-9.48425923743688,38.351879430098,27.6411482518881));
#51858=CARTESIAN_POINT('Ctrl Pts',(-9.58690422830258,38.3660810321104,27.6472499345976));
#51859=CARTESIAN_POINT('Ctrl Pts',(-9.69012622107235,38.3755567398035,27.653351617307));
#51860=CARTESIAN_POINT('Ctrl Pts',(-9.79321244377338,38.3850199838981,27.6594452743442));
#51861=CARTESIAN_POINT('Ctrl Pts',(-9.89687373720429,38.3897696526902,27.6655389313814));
#51862=CARTESIAN_POINT('Ctrl Pts',(-10.0006439713222,38.3897499388304,27.6716325884186));
#51863=CARTESIAN_POINT('Ctrl Pts',(-10.1043074050542,38.3897302452602,27.6777199738605));
#51864=CARTESIAN_POINT('Ctrl Pts',(-10.208079131036,38.384950930002,27.6838073593023));
#51865=CARTESIAN_POINT('Ctrl Pts',(-10.3114889697607,38.3754080766949,27.6898947447441));
#51866=CARTESIAN_POINT('Ctrl Pts',(-10.4148252484858,38.3658720116422,27.6959777999589));
#51867=CARTESIAN_POINT('Ctrl Pts',(-10.5177997271705,38.351579186081,27.7020608551738));
#51868=CARTESIAN_POINT('Ctrl Pts',(-10.6199441358344,38.332577730668,27.7081439103886));
#51869=CARTESIAN_POINT('Ctrl Pts',(-10.7220507280278,38.3135833100795,27.714224713501));
#51870=CARTESIAN_POINT('Ctrl Pts',(-10.8233274408911,38.2898838024001,27.7203055166133));
#51871=CARTESIAN_POINT('Ctrl Pts',(-10.9233138194449,38.2615788589764,27.7263863197257));
#51872=CARTESIAN_POINT('Ctrl Pts',(-11.0232890839676,38.2332770618016,27.7324664469236));
#51873=CARTESIAN_POINT('Ctrl Pts',(-11.1219738878181,38.2003709633452,27.7385465741215));
#51874=CARTESIAN_POINT('Ctrl Pts',(-11.2189215086733,38.1630104992228,27.7446267013194));
#51875=CARTESIAN_POINT('Ctrl Pts',(-11.3158834691591,38.1256445090725,27.7507077278358));
#51876=CARTESIAN_POINT('Ctrl Pts',(-11.4111073369849,38.0838229981179,27.7567887543521));
#51877=CARTESIAN_POINT('Ctrl Pts',(-11.5041658512638,38.0377442542768,27.7628697808684));
#51878=CARTESIAN_POINT('Ctrl Pts',(-11.597320952198,37.9916176847017,27.7689571189621));
#51879=CARTESIAN_POINT('Ctrl Pts',(-11.6883058271688,37.9412252480255,27.7750444570557));
#51880=CARTESIAN_POINT('Ctrl Pts',(-11.7767173813687,37.8868114606331,27.7811317951494));
#51881=CARTESIAN_POINT('Ctrl Pts',(-11.86517643494,37.832368439271,27.7872224036837));
#51882=CARTESIAN_POINT('Ctrl Pts',(-11.9510590602153,37.7739000044431,27.7933130122179));
#51883=CARTESIAN_POINT('Ctrl Pts',(-12.03399240966,37.7116931869121,27.7994036207521));
#51884=CARTESIAN_POINT('Ctrl Pts',(-12.1170611458879,37.649384818184,27.8055041720646));
#51885=CARTESIAN_POINT('Ctrl Pts',(-12.1971706578459,37.5833261474703,27.811604723377));
#51886=CARTESIAN_POINT('Ctrl Pts',(-12.2739821794322,37.5138436924608,27.8177052746894));
#51887=CARTESIAN_POINT('Ctrl Pts',(-12.3345056451099,37.4590951483085,27.8225121903753));
#51888=CARTESIAN_POINT('Ctrl Pts',(-12.3929821821247,37.402221717251,27.8273191060612));
#51889=CARTESIAN_POINT('Ctrl Pts',(-12.4492635142395,37.3433978109393,27.8321260217471));
#51890=CARTESIAN_POINT('Ctrl Pts',(-12.5197884181869,37.2696868629828,27.8381494624564));
#51891=CARTESIAN_POINT('Ctrl Pts',(-12.5871173059483,37.1926485687336,27.8441729031657));
#51892=CARTESIAN_POINT('Ctrl Pts',(-12.6509144165922,37.1125950436379,27.8501963438749));
#51893=CARTESIAN_POINT('Ctrl Pts',(-12.7146125115311,37.0326657648623,27.8562104359597));
#51894=CARTESIAN_POINT('Ctrl Pts',(-12.7747894584714,36.9497309025452,27.8622245280446));
#51895=CARTESIAN_POINT('Ctrl Pts',(-12.8311464857577,36.8641391146269,27.8682386201294));
#51896=CARTESIAN_POINT('Ctrl Pts',(-12.887452973542,36.7786240831761,27.8742473189344));
#51897=CARTESIAN_POINT('Ctrl Pts',(-12.9399461035467,36.6904572226187,27.8802560177393));
#51898=CARTESIAN_POINT('Ctrl Pts',(-12.9883678913794,36.6000195024663,27.8862647165443));
#51899=CARTESIAN_POINT('Ctrl Pts',(-13.0367575357117,36.50964181696,27.8922694266363));
#51900=CARTESIAN_POINT('Ctrl Pts',(-13.0810810016637,36.4169966542195,27.8982741367283));
#51901=CARTESIAN_POINT('Ctrl Pts',(-13.1211247158629,36.3224921816516,27.9042788468204));
#51902=CARTESIAN_POINT('Ctrl Pts',(-13.1414419477865,36.2745428511419,27.9073254944656));
#51903=CARTESIAN_POINT('Ctrl Pts',(-13.160658162689,36.2261152885534,27.9103721421109));
#51904=CARTESIAN_POINT('Ctrl Pts',(-13.1787500671536,36.1772650819042,27.9134187897562));
#51905=CARTESIAN_POINT('Origin',(-10.,35.,23.));
#51906=CARTESIAN_POINT('',(-13.1787500528927,36.1772651204102,29.1634930667589));
#51907=CARTESIAN_POINT('',(-13.1787500671537,36.177265081904,28.8235277009158));
#51908=CARTESIAN_POINT('',(-13.1787500671536,36.1772650819043,23.));
#51909=CARTESIAN_POINT('',(-7.42676557298528,37.2065515280922,30.));
#51910=CARTESIAN_POINT('Ctrl Pts',(-7.42676557298526,37.2065515280922,30.));
#51911=CARTESIAN_POINT('Ctrl Pts',(-7.42044787186859,37.1991839566551,29.9994303932239));
#51912=CARTESIAN_POINT('Ctrl Pts',(-7.41416177089548,37.1917892038426,29.9988626237233));
#51913=CARTESIAN_POINT('Ctrl Pts',(-7.40027527655973,37.1753107133754,29.9976058906998));
#51914=CARTESIAN_POINT('Ctrl Pts',(-7.39269053096667,37.1662139038115,29.9969177930047));
#51915=CARTESIAN_POINT('Ctrl Pts',(-7.36359004725985,37.1309377951778,29.994270531793));
#51916=CARTESIAN_POINT('Ctrl Pts',(-7.34241906846593,37.1044754836715,29.9923291917595));
#51917=CARTESIAN_POINT('Ctrl Pts',(-7.2301273078817,36.9597207178191,29.9819237473292));
#51918=CARTESIAN_POINT('Ctrl Pts',(-7.14649535007684,36.8358152200063,29.9737735088464));
#51919=CARTESIAN_POINT('Ctrl Pts',(-6.99394268335336,36.5740487549211,29.9573004080105));
#51920=CARTESIAN_POINT('Ctrl Pts',(-6.92569854003083,36.4362028734202,29.9489953670567));
#51921=CARTESIAN_POINT('Ctrl Pts',(-6.83268627949556,36.2110431793853,29.9355077349894));
#51922=CARTESIAN_POINT('Ctrl Pts',(-6.80165808509507,36.1265474919904,29.9304643713169));
#51923=CARTESIAN_POINT('Ctrl Pts',(-6.76217732629905,36.0041907195728,29.923124350649));
#51924=CARTESIAN_POINT('Ctrl Pts',(-6.7509539859517,35.9672613470769,29.9209045127161));
#51925=CARTESIAN_POINT('Ctrl Pts',(-6.73224036891425,35.9016809286153,29.9169499801724));
#51926=CARTESIAN_POINT('Ctrl Pts',(-6.72449028298769,35.8731079678905,29.9152228946107));
#51927=CARTESIAN_POINT('Ctrl Pts',(-6.70890731199449,35.8125267203424,29.9115503843584));
#51928=CARTESIAN_POINT('Ctrl Pts',(-6.70116494633203,35.7804985172093,29.9096025428753));
#51929=CARTESIAN_POINT('Ctrl Pts',(-6.68142266347274,35.6932813309301,29.9042785794563));
#51930=CARTESIAN_POINT('Ctrl Pts',(-6.67033349861846,35.6378988872998,29.9008764684895));
#51931=CARTESIAN_POINT('Ctrl Pts',(-6.60768262401444,35.2785894246722,29.8786459957547));
#51932=CARTESIAN_POINT('Ctrl Pts',(-6.59641207396922,34.9691496330044,29.8585946837763));
#51933=CARTESIAN_POINT('Ctrl Pts',(-6.64229018594765,34.5106134504596,29.8287625927251));
#51934=CARTESIAN_POINT('Ctrl Pts',(-6.66773753543461,34.3598823643459,29.8189728421815));
#51935=CARTESIAN_POINT('Ctrl Pts',(-6.70996561949286,34.1833553682101,29.8078529773363));
#51936=CARTESIAN_POINT('Ctrl Pts',(-6.71702372747825,34.1554281587476,29.8061045002741));
#51937=CARTESIAN_POINT('Ctrl Pts',(-6.72873899736422,34.1114416756164,29.8033709372274));
#51938=CARTESIAN_POINT('Ctrl Pts',(-6.73316029745685,34.0953216995518,29.8023735063816));
#51939=CARTESIAN_POINT('Ctrl Pts',(-6.74176270860991,34.064843096824,29.8004966956275));
#51940=CARTESIAN_POINT('Ctrl Pts',(-6.7459197690407,34.0504787783796,29.7996161030741));
#51941=CARTESIAN_POINT('Ctrl Pts',(-6.75629356760114,34.0155015871302,29.7974812803449));
#51942=CARTESIAN_POINT('Ctrl Pts',(-6.76261179601755,33.9949197966454,29.7962329050143));
#51943=CARTESIAN_POINT('Ctrl Pts',(-6.78594519021965,33.9214143493779,29.7917978131322));
#51944=CARTESIAN_POINT('Ctrl Pts',(-6.80406637841891,33.8688482188654,29.7886696479653));
#51945=CARTESIAN_POINT('Ctrl Pts',(-6.89322020342415,33.6295081292945,29.7745239865511));
#51946=CARTESIAN_POINT('Ctrl Pts',(-6.97939137300909,33.4487857673895,29.7640987033258));
#51947=CARTESIAN_POINT('Ctrl Pts',(-7.14589102066328,33.1667610831271,29.7467532846791));
#51948=CARTESIAN_POINT('Ctrl Pts',(-7.21694898265522,33.060585862539,29.7399459310837));
#51949=CARTESIAN_POINT('Ctrl Pts',(-7.34395608773212,32.8922128759651,29.7283946348034));
#51950=CARTESIAN_POINT('Ctrl Pts',(-7.39651860311298,32.8276236744837,29.7237618910563));
#51951=CARTESIAN_POINT('Ctrl Pts',(-7.47418650544213,32.739056525246,29.7170706588259));
#51952=CARTESIAN_POINT('Ctrl Pts',(-7.49736585125607,32.7134258390944,29.7150918567539));
#51953=CARTESIAN_POINT('Ctrl Pts',(-7.53838042752792,32.6694445629033,29.711618665269));
#51954=CARTESIAN_POINT('Ctrl Pts',(-7.55603934628222,32.6509329866654,29.7101320156842));
#51955=CARTESIAN_POINT('Ctrl Pts',(-7.59302291324448,32.6130321216308,29.7070352759142));
#51956=CARTESIAN_POINT('Ctrl Pts',(-7.61237622756455,32.5936735464382,29.7054239456122));
#51957=CARTESIAN_POINT('Ctrl Pts',(-7.66334213201807,32.5439139874644,29.7012029078186));
#51958=CARTESIAN_POINT('Ctrl Pts',(-7.69531323036121,32.5138891612483,29.6985767347992));
#51959=CARTESIAN_POINT('Ctrl Pts',(-7.85832597731241,32.3666470804838,29.6852872972427));
#51960=CARTESIAN_POINT('Ctrl Pts',(-7.99774650970611,32.2591460760691,29.6742181312849));
#51961=CARTESIAN_POINT('Ctrl Pts',(-8.31022565522744,32.0548160388896,29.6501911371802));
#51962=CARTESIAN_POINT('Ctrl Pts',(-8.48473044029537,31.9613484769058,29.63721135416));
#51963=CARTESIAN_POINT('Ctrl Pts',(-8.72024718768592,31.8605620443076,29.6208810910153));
#51964=CARTESIAN_POINT('Ctrl Pts',(-8.77470449408973,31.8389100633464,29.617184874961));
#51965=CARTESIAN_POINT('Ctrl Pts',(-8.86804894544407,31.8045717551782,29.6110143771785));
#51966=CARTESIAN_POINT('Ctrl Pts',(-8.90665343930957,31.7911577639238,29.608509339066));
#51967=CARTESIAN_POINT('Ctrl Pts',(-8.96296752398051,31.7727245570946,29.6049324284727));
#51968=CARTESIAN_POINT('Ctrl Pts',(-8.98048881279557,31.7671467531446,29.6038302571288));
#51969=CARTESIAN_POINT('Ctrl Pts',(-9.01199194320197,31.7573995045647,29.6018688893715));
#51970=CARTESIAN_POINT('Ctrl Pts',(-9.02595653883095,31.7531773630961,29.6010066499992));
#51971=CARTESIAN_POINT('Ctrl Pts',(-9.05730530849841,31.7439196375393,29.5990862906916));
#51972=CARTESIAN_POINT('Ctrl Pts',(-9.07470368620323,31.7389327863549,29.5980309472168));
#51973=CARTESIAN_POINT('Ctrl Pts',(-9.1257739054026,31.7247362951594,29.5949614409659));
#51974=CARTESIAN_POINT('Ctrl Pts',(-9.1595500061878,31.7159068821048,29.5929672208399));
#51975=CARTESIAN_POINT('Ctrl Pts',(-9.33016597049147,31.6741109306034,29.5830459396973));
#51976=CARTESIAN_POINT('Ctrl Pts',(-9.4688406102282,31.6491653649432,29.5754687058191));
#51977=CARTESIAN_POINT('Ctrl Pts',(-9.8580781706075,31.6039280059719,29.5546030013781));
#51978=CARTESIAN_POINT('Ctrl Pts',(-10.1099113486465,31.6027422679523,29.5415006238399));
#51979=CARTESIAN_POINT('Ctrl Pts',(-10.4241097814455,31.636259587128,29.5239583435427));
#51980=CARTESIAN_POINT('Ctrl Pts',(-10.4884416191561,31.6449973609881,29.520307208312));
#51981=CARTESIAN_POINT('Ctrl Pts',(-10.5847409741776,31.660905480538,29.5147328332933));
#51982=CARTESIAN_POINT('Ctrl Pts',(-10.6169220393908,31.6667011372861,29.5128516084428));
#51983=CARTESIAN_POINT('Ctrl Pts',(-10.6727287650557,31.677587489654,29.5095551455745));
#51984=CARTESIAN_POINT('Ctrl Pts',(-10.69639347101,31.6824670356265,29.5081465433602));
#51985=CARTESIAN_POINT('Ctrl Pts',(-10.7497964823286,31.6940750379833,29.5049426189362));
#51986=CARTESIAN_POINT('Ctrl Pts',(-10.7794999355984,31.7009525041008,29.5031427660733));
#51987=CARTESIAN_POINT('Ctrl Pts',(-10.8598040498489,31.7206909797798,29.4982269605688));
#51988=CARTESIAN_POINT('Ctrl Pts',(-10.9102053492972,31.7343214438424,29.4950874658728));
#51989=CARTESIAN_POINT('Ctrl Pts',(-11.1668290533207,31.8101246808292,29.4788174245134));
#51990=CARTESIAN_POINT('Ctrl Pts',(-11.3670760940175,31.8906794914953,29.4651240321363));
#51991=CARTESIAN_POINT('Ctrl Pts',(-11.6765185520715,32.0508627371648,29.442757184862));
#51992=CARTESIAN_POINT('Ctrl Pts',(-11.7910317449351,32.1189701916702,29.4341939055577));
#51993=CARTESIAN_POINT('Ctrl Pts',(-11.9597299130344,32.2332593221212,29.4213828282598));
#51994=CARTESIAN_POINT('Ctrl Pts',(-12.0169651572732,32.2747021808372,29.4170001106056));
#51995=CARTESIAN_POINT('Ctrl Pts',(-12.0915185977888,32.3323211035021,29.4112841620895));
#51996=CARTESIAN_POINT('Ctrl Pts',(-12.1100199525093,32.3469307197105,29.4098651015657));
#51997=CARTESIAN_POINT('Ctrl Pts',(-12.1406319303622,32.3716263027181,29.4075182790486));
#51998=CARTESIAN_POINT('Ctrl Pts',(-12.1528271153108,32.3816056843917,29.4065836590477));
#51999=CARTESIAN_POINT('Ctrl Pts',(-12.1777639627951,32.4023036378329,29.4046739529542));
#52000=CARTESIAN_POINT('Ctrl Pts',(-12.190497105323,32.4130317503896,29.4036995700603));
#52001=CARTESIAN_POINT('Ctrl Pts',(-12.2247738913503,32.4423456633217,29.4010770272111));
#52002=CARTESIAN_POINT('Ctrl Pts',(-12.2461638773938,32.461109982511,29.399440930781));
#52003=CARTESIAN_POINT('Ctrl Pts',(-12.3796482556495,32.5812164500226,29.3892153702647));
#52004=CARTESIAN_POINT('Ctrl Pts',(-12.4851086121436,32.6897003778855,29.381062463495));
#52005=CARTESIAN_POINT('Ctrl Pts',(-12.7063310003824,32.9500104331378,29.3628440577734));
#52006=CARTESIAN_POINT('Ctrl Pts',(-12.8172205559896,33.1052832861524,29.3528527105587));
#52007=CARTESIAN_POINT('Ctrl Pts',(-12.9511161285198,33.3307290475532,29.3385974614388));
#52008=CARTESIAN_POINT('Ctrl Pts',(-12.9857814087657,33.3935565797701,29.334652146283));
#52009=CARTESIAN_POINT('Ctrl Pts',(-13.0439817218624,33.5074404343609,29.3275075610989));
#52010=CARTESIAN_POINT('Ctrl Pts',(-13.0682896832628,33.5580718805099,29.3243336039601));
#52011=CARTESIAN_POINT('Ctrl Pts',(-13.1039865417543,33.63741987352,29.3193506024849));
#52012=CARTESIAN_POINT('Ctrl Pts',(-13.1162601177284,33.6657287228074,29.3175711608442));
#52013=CARTESIAN_POINT('Ctrl Pts',(-13.1383771508478,33.7187118136351,29.3142357781199));
#52014=CARTESIAN_POINT('Ctrl Pts',(-13.1483203671356,33.7433419859982,29.3126833016252));
#52015=CARTESIAN_POINT('Ctrl Pts',(-13.169917480196,33.7987055062604,29.3091881646942));
#52016=CARTESIAN_POINT('Ctrl Pts',(-13.1814157677096,33.8294963087346,29.3072405698236));
#52017=CARTESIAN_POINT('Ctrl Pts',(-13.214881543688,33.9232510065904,29.3012970394068));
#52018=CARTESIAN_POINT('Ctrl Pts',(-13.2354395434981,33.9866975941466,29.2972565361413));
#52019=CARTESIAN_POINT('Ctrl Pts',(-13.3389887715299,34.3416569667822,29.2745422681367));
#52020=CARTESIAN_POINT('Ctrl Pts',(-13.3844515865375,34.6426550315855,29.2547080383822));
#52021=CARTESIAN_POINT('Ctrl Pts',(-13.3904139810993,35.0141741504821,29.2310163158062));
#52022=CARTESIAN_POINT('Ctrl Pts',(-13.3894334358754,35.0827635834291,29.2266835485809));
#52023=CARTESIAN_POINT('Ctrl Pts',(-13.3843135361265,35.1973720898942,29.2195582491029));
#52024=CARTESIAN_POINT('Ctrl Pts',(-13.3813134624638,35.2434205496467,29.2167264757905));
#52025=CARTESIAN_POINT('Ctrl Pts',(-13.375669953646,35.3092827603988,29.2127339396693));
#52026=CARTESIAN_POINT('Ctrl Pts',(-13.3737902332312,35.3291549280024,29.2115368530168));
#52027=CARTESIAN_POINT('Ctrl Pts',(-13.3701959684134,35.3638786139674,29.2094596887173));
#52028=CARTESIAN_POINT('Ctrl Pts',(-13.3685585447885,35.378737206747,29.2085755810229));
#52029=CARTESIAN_POINT('Ctrl Pts',(-13.364749816301,35.4113179805376,29.2066476681809));
#52030=CARTESIAN_POINT('Ctrl Pts',(-13.3625367351179,35.4290344314555,29.2056061203588));
#52031=CARTESIAN_POINT('Ctrl Pts',(-13.3555738011611,35.4814074092704,29.202545070484));
#52032=CARTESIAN_POINT('Ctrl Pts',(-13.3504272403609,35.5160098224672,29.2005459625742));
#52033=CARTESIAN_POINT('Ctrl Pts',(-13.3143118316057,35.7354299294076,29.1879827814945));
#52034=CARTESIAN_POINT('Ctrl Pts',(-13.2685943706197,35.917510735033,29.178059014632));
#52035=CARTESIAN_POINT('Ctrl Pts',(-13.1986388559469,36.1224812787303,29.1665818236184));
#52036=CARTESIAN_POINT('Ctrl Pts',(-13.1888698716654,36.1499404558964,29.1650380334421));
#52037=CARTESIAN_POINT('Ctrl Pts',(-13.1787500528927,36.1772651204102,29.1634930667589));
#52038=CARTESIAN_POINT('',(-12.5373008502128,37.2477787831567,30.));
#52039=CARTESIAN_POINT('Origin',(-10.,35.,30.));
#52040=CARTESIAN_POINT('Ctrl Pts',(-12.5373008502128,37.2477787831567,30.));
#52041=CARTESIAN_POINT('Ctrl Pts',(-12.5209396269508,37.2662473913687,29.9984867864796));
#52042=CARTESIAN_POINT('Ctrl Pts',(-12.5043772682535,37.2845367879542,29.9969623568916));
#52043=CARTESIAN_POINT('Ctrl Pts',(-12.3453284488148,37.4563621161872,29.9824055457391));
#52044=CARTESIAN_POINT('Ctrl Pts',(-12.1891050598384,37.5965540829986,29.9687575740533));
#52045=CARTESIAN_POINT('Ctrl Pts',(-11.889180987769,37.8192798357995,29.9447572538372));
#52046=CARTESIAN_POINT('Ctrl Pts',(-11.7504662075106,37.9074425883838,29.9343556202805));
#52047=CARTESIAN_POINT('Ctrl Pts',(-11.5488536037137,38.0159000158817,29.9203139605392));
#52048=CARTESIAN_POINT('Ctrl Pts',(-11.490941690947,38.0449456670797,29.9163937485696));
#52049=CARTESIAN_POINT('Ctrl Pts',(-11.4026183240444,38.0861196186118,29.9105799145652));
#52050=CARTESIAN_POINT('Ctrl Pts',(-11.3728079672304,38.0994952587838,29.9086451107208));
#52051=CARTESIAN_POINT('Ctrl Pts',(-11.3206255736704,38.1220084578819,29.905304492922));
#52052=CARTESIAN_POINT('Ctrl Pts',(-11.2983409675913,38.131341484563,29.9038923030429));
#52053=CARTESIAN_POINT('Ctrl Pts',(-11.2476965406407,38.1519182999373,29.9007145484011));
#52054=CARTESIAN_POINT('Ctrl Pts',(-11.2192806844991,38.1630191788191,29.8989537416988));
#52055=CARTESIAN_POINT('Ctrl Pts',(-11.141762425252,38.1921023863124,29.8942074610472));
#52056=CARTESIAN_POINT('Ctrl Pts',(-11.0923866097706,38.2093349739042,29.8912459757493));
#52057=CARTESIAN_POINT('Ctrl Pts',(-10.8409828617183,38.2906022717227,29.8764429922407));
#52058=CARTESIAN_POINT('Ctrl Pts',(-10.633663954766,38.3367342160331,29.8651626739669));
#52059=CARTESIAN_POINT('Ctrl Pts',(-10.2889264735885,38.3801317635053,29.8466594289939));
#52060=CARTESIAN_POINT('Ctrl Pts',(-10.1535860127577,38.3889787179865,29.8394465161247));
#52061=CARTESIAN_POINT('Ctrl Pts',(-9.94672665429997,38.3900825267069,29.8280696073382));
#52062=CARTESIAN_POINT('Ctrl Pts',(-9.87537613772187,38.388209722915,29.8240805287763));
#52063=CARTESIAN_POINT('Ctrl Pts',(-9.78052898184786,38.3827203578675,29.8186306161271));
#52064=CARTESIAN_POINT('Ctrl Pts',(-9.75693070932611,38.381106594221,29.8172624785278));
#52065=CARTESIAN_POINT('Ctrl Pts',(-9.71762699695598,38.3780052344146,29.8149606568456));
#52066=CARTESIAN_POINT('Ctrl Pts',(-9.70191116678088,38.3766546916441,29.814034078292));
#52067=CARTESIAN_POINT('Ctrl Pts',(-9.66965296072587,38.3736556218104,29.8121184567339));
#52068=CARTESIAN_POINT('Ctrl Pts',(-9.65311223514773,38.3719949991171,29.8111287971063));
#52069=CARTESIAN_POINT('Ctrl Pts',(-9.60841641350148,38.3671753800673,29.8084357371168));
#52070=CARTESIAN_POINT('Ctrl Pts',(-9.58028821460886,38.3637850182946,29.8067206857173));
#52071=CARTESIAN_POINT('Ctrl Pts',(-9.41608043113668,38.3419010329106,29.7966025993656));
#52072=CARTESIAN_POINT('Ctrl Pts',(-9.28119394985866,38.3155053374668,29.7878696586115));
#52073=CARTESIAN_POINT('Ctrl Pts',(-8.95383218171039,38.230526484566,29.7661553880092));
#52074=CARTESIAN_POINT('Ctrl Pts',(-8.76422704821641,38.1628539162094,29.7531416767803));
#52075=CARTESIAN_POINT('Ctrl Pts',(-8.5149303884167,38.0480127538378,29.7359279937534));
#52076=CARTESIAN_POINT('Ctrl Pts',(-8.44915074034565,38.0150756544054,29.7313715525671));
#52077=CARTESIAN_POINT('Ctrl Pts',(-8.33420404022636,37.9527615635442,29.7233906840237));
#52078=CARTESIAN_POINT('Ctrl Pts',(-8.28461295995801,37.9242306549314,29.7199408904801));
#52079=CARTESIAN_POINT('Ctrl Pts',(-8.20924299603481,37.8782910190496,29.7146852705358));
#52080=CARTESIAN_POINT('Ctrl Pts',(-8.18294343888853,37.8617608892065,29.7128488972518));
#52081=CARTESIAN_POINT('Ctrl Pts',(-8.13459468532429,37.8304368564147,29.7094672144109));
#52082=CARTESIAN_POINT('Ctrl Pts',(-8.11248512401191,37.8157410104619,29.7079185172302));
#52083=CARTESIAN_POINT('Ctrl Pts',(-8.06361086845244,37.7824207476384,29.7044888010652));
#52084=CARTESIAN_POINT('Ctrl Pts',(-8.03693747063544,37.763666712362,29.7026127608475));
#52085=CARTESIAN_POINT('Ctrl Pts',(-7.96934302950577,37.7146686871443,29.6978444695392));
#52086=CARTESIAN_POINT('Ctrl Pts',(-7.92882413539501,37.6838823968095,29.6949726764167));
#52087=CARTESIAN_POINT('Ctrl Pts',(-7.63999469295613,37.4539914695313,29.6743581788488));
#52088=CARTESIAN_POINT('Ctrl Pts',(-7.42015155987203,37.2217270340292,29.6580610057696));
#52089=CARTESIAN_POINT('Ctrl Pts',(-7.1957217566724,36.9055845152184,29.6371032174982));
#52090=CARTESIAN_POINT('Ctrl Pts',(-7.15726955445118,36.8477314318024,29.6333029118373));
#52091=CARTESIAN_POINT('Ctrl Pts',(-7.09605716183785,36.749196487882,29.6268188413329));
#52092=CARTESIAN_POINT('Ctrl Pts',(-7.07230938446741,36.7091517139359,29.6241806288692));
#52093=CARTESIAN_POINT('Ctrl Pts',(-7.03953556508414,36.6511985196832,29.6203399572476));
#52094=CARTESIAN_POINT('Ctrl Pts',(-7.02983111444626,36.6336777438702,29.6191759241695));
#52095=CARTESIAN_POINT('Ctrl Pts',(-7.01321621451732,36.6030431622358,29.6171338441503));
#52096=CARTESIAN_POINT('Ctrl Pts',(-7.00623558765716,36.5899683635448,29.6162601067456));
#52097=CARTESIAN_POINT('Ctrl Pts',(-6.99108621974016,36.5611399030567,29.6143283056083));
#52098=CARTESIAN_POINT('Ctrl Pts',(-6.98295542671353,36.5453678998681,29.6132681268058));
#52099=CARTESIAN_POINT('Ctrl Pts',(-6.95987361924039,36.4997176028676,29.6101916861547));
#52100=CARTESIAN_POINT('Ctrl Pts',(-6.94524042811648,36.4696819642634,29.6081579069329));
#52101=CARTESIAN_POINT('Ctrl Pts',(-6.84412820607362,36.2541059421147,29.5935180623731));
#52102=CARTESIAN_POINT('Ctrl Pts',(-6.7741746252472,36.0612955692302,29.5802282225884));
#52103=CARTESIAN_POINT('Ctrl Pts',(-6.68450100595008,35.7208313936711,29.5575489221594));
#52104=CARTESIAN_POINT('Ctrl Pts',(-6.65629286295052,35.5759866101405,29.5481261198815));
#52105=CARTESIAN_POINT('Ctrl Pts',(-6.62596082143454,35.3386692698542,29.5332252168921));
#52106=CARTESIAN_POINT('Ctrl Pts',(-6.61802418822,35.2471421473609,29.5276032278844));
#52107=CARTESIAN_POINT('Ctrl Pts',(-6.6121337200653,35.1187870857662,29.5198950418595));
#52108=CARTESIAN_POINT('Ctrl Pts',(-6.61104737133741,35.0821495119626,29.5177145840352));
#52109=CARTESIAN_POINT('Ctrl Pts',(-6.61019615423459,35.0187401145605,29.5139736436072));
#52110=CARTESIAN_POINT('Ctrl Pts',(-6.61015384111658,34.9919759570796,29.5124047494517));
#52111=CARTESIAN_POINT('Ctrl Pts',(-6.61071936862101,34.9368713382597,29.509194389416));
#52112=CARTESIAN_POINT('Ctrl Pts',(-6.6113657110771,34.9085333207337,29.5075542379979));
#52113=CARTESIAN_POINT('Ctrl Pts',(-6.61395421772528,34.8353333556793,29.5033436036199));
#52114=CARTESIAN_POINT('Ctrl Pts',(-6.61643248272675,34.7904951873941,29.5007897592267));
#52115=CARTESIAN_POINT('Ctrl Pts',(-6.63459402809224,34.5490717863472,29.4871554454963));
#52116=CARTESIAN_POINT('Ctrl Pts',(-6.66651870138317,34.3540840183654,29.4765897419547));
#52117=CARTESIAN_POINT('Ctrl Pts',(-6.75666823990741,34.0003116434927,29.4572284040476));
#52118=CARTESIAN_POINT('Ctrl Pts',(-6.81013619776005,33.8409742157929,29.4484213260463));
#52119=CARTESIAN_POINT('Ctrl Pts',(-6.89625318544574,33.636138897112,29.4362920852963));
#52120=CARTESIAN_POINT('Ctrl Pts',(-6.91852774618704,33.5865327733839,29.4332877382476));
#52121=CARTESIAN_POINT('Ctrl Pts',(-6.95880171285986,33.5023226884867,29.4280370032332));
#52122=CARTESIAN_POINT('Ctrl Pts',(-6.97622337510505,33.4674534258208,29.425817175743));
#52123=CARTESIAN_POINT('Ctrl Pts',(-7.00283920762476,33.4164034283052,29.4224881002581));
#52124=CARTESIAN_POINT('Ctrl Pts',(-7.01157216102883,33.3999843957678,29.4214050693375));
#52125=CARTESIAN_POINT('Ctrl Pts',(-7.02752378732178,33.370579566588,29.4194417385407));
#52126=CARTESIAN_POINT('Ctrl Pts',(-7.03469337341124,33.3575681535262,29.4185644181907));
#52127=CARTESIAN_POINT('Ctrl Pts',(-7.05120597351274,33.3280615392013,29.4165553827969));
#52128=CARTESIAN_POINT('Ctrl Pts',(-7.06060202136618,33.3115972300352,29.415420498807));
#52129=CARTESIAN_POINT('Ctrl Pts',(-7.09050791962363,33.2602006431111,29.4118361111738));
#52130=CARTESIAN_POINT('Ctrl Pts',(-7.11150544701686,33.2255578690523,29.4093592635796));
#52131=CARTESIAN_POINT('Ctrl Pts',(-7.24819545161236,33.0088970326594,29.3935193328223));
#52132=CARTESIAN_POINT('Ctrl Pts',(-7.38041216586462,32.8379013365208,29.3794691012816));
#52133=CARTESIAN_POINT('Ctrl Pts',(-7.56237680253748,32.6439594356501,29.3623812090118));
#52134=CARTESIAN_POINT('Ctrl Pts',(-7.5975981204726,32.6080553118372,29.3591605227291));
#52135=CARTESIAN_POINT('Ctrl Pts',(-7.7437955640887,32.4655117260328,29.3461577608832));
#52136=CARTESIAN_POINT('Ctrl Pts',(-7.86118405595141,32.3656944248076,29.3365537202643));
#52137=CARTESIAN_POINT('Ctrl Pts',(-8.01952131852312,32.2486446882893,29.3246683838735));
#52138=CARTESIAN_POINT('Ctrl Pts',(-8.05456221067293,32.2237572294516,29.3220989480786));
#52139=CARTESIAN_POINT('Ctrl Pts',(-8.1132847542766,32.1837080464183,29.3178905598686));
#52140=CARTESIAN_POINT('Ctrl Pts',(-8.13669787798292,32.1681631298337,29.3162375118986));
#52141=CARTESIAN_POINT('Ctrl Pts',(-8.18292643767467,32.1382917150435,29.3130209227098));
#52142=CARTESIAN_POINT('Ctrl Pts',(-8.20572464058836,32.1239425188523,29.3114566312738));
#52143=CARTESIAN_POINT('Ctrl Pts',(-8.25623278564863,32.0929870362857,29.3080377681723));
#52144=CARTESIAN_POINT('Ctrl Pts',(-8.28401411557813,32.0765019215338,29.3061876098534));
#52145=CARTESIAN_POINT('Ctrl Pts',(-8.38119318868305,32.0206996036542,29.2998156412589));
#52146=CARTESIAN_POINT('Ctrl Pts',(-8.45174213620083,31.9834348595183,29.2953645908614));
#52147=CARTESIAN_POINT('Ctrl Pts',(-8.77624245161622,31.8264168248332,29.2755445854091));
#52148=CARTESIAN_POINT('Ctrl Pts',(-9.04313207141249,31.7360136239522,29.2611013552682));
#52149=CARTESIAN_POINT('Ctrl Pts',(-9.38365250996888,31.6660835854944,29.2422781176924));
#52150=CARTESIAN_POINT('Ctrl Pts',(-9.44958218530448,31.6545669602589,29.2386105305425));
#52151=CARTESIAN_POINT('Ctrl Pts',(-9.56066917573313,31.638534825396,29.2323304537426));
#52152=CARTESIAN_POINT('Ctrl Pts',(-9.60565556225182,31.6329609817424,29.2297598276176));
#52153=CARTESIAN_POINT('Ctrl Pts',(-9.6704657282075,31.6262475505551,29.2260000929369));
#52154=CARTESIAN_POINT('Ctrl Pts',(-9.69021061456033,31.6243772541966,29.224847172381));
#52155=CARTESIAN_POINT('Ctrl Pts',(-9.72489391099103,31.6213988012479,29.2228070939141));
#52156=CARTESIAN_POINT('Ctrl Pts',(-9.73982503168357,31.6202162206567,29.2219239385905));
#52157=CARTESIAN_POINT('Ctrl Pts',(-9.7728035987184,31.6178240735557,29.2199620737127));
#52158=CARTESIAN_POINT('Ctrl Pts',(-9.79085294767274,31.6166599815685,29.2188810845482));
#52159=CARTESIAN_POINT('Ctrl Pts',(-9.84360728723493,31.6136813349682,29.2157021068948));
#52160=CARTESIAN_POINT('Ctrl Pts',(-9.8783309369857,31.6122560280276,29.2135850617306));
#52161=CARTESIAN_POINT('Ctrl Pts',(-10.0981263677544,31.6066174553222,29.2000541810209));
#52162=CARTESIAN_POINT('Ctrl Pts',(-10.2832483732874,31.6170376190416,29.1880914295951));
#52163=CARTESIAN_POINT('Ctrl Pts',(-10.6239784709893,31.6643877498171,29.1659230141077));
#52164=CARTESIAN_POINT('Ctrl Pts',(-10.7796569781257,31.6973040163098,29.1557331274996));
#52165=CARTESIAN_POINT('Ctrl Pts',(-11.0248254515854,31.7674518777504,29.1398229311888));
#52166=CARTESIAN_POINT('Ctrl Pts',(-11.1160301687483,31.7977954588283,29.1339328961468));
#52167=CARTESIAN_POINT('Ctrl Pts',(-11.2407477939109,31.8452661125389,29.1259222172468));
#52168=CARTESIAN_POINT('Ctrl Pts',(-11.2754448838168,31.8591336378877,29.1236981799086));
#52169=CARTESIAN_POINT('Ctrl Pts',(-11.3348213199839,31.8840111021375,29.1198987602241));
#52170=CARTESIAN_POINT('Ctrl Pts',(-11.3596107978847,31.894747464534,29.1183144979025));
#52171=CARTESIAN_POINT('Ctrl Pts',(-11.4070719875209,31.9159803041733,29.1152842291648));
#52172=CARTESIAN_POINT('Ctrl Pts',(-11.4297611101642,31.926433296835,29.113836889095));
#52173=CARTESIAN_POINT('Ctrl Pts',(-11.489709738225,31.9548594315303,29.1100149306547));
#52174=CARTESIAN_POINT('Ctrl Pts',(-11.5267599390454,31.9732657063701,29.1076551260102));
#52175=CARTESIAN_POINT('Ctrl Pts',(-11.6730874650145,32.0493309696961,29.0983330598165));
#52176=CARTESIAN_POINT('Ctrl Pts',(-11.7795182426047,32.112269338126,29.0915521627291));
#52177=CARTESIAN_POINT('Ctrl Pts',(-12.0757893280323,32.3100852188785,29.0723399803462));
#52178=CARTESIAN_POINT('Ctrl Pts',(-12.2554677453518,32.4588585975599,29.0602912873199));
#52179=CARTESIAN_POINT('Ctrl Pts',(-12.4834735946583,32.6910249054707,29.0426296952372));
#52180=CARTESIAN_POINT('Ctrl Pts',(-12.5457117965855,32.7598313137064,29.0375050969097));
#52181=CARTESIAN_POINT('Ctrl Pts',(-12.6212677042778,32.8505806660665,29.030753781437));
#52182=CARTESIAN_POINT('Ctrl Pts',(-12.6372701627646,32.8702455875169,29.0292912021241));
#52183=CARTESIAN_POINT('Ctrl Pts',(-12.6629383551474,32.9025213331412,29.026887933541));
#52184=CARTESIAN_POINT('Ctrl Pts',(-12.6727389390418,32.9150242249577,29.0259563015219));
#52185=CARTESIAN_POINT('Ctrl Pts',(-12.6909629300947,32.9386127466578,29.0241964444135));
#52186=CARTESIAN_POINT('Ctrl Pts',(-12.6994066599705,32.9496823254402,29.0233696789054));
#52187=CARTESIAN_POINT('Ctrl Pts',(-12.7217820403145,32.9793938529969,29.0211488899844));
#52188=CARTESIAN_POINT('Ctrl Pts',(-12.7355900635766,32.9981274729344,29.0197468853315));
#52189=CARTESIAN_POINT('Ctrl Pts',(-12.7872450041257,33.0697412089155,29.0143853882205));
#52190=CARTESIAN_POINT('Ctrl Pts',(-12.8237584255344,33.1235616294103,29.010352120052));
#52191=CARTESIAN_POINT('Ctrl Pts',(-12.9626053366071,33.3414582233969,28.9941076228168));
#52192=CARTESIAN_POINT('Ctrl Pts',(-13.0523665036986,33.5131081470561,28.9815183798047));
#52193=CARTESIAN_POINT('Ctrl Pts',(-13.1994628265299,33.8646252523959,28.9570765815282));
#52194=CARTESIAN_POINT('Ctrl Pts',(-13.2574225244727,34.0435197481613,28.9452567810019));
#52195=CARTESIAN_POINT('Ctrl Pts',(-13.31045493455,34.2697382096425,28.9312105266925));
#52196=CARTESIAN_POINT('Ctrl Pts',(-13.3197767551102,34.313358363635,28.9285407689065));
#52197=CARTESIAN_POINT('Ctrl Pts',(-13.3336175666805,34.3850167268999,28.92421618508));
#52198=CARTESIAN_POINT('Ctrl Pts',(-13.3386497105125,34.4129491582204,28.9225455342672));
#52199=CARTESIAN_POINT('Ctrl Pts',(-13.3477773477245,34.4675351162431,28.9193090562825));
#52200=CARTESIAN_POINT('Ctrl Pts',(-13.3519067643714,34.4941807368721,28.9177422826077));
#52201=CARTESIAN_POINT('Ctrl Pts',(-13.3609760471372,34.557700384283,28.9140369870926));
#52202=CARTESIAN_POINT('Ctrl Pts',(-13.3656277297902,34.5946124337918,28.9119075184641));
#52203=CARTESIAN_POINT('Ctrl Pts',(-13.3793601028952,34.7202175005973,28.9047350133045));
#52204=CARTESIAN_POINT('Ctrl Pts',(-13.3855497600678,34.809192343585,28.8997797086442));
#52205=CARTESIAN_POINT('Ctrl Pts',(-13.3963455872416,35.1689113805965,28.8800933739847));
#52206=CARTESIAN_POINT('Ctrl Pts',(-13.3720223036886,35.4394889413582,28.866159333191));
#52207=CARTESIAN_POINT('Ctrl Pts',(-13.302020701116,35.7690573393126,28.8479157063941));
#52208=CARTESIAN_POINT('Ctrl Pts',(-13.2863682651649,35.833410253715,28.8442859466476));
#52209=CARTESIAN_POINT('Ctrl Pts',(-13.2569379098682,35.9406290968532,28.8380642975009));
#52210=CARTESIAN_POINT('Ctrl Pts',(-13.244172277261,35.9837547873549,28.8355135626861));
#52211=CARTESIAN_POINT('Ctrl Pts',(-13.2245784949098,36.0454127285732,28.8317802351001));
#52212=CARTESIAN_POINT('Ctrl Pts',(-13.2184399656098,36.0641608853992,28.8306334098665));
#52213=CARTESIAN_POINT('Ctrl Pts',(-13.207368136938,36.0970039540344,28.8286021549514));
#52214=CARTESIAN_POINT('Ctrl Pts',(-13.2025048060993,36.1111215033851,28.8277216735734));
#52215=CARTESIAN_POINT('Ctrl Pts',(-13.1915487528986,36.1422557851853,28.8257632687472));
#52216=CARTESIAN_POINT('Ctrl Pts',(-13.1854131894937,36.15925601176,28.8246830364101));
#52217=CARTESIAN_POINT('Ctrl Pts',(-13.1790114989384,36.1765590056772,28.8235730107745));
#52218=CARTESIAN_POINT('Ctrl Pts',(-13.1788808123799,36.176912054873,28.8235503573816));
#52219=CARTESIAN_POINT('Ctrl Pts',(-13.1787500671537,36.177265081904,28.8235277009158));
#52220=CARTESIAN_POINT('Origin',(-10.,35.,23.));
#52221=CARTESIAN_POINT('',(-13.3897499995487,35.0000553150526,27.6441403738275));
#52222=CARTESIAN_POINT('Ctrl Pts',(-13.1787500671537,36.177265081904,28.8235277009158));
#52223=CARTESIAN_POINT('Ctrl Pts',(-13.166434766078,36.210517800194,28.8213936176659));
#52224=CARTESIAN_POINT('Ctrl Pts',(-13.1535989446877,36.2435738652805,28.8192322861915));
#52225=CARTESIAN_POINT('Ctrl Pts',(-13.0858169506057,36.4103309352554,28.8081469722261));
#52226=CARTESIAN_POINT('Ctrl Pts',(-13.022880744743,36.5406118917708,28.7988926786411));
#52227=CARTESIAN_POINT('Ctrl Pts',(-12.8184861727369,36.9026578936524,28.7721200136203));
#52228=CARTESIAN_POINT('Ctrl Pts',(-12.6572519859891,37.1220346140764,28.7546511910919));
#52229=CARTESIAN_POINT('Ctrl Pts',(-12.4383388202369,37.3552635424168,28.7352501428755));
#52230=CARTESIAN_POINT('Ctrl Pts',(-12.4043516353376,37.389948981851,28.7323361799766));
#52231=CARTESIAN_POINT('Ctrl Pts',(-12.3487390154015,37.4443165943742,28.7277198463628));
#52232=CARTESIAN_POINT('Ctrl Pts',(-12.3275847858441,37.4644690545115,28.7259973978757));
#52233=CARTESIAN_POINT('Ctrl Pts',(-12.2866205591494,37.5024953838658,28.7227243024674));
#52234=CARTESIAN_POINT('Ctrl Pts',(-12.2668549948662,37.5204137001373,28.7211718498571));
#52235=CARTESIAN_POINT('Ctrl Pts',(-12.2205451806129,37.5614099921634,28.717594812036));
#52236=CARTESIAN_POINT('Ctrl Pts',(-12.1938489277326,37.5843121059695,28.7155774902595));
#52237=CARTESIAN_POINT('Ctrl Pts',(-12.1045808818177,37.6585128069503,28.708972195594));
#52238=CARTESIAN_POINT('Ctrl Pts',(-12.0405269200284,37.7079886084641,28.7044553655199));
#52239=CARTESIAN_POINT('Ctrl Pts',(-11.8769317184796,37.8252468018461,28.6933885358282));
#52240=CARTESIAN_POINT('Ctrl Pts',(-11.7754341422537,37.8901087047309,28.6869311280284));
#52241=CARTESIAN_POINT('Ctrl Pts',(-11.4581549298229,38.0698302985159,28.667530135191));
#52242=CARTESIAN_POINT('Ctrl Pts',(-11.2332480888688,38.1668825137047,28.6548423315028));
#52243=CARTESIAN_POINT('Ctrl Pts',(-10.9661459976826,38.2493406884846,28.6390527818522));
#52244=CARTESIAN_POINT('Ctrl Pts',(-10.9322322711635,38.2592323921266,28.6370344486184));
#52245=CARTESIAN_POINT('Ctrl Pts',(-10.8808368575517,38.2733552626088,28.6339468710406));
#52246=CARTESIAN_POINT('Ctrl Pts',(-10.8634649382657,38.2779805542203,28.6328983228947));
#52247=CARTESIAN_POINT('Ctrl Pts',(-10.8315762262773,38.2861998845013,28.6309631796081));
#52248=CARTESIAN_POINT('Ctrl Pts',(-10.817071278103,38.2898363485813,28.6300789340397));
#52249=CARTESIAN_POINT('Ctrl Pts',(-10.7832176212011,38.2980859386765,28.6280059826253));
#52250=CARTESIAN_POINT('Ctrl Pts',(-10.7638518991496,38.3026248553185,28.6268133336086));
#52251=CARTESIAN_POINT('Ctrl Pts',(-10.699685028846,38.3170696670052,28.6228415648047));
#52252=CARTESIAN_POINT('Ctrl Pts',(-10.6547244550655,38.3262359758911,28.6200265089239));
#52253=CARTESIAN_POINT('Ctrl Pts',(-10.5425962849199,38.3467346868527,28.612949033971));
#52254=CARTESIAN_POINT('Ctrl Pts',(-10.4752477666643,38.3569602935189,28.6086479006761));
#52255=CARTESIAN_POINT('Ctrl Pts',(-10.1121661262008,38.4009425370305,28.5853366893942));
#52256=CARTESIAN_POINT('Ctrl Pts',(-9.81320160132118,38.3976679133283,28.5658578659115));
#52257=CARTESIAN_POINT('Ctrl Pts',(-9.4497784236149,38.3455166363152,28.5432673969683));
#52258=CARTESIAN_POINT('Ctrl Pts',(-9.38136995557253,38.3335451495908,28.5390552259866));
#52259=CARTESIAN_POINT('Ctrl Pts',(-9.28080837533687,38.3127442300193,28.5329208956245));
#52260=CARTESIAN_POINT('Ctrl Pts',(-9.24834326895999,38.30552918659,28.5309493985302));
#52261=CARTESIAN_POINT('Ctrl Pts',(-9.19024481020219,38.2917171506692,28.5274361100453));
#52262=CARTESIAN_POINT('Ctrl Pts',(-9.16457294883622,38.2852955678993,28.525888941759));
#52263=CARTESIAN_POINT('Ctrl Pts',(-9.10968953863327,38.2708820438247,28.522591511108));
#52264=CARTESIAN_POINT('Ctrl Pts',(-9.08050444941199,38.2627978914372,28.5208443241915));
#52265=CARTESIAN_POINT('Ctrl Pts',(-8.99979037213182,38.2392713803137,28.5160271820677));
#52266=CARTESIAN_POINT('Ctrl Pts',(-8.9485136156673,38.2229916540452,28.5129839885266));
#52267=CARTESIAN_POINT('Ctrl Pts',(-8.72554797795612,38.1463147910459,28.4997960289365));
#52268=CARTESIAN_POINT('Ctrl Pts',(-8.55849118790347,38.0733671443277,28.4900526261314));
#52269=CARTESIAN_POINT('Ctrl Pts',(-8.21039392337908,37.8867063059201,28.4690851937724));
#52270=CARTESIAN_POINT('Ctrl Pts',(-8.03262348458114,37.7686052114341,28.457938027921));
#52271=CARTESIAN_POINT('Ctrl Pts',(-7.83354885916886,37.6074433426528,28.4435819969441));
#52272=CARTESIAN_POINT('Ctrl Pts',(-7.80049643429137,37.579623041644,28.441128671115));
#52273=CARTESIAN_POINT('Ctrl Pts',(-7.75351541099053,37.5385195978483,28.4375242156927));
#52274=CARTESIAN_POINT('Ctrl Pts',(-7.73915287529624,37.5257365259102,28.4364059509919));
#52275=CARTESIAN_POINT('Ctrl Pts',(-7.71383564177686,37.5028144899695,28.4344038779858));
#52276=CARTESIAN_POINT('Ctrl Pts',(-7.70283798582009,37.4927243151097,28.4335235562481));
#52277=CARTESIAN_POINT('Ctrl Pts',(-7.67856540180816,37.4701575509501,28.4315565585262));
#52278=CARTESIAN_POINT('Ctrl Pts',(-7.66532432703466,37.457646514294,28.4304674450363));
#52279=CARTESIAN_POINT('Ctrl Pts',(-7.62579816065501,37.4196919142239,28.4271693389946));
#52280=CARTESIAN_POINT('Ctrl Pts',(-7.59982427665488,37.3939297394818,28.4249385988885));
#52281=CARTESIAN_POINT('Ctrl Pts',(-7.53947191510846,37.3320996870264,28.4196140352381));
#52282=CARTESIAN_POINT('Ctrl Pts',(-7.50546208284561,37.2956845470343,28.4165007860368));
#52283=CARTESIAN_POINT('Ctrl Pts',(-7.37794915451968,37.1529732608738,28.404427436929));
#52284=CARTESIAN_POINT('Ctrl Pts',(-7.29033809915329,37.0416106891168,28.3952751547634));
#52285=CARTESIAN_POINT('Ctrl Pts',(-7.08835706118761,36.7488794491795,28.3723617308675));
#52286=CARTESIAN_POINT('Ctrl Pts',(-6.98371889729,36.5615108978639,28.3587208858197));
#52287=CARTESIAN_POINT('Ctrl Pts',(-6.87617075894826,36.3171508286412,28.3424664533197));
#52288=CARTESIAN_POINT('Ctrl Pts',(-6.85602381318998,36.2683097565836,28.3392865892569));
#52289=CARTESIAN_POINT('Ctrl Pts',(-6.82610028714547,36.190667319821,28.3343370700035));
#52290=CARTESIAN_POINT('Ctrl Pts',(-6.81555615816321,36.1621727762971,28.3325425193558));
#52291=CARTESIAN_POINT('Ctrl Pts',(-6.79655229936173,36.1086150554803,28.3292092334463));
#52292=CARTESIAN_POINT('Ctrl Pts',(-6.78800015065401,36.0835873468427,28.3276675833656));
#52293=CARTESIAN_POINT('Ctrl Pts',(-6.76940491919353,36.0270133043127,28.3242174810881));
#52294=CARTESIAN_POINT('Ctrl Pts',(-6.75952921702349,35.9954145461676,28.3223145466611));
#52295=CARTESIAN_POINT('Ctrl Pts',(-6.7306186575016,35.8979170714287,28.3165126872897));
#52296=CARTESIAN_POINT('Ctrl Pts',(-6.71311909975902,35.8315793737517,28.3126622931271));
#52297=CARTESIAN_POINT('Ctrl Pts',(-6.67632132206091,35.6726792268013,28.3036306435247));
#52298=CARTESIAN_POINT('Ctrl Pts',(-6.65885818356737,35.5797501734478,28.2985010166764));
#52299=CARTESIAN_POINT('Ctrl Pts',(-6.61365159120521,35.2678376817111,28.2815899001262));
#52300=CARTESIAN_POINT('Ctrl Pts',(-6.60340128422791,35.0469117972492,28.2701381474515));
#52301=CARTESIAN_POINT('Ctrl Pts',(-6.61905258039951,34.7414046191699,28.2534839635711));
#52302=CARTESIAN_POINT('Ctrl Pts',(-6.62662742200177,34.6564417704503,28.2487592141704));
#52303=CARTESIAN_POINT('Ctrl Pts',(-6.64060342594177,34.5466740373212,28.2424332344298));
#52304=CARTESIAN_POINT('Ctrl Pts',(-6.64409321938054,34.5215239107456,28.2409685636642));
#52305=CARTESIAN_POINT('Ctrl Pts',(-6.65022631922119,34.4806985767634,28.2385627653547));
#52306=CARTESIAN_POINT('Ctrl Pts',(-6.65269800261716,34.4649981341706,28.2376307331641));
#52307=CARTESIAN_POINT('Ctrl Pts',(-6.65784846929929,34.433715457829,28.2357590394871));
#52308=CARTESIAN_POINT('Ctrl Pts',(-6.66052604122618,34.4181334416889,28.2348194596194));
#52309=CARTESIAN_POINT('Ctrl Pts',(-6.6677180458531,34.377965528228,28.2323795603338));
#52310=CARTESIAN_POINT('Ctrl Pts',(-6.67239553410521,34.3534102195046,28.2308707362243));
#52311=CARTESIAN_POINT('Ctrl Pts',(-6.69483918722206,34.2422887538044,28.2239711100712));
#52312=CARTESIAN_POINT('Ctrl Pts',(-6.71571365780099,34.1563916326028,28.2184404451808));
#52313=CARTESIAN_POINT('Ctrl Pts',(-6.79657066806341,33.8725181833984,28.1997033414331));
#52314=CARTESIAN_POINT('Ctrl Pts',(-6.87130623137782,33.6792222410189,28.1862135929335));
#52315=CARTESIAN_POINT('Ctrl Pts',(-7.02953877504176,33.3601639195086,28.1635501502474));
#52316=CARTESIAN_POINT('Ctrl Pts',(-7.10465536211101,33.2309067137465,28.1542355015247));
#52317=CARTESIAN_POINT('Ctrl Pts',(-7.21242016325755,33.0708275474554,28.1425801046868));
#52318=CARTESIAN_POINT('Ctrl Pts',(-7.23747603525473,33.035115955559,28.1399708178252));
#52319=CARTESIAN_POINT('Ctrl Pts',(-7.27985152129769,32.9771326576891,28.1357172856535));
#52320=CARTESIAN_POINT('Ctrl Pts',(-7.29677166386621,32.9545766537819,28.134058243212));
#52321=CARTESIAN_POINT('Ctrl Pts',(-7.33050206972609,32.9107608544167,28.1308258341812));
#52322=CARTESIAN_POINT('Ctrl Pts',(-7.34728971977179,32.8894864040244,28.1292517651311));
#52323=CARTESIAN_POINT('Ctrl Pts',(-7.38817006293192,32.8389385460768,28.1254992324593));
#52324=CARTESIAN_POINT('Ctrl Pts',(-7.41250252468886,32.8098631991498,28.123330435319));
#52325=CARTESIAN_POINT('Ctrl Pts',(-7.50301080324101,32.7053273949843,28.115486990426));
#52326=CARTESIAN_POINT('Ctrl Pts',(-7.57204378715094,32.6324044885922,28.1099279342807));
#52327=CARTESIAN_POINT('Ctrl Pts',(-7.88452936670291,32.3303765138965,28.0862607191016));
#52328=CARTESIAN_POINT('Ctrl Pts',(-8.15782883654959,32.1349604411043,28.0693995454902));
#52329=CARTESIAN_POINT('Ctrl Pts',(-8.48927744379643,31.9652703185237,28.0484302233606));
#52330=CARTESIAN_POINT('Ctrl Pts',(-8.52360118212731,31.9484244796703,28.0462509021404));
#52331=CARTESIAN_POINT('Ctrl Pts',(-8.57497476987081,31.9242803017925,28.0429669458511));
#52332=CARTESIAN_POINT('Ctrl Pts',(-8.59181253280937,31.9165349699536,28.0418871551777));
#52333=CARTESIAN_POINT('Ctrl Pts',(-8.62230909918148,31.9028085040565,28.039923725885));
#52334=CARTESIAN_POINT('Ctrl Pts',(-8.63594507271467,31.8967788486542,28.0390429581787));
#52335=CARTESIAN_POINT('Ctrl Pts',(-8.66721666144278,31.8831968837593,28.0370165559367));
#52336=CARTESIAN_POINT('Ctrl Pts',(-8.68487690848522,31.8757041899131,28.0358676033863));
#52337=CARTESIAN_POINT('Ctrl Pts',(-8.74120272284559,31.852369069814,28.0321908458046));
#52338=CARTESIAN_POINT('Ctrl Pts',(-8.78009670456377,31.8370920547107,28.0296337451941));
#52339=CARTESIAN_POINT('Ctrl Pts',(-8.87526239433176,31.8017286587729,28.023349752761));
#52340=CARTESIAN_POINT('Ctrl Pts',(-8.93180135754353,31.7824038135626,28.0195936690612));
#52341=CARTESIAN_POINT('Ctrl Pts',(-9.1851135692938,31.7032348191335,28.0027476023511));
#52342=CARTESIAN_POINT('Ctrl Pts',(-9.38658461972464,31.6598763903841,27.9893341662665));
#52343=CARTESIAN_POINT('Ctrl Pts',(-9.7402021627914,31.6168687271918,27.966658038071));
#52344=CARTESIAN_POINT('Ctrl Pts',(-9.89071545135332,31.6086671354038,27.9572633126712));
#52345=CARTESIAN_POINT('Ctrl Pts',(-10.0849832157498,31.6110337674961,27.9455280399593));
#52346=CARTESIAN_POINT('Ctrl Pts',(-10.1286615352161,31.612410776265,27.9429141082112));
#52347=CARTESIAN_POINT('Ctrl Pts',(-10.200475782283,31.6160658536245,27.9386551017424));
#52348=CARTESIAN_POINT('Ctrl Pts',(-10.2286305681341,31.6178514252808,27.9369951523507));
#52349=CARTESIAN_POINT('Ctrl Pts',(-10.2837708184416,31.6220401192642,27.9337624192067));
#52350=CARTESIAN_POINT('Ctrl Pts',(-10.3107561868358,31.6244156819909,27.93218891404));
#52351=CARTESIAN_POINT('Ctrl Pts',(-10.3753764693928,31.6308857994462,27.9284400918272));
#52352=CARTESIAN_POINT('Ctrl Pts',(-10.4129773641417,31.6352878504166,27.9262743922546));
#52353=CARTESIAN_POINT('Ctrl Pts',(-10.5495374420043,31.6535991142344,27.918458344247));
#52354=CARTESIAN_POINT('Ctrl Pts',(-10.647946512712,31.6712527819722,27.9129224842524));
#52355=CARTESIAN_POINT('Ctrl Pts',(-10.9116584652689,31.7307008266765,27.8981978993259));
#52356=CARTESIAN_POINT('Ctrl Pts',(-11.0748219585882,31.7806524029079,27.8892165004611));
#52357=CARTESIAN_POINT('Ctrl Pts',(-11.3902058864393,31.903869561698,27.8712460553602));
#52358=CARTESIAN_POINT('Ctrl Pts',(-11.5420849235255,31.9766477486335,27.8622788915445));
#52359=CARTESIAN_POINT('Ctrl Pts',(-11.7187326588042,32.0780784385183,27.8507760115731));
#52360=CARTESIAN_POINT('Ctrl Pts',(-11.7492646305123,32.0962540387456,27.8487463104989));
#52361=CARTESIAN_POINT('Ctrl Pts',(-11.7948351459586,32.1243615796153,27.8456450888389));
#52362=CARTESIAN_POINT('Ctrl Pts',(-11.810090325006,32.1339395488428,27.8445945598758));
#52363=CARTESIAN_POINT('Ctrl Pts',(-11.8378618705159,32.1516860818681,27.8426579999226));
#52364=CARTESIAN_POINT('Ctrl Pts',(-11.8504015771968,32.1598164834571,27.8417743567319));
#52365=CARTESIAN_POINT('Ctrl Pts',(-11.8794502638822,32.1789248830082,27.8397059805173));
#52366=CARTESIAN_POINT('Ctrl Pts',(-11.8959171003914,32.1899650506282,27.8385173577485));
#52367=CARTESIAN_POINT('Ctrl Pts',(-11.9498548729703,32.226817466587,27.8345730473586));
#52368=CARTESIAN_POINT('Ctrl Pts',(-11.9869015202532,32.2532387595667,27.8317820638421));
#52369=CARTESIAN_POINT('Ctrl Pts',(-12.0774044158213,32.3205735126223,27.8247799211133));
#52370=CARTESIAN_POINT('Ctrl Pts',(-12.1301943867381,32.3623483234418,27.82053100087));
#52371=CARTESIAN_POINT('Ctrl Pts',(-12.4002276476061,32.5894324375087,27.7980505522779));
#52372=CARTESIAN_POINT('Ctrl Pts',(-12.5946974596593,32.8001105182745,27.7793635235968));
#52373=CARTESIAN_POINT('Ctrl Pts',(-12.8060343545539,33.0966487722939,27.7568413044733));
#52374=CARTESIAN_POINT('Ctrl Pts',(-12.8493863001078,33.16218229632,27.752057380962));
#52375=CARTESIAN_POINT('Ctrl Pts',(-12.9084048960482,33.2585148320735,27.7452955753604));
#52376=CARTESIAN_POINT('Ctrl Pts',(-12.9259373587927,33.2881354221329,27.7432516162175));
#52377=CARTESIAN_POINT('Ctrl Pts',(-12.9562394189953,33.3411559015445,27.7396535727117));
#52378=CARTESIAN_POINT('Ctrl Pts',(-12.9691896438078,33.3644486664253,27.7380931861911));
#52379=CARTESIAN_POINT('Ctrl Pts',(-12.9957871453947,33.4136452135046,27.7348387981648));
#52380=CARTESIAN_POINT('Ctrl Pts',(-13.0093762668814,33.4395780406389,27.733146920061));
#52381=CARTESIAN_POINT('Ctrl Pts',(-13.0447510724429,33.5092670080002,27.7286607142981));
#52382=CARTESIAN_POINT('Ctrl Pts',(-13.0659296237242,33.5533245606395,27.7258872006604));
#52383=CARTESIAN_POINT('Ctrl Pts',(-13.1108486158215,33.6521901262051,27.7197899350797));
#52384=CARTESIAN_POINT('Ctrl Pts',(-13.1341085391091,33.7071988716986,27.7164816470441));
#52385=CARTESIAN_POINT('Ctrl Pts',(-13.2051817426865,33.8884948592549,27.7058098885118));
#52386=CARTESIAN_POINT('Ctrl Pts',(-13.2469075289949,34.0170309436269,27.69860806261));
#52387=CARTESIAN_POINT('Ctrl Pts',(-13.337171070746,34.3645000702773,27.679556706201));
#52388=CARTESIAN_POINT('Ctrl Pts',(-13.3718546197707,34.5863045927268,27.6678347172914));
#52389=CARTESIAN_POINT('Ctrl Pts',(-13.3862616624626,34.8427671081477,27.6532987185319));
#52390=CARTESIAN_POINT('Ctrl Pts',(-13.3876296810394,34.8756810358968,27.6514142305087));
#52391=CARTESIAN_POINT('Ctrl Pts',(-13.3889697175852,34.9253654300795,27.6485340617883));
#52392=CARTESIAN_POINT('Ctrl Pts',(-13.3892973536265,34.942125230214,27.6475564189619));
#52393=CARTESIAN_POINT('Ctrl Pts',(-13.3896044073129,34.967439442401,27.6460696673787));
#52394=CARTESIAN_POINT('Ctrl Pts',(-13.3896757778973,34.9759927583652,27.6455655660513));
#52395=CARTESIAN_POINT('Ctrl Pts',(-13.3897383420373,34.989715973186,27.6447538687426));
#52396=CARTESIAN_POINT('Ctrl Pts',(-13.3897500839088,34.9948856619753,27.6444474400273));
#52397=CARTESIAN_POINT('Ctrl Pts',(-13.3897499995487,35.0000553150526,27.6441403738275));
#52398=CARTESIAN_POINT('Ctrl Pts',(-13.3897499995573,35.0000547843624,27.6441404053493));
#52399=CARTESIAN_POINT('Ctrl Pts',(-13.3897499123479,35.0054508158919,27.6438198928052));
#52400=CARTESIAN_POINT('Ctrl Pts',(-13.3897369404911,35.0108468044594,27.6434986859644));
#52401=CARTESIAN_POINT('Ctrl Pts',(-13.3896570780152,35.0275134090258,27.6425044687922));
#52402=CARTESIAN_POINT('Ctrl Pts',(-13.3895468603506,35.0387836045129,27.6418291920736));
#52403=CARTESIAN_POINT('Ctrl Pts',(-13.3888732877613,35.0843952519037,27.6390848093052));
#52404=CARTESIAN_POINT('Ctrl Pts',(-13.3878442304446,35.1187265535147,27.6369928438969));
#52405=CARTESIAN_POINT('Ctrl Pts',(-13.3760311601969,35.3801214671601,27.620893719586));
#52406=CARTESIAN_POINT('Ctrl Pts',(-13.3429528571328,35.6055865388991,27.6060657679701));
#52407=CARTESIAN_POINT('Ctrl Pts',(-13.2576688564896,35.9450126906287,27.5835867882404));
#52408=CARTESIAN_POINT('Ctrl Pts',(-13.2213420677615,36.0622618086893,27.5757825549973));
#52409=CARTESIAN_POINT('Ctrl Pts',(-13.1787501041618,36.1772649819778,27.5681446579994));
#52410=CARTESIAN_POINT('',(-13.3897486873307,34.9970168406318,27.9839821967053));
#52411=CARTESIAN_POINT('Ctrl Pts',(-13.1787500671536,36.1772650819042,27.9134187897562));
#52412=CARTESIAN_POINT('Ctrl Pts',(-13.2144035502327,36.0809966089206,27.9194227790256));
#52413=CARTESIAN_POINT('Ctrl Pts',(-13.2456875617548,35.9830857988981,27.925426768295));
#52414=CARTESIAN_POINT('Ctrl Pts',(-13.2724606689644,35.8839718505592,27.9314307575644));
#52415=CARTESIAN_POINT('Ctrl Pts',(-13.2992339653125,35.7848572020301,27.937434789249));
#52416=CARTESIAN_POINT('Ctrl Pts',(-13.321496186599,35.6845398253861,27.9434388209335));
#52417=CARTESIAN_POINT('Ctrl Pts',(-13.3391564363488,35.5834718125927,27.9494428526181));
#52418=CARTESIAN_POINT('Ctrl Pts',(-13.3568325931257,35.4823127653216,27.9554522922836));
#52419=CARTESIAN_POINT('Ctrl Pts',(-13.3698984291381,35.3804021667328,27.9614617319492));
#52420=CARTESIAN_POINT('Ctrl Pts',(-13.3783146635796,35.2781997418099,27.9674711716147));
#52421=CARTESIAN_POINT('Ctrl Pts',(-13.3860225734551,35.1845988463221,27.9729748466449));
#52422=CARTESIAN_POINT('Ctrl Pts',(-13.3898311805857,35.0907535031083,27.9784785216751));
#52423=CARTESIAN_POINT('Ctrl Pts',(-13.3897486873307,34.9970168406318,27.9839821967053));
#52424=CARTESIAN_POINT('Ctrl Pts',(-13.1787500528927,36.1772651204102,29.1634930667589));
#52425=CARTESIAN_POINT('Ctrl Pts',(-13.1340997732529,36.2978259663116,29.1566764234979));
#52426=CARTESIAN_POINT('Ctrl Pts',(-13.0826198232573,36.41576798799,29.1498320161008));
#52427=CARTESIAN_POINT('Ctrl Pts',(-12.9813950356215,36.6158049004878,29.1376012013059));
#52428=CARTESIAN_POINT('Ctrl Pts',(-12.9346513179956,36.6992237348765,29.1322991726627));
#52429=CARTESIAN_POINT('Ctrl Pts',(-12.8649284543159,36.8121729879274,29.1247662297391));
#52430=CARTESIAN_POINT('Ctrl Pts',(-12.8448907318852,36.8434702479803,29.1226396230188));
#52431=CARTESIAN_POINT('Ctrl Pts',(-12.8094970446573,36.8968005226064,29.1189441170519));
#52432=CARTESIAN_POINT('Ctrl Pts',(-12.7943861046324,36.9189924709694,29.1173843508491));
#52433=CARTESIAN_POINT('Ctrl Pts',(-12.7628785646721,36.9641031262805,29.1141671402946));
#52434=CARTESIAN_POINT('Ctrl Pts',(-12.7464566298163,36.9870015003217,29.112508814953));
#52435=CARTESIAN_POINT('Ctrl Pts',(-12.703611945471,37.0451971554304,29.1082275934675));
#52436=CARTESIAN_POINT('Ctrl Pts',(-12.6767831641732,37.0801876290235,29.1055892428217));
#52437=CARTESIAN_POINT('Ctrl Pts',(-12.5489147893049,37.2403844470123,29.0932020505005));
#52438=CARTESIAN_POINT('Ctrl Pts',(-12.4397375318726,37.3588044030552,29.083135192241));
#52439=CARTESIAN_POINT('Ctrl Pts',(-12.1783483932242,37.604690743149,29.0602208107304));
#52440=CARTESIAN_POINT('Ctrl Pts',(-12.0225113048132,37.7274643236076,29.047303568469));
#52441=CARTESIAN_POINT('Ctrl Pts',(-11.7843239013872,37.8834195910559,29.0292318324245));
#52442=CARTESIAN_POINT('Ctrl Pts',(-11.7099957716762,37.9281115361742,29.0238068166022));
#52443=CARTESIAN_POINT('Ctrl Pts',(-11.6123415322459,37.9818404798989,29.0170234193192));
#52444=CARTESIAN_POINT('Ctrl Pts',(-11.5905219747764,37.9935360012297,29.0155291620398));
#52445=CARTESIAN_POINT('Ctrl Pts',(-11.5546660594003,38.0122524291996,29.0131108283773));
#52446=CARTESIAN_POINT('Ctrl Pts',(-11.5407058922779,38.0194166054924,29.0121783622819));
#52447=CARTESIAN_POINT('Ctrl Pts',(-11.5124972722046,38.0336463159682,29.0103131610728));
#52448=CARTESIAN_POINT('Ctrl Pts',(-11.498247964132,38.0407089682028,29.0093805753041));
#52449=CARTESIAN_POINT('Ctrl Pts',(-11.4610946009087,38.058799404492,29.0069724922851));
#52450=CARTESIAN_POINT('Ctrl Pts',(-11.4381148559781,38.0696704990969,29.005506114745));
#52451=CARTESIAN_POINT('Ctrl Pts',(-11.3372718719565,38.1159955572945,28.9991620347915));
#52452=CARTESIAN_POINT('Ctrl Pts',(-11.2581991612164,38.1487555447543,28.9944218014761));
#52453=CARTESIAN_POINT('Ctrl Pts',(-10.9923722884826,38.2472724304766,28.9789898181308));
#52454=CARTESIAN_POINT('Ctrl Pts',(-10.8011041296688,38.2996697364071,28.9686683052612));
#52455=CARTESIAN_POINT('Ctrl Pts',(-10.4494835159672,38.3635977653688,28.9495866759908));
#52456=CARTESIAN_POINT('Ctrl Pts',(-10.2908164197036,38.3810122252611,28.9409407273694));
#52457=CARTESIAN_POINT('Ctrl Pts',(-10.0873559290081,38.3889124561683,28.9294613299639));
#52458=CARTESIAN_POINT('Ctrl Pts',(-10.043161520813,38.3897633433184,28.9269452563885));
#52459=CARTESIAN_POINT('Ctrl Pts',(-9.97061338937728,38.3897411810286,28.9227720342434));
#52460=CARTESIAN_POINT('Ctrl Pts',(-9.94226416880182,38.389376838031,28.9211305507055));
#52461=CARTESIAN_POINT('Ctrl Pts',(-9.88683586167956,38.3879688829505,28.9178987169633));
#52462=CARTESIAN_POINT('Ctrl Pts',(-9.85975809258015,38.3869560697033,28.916309435822));
#52463=CARTESIAN_POINT('Ctrl Pts',(-9.79508235974244,38.3837600476191,28.9124872327553));
#52464=CARTESIAN_POINT('Ctrl Pts',(-9.75750355804307,38.3812747009975,28.9102452089159));
#52465=CARTESIAN_POINT('Ctrl Pts',(-9.62219348183156,38.3700584908048,28.9020929210222));
#52466=CARTESIAN_POINT('Ctrl Pts',(-9.52481804690792,38.3577122057406,28.8960746001056));
#52467=CARTESIAN_POINT('Ctrl Pts',(-9.26544685933983,38.3133178482844,28.8796442399029));
#52468=CARTESIAN_POINT('Ctrl Pts',(-9.1050346499253,38.2736329086204,28.8690476126876));
#52469=CARTESIAN_POINT('Ctrl Pts',(-8.78242301563198,38.1683289195128,28.8471837095783));
#52470=CARTESIAN_POINT('Ctrl Pts',(-8.62109057411236,38.1015189170032,28.8359452921324));
#52471=CARTESIAN_POINT('Ctrl Pts',(-8.43387924625587,38.0064824601605,28.8230213642665));
#52472=CARTESIAN_POINT('Ctrl Pts',(-8.40240727777856,37.9898777077718,28.8208535137542));
#52473=CARTESIAN_POINT('Ctrl Pts',(-8.35536573074415,37.9641034441352,28.8176269048468));
#52474=CARTESIAN_POINT('Ctrl Pts',(-8.33959935001169,37.9553004620166,28.8165478431187));
#52475=CARTESIAN_POINT('Ctrl Pts',(-8.31088455279339,37.9389655352719,28.8145879785283));
#52476=CARTESIAN_POINT('Ctrl Pts',(-8.29791504920588,37.9314733913885,28.8137049220446));
#52477=CARTESIAN_POINT('Ctrl Pts',(-8.2678448661108,37.9138357824356,28.811662177695));
#52478=CARTESIAN_POINT('Ctrl Pts',(-8.25078324390662,37.903625519335,28.8105065403981));
#52479=CARTESIAN_POINT('Ctrl Pts',(-8.19474615306908,37.8694177915735,28.8067189357706));
#52480=CARTESIAN_POINT('Ctrl Pts',(-8.15616533025121,37.8447801399108,28.8041240519016));
#52481=CARTESIAN_POINT('Ctrl Pts',(-8.06165447403324,37.7816948555124,28.7977693707605));
#52482=CARTESIAN_POINT('Ctrl Pts',(-8.00635648869059,37.7423340650285,28.7940529073192));
#52483=CARTESIAN_POINT('Ctrl Pts',(-7.71814109732992,37.5238549503901,28.7744865493603));
#52484=CARTESIAN_POINT('Ctrl Pts',(-7.50807853074206,37.3166918242718,28.7594026136538));
#52485=CARTESIAN_POINT('Ctrl Pts',(-7.28297096457466,37.0281430574878,28.7391799358052));
#52486=CARTESIAN_POINT('Ctrl Pts',(-7.24042011243293,36.969855039468,28.7351364129057));
#52487=CARTESIAN_POINT('Ctrl Pts',(-7.18075111425743,36.8823865114958,28.7291003182185));
#52488=CARTESIAN_POINT('Ctrl Pts',(-7.16215655099264,36.8542350715453,28.7271623450142));
#52489=CARTESIAN_POINT('Ctrl Pts',(-7.12970434838394,36.8034719152132,28.7236736095929));
#52490=CARTESIAN_POINT('Ctrl Pts',(-7.1156858742824,36.7809660417894,28.722128887862));
#52491=CARTESIAN_POINT('Ctrl Pts',(-7.08637570856987,36.7326563719046,28.7188162153526));
#52492=CARTESIAN_POINT('Ctrl Pts',(-7.07115966698711,36.7068095476301,28.7170457175915));
#52493=CARTESIAN_POINT('Ctrl Pts',(-7.03034491185258,36.6353261112097,28.712152665751));
#52494=CARTESIAN_POINT('Ctrl Pts',(-7.00545757521113,36.5892948255175,28.709005594645));
#52495=CARTESIAN_POINT('Ctrl Pts',(-6.9041052258938,36.390995958567,28.6954584094061));
#52496=CARTESIAN_POINT('Ctrl Pts',(-6.83812190722855,36.2336726590953,28.6847183628502));
#52497=CARTESIAN_POINT('Ctrl Pts',(-6.72459255235124,35.8931346448058,28.6617034042423));
#52498=CARTESIAN_POINT('Ctrl Pts',(-6.67997647958966,35.7095272700911,28.6494250784797));
#52499=CARTESIAN_POINT('Ctrl Pts',(-6.63987052987213,35.4527795868413,28.6330367752806));
#52500=CARTESIAN_POINT('Ctrl Pts',(-6.63109697931263,35.3820644678309,28.6286055876014));
#52501=CARTESIAN_POINT('Ctrl Pts',(-6.62235174607254,35.2871848434436,28.6228139225835));
#52502=CARTESIAN_POINT('Ctrl Pts',(-6.6204001168107,35.2632253085789,28.6213644529538));
#52503=CARTESIAN_POINT('Ctrl Pts',(-6.61771077589324,35.2252165336518,28.619087883612));
#52504=CARTESIAN_POINT('Ctrl Pts',(-6.61680539691678,35.2111804345761,28.6182521064136));
#52505=CARTESIAN_POINT('Ctrl Pts',(-6.61507480444282,35.1814737210962,28.6164942243093));
#52506=CARTESIAN_POINT('Ctrl Pts',(-6.61427098986582,35.1658022214602,28.6155733718771));
#52507=CARTESIAN_POINT('Ctrl Pts',(-6.61249248523683,35.1256839683633,28.6132314091921));
#52508=CARTESIAN_POINT('Ctrl Pts',(-6.61167356374995,35.1012307161939,28.6118185077685));
#52509=CARTESIAN_POINT('Ctrl Pts',(-6.60925192835746,34.9943317482969,28.6056974598744));
#52510=CARTESIAN_POINT('Ctrl Pts',(-6.61039300101457,34.9118463935938,28.6011184023175));
#52511=CARTESIAN_POINT('Ctrl Pts',(-6.62349217277806,34.6517805178474,28.5869136834067));
#52512=CARTESIAN_POINT('Ctrl Pts',(-6.64641977743063,34.4750543916973,28.5775920815758));
#52513=CARTESIAN_POINT('Ctrl Pts',(-6.72082339736006,34.1220268081602,28.558407957436));
#52514=CARTESIAN_POINT('Ctrl Pts',(-6.77293962969238,33.9464784832982,28.5485639389132));
#52515=CARTESIAN_POINT('Ctrl Pts',(-6.85511764533768,33.734249503145,28.5357410936755));
#52516=CARTESIAN_POINT('Ctrl Pts',(-6.87210824112787,33.6928266272056,28.5331938811931));
#52517=CARTESIAN_POINT('Ctrl Pts',(-6.90121583554541,33.6256822701297,28.5289856285119));
#52518=CARTESIAN_POINT('Ctrl Pts',(-6.91284511967554,33.5997545951006,28.5273409158588));
#52519=CARTESIAN_POINT('Ctrl Pts',(-6.93613455580945,33.5495312182144,28.524114986212));
#52520=CARTESIAN_POINT('Ctrl Pts',(-6.94776119364708,33.5252222697665,28.5225350004613));
#52521=CARTESIAN_POINT('Ctrl Pts',(-6.97608076226448,33.4677814289795,28.5187560223172));
#52522=CARTESIAN_POINT('Ctrl Pts',(-6.99302996320553,33.4347804181616,28.5165483558338));
#52523=CARTESIAN_POINT('Ctrl Pts',(-7.05495576317059,33.3189270482988,28.5086647420849));
#52524=CARTESIAN_POINT('Ctrl Pts',(-7.10283983064361,33.2376855484804,28.5028895216227));
#52525=CARTESIAN_POINT('Ctrl Pts',(-7.23758730060364,33.0294336322828,28.4874257376625));
#52526=CARTESIAN_POINT('Ctrl Pts',(-7.3298143872892,32.9061620302669,28.4775795336394));
#52527=CARTESIAN_POINT('Ctrl Pts',(-7.55611262699796,32.6430584241577,28.4552184612015));
#52528=CARTESIAN_POINT('Ctrl Pts',(-7.69445205054928,32.5075678686494,28.4427018649977));
#52529=CARTESIAN_POINT('Ctrl Pts',(-7.87029390474128,32.3625856290245,28.42867691504));
#52530=CARTESIAN_POINT('Ctrl Pts',(-7.89733100112303,32.3409802752037,28.4265686793645));
#52531=CARTESIAN_POINT('Ctrl Pts',(-7.93895651029983,32.308749339852,28.4234013367194));
#52532=CARTESIAN_POINT('Ctrl Pts',(-7.9533059718195,32.2978205149634,28.4223233064071));
#52533=CARTESIAN_POINT('Ctrl Pts',(-7.97969701894987,32.278051426867,28.4203668266139));
#52534=CARTESIAN_POINT('Ctrl Pts',(-7.9917103766311,32.2691757708859,28.4194861033334));
#52535=CARTESIAN_POINT('Ctrl Pts',(-8.01976187803375,32.2487361194797,28.417452028865));
#52536=CARTESIAN_POINT('Ctrl Pts',(-8.03584302472087,32.2372326595824,28.4163026635101));
#52537=CARTESIAN_POINT('Ctrl Pts',(-8.08899271888234,32.1999112934116,28.4125551998561));
#52538=CARTESIAN_POINT('Ctrl Pts',(-8.12647818199344,32.1746925838617,28.4099931820598));
#52539=CARTESIAN_POINT('Ctrl Pts',(-8.2204679809656,32.1141536069279,28.4037379308024));
#52540=CARTESIAN_POINT('Ctrl Pts',(-8.27753189213291,32.0797349234868,28.4000863663814));
#52541=CARTESIAN_POINT('Ctrl Pts',(-8.57608129324753,31.9114599425304,28.3815326206433));
#52542=CARTESIAN_POINT('Ctrl Pts',(-8.83224366531921,31.8057897946612,28.3673297398342));
#52543=CARTESIAN_POINT('Ctrl Pts',(-9.17958725809878,31.7099510199929,28.3475727265831));
#52544=CARTESIAN_POINT('Ctrl Pts',(-9.26158267448962,31.6905834830818,28.3428829923911));
#52545=CARTESIAN_POINT('Ctrl Pts',(-9.37664190367164,31.6678951903215,28.3362217466616));
#52546=CARTESIAN_POINT('Ctrl Pts',(-9.40916462110694,31.6619749513302,28.3343301857832));
#52547=CARTESIAN_POINT('Ctrl Pts',(-9.46848796849109,31.652070208988,28.3308615696132));
#52548=CARTESIAN_POINT('Ctrl Pts',(-9.49525993021783,31.6479295465497,28.3292894900063));
#52549=CARTESIAN_POINT('Ctrl Pts',(-9.54958058399104,31.6401935859481,28.3260848844295));
#52550=CARTESIAN_POINT('Ctrl Pts',(-9.57712954967957,31.6366152013296,28.3244519636475));
#52551=CARTESIAN_POINT('Ctrl Pts',(-9.64595472657706,31.6285343171899,28.3203520776345));
#52552=CARTESIAN_POINT('Ctrl Pts',(-9.68727468149272,31.6244509259057,28.3178724010656));
#52553=CARTESIAN_POINT('Ctrl Pts',(-9.86319511018777,31.6103235438391,28.3072335234283));
#52554=CARTESIAN_POINT('Ctrl Pts',(-9.99824260213392,31.6075654936302,28.2988570401372));
#52555=CARTESIAN_POINT('Ctrl Pts',(-10.2714192023481,31.6182987677193,28.2815427891607));
#52556=CARTESIAN_POINT('Ctrl Pts',(-10.4092872932831,31.6322036499239,28.2726120659514));
#52557=CARTESIAN_POINT('Ctrl Pts',(-10.7119507475226,31.6815916154419,28.2528520401303));
#52558=CARTESIAN_POINT('Ctrl Pts',(-10.8757576764483,31.7210113430549,28.2420520586333));
#52559=CARTESIAN_POINT('Ctrl Pts',(-11.0632901221813,31.7812048275565,28.2300109273435));
#52560=CARTESIAN_POINT('Ctrl Pts',(-11.0904971058809,31.7903201987758,28.2282725536309));
#52561=CARTESIAN_POINT('Ctrl Pts',(-11.1332663717901,31.8052561523624,28.2255569506633));
#52562=CARTESIAN_POINT('Ctrl Pts',(-11.1489066268253,31.8108473680556,28.2245675332994));
#52563=CARTESIAN_POINT('Ctrl Pts',(-11.1788958591213,31.8218174363999,28.2226782837185));
#52564=CARTESIAN_POINT('Ctrl Pts',(-11.1932503498736,31.8271789424723,28.2217775833855));
#52565=CARTESIAN_POINT('Ctrl Pts',(-11.2286286510776,31.840667045969,28.2195656129329));
#52566=CARTESIAN_POINT('Ctrl Pts',(-11.2496091217785,31.8489065107042,28.2182607486445));
#52567=CARTESIAN_POINT('Ctrl Pts',(-11.3301577382648,31.8814706509055,28.2132721469493));
#52568=CARTESIAN_POINT('Ctrl Pts',(-11.3891142118089,31.9072815072418,28.2096654236234));
#52569=CARTESIAN_POINT('Ctrl Pts',(-11.5499393493573,31.9832176724604,28.1998584665326));
#52570=CARTESIAN_POINT('Ctrl Pts',(-11.6500822268752,32.0368059221728,28.1937865090452));
#52571=CARTESIAN_POINT('Ctrl Pts',(-11.9698095288514,32.2291425492032,28.1739537020739));
#52572=CARTESIAN_POINT('Ctrl Pts',(-12.1761372084177,32.3880626871785,28.1603498002044));
#52573=CARTESIAN_POINT('Ctrl Pts',(-12.3981429066633,32.603791988108,28.1429838574218));
#52574=CARTESIAN_POINT('Ctrl Pts',(-12.4332053684795,32.6394039921987,28.1401503273009));
#52575=CARTESIAN_POINT('Ctrl Pts',(-12.4876955319896,32.6972524207712,28.1355904487289));
#52576=CARTESIAN_POINT('Ctrl Pts',(-12.5076427218605,32.7189907116535,28.1338861811608));
#52577=CARTESIAN_POINT('Ctrl Pts',(-12.5450267154039,32.7608145740583,28.1306229617614));
#52578=CARTESIAN_POINT('Ctrl Pts',(-12.5625158976558,32.7808504853694,28.1290663541624));
#52579=CARTESIAN_POINT('Ctrl Pts',(-12.6021888880244,32.8273949384578,28.1254643061819));
#52580=CARTESIAN_POINT('Ctrl Pts',(-12.6242063182923,32.8540408138312,28.1234123875122));
#52581=CARTESIAN_POINT('Ctrl Pts',(-12.6940337166738,32.9412289812792,28.1167284925802));
#52582=CARTESIAN_POINT('Ctrl Pts',(-12.7401830228991,33.0030645107109,28.1120334800256));
#52583=CARTESIAN_POINT('Ctrl Pts',(-12.8480817564917,33.15842867765,28.1003430847857));
#52584=CARTESIAN_POINT('Ctrl Pts',(-12.9073777637715,33.2535448074914,28.0932732335558));
#52585=CARTESIAN_POINT('Ctrl Pts',(-13.0535958821052,33.5162407491064,28.0740631072902));
#52586=CARTESIAN_POINT('Ctrl Pts',(-13.1314182896993,33.68843310281,28.0617804378806));
#52587=CARTESIAN_POINT('Ctrl Pts',(-13.2235449280478,33.9480032103652,28.0442983313558));
#52588=CARTESIAN_POINT('Ctrl Pts',(-13.249427069796,34.0308946335839,28.0388649674589));
#52589=CARTESIAN_POINT('Ctrl Pts',(-13.2787663606448,34.1393329772367,28.0320231382096));
#52590=CARTESIAN_POINT('Ctrl Pts',(-13.2851543917797,34.1640470831912,28.0304814613219));
#52591=CARTESIAN_POINT('Ctrl Pts',(-13.2950731792533,34.2042919250356,28.0280021316696));
#52592=CARTESIAN_POINT('Ctrl Pts',(-13.2987746104736,34.2197790766284,28.0270554746875));
#52593=CARTESIAN_POINT('Ctrl Pts',(-13.3059269514276,34.2506662337536,28.0251830800681));
#52594=CARTESIAN_POINT('Ctrl Pts',(-13.3093797099731,34.2660653598568,28.0242572714105));
#52595=CARTESIAN_POINT('Ctrl Pts',(-13.3179952213584,34.3057874969596,28.021887629523));
#52596=CARTESIAN_POINT('Ctrl Pts',(-13.3229982254408,34.3301446727635,28.0204523801437));
#52597=CARTESIAN_POINT('Ctrl Pts',(-13.3334405736123,34.3839825207823,28.0173147761501));
#52598=CARTESIAN_POINT('Ctrl Pts',(-13.3387578257398,34.4134849626792,28.0156182857639));
#52599=CARTESIAN_POINT('Ctrl Pts',(-13.3741761586187,34.626122980991,28.0035303339155));
#52600=CARTESIAN_POINT('Ctrl Pts',(-13.3895850560083,34.8113982025932,27.9937269914139));
#52601=CARTESIAN_POINT('Ctrl Pts',(-13.3897486828745,34.99701178137,27.9838867651182));
#52602=CARTESIAN_POINT('Origin',(-10.,35.,32.7603849714045));
#52603=CARTESIAN_POINT('',(-14.0849984180973,34.9964049836978,28.3853849713664));
#52604=CARTESIAN_POINT('Ctrl Pts',(-7.51282733495086,38.2405550657615,29.1925543226443));
#52605=CARTESIAN_POINT('Ctrl Pts',(-7.4182955070919,38.168000526969,29.1867402514207));
#52606=CARTESIAN_POINT('Ctrl Pts',(-7.326830655408,38.0912213338729,29.1809261801971));
#52607=CARTESIAN_POINT('Ctrl Pts',(-7.23882967629141,38.0105088346442,29.1751121089736));
#52608=CARTESIAN_POINT('Ctrl Pts',(-7.15090483531155,37.9298661675852,29.1693030680639));
#52609=CARTESIAN_POINT('Ctrl Pts',(-7.06643820360961,37.8452972399229,29.1634940271543));
#52610=CARTESIAN_POINT('Ctrl Pts',(-6.98579419832905,37.7571340890811,29.1576849862446));
#52611=CARTESIAN_POINT('Ctrl Pts',(-6.90519362828907,37.6690184233271,29.1518790741118));
#52612=CARTESIAN_POINT('Ctrl Pts',(-6.8284118645769,37.5773126851313,29.1460731619789));
#52613=CARTESIAN_POINT('Ctrl Pts',(-6.75577661811945,37.4823858782348,29.140267249846));
#52614=CARTESIAN_POINT('Ctrl Pts',(-6.68316100431293,37.3874847291966,29.1344629069987));
#52615=CARTESIAN_POINT('Ctrl Pts',(-6.6146899270105,37.289364566574,29.1286585641514));
#52616=CARTESIAN_POINT('Ctrl Pts',(-6.55065054055114,37.1884271307493,29.1228542213041));
#52617=CARTESIAN_POINT('Ctrl Pts',(-6.48661336469559,37.0874931792285,29.1170500788195));
#52618=CARTESIAN_POINT('Ctrl Pts',(-6.42700779398407,36.9837424926554,29.1112459363349));
#52619=CARTESIAN_POINT('Ctrl Pts',(-6.37207704802374,36.8776048717778,29.1054417938503));
#52620=CARTESIAN_POINT('Ctrl Pts',(-6.3171352472389,36.7714458906811,29.0996364832807));
#52621=CARTESIAN_POINT('Ctrl Pts',(-6.26687032970223,36.6628993824746,29.0938311727112));
#52622=CARTESIAN_POINT('Ctrl Pts',(-6.22147875497343,36.5524181784825,29.0880258621416));
#52623=CARTESIAN_POINT('Ctrl Pts',(-6.17603959747876,36.4418211600183,29.0822144660213));
#52624=CARTESIAN_POINT('Ctrl Pts',(-6.13548414107057,36.3292857734194,29.0764030699009));
#52625=CARTESIAN_POINT('Ctrl Pts',(-6.09996010488476,36.2152834305254,29.0705916737806));
#52626=CARTESIAN_POINT('Ctrl Pts',(-6.0644166719999,36.1012188405059,29.0647771045439));
#52627=CARTESIAN_POINT('Ctrl Pts',(-6.03391023664728,35.9856860929482,29.0589625353071));
#52628=CARTESIAN_POINT('Ctrl Pts',(-6.00853774778895,35.8691686195292,29.0531479660704));
#52629=CARTESIAN_POINT('Ctrl Pts',(-5.98312519279018,35.7524671513322,29.0473242149458));
#52630=CARTESIAN_POINT('Ctrl Pts',(-5.96286284996756,35.6347782530207,29.0415004638212));
#52631=CARTESIAN_POINT('Ctrl Pts',(-5.94779605265521,35.5165928465662,29.0356767126966));
#52632=CARTESIAN_POINT('Ctrl Pts',(-5.93586929503933,35.4230382133355,29.031066677356));
#52633=CARTESIAN_POINT('Ctrl Pts',(-5.92719713286778,35.3291726322501,29.0264566420155));
#52634=CARTESIAN_POINT('Ctrl Pts',(-5.92177888757647,35.2352393635917,29.021846606675));
#52635=CARTESIAN_POINT('Ctrl Pts',(-5.91493527095027,35.1165951818349,29.0160238148286));
#52636=CARTESIAN_POINT('Ctrl Pts',(-5.91326230607475,34.9974602544536,29.0102010229823));
#52637=CARTESIAN_POINT('Ctrl Pts',(-5.91681257285023,34.8783224146935,29.0043782311359));
#52638=CARTESIAN_POINT('Ctrl Pts',(-5.92035835323838,34.7593351265758,28.9985627974125));
#52639=CARTESIAN_POINT('Ctrl Pts',(-5.92911422513116,34.6403453380733,28.9927473636891));
#52640=CARTESIAN_POINT('Ctrl Pts',(-5.94308090843529,34.5218447067137,28.9869319299657));
#52641=CARTESIAN_POINT('Ctrl Pts',(-5.95703358566419,34.4034629102071,28.9811223280781));
#52642=CARTESIAN_POINT('Ctrl Pts',(-5.97618663134419,34.2855696983084,28.9753127261904));
#52643=CARTESIAN_POINT('Ctrl Pts',(-6.00048875566094,34.168654821145,28.9695031243027));
#52644=CARTESIAN_POINT('Ctrl Pts',(-6.02571561004793,34.0472911681807,28.9634724588778));
#52645=CARTESIAN_POINT('Ctrl Pts',(-6.05649117123816,33.9269822308918,28.957441793453));
#52646=CARTESIAN_POINT('Ctrl Pts',(-6.09269907735653,33.8082682768721,28.9514111280282));
#52647=CARTESIAN_POINT('Ctrl Pts',(-6.12754034506295,33.6940350859505,28.9456080852389));
#52648=CARTESIAN_POINT('Ctrl Pts',(-6.16741118247509,33.5812790842382,28.9398050424496));
#52649=CARTESIAN_POINT('Ctrl Pts',(-6.21215642369427,33.4704686856951,28.9340019996604));
#52650=CARTESIAN_POINT('Ctrl Pts',(-6.25689501143066,33.3596747643249,28.9281998197661));
#52651=CARTESIAN_POINT('Ctrl Pts',(-6.30650640866777,33.2508262494438,28.9223976398718));
#52652=CARTESIAN_POINT('Ctrl Pts',(-6.36078684226828,33.1443727226104,28.9165954599776));
#52653=CARTESIAN_POINT('Ctrl Pts',(-6.41507202504557,33.0379098818017,28.9107927724312));
#52654=CARTESIAN_POINT('Ctrl Pts',(-6.47402687083369,32.933842809575,28.9049900848848));
#52655=CARTESIAN_POINT('Ctrl Pts',(-6.53740137837309,32.8325969951328,28.8991873973384));
#52656=CARTESIAN_POINT('Ctrl Pts',(-6.60079639912306,32.7313184092058,28.8933828315644));
#52657=CARTESIAN_POINT('Ctrl Pts',(-6.66861371006093,32.6328632432358,28.8875782657903));
#52658=CARTESIAN_POINT('Ctrl Pts',(-6.74056004306344,32.5376279389326,28.8817737000163));
#52659=CARTESIAN_POINT('Ctrl Pts',(-6.81258604500554,32.4422871769168,28.8759627066235));
#52660=CARTESIAN_POINT('Ctrl Pts',(-6.88874994918451,32.3501737196662,28.8701517132307));
#52661=CARTESIAN_POINT('Ctrl Pts',(-6.96871816790781,32.2616509619065,28.8643407198379));
#52662=CARTESIAN_POINT('Ctrl Pts',(-7.04873889325022,32.1730700806722,28.8585259109842));
#52663=CARTESIAN_POINT('Ctrl Pts',(-7.13256862151863,32.0880848843044,28.8527111021304));
#52664=CARTESIAN_POINT('Ctrl Pts',(-7.21983808480828,32.0070207609612,28.8468962932767));
#52665=CARTESIAN_POINT('Ctrl Pts',(-7.30723262912441,31.925840450542,28.8410731502103));
#52666=CARTESIAN_POINT('Ctrl Pts',(-7.39807643854486,31.8485926939445,28.835250007144));
#52667=CARTESIAN_POINT('Ctrl Pts',(-7.49196839527695,31.7755616815156,28.8294268640776));
#52668=CARTESIAN_POINT('Ctrl Pts',(-7.5170126758887,31.7560817470006,28.8278736274206));
#52669=CARTESIAN_POINT('Ctrl Pts',(-7.54227367435121,31.7369015790538,28.8263203907635));
#52670=CARTESIAN_POINT('Ctrl Pts',(-7.56774346416096,31.7180260293737,28.8247671541065));
#52671=CARTESIAN_POINT('Ctrl Pts',(-7.66324135127727,31.6472529634761,28.8189433597193));
#52672=CARTESIAN_POINT('Ctrl Pts',(-7.76198471764007,31.5805374438546,28.8131195653321));
#52673=CARTESIAN_POINT('Ctrl Pts',(-7.86359415317665,31.5181908355484,28.8072957709449));
#52674=CARTESIAN_POINT('Ctrl Pts',(-7.96507542051418,31.4559228700618,28.8014793225805));
#52675=CARTESIAN_POINT('Ctrl Pts',(-8.06941522150667,31.3980130665553,28.7956628742162));
#52676=CARTESIAN_POINT('Ctrl Pts',(-8.17620253501886,31.3447315000498,28.7898464258519));
#52677=CARTESIAN_POINT('Ctrl Pts',(-8.28288297680706,31.2915032572274,28.7840357985335));
#52678=CARTESIAN_POINT('Ctrl Pts',(-8.39200569498173,31.2428942180532,28.7782251712152));
#52679=CARTESIAN_POINT('Ctrl Pts',(-8.50313276851186,31.1991299033909,28.7724145438969));
#52680=CARTESIAN_POINT('Ctrl Pts',(-8.61846075270562,31.1537111766191,28.7663842587986));
#52681=CARTESIAN_POINT('Ctrl Pts',(-8.73594724104708,31.11351092483,28.7603539737003));
#52682=CARTESIAN_POINT('Ctrl Pts',(-8.85507675928502,31.0787277864358,28.754323688602));
#52683=CARTESIAN_POINT('Ctrl Pts',(-8.96973771927774,31.0452493664872,28.7485196000048));
#52684=CARTESIAN_POINT('Ctrl Pts',(-9.08592024167654,31.0167891113456,28.7427155114076));
#52685=CARTESIAN_POINT('Ctrl Pts',(-9.20314733844475,30.9934739691633,28.7369114228103));
#52686=CARTESIAN_POINT('Ctrl Pts',(-9.32035712252227,30.9701622702791,28.7311081913903));
#52687=CARTESIAN_POINT('Ctrl Pts',(-9.4386107738259,30.9519942528622,28.7253049599702));
#52688=CARTESIAN_POINT('Ctrl Pts',(-9.5574204195789,30.9390458861255,28.7195017285501));
#52689=CARTESIAN_POINT('Ctrl Pts',(-9.6762405524279,30.9260963764617,28.7136979848901));
#52690=CARTESIAN_POINT('Ctrl Pts',(-9.79561637138188,30.9183674777574,28.7078942412301));
#52691=CARTESIAN_POINT('Ctrl Pts',(-9.91505482028812,30.9158832880972,28.7020904975701));
#52692=CARTESIAN_POINT('Ctrl Pts',(-10.0345319934913,30.9133982930138,28.6962848722221));
#52693=CARTESIAN_POINT('Ctrl Pts',(-10.1540714290248,30.9161613972532,28.6904792468742));
#52694=CARTESIAN_POINT('Ctrl Pts',(-10.273180652745,30.9241445890506,28.6846736215262));
#52695=CARTESIAN_POINT('Ctrl Pts',(-10.3924217429472,30.9321366190838,28.6788615687382));
#52696=CARTESIAN_POINT('Ctrl Pts',(-10.5112312629886,30.9453602451132,28.6730495159502));
#52697=CARTESIAN_POINT('Ctrl Pts',(-10.6291222796832,30.9637356185197,28.6672374631622));
#52698=CARTESIAN_POINT('Ctrl Pts',(-10.7470907118857,30.9821230584849,28.6614215937729));
#52699=CARTESIAN_POINT('Ctrl Pts',(-10.8641390401765,31.0056689028319,28.6556057243835));
#52700=CARTESIAN_POINT('Ctrl Pts',(-10.979792560757,31.0342426274562,28.6497898549941));
#52701=CARTESIAN_POINT('Ctrl Pts',(-11.0956116870234,31.0628572671452,28.6439656577905));
#52702=CARTESIAN_POINT('Ctrl Pts',(-11.2100316288698,31.0965140420848,28.6381414605868));
#52703=CARTESIAN_POINT('Ctrl Pts',(-11.3225946799007,31.1350332067793,28.6323172633832));
#52704=CARTESIAN_POINT('Ctrl Pts',(-11.3524195403347,31.1452392975038,28.6307740761015));
#52705=CARTESIAN_POINT('Ctrl Pts',(-11.3821141592751,31.1557864931314,28.6292308888198));
#52706=CARTESIAN_POINT('Ctrl Pts',(-11.4116702973451,31.1666709022582,28.6276877015381));
#52707=CARTESIAN_POINT('Ctrl Pts',(-11.5232093526256,31.2077465227747,28.6218640160785));
#52708=CARTESIAN_POINT('Ctrl Pts',(-11.6331339345893,31.2537606017622,28.6160403306189));
#52709=CARTESIAN_POINT('Ctrl Pts',(-11.7409756606022,31.3045665005049,28.6102166451593));
#52710=CARTESIAN_POINT('Ctrl Pts',(-11.8486813676145,31.3553083186006,28.6044003050186));
#52711=CARTESIAN_POINT('Ctrl Pts',(-11.9543090777373,31.4108297628885,28.598583964878));
#52712=CARTESIAN_POINT('Ctrl Pts',(-12.0574076135075,31.4709351221774,28.5927676247373));
#52713=CARTESIAN_POINT('Ctrl Pts',(-12.1604029821413,31.5309803361135,28.586957104807));
#52714=CARTESIAN_POINT('Ctrl Pts',(-12.260873860528,31.5956001353734,28.5811465848766));
#52715=CARTESIAN_POINT('Ctrl Pts',(-12.3583915891281,31.6645518873276,28.5753360649462));
#52716=CARTESIAN_POINT('Ctrl Pts',(-12.4595983087819,31.7361120100853,28.5693057392805));
#52717=CARTESIAN_POINT('Ctrl Pts',(-12.5576236322438,31.8123381126629,28.5632754136148));
#52718=CARTESIAN_POINT('Ctrl Pts',(-12.6520188398351,31.8929079393813,28.5572450879491));
#52719=CARTESIAN_POINT('Ctrl Pts',(-12.742871027128,31.9704536662669,28.551441103925));
#52720=CARTESIAN_POINT('Ctrl Pts',(-12.8303603536366,32.0520226312833,28.5456371199008));
#52721=CARTESIAN_POINT('Ctrl Pts',(-12.91411918878,32.1372854921274,28.5398331358767));
#52722=CARTESIAN_POINT('Ctrl Pts',(-12.9978656715284,32.2225357787692,28.5340300077993));
#52723=CARTESIAN_POINT('Ctrl Pts',(-13.0778824709313,32.3114785866766,28.5282268797219));
#52724=CARTESIAN_POINT('Ctrl Pts',(-13.1538386274584,32.4037475253836,28.5224237516445));
#52725=CARTESIAN_POINT('Ctrl Pts',(-13.2298015062869,32.4960246301124,28.5166201099764));
#52726=CARTESIAN_POINT('Ctrl Pts',(-13.3017027681857,32.5916281356603,28.5108164683083));
#52727=CARTESIAN_POINT('Ctrl Pts',(-13.3692519962592,32.6901588830175,28.5050128266402));
#52728=CARTESIAN_POINT('Ctrl Pts',(-13.4368231426422,32.788721601538,28.4992073018119));
#52729=CARTESIAN_POINT('Ctrl Pts',(-13.5000392159967,32.8902131142603,28.4934017769837));
#52730=CARTESIAN_POINT('Ctrl Pts',(-13.5586537021487,32.9942061850271,28.4875962521554));
#52731=CARTESIAN_POINT('Ctrl Pts',(-13.6173331091752,33.0983144375784,28.4817842971804));
#52732=CARTESIAN_POINT('Ctrl Pts',(-13.6714005549847,33.2049294228149,28.4759723422054));
#52733=CARTESIAN_POINT('Ctrl Pts',(-13.7206559180211,33.3136001246162,28.4701603872304));
#52734=CARTESIAN_POINT('Ctrl Pts',(-13.7699436385356,33.4223422157981,28.4643446141898));
#52735=CARTESIAN_POINT('Ctrl Pts',(-13.8144128288937,33.5331423349686,28.4585288411492));
#52736=CARTESIAN_POINT('Ctrl Pts',(-13.8539124552631,33.6455319172575,28.4527130681086));
#52737=CARTESIAN_POINT('Ctrl Pts',(-13.8934686622217,33.7580824901526,28.4468889643597));
#52738=CARTESIAN_POINT('Ctrl Pts',(-13.9280409789672,33.872226681134,28.4410648606108));
#52739=CARTESIAN_POINT('Ctrl Pts',(-13.9575288567085,33.9874831614638,28.4352407568619));
#52740=CARTESIAN_POINT('Ctrl Pts',(-13.9653471026424,34.0180416003109,28.4336965875645));
#52741=CARTESIAN_POINT('Ctrl Pts',(-13.9728082133453,34.0486781888914,28.4321524182671));
#52742=CARTESIAN_POINT('Ctrl Pts',(-13.9799109248485,34.0793838855029,28.4306082489697));
#52743=CARTESIAN_POINT('Ctrl Pts',(-14.015654940968,34.233908662999,28.4228372994904));
#52744=CARTESIAN_POINT('Ctrl Pts',(-14.0424112738778,34.3905837664468,28.4150663500111));
#52745=CARTESIAN_POINT('Ctrl Pts',(-14.0599741476013,34.5485191910954,28.4072954005318));
#52746=CARTESIAN_POINT('Ctrl Pts',(-14.0764805003541,34.6969537737527,28.399991924156));
#52747=CARTESIAN_POINT('Ctrl Pts',(-14.0848664953181,34.8465018450429,28.3926884477803));
#52748=CARTESIAN_POINT('Ctrl Pts',(-14.0849984180967,34.9964049829165,28.3853849714045));
#52749=CARTESIAN_POINT('Ctrl Pts',(-14.0849984180973,34.9964049836978,28.3853849713664));
#52750=CARTESIAN_POINT('Ctrl Pts',(-14.085102030525,35.1141392490068,28.3796488044156));
#52751=CARTESIAN_POINT('Ctrl Pts',(-14.0801115810811,35.2320158016211,28.3739126374648));
#52752=CARTESIAN_POINT('Ctrl Pts',(-14.0700169342151,35.3495527931545,28.368176470514));
#52753=CARTESIAN_POINT('Ctrl Pts',(-14.059929581389,35.4670048565564,28.3624444483174));
#52754=CARTESIAN_POINT('Ctrl Pts',(-14.0447454007801,35.5841174298377,28.3567124261208));
#52755=CARTESIAN_POINT('Ctrl Pts',(-14.0245063239988,35.7004097715579,28.3509804039242));
#52756=CARTESIAN_POINT('Ctrl Pts',(-14.0042749104805,35.8166580806968,28.3452505520831));
#52757=CARTESIAN_POINT('Ctrl Pts',(-13.9789924760443,35.9320863622645,28.3395207002421));
#52758=CARTESIAN_POINT('Ctrl Pts',(-13.9487526026871,36.0462207619676,28.3337908484011));
#52759=CARTESIAN_POINT('Ctrl Pts',(-13.9185165913529,36.1603405852314,28.3280617283363));
#52760=CARTESIAN_POINT('Ctrl Pts',(-13.8833245073619,36.2731664492456,28.3223326082715));
#52761=CARTESIAN_POINT('Ctrl Pts',(-13.8433204827315,36.3842372148646,28.3166034882066));
#52762=CARTESIAN_POINT('Ctrl Pts',(-13.8033115287939,36.495321666655,28.310873662198));
#52763=CARTESIAN_POINT('Ctrl Pts',(-13.7584895988473,36.6046501953671,28.3051438361894));
#52764=CARTESIAN_POINT('Ctrl Pts',(-13.7090476007998,36.7117800369793,28.2994140101808));
#52765=CARTESIAN_POINT('Ctrl Pts',(-13.6595570467352,36.8190150887092,28.2936785570223));
#52766=CARTESIAN_POINT('Ctrl Pts',(-13.6054375399421,36.9240467592881,28.2879431038639));
#52767=CARTESIAN_POINT('Ctrl Pts',(-13.5469287910702,37.0264553168223,28.2822076507054));
#52768=CARTESIAN_POINT('Ctrl Pts',(-13.4883905757711,37.1289154497938,28.2764693090334));
#52769=CARTESIAN_POINT('Ctrl Pts',(-13.4254589412614,37.2287494844963,28.2707309673615));
#52770=CARTESIAN_POINT('Ctrl Pts',(-13.358416910452,37.3255667815803,28.2649926256895));
#52771=CARTESIAN_POINT('Ctrl Pts',(-13.2912691757575,37.4225367286412,28.2592452364842));
#52772=CARTESIAN_POINT('Ctrl Pts',(-13.2199983543175,37.5164801034817,28.2534978472788));
#52773=CARTESIAN_POINT('Ctrl Pts',(-13.1449279379471,37.6070391759848,28.2477504580735));
#52774=CARTESIAN_POINT('Ctrl Pts',(-13.0830084573461,37.6817339892577,28.2430099041828));
#52775=CARTESIAN_POINT('Ctrl Pts',(-13.0185048127787,37.7541269409643,28.238269350292));
#52776=CARTESIAN_POINT('Ctrl Pts',(-12.9516163303101,37.8240371879008,28.2335287964012));
#52777=CARTESIAN_POINT('Ctrl Pts',(-12.8694458647662,37.9099197991524,28.2277051701839));
#52778=CARTESIAN_POINT('Ctrl Pts',(-12.7833914299211,37.9923515654202,28.2218815439666));
#52779=CARTESIAN_POINT('Ctrl Pts',(-12.6937743662288,38.0709615210629,28.2160579177493));
#52780=CARTESIAN_POINT('Ctrl Pts',(-12.6042703627787,38.1494723029516,28.2102416385769));
#52781=CARTESIAN_POINT('Ctrl Pts',(-12.511212974376,38.2241705973116,28.2044253594046));
#52782=CARTESIAN_POINT('Ctrl Pts',(-12.4149616736329,38.2947207946781,28.1986090802322));
#52783=CARTESIAN_POINT('Ctrl Pts',(-12.3188067164321,38.365200374236,28.1927986229129));
#52784=CARTESIAN_POINT('Ctrl Pts',(-12.2194645343185,38.431539876827,28.1869881655937));
#52785=CARTESIAN_POINT('Ctrl Pts',(-12.1173286397876,38.4934430625295,28.1811777082744));
#52786=CARTESIAN_POINT('Ctrl Pts',(-12.011327510028,38.5576889150802,28.175147359756));
#52787=CARTESIAN_POINT('Ctrl Pts',(-11.902317376978,38.6171557457961,28.1691170112376));
#52788=CARTESIAN_POINT('Ctrl Pts',(-11.7907727880757,38.6715606792599,28.1630866627192));
#52789=CARTESIAN_POINT('Ctrl Pts',(-11.6834165364236,38.723922786517,28.1572827450262));
#52790=CARTESIAN_POINT('Ctrl Pts',(-11.5737131275375,38.7715960814058,28.1514788273331));
#52791=CARTESIAN_POINT('Ctrl Pts',(-11.4621112314634,38.8143748828384,28.1456749096401));
#52792=CARTESIAN_POINT('Ctrl Pts',(-11.3505258184501,38.8571473660488,28.1398718491577));
#52793=CARTESIAN_POINT('Ctrl Pts',(-11.237042857048,38.8950266472981,28.1340687886753));
#52794=CARTESIAN_POINT('Ctrl Pts',(-11.122130356333,38.9278554534753,28.1282657281928));
#52795=CARTESIAN_POINT('Ctrl Pts',(-11.0072077091431,38.9606871583508,28.1224621553152));
#52796=CARTESIAN_POINT('Ctrl Pts',(-10.8908556643181,38.9884673893376,28.1166585824377));
#52797=CARTESIAN_POINT('Ctrl Pts',(-10.7735561008546,39.0110891237706,28.1108550095601));
#52798=CARTESIAN_POINT('Ctrl Pts',(-10.6562184984889,39.0337181941724,28.1050495546504));
#52799=CARTESIAN_POINT('Ctrl Pts',(-10.5379331671322,39.0511853638317,28.0992440997407));
#52800=CARTESIAN_POINT('Ctrl Pts',(-10.4191902130979,39.0634350696477,28.0934386448311));
#52801=CARTESIAN_POINT('Ctrl Pts',(-10.3003157660994,39.0756983404802,28.0876267611065));
#52802=CARTESIAN_POINT('Ctrl Pts',(-10.1809830913039,39.082732572781,28.0818148773819));
#52803=CARTESIAN_POINT('Ctrl Pts',(-10.0616855883498,39.0845342314871,28.0760029936573));
#52804=CARTESIAN_POINT('Ctrl Pts',(-9.94230973161859,39.0863370735102,28.0701872927276));
#52805=CARTESIAN_POINT('Ctrl Pts',(-9.8229694999585,39.0829005093515,28.0643715917978));
#52806=CARTESIAN_POINT('Ctrl Pts',(-9.70415479724293,39.0742730168713,28.0585558908681));
#52807=CARTESIAN_POINT('Ctrl Pts',(-9.58516991295967,39.0656331669962,28.0527318599499));
#52808=CARTESIAN_POINT('Ctrl Pts',(-9.46671246415969,39.0517875959597,28.0469078290317));
#52809=CARTESIAN_POINT('Ctrl Pts',(-9.34926391381397,39.0328361665378,28.0410837981136));
#52810=CARTESIAN_POINT('Ctrl Pts',(-9.31811080899898,39.0278093197573,28.03953898002));
#52811=CARTESIAN_POINT('Ctrl Pts',(-9.28702861156906,39.0224235141799,28.0379941619264));
#52812=CARTESIAN_POINT('Ctrl Pts',(-9.25602612783251,39.0166812018795,28.0364493438328));
#52813=CARTESIAN_POINT('Ctrl Pts',(-9.13915033330484,38.9950333455904,28.0306255574671));
#52814=CARTESIAN_POINT('Ctrl Pts',(-9.02303170445215,38.9682451382139,28.0248017711013));
#52815=CARTESIAN_POINT('Ctrl Pts',(-8.90815669635618,38.9363819936952,28.0189779847356));
#52816=CARTESIAN_POINT('Ctrl Pts',(-8.79342204162478,38.9045577793113,28.0131613138254));
#52817=CARTESIAN_POINT('Ctrl Pts',(-8.67992837610771,38.8676710665984,28.0073446429152));
#52818=CARTESIAN_POINT('Ctrl Pts',(-8.56815354267933,38.8258385646363,28.001527972005));
#52819=CARTESIAN_POINT('Ctrl Pts',(-8.45650821867766,38.7840545324699,27.9957180406594));
#52820=CARTESIAN_POINT('Ctrl Pts',(-8.34657814234692,38.7373362614064,27.9899081093138));
#52821=CARTESIAN_POINT('Ctrl Pts',(-8.23882666589127,38.6858504428726,27.9840981779682));
#52822=CARTESIAN_POINT('Ctrl Pts',(-8.13114729438493,38.6343990775311,27.9782921345026));
#52823=CARTESIAN_POINT('Ctrl Pts',(-8.02564399048193,38.5781866849026,27.972486091037));
#52824=CARTESIAN_POINT('Ctrl Pts',(-7.92276051150401,38.5174281950642,27.9666800475714));
#52825=CARTESIAN_POINT('Ctrl Pts',(-7.81992215509368,38.4566963526439,27.9608765505164));
#52826=CARTESIAN_POINT('Ctrl Pts',(-7.71970168852476,38.3914225871742,27.9550730534615));
#52827=CARTESIAN_POINT('Ctrl Pts',(-7.62251803980665,38.3218676266455,27.9492695564065));
#52828=CARTESIAN_POINT('Ctrl Pts',(-7.58550695103065,38.2953785530935,27.9470593724142));
#52829=CARTESIAN_POINT('Ctrl Pts',(-7.54893603282149,38.2682690112097,27.9448491884219));
#52830=CARTESIAN_POINT('Ctrl Pts',(-7.51282733495086,38.2405550657615,27.9426390044296));
#52831=CARTESIAN_POINT('',(-14.0849988977597,35.0030008835013,28.4896150285548));
#52832=CARTESIAN_POINT('Ctrl Pts',(-14.0849988977597,35.0030008835013,28.4896150285547));
#52833=CARTESIAN_POINT('Ctrl Pts',(-14.0848971430991,35.1415159828826,28.4828893615456));
#52834=CARTESIAN_POINT('Ctrl Pts',(-14.0777462435019,35.2797471812976,28.4761636945364));
#52835=CARTESIAN_POINT('Ctrl Pts',(-14.0636562889874,35.4170402438294,28.4694380275272));
#52836=CARTESIAN_POINT('Ctrl Pts',(-14.0494857339381,35.5551186810943,28.4626738868411));
#52837=CARTESIAN_POINT('Ctrl Pts',(-14.0282966187928,35.6922481018684,28.455909746155));
#52838=CARTESIAN_POINT('Ctrl Pts',(-14.0002502032237,35.8277821643456,28.4491456054689));
#52839=CARTESIAN_POINT('Ctrl Pts',(-13.9720233512023,35.9641881844296,28.4423379477228));
#52840=CARTESIAN_POINT('Ctrl Pts',(-13.93685076543,36.098978139626,28.4355302899768));
#52841=CARTESIAN_POINT('Ctrl Pts',(-13.8949451424515,36.2315142456721,28.4287226322307));
#52842=CARTESIAN_POINT('Ctrl Pts',(-13.8839506159381,36.2662869474801,28.4269365479713));
#52843=CARTESIAN_POINT('Ctrl Pts',(-13.8724928746765,36.3009046230714,28.4251504637118));
#52844=CARTESIAN_POINT('Ctrl Pts',(-13.86057629548,36.3353560075044,28.4233643794524));
#52845=CARTESIAN_POINT('Ctrl Pts',(-13.821720511137,36.4476898863606,28.4175405852529));
#52846=CARTESIAN_POINT('Ctrl Pts',(-13.7778950472024,36.5585074874179,28.4117167910535));
#52847=CARTESIAN_POINT('Ctrl Pts',(-13.7292372320862,36.6673375983352,28.405892996854));
#52848=CARTESIAN_POINT('Ctrl Pts',(-13.6806407930243,36.776030432994,28.4000765486791));
#52849=CARTESIAN_POINT('Ctrl Pts',(-13.6272242916691,36.8827403943895,28.3942601005043));
#52850=CARTESIAN_POINT('Ctrl Pts',(-13.5691744603437,36.9870124991127,28.3884436523295));
#52851=CARTESIAN_POINT('Ctrl Pts',(-13.5111827247524,37.0911802492783,28.3826330252022));
#52852=CARTESIAN_POINT('Ctrl Pts',(-13.4485670813968,37.1929146417315,28.3768223980748));
#52853=CARTESIAN_POINT('Ctrl Pts',(-13.3815616213169,37.2917822761415,28.3710117709475));
#52854=CARTESIAN_POINT('Ctrl Pts',(-13.3120231664601,37.3943873850987,28.3649814857782));
#52855=CARTESIAN_POINT('Ctrl Pts',(-13.2377566335247,37.4939043067719,28.3589512006089));
#52856=CARTESIAN_POINT('Ctrl Pts',(-13.1590752998962,37.589878037589,28.3529209154396));
#52857=CARTESIAN_POINT('Ctrl Pts',(-13.0833453131256,37.6822517815245,28.347116827036));
#52858=CARTESIAN_POINT('Ctrl Pts',(-13.0035260420673,37.7713430141043,28.3413127386323));
#52859=CARTESIAN_POINT('Ctrl Pts',(-12.9199394797829,37.8567776312491,28.3355086502287));
#52860=CARTESIAN_POINT('Ctrl Pts',(-12.8363652619942,37.9421996309679,28.3297054190029));
#52861=CARTESIAN_POINT('Ctrl Pts',(-12.7490251448956,38.023965797424,28.323902187777));
#52862=CARTESIAN_POINT('Ctrl Pts',(-12.6582788901612,38.1017379551025,28.3180989565512));
#52863=CARTESIAN_POINT('Ctrl Pts',(-12.5675246254377,38.1795169775727,28.3122952130858));
#52864=CARTESIAN_POINT('Ctrl Pts',(-12.4733639353473,38.2533010246102,28.3064914696205));
#52865=CARTESIAN_POINT('Ctrl Pts',(-12.3761901484246,38.3227918048728,28.3006877261551));
#52866=CARTESIAN_POINT('Ctrl Pts',(-12.2789848558491,38.3923051154131,28.294882101002));
#52867=CARTESIAN_POINT('Ctrl Pts',(-12.178764855543,38.4575221534938,28.2890764758488));
#52868=CARTESIAN_POINT('Ctrl Pts',(-12.075952419332,38.5181879643745,28.2832708506957));
#52869=CARTESIAN_POINT('Ctrl Pts',(-11.9730261588869,38.5789209387202,28.2774587981019));
#52870=CARTESIAN_POINT('Ctrl Pts',(-11.8675020854263,38.6350924205865,28.2716467455081));
#52871=CARTESIAN_POINT('Ctrl Pts',(-11.7598271671377,38.6864933665754,28.2658346929142));
#52872=CARTESIAN_POINT('Ctrl Pts',(-11.6520815419422,38.7379280660322,28.2600188237188));
#52873=CARTESIAN_POINT('Ctrl Pts',(-11.5421826340632,38.7845858316132,28.2542029545235));
#52874=CARTESIAN_POINT('Ctrl Pts',(-11.4305959321059,38.8263063493455,28.2483870853281));
#52875=CARTESIAN_POINT('Ctrl Pts',(-11.3188494477517,38.86808660721,28.2425628883167));
#52876=CARTESIAN_POINT('Ctrl Pts',(-11.2054107325405,38.9049153808315,28.2367386913053));
#52877=CARTESIAN_POINT('Ctrl Pts',(-11.0907590392455,38.9366825777937,28.230914494294));
#52878=CARTESIAN_POINT('Ctrl Pts',(-11.060380731773,38.9450996682798,28.2293713051573));
#52879=CARTESIAN_POINT('Ctrl Pts',(-11.0299173130036,38.9531616924201,28.2278281160206));
#52880=CARTESIAN_POINT('Ctrl Pts',(-10.9993777804663,38.960867209578,28.226284926884));
#52881=CARTESIAN_POINT('Ctrl Pts',(-10.884120738893,38.9899480447325,28.2204608883444));
#52882=CARTESIAN_POINT('Ctrl Pts',(-10.7674075153923,39.0140407957942,28.2146368498048));
#52883=CARTESIAN_POINT('Ctrl Pts',(-10.6497075664999,39.0330019933088,28.2088128112652));
#52884=CARTESIAN_POINT('Ctrl Pts',(-10.5321577796459,39.0519390000562,28.2029962030559));
#52885=CARTESIAN_POINT('Ctrl Pts',(-10.4136241710923,39.0657574111683,28.1971795948466));
#52886=CARTESIAN_POINT('Ctrl Pts',(-10.2945896878623,39.074363989116,28.1913629866373));
#52887=CARTESIAN_POINT('Ctrl Pts',(-10.171460887861,39.0832665994022,28.1853463100453));
#52888=CARTESIAN_POINT('Ctrl Pts',(-10.0477965568257,39.086592258203,28.1793296334533));
#52889=CARTESIAN_POINT('Ctrl Pts',(-9.92414171060296,39.0842955965417,28.1733129568613));
#52890=CARTESIAN_POINT('Ctrl Pts',(-9.80481591212125,39.0820793389913,28.1675069188412));
#52891=CARTESIAN_POINT('Ctrl Pts',(-9.68549939383176,39.0746278174157,28.1617008808211));
#52892=CARTESIAN_POINT('Ctrl Pts',(-9.56668511033785,39.0619531270556,28.1558948428009));
#52893=CARTESIAN_POINT('Ctrl Pts',(-9.44791893666366,39.0492835688821,28.1500911557392));
#52894=CARTESIAN_POINT('Ctrl Pts',(-9.32965499864144,39.0313950916617,28.1442874686775));
#52895=CARTESIAN_POINT('Ctrl Pts',(-9.21238261929791,39.0083517637074,28.1384837816158));
#52896=CARTESIAN_POINT('Ctrl Pts',(-9.09513005178673,38.9853123286608,28.1326810750209));
#52897=CARTESIAN_POINT('Ctrl Pts',(-8.97886910998498,38.9571198547666,28.126878368426));
#52898=CARTESIAN_POINT('Ctrl Pts',(-8.86407975983748,38.9238896783662,28.1210756618311));
#52899=CARTESIAN_POINT('Ctrl Pts',(-8.74928271508907,38.8906572744688,28.1152725662671));
#52900=CARTESIAN_POINT('Ctrl Pts',(-8.63595784977484,38.8523866115704,28.1094694707031));
#52901=CARTESIAN_POINT('Ctrl Pts',(-8.52457016431055,38.8092429431525,28.1036663751391));
#52902=CARTESIAN_POINT('Ctrl Pts',(-8.41310151663988,38.7660679157333,28.0978590615916));
#52903=CARTESIAN_POINT('Ctrl Pts',(-8.30357324099135,38.7180129588992,28.092051748044));
#52904=CARTESIAN_POINT('Ctrl Pts',(-8.19643051481694,38.6652915453094,28.0862444344965));
#52905=CARTESIAN_POINT('Ctrl Pts',(-8.08924103627097,38.6125471264144,28.0804345868929));
#52906=CARTESIAN_POINT('Ctrl Pts',(-7.9844395396861,38.5551323885469,28.0746247392892));
#52907=CARTESIAN_POINT('Ctrl Pts',(-7.88244548988597,38.4933061555918,28.0688148916856));
#52908=CARTESIAN_POINT('Ctrl Pts',(-7.78033800943058,38.4314111638206,28.0629985827754));
#52909=CARTESIAN_POINT('Ctrl Pts',(-7.68104454798937,38.3650951086807,28.0571822738652));
#52910=CARTESIAN_POINT('Ctrl Pts',(-7.5849545492095,38.2946593861302,28.0513659649551));
#52911=CARTESIAN_POINT('Ctrl Pts',(-7.5607063489003,38.2768850128238,28.0498982261133));
#52912=CARTESIAN_POINT('Ctrl Pts',(-7.53666197551205,38.2588484955234,28.0484304872715));
#52913=CARTESIAN_POINT('Ctrl Pts',(-7.51282733495086,38.2405550657615,28.0469627484298));
#52914=CARTESIAN_POINT('Ctrl Pts',(-7.51282733495086,38.2405550657615,29.2969304734038));
#52915=CARTESIAN_POINT('Ctrl Pts',(-7.41787327012908,38.1676764540214,29.291116388497));
#52916=CARTESIAN_POINT('Ctrl Pts',(-7.32614665447589,38.0906374940038,29.2853023035901));
#52917=CARTESIAN_POINT('Ctrl Pts',(-7.23801898436614,38.0097650853976,29.2794882186833));
#52918=CARTESIAN_POINT('Ctrl Pts',(-7.14979912665956,37.9288080786964,29.2736680518442));
#52919=CARTESIAN_POINT('Ctrl Pts',(-7.06518603454948,37.8440098891537,29.2678478850052));
#52920=CARTESIAN_POINT('Ctrl Pts',(-6.98451504536394,37.7557350178062,29.2620277181661));
#52921=CARTESIAN_POINT('Ctrl Pts',(-6.90380113162585,37.6674131759258,29.256204454451));
#52922=CARTESIAN_POINT('Ctrl Pts',(-6.82703376120211,37.5756112782869,29.2503811907358));
#52923=CARTESIAN_POINT('Ctrl Pts',(-6.75450747661353,37.4807263615003,29.2445579270207));
#52924=CARTESIAN_POINT('Ctrl Pts',(-6.68186468771735,37.38568902409,29.2387253089685));
#52925=CARTESIAN_POINT('Ctrl Pts',(-6.61347683034987,37.287559105778,29.2328926909164));
#52926=CARTESIAN_POINT('Ctrl Pts',(-6.54959499587365,37.1867625173987,29.2270600728643));
#52927=CARTESIAN_POINT('Ctrl Pts',(-6.49345283258686,37.0981780462428,29.2219341118182));
#52928=CARTESIAN_POINT('Ctrl Pts',(-6.44079037335608,37.0075344876291,29.2168081507722));
#52929=CARTESIAN_POINT('Ctrl Pts',(-6.39174780557274,36.9151347475859,29.2116821897262));
#52930=CARTESIAN_POINT('Ctrl Pts',(-6.33608961750155,36.8102707010749,29.2058647597498));
#52931=CARTESIAN_POINT('Ctrl Pts',(-6.28491498682052,36.7028056730188,29.2000473297733));
#52932=CARTESIAN_POINT('Ctrl Pts',(-6.23847551375534,36.5931599227265,29.1942298997969));
#52933=CARTESIAN_POINT('Ctrl Pts',(-6.19209531410575,36.4836541197182,29.1884198949466));
#52934=CARTESIAN_POINT('Ctrl Pts',(-6.15043841006421,36.3719735037468,29.1826098900963));
#52935=CARTESIAN_POINT('Ctrl Pts',(-6.11371091804858,36.2585635349498,29.176799885246));
#52936=CARTESIAN_POINT('Ctrl Pts',(-6.07702067142689,36.1452685753388,29.1709957723286));
#52937=CARTESIAN_POINT('Ctrl Pts',(-6.04525001802544,36.0302481386786,29.1651916594112));
#52938=CARTESIAN_POINT('Ctrl Pts',(-6.01855704784319,35.9139677339605,29.1593875464938));
#52939=CARTESIAN_POINT('Ctrl Pts',(-5.99081280959456,35.7931077760719,29.1533548461048));
#52940=CARTESIAN_POINT('Ctrl Pts',(-5.96855459914305,35.6708869823752,29.1473221457158));
#52941=CARTESIAN_POINT('Ctrl Pts',(-5.95190294454598,35.5478459907898,29.1412894453268));
#52942=CARTESIAN_POINT('Ctrl Pts',(-5.9359006682298,35.4296033300327,29.1354920071206));
#52943=CARTESIAN_POINT('Ctrl Pts',(-5.92507592136629,35.3106036875415,29.1296945689144));
#52944=CARTESIAN_POINT('Ctrl Pts',(-5.91948345438878,35.1913366692327,29.1238971307082));
#52945=CARTESIAN_POINT('Ctrl Pts',(-5.91389185178974,35.0720880849788,29.1181005885611));
#52946=CARTESIAN_POINT('Ctrl Pts',(-5.91353094007082,34.9525726158708,29.112304046414));
#52947=CARTESIAN_POINT('Ctrl Pts',(-5.91840344120809,34.8332830804685,29.1065075042668));
#52948=CARTESIAN_POINT('Ctrl Pts',(-5.92327634618274,34.7139836582398,29.100710481697));
#52949=CARTESIAN_POINT('Ctrl Pts',(-5.93338350962639,34.5949106159771,29.0949134591271));
#52950=CARTESIAN_POINT('Ctrl Pts',(-5.94867558759209,34.476554200105,29.0891164365572));
#52951=CARTESIAN_POINT('Ctrl Pts',(-5.96397256395702,34.3581598719899,29.0833175570696));
#52952=CARTESIAN_POINT('Ctrl Pts',(-5.98445770525062,34.2404830325342,29.077518677582));
#52953=CARTESIAN_POINT('Ctrl Pts',(-6.01003022317322,34.1240056050357,29.0717197980944));
#52954=CARTESIAN_POINT('Ctrl Pts',(-6.03563107169448,34.0073991376334,29.0659144942989));
#52955=CARTESIAN_POINT('Ctrl Pts',(-6.06633045893937,33.8919951345671,29.0601091905035));
#52956=CARTESIAN_POINT('Ctrl Pts',(-6.10197716192871,33.7782623219878,29.054303886708));
#52957=CARTESIAN_POINT('Ctrl Pts',(-6.1376472397103,33.664454930818,29.0484947761714));
#52958=CARTESIAN_POINT('Ctrl Pts',(-6.17827095449689,33.5523212964051,29.0426856656348));
#52959=CARTESIAN_POINT('Ctrl Pts',(-6.22364879898165,33.4423104909619,29.0368765550983));
#52960=CARTESIAN_POINT('Ctrl Pts',(-6.26909198485532,33.3321412765219,29.0310590797891));
#52961=CARTESIAN_POINT('Ctrl Pts',(-6.31930279186957,33.2241013619347,29.0252416044799));
#52962=CARTESIAN_POINT('Ctrl Pts',(-6.37403557954917,33.1186156635008,29.0194241291707));
#52963=CARTESIAN_POINT('Ctrl Pts',(-6.38915601188665,33.0894742761649,29.0178169984997));
#52964=CARTESIAN_POINT('Ctrl Pts',(-6.40462130285063,33.0605276540963,29.0162098678287));
#52965=CARTESIAN_POINT('Ctrl Pts',(-6.42042570108141,33.0317843516216,29.0146027371578));
#52966=CARTESIAN_POINT('Ctrl Pts',(-6.47770523441605,32.927610631863,29.0087780487706));
#52967=CARTESIAN_POINT('Ctrl Pts',(-6.53962822579674,32.8257718442912,29.0029533603834));
#52968=CARTESIAN_POINT('Ctrl Pts',(-6.60597959959592,32.7267093187098,28.9971286719963));
#52969=CARTESIAN_POINT('Ctrl Pts',(-6.67224730713684,32.6277717067568,28.9913113282932));
#52970=CARTESIAN_POINT('Ctrl Pts',(-6.74293206540356,32.5316037299637,28.9854939845902));
#52971=CARTESIAN_POINT('Ctrl Pts',(-6.81777285021209,32.43862236928,28.9796766408872));
#52972=CARTESIAN_POINT('Ctrl Pts',(-6.89253874937611,32.3457340456902,28.9738651180148));
#52973=CARTESIAN_POINT('Ctrl Pts',(-6.9714521476959,32.25602631111,28.9680535951424));
#52974=CARTESIAN_POINT('Ctrl Pts',(-7.05420899246627,32.1698868679974,28.96224207227));
#52975=CARTESIAN_POINT('Ctrl Pts',(-7.14007626075387,32.0805098661021,28.9562121227833));
#52976=CARTESIAN_POINT('Ctrl Pts',(-7.2300813083146,31.9949750204064,28.9501821732966));
#52977=CARTESIAN_POINT('Ctrl Pts',(-7.32383862184878,31.9136777099448,28.9441522238099));
#52978=CARTESIAN_POINT('Ctrl Pts',(-7.41409795379706,31.8354135121466,28.9383472450639));
#52979=CARTESIAN_POINT('Ctrl Pts',(-7.50783424477259,31.7610766086199,28.9325422663178));
#52980=CARTESIAN_POINT('Ctrl Pts',(-7.60466683284577,31.6909814116069,28.9267372875718));
#52981=CARTESIAN_POINT('Ctrl Pts',(-7.70148506252334,31.6208966083528,28.9209331695916));
#52982=CARTESIAN_POINT('Ctrl Pts',(-7.80139834570489,31.5550525000547,28.9151290516114));
#52983=CARTESIAN_POINT('Ctrl Pts',(-7.9039948635413,31.4937217070035,28.9093249336312));
#52984=CARTESIAN_POINT('Ctrl Pts',(-8.00660035487121,31.4323855497207,28.903520308));
#52985=CARTESIAN_POINT('Ctrl Pts',(-8.11188919711753,31.3755637019829,28.8977156823689));
#52986=CARTESIAN_POINT('Ctrl Pts',(-8.21942322233681,31.3234838040821,28.8919110567378));
#52987=CARTESIAN_POINT('Ctrl Pts',(-8.3269920032866,31.271387073603,28.8861045550121));
#52988=CARTESIAN_POINT('Ctrl Pts',(-8.43680704323431,31.2240355188569,28.8802980532863));
#52989=CARTESIAN_POINT('Ctrl Pts',(-8.54840896352329,31.1816091788791,28.8744915515606));
#52990=CARTESIAN_POINT('Ctrl Pts',(-8.66013417455606,31.1391359689639,28.868678635179));
#52991=CARTESIAN_POINT('Ctrl Pts',(-8.7736498245319,31.1015989798057,28.8628657187974));
#52992=CARTESIAN_POINT('Ctrl Pts',(-8.88847994430274,31.0691288286459,28.8570528024157));
#52993=CARTESIAN_POINT('Ctrl Pts',(-9.00338533099471,31.036637394496,28.8512360758812));
#52994=CARTESIAN_POINT('Ctrl Pts',(-9.11960650702794,31.0092195060462,28.8454193493466));
#52995=CARTESIAN_POINT('Ctrl Pts',(-9.23665747217893,30.986954624575,28.839602622812));
#52996=CARTESIAN_POINT('Ctrl Pts',(-9.35387569657673,30.9646579278403,28.8337775845024));
#52997=CARTESIAN_POINT('Ctrl Pts',(-9.47192567423361,30.9475289934098,28.8279525461927));
#52998=CARTESIAN_POINT('Ctrl Pts',(-9.59031631377747,30.9355954584659,28.822127507883));
#52999=CARTESIAN_POINT('Ctrl Pts',(-9.62150906658929,30.932451292617,28.8205927667851));
#53000=CARTESIAN_POINT('Ctrl Pts',(-9.65272546992431,30.9296675006439,28.8190580256872));
#53001=CARTESIAN_POINT('Ctrl Pts',(-9.68395656233487,30.927243986499,28.8175232845893));
#53002=CARTESIAN_POINT('Ctrl Pts',(-9.80248275775051,30.9180464244235,28.8116987357426));
#53003=CARTESIAN_POINT('Ctrl Pts',(-9.92160116571264,30.9140124436722,28.8058741868959));
#53004=CARTESIAN_POINT('Ctrl Pts',(-10.0408247702119,30.9152040028739,28.8000496380493));
#53005=CARTESIAN_POINT('Ctrl Pts',(-10.1598983591033,30.9163940627712,28.7942324180637));
#53006=CARTESIAN_POINT('Ctrl Pts',(-10.2790764766751,30.9227965806436,28.7884151980781));
#53007=CARTESIAN_POINT('Ctrl Pts',(-10.3978672944792,30.9344217365812,28.7825979780924));
#53008=CARTESIAN_POINT('Ctrl Pts',(-10.5165395726682,30.9460352919461,28.7767865630254));
#53009=CARTESIAN_POINT('Ctrl Pts',(-10.6348249160352,30.9628610779299,28.7709751479583));
#53010=CARTESIAN_POINT('Ctrl Pts',(-10.7522324076423,30.9848572372962,28.7651637328912));
#53011=CARTESIAN_POINT('Ctrl Pts',(-10.874055867381,31.0076807232449,28.7591337370216));
#53012=CARTESIAN_POINT('Ctrl Pts',(-10.9949336946401,31.0360711550509,28.753103741152));
#53013=CARTESIAN_POINT('Ctrl Pts',(-11.1143238744396,31.0699227357654,28.7470737452824));
#53014=CARTESIAN_POINT('Ctrl Pts',(-11.2292575272157,31.1025107244114,28.741268833583));
#53015=CARTESIAN_POINT('Ctrl Pts',(-11.3428121747645,31.1401593453216,28.7354639218835));
#53016=CARTESIAN_POINT('Ctrl Pts',(-11.4545162236956,31.1827224943677,28.7296590101841));
#53017=CARTESIAN_POINT('Ctrl Pts',(-11.5662040024583,31.2252794439107,28.7238549439946));
#53018=CARTESIAN_POINT('Ctrl Pts',(-11.6760413373258,31.2727493527382,28.7180508778052));
#53019=CARTESIAN_POINT('Ctrl Pts',(-11.7835745203653,31.324937152877,28.7122468116158));
#53020=CARTESIAN_POINT('Ctrl Pts',(-11.8911173938996,31.3771296559883,28.7064422223852));
#53021=CARTESIAN_POINT('Ctrl Pts',(-11.9963553355207,31.4340407175232,28.7006376331547));
#53022=CARTESIAN_POINT('Ctrl Pts',(-12.0988578243006,31.4954285806432,28.6948330439242));
#53023=CARTESIAN_POINT('Ctrl Pts',(-12.2013937171359,31.5568364491661,28.6890265630633));
#53024=CARTESIAN_POINT('Ctrl Pts',(-12.3011920342285,31.6227238111686,28.6832200822024));
#53025=CARTESIAN_POINT('Ctrl Pts',(-12.3978504501752,31.6928050830659,28.6774136013415));
#53026=CARTESIAN_POINT('Ctrl Pts',(-12.4946160366207,31.7629640579216,28.6716006825161));
#53027=CARTESIAN_POINT('Ctrl Pts',(-12.588234442121,31.8373259847854,28.6657877636907));
#53028=CARTESIAN_POINT('Ctrl Pts',(-12.6783355901023,31.9155643195567,28.6599748448653));
#53029=CARTESIAN_POINT('Ctrl Pts',(-12.76849600687,31.993854119723,28.6541581022857));
#53030=CARTESIAN_POINT('Ctrl Pts',(-12.855134262889,32.076025125808,28.6483413597061));
#53031=CARTESIAN_POINT('Ctrl Pts',(-12.9379175774703,32.1617143716689,28.6425246171265));
#53032=CARTESIAN_POINT('Ctrl Pts',(-13.020819468138,32.2475263559762,28.6366995428368));
#53033=CARTESIAN_POINT('Ctrl Pts',(-13.0998551268564,32.3368663338371,28.6308744685472));
#53034=CARTESIAN_POINT('Ctrl Pts',(-13.1747323336447,32.4293386824183,28.6250493942576));
#53035=CARTESIAN_POINT('Ctrl Pts',(-13.1944660811659,32.4537095965838,28.6235142068454));
#53036=CARTESIAN_POINT('Ctrl Pts',(-13.2139112289294,32.4782979258235,28.6219790194332));
#53037=CARTESIAN_POINT('Ctrl Pts',(-13.2330629426428,32.5030961154041,28.6204438320209));
#53038=CARTESIAN_POINT('Ctrl Pts',(-13.30569343614,32.5971401667112,28.6146218246001));
#53039=CARTESIAN_POINT('Ctrl Pts',(-13.3743387912988,32.6945133666739,28.6087998171793));
#53040=CARTESIAN_POINT('Ctrl Pts',(-13.4386788632778,32.7948440700834,28.6029778097585));
#53041=CARTESIAN_POINT('Ctrl Pts',(-13.5029393080696,32.8950506043481,28.5971630076463));
#53042=CARTESIAN_POINT('Ctrl Pts',(-13.5629048454414,32.9982070248374,28.5913482055341));
#53043=CARTESIAN_POINT('Ctrl Pts',(-13.6182957135303,33.1039089870346,28.5855334034219));
#53044=CARTESIAN_POINT('Ctrl Pts',(-13.6736310844335,33.2095050443844,28.5797244272729));
#53045=CARTESIAN_POINT('Ctrl Pts',(-13.7244007130429,33.3176412124539,28.5739154511238));
#53046=CARTESIAN_POINT('Ctrl Pts',(-13.7703686407808,33.4278850828846,28.5681064749747));
#53047=CARTESIAN_POINT('Ctrl Pts',(-13.8163013438007,33.5380444746485,28.5623019501802));
#53048=CARTESIAN_POINT('Ctrl Pts',(-13.8574395091137,33.6503079807764,28.5564974253857));
#53049=CARTESIAN_POINT('Ctrl Pts',(-13.8935938540381,33.7642201248616,28.5506929005912));
#53050=CARTESIAN_POINT('Ctrl Pts',(-13.9297310874388,33.8780783553618,28.5448911230257));
#53051=CARTESIAN_POINT('Ctrl Pts',(-13.9608890686761,33.9935832837857,28.5390893454601));
#53052=CARTESIAN_POINT('Ctrl Pts',(-13.9869274552809,34.1102615742101,28.5332875678946));
#53053=CARTESIAN_POINT('Ctrl Pts',(-14.012958527511,34.2269070888423,28.5274874200912));
#53054=CARTESIAN_POINT('Ctrl Pts',(-14.0338727805242,34.3447249111311,28.5216872722878));
#53055=CARTESIAN_POINT('Ctrl Pts',(-14.0495805146343,34.463229420055,28.5158871244843));
#53056=CARTESIAN_POINT('Ctrl Pts',(-14.0652908308943,34.5817534095995,28.510086023211));
#53057=CARTESIAN_POINT('Ctrl Pts',(-14.0757928630313,34.700963906997,28.5042849219377));
#53058=CARTESIAN_POINT('Ctrl Pts',(-14.081048575542,34.8203683656302,28.4984838206644));
#53059=CARTESIAN_POINT('Ctrl Pts',(-14.0837269073067,34.881217347334,28.4955275566415));
#53060=CARTESIAN_POINT('Ctrl Pts',(-14.0850436239649,34.9421166306784,28.4925712926185));
#53061=CARTESIAN_POINT('Ctrl Pts',(-14.0849988977603,35.0030008826619,28.4896150285955));
#53062=CARTESIAN_POINT('Origin',(130.,35.,23.));
#53063=CARTESIAN_POINT('',(126.610250000496,35.0000579986539,27.6441866060966));
#53064=CARTESIAN_POINT('Ctrl Pts',(126.821241918358,36.1772434416436,28.8235740826546));
#53065=CARTESIAN_POINT('Ctrl Pts',(126.833574096516,36.2105424260322,28.821437007519));
#53066=CARTESIAN_POINT('Ctrl Pts',(126.846428242073,36.2436442112275,28.819272610919));
#53067=CARTESIAN_POINT('Ctrl Pts',(126.914370492875,36.4107779264545,28.808161660815));
#53068=CARTESIAN_POINT('Ctrl Pts',(126.977489366515,36.54137167997,28.7988833094481));
#53069=CARTESIAN_POINT('Ctrl Pts',(127.181891381596,36.9031307712913,28.7721256404083));
#53070=CARTESIAN_POINT('Ctrl Pts',(127.342781788506,37.1219994400736,28.7546975621398));
#53071=CARTESIAN_POINT('Ctrl Pts',(127.561297458281,37.354888726488,28.7353266802008));
#53072=CARTESIAN_POINT('Ctrl Pts',(127.595340568098,37.3896410578469,28.7324073475024));
#53073=CARTESIAN_POINT('Ctrl Pts',(127.651025034136,37.4440901040894,28.7277844298354));
#53074=CARTESIAN_POINT('Ctrl Pts',(127.672192882417,37.4642593066907,28.7260606699848));
#53075=CARTESIAN_POINT('Ctrl Pts',(127.713169923754,37.5023039290061,28.7227862196759));
#53076=CARTESIAN_POINT('Ctrl Pts',(127.732934307613,37.5202241878357,28.721233706764));
#53077=CARTESIAN_POINT('Ctrl Pts',(127.779220503777,37.561206463623,28.7176581506043));
#53078=CARTESIAN_POINT('Ctrl Pts',(127.805893764433,37.584093279777,28.7156423451266));
#53079=CARTESIAN_POINT('Ctrl Pts',(127.894978973599,37.6581582332843,28.7090497772128));
#53080=CARTESIAN_POINT('Ctrl Pts',(127.958864831683,37.7075242034752,28.7045437604119));
#53081=CARTESIAN_POINT('Ctrl Pts',(128.12188887874,37.8244432791715,28.6935122432114));
#53082=CARTESIAN_POINT('Ctrl Pts',(128.222964918218,37.889105410943,28.6870785000955));
#53083=CARTESIAN_POINT('Ctrl Pts',(128.540674672581,38.06936184029,28.6676419050387));
#53084=CARTESIAN_POINT('Ctrl Pts',(128.766579897165,38.1669005061827,28.6549012043865));
#53085=CARTESIAN_POINT('Ctrl Pts',(129.034181054551,38.2494314344403,28.6390804729221));
#53086=CARTESIAN_POINT('Ctrl Pts',(129.067517663182,38.2591543963013,28.6370964543856));
#53087=CARTESIAN_POINT('Ctrl Pts',(129.118425341683,38.2731571817028,28.6340386777282));
#53088=CARTESIAN_POINT('Ctrl Pts',(129.135891951924,38.277811627241,28.6329845693424));
#53089=CARTESIAN_POINT('Ctrl Pts',(129.167868336798,38.2860592486628,28.6310443448697));
#53090=CARTESIAN_POINT('Ctrl Pts',(129.182365836565,38.2896964661152,28.6301606694589));
#53091=CARTESIAN_POINT('Ctrl Pts',(129.216088875176,38.2979204135607,28.6280959715622));
#53092=CARTESIAN_POINT('Ctrl Pts',(129.235330919935,38.3024349898655,28.6269111191426));
#53093=CARTESIAN_POINT('Ctrl Pts',(129.298619744966,38.3167010710799,28.6229943712998));
#53094=CARTESIAN_POINT('Ctrl Pts',(129.342820124311,38.3257411883443,28.6202278372197));
#53095=CARTESIAN_POINT('Ctrl Pts',(129.452582019679,38.3459168903911,28.6133024222603));
#53096=CARTESIAN_POINT('Ctrl Pts',(129.518315040751,38.3560102788485,28.6091067580621));
#53097=CARTESIAN_POINT('Ctrl Pts',(129.856441550266,38.3977917206956,28.5874072431919));
#53098=CARTESIAN_POINT('Ctrl Pts',(130.131704953603,38.3982765411878,28.5694624413171));
#53099=CARTESIAN_POINT('Ctrl Pts',(130.489228049749,38.3553577860524,28.5470864165132));
#53100=CARTESIAN_POINT('Ctrl Pts',(130.57402109284,38.3418964197762,28.541839332944));
#53101=CARTESIAN_POINT('Ctrl Pts',(130.690782750783,38.3187838572289,28.5346981223825));
#53102=CARTESIAN_POINT('Ctrl Pts',(130.723252208328,38.3118595170262,28.532721252984));
#53103=CARTESIAN_POINT('Ctrl Pts',(130.779656462399,38.2989618134617,28.5293018560984));
#53104=CARTESIAN_POINT('Ctrl Pts',(130.803637074221,38.2932022025586,28.5278527470299));
#53105=CARTESIAN_POINT('Ctrl Pts',(130.854017546788,38.2805188375112,28.5248174606695));
#53106=CARTESIAN_POINT('Ctrl Pts',(130.88040103618,38.2735369087089,28.5232332466146));
#53107=CARTESIAN_POINT('Ctrl Pts',(130.944230241851,38.2558181063316,28.5194120346597));
#53108=CARTESIAN_POINT('Ctrl Pts',(130.981581228048,38.2447528042198,28.5171856439566));
#53109=CARTESIAN_POINT('Ctrl Pts',(131.122653691527,38.20030080222,28.5088047971692));
#53110=CARTESIAN_POINT('Ctrl Pts',(131.224939304439,38.1625627722472,28.5027890182928));
#53111=CARTESIAN_POINT('Ctrl Pts',(131.510649137383,38.0412044530307,28.4859461301745));
#53112=CARTESIAN_POINT('Ctrl Pts',(131.688668891005,37.9460792807847,28.4754226666234));
#53113=CARTESIAN_POINT('Ctrl Pts',(131.972756390827,37.7600220255037,28.4572814280134));
#53114=CARTESIAN_POINT('Ctrl Pts',(132.083576931231,37.677347357494,28.4497979678272));
#53115=CARTESIAN_POINT('Ctrl Pts',(132.210561844483,37.5699448278629,28.4403258518178));
#53116=CARTESIAN_POINT('Ctrl Pts',(132.231861511741,37.551469021785,28.438704312997));
#53117=CARTESIAN_POINT('Ctrl Pts',(132.265256998767,37.5217628939599,28.436104913713));
#53118=CARTESIAN_POINT('Ctrl Pts',(132.277505987065,37.5107058405614,28.4351390354572));
#53119=CARTESIAN_POINT('Ctrl Pts',(132.301013279964,37.4891724410913,28.4332600638386));
#53120=CARTESIAN_POINT('Ctrl Pts',(132.312281799851,37.4787082119455,28.4323478046554));
#53121=CARTESIAN_POINT('Ctrl Pts',(132.340106719763,37.4525144521483,28.4300671027297));
#53122=CARTESIAN_POINT('Ctrl Pts',(132.356575955877,37.4366937230096,28.4286921179166));
#53123=CARTESIAN_POINT('Ctrl Pts',(132.420583871252,37.3739503793387,28.4232534288863));
#53124=CARTESIAN_POINT('Ctrl Pts',(132.466888591852,37.3257958111954,28.4191104930551));
#53125=CARTESIAN_POINT('Ctrl Pts',(132.592813814293,37.1868466740585,28.4073173935482));
#53126=CARTESIAN_POINT('Ctrl Pts',(132.669049190715,37.0931210438606,28.3995479409319));
#53127=CARTESIAN_POINT('Ctrl Pts',(132.884966326899,36.7966396200247,28.375907466975));
#53128=CARTESIAN_POINT('Ctrl Pts',(133.007750641083,36.5825347719095,28.3601290816689));
#53129=CARTESIAN_POINT('Ctrl Pts',(133.126738615134,36.3101613862715,28.3420566371341));
#53130=CARTESIAN_POINT('Ctrl Pts',(133.146137795041,36.2628676199947,28.3389830676894));
#53131=CARTESIAN_POINT('Ctrl Pts',(133.175222075742,36.1871271972444,28.3341601121192));
#53132=CARTESIAN_POINT('Ctrl Pts',(133.185610797525,36.1589608044419,28.3323879069868));
#53133=CARTESIAN_POINT('Ctrl Pts',(133.204464349062,36.1056743196671,28.3290741357947));
#53134=CARTESIAN_POINT('Ctrl Pts',(133.213011305906,36.0805858931559,28.3275299912826));
#53135=CARTESIAN_POINT('Ctrl Pts',(133.231747720515,36.0233990757995,28.3240453554249));
#53136=CARTESIAN_POINT('Ctrl Pts',(133.241754947344,35.9912436506845,28.3221108586675));
#53137=CARTESIAN_POINT('Ctrl Pts',(133.271595996234,35.8900680921034,28.3160972431502));
#53138=CARTESIAN_POINT('Ctrl Pts',(133.289717518608,35.8205615243723,28.3120721663896));
#53139=CARTESIAN_POINT('Ctrl Pts',(133.327957934295,35.6521358445925,28.302527182361));
#53140=CARTESIAN_POINT('Ctrl Pts',(133.345894348628,35.5527911204698,28.2970678938955));
#53141=CARTESIAN_POINT('Ctrl Pts',(133.376399624132,35.3264639920828,28.2848461073165));
#53142=CARTESIAN_POINT('Ctrl Pts',(133.386287257647,35.1992787054487,28.2781302437978));
#53143=CARTESIAN_POINT('Ctrl Pts',(133.392139470349,34.9231995487549,28.2634428995431));
#53144=CARTESIAN_POINT('Ctrl Pts',(133.385507710175,34.7745277664282,28.2554643235251));
#53145=CARTESIAN_POINT('Ctrl Pts',(133.365194750099,34.591154525106,28.2450493284386));
#53146=CARTESIAN_POINT('Ctrl Pts',(133.360682709541,34.5555882088104,28.2430019516411));
#53147=CARTESIAN_POINT('Ctrl Pts',(133.353048295232,34.5022058639237,28.2398789605673));
#53148=CARTESIAN_POINT('Ctrl Pts',(133.350345892762,34.4843312700863,28.2388247766148));
#53149=CARTESIAN_POINT('Ctrl Pts',(133.345148708232,34.4517222480562,28.2368847150788));
#53150=CARTESIAN_POINT('Ctrl Pts',(133.342699283756,34.4369814873771,28.2360012830928));
#53151=CARTESIAN_POINT('Ctrl Pts',(133.336786226334,34.4027958245229,28.2339376878709));
#53152=CARTESIAN_POINT('Ctrl Pts',(133.333250038459,34.383364542749,28.232753703952));
#53153=CARTESIAN_POINT('Ctrl Pts',(133.321094325853,34.3197311973542,28.2288426414629));
#53154=CARTESIAN_POINT('Ctrl Pts',(133.311764046651,34.2756715868186,28.2260810522973));
#53155=CARTESIAN_POINT('Ctrl Pts',(133.286527659243,34.167209116851,28.2191709669556));
#53156=CARTESIAN_POINT('Ctrl Pts',(133.26960368074,34.1030632157658,28.214985875343));
#53157=CARTESIAN_POINT('Ctrl Pts',(133.173709768274,33.7785245138152,28.1934336083411));
#53158=CARTESIAN_POINT('Ctrl Pts',(133.065458717479,33.527780728012,28.1756283372013));
#53159=CARTESIAN_POINT('Ctrl Pts',(132.884167711508,33.2168315288207,28.153242215087));
#53160=CARTESIAN_POINT('Ctrl Pts',(132.837014767794,33.1427271435099,28.1478709441991));
#53161=CARTESIAN_POINT('Ctrl Pts',(132.765949209058,33.0400759752863,28.1403789175242));
#53162=CARTESIAN_POINT('Ctrl Pts',(132.744365967886,33.0099666315855,28.1381745482307));
#53163=CARTESIAN_POINT('Ctrl Pts',(132.706230030744,32.9585664821669,28.134398104556));
#53164=CARTESIAN_POINT('Ctrl Pts',(132.689909176583,32.9371087107543,28.1328174253524));
#53165=CARTESIAN_POINT('Ctrl Pts',(132.655825604829,32.8933898564772,28.1295872998555));
#53166=CARTESIAN_POINT('Ctrl Pts',(132.638034824803,32.8711532993092,28.1279391223822));
#53167=CARTESIAN_POINT('Ctrl Pts',(132.591431823204,32.8143860376986,28.1237159343819));
#53168=CARTESIAN_POINT('Ctrl Pts',(132.562208408018,32.7801991920771,28.121157438277));
#53169=CARTESIAN_POINT('Ctrl Pts',(132.400390699791,32.5983524299034,28.1074441504082));
#53170=CARTESIAN_POINT('Ctrl Pts',(132.255700942443,32.4619670583649,28.0968078114157));
#53171=CARTESIAN_POINT('Ctrl Pts',(131.932718725283,32.2070883032422,28.0749666129233));
#53172=CARTESIAN_POINT('Ctrl Pts',(131.753499001965,32.0912235161095,28.0638198653989));
#53173=CARTESIAN_POINT('Ctrl Pts',(131.52631227605,31.9730146144893,28.0494653606025));
#53174=CARTESIAN_POINT('Ctrl Pts',(131.487630512196,31.9538179979563,28.0470130775307));
#53175=CARTESIAN_POINT('Ctrl Pts',(131.431210476031,31.9271493101097,28.0434096494183));
#53176=CARTESIAN_POINT('Ctrl Pts',(131.413757256599,31.9190804666867,28.0422913299573));
#53177=CARTESIAN_POINT('Ctrl Pts',(131.38263105902,31.9050106046708,28.0402888855845));
#53178=CARTESIAN_POINT('Ctrl Pts',(131.36898565294,31.8989507790011,28.0394082437586));
#53179=CARTESIAN_POINT('Ctrl Pts',(131.338590327462,31.8856921557224,28.0374401100009));
#53180=CARTESIAN_POINT('Ctrl Pts',(131.321822271987,31.8785382812092,28.0363501729915));
#53181=CARTESIAN_POINT('Ctrl Pts',(131.27118979176,31.8574177124802,28.0330482507067));
#53182=CARTESIAN_POINT('Ctrl Pts',(131.237156899003,31.8438647852612,28.0308144569166));
#53183=CARTESIAN_POINT('Ctrl Pts',(131.156252302406,31.8131557088708,28.0254814149447));
#53184=CARTESIAN_POINT('Ctrl Pts',(131.109208581425,31.7964782197383,28.0223626702654));
#53185=CARTESIAN_POINT('Ctrl Pts',(130.926970608384,31.7363682596789,28.0102561281204));
#53186=CARTESIAN_POINT('Ctrl Pts',(130.7894684363,31.7004085762799,28.0010753060825));
#53187=CARTESIAN_POINT('Ctrl Pts',(130.440615309178,31.6322362729187,27.9781757098992));
#53188=CARTESIAN_POINT('Ctrl Pts',(130.227682664944,31.6111714678352,27.9645769625097));
#53189=CARTESIAN_POINT('Ctrl Pts',(129.961316669213,31.6100588467737,27.9483596134753));
#53190=CARTESIAN_POINT('Ctrl Pts',(129.908474349767,31.6110737766308,27.9451785888353));
#53191=CARTESIAN_POINT('Ctrl Pts',(129.825310921066,31.6146178291803,27.9402272715984));
#53192=CARTESIAN_POINT('Ctrl Pts',(129.794964866568,31.616320139112,27.9384320690286));
#53193=CARTESIAN_POINT('Ctrl Pts',(129.738251764589,31.620267332518,27.9350975468225));
#53194=CARTESIAN_POINT('Ctrl Pts',(129.711880360391,31.6224132617813,27.9335553110492));
#53195=CARTESIAN_POINT('Ctrl Pts',(129.652561798925,31.6279400198095,27.9301038342263));
#53196=CARTESIAN_POINT('Ctrl Pts',(129.619633381831,31.6314954118846,27.9282001156446));
#53197=CARTESIAN_POINT('Ctrl Pts',(129.518648781878,31.64389878017,27.922395438506));
#53198=CARTESIAN_POINT('Ctrl Pts',(129.450802987556,31.6543314699426,27.9185430592683));
#53199=CARTESIAN_POINT('Ctrl Pts',(129.290322762465,31.6840224234511,27.9095060937393));
#53200=CARTESIAN_POINT('Ctrl Pts',(129.1980851807,31.7051125513866,27.9043732066077));
#53201=CARTESIAN_POINT('Ctrl Pts',(128.893629976027,31.7882709988625,27.8874389572777));
#53202=CARTESIAN_POINT('Ctrl Pts',(128.686634037005,31.8672187251832,27.8759683917868));
#53203=CARTESIAN_POINT('Ctrl Pts',(128.412862467222,32.0035692048123,27.8593137643252));
#53204=CARTESIAN_POINT('Ctrl Pts',(128.338371434693,32.0442274476537,27.8546121156365));
#53205=CARTESIAN_POINT('Ctrl Pts',(128.243701809941,32.1006095764349,27.8483124653107));
#53206=CARTESIAN_POINT('Ctrl Pts',(128.222060820479,32.1138294657378,27.8468495602163));
#53207=CARTESIAN_POINT('Ctrl Pts',(128.187103791365,32.1357261091945,27.8444457109528));
#53208=CARTESIAN_POINT('Ctrl Pts',(128.173696480614,32.1442561358848,27.8435138275415));
#53209=CARTESIAN_POINT('Ctrl Pts',(128.147059234748,32.1614676372031,27.8416414792382));
#53210=CARTESIAN_POINT('Ctrl Pts',(128.13382913687,32.1701481063337,27.8407010842539));
#53211=CARTESIAN_POINT('Ctrl Pts',(128.099816354184,32.1928066546411,27.8382573679144));
#53212=CARTESIAN_POINT('Ctrl Pts',(128.079127295868,32.2069227830563,27.8367454978581));
#53213=CARTESIAN_POINT('Ctrl Pts',(127.985713698667,32.272187555466,27.8298095856459));
#53214=CARTESIAN_POINT('Ctrl Pts',(127.914867325037,32.3259526462293,27.8242439687613));
#53215=CARTESIAN_POINT('Ctrl Pts',(127.684253361076,32.515705840765,27.8052821371633));
#53216=CARTESIAN_POINT('Ctrl Pts',(127.535002937455,32.6637221961105,27.7915971812811));
#53217=CARTESIAN_POINT('Ctrl Pts',(127.306577432178,32.9366902875799,27.7689661052399));
#53218=CARTESIAN_POINT('Ctrl Pts',(127.220108955343,33.0547527909872,27.7598556584501));
#53219=CARTESIAN_POINT('Ctrl Pts',(127.118191512677,33.2146514210372,27.7484050943926));
#53220=CARTESIAN_POINT('Ctrl Pts',(127.095562389508,33.2517059357571,27.7458085595277));
#53221=CARTESIAN_POINT('Ctrl Pts',(127.059439203084,33.3134947010813,27.7415699269521));
#53222=CARTESIAN_POINT('Ctrl Pts',(127.045531039314,33.3379797969184,27.7399132440909));
#53223=CARTESIAN_POINT('Ctrl Pts',(127.018823445137,33.3863929932172,27.7366813475991));
#53224=CARTESIAN_POINT('Ctrl Pts',(127.006003069917,33.4103070519976,27.7351054849422));
#53225=CARTESIAN_POINT('Ctrl Pts',(126.97588557156,33.4681427520691,27.7313419316012));
#53226=CARTESIAN_POINT('Ctrl Pts',(126.958869956927,33.5022073137825,27.7291640518083));
#53227=CARTESIAN_POINT('Ctrl Pts',(126.898556323856,33.6282200685959,27.7212408916887));
#53228=CARTESIAN_POINT('Ctrl Pts',(126.858823561132,33.7218191899794,27.7156144660151));
#53229=CARTESIAN_POINT('Ctrl Pts',(126.76417014344,33.9760016402912,27.7008517446808));
#53230=CARTESIAN_POINT('Ctrl Pts',(126.716995332061,34.1391570156289,27.6919145493355));
#53231=CARTESIAN_POINT('Ctrl Pts',(126.648215593138,34.4675707085868,27.67410429333));
#53232=CARTESIAN_POINT('Ctrl Pts',(126.626176428229,34.6322456405921,27.6652534687727));
#53233=CARTESIAN_POINT('Ctrl Pts',(126.614173352631,34.8331639056892,27.6538934721961));
#53234=CARTESIAN_POINT('Ctrl Pts',(126.612616790041,34.8685041737009,27.6518740875299));
#53235=CARTESIAN_POINT('Ctrl Pts',(126.611111539139,34.9215561476712,27.6488023239765));
#53236=CARTESIAN_POINT('Ctrl Pts',(126.610748103906,34.9392546862154,27.6477708333819));
#53237=CARTESIAN_POINT('Ctrl Pts',(126.610410290085,34.9658549347967,27.646209363987));
#53238=CARTESIAN_POINT('Ctrl Pts',(126.610332318059,34.9747553592404,27.6456850120307));
#53239=CARTESIAN_POINT('Ctrl Pts',(126.610263040683,34.9891233453301,27.6448353861475));
#53240=CARTESIAN_POINT('Ctrl Pts',(126.61024990695,34.9945906917616,27.6445113526269));
#53241=CARTESIAN_POINT('Ctrl Pts',(126.610250000496,35.0000579986539,27.6441866060966));
#53242=CARTESIAN_POINT('Ctrl Pts',(126.610250000487,35.0000574599859,27.6441866380923));
#53243=CARTESIAN_POINT('Ctrl Pts',(126.610250090869,35.0053893568261,27.6438699346801));
#53244=CARTESIAN_POINT('Ctrl Pts',(126.610262761436,35.0107212118073,27.6435525533915));
#53245=CARTESIAN_POINT('Ctrl Pts',(126.610341021443,35.0272464228444,27.6425668195178));
#53246=CARTESIAN_POINT('Ctrl Pts',(126.610449474336,35.0384393661142,27.6418962240595));
#53247=CARTESIAN_POINT('Ctrl Pts',(126.6111108585,35.0836060713677,27.6391788960502));
#53248=CARTESIAN_POINT('Ctrl Pts',(126.612119143323,35.1175699816628,27.6371097940641));
#53249=CARTESIAN_POINT('Ctrl Pts',(126.624079589182,35.3848921680719,27.6206508155777));
#53250=CARTESIAN_POINT('Ctrl Pts',(126.658618390739,35.6165549798459,27.6053930793298));
#53251=CARTESIAN_POINT('Ctrl Pts',(126.74576514076,35.9560478668779,27.5828983791518));
#53252=CARTESIAN_POINT('Ctrl Pts',(126.780662504909,36.0676720844525,27.5754697298841));
#53253=CARTESIAN_POINT('Ctrl Pts',(126.821241849407,36.1772432554656,27.5681926079129));
#53254=CARTESIAN_POINT('',(126.610251311732,34.9970179063717,27.9839821967168));
#53255=CARTESIAN_POINT('Ctrl Pts',(126.821241918358,36.1772434416438,27.913420165303));
#53256=CARTESIAN_POINT('Ctrl Pts',(126.78558888443,36.0809741691002,27.9194241936204));
#53257=CARTESIAN_POINT('Ctrl Pts',(126.754305384126,35.983062571326,27.9254282219378));
#53258=CARTESIAN_POINT('Ctrl Pts',(126.72753284865,35.8839478524425,27.9314322502553));
#53259=CARTESIAN_POINT('Ctrl Pts',(126.700760124204,35.7848324339714,27.9374363209513));
#53260=CARTESIAN_POINT('Ctrl Pts',(126.678498535277,35.6845143046025,27.9434403916474));
#53261=CARTESIAN_POINT('Ctrl Pts',(126.660838976721,35.5834455613996,27.9494444623435));
#53262=CARTESIAN_POINT('Ctrl Pts',(126.643163513312,35.4822857919401,27.9554539405282));
#53263=CARTESIAN_POINT('Ctrl Pts',(126.630098428797,35.380374493645,27.9614634187129));
#53264=CARTESIAN_POINT('Ctrl Pts',(126.621683002323,35.2781713962731,27.9674728968976));
#53265=CARTESIAN_POINT('Ctrl Pts',(126.613976687149,35.1845802654455,27.9729759968373));
#53266=CARTESIAN_POINT('Ctrl Pts',(126.610168856573,35.0907447639098,27.978479096777));
#53267=CARTESIAN_POINT('Ctrl Pts',(126.610251311732,34.9970179063717,27.9839821967168));
#53268=CARTESIAN_POINT('Ctrl Pts',(126.821241934448,36.17724348509,29.1634527466974));
#53269=CARTESIAN_POINT('Ctrl Pts',(126.865650457316,36.2971540660655,29.1566721127873));
#53270=CARTESIAN_POINT('Ctrl Pts',(126.916815953089,36.4144761966767,29.1498639293176));
#53271=CARTESIAN_POINT('Ctrl Pts',(127.017822426018,36.6143887349965,29.1376463261198));
#53272=CARTESIAN_POINT('Ctrl Pts',(127.064767641159,36.6982469982982,29.132318279004));
#53273=CARTESIAN_POINT('Ctrl Pts',(127.134768480411,36.8116956160826,29.1247531624993));
#53274=CARTESIAN_POINT('Ctrl Pts',(127.154849794449,36.8430715716172,29.1226214602806));
#53275=CARTESIAN_POINT('Ctrl Pts',(127.190309125222,36.8965139603084,29.1189184872974));
#53276=CARTESIAN_POINT('Ctrl Pts',(127.205440417,36.9187403912989,29.1173564039352));
#53277=CARTESIAN_POINT('Ctrl Pts',(127.23697945629,36.9639036958967,29.1141356107022));
#53278=CARTESIAN_POINT('Ctrl Pts',(127.253412192638,36.9868204740305,29.1124760341176));
#53279=CARTESIAN_POINT('Ctrl Pts',(127.296261535642,37.0450297329475,29.1081940013818));
#53280=CARTESIAN_POINT('Ctrl Pts',(127.323083530223,37.0800159206566,29.1055561301045));
#53281=CARTESIAN_POINT('Ctrl Pts',(127.450381060313,37.2395192722143,29.093223471913));
#53282=CARTESIAN_POINT('Ctrl Pts',(127.558898350999,37.3573320943317,29.0832148366242));
#53283=CARTESIAN_POINT('Ctrl Pts',(127.81990481958,37.6032786160111,29.06032154642));
#53284=CARTESIAN_POINT('Ctrl Pts',(127.976187864314,37.7265466963254,29.0473620849306));
#53285=CARTESIAN_POINT('Ctrl Pts',(128.214994438526,37.8830018466142,29.029240114234));
#53286=CARTESIAN_POINT('Ctrl Pts',(128.289432491016,37.9277817013019,29.023806283354));
#53287=CARTESIAN_POINT('Ctrl Pts',(128.387226810324,37.9816072824505,29.0170125257965));
#53288=CARTESIAN_POINT('Ctrl Pts',(128.409071128837,37.9933200219717,29.0155164482157));
#53289=CARTESIAN_POINT('Ctrl Pts',(128.444967151292,38.0120631894446,29.0130952337504));
#53290=CARTESIAN_POINT('Ctrl Pts',(128.458942445982,38.0192372319407,29.0121616944514));
#53291=CARTESIAN_POINT('Ctrl Pts',(128.487168252057,38.0334795481558,29.0102952467849));
#53292=CARTESIAN_POINT('Ctrl Pts',(128.501419540881,38.04054513151,29.0093624804291));
#53293=CARTESIAN_POINT('Ctrl Pts',(128.538582721673,38.0586453338267,29.0069536391171));
#53294=CARTESIAN_POINT('Ctrl Pts',(128.561570399773,38.0695231074417,29.0054866950883));
#53295=CARTESIAN_POINT('Ctrl Pts',(128.662514647195,38.1159068561669,28.9991360347455));
#53296=CARTESIAN_POINT('Ctrl Pts',(128.741684139075,38.1487118071384,28.9943901677296));
#53297=CARTESIAN_POINT('Ctrl Pts',(129.008138199996,38.2474627509051,28.9789226807803));
#53298=CARTESIAN_POINT('Ctrl Pts',(129.199965139118,38.299962968452,28.9685732098983));
#53299=CARTESIAN_POINT('Ctrl Pts',(129.551444970943,38.3636868144409,28.9494982576423));
#53300=CARTESIAN_POINT('Ctrl Pts',(129.709378818467,38.3809943068604,28.9408905818149));
#53301=CARTESIAN_POINT('Ctrl Pts',(129.912060243996,38.3888968272813,28.9294548975422));
#53302=CARTESIAN_POINT('Ctrl Pts',(129.956213899416,38.3897548040091,28.9269411093992));
#53303=CARTESIAN_POINT('Ctrl Pts',(130.028707639274,38.3897468838245,28.9227709955705));
#53304=CARTESIAN_POINT('Ctrl Pts',(130.057043132898,38.3893884514982,28.9211303033685));
#53305=CARTESIAN_POINT('Ctrl Pts',(130.112453006022,38.3879925218593,28.9178995463875));
#53306=CARTESIAN_POINT('Ctrl Pts',(130.139526057678,38.3869855952781,28.9163105440226));
#53307=CARTESIAN_POINT('Ctrl Pts',(130.204203437771,38.3838032891687,28.9124882492052));
#53308=CARTESIAN_POINT('Ctrl Pts',(130.241788651226,38.3813254532137,28.9102458398722));
#53309=CARTESIAN_POINT('Ctrl Pts',(130.377189888425,38.3701299864737,28.902088019353));
#53310=CARTESIAN_POINT('Ctrl Pts',(130.47465010442,38.3577898616422,28.8960642659392));
#53311=CARTESIAN_POINT('Ctrl Pts',(130.734308539463,38.3133821432914,28.8796147203478));
#53312=CARTESIAN_POINT('Ctrl Pts',(130.894919538314,38.2736556264363,28.8690036366284));
#53313=CARTESIAN_POINT('Ctrl Pts',(131.217728518421,38.1682712559772,28.8471232641739));
#53314=CARTESIAN_POINT('Ctrl Pts',(131.37906738404,38.1014492754746,28.8358830053645));
#53315=CARTESIAN_POINT('Ctrl Pts',(131.566289529084,38.0063946240017,28.8229572808464));
#53316=CARTESIAN_POINT('Ctrl Pts',(131.597767082269,37.9897846227255,28.8207888902099));
#53317=CARTESIAN_POINT('Ctrl Pts',(131.644809219965,37.9640063358149,28.8175620463634));
#53318=CARTESIAN_POINT('Ctrl Pts',(131.66057077583,37.9552048422108,28.8164832550982));
#53319=CARTESIAN_POINT('Ctrl Pts',(131.689276889293,37.9388727231796,28.8145238841537));
#53320=CARTESIAN_POINT('Ctrl Pts',(131.702242517314,37.9313818782885,28.813641050877));
#53321=CARTESIAN_POINT('Ctrl Pts',(131.732300127542,37.9137495200397,28.8115990653595));
#53322=CARTESIAN_POINT('Ctrl Pts',(131.749353108451,37.9035433078895,28.810443959665));
#53323=CARTESIAN_POINT('Ctrl Pts',(131.805326947851,37.8693707981458,28.8066604578366));
#53324=CARTESIAN_POINT('Ctrl Pts',(131.843854383611,37.8447663517038,28.8040690405227));
#53325=CARTESIAN_POINT('Ctrl Pts',(131.938202052553,37.7817915546806,28.7977250920237));
#53326=CARTESIAN_POINT('Ctrl Pts',(131.993393393891,37.7425125615829,28.7940157131865));
#53327=CARTESIAN_POINT('Ctrl Pts',(132.279839238729,37.525433561398,28.774570146116));
#53328=CARTESIAN_POINT('Ctrl Pts',(132.488591531801,37.3200007649064,28.7595919516378));
#53329=CARTESIAN_POINT('Ctrl Pts',(132.713969482376,37.0322937362579,28.7394161866236));
#53330=CARTESIAN_POINT('Ctrl Pts',(132.757555444751,36.9727481030679,28.7352847121568));
#53331=CARTESIAN_POINT('Ctrl Pts',(132.818349626506,36.883737726,28.7291421063803));
#53332=CARTESIAN_POINT('Ctrl Pts',(132.837112617516,36.8553582709199,28.7271884753924));
#53333=CARTESIAN_POINT('Ctrl Pts',(132.869752327104,36.8043368710607,28.7236821375369));
#53334=CARTESIAN_POINT('Ctrl Pts',(132.88379627074,36.7818049761453,28.722135705659));
#53335=CARTESIAN_POINT('Ctrl Pts',(132.913058461344,36.7336048557974,28.7188307241416));
#53336=CARTESIAN_POINT('Ctrl Pts',(132.928205284585,36.707896109656,28.7170697782943));
#53337=CARTESIAN_POINT('Ctrl Pts',(132.968585365462,36.6372423590641,28.7122337770239));
#53338=CARTESIAN_POINT('Ctrl Pts',(132.993135267547,36.5919178522079,28.7091351631451));
#53339=CARTESIAN_POINT('Ctrl Pts',(133.091666410476,36.3996649932213,28.6960014977137));
#53340=CARTESIAN_POINT('Ctrl Pts',(133.155927427618,36.2480278867025,28.6856509776992));
#53341=CARTESIAN_POINT('Ctrl Pts',(133.288738733609,35.8578743804535,28.6592596571671));
#53342=CARTESIAN_POINT('Ctrl Pts',(133.342617059639,35.615361432157,28.6430347130332));
#53343=CARTESIAN_POINT('Ctrl Pts',(133.37333134148,35.3349934103167,28.6256826190535));
#53344=CARTESIAN_POINT('Ctrl Pts',(133.376552849037,35.3007922489946,28.6235904640387));
#53345=CARTESIAN_POINT('Ctrl Pts',(133.380669138672,35.2486063073163,28.6204413940224));
#53346=CARTESIAN_POINT('Ctrl Pts',(133.381941371965,35.2306545246443,28.6193659068443));
#53347=CARTESIAN_POINT('Ctrl Pts',(133.384008576429,35.197773809985,28.6174113110888));
#53348=CARTESIAN_POINT('Ctrl Pts',(133.384847820655,35.1828490307917,28.6165299727953));
#53349=CARTESIAN_POINT('Ctrl Pts',(133.386571858428,35.1480887839398,28.6144905617265));
#53350=CARTESIAN_POINT('Ctrl Pts',(133.387381156365,35.128250470195,28.6133365440452));
#53351=CARTESIAN_POINT('Ctrl Pts',(133.389477131792,35.0627446876347,28.6095553858785));
#53352=CARTESIAN_POINT('Ctrl Pts',(133.39001498757,35.0170565173093,28.6069652563475));
#53353=CARTESIAN_POINT('Ctrl Pts',(133.389057286393,34.9036732441961,28.6006240965911));
#53354=CARTESIAN_POINT('Ctrl Pts',(133.386457595868,34.8360060684183,28.5969162730125));
#53355=CARTESIAN_POINT('Ctrl Pts',(133.361924339353,34.4776791621796,28.5774854715992));
#53356=CARTESIAN_POINT('Ctrl Pts',(133.30459925731,34.1906867837349,28.5625212117561));
#53357=CARTESIAN_POINT('Ctrl Pts',(133.18987109863,33.8512655145781,28.5427470261242));
#53358=CARTESIAN_POINT('Ctrl Pts',(133.166612476095,33.7886234360696,28.5390117054158));
#53359=CARTESIAN_POINT('Ctrl Pts',(133.129074041698,33.696006747606,28.533336134345));
#53360=CARTESIAN_POINT('Ctrl Pts',(133.116179705843,33.6654863461253,28.5314404835134));
#53361=CARTESIAN_POINT('Ctrl Pts',(133.09292065392,33.6126089708988,28.5281092990482));
#53362=CARTESIAN_POINT('Ctrl Pts',(133.082755557594,33.5901666182129,28.5266804988298));
#53363=CARTESIAN_POINT('Ctrl Pts',(133.060818402026,33.5431059307594,28.5236516882624));
#53364=CARTESIAN_POINT('Ctrl Pts',(133.048991941846,33.5185150379379,28.5220499082525));
#53365=CARTESIAN_POINT('Ctrl Pts',(133.019547383566,33.4591369079057,28.5181343105906));
#53366=CARTESIAN_POINT('Ctrl Pts',(133.001623730231,33.4245063434621,28.51581013273));
#53367=CARTESIAN_POINT('Ctrl Pts',(132.931143928456,33.2939013083417,28.5068858758715));
#53368=CARTESIAN_POINT('Ctrl Pts',(132.874553595752,33.2001902360918,28.5001479255731));
#53369=CARTESIAN_POINT('Ctrl Pts',(132.700212762543,32.9407431501739,28.4805317591112));
#53370=CARTESIAN_POINT('Ctrl Pts',(132.571962248077,32.7826398048713,28.4673550572921));
#53371=CARTESIAN_POINT('Ctrl Pts',(132.335491832914,32.5394316512585,28.4455599674143));
#53372=CARTESIAN_POINT('Ctrl Pts',(132.234843370349,32.4476676254561,28.4369021200079));
#53373=CARTESIAN_POINT('Ctrl Pts',(132.107047144835,32.34452469855,28.4268678493928));
#53374=CARTESIAN_POINT('Ctrl Pts',(132.084931879327,32.327125906852,28.4251638857455));
#53375=CARTESIAN_POINT('Ctrl Pts',(132.049522107146,32.2999748418779,28.4224899792002));
#53376=CARTESIAN_POINT('Ctrl Pts',(132.036369167066,32.2900410773152,28.4215084137486));
#53377=CARTESIAN_POINT('Ctrl Pts',(132.010802278945,32.271022928489,28.4196236910182));
#53378=CARTESIAN_POINT('Ctrl Pts',(131.99839817806,32.2619265182791,28.4187197965125));
#53379=CARTESIAN_POINT('Ctrl Pts',(131.96740642698,32.2395218537389,28.4164863234166));
#53380=CARTESIAN_POINT('Ctrl Pts',(131.948744868507,32.2263163223643,28.4151634437478));
#53381=CARTESIAN_POINT('Ctrl Pts',(131.874886732048,32.1751652958098,28.410007598271));
#53382=CARTESIAN_POINT('Ctrl Pts',(131.818700958593,32.1386682529056,28.406258413104));
#53383=CARTESIAN_POINT('Ctrl Pts',(131.657826647824,32.0408226405472,28.3958935495562));
#53384=CARTESIAN_POINT('Ctrl Pts',(131.550871247584,31.9833923826728,28.3894243154397));
#53385=CARTESIAN_POINT('Ctrl Pts',(131.219207146427,31.8276166196265,28.3699716943244));
#53386=CARTESIAN_POINT('Ctrl Pts',(130.986726819905,31.7477943755422,28.3570805717256));
#53387=CARTESIAN_POINT('Ctrl Pts',(130.697720302912,31.68243840353,28.3404823472541));
#53388=CARTESIAN_POINT('Ctrl Pts',(130.647513972822,31.6722749756741,28.3375817021378));
#53389=CARTESIAN_POINT('Ctrl Pts',(130.567519916183,31.6579603368981,28.3329234675449));
#53390=CARTESIAN_POINT('Ctrl Pts',(130.537873072096,31.6530610343861,28.3311891878952));
#53391=CARTESIAN_POINT('Ctrl Pts',(130.484579097376,31.6449802864875,28.328055865857));
#53392=CARTESIAN_POINT('Ctrl Pts',(130.460955878357,31.6416531127989,28.3266614686194));
#53393=CARTESIAN_POINT('Ctrl Pts',(130.405248885379,31.634405987085,28.3233594725153));
#53394=CARTESIAN_POINT('Ctrl Pts',(130.373140699676,31.6306950822682,28.3214455231618));
#53395=CARTESIAN_POINT('Ctrl Pts',(130.277084163365,31.6209832038168,28.315685690669));
#53396=CARTESIAN_POINT('Ctrl Pts',(130.21301596426,31.61634022,28.3117988519883));
#53397=CARTESIAN_POINT('Ctrl Pts',(129.896301421753,31.602418573742,28.2923553739511));
#53398=CARTESIAN_POINT('Ctrl Pts',(129.643324707481,31.6196063153522,28.27602309344));
#53399=CARTESIAN_POINT('Ctrl Pts',(129.248223399285,31.6913166453197,28.2501853300543));
#53400=CARTESIAN_POINT('Ctrl Pts',(129.103686967136,31.7275109423525,28.2406823804366));
#53401=CARTESIAN_POINT('Ctrl Pts',(128.93503823822,31.7817609048842,28.2298562266376));
#53402=CARTESIAN_POINT('Ctrl Pts',(128.908198448345,31.7907670833852,28.2281416562374));
#53403=CARTESIAN_POINT('Ctrl Pts',(128.865870964788,31.8055627122895,28.2254544641373));
#53404=CARTESIAN_POINT('Ctrl Pts',(128.850307962199,31.8111308435338,28.2244700586326));
#53405=CARTESIAN_POINT('Ctrl Pts',(128.820353738658,31.8220956655272,28.2225832317353));
#53406=CARTESIAN_POINT('Ctrl Pts',(128.805957589125,31.8274767157732,28.2216800333339));
#53407=CARTESIAN_POINT('Ctrl Pts',(128.770317979797,31.8410751869875,28.2194520079547));
#53408=CARTESIAN_POINT('Ctrl Pts',(128.749119364781,31.8494093344111,28.2181338009025));
#53409=CARTESIAN_POINT('Ctrl Pts',(128.666574782292,31.8828258809621,28.2130225573489));
#53410=CARTESIAN_POINT('Ctrl Pts',(128.605882259017,31.90949289428,28.209311459649));
#53411=CARTESIAN_POINT('Ctrl Pts',(128.438353390463,31.9890421331644,28.1990980972361));
#53412=CARTESIAN_POINT('Ctrl Pts',(128.333464171249,32.0458048586648,28.1927372108013));
#53413=CARTESIAN_POINT('Ctrl Pts',(128.019115313631,32.238002050537,28.173171193243));
#53414=CARTESIAN_POINT('Ctrl Pts',(127.821462669881,32.391072875728,28.160074203684));
#53415=CARTESIAN_POINT('Ctrl Pts',(127.605609359429,32.6000171651751,28.1432371133889));
#53416=CARTESIAN_POINT('Ctrl Pts',(127.569650312907,32.6364382469302,28.1403374054098));
#53417=CARTESIAN_POINT('Ctrl Pts',(127.514109692311,32.6953004851045,28.1356959956543));
#53418=CARTESIAN_POINT('Ctrl Pts',(127.493974950627,32.7172102930258,28.1339778050777));
#53419=CARTESIAN_POINT('Ctrl Pts',(127.456424337209,32.7591669160105,28.1307035064515));
#53420=CARTESIAN_POINT('Ctrl Pts',(127.438950427376,32.7791589229117,28.1291499781799));
#53421=CARTESIAN_POINT('Ctrl Pts',(127.399558010848,32.8253112444638,28.1255775324848));
#53422=CARTESIAN_POINT('Ctrl Pts',(127.377796382142,32.8516011121898,28.1235525109746));
#53423=CARTESIAN_POINT('Ctrl Pts',(127.309828184662,32.936283692104,28.1170587617667));
#53424=CARTESIAN_POINT('Ctrl Pts',(127.265149364582,32.995869238157,28.1125319500083));
#53425=CARTESIAN_POINT('Ctrl Pts',(127.161516698363,33.144003102298,28.1013756354379));
#53426=CARTESIAN_POINT('Ctrl Pts',(127.10470030721,33.2339454659358,28.0946805491506));
#53427=CARTESIAN_POINT('Ctrl Pts',(126.956433718969,33.4950950151653,28.0755308302079));
#53428=CARTESIAN_POINT('Ctrl Pts',(126.875319596041,33.6716910429383,28.0628946674612));
#53429=CARTESIAN_POINT('Ctrl Pts',(126.77924151185,33.9392129151538,28.0448296209382));
#53430=CARTESIAN_POINT('Ctrl Pts',(126.752132136427,34.0253660160909,28.0391708453404));
#53431=CARTESIAN_POINT('Ctrl Pts',(126.721709489226,34.1375107555842,28.032090434298));
#53432=CARTESIAN_POINT('Ctrl Pts',(126.715212603212,34.162594353656,28.0305248767131));
#53433=CARTESIAN_POINT('Ctrl Pts',(126.705167702483,34.2032933536749,28.0280166594166));
#53434=CARTESIAN_POINT('Ctrl Pts',(126.70144171656,34.2188632495394,28.0270646289969));
#53435=CARTESIAN_POINT('Ctrl Pts',(126.694277203055,34.2497675106689,28.0251906422662));
#53436=CARTESIAN_POINT('Ctrl Pts',(126.690834745472,34.2651004605382,28.0242685122559));
#53437=CARTESIAN_POINT('Ctrl Pts',(126.682291777531,34.3044290235944,28.0219215344808));
#53438=CARTESIAN_POINT('Ctrl Pts',(126.677344789056,34.328457554312,28.0205049468539));
#53439=CARTESIAN_POINT('Ctrl Pts',(126.667033082523,34.3814499865233,28.0174147237341));
#53440=CARTESIAN_POINT('Ctrl Pts',(126.661784110045,34.4104345885619,28.0157466677298));
#53441=CARTESIAN_POINT('Ctrl Pts',(126.62602528337,34.6237113359987,28.0036111025836));
#53442=CARTESIAN_POINT('Ctrl Pts',(126.610416088327,34.8101883435728,27.9937443927268));
#53443=CARTESIAN_POINT('Ctrl Pts',(126.61025131837,34.9970103699449,27.9838400398653));
#53444=CARTESIAN_POINT('Origin',(130.,35.,32.7603849714045));
#53445=CARTESIAN_POINT('',(125.915001580773,34.9964062680618,28.3853849713761));
#53446=CARTESIAN_POINT('Ctrl Pts',(132.487160689988,38.2405642567579,29.1925548573102));
#53447=CARTESIAN_POINT('Ctrl Pts',(132.581690765635,38.1680116179144,29.1867409038837));
#53448=CARTESIAN_POINT('Ctrl Pts',(132.67315408253,38.0912344395281,29.1809269504572));
#53449=CARTESIAN_POINT('Ctrl Pts',(132.761153744737,38.0105240404164,29.1751129970307));
#53450=CARTESIAN_POINT('Ctrl Pts',(132.849077229458,37.9298835087917,29.1693040764911));
#53451=CARTESIAN_POINT('Ctrl Pts',(132.933542725555,37.845316805426,29.1634951559516));
#53452=CARTESIAN_POINT('Ctrl Pts',(133.014185814076,37.7571559401356,29.1576862354121));
#53453=CARTESIAN_POINT('Ctrl Pts',(133.094785419096,37.6690426120001,29.1518804470963));
#53454=CARTESIAN_POINT('Ctrl Pts',(133.171566440987,37.5773392769486,29.1460746587805));
#53455=CARTESIAN_POINT('Ctrl Pts',(133.244201165315,37.4824149127345,29.1402688704647));
#53456=CARTESIAN_POINT('Ctrl Pts',(133.316816230649,37.3875162403308,29.134464653518));
#53457=CARTESIAN_POINT('Ctrl Pts',(133.385286982042,37.2893985962056,29.1286604365713));
#53458=CARTESIAN_POINT('Ctrl Pts',(133.449326260106,37.1884636966017,29.1228562196246));
#53459=CARTESIAN_POINT('Ctrl Pts',(133.513363305932,37.0875323153176,29.1170522049974));
#53460=CARTESIAN_POINT('Ctrl Pts',(133.572968967077,36.98378421861,29.1112481903701));
#53461=CARTESIAN_POINT('Ctrl Pts',(133.627900017705,36.8776491848945,29.1054441757429));
#53462=CARTESIAN_POINT('Ctrl Pts',(133.682842106129,36.7714928245,29.0996389948621));
#53463=CARTESIAN_POINT('Ctrl Pts',(133.733107528507,36.6629489357843,29.0938338139814));
#53464=CARTESIAN_POINT('Ctrl Pts',(133.778499818206,36.5524703294487,29.0880286331006));
#53465=CARTESIAN_POINT('Ctrl Pts',(133.823939675865,36.4418759492238,29.0822173687943));
#53466=CARTESIAN_POINT('Ctrl Pts',(133.864496046327,36.3293431803229,29.0764061044881));
#53467=CARTESIAN_POINT('Ctrl Pts',(133.900021202843,36.2153434154088,29.0705948401819));
#53468=CARTESIAN_POINT('Ctrl Pts',(133.935565748714,36.1012814303058,29.0647804041326));
#53469=CARTESIAN_POINT('Ctrl Pts',(133.966073505789,35.9857512485749,29.0589659680832));
#53470=CARTESIAN_POINT('Ctrl Pts',(133.99144751717,35.8692362841478,29.0531515320339));
#53471=CARTESIAN_POINT('Ctrl Pts',(134.016861593775,35.7525373441513,29.0473279150679));
#53472=CARTESIAN_POINT('Ctrl Pts',(134.037125660968,35.6348509173009,29.0415042981019));
#53473=CARTESIAN_POINT('Ctrl Pts',(134.052194377336,35.5166679090954,29.0356806811359));
#53474=CARTESIAN_POINT('Ctrl Pts',(134.064126351656,35.4230861742918,29.0310693229823));
#53475=CARTESIAN_POINT('Ctrl Pts',(134.072801833475,35.3291932530324,29.0264579648287));
#53476=CARTESIAN_POINT('Ctrl Pts',(134.078221501167,35.235232624052,29.021846606675));
#53477=CARTESIAN_POINT('Ctrl Pts',(134.085065207076,35.1165834838716,29.016023596698));
#53478=CARTESIAN_POINT('Ctrl Pts',(134.086737820651,34.9974437193359,29.0102005867211));
#53479=CARTESIAN_POINT('Ctrl Pts',(134.083186794953,34.8783012016325,29.0043775767441));
#53480=CARTESIAN_POINT('Ctrl Pts',(134.079640254598,34.7593091742895,28.9985619218818));
#53481=CARTESIAN_POINT('Ctrl Pts',(134.07088321031,34.6403148053383,28.9927462670194));
#53482=CARTESIAN_POINT('Ctrl Pts',(134.05691497557,34.5218097857627,28.986930612157));
#53483=CARTESIAN_POINT('Ctrl Pts',(134.042960741383,34.4034235453878,28.981120786405));
#53484=CARTESIAN_POINT('Ctrl Pts',(134.023805755227,34.2855260819284,28.975310960653));
#53485=CARTESIAN_POINT('Ctrl Pts',(133.999501340222,34.1686071749385,28.9695011349009));
#53486=CARTESIAN_POINT('Ctrl Pts',(133.97427342688,34.0472456834969,28.9634705523678));
#53487=CARTESIAN_POINT('Ctrl Pts',(133.943497010083,33.9269390362428,28.9574399698347));
#53488=CARTESIAN_POINT('Ctrl Pts',(133.907288468512,33.8082274445867,28.9514093873016));
#53489=CARTESIAN_POINT('Ctrl Pts',(133.872444733883,33.6939904436618,28.9456061152471));
#53490=CARTESIAN_POINT('Ctrl Pts',(133.832571097199,33.5812308562466,28.9398028431925));
#53491=CARTESIAN_POINT('Ctrl Pts',(133.787822753732,33.4704171201558,28.9339995711379));
#53492=CARTESIAN_POINT('Ctrl Pts',(133.743081051571,33.3596198304379,28.9281971603735));
#53493=CARTESIAN_POINT('Ctrl Pts',(133.69346623428,33.2507681963479,28.922394749609));
#53494=CARTESIAN_POINT('Ctrl Pts',(133.639182103552,33.1443118211332,28.9165923388446));
#53495=CARTESIAN_POINT('Ctrl Pts',(133.584893210769,33.0378461070718,28.9107894190658));
#53496=CARTESIAN_POINT('Ctrl Pts',(133.525934375693,32.933776433535,28.9049864992869));
#53497=CARTESIAN_POINT('Ctrl Pts',(133.462555627298,32.832528309788,28.8991835795081));
#53498=CARTESIAN_POINT('Ctrl Pts',(133.399156352903,32.7312473955718,28.8933787803813));
#53499=CARTESIAN_POINT('Ctrl Pts',(133.331334534987,32.6327901944861,28.8875739812544));
#53500=CARTESIAN_POINT('Ctrl Pts',(133.259383468629,32.5375531671871,28.8817691821275));
#53501=CARTESIAN_POINT('Ctrl Pts',(133.187352725038,32.4422106762284,28.8759579548773));
#53502=CARTESIAN_POINT('Ctrl Pts',(133.111183851963,32.3500958030861,28.8701467276271));
#53503=CARTESIAN_POINT('Ctrl Pts',(133.031210463438,32.2615719607152,28.8643355003769));
#53504=CARTESIAN_POINT('Ctrl Pts',(132.951184559165,32.1729899878093,28.8585204570954));
#53505=CARTESIAN_POINT('Ctrl Pts',(132.867349450225,32.0880040319731,28.852705413814));
#53506=CARTESIAN_POINT('Ctrl Pts',(132.780074430544,32.0069394993355,28.8468903705325));
#53507=CARTESIAN_POINT('Ctrl Pts',(132.692674341008,31.92575879681,28.8410669939775));
#53508=CARTESIAN_POINT('Ctrl Pts',(132.601824811626,31.8485109975396,28.8352436174225));
#53509=CARTESIAN_POINT('Ctrl Pts',(132.507926985996,31.7754803097343,28.8294202408675));
#53510=CARTESIAN_POINT('Ctrl Pts',(132.482917742351,31.7560289299747,28.8278692119472));
#53511=CARTESIAN_POINT('Ctrl Pts',(132.457692403287,31.7368764672564,28.8263181830269));
#53512=CARTESIAN_POINT('Ctrl Pts',(132.432258861009,31.7180277525484,28.8247671541066));
#53513=CARTESIAN_POINT('Ctrl Pts',(132.336762586141,31.6472557766668,28.8189434476609));
#53514=CARTESIAN_POINT('Ctrl Pts',(132.238020892333,31.5805411803083,28.8131197412152));
#53515=CARTESIAN_POINT('Ctrl Pts',(132.136413171174,31.5181953297125,28.8072960347695));
#53516=CARTESIAN_POINT('Ctrl Pts',(132.034933632443,31.4559281310388,28.8014796751753));
#53517=CARTESIAN_POINT('Ctrl Pts',(131.930595602701,31.398018927822,28.7956633155811));
#53518=CARTESIAN_POINT('Ctrl Pts',(131.823810085798,31.3447377972379,28.7898469559869));
#53519=CARTESIAN_POINT('Ctrl Pts',(131.717131453584,31.2915099972665,28.7840364181539));
#53520=CARTESIAN_POINT('Ctrl Pts',(131.608010570973,31.2429012356439,28.778225880321));
#53521=CARTESIAN_POINT('Ctrl Pts',(131.496885342853,31.1991370360993,28.772415342488));
#53522=CARTESIAN_POINT('Ctrl Pts',(131.381556861378,31.1537174787061,28.7663850241151));
#53523=CARTESIAN_POINT('Ctrl Pts',(131.264069795977,31.1135164398812,28.7603547057422));
#53524=CARTESIAN_POINT('Ctrl Pts',(131.14493963677,31.078732573752,28.7543243873693));
#53525=CARTESIAN_POINT('Ctrl Pts',(131.030280484246,31.0452541612459,28.7485203894674));
#53526=CARTESIAN_POINT('Ctrl Pts',(130.914099774573,31.0167937561008,28.7427163915656));
#53527=CARTESIAN_POINT('Ctrl Pts',(130.796874481907,30.9934783090459,28.7369123936637));
#53528=CARTESIAN_POINT('Ctrl Pts',(130.679666507778,30.97016630655,28.7311092532284));
#53529=CARTESIAN_POINT('Ctrl Pts',(130.561414657923,30.9519978301704,28.725306112793));
#53530=CARTESIAN_POINT('Ctrl Pts',(130.442606791871,30.9390488518342,28.7195029723576));
#53531=CARTESIAN_POINT('Ctrl Pts',(130.32378844262,30.9260987309244,28.713699319873));
#53532=CARTESIAN_POINT('Ctrl Pts',(130.204414385562,30.9183690679873,28.7078956673884));
#53533=CARTESIAN_POINT('Ctrl Pts',(130.084977664052,30.9158839638653,28.7020920149038));
#53534=CARTESIAN_POINT('Ctrl Pts',(129.965502220096,30.9133980540505,28.6962864808235));
#53535=CARTESIAN_POINT('Ctrl Pts',(129.845964479303,30.916160093121,28.6904809467431));
#53536=CARTESIAN_POINT('Ctrl Pts',(129.72685690328,30.9241420720646,28.6846754126628));
#53537=CARTESIAN_POINT('Ctrl Pts',(129.607617453919,30.932132888483,28.6788634508204));
#53538=CARTESIAN_POINT('Ctrl Pts',(129.488809527649,30.9453551536462,28.6730514889781));
#53539=CARTESIAN_POINT('Ctrl Pts',(129.370920045251,30.963729021667,28.6672395271357));
#53540=CARTESIAN_POINT('Ctrl Pts',(129.252953145497,30.982114955703,28.6614237486109));
#53541=CARTESIAN_POINT('Ctrl Pts',(129.135906290161,31.0056591496562,28.655607970086));
#53542=CARTESIAN_POINT('Ctrl Pts',(129.020254170505,31.034231082175,28.6497921915611));
#53543=CARTESIAN_POINT('Ctrl Pts',(128.904436428454,31.0628439318158,28.643968084411));
#53544=CARTESIAN_POINT('Ctrl Pts',(128.790017799052,31.0964987762113,28.6381439772608));
#53545=CARTESIAN_POINT('Ctrl Pts',(128.677455975987,31.1350158726654,28.6323198701107));
#53546=CARTESIAN_POINT('Ctrl Pts',(128.64761418646,31.1452273196222,28.6307758139198));
#53547=CARTESIAN_POINT('Ctrl Pts',(128.61790278324,31.1557802566211,28.629231757729));
#53548=CARTESIAN_POINT('Ctrl Pts',(128.588330019733,31.1666707854902,28.6276877015381));
#53549=CARTESIAN_POINT('Ctrl Pts',(128.476791316995,31.2077462657013,28.6218640312394));
#53550=CARTESIAN_POINT('Ctrl Pts',(128.366867061984,31.253760178499,28.6160403609406));
#53551=CARTESIAN_POINT('Ctrl Pts',(128.259025636051,31.3045658896317,28.6102166906419));
#53552=CARTESIAN_POINT('Ctrl Pts',(128.151320237252,31.3553075163439,28.6044003661027));
#53553=CARTESIAN_POINT('Ctrl Pts',(128.045692808213,31.4108287471307,28.5985840415635));
#53554=CARTESIAN_POINT('Ctrl Pts',(127.942594525573,31.470933875117,28.5927677170243));
#53555=CARTESIAN_POINT('Ctrl Pts',(127.839599417534,31.5309788534823,28.5869572131151));
#53556=CARTESIAN_POINT('Ctrl Pts',(127.73912877147,31.5955983987234,28.581146709206));
#53557=CARTESIAN_POINT('Ctrl Pts',(127.641611246505,31.6645498823413,28.5753362052969));
#53558=CARTESIAN_POINT('Ctrl Pts',(127.540404360988,31.736109993319,28.5693058737833));
#53559=CARTESIAN_POINT('Ctrl Pts',(127.442378864502,31.8123361035121,28.5632755422696));
#53560=CARTESIAN_POINT('Ctrl Pts',(127.347983481711,31.8929059578566,28.557245210756));
#53561=CARTESIAN_POINT('Ctrl Pts',(127.257131479608,31.9704514093396,28.5514412437063));
#53562=CARTESIAN_POINT('Ctrl Pts',(127.16964231007,32.0520200861198,28.5456372766565));
#53563=CARTESIAN_POINT('Ctrl Pts',(127.085883603764,32.1372826494414,28.5398333096068));
#53564=CARTESIAN_POINT('Ctrl Pts',(127.002137254553,32.2225326338013,28.5340301988283));
#53565=CARTESIAN_POINT('Ctrl Pts',(126.922120560146,32.3114751297278,28.5282270880498));
#53566=CARTESIAN_POINT('Ctrl Pts',(126.846164480396,32.4037437500732,28.5224239772712));
#53567=CARTESIAN_POINT('Ctrl Pts',(126.770201682356,32.496020531548,28.5166203532095));
#53568=CARTESIAN_POINT('Ctrl Pts',(126.698300472598,32.5916237071096,28.5108167291477));
#53569=CARTESIAN_POINT('Ctrl Pts',(126.63075126853,32.6901541208372,28.5050131050859));
#53570=CARTESIAN_POINT('Ctrl Pts',(126.563180149476,32.7887165007823,28.4992075981547));
#53571=CARTESIAN_POINT('Ctrl Pts',(126.499964074872,32.8902076709954,28.4934020912234));
#53572=CARTESIAN_POINT('Ctrl Pts',(126.441349559543,32.9942003981873,28.4875965842922));
#53573=CARTESIAN_POINT('Ctrl Pts',(126.382670126589,33.09830830096,28.481784647559));
#53574=CARTESIAN_POINT('Ctrl Pts',(126.32860262635,33.2049229350681,28.4759727108259));
#53575=CARTESIAN_POINT('Ctrl Pts',(126.279347181127,33.3135932870715,28.4701607740928));
#53576=CARTESIAN_POINT('Ctrl Pts',(126.230059380157,33.4223350242861,28.4643450195168));
#53577=CARTESIAN_POINT('Ctrl Pts',(126.185590081203,33.5331347906707,28.4585292649407));
#53578=CARTESIAN_POINT('Ctrl Pts',(126.146090318909,33.6455240238415,28.4527135103647));
#53579=CARTESIAN_POINT('Ctrl Pts',(126.106533976932,33.7580742439836,28.446889425269));
#53580=CARTESIAN_POINT('Ctrl Pts',(126.071961497484,33.8722180857994,28.4410653401734));
#53581=CARTESIAN_POINT('Ctrl Pts',(126.042473430204,33.9874742228666,28.4352412550777));
#53582=CARTESIAN_POINT('Ctrl Pts',(126.034654268134,34.0180359550677,28.4336969197083));
#53583=CARTESIAN_POINT('Ctrl Pts',(126.027192318522,34.0486758547276,28.432152584339));
#53584=CARTESIAN_POINT('Ctrl Pts',(126.020088845761,34.0793848771795,28.4306082489696));
#53585=CARTESIAN_POINT('Ctrl Pts',(125.984344514023,34.2339111944862,28.4228372280037));
#53586=CARTESIAN_POINT('Ctrl Pts',(125.957588052264,34.3905878428019,28.4150662070378));
#53587=CARTESIAN_POINT('Ctrl Pts',(125.940025229609,34.5485247916084,28.407295186072));
#53588=CARTESIAN_POINT('Ctrl Pts',(125.923519238259,34.6969579883735,28.3999917811828));
#53589=CARTESIAN_POINT('Ctrl Pts',(125.915133455108,34.8465046131736,28.3926883762936));
#53590=CARTESIAN_POINT('Ctrl Pts',(125.915001580773,34.9964062674799,28.3853849714045));
#53591=CARTESIAN_POINT('Ctrl Pts',(125.915001580773,34.9964062680618,28.3853849713761));
#53592=CARTESIAN_POINT('Ctrl Pts',(125.914898004711,35.1141412731948,28.3796487677559));
#53593=CARTESIAN_POINT('Ctrl Pts',(125.919888554547,35.2320185491245,28.3739125641357));
#53594=CARTESIAN_POINT('Ctrl Pts',(125.929983362015,35.3495562422898,28.3681763605155));
#53595=CARTESIAN_POINT('Ctrl Pts',(125.940070876034,35.4670090150511,28.3624443012741));
#53596=CARTESIAN_POINT('Ctrl Pts',(125.955255278668,35.5841222759973,28.3567122420327));
#53597=CARTESIAN_POINT('Ctrl Pts',(125.975494634492,35.700415278957,28.3509801827913));
#53598=CARTESIAN_POINT('Ctrl Pts',(125.995726327814,35.8166642540619,28.3452502936742));
#53599=CARTESIAN_POINT('Ctrl Pts',(126.021009099457,35.9320931751257,28.3395204045571));
#53600=CARTESIAN_POINT('Ctrl Pts',(126.051249363658,36.0462281835202,28.33379051544));
#53601=CARTESIAN_POINT('Ctrl Pts',(126.0814857669,36.1603486195975,28.3280613578931));
#53602=CARTESIAN_POINT('Ctrl Pts',(126.116678296784,36.2731750655389,28.3223322003461));
#53603=CARTESIAN_POINT('Ctrl Pts',(126.156682817604,36.3842463781795,28.3166030427991));
#53604=CARTESIAN_POINT('Ctrl Pts',(126.196692269025,36.495331380479,28.3108731791273));
#53605=CARTESIAN_POINT('Ctrl Pts',(126.24151474706,36.6046604246836,28.3051433154555));
#53606=CARTESIAN_POINT('Ctrl Pts',(126.290957340198,36.7117907429857,28.2994134517837));
#53607=CARTESIAN_POINT('Ctrl Pts',(126.340448490637,36.8190262733863,28.2936779608442));
#53608=CARTESIAN_POINT('Ctrl Pts',(126.394568641031,36.9240583837005,28.2879424699047));
#53609=CARTESIAN_POINT('Ctrl Pts',(126.453078077212,37.0264673384101,28.2822069789652));
#53610=CARTESIAN_POINT('Ctrl Pts',(126.511616981188,37.1289278705461,28.2764685993929));
#53611=CARTESIAN_POINT('Ctrl Pts',(126.574549348282,37.2287622617238,28.2707302198206));
#53612=CARTESIAN_POINT('Ctrl Pts',(126.641592152127,37.3255798690533,28.2649918402483));
#53613=CARTESIAN_POINT('Ctrl Pts',(126.708740659179,37.4225501241103,28.2592444132453));
#53614=CARTESIAN_POINT('Ctrl Pts',(126.780012293326,37.5164937607468,28.2534969862422));
#53615=CARTESIAN_POINT('Ctrl Pts',(126.855083559348,37.6070530453589,28.2477495592392));
#53616=CARTESIAN_POINT('Ctrl Pts',(126.916999420102,37.6817428215291,28.2430093049598));
#53617=CARTESIAN_POINT('Ctrl Pts',(126.981499109161,37.754131023783,28.2382690506805));
#53618=CARTESIAN_POINT('Ctrl Pts',(127.04838334079,37.8240368441422,28.2335287964012));
#53619=CARTESIAN_POINT('Ctrl Pts',(127.130553566367,37.9099192246102,28.2277051851563));
#53620=CARTESIAN_POINT('Ctrl Pts',(127.21660774636,37.9923507865766,28.2218815739113));
#53621=CARTESIAN_POINT('Ctrl Pts',(127.306224543499,38.0709605647014,28.2160579626664));
#53622=CARTESIAN_POINT('Ctrl Pts',(127.395728278124,38.1494711670094,28.2102416986169));
#53623=CARTESIAN_POINT('Ctrl Pts',(127.488785385822,38.2241693087236,28.2044254345674));
#53624=CARTESIAN_POINT('Ctrl Pts',(127.585036396985,38.2947193804804,28.1986091705178));
#53625=CARTESIAN_POINT('Ctrl Pts',(127.681191062474,38.3651988327794,28.1927987284527));
#53626=CARTESIAN_POINT('Ctrl Pts',(127.780532943856,38.4315382352989,28.1869882863875));
#53627=CARTESIAN_POINT('Ctrl Pts',(127.882668531465,38.4934413480623,28.1811778443223));
#53628=CARTESIAN_POINT('Ctrl Pts',(127.988669720613,38.5576873539699,28.1751474901353));
#53629=CARTESIAN_POINT('Ctrl Pts',(128.097679927859,38.617154333157,28.1691171359482));
#53630=CARTESIAN_POINT('Ctrl Pts',(128.209224603579,38.6715594070603,28.1630867817611));
#53631=CARTESIAN_POINT('Ctrl Pts',(128.316580551466,38.72392146057,28.1572828795518));
#53632=CARTESIAN_POINT('Ctrl Pts',(128.426283651319,38.77159472813,28.1514789773425));
#53633=CARTESIAN_POINT('Ctrl Pts',(128.53788523552,38.8143735285746,28.1456750751332));
#53634=CARTESIAN_POINT('Ctrl Pts',(128.649470335548,38.857146010353,28.1398720301924));
#53635=CARTESIAN_POINT('Ctrl Pts',(128.762952981085,38.8950253166028,28.1340689852517));
#53636=CARTESIAN_POINT('Ctrl Pts',(128.877865165376,38.9278541740908,28.1282659403109));
#53637=CARTESIAN_POINT('Ctrl Pts',(128.992787495324,38.9606859300563,28.1224623830162));
#53638=CARTESIAN_POINT('Ctrl Pts',(129.109139222327,38.988466238516,28.1166588257215));
#53639=CARTESIAN_POINT('Ctrl Pts',(129.226438469627,39.0110880766603,28.1108552684268));
#53640=CARTESIAN_POINT('Ctrl Pts',(129.343775755335,39.0337172507317,28.1050498291244));
#53641=CARTESIAN_POINT('Ctrl Pts',(129.462060771685,39.0511845503497,28.099244389822));
#53642=CARTESIAN_POINT('Ctrl Pts',(129.580803414552,39.0634344122613,28.0934389505196));
#53643=CARTESIAN_POINT('Ctrl Pts',(129.699677551255,39.0756978394876,28.0876270823602));
#53644=CARTESIAN_POINT('Ctrl Pts',(129.819009919609,39.08273225427,28.0818152142007));
#53645=CARTESIAN_POINT('Ctrl Pts',(129.938307122138,39.0845341213927,28.0760033460413));
#53646=CARTESIAN_POINT('Ctrl Pts',(130.057682678586,39.0863371719744,28.0701876606704));
#53647=CARTESIAN_POINT('Ctrl Pts',(130.177022615984,39.0829008423141,28.0643719752995));
#53648=CARTESIAN_POINT('Ctrl Pts',(130.295837032635,39.0742736101202,28.0585562899286));
#53649=CARTESIAN_POINT('Ctrl Pts',(130.414821633508,39.0656340206817,28.0527322744416));
#53650=CARTESIAN_POINT('Ctrl Pts',(130.533278807089,39.0517887356762,28.0469082589546));
#53651=CARTESIAN_POINT('Ctrl Pts',(130.650727092607,39.0328376177262,28.0410842434676));
#53652=CARTESIAN_POINT('Ctrl Pts',(130.681883203419,39.0278103571897,28.0395392769226));
#53653=CARTESIAN_POINT('Ctrl Pts',(130.712968393572,39.0224240687474,28.0379943103777));
#53654=CARTESIAN_POINT('Ctrl Pts',(130.743973854194,39.0166812052085,28.0364493438327));
#53655=CARTESIAN_POINT('Ctrl Pts',(130.860849615099,38.995033355688,28.0306255587031));
#53656=CARTESIAN_POINT('Ctrl Pts',(130.976968212525,38.9682451577193,28.0248017735734));
#53657=CARTESIAN_POINT('Ctrl Pts',(131.091843191552,38.9363820247865,28.0189779884437));
#53658=CARTESIAN_POINT('Ctrl Pts',(131.20657781608,38.9045578222985,28.0131613188273));
#53659=CARTESIAN_POINT('Ctrl Pts',(131.320071453772,38.8676711237568,28.007344649211));
#53660=CARTESIAN_POINT('Ctrl Pts',(131.431846261862,38.8258386377879,28.0015279795946));
#53661=CARTESIAN_POINT('Ctrl Pts',(131.543491558863,38.7840546222295,27.9957180496294));
#53662=CARTESIAN_POINT('Ctrl Pts',(131.653421610726,38.7373363697412,27.9899081196642));
#53663=CARTESIAN_POINT('Ctrl Pts',(131.761173065314,38.685850571308,27.984098189699));
#53664=CARTESIAN_POINT('Ctrl Pts',(131.868852414126,38.6343992264558,27.9782921476582));
#53665=CARTESIAN_POINT('Ctrl Pts',(131.974355697965,38.5781868559141,27.9724861056175));
#53666=CARTESIAN_POINT('Ctrl Pts',(132.07723915953,38.517428389337,27.9666800635767));
#53667=CARTESIAN_POINT('Ctrl Pts',(132.180077496822,38.4566965711794,27.9608765680427));
#53668=CARTESIAN_POINT('Ctrl Pts',(132.280297947008,38.3914228312968,27.9550730725086));
#53669=CARTESIAN_POINT('Ctrl Pts',(132.377481582068,38.3218678972719,27.9492695769746));
#53670=CARTESIAN_POINT('Ctrl Pts',(132.414488708325,38.295381666091,27.9470596298799));
#53671=CARTESIAN_POINT('Ctrl Pts',(132.451055758543,38.2682750994043,27.9448496827852));
#53672=CARTESIAN_POINT('Ctrl Pts',(132.487160689988,38.2405642567579,27.9426397356904));
#53673=CARTESIAN_POINT('',(125.915001103447,35.0030025254734,28.4896150285558));
#53674=CARTESIAN_POINT('Ctrl Pts',(125.915001103447,35.0030025254734,28.4896150285558));
#53675=CARTESIAN_POINT('Ctrl Pts',(125.915102919105,35.1415248644931,28.4828889783069));
#53676=CARTESIAN_POINT('Ctrl Pts',(125.922254616048,35.2797632987396,28.4761629280581));
#53677=CARTESIAN_POINT('Ctrl Pts',(125.936346099466,35.4170635163571,28.4694368778092));
#53678=CARTESIAN_POINT('Ctrl Pts',(125.950518218314,35.5551494044232,28.4626723392097));
#53679=CARTESIAN_POINT('Ctrl Pts',(125.971709663148,35.6922861909673,28.4559078006102));
#53680=CARTESIAN_POINT('Ctrl Pts',(125.999759168527,35.8278274519563,28.4491432620107));
#53681=CARTESIAN_POINT('Ctrl Pts',(126.027989137381,35.9642407513876,28.4423352020683));
#53682=CARTESIAN_POINT('Ctrl Pts',(126.063165613499,36.0990378158406,28.4355271421258));
#53683=CARTESIAN_POINT('Ctrl Pts',(126.10507589336,36.2315807742544,28.4287190821834));
#53684=CARTESIAN_POINT('Ctrl Pts',(126.116063707408,36.2663301814467,28.4269341812731));
#53685=CARTESIAN_POINT('Ctrl Pts',(126.12751412061,36.3009247684037,28.4251492803627));
#53686=CARTESIAN_POINT('Ctrl Pts',(126.139422765552,36.3353532929025,28.4233643794524));
#53687=CARTESIAN_POINT('Ctrl Pts',(126.178277840155,36.4476853755434,28.4175406725268));
#53688=CARTESIAN_POINT('Ctrl Pts',(126.222102451514,36.558501283174,28.4117169656011));
#53689=CARTESIAN_POINT('Ctrl Pts',(126.270759287032,36.667329812827,28.4058932586755));
#53690=CARTESIAN_POINT('Ctrl Pts',(126.319354739941,36.7760210507917,28.4000768985968));
#53691=CARTESIAN_POINT('Ctrl Pts',(126.372770126904,36.8827295279913,28.3942605385182));
#53692=CARTESIAN_POINT('Ctrl Pts',(126.430818730963,36.9870002689362,28.3884441784395));
#53693=CARTESIAN_POINT('Ctrl Pts',(126.488809232551,37.0911666423827,28.3826336401182));
#53694=CARTESIAN_POINT('Ctrl Pts',(126.551423527991,37.1928997789442,28.3768231017969));
#53695=CARTESIAN_POINT('Ctrl Pts',(126.61842754107,37.2917662849882,28.3710125634756));
#53696=CARTESIAN_POINT('Ctrl Pts',(126.687965937794,37.3943723529533,28.3649822452843));
#53697=CARTESIAN_POINT('Ctrl Pts',(126.762232502365,37.493890242639,28.358951927093));
#53698=CARTESIAN_POINT('Ctrl Pts',(126.840913953207,37.5898649287092,28.3529216089017));
#53699=CARTESIAN_POINT('Ctrl Pts',(126.916642463719,37.6822376537309,28.3471176105049));
#53700=CARTESIAN_POINT('Ctrl Pts',(126.996460165988,37.771327993409,28.3413136121082));
#53701=CARTESIAN_POINT('Ctrl Pts',(127.080045079766,37.8567618493323,28.3355096137114));
#53702=CARTESIAN_POINT('Ctrl Pts',(127.163617644965,37.94218308352,28.3297064727796));
#53703=CARTESIAN_POINT('Ctrl Pts',(127.250956029385,38.0239486164502,28.3239033318477));
#53704=CARTESIAN_POINT('Ctrl Pts',(127.341700483724,38.1017202778081,28.3181001909158));
#53705=CARTESIAN_POINT('Ctrl Pts',(127.432452945057,38.1794988014839,28.3122965379338));
#53706=CARTESIAN_POINT('Ctrl Pts',(127.526611763807,38.2532824871939,28.3064928849517));
#53707=CARTESIAN_POINT('Ctrl Pts',(127.623783623465,38.3227730485074,28.3006892319696));
#53708=CARTESIAN_POINT('Ctrl Pts',(127.72098698711,38.3922861392827,28.2948836973912));
#53709=CARTESIAN_POINT('Ctrl Pts',(127.821205002449,38.4575031001514,28.2890781628129));
#53710=CARTESIAN_POINT('Ctrl Pts',(127.92401540947,38.518168981144,28.2832726282346));
#53711=CARTESIAN_POINT('Ctrl Pts',(128.026939645913,38.578902030066,28.2774606658961));
#53712=CARTESIAN_POINT('Ctrl Pts',(128.132461651413,38.6350737334926,28.2716487035575));
#53713=CARTESIAN_POINT('Ctrl Pts',(128.240134469473,38.6864750527383,28.2658367412189));
#53714=CARTESIAN_POINT('Ctrl Pts',(128.347877995648,38.7379101269329,28.2600209621984));
#53715=CARTESIAN_POINT('Ctrl Pts',(128.457774772286,38.7845684189146,28.2542051831778));
#53716=CARTESIAN_POINT('Ctrl Pts',(128.56935932259,38.82628961948,28.2483894041572));
#53717=CARTESIAN_POINT('Ctrl Pts',(128.68110367013,38.8680705678554,28.2425652965157));
#53718=CARTESIAN_POINT('Ctrl Pts',(128.794540228585,38.9049001872796,28.2367411888743));
#53719=CARTESIAN_POINT('Ctrl Pts',(128.909189757158,38.9366683901633,28.2309170812329));
#53720=CARTESIAN_POINT('Ctrl Pts',(128.939584932126,38.9450905799192,28.2293730297833));
#53721=CARTESIAN_POINT('Ctrl Pts',(128.970065315596,38.953157306727,28.2278289783336));
#53722=CARTESIAN_POINT('Ctrl Pts',(129.000621894753,38.9608671276318,28.226284926884));
#53723=CARTESIAN_POINT('Ctrl Pts',(129.115878570033,38.9899478804179,28.2204609033366));
#53724=CARTESIAN_POINT('Ctrl Pts',(129.232591433716,39.0140405845588,28.2146368797891));
#53725=CARTESIAN_POINT('Ctrl Pts',(129.350291032808,39.0330017676603,28.2088128562417));
#53726=CARTESIAN_POINT('Ctrl Pts',(129.467840460985,39.0519387585109,28.2029962634668));
#53727=CARTESIAN_POINT('Ctrl Pts',(129.586373720696,39.0657571869573,28.1971796706919));
#53728=CARTESIAN_POINT('Ctrl Pts',(129.705407868,39.0743638123962,28.1913630779171));
#53729=CARTESIAN_POINT('Ctrl Pts',(129.828536064991,39.0832664533314,28.1853464297768));
#53730=CARTESIAN_POINT('Ctrl Pts',(129.952199804614,39.0865921982106,28.1793297816366));
#53731=CARTESIAN_POINT('Ctrl Pts',(130.075854077224,39.0842956747729,28.1733131334963));
#53732=CARTESIAN_POINT('Ctrl Pts',(130.19517954854,39.082079546403,28.1675071119176));
#53733=CARTESIAN_POINT('Ctrl Pts',(130.314495756203,39.0746281826785,28.1617010903388));
#53734=CARTESIAN_POINT('Ctrl Pts',(130.433309747874,39.0619536755602,28.1558950687601));
#53735=CARTESIAN_POINT('Ctrl Pts',(130.552075622451,39.049284301343,28.1500913984944));
#53736=CARTESIAN_POINT('Ctrl Pts',(130.670339280224,39.0313960340944,28.1442877282288));
#53737=CARTESIAN_POINT('Ctrl Pts',(130.787611400039,39.0083529388677,28.1384840579631));
#53738=CARTESIAN_POINT('Ctrl Pts',(130.904863701188,38.9853137378605,28.1326813685017));
#53739=CARTESIAN_POINT('Ctrl Pts',(131.021124397455,38.9571215213546,28.1268786790403));
#53740=CARTESIAN_POINT('Ctrl Pts',(131.13591352441,38.9238916224918,28.1210759895789));
#53741=CARTESIAN_POINT('Ctrl Pts',(131.250710339632,38.8906594979799,28.115272911469));
#53742=CARTESIAN_POINT('Ctrl Pts',(131.364034997925,38.852389135171,28.1094698333591));
#53743=CARTESIAN_POINT('Ctrl Pts',(131.475422500075,38.8092457844398,28.1036667552492));
#53744=CARTESIAN_POINT('Ctrl Pts',(131.586890956033,38.7660710781394,28.0978594595991));
#53745=CARTESIAN_POINT('Ctrl Pts',(131.696419063995,38.7180164607688,28.0920521639489));
#53746=CARTESIAN_POINT('Ctrl Pts',(131.803561647476,38.6652954019771,28.0862448682988));
#53747=CARTESIAN_POINT('Ctrl Pts',(131.910750978871,38.6125513401973,28.0804350388386));
#53748=CARTESIAN_POINT('Ctrl Pts',(132.015552353511,38.5551369751747,28.0746252093783));
#53749=CARTESIAN_POINT('Ctrl Pts',(132.117546307303,38.4933111279171,28.068815379918));
#53750=CARTESIAN_POINT('Ctrl Pts',(132.219653685798,38.4314165258152,28.0629990895044));
#53751=CARTESIAN_POINT('Ctrl Pts',(132.318947071591,38.3651008737315,28.0571827990907));
#53752=CARTESIAN_POINT('Ctrl Pts',(132.415037021597,38.294665564866,28.051366508677));
#53753=CARTESIAN_POINT('Ctrl Pts',(132.439284017914,38.2768921694744,28.0498988466351));
#53754=CARTESIAN_POINT('Ctrl Pts',(132.463327209055,38.2588566565333,28.0484311845931));
#53755=CARTESIAN_POINT('Ctrl Pts',(132.487160689988,38.2405642567579,28.0469635225512));
#53756=CARTESIAN_POINT('Ctrl Pts',(132.487160689988,38.2405642567579,29.2969312480094));
#53757=CARTESIAN_POINT('Ctrl Pts',(132.582108042264,38.1676913545445,29.2911177030164));
#53758=CARTESIAN_POINT('Ctrl Pts',(132.673828553593,38.09065861231,29.2853041580235));
#53759=CARTESIAN_POINT('Ctrl Pts',(132.761950750955,38.0097928582048,29.2794906130305));
#53760=CARTESIAN_POINT('Ctrl Pts',(132.85016499061,37.9288426410506,29.2736709958783));
#53761=CARTESIAN_POINT('Ctrl Pts',(132.934773108887,37.8440516908564,29.2678513787261));
#53762=CARTESIAN_POINT('Ctrl Pts',(133.015439789088,37.7557844397532,29.2620317615739));
#53763=CARTESIAN_POINT('Ctrl Pts',(133.096149315893,37.6674703049552,29.2562090532962));
#53764=CARTESIAN_POINT('Ctrl Pts',(133.172912972251,37.5756765022524,29.2503863450185));
#53765=CARTESIAN_POINT('Ctrl Pts',(133.245436233957,37.4808000022812,29.2445636367407));
#53766=CARTESIAN_POINT('Ctrl Pts',(133.318075930572,37.3857711796431,29.2387315802002));
#53767=CARTESIAN_POINT('Ctrl Pts',(133.386461396551,37.287650104556,29.2328995236597));
#53768=CARTESIAN_POINT('Ctrl Pts',(133.450341557546,37.1868626240052,29.2270674671192));
#53769=CARTESIAN_POINT('Ctrl Pts',(133.506514652462,37.0982350341065,29.2219390413216));
#53770=CARTESIAN_POINT('Ctrl Pts',(133.559204577721,37.0075461828279,29.2168106155239));
#53771=CARTESIAN_POINT('Ctrl Pts',(133.608270922278,36.915099462545,29.2116821897262));
#53772=CARTESIAN_POINT('Ctrl Pts',(133.663941025846,36.8102104894807,29.2058635374938));
#53773=CARTESIAN_POINT('Ctrl Pts',(133.71512506242,36.7027201243151,29.2000448852614));
#53774=CARTESIAN_POINT('Ctrl Pts',(133.761571509473,36.5930488941413,29.194226233029));
#53775=CARTESIAN_POINT('Ctrl Pts',(133.807958816077,36.4835173087863,29.1884149897099));
#53776=CARTESIAN_POINT('Ctrl Pts',(133.849620372773,36.3718107547191,29.1826037463907));
#53777=CARTESIAN_POINT('Ctrl Pts',(133.886350153383,36.2583749382828,29.1767925030716));
#53778=CARTESIAN_POINT('Ctrl Pts',(133.923042786988,36.1450538462129,29.1709871370074));
#53779=CARTESIAN_POINT('Ctrl Pts',(133.954813441367,36.0300073578089,29.1651817709432));
#53780=CARTESIAN_POINT('Ctrl Pts',(133.981504125685,35.9137012078085,29.159376404879));
#53781=CARTESIAN_POINT('Ctrl Pts',(134.009237865327,35.7928498858889,29.153344168724));
#53782=CARTESIAN_POINT('Ctrl Pts',(134.031486323361,35.6706388565263,29.1473119325689));
#53783=CARTESIAN_POINT('Ctrl Pts',(134.048129187758,35.5476085090839,29.1412796964139));
#53784=CARTESIAN_POINT('Ctrl Pts',(134.064127785092,35.4293408274173,29.1354809760156));
#53785=CARTESIAN_POINT('Ctrl Pts',(134.074946651782,35.3103165242915,29.1296822556173));
#53786=CARTESIAN_POINT('Ctrl Pts',(134.080531129495,35.1910253941776,29.123883535219));
#53787=CARTESIAN_POINT('Ctrl Pts',(134.08611475254,35.071752520806,29.1180857022776));
#53788=CARTESIAN_POINT('Ctrl Pts',(134.086465560523,34.9522133102423,29.1122878693363));
#53789=CARTESIAN_POINT('Ctrl Pts',(134.081580924464,34.8329007568704,29.1064900363949));
#53790=CARTESIAN_POINT('Ctrl Pts',(134.07669587751,34.7135781669593,29.1006917157415));
#53791=CARTESIAN_POINT('Ctrl Pts',(134.066574527684,34.5944826809788,29.094893395088));
#53792=CARTESIAN_POINT('Ctrl Pts',(134.051266311449,34.4761047111119,29.0890950744346));
#53793=CARTESIAN_POINT('Ctrl Pts',(134.035953176953,34.3576887084832,29.0832948908826));
#53794=CARTESIAN_POINT('Ctrl Pts',(134.015449914474,34.2399910859764,29.0774947073306));
#53795=CARTESIAN_POINT('Ctrl Pts',(133.989857403606,34.1234939253545,29.0716945237786));
#53796=CARTESIAN_POINT('Ctrl Pts',(133.964236535414,34.0068676821355,29.0658879134368));
#53797=CARTESIAN_POINT('Ctrl Pts',(133.933515250763,33.8914449557314,29.0600813030951));
#53798=CARTESIAN_POINT('Ctrl Pts',(133.897844862505,33.7776946257816,29.0542746927534));
#53799=CARTESIAN_POINT('Ctrl Pts',(133.862151070597,33.6638696632573,29.0484642726444));
#53800=CARTESIAN_POINT('Ctrl Pts',(133.82150184772,33.5517196660969,29.0426538525354));
#53801=CARTESIAN_POINT('Ctrl Pts',(133.77609679007,33.4416938580555,29.0368434324265));
#53802=CARTESIAN_POINT('Ctrl Pts',(133.730626409303,33.3315097586448,29.0310246530119));
#53803=CARTESIAN_POINT('Ctrl Pts',(133.680386709373,33.2234563175936,29.0252058735973));
#53804=CARTESIAN_POINT('Ctrl Pts',(133.625623418858,33.1179586017766,29.0193870941828));
#53805=CARTESIAN_POINT('Ctrl Pts',(133.610614135122,33.0890442481051,29.0177923085078));
#53806=CARTESIAN_POINT('Ctrl Pts',(133.595265301974,33.0603217062284,29.0161975228328));
#53807=CARTESIAN_POINT('Ctrl Pts',(133.579582536377,33.0317993330807,29.0146027371578));
#53808=CARTESIAN_POINT('Ctrl Pts',(133.522308781787,32.9276350904959,29.0087785499115));
#53809=CARTESIAN_POINT('Ctrl Pts',(133.460392278334,32.8258050587369,29.0029543626652));
#53810=CARTESIAN_POINT('Ctrl Pts',(133.394048002963,32.7267505298394,28.9971301754189));
#53811=CARTESIAN_POINT('Ctrl Pts',(133.327787445879,32.6278209955326,28.9913133375782));
#53812=CARTESIAN_POINT('Ctrl Pts',(133.257110455119,32.5316603341817,28.9854964997374));
#53813=CARTESIAN_POINT('Ctrl Pts',(133.182277960134,32.4386854967721,28.9796796618966));
#53814=CARTESIAN_POINT('Ctrl Pts',(133.107520401396,32.345803763106,28.9738686489585));
#53815=CARTESIAN_POINT('Ctrl Pts',(133.028615871292,32.2561018229628,28.9680576360204));
#53816=CARTESIAN_POINT('Ctrl Pts',(132.945868332009,32.1699673552296,28.9622466230823));
#53817=CARTESIAN_POINT('Ctrl Pts',(132.86000048458,32.0805848624353,28.9562164839784));
#53818=CARTESIAN_POINT('Ctrl Pts',(132.769994341324,31.9950445607963,28.9501863448745));
#53819=CARTESIAN_POINT('Ctrl Pts',(132.676235460261,31.9137419483712,28.9441562057706));
#53820=CARTESIAN_POINT('Ctrl Pts',(132.585985493001,31.8354820755325,28.9383517438303));
#53821=CARTESIAN_POINT('Ctrl Pts',(132.492258968244,31.7611486928278,28.93254728189));
#53822=CARTESIAN_POINT('Ctrl Pts',(132.395436469808,31.6910561928139,28.9267428199497));
#53823=CARTESIAN_POINT('Ctrl Pts',(132.298628356826,31.6209741068308,28.9209392204105));
#53824=CARTESIAN_POINT('Ctrl Pts',(132.198725515535,31.5551318898012,28.9151356208712));
#53825=CARTESIAN_POINT('Ctrl Pts',(132.096139689627,31.4938021445485,28.909332021332));
#53826=CARTESIAN_POINT('Ctrl Pts',(131.993544909283,31.4324670459909,28.9035279152125));
#53827=CARTESIAN_POINT('Ctrl Pts',(131.888267029112,31.3756454118286,28.897723809093));
#53828=CARTESIAN_POINT('Ctrl Pts',(131.780744144132,31.3235648661862,28.8919197029735));
#53829=CARTESIAN_POINT('Ctrl Pts',(131.673186513296,31.2714674907951,28.8861137212659));
#53830=CARTESIAN_POINT('Ctrl Pts',(131.563382802075,31.2241144287547,28.8803077395584));
#53831=CARTESIAN_POINT('Ctrl Pts',(131.45179231755,31.1816857035201,28.8745017578509));
#53832=CARTESIAN_POINT('Ctrl Pts',(131.34007850799,31.1392100878714,28.8686893596204));
#53833=CARTESIAN_POINT('Ctrl Pts',(131.226574365335,31.1016698172517,28.86287696139));
#53834=CARTESIAN_POINT('Ctrl Pts',(131.111755787906,31.0691954935335,28.8570645631596));
#53835=CARTESIAN_POINT('Ctrl Pts',(130.996861934853,31.0366998794891,28.8512483542924));
#53836=CARTESIAN_POINT('Ctrl Pts',(130.880652327236,31.0092769203217,28.8454321454251));
#53837=CARTESIAN_POINT('Ctrl Pts',(130.763612893707,30.9870060617333,28.8396159365578));
#53838=CARTESIAN_POINT('Ctrl Pts',(130.646406108926,30.9647033586978,28.8337914112642));
#53839=CARTESIAN_POINT('Ctrl Pts',(130.528367532529,30.9475675185305,28.8279668859706));
#53840=CARTESIAN_POINT('Ctrl Pts',(130.409988183316,30.9356261626738,28.8221423606769));
#53841=CARTESIAN_POINT('Ctrl Pts',(130.37869503388,30.932469508783,28.8206026686477));
#53842=CARTESIAN_POINT('Ctrl Pts',(130.347378069137,30.929675557665,28.8190629766185));
#53843=CARTESIAN_POINT('Ctrl Pts',(130.316046338524,30.9272442116049,28.8175232845893));
#53844=CARTESIAN_POINT('Ctrl Pts',(130.197522854099,30.9180467749729,28.8116988484452));
#53845=CARTESIAN_POINT('Ctrl Pts',(130.078407074767,30.9140126755592,28.8058744123011));
#53846=CARTESIAN_POINT('Ctrl Pts',(129.959185995004,30.9152038952971,28.8000499761569));
#53847=CARTESIAN_POINT('Ctrl Pts',(129.840114987407,30.9163936155608,28.7942328716504));
#53848=CARTESIAN_POINT('Ctrl Pts',(129.720939347617,30.9227955683593,28.7884157671439));
#53849=CARTESIAN_POINT('Ctrl Pts',(129.602150885732,30.9344199574629,28.7825986626374));
#53850=CARTESIAN_POINT('Ctrl Pts',(129.483481017092,30.9460327412809,28.7767873656756));
#53851=CARTESIAN_POINT('Ctrl Pts',(129.365197961308,30.962857549474,28.7709760687138));
#53852=CARTESIAN_POINT('Ctrl Pts',(129.247792619923,30.9848525484912,28.765164771752));
#53853=CARTESIAN_POINT('Ctrl Pts',(129.125968040959,31.0076754581049,28.7591347325965));
#53854=CARTESIAN_POINT('Ctrl Pts',(129.005088998645,31.0360654235347,28.753104693441));
#53855=CARTESIAN_POINT('Ctrl Pts',(128.885697539091,31.0699166642917,28.7470746542856));
#53856=CARTESIAN_POINT('Ctrl Pts',(128.770765933651,31.1025033958794,28.7412698665429));
#53857=CARTESIAN_POINT('Ctrl Pts',(128.657213194814,31.1401505878394,28.7354650788002));
#53858=CARTESIAN_POINT('Ctrl Pts',(128.545510905086,31.1827121574636,28.7296602910574));
#53859=CARTESIAN_POINT('Ctrl Pts',(128.433824923314,31.225267513319,28.7238563507837));
#53860=CARTESIAN_POINT('Ctrl Pts',(128.323989234738,31.2727356746992,28.7180524105099));
#53861=CARTESIAN_POINT('Ctrl Pts',(128.216457538374,31.3249215943634,28.7122484702361));
#53862=CARTESIAN_POINT('Ctrl Pts',(128.108916185418,31.3771122004423,28.7064440087553));
#53863=CARTESIAN_POINT('Ctrl Pts',(128.003679603309,31.4340212289403,28.7006395472745));
#53864=CARTESIAN_POINT('Ctrl Pts',(127.901178305706,31.4954069429446,28.6948350857936));
#53865=CARTESIAN_POINT('Ctrl Pts',(127.798643633902,31.5568126440047,28.6890287343927));
#53866=CARTESIAN_POINT('Ctrl Pts',(127.698846367849,31.6226977198201,28.6832223829917));
#53867=CARTESIAN_POINT('Ctrl Pts',(127.602188827012,31.6927766058683,28.6774160315907));
#53868=CARTESIAN_POINT('Ctrl Pts',(127.505424146079,31.7629331708897,28.6716032441369));
#53869=CARTESIAN_POINT('Ctrl Pts',(127.411806467881,31.8372925854792,28.6657904566831));
#53870=CARTESIAN_POINT('Ctrl Pts',(127.321705864026,31.9155283238118,28.6599776692293));
#53871=CARTESIAN_POINT('Ctrl Pts',(127.231546010086,31.9938155099036,28.6541610592911));
#53872=CARTESIAN_POINT('Ctrl Pts',(127.144908132067,32.0759838160554,28.6483444493528));
#53873=CARTESIAN_POINT('Ctrl Pts',(127.062125006479,32.1616702935631,28.6425278394146));
#53874=CARTESIAN_POINT('Ctrl Pts',(126.979223314766,32.2474794955207,28.6367028986373));
#53875=CARTESIAN_POINT('Ctrl Pts',(126.900187664572,32.3368166215831,28.6308779578601));
#53876=CARTESIAN_POINT('Ctrl Pts',(126.825310272269,32.4292860655764,28.6250530170828));
#53877=CARTESIAN_POINT('Ctrl Pts',(126.805560500196,32.4536759433008,28.6235166220622));
#53878=CARTESIAN_POINT('Ctrl Pts',(126.78609978188,32.478283584601,28.6219802270415));
#53879=CARTESIAN_POINT('Ctrl Pts',(126.766932963214,32.5031014166276,28.6204438320209));
#53880=CARTESIAN_POINT('Ctrl Pts',(126.694299734928,32.5971493277878,28.6146216174838));
#53881=CARTESIAN_POINT('Ctrl Pts',(126.625652059009,32.6945265269436,28.6087994029467));
#53882=CARTESIAN_POINT('Ctrl Pts',(126.561310074298,32.7948613207151,28.6029771884095));
#53883=CARTESIAN_POINT('Ctrl Pts',(126.497047686161,32.8950719917106,28.5971621764529));
#53884=CARTESIAN_POINT('Ctrl Pts',(126.437080616818,32.9982326428979,28.5913471644963));
#53885=CARTESIAN_POINT('Ctrl Pts',(126.381688619243,33.1039388849808,28.5855321525397));
#53886=CARTESIAN_POINT('Ctrl Pts',(126.326352094297,33.209539266951,28.5797229640596));
#53887=CARTESIAN_POINT('Ctrl Pts',(126.275581717512,33.3176798110937,28.5739137755795));
#53888=CARTESIAN_POINT('Ctrl Pts',(126.229613436349,33.4279280675994,28.5681045870994));
#53889=CARTESIAN_POINT('Ctrl Pts',(126.183680361098,33.5380918878319,28.5622998477258));
#53890=CARTESIAN_POINT('Ctrl Pts',(126.142542221637,33.6503598341763,28.5564951083521));
#53891=CARTESIAN_POINT('Ctrl Pts',(126.106388287917,33.7642763919362,28.5506903689784));
#53892=CARTESIAN_POINT('Ctrl Pts',(126.070251448661,33.8781390871565,28.5448883742277));
#53893=CARTESIAN_POINT('Ctrl Pts',(126.039094251164,33.9936484553415,28.5390863794771));
#53894=CARTESIAN_POINT('Ctrl Pts',(126.013057024121,34.1103311250293,28.5332843847264));
#53895=CARTESIAN_POINT('Ctrl Pts',(125.987027103937,34.2269810499178,28.5274840181966));
#53896=CARTESIAN_POINT('Ctrl Pts',(125.966114381374,34.3448032226732,28.5216836516667));
#53897=CARTESIAN_POINT('Ctrl Pts',(125.950408541689,34.4633119893528,28.5158832851369));
#53898=CARTESIAN_POINT('Ctrl Pts',(125.934700116696,34.5818402635305,28.51008196382));
#53899=CARTESIAN_POINT('Ctrl Pts',(125.924200342196,34.7010549531536,28.5042806425031));
#53900=CARTESIAN_POINT('Ctrl Pts',(125.91894723897,34.8204634808992,28.4984793211861));
#53901=CARTESIAN_POINT('Ctrl Pts',(125.91627169654,34.8812813572605,28.4955245569893));
#53902=CARTESIAN_POINT('Ctrl Pts',(125.914956375683,34.9421494485323,28.4925697927924));
#53903=CARTESIAN_POINT('Ctrl Pts',(125.915001103446,35.0030025246561,28.4896150285955));
#53904=CARTESIAN_POINT('Origin',(-10.,-35.,23.));
#53905=CARTESIAN_POINT('',(-13.3897499995485,-34.9999446770898,27.6441405118761));
#53906=CARTESIAN_POINT('Ctrl Pts',(-13.1787501240208,-33.8227350716437,
28.823527842849));
#53907=CARTESIAN_POINT('Ctrl Pts',(-13.1664347419393,-33.7894821296968,
28.8213937451837));
#53908=CARTESIAN_POINT('Ctrl Pts',(-13.1535988325558,-33.7564258435817,
28.8192323989357));
#53909=CARTESIAN_POINT('Ctrl Pts',(-13.085816098104,-33.5896670296809,28.80814696636));
#53910=CARTESIAN_POINT('Ctrl Pts',(-13.022879052973,-33.4593846333745,28.7988925620819));
#53911=CARTESIAN_POINT('Ctrl Pts',(-12.8184844407376,-33.097339935892,28.7721199648883));
#53912=CARTESIAN_POINT('Ctrl Pts',(-12.6572518256493,-32.8779655398593,
28.7546513287065));
#53913=CARTESIAN_POINT('Ctrl Pts',(-12.4383404821078,-32.6447381700147,
28.7352504188843));
#53914=CARTESIAN_POINT('Ctrl Pts',(-12.4043530459316,-32.6100524293014,
28.7323364318189));
#53915=CARTESIAN_POINT('Ctrl Pts',(-12.3487401089221,-32.5556844553309,
28.7277200690391));
#53916=CARTESIAN_POINT('Ctrl Pts',(-12.327585824062,-32.5355319249923,28.7259976151087));
#53917=CARTESIAN_POINT('Ctrl Pts',(-12.2866215554542,-32.4975055266092,
28.7227245147918));
#53918=CARTESIAN_POINT('Ctrl Pts',(-12.2668560063183,-32.4795872096751,
28.7211720626376));
#53919=CARTESIAN_POINT('Ctrl Pts',(-12.2205463282811,-32.4385910048228,
28.7175950336669));
#53920=CARTESIAN_POINT('Ctrl Pts',(-12.1938501992873,-32.4156889754949,
28.7155777201542));
#53921=CARTESIAN_POINT('Ctrl Pts',(-12.1045830844938,-32.3414889675122,
28.70897249035));
#53922=CARTESIAN_POINT('Ctrl Pts',(-12.0405299715053,-32.2920137210762,
28.7044557148758));
#53923=CARTESIAN_POINT('Ctrl Pts',(-11.8769376434677,-32.1747572331746,
28.6933890627615));
#53924=CARTESIAN_POINT('Ctrl Pts',(-11.7754421846986,-32.1098963324565,
28.6869317737568));
#53925=CARTESIAN_POINT('Ctrl Pts',(-11.4581608150141,-31.9301720579015,
28.6675306025401));
#53926=CARTESIAN_POINT('Ctrl Pts',(-11.233248967079,-31.8331174030263,28.6548425334432));
#53927=CARTESIAN_POINT('Ctrl Pts',(-10.9661423848162,-31.7506582474366,
28.6390527099184));
#53928=CARTESIAN_POINT('Ctrl Pts',(-10.9322295454276,-31.7407668383586,
28.6370344285241));
#53929=CARTESIAN_POINT('Ctrl Pts',(-10.8808352001012,-31.726644292384,28.6339469142761));
#53930=CARTESIAN_POINT('Ctrl Pts',(-10.8634634546689,-31.7220190559795,
28.6328983763595));
#53931=CARTESIAN_POINT('Ctrl Pts',(-10.8315748877775,-31.7137997766585,
28.6309632414602));
#53932=CARTESIAN_POINT('Ctrl Pts',(-10.817069909998,-31.710163311502,28.6300789938724));
#53933=CARTESIAN_POINT('Ctrl Pts',(-10.7832159560899,-31.7019136642517,
28.6280060237918));
#53934=CARTESIAN_POINT('Ctrl Pts',(-10.763849965576,-31.6973746958279,28.6268133578898));
#53935=CARTESIAN_POINT('Ctrl Pts',(-10.6996812680255,-31.6829295177165,
28.6228414746318));
#53936=CARTESIAN_POINT('Ctrl Pts',(-10.6547191234464,-31.6737629527302,
28.620026318491));
#53937=CARTESIAN_POINT('Ctrl Pts',(-10.5425860673905,-31.6532635887739,
28.6129485295212));
#53938=CARTESIAN_POINT('Ctrl Pts',(-10.4752342145489,-31.6430377202951,
28.6086471784615));
#53939=CARTESIAN_POINT('Ctrl Pts',(-10.1120966137231,-31.599050548723,28.5853323537151));
#53940=CARTESIAN_POINT('Ctrl Pts',(-9.8130786471456,-31.6023342153103,28.5658500816704));
#53941=CARTESIAN_POINT('Ctrl Pts',(-9.4496437434001,-31.6545063114903,28.5432592343292));
#53942=CARTESIAN_POINT('Ctrl Pts',(-9.38127345527458,-31.6664735580105,
28.5390494595316));
#53943=CARTESIAN_POINT('Ctrl Pts',(-9.2807563734005,-31.6872671276796,28.5329178761918));
#53944=CARTESIAN_POINT('Ctrl Pts',(-9.24829796176518,-31.6944811842009,
28.5309467941138));
#53945=CARTESIAN_POINT('Ctrl Pts',(-9.19020673427615,-31.7082922203206,
28.5274339545297));
#53946=CARTESIAN_POINT('Ctrl Pts',(-9.16453544904484,-31.7147139724268,
28.5258868258147));
#53947=CARTESIAN_POINT('Ctrl Pts',(-9.10964819946747,-31.7291291655765,
28.5225891741485));
#53948=CARTESIAN_POINT('Ctrl Pts',(-9.08045873089549,-31.7372149497202,
28.5208417308572));
#53949=CARTESIAN_POINT('Ctrl Pts',(-8.99971853060223,-31.7607504226347,
28.5160230464574));
#53950=CARTESIAN_POINT('Ctrl Pts',(-8.94842032282783,-31.7770384009335,
28.512978596222));
#53951=CARTESIAN_POINT('Ctrl Pts',(-8.72526038916927,-31.8537909843778,
28.4997792099716));
#53952=CARTESIAN_POINT('Ctrl Pts',(-8.55804144064753,-31.926832853801,28.4900265194022));
#53953=CARTESIAN_POINT('Ctrl Pts',(-8.2094493043554,-32.1138486150595,28.4690274416487));
#53954=CARTESIAN_POINT('Ctrl Pts',(-8.03137366801509,-32.2322511425002,
28.4578582595488));
#53955=CARTESIAN_POINT('Ctrl Pts',(-7.83560566151058,-32.3909205510743,
28.4437285522146));
#53956=CARTESIAN_POINT('Ctrl Pts',(-7.80600363805133,-32.4157635299367,
28.4415360098675));
#53957=CARTESIAN_POINT('Ctrl Pts',(-7.76256052289224,-32.4535068891171,
28.4382227911626));
#53958=CARTESIAN_POINT('Ctrl Pts',(-7.74839133873374,-32.4660266420265,
28.4371265850077));
#53959=CARTESIAN_POINT('Ctrl Pts',(-7.72304488023586,-32.4888029641643,
28.4351357902192));
#53960=CARTESIAN_POINT('Ctrl Pts',(-7.71183010523102,-32.4990174538065,
28.434244187484));
#53961=CARTESIAN_POINT('Ctrl Pts',(-7.68852743559765,-32.5205296158759,
28.4323681017364));
#53962=CARTESIAN_POINT('Ctrl Pts',(-7.67645319261137,-32.5318409673775,
28.4313826781284));
#53963=CARTESIAN_POINT('Ctrl Pts',(-7.64386740223262,-32.5628188953921,
28.4286879622769));
#53964=CARTESIAN_POINT('Ctrl Pts',(-7.62352001762466,-32.5826553135429,
28.4269667644949));
#53965=CARTESIAN_POINT('Ctrl Pts',(-7.49095166150049,-32.7151860271487,
28.4155098764389));
#53966=CARTESIAN_POINT('Ctrl Pts',(-7.38654065519599,-32.8353939064203,
28.4053276982853));
#53967=CARTESIAN_POINT('Ctrl Pts',(-7.1294576219205,-33.1772041027171,28.3777820827545));
#53968=CARTESIAN_POINT('Ctrl Pts',(-6.9940278645292,-33.4104163243334,28.3604840768473));
#53969=CARTESIAN_POINT('Ctrl Pts',(-6.86818528590019,-33.7021043720864,
28.3412107000448));
#53970=CARTESIAN_POINT('Ctrl Pts',(-6.8497867398924,-33.7474213582024,28.3382752064751));
#53971=CARTESIAN_POINT('Ctrl Pts',(-6.821949819122,-33.820483401488,28.3336337200535));
#53972=CARTESIAN_POINT('Ctrl Pts',(-6.81187988924761,-33.8479789071961,
28.3319072409461));
#53973=CARTESIAN_POINT('Ctrl Pts',(-6.79332876434943,-33.9007390510442,
28.3286318459368));
#53974=CARTESIAN_POINT('Ctrl Pts',(-6.78478681449628,-33.9259798517561,
28.3270810492658));
#53975=CARTESIAN_POINT('Ctrl Pts',(-6.7657166710736,-33.9845980595745,28.3235155446851));
#53976=CARTESIAN_POINT('Ctrl Pts',(-6.75540588451315,-34.0180433268239,
28.3215079593414));
#53977=CARTESIAN_POINT('Ctrl Pts',(-6.72327730335093,-34.1282959067011,
28.3149720740905));
#53978=CARTESIAN_POINT('Ctrl Pts',(-6.70365412882489,-34.205717375016,28.3105128326565));
#53979=CARTESIAN_POINT('Ctrl Pts',(-6.66185766426764,-34.399062555541,28.2996307381464));
#53980=CARTESIAN_POINT('Ctrl Pts',(-6.6429674047542,-34.515588303047,28.293296213856));
#53981=CARTESIAN_POINT('Ctrl Pts',(-6.60310749272352,-34.8814508267982,
28.2737057227833));
#53982=CARTESIAN_POINT('Ctrl Pts',(-6.60361725714158,-35.1322368507821,
28.2607399063069));
#53983=CARTESIAN_POINT('Ctrl Pts',(-6.63549774844189,-35.4143420090158,
28.2446869956881));
#53984=CARTESIAN_POINT('Ctrl Pts',(-6.63981038557455,-35.4479735188258,
28.2427484127442));
#53985=CARTESIAN_POINT('Ctrl Pts',(-6.64716905914354,-35.4992495088584,
28.2397471785014));
#53986=CARTESIAN_POINT('Ctrl Pts',(-6.64985173843999,-35.5169448564233,
28.2387031183569));
#53987=CARTESIAN_POINT('Ctrl Pts',(-6.65503356128081,-35.5493890656727,
28.2367721788914));
#53988=CARTESIAN_POINT('Ctrl Pts',(-6.65749037941416,-35.5641438026397,
28.2358875785823));
#53989=CARTESIAN_POINT('Ctrl Pts',(-6.66345765598603,-35.5985730059391,
28.2338085276069));
#53990=CARTESIAN_POINT('Ctrl Pts',(-6.66704453521932,-35.6182331953278,
28.2326100459078));
#53991=CARTESIAN_POINT('Ctrl Pts',(-6.67954720466424,-35.683488621804,28.2285971216631));
#53992=CARTESIAN_POINT('Ctrl Pts',(-6.68922614790436,-35.7289303884995,
28.22574575664));
#53993=CARTESIAN_POINT('Ctrl Pts',(-6.71566829159229,-35.8416510562581,
28.2185538255722));
#53994=CARTESIAN_POINT('Ctrl Pts',(-6.73356735854304,-35.9086407933472,
28.214173060421));
#53995=CARTESIAN_POINT('Ctrl Pts',(-6.84517293719294,-36.2802461910706,
28.1894291968761));
#53996=CARTESIAN_POINT('Ctrl Pts',(-6.97945000499741,-36.5710859836512,
28.1685799872428));
#53997=CARTESIAN_POINT('Ctrl Pts',(-7.18196389076624,-36.8846881545117,
28.1458237051035));
#53998=CARTESIAN_POINT('Ctrl Pts',(-7.21263918001192,-36.9297660808519,
28.1425389127532));
#53999=CARTESIAN_POINT('Ctrl Pts',(-7.26229310237735,-36.9990775583663,
28.1374642901982));
#54000=CARTESIAN_POINT('Ctrl Pts',(-7.28053594663425,-37.0238244729718,
28.1356474544839));
#54001=CARTESIAN_POINT('Ctrl Pts',(-7.31507781192188,-37.0693708927981,
28.1322931276101));
#54002=CARTESIAN_POINT('Ctrl Pts',(-7.33128811514864,-37.090234432301,28.1307524030424));
#54003=CARTESIAN_POINT('Ctrl Pts',(-7.36805899127428,-37.136435376639,28.1273299518131));
#54004=CARTESIAN_POINT('Ctrl Pts',(-7.38874495738245,-37.161669910167,28.1254533369255));
#54005=CARTESIAN_POINT('Ctrl Pts',(-7.45232472404222,-37.2369852839618,
28.1198262986822));
#54006=CARTESIAN_POINT('Ctrl Pts',(-7.4963195580903,-37.2861184359444,28.1161200621157));
#54007=CARTESIAN_POINT('Ctrl Pts',(-7.60328320952698,-37.3987804986427,
28.1075033630551));
#54008=CARTESIAN_POINT('Ctrl Pts',(-7.66738850552402,-37.4611631984061,
28.1026378628716));
#54009=CARTESIAN_POINT('Ctrl Pts',(-7.83832518800311,-37.6148207464233,
28.0902757237925));
#54010=CARTESIAN_POINT('Ctrl Pts',(-7.94849654350741,-37.7021213735162,
28.0828776112622));
#54011=CARTESIAN_POINT('Ctrl Pts',(-8.20191219381496,-37.8784739635882,
28.0664724638875));
#54012=CARTESIAN_POINT('Ctrl Pts',(-8.34701326926217,-37.9641785485708,
28.0574602499881));
#54013=CARTESIAN_POINT('Ctrl Pts',(-8.52358290915223,-38.051462123326,28.0462496381849));
#54014=CARTESIAN_POINT('Ctrl Pts',(-8.54946691244673,-38.0638508715059,
28.0446002030662));
#54015=CARTESIAN_POINT('Ctrl Pts',(-8.59057299499792,-38.0828876642906,
28.0419665171148));
#54016=CARTESIAN_POINT('Ctrl Pts',(-8.60569256655494,-38.0897552635778,
28.0409947958848));
#54017=CARTESIAN_POINT('Ctrl Pts',(-8.63485571349489,-38.1027440791559,
28.0391136219904));
#54018=CARTESIAN_POINT('Ctrl Pts',(-8.64889127286791,-38.108881618297,28.0382051265547));
#54019=CARTESIAN_POINT('Ctrl Pts',(-8.68366834833717,-38.1238091365963,
28.0359471032101));
#54020=CARTESIAN_POINT('Ctrl Pts',(-8.70445663342249,-38.132487807545,28.034591307251));
#54021=CARTESIAN_POINT('Ctrl Pts',(-8.78486662299587,-38.1651199693079,
28.0293281096639));
#54022=CARTESIAN_POINT('Ctrl Pts',(-8.84507517890134,-38.1875823311257,
28.0253475628698));
#54023=CARTESIAN_POINT('Ctrl Pts',(-9.01305746573739,-38.2448685785511,
28.01420063812));
#54024=CARTESIAN_POINT('Ctrl Pts',(-9.12199280763895,-38.2760232947801,
28.0069281239153));
#54025=CARTESIAN_POINT('Ctrl Pts',(-9.48522498506772,-38.3604841774746,
27.9829007361708));
#54026=CARTESIAN_POINT('Ctrl Pts',(-9.74413799887095,-38.3900477324314,
27.9662071153393));
#54027=CARTESIAN_POINT('Ctrl Pts',(-10.0540330706947,-38.3896898622973,
27.9473877283307));
#54028=CARTESIAN_POINT('Ctrl Pts',(-10.1041460406995,-38.3885204646458,
27.9443769768559));
#54029=CARTESIAN_POINT('Ctrl Pts',(-10.1837181311802,-38.3848965786457,
27.9396460148026));
#54030=CARTESIAN_POINT('Ctrl Pts',(-10.2132013754226,-38.3831675181686,
27.937903914336));
#54031=CARTESIAN_POINT('Ctrl Pts',(-10.2691769407077,-38.3791501389735,
27.9346160004409));
#54032=CARTESIAN_POINT('Ctrl Pts',(-10.2956721313698,-38.3769349915463,
27.9330680621092));
#54033=CARTESIAN_POINT('Ctrl Pts',(-10.3564852158984,-38.3711294488342,
27.9295331155057));
#54034=CARTESIAN_POINT('Ctrl Pts',(-10.3907801338895,-38.3673263105263,
27.9275528074438));
#54035=CARTESIAN_POINT('Ctrl Pts',(-10.5011727091637,-38.3533750288404,
27.921216074775));
#54036=CARTESIAN_POINT('Ctrl Pts',(-10.5769879324629,-38.3411651099419,
27.9169227465679));
#54037=CARTESIAN_POINT('Ctrl Pts',(-10.7614770837294,-38.3049855625242,
27.9065624743554));
#54038=CARTESIAN_POINT('Ctrl Pts',(-10.86951169189,-38.2782203349786,27.9005722860236));
#54039=CARTESIAN_POINT('Ctrl Pts',(-11.1859260865101,-38.1830832972969,
27.882951953015));
#54040=CARTESIAN_POINT('Ctrl Pts',(-11.3891806596632,-38.0997746908322,
27.8715545986186));
#54041=CARTESIAN_POINT('Ctrl Pts',(-11.6385461628331,-37.9680841716859,
27.8560008211231));
#54042=CARTESIAN_POINT('Ctrl Pts',(-11.6933054711164,-37.9371879023392,
27.8524775299477));
#54043=CARTESIAN_POINT('Ctrl Pts',(-11.7668766783237,-37.892936343102,27.8475515907463));
#54044=CARTESIAN_POINT('Ctrl Pts',(-11.7864610685216,-37.8808836613223,
27.8462211614423));
#54045=CARTESIAN_POINT('Ctrl Pts',(-11.8188283880511,-37.8605071219958,
27.8439876874902));
#54046=CARTESIAN_POINT('Ctrl Pts',(-11.8316808914577,-37.8522943052936,
27.843091576731));
#54047=CARTESIAN_POINT('Ctrl Pts',(-11.8582286660767,-37.8350767043949,
27.8412204692755));
#54048=CARTESIAN_POINT('Ctrl Pts',(-11.8719146905146,-37.8260589275569,
27.8402447020276));
#54049=CARTESIAN_POINT('Ctrl Pts',(-11.9085456035975,-37.8015398435209,
27.8376040333474));
#54050=CARTESIAN_POINT('Ctrl Pts',(-11.9313663563749,-37.7858563685581,
27.8359279845345));
#54051=CARTESIAN_POINT('Ctrl Pts',(-12.0634906679487,-37.6926507652265,
27.826054018356));
#54052=CARTESIAN_POINT('Ctrl Pts',(-12.1683034294526,-37.6089874577042,
27.8175367606907));
#54053=CARTESIAN_POINT('Ctrl Pts',(-12.4839926721803,-37.324808943195,27.7902588940564));
#54054=CARTESIAN_POINT('Ctrl Pts',(-12.67421994575,-37.1032261240233,27.7714091509572));
#54055=CARTESIAN_POINT('Ctrl Pts',(-12.8619574118325,-36.8172044970381,
27.7506137814449));
#54056=CARTESIAN_POINT('Ctrl Pts',(-12.8891095031233,-36.7737190080863,
27.7475325195256));
#54057=CARTESIAN_POINT('Ctrl Pts',(-12.9304541467555,-36.7040333202694,
27.7427179377951));
#54058=CARTESIAN_POINT('Ctrl Pts',(-12.9453047393154,-36.6782345306933,
27.7409613767008));
#54059=CARTESIAN_POINT('Ctrl Pts',(-12.9727492137851,-36.6290707297088,
27.7376614990967));
#54060=CARTESIAN_POINT('Ctrl Pts',(-12.9854121699783,-36.6057470425886,
27.7361158348853));
#54061=CARTESIAN_POINT('Ctrl Pts',(-13.0137066887149,-36.5521399070339,
27.7326070554025));
#54062=CARTESIAN_POINT('Ctrl Pts',(-13.0291582335005,-36.5217643750974,
27.730650279473));
#54063=CARTESIAN_POINT('Ctrl Pts',(-13.0767917358651,-36.424522305688,27.7244804309158));
#54064=CARTESIAN_POINT('Ctrl Pts',(-13.1072384853675,-36.3568276497573,
27.7203256902728));
#54065=CARTESIAN_POINT('Ctrl Pts',(-13.1756517811604,-36.1903097389848,
27.7103905806528));
#54066=CARTESIAN_POINT('Ctrl Pts',(-13.2112600960353,-36.0906017298781,
27.7046782686266));
#54067=CARTESIAN_POINT('Ctrl Pts',(-13.3039133994116,-35.7869837233182,
27.6877200675271));
#54068=CARTESIAN_POINT('Ctrl Pts',(-13.346586441733,-35.5792549246931,27.6767111850404));
#54069=CARTESIAN_POINT('Ctrl Pts',(-13.377918515725,-35.2930745769432,27.6609627759639));
#54070=CARTESIAN_POINT('Ctrl Pts',(-13.3836585457924,-35.2169778751103,
27.6567169058938));
#54071=CARTESIAN_POINT('Ctrl Pts',(-13.3878253891392,-35.1167180987123,
27.6509730333547));
#54072=CARTESIAN_POINT('Ctrl Pts',(-13.3885684869205,-35.0926688788554,
27.6495839276084));
#54073=CARTESIAN_POINT('Ctrl Pts',(-13.389334991484,-35.0548091612999,27.6473764827574));
#54074=CARTESIAN_POINT('Ctrl Pts',(-13.3895301311732,-35.0410024856843,
27.6465671551311));
#54075=CARTESIAN_POINT('Ctrl Pts',(-13.3897137852033,-35.0181116961334,
27.6452176133072));
#54076=CARTESIAN_POINT('Ctrl Pts',(-13.389750147796,-35.0090281067772,27.644680047935));
#54077=CARTESIAN_POINT('Ctrl Pts',(-13.3897499995485,-34.9999446770898,
27.6441405118761));
#54078=CARTESIAN_POINT('Ctrl Pts',(-13.3897499995572,-34.999945207804,27.6441405433994));
#54079=CARTESIAN_POINT('Ctrl Pts',(-13.3897499123749,-34.994551631023,27.6438201766608));
#54080=CARTESIAN_POINT('Ctrl Pts',(-13.3897369522656,-34.989158097162,27.6434991162569));
#54081=CARTESIAN_POINT('Ctrl Pts',(-13.3896571545376,-34.9724974592523,
27.6425052569258));
#54082=CARTESIAN_POINT('Ctrl Pts',(-13.3895470131806,-34.9612307753627,
27.6418301927998));
#54083=CARTESIAN_POINT('Ctrl Pts',(-13.3888739786967,-34.9156392667992,
27.639087033885));
#54084=CARTESIAN_POINT('Ctrl Pts',(-13.3878458534473,-34.8813245789518,
27.6369961020113));
#54085=CARTESIAN_POINT('Ctrl Pts',(-13.3760246063147,-34.6196327011655,
27.6208789136258));
#54086=CARTESIAN_POINT('Ctrl Pts',(-13.3428736881132,-34.3938588597364,
27.6060295639237));
#54087=CARTESIAN_POINT('Ctrl Pts',(-13.2574968510191,-34.0544322309172,
27.583549957105));
#54088=CARTESIAN_POINT('Ctrl Pts',(-13.2212412264666,-33.9374659252775,
27.5757646113467));
#54089=CARTESIAN_POINT('Ctrl Pts',(-13.1787501609633,-33.8227351713926,
27.5681448070208));
#54090=CARTESIAN_POINT('',(-13.3897486873357,-35.0029831537265,27.9839821967052));
#54091=CARTESIAN_POINT('Ctrl Pts',(-13.1787501240207,-33.8227350716434,
27.9134187994658));
#54092=CARTESIAN_POINT('Ctrl Pts',(-13.2144036035584,-33.9190035493433,
27.9194227889449));
#54093=CARTESIAN_POINT('Ctrl Pts',(-13.2456876111846,-34.016914363963,27.925426778424));
#54094=CARTESIAN_POINT('Ctrl Pts',(-13.2724607141584,-34.1160283167489,
27.9314307679031));
#54095=CARTESIAN_POINT('Ctrl Pts',(-13.2992340062708,-34.2151429697253,
27.9374347997973));
#54096=CARTESIAN_POINT('Ctrl Pts',(-13.3214962229816,-34.3154603506665,
27.9434388316916));
#54097=CARTESIAN_POINT('Ctrl Pts',(-13.3391564678312,-34.4165283675782,
27.9494428635859));
#54098=CARTESIAN_POINT('Ctrl Pts',(-13.3568326196948,-34.5176874189217,
27.9554523034583));
#54099=CARTESIAN_POINT('Ctrl Pts',(-13.3698984504733,-34.6195980214031,
27.9614617433308));
#54100=CARTESIAN_POINT('Ctrl Pts',(-13.3783146793759,-34.7218004500127,
27.9674711832033));
#54101=CARTESIAN_POINT('Ctrl Pts',(-13.3860225785033,-34.8154012799579,
27.9729748543706));
#54102=CARTESIAN_POINT('Ctrl Pts',(-13.3898311803767,-34.9092465570969,
27.9784785255379));
#54103=CARTESIAN_POINT('Ctrl Pts',(-13.3897486873357,-35.0029831537265,
27.9839821967052));
#54104=CARTESIAN_POINT('Ctrl Pts',(-13.1787501097524,-33.8227350331175,
29.1634929519179));
#54105=CARTESIAN_POINT('Ctrl Pts',(-13.1341008506572,-33.7021769249243,
29.1566764597228));
#54106=CARTESIAN_POINT('Ctrl Pts',(-13.0826222281607,-33.5842375125987,
29.1498322043012));
#54107=CARTESIAN_POINT('Ctrl Pts',(-12.9813983847272,-33.3842011618824,
29.1376014467608));
#54108=CARTESIAN_POINT('Ctrl Pts',(-12.9346538431717,-33.3007805148027,
29.1322993107299));
#54109=CARTESIAN_POINT('Ctrl Pts',(-12.8649298389742,-33.1878291933825,
29.1247662346228));
#54110=CARTESIAN_POINT('Ctrl Pts',(-12.8448919349152,-33.1565316009532,
29.122639606394));
#54111=CARTESIAN_POINT('Ctrl Pts',(-12.8094979716464,-33.1032008479741,
29.1189440686014));
#54112=CARTESIAN_POINT('Ctrl Pts',(-12.7943869442591,-33.081008749247,29.1173842923023));
#54113=CARTESIAN_POINT('Ctrl Pts',(-12.7628792651954,-33.0358978577039,
29.1141670656781));
#54114=CARTESIAN_POINT('Ctrl Pts',(-12.7464572799425,-33.0129993968743,
29.1125087344198));
#54115=CARTESIAN_POINT('Ctrl Pts',(-12.7036125563011,-32.9548036521409,
29.1082275071958));
#54116=CARTESIAN_POINT('Ctrl Pts',(-12.6767837881576,-32.9198131740124,
29.1055891568768));
#54117=CARTESIAN_POINT('Ctrl Pts',(-12.5489175186532,-32.7596188946876,
29.0932021646422));
#54118=CARTESIAN_POINT('Ctrl Pts',(-12.4397427093475,-32.6412011765305,
29.0831355219448));
#54119=CARTESIAN_POINT('Ctrl Pts',(-12.1783550529947,-32.3953146486059,
29.0602212240801));
#54120=CARTESIAN_POINT('Ctrl Pts',(-12.02251638337,-32.2725392724793,29.0473038315074));
#54121=CARTESIAN_POINT('Ctrl Pts',(-11.7843267739212,-32.116582171182,29.029231915516));
#54122=CARTESIAN_POINT('Ctrl Pts',(-11.7099982471548,-32.0718898943673,
29.0238068675787));
#54123=CARTESIAN_POINT('Ctrl Pts',(-11.6123434904894,-32.0181605779497,
29.0170234316381));
#54124=CARTESIAN_POINT('Ctrl Pts',(-11.5905238328035,-32.0064649849654,
29.0155291669482));
#54125=CARTESIAN_POINT('Ctrl Pts',(-11.5546677528406,-31.9877484444146,
29.013110821397));
#54126=CARTESIAN_POINT('Ctrl Pts',(-11.540707522233,-31.9805842258255,29.0121783507766));
#54127=CARTESIAN_POINT('Ctrl Pts',(-11.5124988338076,-31.9663544625593,
29.0103131445429));
#54128=CARTESIAN_POINT('Ctrl Pts',(-11.498249521214,-31.9592917989708,29.009380558242));
#54129=CARTESIAN_POINT('Ctrl Pts',(-11.4610961217925,-31.9412013216437,
29.0069724723049));
#54130=CARTESIAN_POINT('Ctrl Pts',(-11.4381163447554,-31.9303301980402,
29.0055060924296));
#54131=CARTESIAN_POINT('Ctrl Pts',(-11.3372728856087,-31.8840048638483,
28.9991619815716));
#54132=CARTESIAN_POINT('Ctrl Pts',(-11.2581997154204,-31.8512446629565,
28.9944217215085));
#54133=CARTESIAN_POINT('Ctrl Pts',(-10.9923698373936,-31.7527266557703,
28.9789895680065));
#54134=CARTESIAN_POINT('Ctrl Pts',(-10.8010989965715,-31.7003288552688,
28.9686679209581));
#54135=CARTESIAN_POINT('Ctrl Pts',(-10.4494790577306,-31.6364018067372,
28.9495863238047));
#54136=CARTESIAN_POINT('Ctrl Pts',(-10.2908154804733,-31.6189878608985,
28.9409405588369));
#54137=CARTESIAN_POINT('Ctrl Pts',(-10.0873587375544,-31.6110876188855,
28.9294613717095));
#54138=CARTESIAN_POINT('Ctrl Pts',(-10.0431645338026,-31.6102366977027,
28.9269453096083));
#54139=CARTESIAN_POINT('Ctrl Pts',(-9.97061668238919,-31.6102587910637,
28.9227721034821));
#54140=CARTESIAN_POINT('Ctrl Pts',(-9.94226753781605,-31.6106231052204,
28.9211306243353));
#54141=CARTESIAN_POINT('Ctrl Pts',(-9.88683934256462,-31.6120310010794,
28.9178987971465));
#54142=CARTESIAN_POINT('Ctrl Pts',(-9.8597616093796,-31.6130437849761,28.9163095181377));
#54143=CARTESIAN_POINT('Ctrl Pts',(-9.79508590705522,-31.6162397375263,
28.9124873169503));
#54144=CARTESIAN_POINT('Ctrl Pts',(-9.75750709968905,-31.6187250449724,
28.9102452928013));
#54145=CARTESIAN_POINT('Ctrl Pts',(-9.62219673189963,-31.6299411367559,
28.902092987353));
#54146=CARTESIAN_POINT('Ctrl Pts',(-9.52482100973745,-31.642287366852,28.8960746481012));
#54147=CARTESIAN_POINT('Ctrl Pts',(-9.26544890108731,-31.6866816681431,
28.8796442261479));
#54148=CARTESIAN_POINT('Ctrl Pts',(-9.10503606589438,-31.7263666729971,
28.869047553));
#54149=CARTESIAN_POINT('Ctrl Pts',(-8.78242321748637,-31.8316709683176,
28.8471835559908));
#54150=CARTESIAN_POINT('Ctrl Pts',(-8.62109019404132,-31.8984812166077,
28.8359450909284));
#54151=CARTESIAN_POINT('Ctrl Pts',(-8.43387832991036,-31.9935180171217,
28.8230211210226));
#54152=CARTESIAN_POINT('Ctrl Pts',(-8.40240636232595,-32.0101227813293,
28.8208532698331));
#54153=CARTESIAN_POINT('Ctrl Pts',(-8.35536484955722,-32.0358970450037,
28.8176266623488));
#54154=CARTESIAN_POINT('Ctrl Pts',(-8.33959850175203,-32.0447000147807,
28.8165476025892));
#54155=CARTESIAN_POINT('Ctrl Pts',(-8.31088376206896,-32.0610349193159,
28.8145877414521));
#54156=CARTESIAN_POINT('Ctrl Pts',(-8.29791428321023,-32.0685270535017,
28.8137046864572));
#54157=CARTESIAN_POINT('Ctrl Pts',(-8.26784417326212,-32.0861646297984,
28.811661946619));
#54158=CARTESIAN_POINT('Ctrl Pts',(-8.2507825991845,-32.0963748694272,28.8105063123233));
#54159=CARTESIAN_POINT('Ctrl Pts',(-8.19474583146499,-32.1305824158147,
28.8067187287056));
#54160=CARTESIAN_POINT('Ctrl Pts',(-8.15616527750445,-32.1552198993775,
28.8041238623235));
#54161=CARTESIAN_POINT('Ctrl Pts',(-8.06165523712683,-32.2183046290798,
28.797769234912));
#54162=CARTESIAN_POINT('Ctrl Pts',(-8.00635778306566,-32.2576650105475,
28.7940528068173));
#54163=CARTESIAN_POINT('Ctrl Pts',(-7.71815124300348,-32.4761371130312,
28.7744870534131));
#54164=CARTESIAN_POINT('Ctrl Pts',(-7.50809522385788,-32.6832915669291,
28.7594036472472));
#54165=CARTESIAN_POINT('Ctrl Pts',(-7.28298630627063,-32.9718361012953,
28.7391812061063));
#54166=CARTESIAN_POINT('Ctrl Pts',(-7.24043029172502,-33.0301304032548,
28.7351372438304));
#54167=CARTESIAN_POINT('Ctrl Pts',(-7.18075567495961,-33.1176066325867,
28.7291006171509));
#54168=CARTESIAN_POINT('Ctrl Pts',(-7.16216026879386,-33.1457592127428,
28.72716256565));
#54169=CARTESIAN_POINT('Ctrl Pts',(-7.129707135741,-33.196523646232,28.7236737431847));
#54170=CARTESIAN_POINT('Ctrl Pts',(-7.11568854195321,-33.2190296354606,
28.722129013886));
#54171=CARTESIAN_POINT('Ctrl Pts',(-7.0863786463198,-33.2673387021508,28.7188163836387));
#54172=CARTESIAN_POINT('Ctrl Pts',(-7.07116297257799,-33.2931847944357,
28.7170459364889));
#54173=CARTESIAN_POINT('Ctrl Pts',(-7.03035050290647,-33.3646638671613,
28.7121531846486));
#54174=CARTESIAN_POINT('Ctrl Pts',(-7.00546493573918,-33.4106914410072,
28.7090063679964));
#54175=CARTESIAN_POINT('Ctrl Pts',(-6.90412754409968,-33.6089582018583,
28.6954613785215));
#54176=CARTESIAN_POINT('Ctrl Pts',(-6.8381532885114,-33.7662512326336,28.6847234058602));
#54177=CARTESIAN_POINT('Ctrl Pts',(-6.72464210624342,-34.106696775112,28.6617145854371));
#54178=CARTESIAN_POINT('Ctrl Pts',(-6.68002961627969,-34.2902406705934,
28.6494403593251));
#54179=CARTESIAN_POINT('Ctrl Pts',(-6.63989810842761,-34.5470030944697,
28.6330502692425));
#54180=CARTESIAN_POINT('Ctrl Pts',(-6.63111087840936,-34.6177979345041,
28.6286139039283));
#54181=CARTESIAN_POINT('Ctrl Pts',(-6.62235577805131,-34.7127669700333,
28.6228166986049));
#54182=CARTESIAN_POINT('Ctrl Pts',(-6.62040309298162,-34.736735642969,28.6213666593028));
#54183=CARTESIAN_POINT('Ctrl Pts',(-6.61771264564724,-34.7747552808034,
28.6190894204333));
#54184=CARTESIAN_POINT('Ctrl Pts',(-6.61680704249519,-34.7887930896588,
28.6182535348629));
#54185=CARTESIAN_POINT('Ctrl Pts',(-6.61507624842204,-34.8184995194161,
28.6164956566593));
#54186=CARTESIAN_POINT('Ctrl Pts',(-6.61427240748996,-34.8341690214957,
28.6155749141646));
#54187=CARTESIAN_POINT('Ctrl Pts',(-6.61249405559459,-34.8742755966487,
28.6132336131238));
#54188=CARTESIAN_POINT('Ctrl Pts',(-6.61167513142788,-34.8987191630877,
28.6118212541202));
#54189=CARTESIAN_POINT('Ctrl Pts',(-6.60925421008101,-35.0055033773342,
28.605706686524));
#54190=CARTESIAN_POINT('Ctrl Pts',(-6.61038854584917,-35.0878836361065,
28.6011332281708));
#54191=CARTESIAN_POINT('Ctrl Pts',(-6.62343024225929,-35.3473797153306,
28.5869589228742));
#54192=CARTESIAN_POINT('Ctrl Pts',(-6.64624164788816,-35.5236479487111,
28.5776606781066));
#54193=CARTESIAN_POINT('Ctrl Pts',(-6.72047610361767,-35.8767883349627,
28.5584740101881));
#54194=CARTESIAN_POINT('Ctrl Pts',(-6.77269752704192,-36.0528739573895,
28.5486025110094));
#54195=CARTESIAN_POINT('Ctrl Pts',(-6.85507095372378,-36.265635354014,28.5357479975101));
#54196=CARTESIAN_POINT('Ctrl Pts',(-6.87206954965174,-36.3070816308171,
28.5331994250152));
#54197=CARTESIAN_POINT('Ctrl Pts',(-6.90118750153499,-36.374253946467,28.5289895089035));
#54198=CARTESIAN_POINT('Ctrl Pts',(-6.91281835599816,-36.4001865002447,
28.5273445186338));
#54199=CARTESIAN_POINT('Ctrl Pts',(-6.93610801114565,-36.4504126634799,
28.5241184661231));
#54200=CARTESIAN_POINT('Ctrl Pts',(-6.9477331276999,-36.4747195976138,28.5225386408883));
#54201=CARTESIAN_POINT('Ctrl Pts',(-6.97604373195173,-36.5321451187126,
28.5187607463818));
#54202=CARTESIAN_POINT('Ctrl Pts',(-6.9929850987164,-36.5651330280031,28.516554016426));
#54203=CARTESIAN_POINT('Ctrl Pts',(-7.05484667928038,-36.6808755104915,
28.5086782201529));
#54204=CARTESIAN_POINT('Ctrl Pts',(-7.10266663729085,-36.7620236677082,
28.5029101450212));
#54205=CARTESIAN_POINT('Ctrl Pts',(-7.23715489530556,-36.969935621708,28.4874737473239));
#54206=CARTESIAN_POINT('Ctrl Pts',(-7.3291601632739,-37.0929803967567,28.4776485274617));
#54207=CARTESIAN_POINT('Ctrl Pts',(-7.55541247795924,-37.3562489256483,
28.4552818605003));
#54208=CARTESIAN_POINT('Ctrl Pts',(-7.69401412460238,-37.4920586855317,
28.4427375133697));
#54209=CARTESIAN_POINT('Ctrl Pts',(-7.87019009517371,-37.6373309861613,
28.428684892285));
#54210=CARTESIAN_POINT('Ctrl Pts',(-7.89725291093571,-37.65895841271,28.4265745383328));
#54211=CARTESIAN_POINT('Ctrl Pts',(-7.93891017733314,-37.691215223772,28.4234046817938));
#54212=CARTESIAN_POINT('Ctrl Pts',(-7.95326509800031,-37.7021485730608,
28.4223262128984));
#54213=CARTESIAN_POINT('Ctrl Pts',(-7.97966099617803,-37.721921831851,28.4203693311496));
#54214=CARTESIAN_POINT('Ctrl Pts',(-7.99167367271867,-37.7307972322945,
28.419488637862));
#54215=CARTESIAN_POINT('Ctrl Pts',(-8.01971669637135,-37.7512312923336,
28.4174551325651));
#54216=CARTESIAN_POINT('Ctrl Pts',(-8.03578995516797,-37.7627295428876,
28.4163062980315));
#54217=CARTESIAN_POINT('Ctrl Pts',(-8.08888515917287,-37.8000143910725,
28.4125625485804));
#54218=CARTESIAN_POINT('Ctrl Pts',(-8.12632284978902,-37.8252035086741,
28.4100036156142));
#54219=CARTESIAN_POINT('Ctrl Pts',(-8.22016284563578,-37.8856555154309,
28.4037577383386));
#54220=CARTESIAN_POINT('Ctrl Pts',(-8.27712235126746,-37.9200208119295,
28.40011230084));
#54221=CARTESIAN_POINT('Ctrl Pts',(-8.57418272803949,-38.0875250714524,
28.3816478870716));
#54222=CARTESIAN_POINT('Ctrl Pts',(-8.82879785374734,-38.1928139604689,
28.3675222665316));
#54223=CARTESIAN_POINT('Ctrl Pts',(-9.17584074389774,-38.2891486536877,
28.3477866805065));
#54224=CARTESIAN_POINT('Ctrl Pts',(-9.2591826939759,-38.3089160558987,28.3430213134391));
#54225=CARTESIAN_POINT('Ctrl Pts',(-9.37573350284544,-38.3319360008063,
28.3362743725662));
#54226=CARTESIAN_POINT('Ctrl Pts',(-9.40837939797173,-38.3378872249599,
28.3343758139665));
#54227=CARTESIAN_POINT('Ctrl Pts',(-9.46542756567714,-38.3474236978603,
28.3310404631353));
#54228=CARTESIAN_POINT('Ctrl Pts',(-9.48979167137738,-38.3512237339599,
28.3296104314202));
#54229=CARTESIAN_POINT('Ctrl Pts',(-9.54120745208911,-38.3586692984014,
28.3265799304701));
#54230=CARTESIAN_POINT('Ctrl Pts',(-9.56826594492124,-38.3622545559208,
28.3249777016695));
#54231=CARTESIAN_POINT('Ctrl Pts',(-9.63405956671405,-38.3701649272472,
28.3210627840895));
#54232=CARTESIAN_POINT('Ctrl Pts',(-9.67283100420665,-38.3741494181034,
28.3187397692326));
#54233=CARTESIAN_POINT('Ctrl Pts',(-9.82042713161933,-38.3867498966942,
28.3098324414982));
#54234=CARTESIAN_POINT('Ctrl Pts',(-9.9295679435339,-38.3907752388314,28.3031111114502));
#54235=CARTESIAN_POINT('Ctrl Pts',(-10.2409523380736,-38.3872195929405,
28.2835720651901));
#54236=CARTESIAN_POINT('Ctrl Pts',(-10.4425764903608,-38.3668128946524,
28.2704593358006));
#54237=CARTESIAN_POINT('Ctrl Pts',(-10.7756025125774,-38.3026643305676,
28.2486687382601));
#54238=CARTESIAN_POINT('Ctrl Pts',(-10.9083670477982,-38.2686429996786,
28.2399553930302));
#54239=CARTESIAN_POINT('Ctrl Pts',(-11.0655311581706,-38.2180493717434,
28.2298674715829));
#54240=CARTESIAN_POINT('Ctrl Pts',(-11.0922349017072,-38.2090842057795,
28.2281617377294));
#54241=CARTESIAN_POINT('Ctrl Pts',(-11.1343968820166,-38.1943420161088,
28.2254852114822));
#54242=CARTESIAN_POINT('Ctrl Pts',(-11.1499294545838,-38.1887833849867,
28.224502784887));
#54243=CARTESIAN_POINT('Ctrl Pts',(-11.1798643120017,-38.1778234429967,
28.2226172704239));
#54244=CARTESIAN_POINT('Ctrl Pts',(-11.194271320391,-38.1724371782705,28.2217134377073));
#54245=CARTESIAN_POINT('Ctrl Pts',(-11.2299946806446,-38.158803653946,28.2194802901512));
#54246=CARTESIAN_POINT('Ctrl Pts',(-11.2512656695106,-38.1504383384015,
28.2181576685891));
#54247=CARTESIAN_POINT('Ctrl Pts',(-11.3345206370969,-38.1167201179939,
28.2130028053058));
#54248=CARTESIAN_POINT('Ctrl Pts',(-11.3958358477449,-38.0897464442777,
28.20925430883));
#54249=CARTESIAN_POINT('Ctrl Pts',(-11.5658273270964,-38.0088697802057,
28.1988916781526));
#54250=CARTESIAN_POINT('Ctrl Pts',(-11.6724706396187,-37.9509249117669,
28.1924239175614));
#54251=CARTESIAN_POINT('Ctrl Pts',(-11.9849633252903,-37.7587374229869,
28.1729478360663));
#54252=CARTESIAN_POINT('Ctrl Pts',(-12.1795245139706,-37.6077525295176,
28.1600322001831));
#54253=CARTESIAN_POINT('Ctrl Pts',(-12.3927020634508,-37.4016616550794,
28.1434190878654));
#54254=CARTESIAN_POINT('Ctrl Pts',(-12.4285344539276,-37.3654221391915,
28.1405327830202));
#54255=CARTESIAN_POINT('Ctrl Pts',(-12.4841305742579,-37.3065990912556,
28.1358927807155));
#54256=CARTESIAN_POINT('Ctrl Pts',(-12.5044355110543,-37.2845364443238,
28.1341620910076));
#54257=CARTESIAN_POINT('Ctrl Pts',(-12.542132053673,-37.2424700906363,28.1308784278349));
#54258=CARTESIAN_POINT('Ctrl Pts',(-12.5595869853624,-37.2225260157992,
28.1293282543901));
#54259=CARTESIAN_POINT('Ctrl Pts',(-12.5987131319049,-37.1767480402325,
28.1257839539075));
#54260=CARTESIAN_POINT('Ctrl Pts',(-12.6202360861217,-37.1507916455033,
28.1237840618344));
#54261=CARTESIAN_POINT('Ctrl Pts',(-12.6865471837808,-37.0683485251447,
28.1174600344297));
#54262=CARTESIAN_POINT('Ctrl Pts',(-12.729920631706,-37.0107544767929,28.1130820268668));
#54263=CARTESIAN_POINT('Ctrl Pts',(-12.8298413340573,-36.8688756876391,
28.1023878040694));
#54264=CARTESIAN_POINT('Ctrl Pts',(-12.8845020854608,-36.7833517200597,
28.096013140807));
#54265=CARTESIAN_POINT('Ctrl Pts',(-13.0347698264456,-36.523210528921,28.07689198148));
#54266=CARTESIAN_POINT('Ctrl Pts',(-13.1189289791171,-36.3424889285501,
28.0639261820548));
#54267=CARTESIAN_POINT('Ctrl Pts',(-13.218543037923,-36.0677477931313,28.0453344477974));
#54268=CARTESIAN_POINT('Ctrl Pts',(-13.2467056778762,-35.9787796896697,
28.0394813346878));
#54269=CARTESIAN_POINT('Ctrl Pts',(-13.2780155784685,-35.8635402341408,
28.032202702615));
#54270=CARTESIAN_POINT('Ctrl Pts',(-13.2845751589283,-35.8382445854423,
28.0306234205127));
#54271=CARTESIAN_POINT('Ctrl Pts',(-13.2946914175318,-35.79728993047,28.0280989113837));
#54272=CARTESIAN_POINT('Ctrl Pts',(-13.2984303802658,-35.7816775676792,
28.0271440964218));
#54273=CARTESIAN_POINT('Ctrl Pts',(-13.3055989806115,-35.7507768688988,
28.0252699906278));
#54274=CARTESIAN_POINT('Ctrl Pts',(-13.3090337880532,-35.7354902664808,
28.024350464316));
#54275=CARTESIAN_POINT('Ctrl Pts',(-13.3175298447815,-35.6964139050986,
28.0220180350336));
#54276=CARTESIAN_POINT('Ctrl Pts',(-13.3224413731803,-35.6725919957669,
28.0206131949169));
#54277=CARTESIAN_POINT('Ctrl Pts',(-13.3326711587271,-35.6201262843258,
28.0175525224743));
#54278=CARTESIAN_POINT('Ctrl Pts',(-13.3378774649339,-35.5914624221048,
28.0159020993239));
#54279=CARTESIAN_POINT('Ctrl Pts',(-13.373848976752,-35.3777869694156,28.0037368074046));
#54280=CARTESIAN_POINT('Ctrl Pts',(-13.3895833277203,-35.1905621689522,
27.9938307688362));
#54281=CARTESIAN_POINT('Ctrl Pts',(-13.3897486828724,-35.0029882209942,
27.9838866141078));
#54282=CARTESIAN_POINT('Origin',(-10.,-35.,32.7603849714045));
#54283=CARTESIAN_POINT('',(-14.0849984181033,-35.0035950095037,28.3853849713664));
#54284=CARTESIAN_POINT('Ctrl Pts',(-7.5128274573098,-31.7594448403263,29.1925543292906));
#54285=CARTESIAN_POINT('Ctrl Pts',(-7.41829563611702,-31.8319993683303,
29.1867402586116));
#54286=CARTESIAN_POINT('Ctrl Pts',(-7.32683078998923,-31.9087785501752,
29.1809261879325));
#54287=CARTESIAN_POINT('Ctrl Pts',(-7.23882981532482,-31.9894910378375,
29.1751121172534));
#54288=CARTESIAN_POINT('Ctrl Pts',(-7.1509049789919,-32.070133693158,29.1693030769008));
#54289=CARTESIAN_POINT('Ctrl Pts',(-7.06643835081943,-32.1547026087496,
29.1634940365483));
#54290=CARTESIAN_POINT('Ctrl Pts',(-6.98579434796882,-32.2428657473269,
29.1576849961958));
#54291=CARTESIAN_POINT('Ctrl Pts',(-6.90519378059777,-32.3309814005604,
29.151879084637));
#54292=CARTESIAN_POINT('Ctrl Pts',(-6.82841201843355,-32.4226871260208,
29.1460731730783));
#54293=CARTESIAN_POINT('Ctrl Pts',(-6.75577677243,-32.5176139200972,29.1402672615195));
#54294=CARTESIAN_POINT('Ctrl Pts',(-6.68316115920835,-32.6125150561474,
29.1344629192567));
#54295=CARTESIAN_POINT('Ctrl Pts',(-6.61469008138252,-32.7106352056854,
29.1286585769939));
#54296=CARTESIAN_POINT('Ctrl Pts',(-6.55065069332656,-32.8115726284495,
29.122854234731));
#54297=CARTESIAN_POINT('Ctrl Pts',(-6.48661351598212,-32.9125065667405,
29.1170500928406));
#54298=CARTESIAN_POINT('Ctrl Pts',(-6.42700794269385,-33.016257240098,29.1112459509502));
#54299=CARTESIAN_POINT('Ctrl Pts',(-6.37207719311032,-33.1223948478847,
29.1054418090597));
#54300=CARTESIAN_POINT('Ctrl Pts',(-6.31713538878711,-33.2285538157227,
29.0996364990935));
#54301=CARTESIAN_POINT('Ctrl Pts',(-6.26687046665079,-33.3371003107878,
29.0938311891273));
#54302=CARTESIAN_POINT('Ctrl Pts',(-6.22147888630712,-33.4475815018568,
29.0880258791611));
#54303=CARTESIAN_POINT('Ctrl Pts',(-6.17603972326924,-33.5581785071956,
29.0822144836547));
#54304=CARTESIAN_POINT('Ctrl Pts',(-6.13548426028394,-33.6707138808813,
29.0764030881482));
#54305=CARTESIAN_POINT('Ctrl Pts',(-6.09996021653626,-33.7847162111671,
29.0705916926418));
#54306=CARTESIAN_POINT('Ctrl Pts',(-6.06441677612587,-33.8987807884415,
29.0647771240259));
#54307=CARTESIAN_POINT('Ctrl Pts',(-6.03391033225052,-34.014313523556,29.05896255541));
#54308=CARTESIAN_POINT('Ctrl Pts',(-6.00853783392326,-34.1308309849183,
29.0531479867942));
#54309=CARTESIAN_POINT('Ctrl Pts',(-5.98312526945627,-34.2475324409677,
29.047324236295));
#54310=CARTESIAN_POINT('Ctrl Pts',(-5.96286291620998,-34.3652213275178,
29.0415004857958));
#54311=CARTESIAN_POINT('Ctrl Pts',(-5.94779610757038,-34.4834067226742,
29.0356767352966));
#54312=CARTESIAN_POINT('Ctrl Pts',(-5.9358693202173,-34.5769615098881,29.0310666924227));
#54313=CARTESIAN_POINT('Ctrl Pts',(-5.92719713908413,-34.6708272463293,
29.0264566495489));
#54314=CARTESIAN_POINT('Ctrl Pts',(-5.92177888561108,-34.7647606704813,
29.021846606675));
#54315=CARTESIAN_POINT('Ctrl Pts',(-5.91493526854366,-34.8834048771292,
29.0160238137307));
#54316=CARTESIAN_POINT('Ctrl Pts',(-5.91326230543851,-35.0025398287942,
29.0102010207864));
#54317=CARTESIAN_POINT('Ctrl Pts',(-5.91681257603086,-35.1216776920402,
29.0043782278421));
#54318=CARTESIAN_POINT('Ctrl Pts',(-5.92035836024105,-35.2406650039495,
28.9985627930058));
#54319=CARTESIAN_POINT('Ctrl Pts',(-5.92911423802636,-35.359654815448,28.9927473581695));
#54320=CARTESIAN_POINT('Ctrl Pts',(-5.94308092912631,-35.4781554688398,
28.9869319233332));
#54321=CARTESIAN_POINT('Ctrl Pts',(-5.95703361417853,-35.5965372876561,
28.981122320319));
#54322=CARTESIAN_POINT('Ctrl Pts',(-5.97618666960746,-35.7144305209006,
28.9753127173048));
#54323=CARTESIAN_POINT('Ctrl Pts',(-6.00048880543195,-35.8313454182979,
28.9695031142906));
#54324=CARTESIAN_POINT('Ctrl Pts',(-6.02571566512785,-35.9527090603374,
28.9634724492829));
#54325=CARTESIAN_POINT('Ctrl Pts',(-6.05649123059984,-36.0730179860591,
28.9574417842752));
#54326=CARTESIAN_POINT('Ctrl Pts',(-6.09269913988917,-36.1917319281521,
28.9514111192676));
#54327=CARTESIAN_POINT('Ctrl Pts',(-6.12754041998201,-36.305965138204,28.9456080753249));
#54328=CARTESIAN_POINT('Ctrl Pts',(-6.16741127144981,-36.4187211579221,
28.9398050313822));
#54329=CARTESIAN_POINT('Ctrl Pts',(-6.21215652824688,-36.5295315732267,
28.9340019874395));
#54330=CARTESIAN_POINT('Ctrl Pts',(-6.25689513162165,-36.6403255115113,
28.9281998063839));
#54331=CARTESIAN_POINT('Ctrl Pts',(-6.30650654603254,-36.7491740420576,
28.9223976253283));
#54332=CARTESIAN_POINT('Ctrl Pts',(-6.36078699819927,-36.8556275831978,
28.9165954442726));
#54333=CARTESIAN_POINT('Ctrl Pts',(-6.41507219960668,-36.9620904384367,
28.9107927555581));
#54334=CARTESIAN_POINT('Ctrl Pts',(-6.47402706542833,-37.0661575237296,
28.9049900668436));
#54335=CARTESIAN_POINT('Ctrl Pts',(-6.53740159426591,-37.1674033497731,
28.899187378129));
#54336=CARTESIAN_POINT('Ctrl Pts',(-6.60079663637736,-37.2686819473953,
28.8933828111813));
#54337=CARTESIAN_POINT('Ctrl Pts',(-6.66861396995011,-37.3671371235897,
28.8875782442336));
#54338=CARTESIAN_POINT('Ctrl Pts',(-6.74056032672592,-37.4623724365512,
28.8817736772859));
#54339=CARTESIAN_POINT('Ctrl Pts',(-6.81258635248139,-37.557713207253,28.875962682717));
#54340=CARTESIAN_POINT('Ctrl Pts',(-6.88875028161634,-37.649826671619,28.8701516881482));
#54341=CARTESIAN_POINT('Ctrl Pts',(-6.96871852630632,-37.7383494348314,
28.8643406935793));
#54342=CARTESIAN_POINT('Ctrl Pts',(-7.04873927766027,-37.8269303215528,
28.8585258835466));
#54343=CARTESIAN_POINT('Ctrl Pts',(-7.13256903295501,-37.9119155217405,
28.852711073514));
#54344=CARTESIAN_POINT('Ctrl Pts',(-7.2198385241554,-37.9929796471459,28.8468962634814));
#54345=CARTESIAN_POINT('Ctrl Pts',(-7.30723309632454,-38.0741599595394,
28.841073119241));
#54346=CARTESIAN_POINT('Ctrl Pts',(-7.3980769344774,-38.1514077163572,28.8352499750006));
#54347=CARTESIAN_POINT('Ctrl Pts',(-7.49196892069193,-38.2244387271624,
28.8294268307601));
#54348=CARTESIAN_POINT('Ctrl Pts',(-7.51701302504882,-38.2439185180331,
28.8278736052089));
#54349=CARTESIAN_POINT('Ctrl Pts',(-7.5422738441232,-38.2630985466123,28.8263203796577));
#54350=CARTESIAN_POINT('Ctrl Pts',(-7.56774345158431,-38.2819739613058,
28.8247671541065));
#54351=CARTESIAN_POINT('Ctrl Pts',(-7.66324133017982,-38.3527470214556,
28.8189433601848));
#54352=CARTESIAN_POINT('Ctrl Pts',(-7.76198468770386,-38.4194625362104,
28.8131195662631));
#54353=CARTESIAN_POINT('Ctrl Pts',(-7.86359411418139,-38.4818091405244,
28.8072957723414));
#54354=CARTESIAN_POINT('Ctrl Pts',(-7.96507537238453,-38.5440771019707,
28.8014793244469));
#54355=CARTESIAN_POINT('Ctrl Pts',(-8.06941516401801,-38.6019869023167,
28.7956628765524));
#54356=CARTESIAN_POINT('Ctrl Pts',(-8.17620246803788,-38.65526846653,28.789846428658));
#54357=CARTESIAN_POINT('Ctrl Pts',(-8.2828829002652,-38.7084967070236,28.7840358018133));
#54358=CARTESIAN_POINT('Ctrl Pts',(-8.39200560874236,-38.7571057447421,
28.7782251749687));
#54359=CARTESIAN_POINT('Ctrl Pts',(-8.50313267252363,-38.8008700588068,
28.772414548124));
#54360=CARTESIAN_POINT('Ctrl Pts',(-8.61846065936954,-38.8462887899873,
28.7663842628496));
#54361=CARTESIAN_POINT('Ctrl Pts',(-8.73594715078625,-38.8864890459525,
28.7603539775752));
#54362=CARTESIAN_POINT('Ctrl Pts',(-8.85507667243839,-38.9212721882069,
28.7543236923007));
#54363=CARTESIAN_POINT('Ctrl Pts',(-8.96973762288422,-38.954750608124,28.7485196041836));
#54364=CARTESIAN_POINT('Ctrl Pts',(-9.08592013570892,-38.9832108640657,
28.7427155160664));
#54365=CARTESIAN_POINT('Ctrl Pts',(-9.20314722294913,-39.006526007866,28.7369114279493));
#54366=CARTESIAN_POINT('Ctrl Pts',(-9.32035699746757,-39.0298377083614,
28.7311081970108));
#54367=CARTESIAN_POINT('Ctrl Pts',(-9.43861063925757,-39.04800572821,28.7253049660724));
#54368=CARTESIAN_POINT('Ctrl Pts',(-9.55742027561235,-39.0609540981844,
28.7195017351339));
#54369=CARTESIAN_POINT('Ctrl Pts',(-9.67624039904241,-39.0739036110841,
28.7136979919565));
#54370=CARTESIAN_POINT('Ctrl Pts',(-9.79561620869263,-39.0816325138321,
28.7078942487792));
#54371=CARTESIAN_POINT('Ctrl Pts',(-9.91505464847786,-39.0841167083293,
28.7020905056018));
#54372=CARTESIAN_POINT('Ctrl Pts',(-10.03453181255,-39.0866017082512,28.696284880737));
#54373=CARTESIAN_POINT('Ctrl Pts',(-10.1540712391352,-39.0838386096445,
28.6904792558721));
#54374=CARTESIAN_POINT('Ctrl Pts',(-10.2731804541561,-39.0758554242597,
28.6846736310073));
#54375=CARTESIAN_POINT('Ctrl Pts',(-10.392421535695,-39.067863400643,28.6788615787007));
#54376=CARTESIAN_POINT('Ctrl Pts',(-10.5112310473222,-39.0546397818076,
28.6730495263942));
#54377=CARTESIAN_POINT('Ctrl Pts',(-10.6291220559173,-39.0362644163581,
28.6672374740876));
#54378=CARTESIAN_POINT('Ctrl Pts',(-10.7470904800299,-39.0178769843528,
28.6614216051793));
#54379=CARTESIAN_POINT('Ctrl Pts',(-10.8641388005456,-38.9943311487283,
28.6556057362709));
#54380=CARTESIAN_POINT('Ctrl Pts',(-10.979792313732,-38.9657574335745,28.6497898673626));
#54381=CARTESIAN_POINT('Ctrl Pts',(-11.0956114326921,-38.9371428033454,
28.6439656706357));
#54382=CARTESIAN_POINT('Ctrl Pts',(-11.2100313676118,-38.9034860386072,
28.6381414739088));
#54383=CARTESIAN_POINT('Ctrl Pts',(-11.3225944121625,-38.8649668848409,
28.6323172771819));
#54384=CARTESIAN_POINT('Ctrl Pts',(-11.3524193622157,-38.8547607657566,
28.6307740853006));
#54385=CARTESIAN_POINT('Ctrl Pts',(-11.382114070009,-38.8442135397309,28.6292308934194));
#54386=CARTESIAN_POINT('Ctrl Pts',(-11.4116702960911,-38.8333290982035,
28.6276877015381));
#54387=CARTESIAN_POINT('Ctrl Pts',(-11.5232093497215,-38.7922534783362,
28.6218640161485));
#54388=CARTESIAN_POINT('Ctrl Pts',(-11.6331339301567,-38.7462394001181,
28.616040330759));
#54389=CARTESIAN_POINT('Ctrl Pts',(-11.7409756547684,-38.6954335022435,
28.6102166453694));
#54390=CARTESIAN_POINT('Ctrl Pts',(-11.8486813603392,-38.6446916850346,
28.604400305301));
#54391=CARTESIAN_POINT('Ctrl Pts',(-11.9543090691492,-38.5891702417359,
28.5985839652326));
#54392=CARTESIAN_POINT('Ctrl Pts',(-12.0574076037386,-38.5290648835178,
28.5927676251642));
#54393=CARTESIAN_POINT('Ctrl Pts',(-12.1604029711546,-38.4690196706737,
28.5869571053081));
#54394=CARTESIAN_POINT('Ctrl Pts',(-12.2608738484572,-38.4043998725906,
28.581146585452));
#54395=CARTESIAN_POINT('Ctrl Pts',(-12.3583915761085,-38.3354481218781,
28.575336065596));
#54396=CARTESIAN_POINT('Ctrl Pts',(-12.4595982965265,-38.2638879991726,
28.5693057399032));
#54397=CARTESIAN_POINT('Ctrl Pts',(-12.5576236207883,-38.1876618965559,
28.5632754142105));
#54398=CARTESIAN_POINT('Ctrl Pts',(-12.6520188291916,-38.1070920697033,
28.5572450885177));
#54399=CARTESIAN_POINT('Ctrl Pts',(-12.7428710156203,-38.0295463440933,
28.5514411045726));
#54400=CARTESIAN_POINT('Ctrl Pts',(-12.8303603413976,-37.9479773804106,
28.5456371206276));
#54401=CARTESIAN_POINT('Ctrl Pts',(-12.9141191759421,-37.862714520941,28.5398331366825));
#54402=CARTESIAN_POINT('Ctrl Pts',(-12.9978656580678,-37.7774642356977,
28.5340300086858));
#54403=CARTESIAN_POINT('Ctrl Pts',(-13.0778824569824,-37.688521429232,28.5282268806891));
#54404=CARTESIAN_POINT('Ctrl Pts',(-13.1538386131533,-37.5962524919937,
28.5224237526924));
#54405=CARTESIAN_POINT('Ctrl Pts',(-13.2298014916053,-37.5039753887585,
28.5166201111066));
#54406=CARTESIAN_POINT('Ctrl Pts',(-13.301702753262,-37.408371884733,28.5108164695208));
#54407=CARTESIAN_POINT('Ctrl Pts',(-13.3692519812247,-37.3098411389126,
28.5050128279349));
#54408=CARTESIAN_POINT('Ctrl Pts',(-13.4368231274801,-37.2112784219538,
28.4992073031904));
#54409=CARTESIAN_POINT('Ctrl Pts',(-13.5000392008406,-37.109786910809,28.4934017784459));
#54410=CARTESIAN_POINT('Ctrl Pts',(-13.5586536871284,-37.0057938416217,
28.4875962537014));
#54411=CARTESIAN_POINT('Ctrl Pts',(-13.6173330942738,-36.9016855906822,
28.4817842988119));
#54412=CARTESIAN_POINT('Ctrl Pts',(-13.6714005403349,-36.7950706070611,
28.4759723439225));
#54413=CARTESIAN_POINT('Ctrl Pts',(-13.7206559037518,-36.6863999068659,
28.470160389033));
#54414=CARTESIAN_POINT('Ctrl Pts',(-13.7699436246378,-36.5776578173114,
28.464344616079));
#54415=CARTESIAN_POINT('Ctrl Pts',(-13.814412815498,-36.46685769976,28.4585288431251));
#54416=CARTESIAN_POINT('Ctrl Pts',(-13.8539124424957,-36.35446811907,28.4527130701712));
#54417=CARTESIAN_POINT('Ctrl Pts',(-13.8934686500774,-36.2419175477936,
28.44688896651));
#54418=CARTESIAN_POINT('Ctrl Pts',(-13.9280409675739,-36.1277733584114,
28.4410648628488));
#54419=CARTESIAN_POINT('Ctrl Pts',(-13.9575288461897,-36.0125168796503,
28.4352407591876));
#54420=CARTESIAN_POINT('Ctrl Pts',(-13.9653470963981,-35.9819584254174,
28.4336965891149));
#54421=CARTESIAN_POINT('Ctrl Pts',(-13.972808211015,-35.9513218213683,28.4321524190423));
#54422=CARTESIAN_POINT('Ctrl Pts',(-13.9799109260694,-35.9206161092189,
28.4306082489697));
#54423=CARTESIAN_POINT('Ctrl Pts',(-14.0156549436737,-35.7660913243706,
28.4228372991516));
#54424=CARTESIAN_POINT('Ctrl Pts',(-14.0424112771735,-35.6094162135617,
28.4150663493335));
#54425=CARTESIAN_POINT('Ctrl Pts',(-14.0599741506301,-35.451480781668,28.4072953995154));
#54426=CARTESIAN_POINT('Ctrl Pts',(-14.0764805016467,-35.3030462055577,
28.3999919234785));
#54427=CARTESIAN_POINT('Ctrl Pts',(-14.0848664955798,-35.1534981411174,
28.3926884474415));
#54428=CARTESIAN_POINT('Ctrl Pts',(-14.0849984181026,-35.0035950102863,
28.3853849714045));
#54429=CARTESIAN_POINT('Ctrl Pts',(-14.0849984181033,-35.0035950095037,
28.3853849713664));
#54430=CARTESIAN_POINT('Ctrl Pts',(-14.0851020303385,-34.885860740221,28.3796488042185));
#54431=CARTESIAN_POINT('Ctrl Pts',(-14.0801115803583,-34.7679841837216,
28.3739126370707));
#54432=CARTESIAN_POINT('Ctrl Pts',(-14.0700169326326,-34.6504471884196,
28.3681764699229));
#54433=CARTESIAN_POINT('Ctrl Pts',(-14.0599295789436,-34.5329951212077,
28.3624444475273));
#54434=CARTESIAN_POINT('Ctrl Pts',(-14.0447453971451,-34.4158825442329,
28.3567124251316));
#54435=CARTESIAN_POINT('Ctrl Pts',(-14.024506318868,-34.2995901989612,28.350980402736));
#54436=CARTESIAN_POINT('Ctrl Pts',(-14.0042749038498,-34.1833418862451,
28.3452505506947));
#54437=CARTESIAN_POINT('Ctrl Pts',(-13.9789924676054,-34.0679136012425,
28.3395206986534));
#54438=CARTESIAN_POINT('Ctrl Pts',(-13.948752592152,-33.9537791982699,28.3337908466121));
#54439=CARTESIAN_POINT('Ctrl Pts',(-13.9185165787158,-33.8396593717141,
28.3280617263459));
#54440=CARTESIAN_POINT('Ctrl Pts',(-13.8833244923329,-33.726833504574,28.3223326060797));
#54441=CARTESIAN_POINT('Ctrl Pts',(-13.8433204650405,-33.6157627360163,
28.3166034858135));
#54442=CARTESIAN_POINT('Ctrl Pts',(-13.8033115084338,-33.5046782812685,
28.3108736596025));
#54443=CARTESIAN_POINT('Ctrl Pts',(-13.7584895755464,-33.3953497497871,
28.3051438333915));
#54444=CARTESIAN_POINT('Ctrl Pts',(-13.7090475743058,-33.2882199056139,
28.2994140071806));
#54445=CARTESIAN_POINT('Ctrl Pts',(-13.659557017041,-33.1809848513123,28.2936785538191));
#54446=CARTESIAN_POINT('Ctrl Pts',(-13.6054375067942,-33.0759531783709,
28.2879431004577));
#54447=CARTESIAN_POINT('Ctrl Pts',(-13.5469287542339,-32.9735446187027,
28.2822076470962));
#54448=CARTESIAN_POINT('Ctrl Pts',(-13.4883905352389,-32.8710844835864,
28.2764693052206));
#54449=CARTESIAN_POINT('Ctrl Pts',(-13.4254588967976,-32.7712504469683,
28.270730963345));
#54450=CARTESIAN_POINT('Ctrl Pts',(-13.3584168618395,-32.6744331482169,
28.2649926214694));
#54451=CARTESIAN_POINT('Ctrl Pts',(-13.2912691229998,-32.5774631995006,
28.259245232061));
#54452=CARTESIAN_POINT('Ctrl Pts',(-13.2199982971978,-32.4835198232529,
28.2534978426526));
#54453=CARTESIAN_POINT('Ctrl Pts',(-13.1449278762672,-32.3929607496093,
28.2477504532441));
#54454=CARTESIAN_POINT('Ctrl Pts',(-13.0830084151193,-32.3182659633999,
28.2430099009632));
#54455=CARTESIAN_POINT('Ctrl Pts',(-13.0185047918086,-32.2458730372111,
28.2382693486822));
#54456=CARTESIAN_POINT('Ctrl Pts',(-12.9516163321836,-32.1759628140574,
28.2335287964012));
#54457=CARTESIAN_POINT('Ctrl Pts',(-12.8694458679809,-32.0900802040935,
28.2277051702677));
#54458=CARTESIAN_POINT('Ctrl Pts',(-12.7833914345599,-32.0076484389653,
28.2218815441341));
#54459=CARTESIAN_POINT('Ctrl Pts',(-12.6937743723571,-31.9290384843127,
28.2160579180006));
#54460=CARTESIAN_POINT('Ctrl Pts',(-12.604270370409,-31.8505277034256,28.2102416389128));
#54461=CARTESIAN_POINT('Ctrl Pts',(-12.5112129835747,-31.7758294099165,
28.204425359825));
#54462=CARTESIAN_POINT('Ctrl Pts',(-12.4149616844493,-31.7052792132501,
28.1986090807372));
#54463=CARTESIAN_POINT('Ctrl Pts',(-12.318806728878,-31.6347996344013,28.1927986235032));
#54464=CARTESIAN_POINT('Ctrl Pts',(-12.2194645484442,-31.5684601323676,
28.1869881662693));
#54465=CARTESIAN_POINT('Ctrl Pts',(-12.1173286556274,-31.5065569470708,
28.1811777090354));
#54466=CARTESIAN_POINT('Ctrl Pts',(-12.0113275255331,-31.44231109366,28.1751473604853));
#54467=CARTESIAN_POINT('Ctrl Pts',(-11.9023173920652,-31.3828442621115,
28.1691170119352));
#54468=CARTESIAN_POINT('Ctrl Pts',(-11.7907728026743,-31.3284393278604,
28.1630866633851));
#54469=CARTESIAN_POINT('Ctrl Pts',(-11.6834165527187,-31.2760772209023,
28.1572827457787));
#54470=CARTESIAN_POINT('Ctrl Pts',(-11.5737131455584,-31.2284039261651,
28.1514788281722));
#54471=CARTESIAN_POINT('Ctrl Pts',(-11.4621112512257,-31.1856251247368,
28.1456749105658));
#54472=CARTESIAN_POINT('Ctrl Pts',(-11.3505258399602,-31.1428526415333,
28.1398718501704));
#54473=CARTESIAN_POINT('Ctrl Pts',(-11.2370428803218,-31.1049733601433,
28.1340687897749));
#54474=CARTESIAN_POINT('Ctrl Pts',(-11.1221303813735,-31.0721445536784,
28.1282657293794));
#54475=CARTESIAN_POINT('Ctrl Pts',(-11.0072077359545,-31.0393128485164,
28.122462156589));
#54476=CARTESIAN_POINT('Ctrl Pts',(-10.8908556929035,-31.0115326170957,
28.1166585837986));
#54477=CARTESIAN_POINT('Ctrl Pts',(-10.7735561312046,-30.9889108820826,
28.1108550110081));
#54478=CARTESIAN_POINT('Ctrl Pts',(-10.6562185306065,-30.9662818111008,
28.1050495561858));
#54479=CARTESIAN_POINT('Ctrl Pts',(-10.5379332010082,-30.9488146407147,
28.0992441013634));
#54480=CARTESIAN_POINT('Ctrl Pts',(-10.4191902487106,-30.9365649340262,
28.0934386465411));
#54481=CARTESIAN_POINT('Ctrl Pts',(-10.3003158034443,-30.9243016623195,
28.0876267629036));
#54482=CARTESIAN_POINT('Ctrl Pts',(-10.1809831303593,-30.9172674289987,
28.0818148792661));
#54483=CARTESIAN_POINT('Ctrl Pts',(-10.0616856290819,-30.915465769128,28.0760029956286));
#54484=CARTESIAN_POINT('Ctrl Pts',(-9.94230977402666,-30.9136629259396,
28.0701872947859));
#54485=CARTESIAN_POINT('Ctrl Pts',(-9.82296954400879,-30.917099488788,28.0643715939433));
#54486=CARTESIAN_POINT('Ctrl Pts',(-9.70415484288956,-30.9257269798142,
28.0585558931006));
#54487=CARTESIAN_POINT('Ctrl Pts',(-9.58516996018755,-30.9343668282343,
28.0527318622688));
#54488=CARTESIAN_POINT('Ctrl Pts',(-9.46671251292297,-30.9482123976731,
28.0469078314369));
#54489=CARTESIAN_POINT('Ctrl Pts',(-9.3492639640545,-30.9671638253554,28.0410838006051));
#54490=CARTESIAN_POINT('Ctrl Pts',(-9.31811084242144,-30.9721906744514,
28.039538981681));
#54491=CARTESIAN_POINT('Ctrl Pts',(-9.2870286282477,-30.9775764827311,28.0379941627569));
#54492=CARTESIAN_POINT('Ctrl Pts',(-9.25602612785593,-30.9833187981162,
28.0364493438328));
#54493=CARTESIAN_POINT('Ctrl Pts',(-9.13915033347081,-31.0049666543782,
28.0306255574719));
#54494=CARTESIAN_POINT('Ctrl Pts',(-9.02303170475046,-31.0317548617166,
28.0248017711111));
#54495=CARTESIAN_POINT('Ctrl Pts',(-8.90815669677599,-31.0636180061883,
28.0189779847502));
#54496=CARTESIAN_POINT('Ctrl Pts',(-8.79342204217191,-31.0954422205237,
28.0131613138452));
#54497=CARTESIAN_POINT('Ctrl Pts',(-8.67992837677122,-31.1323289331788,
28.0073446429401));
#54498=CARTESIAN_POINT('Ctrl Pts',(-8.56815354344793,-31.1741614350761,
28.0015279720351));
#54499=CARTESIAN_POINT('Ctrl Pts',(-8.45650821956137,-31.2159454671738,
27.9957180406952));
#54500=CARTESIAN_POINT('Ctrl Pts',(-8.34657814333416,-31.2626637381606,
27.9899081093553));
#54501=CARTESIAN_POINT('Ctrl Pts',(-8.23882666697027,-31.3141495566118,
27.9840981780154));
#54502=CARTESIAN_POINT('Ctrl Pts',(-8.13114729556032,-31.3656009218686,
27.9782921345557));
#54503=CARTESIAN_POINT('Ctrl Pts',(-8.02564399174177,-31.421813314406,27.972486091096));
#54504=CARTESIAN_POINT('Ctrl Pts',(-7.9227605128364,-31.4825718041489,27.9666800476364));
#54505=CARTESIAN_POINT('Ctrl Pts',(-7.81992215651057,-31.5433036464668,
27.960876550588));
#54506=CARTESIAN_POINT('Ctrl Pts',(-7.71970169001365,-31.6085774118287,
27.9550730535397));
#54507=CARTESIAN_POINT('Ctrl Pts',(-7.6225180413552,-31.6781323722462,27.9492695564913));
#54508=CARTESIAN_POINT('Ctrl Pts',(-7.58550699385698,-31.7046214162293,
27.9470593749652));
#54509=CARTESIAN_POINT('Ctrl Pts',(-7.5489361159424,-31.7317309271604,27.944849193439));
#54510=CARTESIAN_POINT('Ctrl Pts',(-7.5128274573098,-31.7594448403263,27.9426390119128));
#54511=CARTESIAN_POINT('',(-14.0849988977546,-34.9969991094922,28.4896150285548));
#54512=CARTESIAN_POINT('Ctrl Pts',(-14.0849988977546,-34.9969991094922,
28.4896150285548));
#54513=CARTESIAN_POINT('Ctrl Pts',(-14.0848971428309,-34.8584839753713,
28.4828893597099));
#54514=CARTESIAN_POINT('Ctrl Pts',(-14.0777462394372,-34.7202527422421,
28.476163690865));
#54515=CARTESIAN_POINT('Ctrl Pts',(-14.0636562776183,-34.5829596453898,
28.4694380220201));
#54516=CARTESIAN_POINT('Ctrl Pts',(-14.0494857150941,-34.4448811723539,
28.4626738794264));
#54517=CARTESIAN_POINT('Ctrl Pts',(-14.028296588798,-34.3077517162237,28.4559097368326));
#54518=CARTESIAN_POINT('Ctrl Pts',(-14.0002501584321,-34.1722176191994,
28.4491455942389));
#54519=CARTESIAN_POINT('Ctrl Pts',(-13.9720232914753,-34.0358115641359,
28.4423379345624));
#54520=CARTESIAN_POINT('Ctrl Pts',(-13.9368506870528,-33.9010215747836,
28.4355302748859));
#54521=CARTESIAN_POINT('Ctrl Pts',(-13.8949450417453,-33.7684854358214,
28.4287226152095));
#54522=CARTESIAN_POINT('Ctrl Pts',(-13.8839505474168,-33.733712845698,28.4269365366238));
#54523=CARTESIAN_POINT('Ctrl Pts',(-13.8724928412928,-33.6990952808039,
28.4251504580381));
#54524=CARTESIAN_POINT('Ctrl Pts',(-13.8605763001412,-33.6646440059715,
28.4233643794524));
#54525=CARTESIAN_POINT('Ctrl Pts',(-13.8217205192481,-33.5523101358198,
28.417540585677));
#54526=CARTESIAN_POINT('Ctrl Pts',(-13.7778950594556,-33.441492542968,28.4117167919016));
#54527=CARTESIAN_POINT('Ctrl Pts',(-13.7292372490971,-33.3326624397121,
28.4058929981261));
#54528=CARTESIAN_POINT('Ctrl Pts',(-13.6806408148247,-33.2239696127895,
28.4000765503793));
#54529=CARTESIAN_POINT('Ctrl Pts',(-13.6272243188804,-33.1172596585844,
28.3942601026325));
#54530=CARTESIAN_POINT('Ctrl Pts',(-13.5691744935128,-33.0129875604673,
28.3884436548858));
#54531=CARTESIAN_POINT('Ctrl Pts',(-13.5111827639121,-32.9088198169708,
28.3826330281899));
#54532=CARTESIAN_POINT('Ctrl Pts',(-13.4485671270989,-32.8070854306003,
28.3768224014941));
#54533=CARTESIAN_POINT('Ctrl Pts',(-13.3815616740415,-32.7082178016544,
28.3710117747983));
#54534=CARTESIAN_POINT('Ctrl Pts',(-13.3120232194584,-32.6056126880183,
28.3649814894685));
#54535=CARTESIAN_POINT('Ctrl Pts',(-13.237756686359,-32.5060957616236,28.3589512041388));
#54536=CARTESIAN_POINT('Ctrl Pts',(-13.1590753521491,-32.410122026148,28.352920918809));
#54537=CARTESIAN_POINT('Ctrl Pts',(-13.0833453725403,-32.317748287147,28.3471168308427));
#54538=CARTESIAN_POINT('Ctrl Pts',(-13.003526109092,-32.2286570588905,28.3413127428765));
#54539=CARTESIAN_POINT('Ctrl Pts',(-12.9199395548036,-32.1432224454303,
28.3355086549102));
#54540=CARTESIAN_POINT('Ctrl Pts',(-12.8363653450308,-32.0578004494171,
28.3297054241231));
#54541=CARTESIAN_POINT('Ctrl Pts',(-12.749025236336,-31.9760342860264,28.323902193336));
#54542=CARTESIAN_POINT('Ctrl Pts',(-12.6582789903332,-31.8982621307478,
28.3180989625489));
#54543=CARTESIAN_POINT('Ctrl Pts',(-12.5675247343561,-31.8204831106898,
28.3122952195232));
#54544=CARTESIAN_POINT('Ctrl Pts',(-12.473364053341,-31.7466990653977,28.3064914764975));
#54545=CARTESIAN_POINT('Ctrl Pts',(-12.3761902757642,-31.6772082861901,
28.3006877334718));
#54546=CARTESIAN_POINT('Ctrl Pts',(-12.2789849925427,-31.6076949767088,
28.2948821087588));
#54547=CARTESIAN_POINT('Ctrl Pts',(-12.1787650018617,-31.5424779389958,
28.2890764840458));
#54548=CARTESIAN_POINT('Ctrl Pts',(-12.0759525754898,-31.4818121277684,
28.2832708593327));
#54549=CARTESIAN_POINT('Ctrl Pts',(-11.9730263248589,-31.4210791530546,
28.2774588071775));
#54550=CARTESIAN_POINT('Ctrl Pts',(-11.8675022614251,-31.3649076701075,
28.2716467550223));
#54551=CARTESIAN_POINT('Ctrl Pts',(-11.7598273533192,-31.3135067223024,
28.265834702867));
#54552=CARTESIAN_POINT('Ctrl Pts',(-11.6520817383006,-31.2620720210222,
28.2600188341098));
#54553=CARTESIAN_POINT('Ctrl Pts',(-11.5421828407542,-31.2154142528824,
28.2542029653526));
#54554=CARTESIAN_POINT('Ctrl Pts',(-11.4305961492278,-31.1736937318329,
28.2483870965954));
#54555=CARTESIAN_POINT('Ctrl Pts',(-11.3188496752328,-31.1319134706142,
28.2425629000184));
#54556=CARTESIAN_POINT('Ctrl Pts',(-11.2054109704769,-31.0950846928856,
28.2367387034413));
#54557=CARTESIAN_POINT('Ctrl Pts',(-11.0907592876752,-31.0633174910402,
28.2309145068642));
#54558=CARTESIAN_POINT('Ctrl Pts',(-11.0603808982341,-31.0549003757783,
28.2293713135375));
#54559=CARTESIAN_POINT('Ctrl Pts',(-11.0299173970239,-31.046838328789,28.2278281202107));
#54560=CARTESIAN_POINT('Ctrl Pts',(-10.9993777816479,-31.0391327907201,
28.226284926884));
#54561=CARTESIAN_POINT('Ctrl Pts',(-10.884120741644,-31.010051955925,28.2204608884079));
#54562=CARTESIAN_POINT('Ctrl Pts',(-10.767407519683,-30.9859592050703,28.2146368499319));
#54563=CARTESIAN_POINT('Ctrl Pts',(-10.6497075722854,-30.9669980076232,
28.2088128114558));
#54564=CARTESIAN_POINT('Ctrl Pts',(-10.532157786967,-30.9480610009502,28.2029962033121));
#54565=CARTESIAN_POINT('Ctrl Pts',(-10.4136241799048,-30.9342425897698,
28.1971795951684));
#54566=CARTESIAN_POINT('Ctrl Pts',(-10.2945896981088,-30.9256360116249,
28.1913629870247));
#54567=CARTESIAN_POINT('Ctrl Pts',(-10.1714609044516,-30.9167334014861,
28.185346310738));
#54568=CARTESIAN_POINT('Ctrl Pts',(-10.0477965797414,-30.9134077422541,
28.1793296344514));
#54569=CARTESIAN_POINT('Ctrl Pts',(-9.92414173974794,-30.915704402917,28.1733129581648));
#54570=CARTESIAN_POINT('Ctrl Pts',(-9.80481594266389,-30.9179206595896,
28.1675069202149));
#54571=CARTESIAN_POINT('Ctrl Pts',(-9.68549942568355,-30.9253721801646,
28.1617008822649));
#54572=CARTESIAN_POINT('Ctrl Pts',(-9.56668514340063,-30.9380468694173,
28.155894844315));
#54573=CARTESIAN_POINT('Ctrl Pts',(-9.44791897097225,-30.9507164264802,
28.1500911573251));
#54574=CARTESIAN_POINT('Ctrl Pts',(-9.32965503409748,-30.9686049024805,
28.1442874703353));
#54575=CARTESIAN_POINT('Ctrl Pts',(-9.21238265579534,-30.9916482291211,
28.1384837833455));
#54576=CARTESIAN_POINT('Ctrl Pts',(-9.09513008935856,-31.0146876628477,
28.1326810768241));
#54577=CARTESIAN_POINT('Ctrl Pts',(-8.97886914852464,-31.0428801353257,
28.1268783703028));
#54578=CARTESIAN_POINT('Ctrl Pts',(-8.86407979923247,-31.0761103102294,
28.1210756637814));
#54579=CARTESIAN_POINT('Ctrl Pts',(-8.74928275537019,-31.1093427126212,
28.1152725682924));
#54580=CARTESIAN_POINT('Ctrl Pts',(-8.6359578908288,-31.1476133739308,28.1094694728035));
#54581=CARTESIAN_POINT('Ctrl Pts',(-8.52457020601974,-31.1907570406923,
28.1036663773146));
#54582=CARTESIAN_POINT('Ctrl Pts',(-8.41310155905027,-31.2339320664363,
28.0978590638446));
#54583=CARTESIAN_POINT('Ctrl Pts',(-8.30357328398359,-31.2819870215234,
28.0920517503745));
#54584=CARTESIAN_POINT('Ctrl Pts',(-8.19643055826853,-31.3347084333095,
28.0862444369045));
#54585=CARTESIAN_POINT('Ctrl Pts',(-8.08924108020353,-31.3874528503895,
28.0804345893796));
#54586=CARTESIAN_POINT('Ctrl Pts',(-7.98443958397608,-31.4448675863832,
28.0746247418546));
#54587=CARTESIAN_POINT('Ctrl Pts',(-7.88244553440794,-31.5066938174201,
28.0688148943297));
#54588=CARTESIAN_POINT('Ctrl Pts',(-7.78033805422457,-31.5685888072469,
28.0629985855006));
#54589=CARTESIAN_POINT('Ctrl Pts',(-7.68104459292747,-31.6349048603944,
28.0571822766715));
#54590=CARTESIAN_POINT('Ctrl Pts',(-7.58495459416272,-31.7053405809182,
28.0513659678423));
#54591=CARTESIAN_POINT('Ctrl Pts',(-7.56070642011141,-31.7231149344685,
28.0498982306102));
#54592=CARTESIAN_POINT('Ctrl Pts',(-7.53666207253144,-31.741151431443,28.048430493378));
#54593=CARTESIAN_POINT('Ctrl Pts',(-7.5128274573098,-31.7594448403263,28.0469627561459));
#54594=CARTESIAN_POINT('Ctrl Pts',(-7.51282745730978,-31.7594448403263,
29.2969304815276));
#54595=CARTESIAN_POINT('Ctrl Pts',(-7.41787341740872,-31.832323427242,29.2911163987806));
#54596=CARTESIAN_POINT('Ctrl Pts',(-7.32614682414379,-31.9093623605148,
29.2853023160336));
#54597=CARTESIAN_POINT('Ctrl Pts',(-7.23801917381052,-31.9902347407544,
29.2794882332866));
#54598=CARTESIAN_POINT('Ctrl Pts',(-7.1497993364812,-32.0711917185269,29.273668068648));
#54599=CARTESIAN_POINT('Ctrl Pts',(-7.06518626208406,-32.155989877465,29.2678479040093));
#54600=CARTESIAN_POINT('Ctrl Pts',(-6.9845152878803,-32.2442647168183,29.2620277393706));
#54601=CARTESIAN_POINT('Ctrl Pts',(-6.90380138944867,-32.332586526341,29.2562044778799));
#54602=CARTESIAN_POINT('Ctrl Pts',(-6.82703403156669,-32.4243883902038,
29.2503812163892));
#54603=CARTESIAN_POINT('Ctrl Pts',(-6.75450775669891,-32.5192732720688,
29.2445579548984));
#54604=CARTESIAN_POINT('Ctrl Pts',(-6.68186497780587,-32.6143105741523,
29.2387253390957));
#54605=CARTESIAN_POINT('Ctrl Pts',(-6.61347712758057,-32.7124404559656,
29.232892723293));
#54606=CARTESIAN_POINT('Ctrl Pts',(-6.54959529733578,-32.8132370069364,
29.2270601074902));
#54607=CARTESIAN_POINT('Ctrl Pts',(-6.49345298970209,-32.9018216788428,
29.2219341349022));
#54608=CARTESIAN_POINT('Ctrl Pts',(-6.44079040224357,-32.9924654483701,
29.2168081623142));
#54609=CARTESIAN_POINT('Ctrl Pts',(-6.39174772339236,-33.0848654072479,
29.2116821897262));
#54610=CARTESIAN_POINT('Ctrl Pts',(-6.33608948362485,-33.1897295620249,
29.2058647544224));
#54611=CARTESIAN_POINT('Ctrl Pts',(-6.28491481213769,-33.2971947001416,
29.2000473191185));
#54612=CARTESIAN_POINT('Ctrl Pts',(-6.2384753088229,-33.4068405611286,29.1942298838146));
#54613=CARTESIAN_POINT('Ctrl Pts',(-6.19209507835399,-33.5163464761266,
29.1884198735675));
#54614=CARTESIAN_POINT('Ctrl Pts',(-6.15043815414528,-33.6280272047772,
29.1826098633204));
#54615=CARTESIAN_POINT('Ctrl Pts',(-6.11371065222675,-33.7414372858756,
29.1767998530732));
#54616=CARTESIAN_POINT('Ctrl Pts',(-6.0770203952809,-33.8547323590058,29.1709957346963));
#54617=CARTESIAN_POINT('Ctrl Pts',(-6.04524974191319,-33.9697529088491,
29.1651916163193));
#54618=CARTESIAN_POINT('Ctrl Pts',(-6.01855678169613,-34.086033425435,29.1593874979423));
#54619=CARTESIAN_POINT('Ctrl Pts',(-5.99081258920605,-34.2068933453828,
29.1533547995763));
#54620=CARTESIAN_POINT('Ctrl Pts',(-5.96855442122842,-34.329114096242,29.1473221012103));
#54621=CARTESIAN_POINT('Ctrl Pts',(-5.9519028048853,-34.45215504118,29.1412894028443));
#54622=CARTESIAN_POINT('Ctrl Pts',(-5.93590054455395,-34.570397810635,29.1354919590548));
#54623=CARTESIAN_POINT('Ctrl Pts',(-5.92507582323453,-34.6893975602768,
29.1296945152653));
#54624=CARTESIAN_POINT('Ctrl Pts',(-5.91948339096502,-34.8086646833706,
29.1238970714758));
#54625=CARTESIAN_POINT('Ctrl Pts',(-5.91389182303259,-34.9279133731616,
29.1181005237088));
#54626=CARTESIAN_POINT('Ctrl Pts',(-5.91353095520818,-35.0474289454461,
29.1123039759419));
#54627=CARTESIAN_POINT('Ctrl Pts',(-5.91840350906871,-35.1667185809002,
29.106507428175));
#54628=CARTESIAN_POINT('Ctrl Pts',(-5.92327646679649,-35.2860181038135,
29.1007103999545));
#54629=CARTESIAN_POINT('Ctrl Pts',(-5.93338369187788,-35.4050912436341,
29.0949133717341));
#54630=CARTESIAN_POINT('Ctrl Pts',(-5.94867583996883,-35.5234477532168,
29.0891163435136));
#54631=CARTESIAN_POINT('Ctrl Pts',(-5.9639728865431,-35.6418421755495,29.0833174583502));
#54632=CARTESIAN_POINT('Ctrl Pts',(-5.9844581065806,-35.7595191053679,29.0775185731868));
#54633=CARTESIAN_POINT('Ctrl Pts',(-6.01003071138977,-35.8759966186848,
29.0717196880234));
#54634=CARTESIAN_POINT('Ctrl Pts',(-6.03563164690813,-35.9926031720654,
29.0659143785427));
#54635=CARTESIAN_POINT('Ctrl Pts',(-6.06633112931651,-36.1080072565552,
29.0601090690619));
#54636=CARTESIAN_POINT('Ctrl Pts',(-6.10197793524993,-36.2217401453344,
29.0543037595812));
#54637=CARTESIAN_POINT('Ctrl Pts',(-6.13764811609673,-36.3355476129251,
29.0484946433469));
#54638=CARTESIAN_POINT('Ctrl Pts',(-6.17827194175445,-36.4476813185244,
29.0426855271125));
#54639=CARTESIAN_POINT('Ctrl Pts',(-6.22364990453442,-36.5576921892585,
29.0368764108782));
#54640=CARTESIAN_POINT('Ctrl Pts',(-6.26909320861608,-36.6678614684592,
29.031058929896));
#54641=CARTESIAN_POINT('Ctrl Pts',(-6.31930414123014,-36.7759014419196,
29.0252414489138));
#54642=CARTESIAN_POINT('Ctrl Pts',(-6.37403706152266,-36.8813871926822,
29.0194239679316));
#54643=CARTESIAN_POINT('Ctrl Pts',(-6.38915701008606,-36.9105275914985,
29.017816891007));
#54644=CARTESIAN_POINT('Ctrl Pts',(-6.4046217940718,-36.9394732379555,29.0162098140824));
#54645=CARTESIAN_POINT('Ctrl Pts',(-6.42042566271007,-36.9682155785928,
29.0146027371578));
#54646=CARTESIAN_POINT('Ctrl Pts',(-6.47770516985146,-37.0723892555243,
29.0087780510453));
#54647=CARTESIAN_POINT('Ctrl Pts',(-6.53962813183109,-37.1742280035309,
29.0029533649328));
#54648=CARTESIAN_POINT('Ctrl Pts',(-6.60597947346715,-37.2732904929801,
28.9971286788204));
#54649=CARTESIAN_POINT('Ctrl Pts',(-6.67224714861135,-37.3722280684371,
28.9913113374133));
#54650=CARTESIAN_POINT('Ctrl Pts',(-6.74293187168987,-37.468396012181,28.9854939960061));
#54651=CARTESIAN_POINT('Ctrl Pts',(-6.81777261894665,-37.5613773433983,
28.979676654599));
#54652=CARTESIAN_POINT('Ctrl Pts',(-6.89253848033271,-37.6542656372235,
28.9738651340407));
#54653=CARTESIAN_POINT('Ctrl Pts',(-6.97145183848653,-37.7439733456366,
28.9680536134824));
#54654=CARTESIAN_POINT('Ctrl Pts',(-7.05420864111179,-37.8301127662868,
28.9622420929242));
#54655=CARTESIAN_POINT('Ctrl Pts',(-7.14007591211693,-37.9194897932207,
28.9562121425769));
#54656=CARTESIAN_POINT('Ctrl Pts',(-7.23008096474498,-38.0050246637825,
28.9501821922296));
#54657=CARTESIAN_POINT('Ctrl Pts',(-7.32383828549135,-38.0863219983984,
28.9441522418823));
#54658=CARTESIAN_POINT('Ctrl Pts',(-7.41409757504367,-38.1645861766676,
28.938347265481));
#54659=CARTESIAN_POINT('Ctrl Pts',(-7.50783382180515,-38.2389230643019,
28.9325422890797));
#54660=CARTESIAN_POINT('Ctrl Pts',(-7.60466636419906,-38.3090182491489,
28.9267373126784));
#54661=CARTESIAN_POINT('Ctrl Pts',(-7.70148454807795,-38.3791030401476,
28.9209331970501));
#54662=CARTESIAN_POINT('Ctrl Pts',(-7.80139778398777,-38.4449471399261,
28.9151290814219));
#54663=CARTESIAN_POINT('Ctrl Pts',(-7.90399425341895,-38.5062779282737,
28.9093249657936));
#54664=CARTESIAN_POINT('Ctrl Pts',(-8.00659969626102,-38.5676140808055,
28.9035203425191));
#54665=CARTESIAN_POINT('Ctrl Pts',(-8.11188848888147,-38.6244359276154,
28.8977157192445));
#54666=CARTESIAN_POINT('Ctrl Pts',(-8.21942246366639,-38.6765158284855,
28.89191109597));
#54667=CARTESIAN_POINT('Ctrl Pts',(-8.32699119414061,-38.7286125619227,
28.886104596603));
#54668=CARTESIAN_POINT('Ctrl Pts',(-8.4368061828024,-38.7759641235285,28.8802980972359));
#54669=CARTESIAN_POINT('Ctrl Pts',(-8.5484080513187,-38.8183904743391,28.8744915978689));
#54670=CARTESIAN_POINT('Ctrl Pts',(-8.66013321073938,-38.8608636951818,
28.8686786838373));
#54671=CARTESIAN_POINT('Ctrl Pts',(-8.77364880862195,-38.89840069923,28.8628657698056));
#54672=CARTESIAN_POINT('Ctrl Pts',(-8.88847887613864,-38.9308708693125,
28.857052855774));
#54673=CARTESIAN_POINT('Ctrl Pts',(-9.0033842106199,-38.9633623224196,28.851236131587));
#54674=CARTESIAN_POINT('Ctrl Pts',(-9.11960533428275,-38.9907802338579,
28.8454194074));
#54675=CARTESIAN_POINT('Ctrl Pts',(-9.23665624722748,-39.0130451424203,
28.839602683213));
#54676=CARTESIAN_POINT('Ctrl Pts',(-9.35387441984046,-39.0353418663793,
28.8337776472296));
#54677=CARTESIAN_POINT('Ctrl Pts',(-9.47192434588376,-39.0524708321049,
28.8279526112462));
#54678=CARTESIAN_POINT('Ctrl Pts',(-9.59031493431379,-39.0644044024868,
28.8221275752628));
#54679=CARTESIAN_POINT('Ctrl Pts',(-9.62150814260123,-39.0675486249412,
28.820592811705));
#54680=CARTESIAN_POINT('Ctrl Pts',(-9.65272500215769,-39.0703324629713,
28.8190580481471));
#54681=CARTESIAN_POINT('Ctrl Pts',(-9.68395655113767,-39.0727560126321,
28.8175232845893));
#54682=CARTESIAN_POINT('Ctrl Pts',(-9.8024827349867,-39.0819535741379,28.811698736222));
#54683=CARTESIAN_POINT('Ctrl Pts',(-9.92160113173807,-39.0859875553614,
28.8058741878547));
#54684=CARTESIAN_POINT('Ctrl Pts',(-10.0408247254744,-39.0847959975732,
28.8000496394874));
#54685=CARTESIAN_POINT('Ctrl Pts',(-10.1598983033553,-39.0836059390902,
28.7942324199933));
#54686=CARTESIAN_POINT('Ctrl Pts',(-10.2790764103628,-39.0772034235936,
28.7884152004993));
#54687=CARTESIAN_POINT('Ctrl Pts',(-10.397867218127,-39.0655782708909,28.7825979810052));
#54688=CARTESIAN_POINT('Ctrl Pts',(-10.5165394860414,-39.0539647187814,
28.7767865664411));
#54689=CARTESIAN_POINT('Ctrl Pts',(-10.6348248196585,-39.0371389369318,
28.7709751518771));
#54690=CARTESIAN_POINT('Ctrl Pts',(-10.7522323021061,-39.0151427824759,
28.765163737313));
#54691=CARTESIAN_POINT('Ctrl Pts',(-10.8740557666081,-38.9923192989492,
28.7591337412592));
#54692=CARTESIAN_POINT('Ctrl Pts',(-10.9949335990444,-38.9639288690956,
28.7531037452054));
#54693=CARTESIAN_POINT('Ctrl Pts',(-11.1143237843018,-38.9300772897921,
28.7470737491515));
#54694=CARTESIAN_POINT('Ctrl Pts',(-11.2292574283504,-38.8974893064685,
28.7412688379809));
#54695=CARTESIAN_POINT('Ctrl Pts',(-11.3428120677675,-38.8598406916114,
28.7354639268102));
#54696=CARTESIAN_POINT('Ctrl Pts',(-11.4545161092082,-38.817277549256,28.7296590156396));
#54697=CARTESIAN_POINT('Ctrl Pts',(-11.5662038803135,-38.7747206064668,
28.7238549499876));
#54698=CARTESIAN_POINT('Ctrl Pts',(-11.6760412081702,-38.7272507050453,
28.7180508843356));
#54699=CARTESIAN_POINT('Ctrl Pts',(-11.7835743848829,-38.675062912875,28.7122468186836));
#54700=CARTESIAN_POINT('Ctrl Pts',(-11.8911172519402,-38.6228704178056,
28.7064422299986));
#54701=CARTESIAN_POINT('Ctrl Pts',(-11.9963551877746,-38.5659593648881,
28.7006376413137));
#54702=CARTESIAN_POINT('Ctrl Pts',(-12.098857671488,-38.5045715108749,28.6948330526287));
#54703=CARTESIAN_POINT('Ctrl Pts',(-12.201393559125,-38.4431636515397,28.689026572321));
#54704=CARTESIAN_POINT('Ctrl Pts',(-12.301191871747,-38.3772762992261,28.6832200920132));
#54705=CARTESIAN_POINT('Ctrl Pts',(-12.3978502839748,-38.3071950374361,
28.6774136117054));
#54706=CARTESIAN_POINT('Ctrl Pts',(-12.4946158665635,-38.237036072796,28.6716006934418));
#54707=CARTESIAN_POINT('Ctrl Pts',(-12.5882342689691,-38.1626741565788,
28.6657877751782));
#54708=CARTESIAN_POINT('Ctrl Pts',(-12.6783354146374,-38.0844358328062,
28.6599748569146));
#54709=CARTESIAN_POINT('Ctrl Pts',(-12.7684958290091,-38.0061460437169,
28.6541581149023));
#54710=CARTESIAN_POINT('Ctrl Pts',(-12.8551340834213,-37.9239750490683,
28.6483413728901));
#54711=CARTESIAN_POINT('Ctrl Pts',(-12.9379173972012,-37.8382858149282,
28.6425246308779));
#54712=CARTESIAN_POINT('Ctrl Pts',(-13.0208192870192,-37.7524738424073,
28.6366995571598));
#54713=CARTESIAN_POINT('Ctrl Pts',(-13.0998549457001,-37.663133876622,28.6308744834417));
#54714=CARTESIAN_POINT('Ctrl Pts',(-13.1747321532766,-37.5706615403338,
28.6250494097237));
#54715=CARTESIAN_POINT('Ctrl Pts',(-13.1944659692104,-37.546290545176,28.6235142171561));
#54716=CARTESIAN_POINT('Ctrl Pts',(-13.2139111834488,-37.5217021334563,
28.6219790245885));
#54717=CARTESIAN_POINT('Ctrl Pts',(-13.2330629616497,-37.4969038599851,
28.6204438320209));
#54718=CARTESIAN_POINT('Ctrl Pts',(-13.3056934675164,-37.4028597911819,
28.6146218236613));
#54719=CARTESIAN_POINT('Ctrl Pts',(-13.3743388331657,-37.3054865730966,
28.6087998153017));
#54720=CARTESIAN_POINT('Ctrl Pts',(-13.4386789137847,-37.205155851157,28.6029778069421));
#54721=CARTESIAN_POINT('Ctrl Pts',(-13.5029393673578,-37.1049492981481,
28.5971630038786));
#54722=CARTESIAN_POINT('Ctrl Pts',(-13.5629049116448,-37.0017928584942,
28.591348200815));
#54723=CARTESIAN_POINT('Ctrl Pts',(-13.6182957848243,-36.8960908769156,
28.5855333977514));
#54724=CARTESIAN_POINT('Ctrl Pts',(-13.6736311609314,-36.7904947999777,
28.5797244206395));
#54725=CARTESIAN_POINT('Ctrl Pts',(-13.7244007929045,-36.6823586120928,
28.5739154435275));
#54726=CARTESIAN_POINT('Ctrl Pts',(-13.7703687222174,-36.5721147218077,
28.5681064664156));
#54727=CARTESIAN_POINT('Ctrl Pts',(-13.8163014268996,-36.4619553099924,
28.5623019406478));
#54728=CARTESIAN_POINT('Ctrl Pts',(-13.8574395920708,-36.349691783766,28.55649741488));
#54729=CARTESIAN_POINT('Ctrl Pts',(-13.8935939351083,-36.235779619709,28.5506928891122));
#54730=CARTESIAN_POINT('Ctrl Pts',(-13.9297311667015,-36.1219213689992,
28.5448911105612));
#54731=CARTESIAN_POINT('Ctrl Pts',(-13.9608891443664,-36.0064164204851,
28.5390893320103));
#54732=CARTESIAN_POINT('Ctrl Pts',(-13.9869275256978,-35.889738110251,28.5332875534593));
#54733=CARTESIAN_POINT('Ctrl Pts',(-14.0129585926891,-35.7730925756662,
28.5274874046633));
#54734=CARTESIAN_POINT('Ctrl Pts',(-14.0338728387506,-35.6552747337021,
28.5216872558673));
#54735=CARTESIAN_POINT('Ctrl Pts',(-14.0495805642629,-35.5367702055292,
28.5158871070713));
#54736=CARTESIAN_POINT('Ctrl Pts',(-14.0652908719406,-35.4182461966059,
28.5100860047991));
#54737=CARTESIAN_POINT('Ctrl Pts',(-14.0757928938376,-35.2990356802547,
28.5042849025269));
#54738=CARTESIAN_POINT('Ctrl Pts',(-14.081048594519,-35.1796312032315,28.4984838002547));
#54739=CARTESIAN_POINT('Ctrl Pts',(-14.0837269136306,-35.1187823626656,
28.495527543035));
#54740=CARTESIAN_POINT('Ctrl Pts',(-14.0850436239602,-35.0578832208542,
28.4925712858152));
#54741=CARTESIAN_POINT('Ctrl Pts',(-14.0849988977552,-34.9969991103314,
28.4896150285955));
#54742=CARTESIAN_POINT('Origin',(130.,-35.,23.));
#54743=CARTESIAN_POINT('',(126.610250000496,-34.9999420099749,27.6441864590851));
#54744=CARTESIAN_POINT('Ctrl Pts',(126.821241915871,-33.8227565650717,28.8235739384178));
#54745=CARTESIAN_POINT('Ctrl Pts',(126.833574063551,-33.7894576627623,28.8214368686364));
#54746=CARTESIAN_POINT('Ctrl Pts',(126.846428176058,-33.7563559586685,28.8192724775167));
#54747=CARTESIAN_POINT('Ctrl Pts',(126.914370105375,-33.5892229961455,28.8081615787155));
#54748=CARTESIAN_POINT('Ctrl Pts',(126.977488607444,-33.4586298771998,28.798883276182));
#54749=CARTESIAN_POINT('Ctrl Pts',(127.181890612654,-33.0968701903928,28.7721255757395));
#54750=CARTESIAN_POINT('Ctrl Pts',(127.342781726071,-32.8780004792562,28.7546974138192));
#54751=CARTESIAN_POINT('Ctrl Pts',(127.561298209235,-32.6451104996121,28.7353264702612));
#54752=CARTESIAN_POINT('Ctrl Pts',(127.595341200996,-32.6103583090058,28.7324071488727));
#54753=CARTESIAN_POINT('Ctrl Pts',(127.651025511273,-32.5559094379489,28.7277842454063));
#54754=CARTESIAN_POINT('Ctrl Pts',(127.672193326602,-32.5357402743224,28.7260604886461));
#54755=CARTESIAN_POINT('Ctrl Pts',(127.713170329732,-32.4976957000816,28.7227860420401));
#54756=CARTESIAN_POINT('Ctrl Pts',(127.732934709085,-32.4797754511263,28.7212335297737));
#54757=CARTESIAN_POINT('Ctrl Pts',(127.779220933771,-32.4387931629945,28.7176579720437));
#54758=CARTESIAN_POINT('Ctrl Pts',(127.805894228396,-32.4159063257433,28.7156421643936));
#54759=CARTESIAN_POINT('Ctrl Pts',(127.894979746538,-32.3418411441775,28.7090495750105));
#54760=CARTESIAN_POINT('Ctrl Pts',(127.958865893956,-32.2924749854509,28.7045435396024));
#54761=CARTESIAN_POINT('Ctrl Pts',(128.121890932563,-32.1755553209706,28.6935119610474));
#54762=CARTESIAN_POINT('Ctrl Pts',(128.222967706627,-32.110892840549,28.6870781766475));
#54763=CARTESIAN_POINT('Ctrl Pts',(128.540676710504,-31.9306373441203,28.6676416436425));
#54764=CARTESIAN_POINT('Ctrl Pts',(128.766580194337,-31.833099526583,28.6549010351605));
#54765=CARTESIAN_POINT('Ctrl Pts',(129.034179783342,-31.7505689400022,28.6390803993295));
#54766=CARTESIAN_POINT('Ctrl Pts',(129.06751669369,-31.7408458776975,28.6370963631631));
#54767=CARTESIAN_POINT('Ctrl Pts',(129.118424733512,-31.7268429817674,28.6340385651005));
#54768=CARTESIAN_POINT('Ctrl Pts',(129.135891400908,-31.722188517689,28.6329844533612));
#54769=CARTESIAN_POINT('Ctrl Pts',(129.167867824993,-31.7139408810249,28.6310442266637));
#54770=CARTESIAN_POINT('Ctrl Pts',(129.182365306507,-31.7103036657101,28.6301605524467));
#54771=CARTESIAN_POINT('Ctrl Pts',(129.216088215963,-31.7020797438125,28.6280958626424));
#54772=CARTESIAN_POINT('Ctrl Pts',(129.235330149403,-31.6975651892273,28.626911017215));
#54773=CARTESIAN_POINT('Ctrl Pts',(129.298618259288,-31.6832992514724,28.6229943141593));
#54774=CARTESIAN_POINT('Ctrl Pts',(129.342818030257,-31.6742592338015,28.620227818892));
#54775=CARTESIAN_POINT('Ctrl Pts',(129.45257805719,-31.6540837830903,28.6133025239753));
#54776=CARTESIAN_POINT('Ctrl Pts',(129.518309811019,-31.6439904968777,28.6091069424881));
#54777=CARTESIAN_POINT('Ctrl Pts',(129.856418489977,-31.6022105947466,28.5874085795202));
#54778=CARTESIAN_POINT('Ctrl Pts',(130.131665077691,-31.6017232560519,28.5694648690226));
#54779=CARTESIAN_POINT('Ctrl Pts',(130.489187791843,-31.6446359471021,28.547088761069));
#54780=CARTESIAN_POINT('Ctrl Pts',(130.573996323768,-31.6580989268164,28.5418407029634));
#54781=CARTESIAN_POINT('Ctrl Pts',(130.690774407546,-31.6812143947729,28.5346984816899));
#54782=CARTESIAN_POINT('Ctrl Pts',(130.723244998124,-31.688138896954,28.5327215419536));
#54783=CARTESIAN_POINT('Ctrl Pts',(130.779650631762,-31.7010368067049,28.5293020596601));
#54784=CARTESIAN_POINT('Ctrl Pts',(130.803631495735,-31.7067964342686,28.5278529346695));
#54785=CARTESIAN_POINT('Ctrl Pts',(130.854011927271,-31.7194797021652,28.5248176494911));
#54786=CARTESIAN_POINT('Ctrl Pts',(130.880395126734,-31.7264615045877,28.523233452141));
#54787=CARTESIAN_POINT('Ctrl Pts',(130.944222511583,-31.7441796710833,28.5194123474784));
#54788=CARTESIAN_POINT('Ctrl Pts',(130.981571980668,-31.7552444176918,28.5171860458989));
#54789=CARTESIAN_POINT('Ctrl Pts',(131.122629814511,-31.7996912944836,28.508806063024));
#54790=CARTESIAN_POINT('Ctrl Pts',(131.224902737554,-31.8374235430999,28.5027910199424));
#54791=CARTESIAN_POINT('Ctrl Pts',(131.510552545927,-31.958751105075,28.4859516864678));
#54792=CARTESIAN_POINT('Ctrl Pts',(131.688528669577,-32.053843998535,28.4754308592064));
#54793=CARTESIAN_POINT('Ctrl Pts',(131.972640357157,-32.2398916211758,28.4572891109635));
#54794=CARTESIAN_POINT('Ctrl Pts',(132.083518499994,-32.3226036463769,28.4498021488128));
#54795=CARTESIAN_POINT('Ctrl Pts',(132.210556912132,-32.4300509138175,28.4403260785439));
#54796=CARTESIAN_POINT('Ctrl Pts',(132.231857693392,-32.4485276223424,28.4387044597264));
#54797=CARTESIAN_POINT('Ctrl Pts',(132.26525450511,-32.4782348640848,28.4361049623113));
#54798=CARTESIAN_POINT('Ctrl Pts',(132.277503724703,-32.4892921052566,28.4351390674826));
#54799=CARTESIAN_POINT('Ctrl Pts',(132.301011118523,-32.5108255619939,28.4332600906378));
#54800=CARTESIAN_POINT('Ctrl Pts',(132.312279512588,-32.5212896555105,28.4323478431613));
#54801=CARTESIAN_POINT('Ctrl Pts',(132.340103641754,-32.5474826196449,28.4300672100993));
#54802=CARTESIAN_POINT('Ctrl Pts',(132.356572224356,-32.5633026769439,28.4286922832698));
#54803=CARTESIAN_POINT('Ctrl Pts',(132.420574008729,-32.6260397841033,28.4232541322682));
#54804=CARTESIAN_POINT('Ctrl Pts',(132.466873568129,-32.6741884779096,28.4191116954963));
#54805=CARTESIAN_POINT('Ctrl Pts',(132.592778907574,-32.8131132428913,28.4073206183791));
#54806=CARTESIAN_POINT('Ctrl Pts',(132.669001151531,-32.9068190616157,28.3995527310962));
#54807=CARTESIAN_POINT('Ctrl Pts',(132.88493735272,-33.2033082280161,28.3759111475075));
#54808=CARTESIAN_POINT('Ctrl Pts',(133.00774475201,-33.4174476411746,28.3601300090901));
#54809=CARTESIAN_POINT('Ctrl Pts',(133.126745709506,-33.689855706075,28.342055373861));
#54810=CARTESIAN_POINT('Ctrl Pts',(133.146143090254,-33.7371457392357,28.3389820605837));
#54811=CARTESIAN_POINT('Ctrl Pts',(133.175225334764,-33.812881542665,28.3341594122556));
#54812=CARTESIAN_POINT('Ctrl Pts',(133.185613668949,-33.8410471117028,28.3323872630832));
#54813=CARTESIAN_POINT('Ctrl Pts',(133.204466835758,-33.8943328847204,28.3290735426164));
#54814=CARTESIAN_POINT('Ctrl Pts',(133.213013770499,-33.9194214324476,28.3275293936847));
#54815=CARTESIAN_POINT('Ctrl Pts',(133.23175051388,-33.9766097001116,28.3240446763439));
#54816=CARTESIAN_POINT('Ctrl Pts',(133.241758054909,-34.0087664656775,28.3221101037009));
#54817=CARTESIAN_POINT('Ctrl Pts',(133.271601419392,-34.1099511904523,28.3160959606109));
#54818=CARTESIAN_POINT('Ctrl Pts',(133.289724486876,-34.1794657058512,28.3120704463795));
#54819=CARTESIAN_POINT('Ctrl Pts',(133.327968512637,-34.3479156109979,28.3025241585312));
#54820=CARTESIAN_POINT('Ctrl Pts',(133.345906057418,-34.4472767692154,28.2970640277362));
#54821=CARTESIAN_POINT('Ctrl Pts',(133.376405108925,-34.6736006892021,28.2848425324381));
#54822=CARTESIAN_POINT('Ctrl Pts',(133.38628910921,-34.8007657868358,28.2781277359795));
#54823=CARTESIAN_POINT('Ctrl Pts',(133.392138767068,-35.0768172722747,28.2634418490839));
#54824=CARTESIAN_POINT('Ctrl Pts',(133.385506759669,-35.2254816572142,28.2554636453605));
#54825=CARTESIAN_POINT('Ctrl Pts',(133.365194542982,-35.4088471412835,28.2450490854384));
#54826=CARTESIAN_POINT('Ctrl Pts',(133.360682542202,-35.4444130213191,28.2430017329154));
#54827=CARTESIAN_POINT('Ctrl Pts',(133.353048190738,-35.497794836456,28.23987877211));
#54828=CARTESIAN_POINT('Ctrl Pts',(133.350345799082,-35.5156693352137,28.2388245935552));
#54829=CARTESIAN_POINT('Ctrl Pts',(133.345148625611,-35.5482782558593,28.2368845377422));
#54830=CARTESIAN_POINT('Ctrl Pts',(133.34269919995,-35.5630190100192,28.2360011060033));
#54831=CARTESIAN_POINT('Ctrl Pts',(133.336786124291,-35.5972047483972,28.2339375059085));
#54832=CARTESIAN_POINT('Ctrl Pts',(133.333249917837,-35.6166361119619,28.2327535167855));
#54833=CARTESIAN_POINT('Ctrl Pts',(133.321094071103,-35.6802700831552,28.2288424149936));
#54834=CARTESIAN_POINT('Ctrl Pts',(133.311763656093,-35.7243302334475,28.2260807907919));
#54835=CARTESIAN_POINT('Ctrl Pts',(133.286526800118,-35.8327943668122,28.2191705954585));
#54836=CARTESIAN_POINT('Ctrl Pts',(133.269602443916,-35.8969413793448,28.214985427496));
#54837=CARTESIAN_POINT('Ctrl Pts',(133.173703284366,-36.2214957508718,28.1934320970228));
#54838=CARTESIAN_POINT('Ctrl Pts',(133.065443947851,-36.4722528640407,28.1756258173543));
#54839=CARTESIAN_POINT('Ctrl Pts',(132.884147298716,-36.7832008180712,28.1532397239967));
#54840=CARTESIAN_POINT('Ctrl Pts',(132.837000973545,-36.8572932845562,28.1478693089175));
#54841=CARTESIAN_POINT('Ctrl Pts',(132.765943672843,-36.959931809334,28.1403782003703));
#54842=CARTESIAN_POINT('Ctrl Pts',(132.744361227893,-36.9900398771756,28.1381739233098));
#54843=CARTESIAN_POINT('Ctrl Pts',(132.706226242686,-37.0414385359868,28.1343975875296));
#54844=CARTESIAN_POINT('Ctrl Pts',(132.689905509209,-37.0628960678669,28.1328169252894));
#54845=CARTESIAN_POINT('Ctrl Pts',(132.655821739017,-37.1066150234773,28.1295867909048));
#54846=CARTESIAN_POINT('Ctrl Pts',(132.638030625693,-37.128851910383,28.1279385881348));
#54847=CARTESIAN_POINT('Ctrl Pts',(132.591425718131,-37.1856212492617,28.1237152429296));
#54848=CARTESIAN_POINT('Ctrl Pts',(132.562200668219,-37.2198097891668,28.1211566173981));
#54849=CARTESIAN_POINT('Ctrl Pts',(132.400324077677,-37.4017211869068,28.1074384328021));
#54850=CARTESIAN_POINT('Ctrl Pts',(132.255566357925,-37.5381592034005,28.0967978208873));
#54851=CARTESIAN_POINT('Ctrl Pts',(131.932366639642,-37.7931679873723,28.0749434529271));
#54852=CARTESIAN_POINT('Ctrl Pts',(131.752988760412,-37.9090961702754,28.0637879604533));
#54853=CARTESIAN_POINT('Ctrl Pts',(131.525782287855,-38.0272500903273,28.0494316278816));
#54854=CARTESIAN_POINT('Ctrl Pts',(131.487253482213,-38.0463636396839,28.0469889181108));
#54855=CARTESIAN_POINT('Ctrl Pts',(131.431015780375,-38.0729411767222,28.0433970359435));
#54856=CARTESIAN_POINT('Ctrl Pts',(131.41358924603,-38.080996437068,28.0422803975341));
#54857=CARTESIAN_POINT('Ctrl Pts',(131.382491333171,-38.0950518027564,28.0402797299016));
#54858=CARTESIAN_POINT('Ctrl Pts',(131.368847325059,-38.1011102745544,28.0393991576625));
#54859=CARTESIAN_POINT('Ctrl Pts',(131.338430368373,-38.114376738193,28.0374295816383));
#54860=CARTESIAN_POINT('Ctrl Pts',(131.321639112141,-38.1215394186853,28.0363381096993));
#54861=CARTESIAN_POINT('Ctrl Pts',(131.270863821115,-38.1427156241531,28.0330267861333));
#54862=CARTESIAN_POINT('Ctrl Pts',(131.236709926645,-38.1563118773537,28.0307849513599));
#54863=CARTESIAN_POINT('Ctrl Pts',(131.155458911971,-38.1871357451455,28.0254288223517));
#54864=CARTESIAN_POINT('Ctrl Pts',(131.108187739638,-38.2038787484316,28.0222948190829));
#54865=CARTESIAN_POINT('Ctrl Pts',(130.924509054455,-38.2643847731338,28.0100921214553));
#54866=CARTESIAN_POINT('Ctrl Pts',(130.785753795227,-38.3005322689072,28.0008278114887));
#54867=CARTESIAN_POINT('Ctrl Pts',(130.437288270604,-38.3680865832329,27.97796250853));
#54868=CARTESIAN_POINT('Ctrl Pts',(130.226098857396,-38.38882440937,27.9644806993655));
#54869=CARTESIAN_POINT('Ctrl Pts',(129.961456414662,-38.3899432452389,27.9483678954458));
#54870=CARTESIAN_POINT('Ctrl Pts',(129.908581967943,-38.3889296286348,27.9451848810891));
#54871=CARTESIAN_POINT('Ctrl Pts',(129.825379583772,-38.3853857744695,27.940231192331));
#54872=CARTESIAN_POINT('Ctrl Pts',(129.79502668014,-38.383683667258,27.9384355684792));
#54873=CARTESIAN_POINT('Ctrl Pts',(129.738307450002,-38.3797369738032,27.9351006612185));
#54874=CARTESIAN_POINT('Ctrl Pts',(129.71193675565,-38.3775915425938,27.9335584555133));
#54875=CARTESIAN_POINT('Ctrl Pts',(129.652628559471,-38.3720667623539,27.930107556462));
#54876=CARTESIAN_POINT('Ctrl Pts',(129.619709768729,-38.3685131168181,27.9282043773497));
#54877=CARTESIAN_POINT('Ctrl Pts',(129.518788811183,-38.3561201829704,27.9224032998985));
#54878=CARTESIAN_POINT('Ctrl Pts',(129.450996586785,-38.3456991824849,27.9185538895824));
#54879=CARTESIAN_POINT('Ctrl Pts',(129.290672756162,-38.3160494238967,27.9095255495407));
#54880=CARTESIAN_POINT('Ctrl Pts',(129.198536670883,-38.2949942421069,27.9043981749614));
#54881=CARTESIAN_POINT('Ctrl Pts',(128.89490598293,-38.2121158915519,27.887509774008));
#54882=CARTESIAN_POINT('Ctrl Pts',(128.688587700696,-38.1335459414615,27.8760771398493));
#54883=CARTESIAN_POINT('Ctrl Pts',(128.414656411637,-37.9974034243499,27.859426531554));
#54884=CARTESIAN_POINT('Ctrl Pts',(128.339431767106,-37.9563918011335,27.8546816818741));
#54885=CARTESIAN_POINT('Ctrl Pts',(128.243997620173,-37.8995701974791,27.8483322501311));
#54886=CARTESIAN_POINT('Ctrl Pts',(128.222296141297,-37.8863160943402,27.8468654561853));
#54887=CARTESIAN_POINT('Ctrl Pts',(128.18726627644,-37.8643768094663,27.8444568225998));
#54888=CARTESIAN_POINT('Ctrl Pts',(128.173845914495,-37.8558395075002,27.843524111636));
#54889=CARTESIAN_POINT('Ctrl Pts',(128.147207344192,-37.8386289605609,27.8416518134364));
#54890=CARTESIAN_POINT('Ctrl Pts',(128.133988757082,-37.82995707004,27.8407123166043));
#54891=CARTESIAN_POINT('Ctrl Pts',(128.10004244536,-37.8073457742072,27.8382736025057));
#54892=CARTESIAN_POINT('Ctrl Pts',(128.07940761048,-37.7932693745054,27.8367658989528));
#54893=CARTESIAN_POINT('Ctrl Pts',(127.986697023176,-37.7285123345843,27.8298833731564));
#54894=CARTESIAN_POINT('Ctrl Pts',(127.916463262321,-37.6752645928473,27.8243695214119));
#54895=CARTESIAN_POINT('Ctrl Pts',(127.689682256208,-37.4889797805725,27.805740958767));
#54896=CARTESIAN_POINT('Ctrl Pts',(127.543151642975,-37.3444590254826,27.792345641333));
#54897=CARTESIAN_POINT('Ctrl Pts',(127.31325831958,-37.0723359830616,27.769667198596));
#54898=CARTESIAN_POINT('Ctrl Pts',(127.223705754414,-36.9507324731433,27.7602541048155));
#54899=CARTESIAN_POINT('Ctrl Pts',(127.119024550753,-36.7866999832605,27.7485000919317));
#54900=CARTESIAN_POINT('Ctrl Pts',(127.096220091915,-36.7493938614791,27.7458846883742));
#54901=CARTESIAN_POINT('Ctrl Pts',(127.059893240694,-36.6872977410977,27.7416236174423));
#54902=CARTESIAN_POINT('Ctrl Pts',(127.045948027024,-36.6627622909291,27.7399630554176));
#54903=CARTESIAN_POINT('Ctrl Pts',(127.01921739195,-36.6143339870321,27.736729338175));
#54904=CARTESIAN_POINT('Ctrl Pts',(127.006408884253,-36.5904563723308,27.7351554585054));
#54905=CARTESIAN_POINT('Ctrl Pts',(126.976393484072,-36.5328541678085,27.7314060545317));
#54906=CARTESIAN_POINT('Ctrl Pts',(126.959462393848,-36.4989894900393,27.7292401466531));
#54907=CARTESIAN_POINT('Ctrl Pts',(126.899928201952,-36.374751302794,27.72142502383));
#54908=CARTESIAN_POINT('Ctrl Pts',(126.86075670556,-36.282786136086,27.7158902365737));
#54909=CARTESIAN_POINT('Ctrl Pts',(126.765709302514,-36.0290828060731,27.7011331877452));
#54910=CARTESIAN_POINT('Ctrl Pts',(126.717917927243,-35.8646316876755,27.6921206186954));
#54911=CARTESIAN_POINT('Ctrl Pts',(126.648436028572,-35.5340743001795,27.6741926342898));
#54912=CARTESIAN_POINT('Ctrl Pts',(126.626225508301,-35.3685797852238,27.6652999999467));
#54913=CARTESIAN_POINT('Ctrl Pts',(126.614173178845,-35.1668323622302,27.653893111756));
#54914=CARTESIAN_POINT('Ctrl Pts',(126.612616692744,-35.1314930595958,27.6518737807094));
#54915=CARTESIAN_POINT('Ctrl Pts',(126.611111507407,-35.0784424023675,27.6488020920364));
#54916=CARTESIAN_POINT('Ctrl Pts',(126.610748086028,-35.0607442141275,27.6477706215128));
#54917=CARTESIAN_POINT('Ctrl Pts',(126.610410284175,-35.0341444448989,27.6462091799433));
#54918=CARTESIAN_POINT('Ctrl Pts',(126.610332314739,-35.0252441494281,27.6456848355043));
#54919=CARTESIAN_POINT('Ctrl Pts',(126.610263040116,-35.0108764159749,27.644835224476));
#54920=CARTESIAN_POINT('Ctrl Pts',(126.610249906966,-35.0054091932058,27.6445111982693));
#54921=CARTESIAN_POINT('Ctrl Pts',(126.610250000496,-34.9999420099749,27.6441864590851));
#54922=CARTESIAN_POINT('Ctrl Pts',(126.610250000487,-34.9999425486175,27.6441864910793));
#54923=CARTESIAN_POINT('Ctrl Pts',(126.610250211739,-34.9874782475485,27.6434461379204));
#54924=CARTESIAN_POINT('Ctrl Pts',(126.610319170897,-34.9750142253258,27.6427020834383));
#54925=CARTESIAN_POINT('Ctrl Pts',(126.610721397634,-34.938608265017,27.6405184802462));
#54926=CARTESIAN_POINT('Ctrl Pts',(126.611239599136,-34.9146696669379,27.6390696402569));
#54927=CARTESIAN_POINT('Ctrl Pts',(126.614490498641,-34.8138647903812,27.6329193133682));
#54928=CARTESIAN_POINT('Ctrl Pts',(126.619585242127,-34.7371021297444,27.6281154409567));
#54929=CARTESIAN_POINT('Ctrl Pts',(126.648696526434,-34.44782777585,27.6097103485302));
#54930=CARTESIAN_POINT('Ctrl Pts',(126.690190415604,-34.2375741406169,27.5957488678196));
#54931=CARTESIAN_POINT('Ctrl Pts',(126.772269698362,-33.9619227091561,27.5774401648129));
#54932=CARTESIAN_POINT('Ctrl Pts',(126.795624121705,-33.8919289802302,27.5727865041634));
#54933=CARTESIAN_POINT('Ctrl Pts',(126.821241909639,-33.8227565818973,27.5681924492054));
#54934=CARTESIAN_POINT('',(126.610251311733,-35.0029820949929,27.9839821967168));
#54935=CARTESIAN_POINT('Ctrl Pts',(126.821241915871,-33.8227565650715,27.9134201656876));
#54936=CARTESIAN_POINT('Ctrl Pts',(126.785588882404,-33.919025836993,27.9194241939558));
#54937=CARTESIAN_POINT('Ctrl Pts',(126.754305382504,-34.0169374341092,27.925428222224));
#54938=CARTESIAN_POINT('Ctrl Pts',(126.727532847368,-34.1160521523038,27.9314322504923));
#54939=CARTESIAN_POINT('Ctrl Pts',(126.700760123262,-34.2151675700899,27.9374363211393));
#54940=CARTESIAN_POINT('Ctrl Pts',(126.678498534611,-34.3154856987428,27.9434403917864));
#54941=CARTESIAN_POINT('Ctrl Pts',(126.660838976266,-34.4165544412042,27.9494444624335));
#54942=CARTESIAN_POINT('Ctrl Pts',(126.643163513067,-34.5177142099312,27.9554539405697));
#54943=CARTESIAN_POINT('Ctrl Pts',(126.630098428695,-34.6196255074683,27.9614634187059));
#54944=CARTESIAN_POINT('Ctrl Pts',(126.621683002295,-34.7218286040624,27.9674728968422));
#54945=CARTESIAN_POINT('Ctrl Pts',(126.613976687101,-34.8154197352465,27.9729759968004));
#54946=CARTESIAN_POINT('Ctrl Pts',(126.610168856536,-34.9092552371277,27.9784790967586));
#54947=CARTESIAN_POINT('Ctrl Pts',(126.610251311733,-35.0029820949929,27.9839821967168));
#54948=CARTESIAN_POINT('Ctrl Pts',(126.821241931958,-33.822756521634,29.1634528404117));
#54949=CARTESIAN_POINT('Ctrl Pts',(126.865650864581,-33.702844833472,29.1566721449487));
#54950=CARTESIAN_POINT('Ctrl Pts',(126.916816893519,-33.5855216471383,29.1498638995743));
#54951=CARTESIAN_POINT('Ctrl Pts',(127.017823728585,-33.3856089084275,29.137646274305));
#54952=CARTESIAN_POINT('Ctrl Pts',(127.064768592437,-33.3017514046476,29.1323182721239));
#54953=CARTESIAN_POINT('Ctrl Pts',(127.134768948841,-33.188303646206,29.124753211007));
#54954=CARTESIAN_POINT('Ctrl Pts',(127.154850188462,-33.15692782321,29.1226215173715));
#54955=CARTESIAN_POINT('Ctrl Pts',(127.190309408356,-33.1034856211516,29.1189185568259));
#54956=CARTESIAN_POINT('Ctrl Pts',(127.205440666592,-33.0812592460935,29.1173564772224));
#54957=CARTESIAN_POINT('Ctrl Pts',(127.23697965579,-33.0360960238724,29.1141356895905));
#54958=CARTESIAN_POINT('Ctrl Pts',(127.253412376225,-33.0131792726201,29.1124761148223));
#54959=CARTESIAN_POINT('Ctrl Pts',(127.2962617206,-32.9549700219748,29.1081940823907));
#54960=CARTESIAN_POINT('Ctrl Pts',(127.323083733854,-32.9199838167422,29.1055562095267));
#54961=CARTESIAN_POINT('Ctrl Pts',(127.450382364417,-32.7604791208009,29.0932234457836));
#54962=CARTESIAN_POINT('Ctrl Pts',(127.558900920604,-32.6426651286359,29.0832146986985));
#54963=CARTESIAN_POINT('Ctrl Pts',(127.819908092753,-32.3967187414527,29.0603213707334));
#54964=CARTESIAN_POINT('Ctrl Pts',(127.976190247168,-32.273451629026,29.0473619932687));
#54965=CARTESIAN_POINT('Ctrl Pts',(128.214995589976,-32.1169974486217,29.0292401220475));
#54966=CARTESIAN_POINT('Ctrl Pts',(128.289433426241,-32.0722177603212,29.0238063083829));
#54967=CARTESIAN_POINT('Ctrl Pts',(128.387227475203,-32.0183923583476,29.0170125706348));
#54968=CARTESIAN_POINT('Ctrl Pts',(128.409071749994,-32.0066796483224,29.0155164962485));
#54969=CARTESIAN_POINT('Ctrl Pts',(128.444967702716,-31.9879365260305,29.0130952867612));
#54970=CARTESIAN_POINT('Ctrl Pts',(128.458942971785,-31.9807624998397,29.0121617492703));
#54971=CARTESIAN_POINT('Ctrl Pts',(128.487168747003,-31.9665202050456,29.010295303811));
#54972=CARTESIAN_POINT('Ctrl Pts',(128.501420030712,-31.9594546271057,29.009362537866));
#54973=CARTESIAN_POINT('Ctrl Pts',(128.538583192545,-31.941354441335,29.0069536979618));
#54974=CARTESIAN_POINT('Ctrl Pts',(128.561570856652,-31.9304766786006,29.0054867549124));
#54975=CARTESIAN_POINT('Ctrl Pts',(128.662514955512,-31.8840930157107,28.9991361042091));
#54976=CARTESIAN_POINT('Ctrl Pts',(128.74168430787,-31.8512881295849,28.9943902453128));
#54977=CARTESIAN_POINT('Ctrl Pts',(129.00813747748,-31.7525375185348,28.9789228088012));
#54978=CARTESIAN_POINT('Ctrl Pts',(129.199963624613,-31.7000374467142,28.9685733775538));
#54979=CARTESIAN_POINT('Ctrl Pts',(129.55144366072,-31.6363133107145,28.9494984156279));
#54980=CARTESIAN_POINT('Ctrl Pts',(129.709378552225,-31.6190056667288,28.9408906852994));
#54981=CARTESIAN_POINT('Ctrl Pts',(129.912061082677,-31.6111031502578,28.9294549390198));
#54982=CARTESIAN_POINT('Ctrl Pts',(129.956214791871,-31.6102451837655,28.9269411478639));
#54983=CARTESIAN_POINT('Ctrl Pts',(130.028708600315,-31.6102531241889,28.922771030121));
#54984=CARTESIAN_POINT('Ctrl Pts',(130.057044108881,-31.6106115648018,28.9211303370611));
#54985=CARTESIAN_POINT('Ctrl Pts',(130.112453997717,-31.6120075110482,28.9178995791691));
#54986=CARTESIAN_POINT('Ctrl Pts',(130.13952705016,-31.6130144455984,28.9163105767614));
#54987=CARTESIAN_POINT('Ctrl Pts',(130.204204410876,-31.6161967697733,28.9124882831013));
#54988=CARTESIAN_POINT('Ctrl Pts',(130.241789604117,-31.6186746151426,28.9102458749964));
#54989=CARTESIAN_POINT('Ctrl Pts',(130.377190647787,-31.6298701035138,28.9020880662825));
#54990=CARTESIAN_POINT('Ctrl Pts',(130.474650690925,-31.6422102262792,28.8960643239744));
#54991=CARTESIAN_POINT('Ctrl Pts',(130.734308518476,-31.6866178739626,28.8796148188599));
#54992=CARTESIAN_POINT('Ctrl Pts',(130.894919092059,-31.7263442737321,28.8690037658878));
#54993=CARTESIAN_POINT('Ctrl Pts',(131.217727904092,-31.8317284950796,28.8471234106422));
#54994=CARTESIAN_POINT('Ctrl Pts',(131.3790669967,-31.8985505391931,28.8358831378486));
#54995=CARTESIAN_POINT('Ctrl Pts',(131.566289333661,-31.9936052744687,28.8229574015941));
#54996=CARTESIAN_POINT('Ctrl Pts',(131.597766866808,-32.0102152624157,28.8207890125636));
#54997=CARTESIAN_POINT('Ctrl Pts',(131.644808987484,-32.0359935351618,28.8175621701658));
#54998=CARTESIAN_POINT('Ctrl Pts',(131.660570545962,-32.0447950286094,28.8164833788081));
#54999=CARTESIAN_POINT('Ctrl Pts',(131.689276664858,-32.0611271478006,28.8145240076353));
#55000=CARTESIAN_POINT('Ctrl Pts',(131.702242295708,-32.0686179930126,28.8136411742244));
#55001=CARTESIAN_POINT('Ctrl Pts',(131.732299918191,-32.0862503554271,28.8115991880103));
#55002=CARTESIAN_POINT('Ctrl Pts',(131.749352908455,-32.0964565715465,28.8104440817585));
#55003=CARTESIAN_POINT('Ctrl Pts',(131.805326829381,-32.1306291259969,28.8066605746648));
#55004=CARTESIAN_POINT('Ctrl Pts',(131.843854335682,-32.1552336159002,28.8040691527834));
#55005=CARTESIAN_POINT('Ctrl Pts',(131.938202223027,-32.2182085597067,28.7977251899512));
#55006=CARTESIAN_POINT('Ctrl Pts',(131.993393707962,-32.2574876622457,28.794015801596));
#55007=CARTESIAN_POINT('Ctrl Pts',(132.279841935849,-32.474568543669,28.7745700720025));
#55008=CARTESIAN_POINT('Ctrl Pts',(132.488595995966,-32.6800036646978,28.7595917353172));
#55009=CARTESIAN_POINT('Ctrl Pts',(132.713973584988,-32.9677118219575,28.7394159075654));
#55010=CARTESIAN_POINT('Ctrl Pts',(132.757558151112,-33.0272557618188,28.7352845515418));
#55011=CARTESIAN_POINT('Ctrl Pts',(132.81835081605,-33.1162640606414,28.7291420893276));
#55012=CARTESIAN_POINT('Ctrl Pts',(132.837113579737,-33.144643207469,28.7271884795051));
#55013=CARTESIAN_POINT('Ctrl Pts',(132.869753033185,-33.1956642527425,28.723682165818));
#55014=CARTESIAN_POINT('Ctrl Pts',(132.883796939454,-33.2181961069571,28.7221357366294));
#55015=CARTESIAN_POINT('Ctrl Pts',(132.913059183982,-33.2663963551876,28.7188307460978));
#55016=CARTESIAN_POINT('Ctrl Pts',(132.928206093067,-33.2921052731478,28.7170697883524));
#55017=CARTESIAN_POINT('Ctrl Pts',(132.968586724072,-33.3627600730744,28.7122337149015));
#55018=CARTESIAN_POINT('Ctrl Pts',(132.993137055083,-33.4080854766099,28.7091350395298));
#55019=CARTESIAN_POINT('Ctrl Pts',(133.091671751514,-33.6003459356898,28.6960008542175));
#55020=CARTESIAN_POINT('Ctrl Pts',(133.155934954993,-33.751990174415,28.6856498456774));
#55021=CARTESIAN_POINT('Ctrl Pts',(133.288741422585,-34.1421396210965,28.6592588276333));
#55022=CARTESIAN_POINT('Ctrl Pts',(133.342616393357,-34.3846400963994,28.6430347561294));
#55023=CARTESIAN_POINT('Ctrl Pts',(133.373330469998,-34.6649975792445,28.6256832696096));
#55024=CARTESIAN_POINT('Ctrl Pts',(133.376552272186,-34.6992010139932,28.6235909713055));
#55025=CARTESIAN_POINT('Ctrl Pts',(133.380668847835,-34.7513897036637,28.6204417316801));
#55026=CARTESIAN_POINT('Ctrl Pts',(133.381941134373,-34.7693419549542,28.6193662152861));
#55027=CARTESIAN_POINT('Ctrl Pts',(133.384008393886,-34.8022230716624,28.6174115938886));
#55028=CARTESIAN_POINT('Ctrl Pts',(133.384847648285,-34.8171477837951,28.6165302587124));
#55029=CARTESIAN_POINT('Ctrl Pts',(133.386571681928,-34.8519072724532,28.6144908902231));
#55030=CARTESIAN_POINT('Ctrl Pts',(133.387380976814,-34.8717448945619,28.6133369114024));
#55031=CARTESIAN_POINT('Ctrl Pts',(133.389476902568,-34.9372459026435,28.6095560235844));
#55032=CARTESIAN_POINT('Ctrl Pts',(133.390014864614,-34.9829299873729,28.6069661183035));
#55033=CARTESIAN_POINT('Ctrl Pts',(133.389057858057,-35.0963006264341,28.6006256429669));
#55034=CARTESIAN_POINT('Ctrl Pts',(133.386459103189,-35.1639592691376,28.5969182674979));
#55035=CARTESIAN_POINT('Ctrl Pts',(133.361939831642,-35.5221489653176,28.5774948197096));
#55036=CARTESIAN_POINT('Ctrl Pts',(133.304660383949,-35.8090170149409,28.5625369696971));
#55037=CARTESIAN_POINT('Ctrl Pts',(133.187667351783,-36.1552834848121,28.5423659962037));
#55038=CARTESIAN_POINT('Ctrl Pts',(133.161635691132,-36.2247292532434,28.5382147262456));
#55039=CARTESIAN_POINT('Ctrl Pts',(133.120353455634,-36.3247489047332,28.5320493436718));
#55040=CARTESIAN_POINT('Ctrl Pts',(133.106884190087,-36.3560368202566,28.5300934798964));
#55041=CARTESIAN_POINT('Ctrl Pts',(133.082089169933,-36.4113239616813,28.5265860795067));
#55042=CARTESIAN_POINT('Ctrl Pts',(133.07094869315,-36.4354034420038,28.5250408761394));
#55043=CARTESIAN_POINT('Ctrl Pts',(133.046713591717,-36.4862123551714,28.5217417350145));
#55044=CARTESIAN_POINT('Ctrl Pts',(133.033547332127,-36.5129049453734,28.5199854463282));
#55045=CARTESIAN_POINT('Ctrl Pts',(132.996750929229,-36.585092063633,28.5151710481448));
#55046=CARTESIAN_POINT('Ctrl Pts',(132.972438231204,-36.6302280558076,28.5120896792608));
#55047=CARTESIAN_POINT('Ctrl Pts',(132.866770448989,-36.8161702651956,28.499090100135));
#55048=CARTESIAN_POINT('Ctrl Pts',(132.776369540242,-36.9515655272575,28.4888637184202));
#55049=CARTESIAN_POINT('Ctrl Pts',(132.522589336101,-37.2781481025811,28.4623892693826));
#55050=CARTESIAN_POINT('Ctrl Pts',(132.347023545526,-37.4586385631106,28.4459352946881));
#55051=CARTESIAN_POINT('Ctrl Pts',(132.127078864026,-37.6395224514217,28.4284255514894));
#55052=CARTESIAN_POINT('Ctrl Pts',(132.10070214109,-37.6605627159295,28.4263716321593));
#55053=CARTESIAN_POINT('Ctrl Pts',(132.059888610862,-37.6921335252834,28.4232685241094));
#55054=CARTESIAN_POINT('Ctrl Pts',(132.045676094596,-37.7029490106906,28.4222015073409));
#55055=CARTESIAN_POINT('Ctrl Pts',(132.019399273316,-37.7226192444384,28.4202545856474));
#55056=CARTESIAN_POINT('Ctrl Pts',(132.007361298214,-37.7315068376044,28.4193725793892));
#55057=CARTESIAN_POINT('Ctrl Pts',(131.979065934881,-37.7521091136718,28.4173220355156));
#55058=CARTESIAN_POINT('Ctrl Pts',(131.96276301018,-37.7637597501321,28.416157714943));
#55059=CARTESIAN_POINT('Ctrl Pts',(131.908077242125,-37.8021121334996,28.4123055047588));
#55060=CARTESIAN_POINT('Ctrl Pts',(131.869243843123,-37.8281653188411,28.4096565257023));
#55061=CARTESIAN_POINT('Ctrl Pts',(131.770993777703,-37.8911727889326,28.4031350224538));
#55062=CARTESIAN_POINT('Ctrl Pts',(131.710947557345,-37.9271075331202,28.399308913883));
#55063=CARTESIAN_POINT('Ctrl Pts',(131.404640359588,-38.0977685712417,28.3803647875889));
#55064=CARTESIAN_POINT('Ctrl Pts',(131.143439428503,-38.2033948837027,28.3659218698166));
#55065=CARTESIAN_POINT('Ctrl Pts',(130.796968171429,-38.2956498261437,28.3461864791395));
#55066=CARTESIAN_POINT('Ctrl Pts',(130.721073707885,-38.3130827807271,28.3418376679014));
#55067=CARTESIAN_POINT('Ctrl Pts',(130.610438711454,-38.3345140538044,28.335425624827));
#55068=CARTESIAN_POINT('Ctrl Pts',(130.57612818682,-38.3406130544841,28.3334272493346));
#55069=CARTESIAN_POINT('Ctrl Pts',(130.515353065313,-38.3504522518076,28.3298673356849));
#55070=CARTESIAN_POINT('Ctrl Pts',(130.488926526695,-38.3544105093142,28.3283127184016));
#55071=CARTESIAN_POINT('Ctrl Pts',(130.433632686867,-38.3620253306843,28.3250448191752));
#55072=CARTESIAN_POINT('Ctrl Pts',(130.404759665552,-38.3656234438039,28.3233298578134));
#55073=CARTESIAN_POINT('Ctrl Pts',(130.328182370857,-38.3741667642635,28.3187574235033));
#55074=CARTESIAN_POINT('Ctrl Pts',(130.280414655935,-38.3784718868008,28.3158805496174));
#55075=CARTESIAN_POINT('Ctrl Pts',(130.02593310052,-38.3959733109343,28.300416783084));
#55076=CARTESIAN_POINT('Ctrl Pts',(129.818454706349,-38.391213019506,28.2872895231079));
#55077=CARTESIAN_POINT('Ctrl Pts',(129.40037926935,-38.3431350981244,28.2602121526972));
#55078=CARTESIAN_POINT('Ctrl Pts',(129.190795683427,-38.298681060548,28.2463138403642));
#55079=CARTESIAN_POINT('Ctrl Pts',(128.955398940729,-38.2249489121988,28.2311599191909));
#55080=CARTESIAN_POINT('Ctrl Pts',(128.92415540516,-38.21466101476,28.2291589720985));
#55081=CARTESIAN_POINT('Ctrl Pts',(128.876346244365,-38.1981432417472,28.2261183644967));
#55082=CARTESIAN_POINT('Ctrl Pts',(128.859672197048,-38.1922359702146,28.2250619347378));
#55083=CARTESIAN_POINT('Ctrl Pts',(128.829081779952,-38.1811281419797,28.2231322082853));
#55084=CARTESIAN_POINT('Ctrl Pts',(128.81515278015,-38.1759664369078,28.2222568734248));
#55085=CARTESIAN_POINT('Ctrl Pts',(128.782334326936,-38.1635588560237,28.2202018837192));
#55086=CARTESIAN_POINT('Ctrl Pts',(128.763475192099,-38.1562352209384,28.2190267065331));
#55087=CARTESIAN_POINT('Ctrl Pts',(128.700148423394,-38.1309885696127,28.2150963704062));
#55088=CARTESIAN_POINT('Ctrl Pts',(128.655993923941,-38.1122904248296,28.2123823065342));
#55089=CARTESIAN_POINT('Ctrl Pts',(128.54609179637,-38.0629746996909,28.2056584663242));
#55090=CARTESIAN_POINT('Ctrl Pts',(128.480900897326,-38.0311717335472,28.2016988991137));
#55091=CARTESIAN_POINT('Ctrl Pts',(128.27496513587,-37.9223931250671,28.1891346521279));
#55092=CARTESIAN_POINT('Ctrl Pts',(128.138644685991,-37.8375140776417,28.1807224070989));
#55093=CARTESIAN_POINT('Ctrl Pts',(127.869299741438,-37.6420166906638,28.1629959554046));
#55094=CARTESIAN_POINT('Ctrl Pts',(127.737702033916,-37.5302440323514,28.1536826941632));
#55095=CARTESIAN_POINT('Ctrl Pts',(127.583536982917,-37.377623746849,28.1414567674077));
#55096=CARTESIAN_POINT('Ctrl Pts',(127.552511254712,-37.3456740560293,28.1389224963165));
#55097=CARTESIAN_POINT('Ctrl Pts',(127.502753839617,-37.2923726811027,28.1347288901729));
#55098=CARTESIAN_POINT('Ctrl Pts',(127.483644651331,-37.2713798851415,28.1330856096267));
#55099=CARTESIAN_POINT('Ctrl Pts',(127.446875756158,-37.2299531195062,28.1298575183643));
#55100=CARTESIAN_POINT('Ctrl Pts',(127.429192116281,-37.2095431839829,28.1282738731182));
#55101=CARTESIAN_POINT('Ctrl Pts',(127.387654791971,-37.1604282943073,28.1244777296392));
#55102=CARTESIAN_POINT('Ctrl Pts',(127.364028005377,-37.1315368580672,28.1222563839726));
#55103=CARTESIAN_POINT('Ctrl Pts',(127.281966709627,-37.02773889171,28.1143138125225));
#55104=CARTESIAN_POINT('Ctrl Pts',(127.226213281078,-36.9507779503513,28.1084918287921));
#55105=CARTESIAN_POINT('Ctrl Pts',(127.087448715858,-36.7412329788623,28.0928172146615));
#55106=CARTESIAN_POINT('Ctrl Pts',(127.010256594028,-36.6050776682874,28.0828006059806));
#55107=CARTESIAN_POINT('Ctrl Pts',(126.860896257594,-36.2931896405955,28.0605166503736));
#55108=CARTESIAN_POINT('Ctrl Pts',(126.793520836425,-36.1157119601657,28.0482568228123));
#55109=CARTESIAN_POINT('Ctrl Pts',(126.731823219316,-35.9003426565637,28.0344717635883));
#55110=CARTESIAN_POINT('Ctrl Pts',(126.722824778079,-35.8670173767127,28.0323692334853));
#55111=CARTESIAN_POINT('Ctrl Pts',(126.709903117556,-35.8160837043503,28.0292079662754));
#55112=CARTESIAN_POINT('Ctrl Pts',(126.705609054892,-35.7985727526427,28.0281304448739));
#55113=CARTESIAN_POINT('Ctrl Pts',(126.698010715842,-35.7664823968006,28.0261738528277));
#55114=CARTESIAN_POINT('Ctrl Pts',(126.694662980902,-35.7519146888537,28.0252925238941));
#55115=CARTESIAN_POINT('Ctrl Pts',(126.687101650162,-35.7179848072703,28.023255393623));
#55116=CARTESIAN_POINT('Ctrl Pts',(126.68296131409,-35.6986072266556,28.0221036095574));
#55117=CARTESIAN_POINT('Ctrl Pts',(126.674518282434,-35.6573239027156,28.0196723419892));
#55118=CARTESIAN_POINT('Ctrl Pts',(126.670261568484,-35.6354096292043,28.0183952069511));
#55119=CARTESIAN_POINT('Ctrl Pts',(126.65909154854,-35.5747068683642,28.0148907004978));
#55120=CARTESIAN_POINT('Ctrl Pts',(126.652637350317,-35.5358365371097,28.0126839168103));
#55121=CARTESIAN_POINT('Ctrl Pts',(126.622634442689,-35.3333576298257,28.0013415814903));
#55122=CARTESIAN_POINT('Ctrl Pts',(126.610397109784,-35.1682933274947,27.9926037001798));
#55123=CARTESIAN_POINT('Ctrl Pts',(126.610251318367,-35.0029896261394,27.9838401394632));
#55124=CARTESIAN_POINT('Origin',(130.,-35.,32.7603849714045));
#55125=CARTESIAN_POINT('',(125.915001580774,-35.0035937335827,28.3853849713762));
#55126=CARTESIAN_POINT('Ctrl Pts',(132.487160670875,-31.7594357285724,29.1925548588025));
#55127=CARTESIAN_POINT('Ctrl Pts',(132.581690749928,-31.8319883691446,29.1867409052004));
#55128=CARTESIAN_POINT('Ctrl Pts',(132.673154069962,-31.9087655494671,29.1809269515982));
#55129=CARTESIAN_POINT('Ctrl Pts',(132.761153735035,-31.9894759506853,29.1751129979961));
#55130=CARTESIAN_POINT('Ctrl Pts',(132.849077222675,-32.0701164844653,29.1693040772775));
#55131=CARTESIAN_POINT('Ctrl Pts',(132.933542721414,-32.1546831901611,29.1634951565588));
#55132=CARTESIAN_POINT('Ctrl Pts',(133.014185812298,-32.242844057921,29.1576862358402));
#55133=CARTESIAN_POINT('Ctrl Pts',(133.094785419747,-32.3309573885969,29.1518804473406));
#55134=CARTESIAN_POINT('Ctrl Pts',(133.171566443781,-32.4226607263339,29.146074658841));
#55135=CARTESIAN_POINT('Ctrl Pts',(133.244201169967,-32.5175850933451,29.1402688703414));
#55136=CARTESIAN_POINT('Ctrl Pts',(133.316816237194,-32.6124837685916,29.1344646532081));
#55137=CARTESIAN_POINT('Ctrl Pts',(133.385286990192,-32.7106014156742,29.1286604360748));
#55138=CARTESIAN_POINT('Ctrl Pts',(133.449326269572,-32.8115363183187,29.1228562189416));
#55139=CARTESIAN_POINT('Ctrl Pts',(133.513363316744,-32.9124677026887,29.1170522041251));
#55140=CARTESIAN_POINT('Ctrl Pts',(133.572968978944,-33.0162158025678,29.1112481893086));
#55141=CARTESIAN_POINT('Ctrl Pts',(133.627900030336,-33.122350839511,29.1054441744922));
#55142=CARTESIAN_POINT('Ctrl Pts',(133.682842119548,-33.2285072031775,29.0996389934198));
#55143=CARTESIAN_POINT('Ctrl Pts',(133.733107542422,-33.3370510952233,29.0938338123474));
#55144=CARTESIAN_POINT('Ctrl Pts',(133.778499832327,-33.4475297049192,29.088028631275));
#55145=CARTESIAN_POINT('Ctrl Pts',(133.823939690213,-33.5581240885591,29.0822173667742));
#55146=CARTESIAN_POINT('Ctrl Pts',(133.864496060608,-33.6706568609073,29.0764061022734));
#55147=CARTESIAN_POINT('Ctrl Pts',(133.900021216767,-33.7846566292745,29.0705948377726));
#55148=CARTESIAN_POINT('Ctrl Pts',(133.935565762292,-33.8987186178653,29.064780401527));
#55149=CARTESIAN_POINT('Ctrl Pts',(133.966073518727,-34.0142488030906,29.0589659652814));
#55150=CARTESIAN_POINT('Ctrl Pts',(133.991447529178,-34.1307637709937,29.0531515290358));
#55151=CARTESIAN_POINT('Ctrl Pts',(134.016861604858,-34.2474627144958,29.047327911872));
#55152=CARTESIAN_POINT('Ctrl Pts',(134.037125670834,-34.3651491448337,29.0415042947082));
#55153=CARTESIAN_POINT('Ctrl Pts',(134.052194385697,-34.4833321564844,29.0356806775443));
#55154=CARTESIAN_POINT('Ctrl Pts',(134.064126355323,-34.5769138665417,29.0310693205879));
#55155=CARTESIAN_POINT('Ctrl Pts',(134.07280183418,-34.6708067628457,29.0264579636314));
#55156=CARTESIAN_POINT('Ctrl Pts',(134.078221500643,-34.7647673668643,29.021846606675));
#55157=CARTESIAN_POINT('Ctrl Pts',(134.085065206428,-34.8834165002981,29.016023596994));
#55158=CARTESIAN_POINT('Ctrl Pts',(134.086737820478,-35.0025562582525,29.0102005873129));
#55159=CARTESIAN_POINT('Ctrl Pts',(134.08318679581,-35.1216987695917,29.0043775776319));
#55160=CARTESIAN_POINT('Ctrl Pts',(134.079640256487,-35.2406907904865,28.9985619230695));
#55161=CARTESIAN_POINT('Ctrl Pts',(134.070883213792,-35.3596851532059,28.9927462685072));
#55162=CARTESIAN_POINT('Ctrl Pts',(134.056914981161,-35.4781901668116,28.9869306139449));
#55163=CARTESIAN_POINT('Ctrl Pts',(134.042960749089,-35.5965764011404,28.9811207884966));
#55164=CARTESIAN_POINT('Ctrl Pts',(134.02380576557,-35.7144738588157,28.9753109630483));
#55165=CARTESIAN_POINT('Ctrl Pts',(133.999501353679,-35.8313927603236,28.9695011376001));
#55166=CARTESIAN_POINT('Ctrl Pts',(133.97427344178,-35.9527542546836,28.9634705549545));
#55167=CARTESIAN_POINT('Ctrl Pts',(133.943497026151,-36.0730609050317,28.957439972309));
#55168=CARTESIAN_POINT('Ctrl Pts',(133.90728848545,-36.1917724998812,28.9514093896634));
#55169=CARTESIAN_POINT('Ctrl Pts',(133.872444754176,-36.3060094956231,28.94560611792));
#55170=CARTESIAN_POINT('Ctrl Pts',(133.8325711213,-36.418769078161,28.9398028461766));
#55171=CARTESIAN_POINT('Ctrl Pts',(133.787822782052,-36.5295828097124,28.9339995744332));
#55172=CARTESIAN_POINT('Ctrl Pts',(133.743081084127,-36.6403800948486,28.9281971639822));
#55173=CARTESIAN_POINT('Ctrl Pts',(133.693466271488,-36.7492317246963,28.9223947535311));
#55174=CARTESIAN_POINT('Ctrl Pts',(133.639182145788,-36.8556880960374,28.9165923430801));
#55175=CARTESIAN_POINT('Ctrl Pts',(133.584893258051,-36.9621538061911,28.9107894236165));
#55176=CARTESIAN_POINT('Ctrl Pts',(133.525934428401,-37.0662234761904,28.9049865041529));
#55177=CARTESIAN_POINT('Ctrl Pts',(133.462555685773,-37.1674715967975,28.8991835846894));
#55178=CARTESIAN_POINT('Ctrl Pts',(133.399156417163,-37.2687525078477,28.8933787858793));
#55179=CARTESIAN_POINT('Ctrl Pts',(133.331334605376,-37.3672097061665,28.8875739870693));
#55180=CARTESIAN_POINT('Ctrl Pts',(133.259383545455,-37.4624467311234,28.8817691882592));
#55181=CARTESIAN_POINT('Ctrl Pts',(133.187352808312,-37.5577892197313,28.8759579613266));
#55182=CARTESIAN_POINT('Ctrl Pts',(133.111183941995,-37.649904090949,28.8701467343939));
#55183=CARTESIAN_POINT('Ctrl Pts',(133.0312105605,-37.7384279318461,28.8643355074612));
#55184=CARTESIAN_POINT('Ctrl Pts',(132.951184663269,-37.8270099032683,28.8585204644981));
#55185=CARTESIAN_POINT('Ctrl Pts',(132.867349561646,-37.911995858073,28.8527054215349));
#55186=CARTESIAN_POINT('Ctrl Pts',(132.780074549519,-37.9930603901556,28.8468903785718));
#55187=CARTESIAN_POINT('Ctrl Pts',(132.692674467523,-38.074241092149,28.8410670023339));
#55188=CARTESIAN_POINT('Ctrl Pts',(132.601824945918,-38.1514888913627,28.835243626096));
#55189=CARTESIAN_POINT('Ctrl Pts',(132.507927128268,-38.2245195796111,28.829420249858));
#55190=CARTESIAN_POINT('Ctrl Pts',(132.482917837064,-38.2439709981313,28.8278692179409));
#55191=CARTESIAN_POINT('Ctrl Pts',(132.457692449597,-38.2631234984578,28.8263181860237));
#55192=CARTESIAN_POINT('Ctrl Pts',(132.432258858119,-38.2819722495937,28.8247671541066));
#55193=CARTESIAN_POINT('Ctrl Pts',(132.336762581187,-38.3527442268744,28.8189434475485));
#55194=CARTESIAN_POINT('Ctrl Pts',(132.238020885238,-38.4194588244185,28.8131197409904));
#55195=CARTESIAN_POINT('Ctrl Pts',(132.136413161883,-38.481804675988,28.8072960344323));
#55196=CARTESIAN_POINT('Ctrl Pts',(132.03493362094,-38.5440718756469,28.8014796747247));
#55197=CARTESIAN_POINT('Ctrl Pts',(131.93059558893,-38.6019810796357,28.7956633150171));
#55198=CARTESIAN_POINT('Ctrl Pts',(131.823810069726,-38.6552622107813,28.7898469553094));
#55199=CARTESIAN_POINT('Ctrl Pts',(131.717131435195,-38.708490011323,28.7840364173621));
#55200=CARTESIAN_POINT('Ctrl Pts',(131.608010550233,-38.7570987733044,28.7782258794148));
#55201=CARTESIAN_POINT('Ctrl Pts',(131.496885319749,-38.8008629729996,28.7724153414675));
#55202=CARTESIAN_POINT('Ctrl Pts',(131.381556838905,-38.846282529335,28.7663850231371));
#55203=CARTESIAN_POINT('Ctrl Pts',(131.264069774235,-38.8864835671572,28.7603547048067));
#55204=CARTESIAN_POINT('Ctrl Pts',(131.144939615841,-38.9212674323589,28.7543243864763));
#55205=CARTESIAN_POINT('Ctrl Pts',(131.030280461001,-38.954745844877,28.7485203884586));
#55206=CARTESIAN_POINT('Ctrl Pts',(130.914099749006,-38.9832062498323,28.7427163904408));
#55207=CARTESIAN_POINT('Ctrl Pts',(130.796874454028,-39.006521696499,28.7369123924231));
#55208=CARTESIAN_POINT('Ctrl Pts',(130.67966647758,-39.0298336986083,28.7311092518715));
#55209=CARTESIAN_POINT('Ctrl Pts',(130.561414625417,-39.0480021744022,28.7253061113198));
#55210=CARTESIAN_POINT('Ctrl Pts',(130.442606757085,-39.0609511519572,28.7195029707682));
#55211=CARTESIAN_POINT('Ctrl Pts',(130.323788405549,-39.0739012720862,28.7136993181671));
#55212=CARTESIAN_POINT('Ctrl Pts',(130.204414346232,-39.0816309340465,28.707895665566));
#55213=CARTESIAN_POINT('Ctrl Pts',(130.084977622509,-39.084116036999,28.7020920129649));
#55214=CARTESIAN_POINT('Ctrl Pts',(129.965502176336,-39.0866019456441,28.696286478768));
#55215=CARTESIAN_POINT('Ctrl Pts',(129.845964433371,-39.0838399052112,28.690480944571));
#55216=CARTESIAN_POINT('Ctrl Pts',(129.726856855235,-39.0758579247157,28.6846754103741));
#55217=CARTESIAN_POINT('Ctrl Pts',(129.607617403772,-39.0678671067446,28.6788634484156));
#55218=CARTESIAN_POINT('Ctrl Pts',(129.488809475458,-39.0546448398398,28.673051486457));
#55219=CARTESIAN_POINT('Ctrl Pts',(129.370919991094,-39.0362709698922,28.6672395244985));
#55220=CARTESIAN_POINT('Ctrl Pts',(129.252953089375,-39.0178850339287,28.6614237458575));
#55221=CARTESIAN_POINT('Ctrl Pts',(129.13590623215,-38.9943408378627,28.6556079672166));
#55222=CARTESIAN_POINT('Ctrl Pts',(129.020254110698,-38.9657689030496,28.6497921885756));
#55223=CARTESIAN_POINT('Ctrl Pts',(128.904436366872,-38.937156051117,28.6439680813105));
#55224=CARTESIAN_POINT('Ctrl Pts',(128.790017735786,-38.9035012042496,28.6381439740453));
#55225=CARTESIAN_POINT('Ctrl Pts',(128.677455911146,-38.8649841051469,28.6323198667801));
#55226=CARTESIAN_POINT('Ctrl Pts',(128.647614143248,-38.8547726650319,28.6307758116994));
#55227=CARTESIAN_POINT('Ctrl Pts',(128.617902761471,-38.844219735367,28.6292317566188));
#55228=CARTESIAN_POINT('Ctrl Pts',(128.588330019206,-38.8333292143154,28.6276877015381));
#55229=CARTESIAN_POINT('Ctrl Pts',(128.476791315952,-38.792253733897,28.6218640312169));
#55230=CARTESIAN_POINT('Ctrl Pts',(128.366867060462,-38.7462398208537,28.6160403608958));
#55231=CARTESIAN_POINT('Ctrl Pts',(128.259025634089,-38.6954341094438,28.6102166905746));
#55232=CARTESIAN_POINT('Ctrl Pts',(128.151320234839,-38.6446924824491,28.6044003660123));
#55233=CARTESIAN_POINT('Ctrl Pts',(128.045692805387,-38.5891712513471,28.5985840414501));
#55234=CARTESIAN_POINT('Ctrl Pts',(127.942594522375,-38.529066123019,28.5927677168878));
#55235=CARTESIAN_POINT('Ctrl Pts',(127.839599413955,-38.469021144306,28.5869572129551));
#55236=CARTESIAN_POINT('Ctrl Pts',(127.73912876755,-38.4044015986898,28.5811467090223));
#55237=CARTESIAN_POINT('Ctrl Pts',(127.641611242286,-38.3354501146752,28.5753362050896));
#55238=CARTESIAN_POINT('Ctrl Pts',(127.540404357014,-38.2638900036794,28.5693058735846));
#55239=CARTESIAN_POINT('Ctrl Pts',(127.442378860784,-38.1876638934963,28.5632755420796));
#55240=CARTESIAN_POINT('Ctrl Pts',(127.347983478252,-38.1070940391907,28.5572452105746));
#55241=CARTESIAN_POINT('Ctrl Pts',(127.257131475877,-38.029548587301,28.5514412434999));
#55242=CARTESIAN_POINT('Ctrl Pts',(127.169642306108,-37.9479799100945,28.5456372764253));
#55243=CARTESIAN_POINT('Ctrl Pts',(127.085883599613,-37.8627173463325,28.5398333093506));
#55244=CARTESIAN_POINT('Ctrl Pts',(127.002137250205,-37.7774673615257,28.5340301985467));
#55245=CARTESIAN_POINT('Ctrl Pts',(126.922120555643,-37.6885248651375,28.5282270877429));
#55246=CARTESIAN_POINT('Ctrl Pts',(126.846164475781,-37.5962562443202,28.522423976939));
#55247=CARTESIAN_POINT('Ctrl Pts',(126.770201677622,-37.5039794623669,28.5166203528514));
#55248=CARTESIAN_POINT('Ctrl Pts',(126.698300467788,-37.4083762863162,28.5108167287639));
#55249=CARTESIAN_POINT('Ctrl Pts',(126.630751263683,-37.3098458720934,28.5050131046763));
#55250=CARTESIAN_POINT('Ctrl Pts',(126.563180144589,-37.2112834916462,28.4992075977189));
#55251=CARTESIAN_POINT('Ctrl Pts',(126.499964069986,-37.1097923209244,28.4934020907615));
#55252=CARTESIAN_POINT('Ctrl Pts',(126.4413495547,-37.0057995932215,28.487596583804));
#55253=CARTESIAN_POINT('Ctrl Pts',(126.382670121785,-36.9016916899297,28.4817846470443));
#55254=CARTESIAN_POINT('Ctrl Pts',(126.328602621627,-36.7950770552998,28.4759727102845));
#55255=CARTESIAN_POINT('Ctrl Pts',(126.279347176525,-36.6864067027756,28.4701607735248));
#55256=CARTESIAN_POINT('Ctrl Pts',(126.230059375674,-36.5776649650346,28.4643450189218));
#55257=CARTESIAN_POINT('Ctrl Pts',(126.185590076881,-36.4668651981246,28.4585292643189));
#55258=CARTESIAN_POINT('Ctrl Pts',(126.146090314788,-36.3544759644327,28.4527135097159));
#55259=CARTESIAN_POINT('Ctrl Pts',(126.106533973011,-36.2419257437652,28.4468894245931));
#55260=CARTESIAN_POINT('Ctrl Pts',(126.071961493804,-36.1277819014283,28.4410653394703));
#55261=CARTESIAN_POINT('Ctrl Pts',(126.042473426805,-36.0125257638479,28.4352412543474));
#55262=CARTESIAN_POINT('Ctrl Pts',(126.034654266078,-35.981964036471,28.4336969192215));
#55263=CARTESIAN_POINT('Ctrl Pts',(126.027192317697,-35.9513241416612,28.4321525840956));
#55264=CARTESIAN_POINT('Ctrl Pts',(126.020088846053,-35.920615124081,28.4306082489697));
#55265=CARTESIAN_POINT('Ctrl Pts',(125.984344514774,-35.766088808985,28.4228372281072));
#55266=CARTESIAN_POINT('Ctrl Pts',(125.957588053208,-35.6094121628919,28.4150662072447));
#55267=CARTESIAN_POINT('Ctrl Pts',(125.940025230487,-35.4514752162833,28.4072951863823));
#55268=CARTESIAN_POINT('Ctrl Pts',(125.923519238621,-35.3030420175071,28.3999917813897));
#55269=CARTESIAN_POINT('Ctrl Pts',(125.915133455172,-35.1534953906131,28.3926883763971));
#55270=CARTESIAN_POINT('Ctrl Pts',(125.915001580775,-35.0035937341642,28.3853849714045));
#55271=CARTESIAN_POINT('Ctrl Pts',(125.915001580774,-35.0035937335827,28.3853849713762));
#55272=CARTESIAN_POINT('Ctrl Pts',(125.914898004666,-34.885858729381,28.3796487678021));
#55273=CARTESIAN_POINT('Ctrl Pts',(125.919888554375,-34.7679814543618,28.373912564228));
#55274=CARTESIAN_POINT('Ctrl Pts',(125.92998336164,-34.6504437620797,28.3681763606539));
#55275=CARTESIAN_POINT('Ctrl Pts',(125.940070875455,-34.5329909902111,28.3624443014591));
#55276=CARTESIAN_POINT('Ctrl Pts',(125.955255277809,-34.4158777301303,28.3567122422643));
#55277=CARTESIAN_POINT('Ctrl Pts',(125.975494633281,-34.2995847280028,28.3509801830696));
#55278=CARTESIAN_POINT('Ctrl Pts',(125.995726326249,-34.183335753736,28.3452502939994));
#55279=CARTESIAN_POINT('Ctrl Pts',(126.021009097467,-34.067906833477,28.3395204049292));
#55280=CARTESIAN_POINT('Ctrl Pts',(126.051249361176,-33.9537718258485,28.333790515859));
#55281=CARTESIAN_POINT('Ctrl Pts',(126.081485763923,-33.8396513905425,28.3280613583592));
#55282=CARTESIAN_POINT('Ctrl Pts',(126.116678293246,-33.7268249453335,28.3223322008594));
#55283=CARTESIAN_POINT('Ctrl Pts',(126.156682813441,-33.6157536333813,28.3166030433596));
#55284=CARTESIAN_POINT('Ctrl Pts',(126.196692264234,-33.5046686317747,28.3108731797352));
#55285=CARTESIAN_POINT('Ctrl Pts',(126.241514741578,-33.3953395882188,28.3051433161108));
#55286=CARTESIAN_POINT('Ctrl Pts',(126.290957333967,-33.2882092705167,28.2994134524864));
#55287=CARTESIAN_POINT('Ctrl Pts',(126.340448483654,-33.1809737407183,28.2936779615944));
#55288=CARTESIAN_POINT('Ctrl Pts',(126.394568633237,-33.0759416309574,28.2879424707024));
#55289=CARTESIAN_POINT('Ctrl Pts',(126.453078068552,-32.9735326767475,28.2822069798104));
#55290=CARTESIAN_POINT('Ctrl Pts',(126.51161697166,-32.8710721451136,28.2764686002858));
#55291=CARTESIAN_POINT('Ctrl Pts',(126.574549337832,-32.7712377543844,28.2707302207612));
#55292=CARTESIAN_POINT('Ctrl Pts',(126.641592140703,-32.674420147445,28.2649918412366));
#55293=CARTESIAN_POINT('Ctrl Pts',(126.708740646782,-32.5774498927753,28.2592444142811));
#55294=CARTESIAN_POINT('Ctrl Pts',(126.780012279904,-32.4835062564679,28.2534969873256));
#55295=CARTESIAN_POINT('Ctrl Pts',(126.855083544856,-32.3929469721224,28.2477495603701));
#55296=CARTESIAN_POINT('Ctrl Pts',(126.916999410163,-32.3182571896145,28.2430093057138));
#55297=CARTESIAN_POINT('Ctrl Pts',(126.981499104198,-32.2458689813848,28.2382690510575));
#55298=CARTESIAN_POINT('Ctrl Pts',(127.048383341174,-32.1759631554559,28.2335287964012));
#55299=CARTESIAN_POINT('Ctrl Pts',(127.130553567039,-32.0900807747109,28.2277051851384));
#55300=CARTESIAN_POINT('Ctrl Pts',(127.216607747338,-32.0076492124992,28.2218815738755));
#55301=CARTESIAN_POINT('Ctrl Pts',(127.306224544795,-31.9290394341611,28.2160579626127));
#55302=CARTESIAN_POINT('Ctrl Pts',(127.395728279743,-31.8505288316373,28.210241698545));
#55303=CARTESIAN_POINT('Ctrl Pts',(127.488785387778,-31.7758306897397,28.2044254344774));
#55304=CARTESIAN_POINT('Ctrl Pts',(127.585036399288,-31.7052806178318,28.1986091704098));
#55305=CARTESIAN_POINT('Ctrl Pts',(127.681191065126,-31.6348011653795,28.1927987283263));
#55306=CARTESIAN_POINT('Ctrl Pts',(127.78053294687,-31.5684617627394,28.1869882862429));
#55307=CARTESIAN_POINT('Ctrl Pts',(127.882668534847,-31.5065586498879,28.1811778441594));
#55308=CARTESIAN_POINT('Ctrl Pts',(127.988669723925,-31.4423126441632,28.1751474899792));
#55309=CARTESIAN_POINT('Ctrl Pts',(128.097679931082,-31.3828456651534,28.1691171357989));
#55310=CARTESIAN_POINT('Ctrl Pts',(128.209224606699,-31.3284405914178,28.1630867816186));
#55311=CARTESIAN_POINT('Ctrl Pts',(128.316580554951,-31.2760785378433,28.1572828793908));
#55312=CARTESIAN_POINT('Ctrl Pts',(128.426283655175,-31.2284052702501,28.1514789771629));
#55313=CARTESIAN_POINT('Ctrl Pts',(128.53788523975,-31.185626469804,28.1456750749351));
#55314=CARTESIAN_POINT('Ctrl Pts',(128.649470340154,-31.1428539880237,28.1398720299757));
#55315=CARTESIAN_POINT('Ctrl Pts',(128.762952986069,-31.1049746818036,28.1340689850164));
#55316=CARTESIAN_POINT('Ctrl Pts',(128.877865170739,-31.0721458243769,28.128265940057));
#55317=CARTESIAN_POINT('Ctrl Pts',(128.992787501069,-31.0393140684723,28.1224623827437));
#55318=CARTESIAN_POINT('Ctrl Pts',(129.109139228453,-31.0115337601051,28.1166588254303));
#55319=CARTESIAN_POINT('Ctrl Pts',(129.226438476133,-30.988911922085,28.1108552681169));
#55320=CARTESIAN_POINT('Ctrl Pts',(129.343775762221,-30.9662827481377,28.1050498287958));
#55321=CARTESIAN_POINT('Ctrl Pts',(129.462060778949,-30.9488154486754,28.0992443894748));
#55322=CARTESIAN_POINT('Ctrl Pts',(129.58080342219,-30.9365655869509,28.0934389501537));
#55323=CARTESIAN_POINT('Ctrl Pts',(129.699677559264,-30.924302159912,28.0876270819757));
#55324=CARTESIAN_POINT('Ctrl Pts',(129.819009927986,-30.9172677453482,28.0818152137976));
#55325=CARTESIAN_POINT('Ctrl Pts',(129.938307130876,-30.9154658784753,28.0760033456196));
#55326=CARTESIAN_POINT('Ctrl Pts',(130.057682687685,-30.9136628281436,28.0701876602301));
#55327=CARTESIAN_POINT('Ctrl Pts',(130.177022625436,-30.917099158085,28.0643719748406));
#55328=CARTESIAN_POINT('Ctrl Pts',(130.29583704243,-30.9257263905911,28.0585562894511));
#55329=CARTESIAN_POINT('Ctrl Pts',(130.414821643643,-30.9343659803418,28.0527322739456));
#55330=CARTESIAN_POINT('Ctrl Pts',(130.533278817554,-30.9482112656903,28.0469082584401));
#55331=CARTESIAN_POINT('Ctrl Pts',(130.65072710339,-30.9671623840138,28.0410842429346));
#55332=CARTESIAN_POINT('Ctrl Pts',(130.681883210605,-30.9721896440553,28.0395392765673));
#55333=CARTESIAN_POINT('Ctrl Pts',(130.712968397176,-30.97757593192,28.0379943102001));
#55334=CARTESIAN_POINT('Ctrl Pts',(130.743973854237,-30.9833187947993,28.0364493438328));
#55335=CARTESIAN_POINT('Ctrl Pts',(130.860849615195,-31.0049666443311,28.030625558701));
#55336=CARTESIAN_POINT('Ctrl Pts',(130.976968212671,-31.0317548423152,28.0248017735693));
#55337=CARTESIAN_POINT('Ctrl Pts',(131.091843191745,-31.0636179752671,28.0189779884375));
#55338=CARTESIAN_POINT('Ctrl Pts',(131.206577816322,-31.0954421777747,28.013161318819));
#55339=CARTESIAN_POINT('Ctrl Pts',(131.320071454059,-31.1323288763398,28.0073446492004));
#55340=CARTESIAN_POINT('Ctrl Pts',(131.431846262191,-31.1741613623352,28.0015279795818));
#55341=CARTESIAN_POINT('Ctrl Pts',(131.543491559234,-31.2159453779204,27.9957180496144));
#55342=CARTESIAN_POINT('Ctrl Pts',(131.653421611136,-31.2626636304388,27.989908119647));
#55343=CARTESIAN_POINT('Ctrl Pts',(131.761173065759,-31.3141494289046,27.9840981896796));
#55344=CARTESIAN_POINT('Ctrl Pts',(131.868852414607,-31.3656007737898,27.9782921476365));
#55345=CARTESIAN_POINT('Ctrl Pts',(131.974355698478,-31.4218131443671,27.9724861055935));
#55346=CARTESIAN_POINT('Ctrl Pts',(132.07723916007,-31.4825716109819,27.9666800635504));
#55347=CARTESIAN_POINT('Ctrl Pts',(132.18007749739,-31.5433034291775,27.9608765680141));
#55348=CARTESIAN_POINT('Ctrl Pts',(132.2802979476,-31.6085771691,27.9550730724778));
#55349=CARTESIAN_POINT('Ctrl Pts',(132.377481582681,-31.6781321031665,27.9492695769414));
#55350=CARTESIAN_POINT('Ctrl Pts',(132.414488702198,-31.7046183295344,27.9470596302487));
#55351=CARTESIAN_POINT('Ctrl Pts',(132.451055745837,-31.7317248911822,27.944849683556));
#55352=CARTESIAN_POINT('Ctrl Pts',(132.487160670875,-31.7594357285724,27.9426397368634));
#55353=CARTESIAN_POINT('',(125.915001103444,-34.9969974781416,28.4896150285558));
#55354=CARTESIAN_POINT('Ctrl Pts',(125.915001103444,-34.9969974781416,28.4896150285558));
#55355=CARTESIAN_POINT('Ctrl Pts',(125.915102918969,-34.8584751532076,28.4828889790542));
#55356=CARTESIAN_POINT('Ctrl Pts',(125.922254614347,-34.7202367330429,28.4761629295526));
#55357=CARTESIAN_POINT('Ctrl Pts',(125.936346094775,-34.5829365293537,28.4694368800511));
#55358=CARTESIAN_POINT('Ctrl Pts',(125.950518210567,-34.4448506557737,28.4626723422266));
#55359=CARTESIAN_POINT('Ctrl Pts',(125.971709650854,-34.3077138835539,28.455907804402));
#55360=CARTESIAN_POINT('Ctrl Pts',(125.999759150207,-34.1721726365672,28.4491432665776));
#55361=CARTESIAN_POINT('Ctrl Pts',(126.027989112987,-34.0357593512738,28.4423352074174));
#55362=CARTESIAN_POINT('Ctrl Pts',(126.063165581529,-33.9009623006317,28.4355271482572));
#55363=CARTESIAN_POINT('Ctrl Pts',(126.105075852321,-33.7684193555327,28.428719089097));
#55364=CARTESIAN_POINT('Ctrl Pts',(126.116063679441,-33.7336699029727,28.4269341858821));
#55365=CARTESIAN_POINT('Ctrl Pts',(126.127514106913,-33.6990752710491,28.4251492826673));
#55366=CARTESIAN_POINT('Ctrl Pts',(126.139422767306,-33.6646467020292,28.4233643794524));
#55367=CARTESIAN_POINT('Ctrl Pts',(126.178277843269,-33.5523146159319,28.4175406723593));
#55368=CARTESIAN_POINT('Ctrl Pts',(126.222102456264,-33.4414987050422,28.4117169652662));
#55369=CARTESIAN_POINT('Ctrl Pts',(126.270759293661,-33.3326701723455,28.4058932581732));
#55370=CARTESIAN_POINT('Ctrl Pts',(126.319354748462,-33.2239789313076,28.4000768979255));
#55371=CARTESIAN_POINT('Ctrl Pts',(126.372770137565,-33.1172704512509,28.3942605376778));
#55372=CARTESIAN_POINT('Ctrl Pts',(126.430818743981,-33.0129997076801,28.3884441774302));
#55373=CARTESIAN_POINT('Ctrl Pts',(126.488809247939,-32.9088333315831,28.3826336389385));
#55374=CARTESIAN_POINT('Ctrl Pts',(126.551423545968,-32.8071001926032,28.3768231004468));
#55375=CARTESIAN_POINT('Ctrl Pts',(126.618427561826,-32.7082336843857,28.3710125619551));
#55376=CARTESIAN_POINT('Ctrl Pts',(126.687965958665,-32.6056276182515,28.3649822438272));
#55377=CARTESIAN_POINT('Ctrl Pts',(126.76223252318,-32.5061097304143,28.3589519256992));
#55378=CARTESIAN_POINT('Ctrl Pts',(126.840913973803,-32.4101350461686,28.3529216075712));
#55379=CARTESIAN_POINT('Ctrl Pts',(126.916642487152,-32.3177623191844,28.3471176090018));
#55380=CARTESIAN_POINT('Ctrl Pts',(126.996460192436,-32.2286719777861,28.3413136104324));
#55381=CARTESIAN_POINT('Ctrl Pts',(127.080045109383,-32.1432381203957,28.335509611863));
#55382=CARTESIAN_POINT('Ctrl Pts',(127.163617677759,-32.0578168847325,28.3297064707579));
#55383=CARTESIAN_POINT('Ctrl Pts',(127.25095606551,-31.9760513505808,28.3239033296529));
#55384=CARTESIAN_POINT('Ctrl Pts',(127.34170052331,-31.898279688265,28.3181001885478));
#55385=CARTESIAN_POINT('Ctrl Pts',(127.43245298811,-31.8205011636266,28.3122965353921));
#55386=CARTESIAN_POINT('Ctrl Pts',(127.526611810458,-31.7467174772185,28.3064928822365));
#55387=CARTESIAN_POINT('Ctrl Pts',(127.623783673822,-31.6772269154805,28.3006892290808));
#55388=CARTESIAN_POINT('Ctrl Pts',(127.720987041176,-31.6077138242792,28.2948836943288));
#55389=CARTESIAN_POINT('Ctrl Pts',(127.821205060333,-31.5424968632586,28.2890781595767));
#55390=CARTESIAN_POINT('Ctrl Pts',(127.924015471257,-31.4818309823975,28.2832726248247));
#55391=CARTESIAN_POINT('Ctrl Pts',(128.026939711592,-31.4210979336155,28.277460662313));
#55392=CARTESIAN_POINT('Ctrl Pts',(128.132461721069,-31.3649262306117,28.2716486998013));
#55393=CARTESIAN_POINT('Ctrl Pts',(128.240134543168,-31.3135249120806,28.2658367372897));
#55394=CARTESIAN_POINT('Ctrl Pts',(128.347878073381,-31.2620898386033,28.2600209580961));
#55395=CARTESIAN_POINT('Ctrl Pts',(128.457774854118,-31.2154315476308,28.2542051789026));
#55396=CARTESIAN_POINT('Ctrl Pts',(128.569359408562,-31.1737103483754,28.248389399709));
#55397=CARTESIAN_POINT('Ctrl Pts',(128.681103760212,-31.1319294013248,28.2425652918962));
#55398=CARTESIAN_POINT('Ctrl Pts',(128.794540322816,-31.0950997835242,28.2367411840834));
#55399=CARTESIAN_POINT('Ctrl Pts',(128.909189855554,-31.0633315825721,28.2309170762706));
#55400=CARTESIAN_POINT('Ctrl Pts',(128.93958499817,-31.0549094025986,28.229373026475));
#55401=CARTESIAN_POINT('Ctrl Pts',(128.970065349101,-31.0468426848124,28.2278289766795));
#55402=CARTESIAN_POINT('Ctrl Pts',(129.000621895564,-31.0391328721638,28.226284926884));
#55403=CARTESIAN_POINT('Ctrl Pts',(129.115878571649,-31.0100521191993,28.2204609033032));
#55404=CARTESIAN_POINT('Ctrl Pts',(129.232591436126,-30.9859594149578,28.2146368797225));
#55405=CARTESIAN_POINT('Ctrl Pts',(129.35029103599,-30.9669982318272,28.2088128561417));
#55406=CARTESIAN_POINT('Ctrl Pts',(129.467840464957,-30.9480612409445,28.2029962633326));
#55407=CARTESIAN_POINT('Ctrl Pts',(129.586373725437,-30.9342428125389,28.1971796705235));
#55408=CARTESIAN_POINT('Ctrl Pts',(129.705407873483,-30.9256361872074,28.1913630777144));
#55409=CARTESIAN_POINT('Ctrl Pts',(129.8285360694,-30.9167335465165,28.1853464296288));
#55410=CARTESIAN_POINT('Ctrl Pts',(129.952199807902,-30.9134078017856,28.1793297815431));
#55411=CARTESIAN_POINT('Ctrl Pts',(130.075854079365,-30.9157043252669,28.1733131334575));
#55412=CARTESIAN_POINT('Ctrl Pts',(130.195179551404,-30.9179204537128,28.1675071118425));
#55413=CARTESIAN_POINT('Ctrl Pts',(130.314495759763,-30.9253718175763,28.1617010902274));
#55414=CARTESIAN_POINT('Ctrl Pts',(130.433309752101,-30.9380463248907,28.1558950686124));
#55415=CARTESIAN_POINT('Ctrl Pts',(130.552075627358,-30.9507156993055,28.1500913983097));
#55416=CARTESIAN_POINT('Ctrl Pts',(130.670339285781,-30.9686039668099,28.1442877280071));
#55417=CARTESIAN_POINT('Ctrl Pts',(130.787611406211,-30.9916470623451,28.1384840577044));
#55418=CARTESIAN_POINT('Ctrl Pts',(130.904863707988,-31.0146862636632,28.1326813682054));
#55419=CARTESIAN_POINT('Ctrl Pts',(131.021124404848,-31.0428784805336,28.1268786787064));
#55420=CARTESIAN_POINT('Ctrl Pts',(131.135913532358,-31.0761083798088,28.1210759892074));
#55421=CARTESIAN_POINT('Ctrl Pts',(131.250710348146,-31.1093405047367,28.1152729110592));
#55422=CARTESIAN_POINT('Ctrl Pts',(131.364035006966,-31.1476108680104,28.1094698329111));
#55423=CARTESIAN_POINT('Ctrl Pts',(131.475422509601,-31.1907542192498,28.1036667547629));
#55424=CARTESIAN_POINT('Ctrl Pts',(131.586890966057,-31.2339289260635,28.0978594590739));
#55425=CARTESIAN_POINT('Ctrl Pts',(131.696419074474,-31.2819835439919,28.0920521633849));
#55426=CARTESIAN_POINT('Ctrl Pts',(131.803561658364,-31.3347046033805,28.0862448676959));
#55427=CARTESIAN_POINT('Ctrl Pts',(131.910750990177,-31.3874486657615,28.0804350381962));
#55428=CARTESIAN_POINT('Ctrl Pts',(132.01555236519,-31.4448630314251,28.0746252086966));
#55429=CARTESIAN_POINT('Ctrl Pts',(132.117546319305,-31.5066888793585,28.068815379197));
#55430=CARTESIAN_POINT('Ctrl Pts',(132.219653698128,-31.5685834821392,28.0629990887437));
#55431=CARTESIAN_POINT('Ctrl Pts',(132.318947084202,-31.6348991349368,28.0571827982904));
#55432=CARTESIAN_POINT('Ctrl Pts',(132.415037034438,-31.7053344445462,28.0513665078371));
#55433=CARTESIAN_POINT('Ctrl Pts',(132.439284019921,-31.7231078321418,28.0498988464445));
#55434=CARTESIAN_POINT('Ctrl Pts',(132.463327200408,-31.7411433370532,28.0484311850518));
#55435=CARTESIAN_POINT('Ctrl Pts',(132.487160670875,-31.7594357285724,28.0469635236591));
#55436=CARTESIAN_POINT('Ctrl Pts',(132.487160670875,-31.7594357285724,29.296931249476));
#55437=CARTESIAN_POINT('Ctrl Pts',(132.582108041547,-31.832308644015,29.2911177031239));
#55438=CARTESIAN_POINT('Ctrl Pts',(132.673828569789,-31.9093414008505,29.2853041567717));
#55439=CARTESIAN_POINT('Ctrl Pts',(132.761950782513,-31.9902071707547,29.2794906104196));
#55440=CARTESIAN_POINT('Ctrl Pts',(132.850165037886,-32.0711574040362,29.2736709918844));
#55441=CARTESIAN_POINT('Ctrl Pts',(132.934773170299,-32.155948371588,29.2678513733491));
#55442=CARTESIAN_POINT('Ctrl Pts',(133.015439862989,-32.2442156411106,29.2620317548139));
#55443=CARTESIAN_POINT('Ctrl Pts',(133.096149402472,-32.3325297945371,29.2562090451393));
#55444=CARTESIAN_POINT('Ctrl Pts',(133.172913069843,-32.4243236169473,29.2503863354646));
#55445=CARTESIAN_POINT('Ctrl Pts',(133.245436340838,-32.5192001375429,29.24456362579));
#55446=CARTESIAN_POINT('Ctrl Pts',(133.318076046915,-32.6142289810455,29.2387315678376));
#55447=CARTESIAN_POINT('Ctrl Pts',(133.386461520609,-32.7123500779307,29.2328995098852));
#55448=CARTESIAN_POINT('Ctrl Pts',(133.450341687516,-32.8131375810553,29.2270674519329));
#55449=CARTESIAN_POINT('Ctrl Pts',(133.506514718584,-32.901765081867,29.2219390311973));
#55450=CARTESIAN_POINT('Ctrl Pts',(133.55920458717,-32.9924538395889,29.2168106104618));
#55451=CARTESIAN_POINT('Ctrl Pts',(133.608270882691,-33.0849004628673,29.2116821897262));
#55452=CARTESIAN_POINT('Ctrl Pts',(133.663940960201,-33.1897893816007,29.2058635401457));
#55453=CARTESIAN_POINT('Ctrl Pts',(133.715124976196,-33.2972796915462,29.2000448905651));
#55454=CARTESIAN_POINT('Ctrl Pts',(133.761571407974,-33.4069508661956,29.1942262409846));
#55455=CARTESIAN_POINT('Ctrl Pts',(133.807958699009,-33.516482395355,29.1884150003534));
#55456=CARTESIAN_POINT('Ctrl Pts',(133.849620245492,-33.6281888928937,29.1826037597221));
#55457=CARTESIAN_POINT('Ctrl Pts',(133.886350021045,-33.7416246530066,29.1767925190909));
#55458=CARTESIAN_POINT('Ctrl Pts',(133.923042649375,-33.8549456881204,29.1709871557472));
#55459=CARTESIAN_POINT('Ctrl Pts',(133.954813303684,-33.9699921197517,29.1651817924034));
#55460=CARTESIAN_POINT('Ctrl Pts',(133.981503992919,-34.086298213656,29.1593764290597));
#55461=CARTESIAN_POINT('Ctrl Pts',(134.009237755298,-34.2071495541052,29.1533441918971));
#55462=CARTESIAN_POINT('Ctrl Pts',(134.031486234473,-34.3293606044579,29.1473119547345));
#55463=CARTESIAN_POINT('Ctrl Pts',(134.048129117943,-34.452390974814,29.141279717572));
#55464=CARTESIAN_POINT('Ctrl Pts',(134.064127723253,-34.5706586019449,29.135480999959));
#55465=CARTESIAN_POINT('Ctrl Pts',(134.07494660272,-34.68968285133,29.1296822823461));
#55466=CARTESIAN_POINT('Ctrl Pts',(134.080531097806,-34.8089739289099,29.1238835647332));
#55467=CARTESIAN_POINT('Ctrl Pts',(134.086114738203,-34.9282467493494,29.1180857345965));
#55468=CARTESIAN_POINT('Ctrl Pts',(134.086465568167,-35.0477859081848,29.1122879044598));
#55469=CARTESIAN_POINT('Ctrl Pts',(134.081580958514,-35.1670984114157,29.1064900743232));
#55470=CARTESIAN_POINT('Ctrl Pts',(134.076695937982,-35.2864209508477,29.1006917564909));
#55471=CARTESIAN_POINT('Ctrl Pts',(134.066574619032,-35.4055163879374,29.0948934386586));
#55472=CARTESIAN_POINT('Ctrl Pts',(134.051266437924,-35.5238943108626,29.0890951208262));
#55473=CARTESIAN_POINT('Ctrl Pts',(134.035953338598,-35.6423102662757,29.083294940109));
#55474=CARTESIAN_POINT('Ctrl Pts',(134.015450115566,-35.7600078435198,29.0774947593917));
#55475=CARTESIAN_POINT('Ctrl Pts',(133.989857648217,-35.8765049611768,29.0716945786744));
#55476=CARTESIAN_POINT('Ctrl Pts',(133.964236823605,-35.993131161322,29.0658879711735));
#55477=CARTESIAN_POINT('Ctrl Pts',(133.933515586623,-36.108553846956,29.0600813636727));
#55478=CARTESIAN_POINT('Ctrl Pts',(133.897845249922,-36.2223041387726,29.0542747561719));
#55479=CARTESIAN_POINT('Ctrl Pts',(133.862151509636,-36.3361290630372,29.0484643389108));
#55480=CARTESIAN_POINT('Ctrl Pts',(133.821502342285,-36.4482790245809,29.0426539216498));
#55481=CARTESIAN_POINT('Ctrl Pts',(133.776097343868,-36.5583047999775,29.0368435043888));
#55482=CARTESIAN_POINT('Ctrl Pts',(133.730627022299,-36.6684888669866,29.0310247278109));
#55483=CARTESIAN_POINT('Ctrl Pts',(133.680387385259,-36.776542278605,29.0252059512331));
#55484=CARTESIAN_POINT('Ctrl Pts',(133.625624161131,-36.8820399682843,29.0193871746552));
#55485=CARTESIAN_POINT('Ctrl Pts',(133.610614635819,-36.9109548152251,29.0177923621561));
#55486=CARTESIAN_POINT('Ctrl Pts',(133.595265549603,-36.9396778439786,29.0161975496569));
#55487=CARTESIAN_POINT('Ctrl Pts',(133.579582519736,-36.9682006971849,29.0146027371578));
#55488=CARTESIAN_POINT('Ctrl Pts',(133.522308753151,-37.0723649594993,29.0087785488726));
#55489=CARTESIAN_POINT('Ctrl Pts',(133.460392236228,-37.1741950094874,29.0029543605875));
#55490=CARTESIAN_POINT('Ctrl Pts',(133.394047946116,-37.2732495550351,28.9971301723023));
#55491=CARTESIAN_POINT('Ctrl Pts',(133.327787374183,-37.3721791061615,28.9913133334128));
#55492=CARTESIAN_POINT('Ctrl Pts',(133.25711036729,-37.4683397827467,28.9854964945232));
#55493=CARTESIAN_POINT('Ctrl Pts',(133.182277855087,-37.5613146337429,28.9796796556337));
#55494=CARTESIAN_POINT('Ctrl Pts',(133.107520279024,-37.6541963811351,28.9738686416383));
#55495=CARTESIAN_POINT('Ctrl Pts',(133.028615730497,-37.7438983333498,28.9680576276429));
#55496=CARTESIAN_POINT('Ctrl Pts',(132.945868171882,-37.8300328114511,28.9622466136476));
#55497=CARTESIAN_POINT('Ctrl Pts',(132.860000325613,-37.9194152929151,28.9562164749368));
#55498=CARTESIAN_POINT('Ctrl Pts',(132.769994184585,-38.0049555832903,28.950186336226));
#55499=CARTESIAN_POINT('Ctrl Pts',(132.676235306726,-38.0862581847653,28.9441561975153));
#55500=CARTESIAN_POINT('Ctrl Pts',(132.585985320004,-38.1645180666153,28.9383517345033));
#55501=CARTESIAN_POINT('Ctrl Pts',(132.492258774949,-38.2388514566586,28.9325472714912));
#55502=CARTESIAN_POINT('Ctrl Pts',(132.395436255544,-38.3089439622979,28.9267428084792));
#55503=CARTESIAN_POINT('Ctrl Pts',(132.298628121535,-38.3790260539491,28.9209392078648));
#55504=CARTESIAN_POINT('Ctrl Pts',(132.198725258541,-38.4448682749289,28.9151356072503));
#55505=CARTESIAN_POINT('Ctrl Pts',(132.09613941041,-38.5061980223776,28.9093320066359));
#55506=CARTESIAN_POINT('Ctrl Pts',(131.993544607804,-38.5675331231544,28.903527899439));
#55507=CARTESIAN_POINT('Ctrl Pts',(131.888266704849,-38.6243547577782,28.897723792242));
#55508=CARTESIAN_POINT('Ctrl Pts',(131.780743796715,-38.6764353020911,28.8919196850451));
#55509=CARTESIAN_POINT('Ctrl Pts',(131.673186142703,-38.7285326761596,28.8861137022589));
#55510=CARTESIAN_POINT('Ctrl Pts',(131.563382407934,-38.7758857350839,28.8803077194728));
#55511=CARTESIAN_POINT('Ctrl Pts',(131.45179189964,-38.818314455377,28.8745017366867));
#55512=CARTESIAN_POINT('Ctrl Pts',(131.34007806638,-38.8607900660422,28.8686893373815));
#55513=CARTESIAN_POINT('Ctrl Pts',(131.226573899806,-38.8983303298574,28.8628769380763));
#55514=CARTESIAN_POINT('Ctrl Pts',(131.111755298385,-38.9308046449186,28.8570645387711));
#55515=CARTESIAN_POINT('Ctrl Pts',(130.996861421357,-38.9633002502909,28.85124832883));
#55516=CARTESIAN_POINT('Ctrl Pts',(130.880651789694,-38.9907231989341,28.8454321188889));
#55517=CARTESIAN_POINT('Ctrl Pts',(130.763612332195,-39.0129940451139,28.8396159089478));
#55518=CARTESIAN_POINT('Ctrl Pts',(130.646405523634,-39.0352967356807,28.8337913825899));
#55519=CARTESIAN_POINT('Ctrl Pts',(130.528366923537,-39.0524325615092,28.827966856232));
#55520=CARTESIAN_POINT('Ctrl Pts',(130.409987550855,-39.0643739011247,28.8221423298741));
#55521=CARTESIAN_POINT('Ctrl Pts',(130.378694609615,-39.067530529095,28.8206026481125));
#55522=CARTESIAN_POINT('Ctrl Pts',(130.347377853411,-39.0703244591297,28.8190629663509));
#55523=CARTESIAN_POINT('Ctrl Pts',(130.316046331496,-39.0727557889405,28.8175232845893));
#55524=CARTESIAN_POINT('Ctrl Pts',(130.197522841049,-39.081953225834,28.8116988481941));
#55525=CARTESIAN_POINT('Ctrl Pts',(130.078407055875,-39.0859873249673,28.8058744117989));
#55526=CARTESIAN_POINT('Ctrl Pts',(129.959185970498,-39.0847961044581,28.8000499754037));
#55527=CARTESIAN_POINT('Ctrl Pts',(129.840114957166,-39.0836063834226,28.7942328706402));
#55528=CARTESIAN_POINT('Ctrl Pts',(129.720939311869,-39.0772044293515,28.7884157658766));
#55529=CARTESIAN_POINT('Ctrl Pts',(129.602150844744,-39.0655800385261,28.782598661113));
#55530=CARTESIAN_POINT('Ctrl Pts',(129.483480970749,-39.0539672529762,28.7767873638884));
#55531=CARTESIAN_POINT('Ctrl Pts',(129.365197909877,-39.0371424425923,28.7709760666639));
#55532=CARTESIAN_POINT('Ctrl Pts',(129.247792563708,-39.0151474409774,28.7651647694393));
#55533=CARTESIAN_POINT('Ctrl Pts',(129.125967987234,-38.9923245300647,28.7591347303802));
#55534=CARTESIAN_POINT('Ctrl Pts',(129.005088947621,-38.9639345635799,28.7531046913211));
#55535=CARTESIAN_POINT('Ctrl Pts',(128.885697490909,-38.9300833220473,28.747074652262));
#55536=CARTESIAN_POINT('Ctrl Pts',(128.770765880917,-38.8974965876467,28.741269864244));
#55537=CARTESIAN_POINT('Ctrl Pts',(128.657213137834,-38.8598493924904,28.735465076226));
#55538=CARTESIAN_POINT('Ctrl Pts',(128.54551084419,-38.8172878193335,28.7296602882079));
#55539=CARTESIAN_POINT('Ctrl Pts',(128.433824858422,-38.7747324599148,28.7238563476546));
#55540=CARTESIAN_POINT('Ctrl Pts',(128.323989166181,-38.7272642946276,28.7180524071013));
#55541=CARTESIAN_POINT('Ctrl Pts',(128.216457466505,-38.6750783707582,28.7122484665481));
#55542=CARTESIAN_POINT('Ctrl Pts',(128.108916110165,-38.6228877604385,28.7064440047837));
#55543=CARTESIAN_POINT('Ctrl Pts',(128.003679525028,-38.5659787273951,28.7006395430194));
#55544=CARTESIAN_POINT('Ctrl Pts',(127.90117822477,-38.5045930085844,28.6948350812551));
#55545=CARTESIAN_POINT('Ctrl Pts',(127.798643550248,-38.4431873026791,28.6890287295671));
#55546=CARTESIAN_POINT('Ctrl Pts',(127.698846281852,-38.3773022217518,28.683222377879));
#55547=CARTESIAN_POINT('Ctrl Pts',(127.602188739063,-38.3072233303669,28.677416026191));
#55548=CARTESIAN_POINT('Ctrl Pts',(127.505424056115,-38.2370667599581,28.6716032384461));
#55549=CARTESIAN_POINT('Ctrl Pts',(127.411806376296,-38.1627073397506,28.6657904507012));
#55550=CARTESIAN_POINT('Ctrl Pts',(127.321705771227,-38.0844715956094,28.6599776629563));
#55551=CARTESIAN_POINT('Ctrl Pts',(127.231545916034,-38.0061844036722,28.6541610527243));
#55552=CARTESIAN_POINT('Ctrl Pts',(127.144908037172,-37.9240160914809,28.6483444424924));
#55553=CARTESIAN_POINT('Ctrl Pts',(127.062124911162,-37.8383296077776,28.6425278322604));
#55554=CARTESIAN_POINT('Ctrl Pts',(126.979223219008,-37.7525203995956,28.6367028911876));
#55555=CARTESIAN_POINT('Ctrl Pts',(126.900187568794,-37.6631832671508,28.6308779501148));
#55556=CARTESIAN_POINT('Ctrl Pts',(126.825310176905,-37.5707138166536,28.625053009042));
#55557=CARTESIAN_POINT('Ctrl Pts',(126.805560440396,-37.5463239809995,28.6235166167016));
#55558=CARTESIAN_POINT('Ctrl Pts',(126.786099756637,-37.5217163825431,28.6219802243613));
#55559=CARTESIAN_POINT('Ctrl Pts',(126.766932971494,-37.4968985940935,28.6204438320209));
#55560=CARTESIAN_POINT('Ctrl Pts',(126.694299748913,-37.4028506909643,28.6146216179148));
#55561=CARTESIAN_POINT('Ctrl Pts',(126.625652077838,-37.3054735001323,28.6087994038087));
#55562=CARTESIAN_POINT('Ctrl Pts',(126.561310097123,-37.2051387148773,28.6029771897026));
#55563=CARTESIAN_POINT('Ctrl Pts',(126.497047713044,-37.1049280524929,28.5971621781826));
#55564=CARTESIAN_POINT('Ctrl Pts',(126.437080646904,-37.0017674101151,28.5913471666625));
#55565=CARTESIAN_POINT('Ctrl Pts',(126.381688651695,-36.8960611769474,28.5855321551425));
#55566=CARTESIAN_POINT('Ctrl Pts',(126.326352129164,-36.790460803983,28.5797229671041));
#55567=CARTESIAN_POINT('Ctrl Pts',(126.27558175395,-36.6823202689564,28.5739137790656));
#55568=CARTESIAN_POINT('Ctrl Pts',(126.229613473537,-36.5720720215907,28.5681045910272));
#55569=CARTESIAN_POINT('Ctrl Pts',(126.183680399074,-36.461908210584,28.5622998520997));
#55570=CARTESIAN_POINT('Ctrl Pts',(126.142542259572,-36.3496402734931,28.5564951131722));
#55571=CARTESIAN_POINT('Ctrl Pts',(126.106388325008,-36.2357237249349,28.5506903742447));
#55572=CARTESIAN_POINT('Ctrl Pts',(126.070251484944,-36.1218610390188,28.5448883799455));
#55573=CARTESIAN_POINT('Ctrl Pts',(126.039094285826,-36.0063516800894,28.5390863856462));
#55574=CARTESIAN_POINT('Ctrl Pts',(126.01305705638,-35.8896690195346,28.533284391347));
#55575=CARTESIAN_POINT('Ctrl Pts',(125.987027133808,-35.7730191038418,28.5274840252717));
#55576=CARTESIAN_POINT('Ctrl Pts',(125.966114408067,-35.655196940161,28.5216836591964));
#55577=CARTESIAN_POINT('Ctrl Pts',(125.950408564446,-35.5366881823662,28.5158832931211));
#55578=CARTESIAN_POINT('Ctrl Pts',(125.934700135524,-35.418159917126,28.5100819722613));
#55579=CARTESIAN_POINT('Ctrl Pts',(125.92420035633,-35.2989452362512,28.5042806514015));
#55580=CARTESIAN_POINT('Ctrl Pts',(125.918947247676,-35.179536717001,28.4984793305417));
#55581=CARTESIAN_POINT('Ctrl Pts',(125.916271699447,-35.1187187759861,28.4955245632263));
#55582=CARTESIAN_POINT('Ctrl Pts',(125.914956375687,-35.0578506198813,28.4925697959109));
#55583=CARTESIAN_POINT('Ctrl Pts',(125.915001103444,-34.9969974789589,28.4896150285955));
#55584=CARTESIAN_POINT('Origin',(130.,-35.,17.));
#55585=CARTESIAN_POINT('Ctrl Pts',(133.378768828602,-35.2726284383002,17.));
#55586=CARTESIAN_POINT('Ctrl Pts',(133.398288246238,-35.1664583073869,17.0000000000001));
#55587=CARTESIAN_POINT('Ctrl Pts',(133.412279037496,-35.0595484327477,17.0000000000002));
#55588=CARTESIAN_POINT('Ctrl Pts',(133.420978754548,-34.9522469234893,17.0000000000001));
#55589=CARTESIAN_POINT('Ctrl Pts',(133.4296784716,-34.8449454142309,17.));
#55590=CARTESIAN_POINT('Ctrl Pts',(133.433086995943,-34.7372515853272,17.));
#55591=CARTESIAN_POINT('Ctrl Pts',(133.431392639095,-34.6294944550508,17.));
#55592=CARTESIAN_POINT('Ctrl Pts',(133.430532659945,-34.5748017936812,17.));
#55593=CARTESIAN_POINT('Ctrl Pts',(133.428357343707,-34.5200925845888,17.0000000000001));
#55594=CARTESIAN_POINT('Ctrl Pts',(133.424886608819,-34.465408836506,17.));
#55595=CARTESIAN_POINT('Ctrl Pts',(133.423593739603,-34.4450388178326,17.));
#55596=CARTESIAN_POINT('Ctrl Pts',(133.422121635848,-34.4246812381163,17.));
#55597=CARTESIAN_POINT('Ctrl Pts',(133.420471959324,-34.4043410098082,17.));
#55598=CARTESIAN_POINT('Ctrl Pts',(133.411386307087,-34.2923164776353,16.9999999999999));
#55599=CARTESIAN_POINT('Ctrl Pts',(133.396916955542,-34.1807930555395,17.0000000000002));
#55600=CARTESIAN_POINT('Ctrl Pts',(133.377281863082,-34.0701359071285,17.0000000000002));
#55601=CARTESIAN_POINT('Ctrl Pts',(133.360260736019,-33.9742102379531,17.0000000000002));
#55602=CARTESIAN_POINT('Ctrl Pts',(133.339356815858,-33.8789349316622,17.0000000000003));
#55603=CARTESIAN_POINT('Ctrl Pts',(133.314680668356,-33.7845430961811,17.0000000000002));
#55604=CARTESIAN_POINT('Ctrl Pts',(133.305738882743,-33.7503387473677,17.0000000000001));
#55605=CARTESIAN_POINT('Ctrl Pts',(133.296301499474,-33.7162503957036,16.9999999999999));
#55606=CARTESIAN_POINT('Ctrl Pts',(133.286372866255,-33.6822891544893,17.));
#55607=CARTESIAN_POINT('Ctrl Pts',(133.279074612109,-33.6573252179607,17.0000000000002));
#55608=CARTESIAN_POINT('Ctrl Pts',(133.271509097602,-33.6324245812173,17.));
#55609=CARTESIAN_POINT('Ctrl Pts',(133.263688075278,-33.6076228894364,17.));
#55610=CARTESIAN_POINT('Ctrl Pts',(133.229059460988,-33.4978101075652,17.));
#55611=CARTESIAN_POINT('Ctrl Pts',(133.189399626582,-33.3898390969386,17.0000000000001));
#55612=CARTESIAN_POINT('Ctrl Pts',(133.144933359838,-33.2840773063132,17.));
#55613=CARTESIAN_POINT('Ctrl Pts',(133.099802502295,-33.176734804779,17.));
#55614=CARTESIAN_POINT('Ctrl Pts',(133.049720392207,-33.0716671799564,16.9999999999999));
#55615=CARTESIAN_POINT('Ctrl Pts',(132.994868514162,-32.9692566318156,17.));
#55616=CARTESIAN_POINT('Ctrl Pts',(132.940479847808,-32.8677109175681,17.0000000000001));
#55617=CARTESIAN_POINT('Ctrl Pts',(132.881401361892,-32.768776718664,17.0000000000001));
#55618=CARTESIAN_POINT('Ctrl Pts',(132.817760633728,-32.6728378225391,17.0000000000001));
#55619=CARTESIAN_POINT('Ctrl Pts',(132.780118924681,-32.616092651352,17.0000000000001));
#55620=CARTESIAN_POINT('Ctrl Pts',(132.740880248093,-32.5603956288563,17.));
#55621=CARTESIAN_POINT('Ctrl Pts',(132.700063340168,-32.5058299364338,16.9999999999999));
#55622=CARTESIAN_POINT('Ctrl Pts',(132.678441129705,-32.476924491469,16.9999999999999));
#55623=CARTESIAN_POINT('Ctrl Pts',(132.65637594081,-32.4483365778201,17.0000000000002));
#55624=CARTESIAN_POINT('Ctrl Pts',(132.633869936992,-32.4200789995526,17.));
#55625=CARTESIAN_POINT('Ctrl Pts',(132.623920095448,-32.4075864029794,17.));
#55626=CARTESIAN_POINT('Ctrl Pts',(132.613884890735,-32.3951594678565,16.9999999999999));
#55627=CARTESIAN_POINT('Ctrl Pts',(132.603772440782,-32.3828086916134,16.9999999999999));
#55628=CARTESIAN_POINT('Ctrl Pts',(132.528293751701,-32.2906232761805,17.));
#55629=CARTESIAN_POINT('Ctrl Pts',(132.448401459479,-32.202535222033,17.0000000000001));
#55630=CARTESIAN_POINT('Ctrl Pts',(132.364286473895,-32.1189321572606,17.0000000000001));
#55631=CARTESIAN_POINT('Ctrl Pts',(132.340801349937,-32.095589962932,17.0000000000001));
#55632=CARTESIAN_POINT('Ctrl Pts',(132.316986747461,-32.0725974700126,16.9999999999999));
#55633=CARTESIAN_POINT('Ctrl Pts',(132.292846130803,-32.0499633408993,16.9999999999999));
#55634=CARTESIAN_POINT('Ctrl Pts',(132.208772055331,-31.9711358815073,16.9999999999999));
#55635=CARTESIAN_POINT('Ctrl Pts',(132.120747300731,-31.8966525443055,16.9999999999999));
#55636=CARTESIAN_POINT('Ctrl Pts',(132.029197860355,-31.8265245910536,16.9999999999999));
#55637=CARTESIAN_POINT('Ctrl Pts',(131.937648419978,-31.7563966378017,17.));
#55638=CARTESIAN_POINT('Ctrl Pts',(131.842573618672,-31.6906237914098,17.));
#55639=CARTESIAN_POINT('Ctrl Pts',(131.744359117884,-31.629251345085,17.));
#55640=CARTESIAN_POINT('Ctrl Pts',(131.6882846066,-31.5942114079436,17.));
#55641=CARTESIAN_POINT('Ctrl Pts',(131.63118595824,-31.5606065213418,17.));
#55642=CARTESIAN_POINT('Ctrl Pts',(131.573130353031,-31.528450628799,17.));
#55643=CARTESIAN_POINT('Ctrl Pts',(131.556946837447,-31.5194868881541,17.));
#55644=CARTESIAN_POINT('Ctrl Pts',(131.540688943071,-31.5106357689599,17.));
#55645=CARTESIAN_POINT('Ctrl Pts',(131.524358087669,-31.5018976324805,17.));
#55646=CARTESIAN_POINT('Ctrl Pts',(131.511363461925,-31.4949446094788,17.));
#55647=CARTESIAN_POINT('Ctrl Pts',(131.498323714352,-31.4880637401771,17.));
#55648=CARTESIAN_POINT('Ctrl Pts',(131.485248425713,-31.4812596596424,17.));
#55649=CARTESIAN_POINT('Ctrl Pts',(131.379202552098,-31.426075817483,17.0000000000001));
#55650=CARTESIAN_POINT('Ctrl Pts',(131.270666658491,-31.375856441141,17.));
#55651=CARTESIAN_POINT('Ctrl Pts',(131.160094992004,-31.3306020577967,17.));
#55652=CARTESIAN_POINT('Ctrl Pts',(131.047641736312,-31.2845775842305,17.0000000000001));
#55653=CARTESIAN_POINT('Ctrl Pts',(130.933082172006,-31.243688134086,17.));
#55654=CARTESIAN_POINT('Ctrl Pts',(130.816854357636,-31.2079719988663,17.));
#55655=CARTESIAN_POINT('Ctrl Pts',(130.69920023221,-31.1718175665076,17.));
#55656=CARTESIAN_POINT('Ctrl Pts',(130.579835885835,-31.1409637990667,17.));
#55657=CARTESIAN_POINT('Ctrl Pts',(130.459186272896,-31.1154946922679,17.));
#55658=CARTESIAN_POINT('Ctrl Pts',(130.384595675,-31.0997486334307,17.));
#55659=CARTESIAN_POINT('Ctrl Pts',(130.309513284361,-31.0860616069785,17.));
#55660=CARTESIAN_POINT('Ctrl Pts',(130.234036026462,-31.0744627946408,17.));
#55661=CARTESIAN_POINT('Ctrl Pts',(130.197795458841,-31.0688935999647,17.));
#55662=CARTESIAN_POINT('Ctrl Pts',(130.161463827202,-31.0638059443293,17.));
#55663=CARTESIAN_POINT('Ctrl Pts',(130.125051741993,-31.0592036806989,17.));
#55664=CARTESIAN_POINT('Ctrl Pts',(130.107528311351,-31.0569888268377,17.));
#55665=CARTESIAN_POINT('Ctrl Pts',(130.089984287133,-31.0548861776152,17.));
#55666=CARTESIAN_POINT('Ctrl Pts',(130.072427070294,-31.052896897432,17.));
#55667=CARTESIAN_POINT('Ctrl Pts',(129.946714827881,-31.0386533601501,17.));
#55668=CARTESIAN_POINT('Ctrl Pts',(129.820703894979,-31.0302595130221,17.));
#55669=CARTESIAN_POINT('Ctrl Pts',(129.69485817944,-31.0277503025434,17.));
#55670=CARTESIAN_POINT('Ctrl Pts',(129.568768654346,-31.0252362307988,17.));
#55671=CARTESIAN_POINT('Ctrl Pts',(129.442844100505,-31.02862930582,17.));
#55672=CARTESIAN_POINT('Ctrl Pts',(129.317528571408,-31.0380119206155,17.));
#55673=CARTESIAN_POINT('Ctrl Pts',(129.194473966571,-31.047225255661,17.));
#55674=CARTESIAN_POINT('Ctrl Pts',(129.072005730894,-31.0622138114403,17.));
#55675=CARTESIAN_POINT('Ctrl Pts',(128.950535741321,-31.0831042418908,17.));
#55676=CARTESIAN_POINT('Ctrl Pts',(128.859102153225,-31.0988290066634,17.));
#55677=CARTESIAN_POINT('Ctrl Pts',(128.768233909816,-31.1178987055077,17.));
#55678=CARTESIAN_POINT('Ctrl Pts',(128.678107868388,-31.1403868954586,17.));
#55679=CARTESIAN_POINT('Ctrl Pts',(128.630400840111,-31.1522907214436,17.));
#55680=CARTESIAN_POINT('Ctrl Pts',(128.582901820088,-31.1651527026015,17.));
#55681=CARTESIAN_POINT('Ctrl Pts',(128.535626875521,-31.178955003241,17.));
#55682=CARTESIAN_POINT('Ctrl Pts',(126.824949217806,-32.429732011932,17.));
#55683=CARTESIAN_POINT('Ctrl Pts',(126.754722564964,-32.5331868396527,17.0000000000001));
#55684=CARTESIAN_POINT('Ctrl Pts',(126.689770328881,-32.6399361026362,17.0000000000001));
#55685=CARTESIAN_POINT('Ctrl Pts',(126.630097033085,-32.7495483500992,17.0000000000001));
#55686=CARTESIAN_POINT('Ctrl Pts',(126.569576097871,-32.8607176032622,17.));
#55687=CARTESIAN_POINT('Ctrl Pts',(126.51448500206,-32.9748326342131,17.0000000000002));
#55688=CARTESIAN_POINT('Ctrl Pts',(126.464879563014,-33.0914584109723,17.0000000000001));
#55689=CARTESIAN_POINT('Ctrl Pts',(126.443235134053,-33.1423459424326,17.0000000000001));
#55690=CARTESIAN_POINT('Ctrl Pts',(126.422635756764,-33.1937115953365,17.0000000000003));
#55691=CARTESIAN_POINT('Ctrl Pts',(126.403089154084,-33.2455194506075,17.0000000000001));
#55692=CARTESIAN_POINT('Ctrl Pts',(126.392820709654,-33.2727357444875,16.9999999999999));
#55693=CARTESIAN_POINT('Ctrl Pts',(126.382841496993,-33.3000781943394,17.));
#55694=CARTESIAN_POINT('Ctrl Pts',(126.37316194691,-33.3275147827857,17.));
#55695=CARTESIAN_POINT('Ctrl Pts',(126.331490200439,-33.4456329337216,16.9999999999999));
#55696=CARTESIAN_POINT('Ctrl Pts',(126.295333265067,-33.5655832581459,17.0000000000001));
#55697=CARTESIAN_POINT('Ctrl Pts',(126.264731200303,-33.686937606849,17.0000000000001));
#55698=CARTESIAN_POINT('Ctrl Pts',(126.239067787757,-33.7887074298646,17.));
#55699=CARTESIAN_POINT('Ctrl Pts',(126.217311899518,-33.8914651743243,17.0000000000002));
#55700=CARTESIAN_POINT('Ctrl Pts',(126.199515422177,-33.9949584531853,17.0000000000001));
#55701=CARTESIAN_POINT('Ctrl Pts',(126.191672483203,-34.0405681238387,17.));
#55702=CARTESIAN_POINT('Ctrl Pts',(126.184598869754,-34.0863206118168,16.9999999999998));
#55703=CARTESIAN_POINT('Ctrl Pts',(126.178300615437,-34.1321940133029,17.));
#55704=CARTESIAN_POINT('Ctrl Pts',(126.175607336728,-34.1518105370754,17.0000000000001));
#55705=CARTESIAN_POINT('Ctrl Pts',(126.173055853477,-34.1714491679886,17.));
#55706=CARTESIAN_POINT('Ctrl Pts',(126.170646691963,-34.1911081767111,17.));
#55707=CARTESIAN_POINT('Ctrl Pts',(126.168408134718,-34.2093750368465,16.9999999999999));
#55708=CARTESIAN_POINT('Ctrl Pts',(126.166292933428,-34.2276559610749,17.0000000000003));
#55709=CARTESIAN_POINT('Ctrl Pts',(126.164302324029,-34.2459397516365,17.0000000000002));
#55710=CARTESIAN_POINT('Ctrl Pts',(126.151067617198,-34.3675008213213,17.0000000000001));
#55711=CARTESIAN_POINT('Ctrl Pts',(126.143320213443,-34.4893160661783,17.));
#55712=CARTESIAN_POINT('Ctrl Pts',(126.141093992317,-34.6109885614732,17.));
#55713=CARTESIAN_POINT('Ctrl Pts',(126.138877610836,-34.7321232781618,16.9999999999999));
#55714=CARTESIAN_POINT('Ctrl Pts',(126.14213377111,-34.8531173504601,17.));
#55715=CARTESIAN_POINT('Ctrl Pts',(126.150946782328,-34.973572328076,17.0000000000001));
#55716=CARTESIAN_POINT('Ctrl Pts',(126.159510425353,-35.0906189768731,17.0000000000001));
#55717=CARTESIAN_POINT('Ctrl Pts',(126.173321132798,-35.2071572701507,17.0000000000001));
#55718=CARTESIAN_POINT('Ctrl Pts',(126.192501970979,-35.322804279403,17.0000000000002));
#55719=CARTESIAN_POINT('Ctrl Pts',(126.204193875272,-35.3932982667441,17.0000000000002));
#55720=CARTESIAN_POINT('Ctrl Pts',(126.217882010487,-35.4634607028539,16.9999999999999));
#55721=CARTESIAN_POINT('Ctrl Pts',(126.233602445872,-35.5332000053698,16.9999999999999));
#55722=CARTESIAN_POINT('Ctrl Pts',(126.243155310077,-35.5755786081459,16.9999999999999));
#55723=CARTESIAN_POINT('Ctrl Pts',(126.253458751899,-35.6178008839807,17.));
#55724=CARTESIAN_POINT('Ctrl Pts',(126.264521983881,-35.6598454466932,16.9999999999999));
#55725=CARTESIAN_POINT('Ctrl Pts',(126.269462009858,-35.6786194570633,16.9999999999999));
#55726=CARTESIAN_POINT('Ctrl Pts',(126.274554024022,-35.6973594264633,17.));
#55727=CARTESIAN_POINT('Ctrl Pts',(126.279792975253,-35.7160432617782,17.));
#55728=CARTESIAN_POINT('Ctrl Pts',(126.311062580707,-35.8275610318175,16.9999999999999));
#55729=CARTESIAN_POINT('Ctrl Pts',(126.34760531646,-35.937246500656,16.9999999999999));
#55730=CARTESIAN_POINT('Ctrl Pts',(126.3894966474,-36.0447443535775,16.9999999999999));
#55731=CARTESIAN_POINT('Ctrl Pts',(126.402466834512,-36.0780273081938,16.9999999999999));
#55732=CARTESIAN_POINT('Ctrl Pts',(126.415950090396,-36.1111004102563,17.));
#55733=CARTESIAN_POINT('Ctrl Pts',(126.429949578689,-36.1439526727213,17.));
#55734=CARTESIAN_POINT('Ctrl Pts',(126.475866127408,-36.2517039332289,17.0000000000001));
#55735=CARTESIAN_POINT('Ctrl Pts',(126.527332973336,-36.3570819762472,17.0000000000002));
#55736=CARTESIAN_POINT('Ctrl Pts',(126.58400504888,-36.45981771484,17.));
#55737=CARTESIAN_POINT('Ctrl Pts',(126.641107329219,-36.5633333332401,16.9999999999998));
#55738=CARTESIAN_POINT('Ctrl Pts',(126.703494928383,-36.6641669871817,17.));
#55739=CARTESIAN_POINT('Ctrl Pts',(126.770850629467,-36.7620050500939,16.9999999999999));
#55740=CARTESIAN_POINT('Ctrl Pts',(126.804493487409,-36.8108732527689,16.9999999999999));
#55741=CARTESIAN_POINT('Ctrl Pts',(126.839376275211,-36.8589934594567,17.0000000000001));
#55742=CARTESIAN_POINT('Ctrl Pts',(126.87546185721,-36.9063223196442,17.0000000000001));
#55743=CARTESIAN_POINT('Ctrl Pts',(126.886663998762,-36.9210147414354,17.0000000000001));
#55744=CARTESIAN_POINT('Ctrl Pts',(126.897982060954,-36.9356308801713,17.));
#55745=CARTESIAN_POINT('Ctrl Pts',(126.909414956083,-36.9501693775893,17.0000000000001));
#55746=CARTESIAN_POINT('Ctrl Pts',(126.919260361815,-36.9626891640644,17.0000000000001));
#55747=CARTESIAN_POINT('Ctrl Pts',(126.929187993614,-36.9751475918217,17.0000000000001));
#55748=CARTESIAN_POINT('Ctrl Pts',(126.93919204257,-36.9875378873469,17.));
#55749=CARTESIAN_POINT('Ctrl Pts',(127.01206530898,-37.0777934739326,16.9999999999999));
#55750=CARTESIAN_POINT('Ctrl Pts',(127.089068527172,-37.1645366085542,16.9999999999999));
#55751=CARTESIAN_POINT('Ctrl Pts',(127.169856641689,-37.2475215103742,16.9999999999999));
#55752=CARTESIAN_POINT('Ctrl Pts',(127.25039235393,-37.3302471466052,17.));
#55753=CARTESIAN_POINT('Ctrl Pts',(127.334690166794,-37.4092384879766,17.0000000000001));
#55754=CARTESIAN_POINT('Ctrl Pts',(127.422439583585,-37.4842112339295,17.));
#55755=CARTESIAN_POINT('Ctrl Pts',(127.509315422489,-37.558437598478,16.9999999999999));
#55756=CARTESIAN_POINT('Ctrl Pts',(127.599575260046,-37.6287253893366,16.9999999999999));
#55757=CARTESIAN_POINT('Ctrl Pts',(127.692936664564,-37.6947520496931,17.0000000000001));
#55758=CARTESIAN_POINT('Ctrl Pts',(127.745228885034,-37.7317339342105,17.0000000000001));
#55759=CARTESIAN_POINT('Ctrl Pts',(127.798494396841,-37.7673781515159,17.));
#55760=CARTESIAN_POINT('Ctrl Pts',(127.852684844814,-37.8016208067591,17.));
#55761=CARTESIAN_POINT('Ctrl Pts',(127.881422150523,-37.8197797570693,17.0000000000001));
#55762=CARTESIAN_POINT('Ctrl Pts',(127.910419576427,-37.8375444684963,16.9999999999999));
#55763=CARTESIAN_POINT('Ctrl Pts',(127.939669941168,-37.8549047719967,16.9999999999999));
#55764=CARTESIAN_POINT('Ctrl Pts',(127.956236675144,-37.8647372486984,17.));
#55765=CARTESIAN_POINT('Ctrl Pts',(127.972886345269,-37.8744409183027,17.));
#55766=CARTESIAN_POINT('Ctrl Pts',(127.989598062667,-37.8840029632689,17.));
#55767=CARTESIAN_POINT('Ctrl Pts',(128.08642888323,-37.9394072426899,17.0000000000001));
#55768=CARTESIAN_POINT('Ctrl Pts',(128.18548331692,-37.9901465489129,16.9999999999999));
#55769=CARTESIAN_POINT('Ctrl Pts',(128.286476552124,-38.0359637356346,16.9999999999999));
#55770=CARTESIAN_POINT('Ctrl Pts',(128.385961066845,-38.0810964673239,16.9999999999999));
#55771=CARTESIAN_POINT('Ctrl Pts',(128.487327606991,-38.1214533278655,17.));
#55772=CARTESIAN_POINT('Ctrl Pts',(128.590315969054,-38.1567401839697,17.));
#55773=CARTESIAN_POINT('Ctrl Pts',(128.690232540977,-38.1909745540018,17.));
#55774=CARTESIAN_POINT('Ctrl Pts',(128.7916762279,-38.220436955216,17.));
#55775=CARTESIAN_POINT('Ctrl Pts',(128.89441127067,-38.2448103330173,17.));
#55776=CARTESIAN_POINT('Ctrl Pts',(128.959370040939,-38.2602214781005,17.));
#55777=CARTESIAN_POINT('Ctrl Pts',(129.024845096459,-38.2735970799981,17.));
#55778=CARTESIAN_POINT('Ctrl Pts',(129.090775666099,-38.2848462111391,17.));
#55779=CARTESIAN_POINT('Ctrl Pts',(129.131408328244,-38.2917789912983,17.));
#55780=CARTESIAN_POINT('Ctrl Pts',(129.172213989212,-38.2979038932228,17.));
#55781=CARTESIAN_POINT('Ctrl Pts',(129.213170804443,-38.3032244865145,17.));
#55782=CARTESIAN_POINT('Ctrl Pts',(132.56705599117,-32.7956090760829,29.9966206630762));
#55783=CARTESIAN_POINT('Ctrl Pts',(133.295540663306,-33.6438478316206,29.9308808351505));
#55784=CARTESIAN_POINT('Ctrl Pts',(133.832377684159,-36.1047329053186,29.7994478563687));
#55785=CARTESIAN_POINT('Ctrl Pts',(131.173363843183,-38.8159059974858,29.6023217267306));
#55786=CARTESIAN_POINT('Ctrl Pts',(127.452981180699,-38.0706344938751,29.4052422741622));
#55787=CARTESIAN_POINT('Ctrl Pts',(126.035010329987,-34.5541540104475,29.2081628215937));
#55788=CARTESIAN_POINT('Ctrl Pts',(128.199728320707,-31.4388221268633,29.0110833690253));
#55789=CARTESIAN_POINT('Ctrl Pts',(131.991478820009,-31.5424762882451,28.8140039164569));
#55790=CARTESIAN_POINT('Ctrl Pts',(133.983498939676,-34.7701917247564,28.6169244638884));
#55791=CARTESIAN_POINT('Ctrl Pts',(132.375780338592,-38.2057763622061,28.41984501132));
#55792=CARTESIAN_POINT('Ctrl Pts',(128.621113687997,-38.744292389259,28.2227655587515));
#55793=CARTESIAN_POINT('Ctrl Pts',(126.112518759346,-35.8992392442492,28.0256861061831));
#55794=CARTESIAN_POINT('Ctrl Pts',(127.116930427117,-32.2415456859938,27.8286066536146));
#55795=CARTESIAN_POINT('Ctrl Pts',(130.726696025998,-31.0766031807178,27.6315272010462));
#55796=CARTESIAN_POINT('Ctrl Pts',(133.679765074078,-33.4571226309144,27.4344477484778));
#55797=CARTESIAN_POINT('Ctrl Pts',(133.307530867572,-37.2319009861223,27.2373682959093));
#55798=CARTESIAN_POINT('Ctrl Pts',(129.946370573864,-38.9897698055861,27.0402888433409));
#55799=CARTESIAN_POINT('Ctrl Pts',(126.633673858793,-37.1421925771597,26.8432093907724));
#55800=CARTESIAN_POINT('Ctrl Pts',(126.363034610644,-33.3587738001739,26.646129938204));
#55801=CARTESIAN_POINT('Ctrl Pts',(129.379022256961,-31.058486712473,26.4490504856355));
#55802=CARTESIAN_POINT('Ctrl Pts',(132.956170614085,-32.3200380901321,26.2519710330671));
#55803=CARTESIAN_POINT('Ctrl Pts',(133.86190786446,-36.0033983074205,26.0548915804986));
#55804=CARTESIAN_POINT('Ctrl Pts',(131.277743838984,-38.780014704575,25.8578121279302));
#55805=CARTESIAN_POINT('Ctrl Pts',(127.538917403056,-38.1407344615195,25.6607326753618));
#55806=CARTESIAN_POINT('Ctrl Pts',(126.024104482112,-34.6632577640359,25.4636532227933));
#55807=CARTESIAN_POINT('Ctrl Pts',(128.102200381387,-31.4900858832021,25.2665737702249));
#55808=CARTESIAN_POINT('Ctrl Pts',(131.895286263836,-31.488728082256,25.0694943176564));
#55809=CARTESIAN_POINT('Ctrl Pts',(133.975653413485,-34.6604113703016,24.872414865088));
#55810=CARTESIAN_POINT('Ctrl Pts',(132.463330526414,-38.1389716817721,24.6753354125196));
#55811=CARTESIAN_POINT('Ctrl Pts',(128.724962730802,-38.7809285187328,24.4782559599511));
#55812=CARTESIAN_POINT('Ctrl Pts',(126.138811493571,-36.0061629188847,24.2811765073827));
#55813=CARTESIAN_POINT('Ctrl Pts',(127.041911464645,-32.3221552101542,24.0840970548142));
#55814=CARTESIAN_POINT('Ctrl Pts',(130.618155722524,-31.0580431250146,23.8870176022458));
#55815=CARTESIAN_POINT('Ctrl Pts',(133.63578943908,-33.3561704296975,23.6899381496773));
#55816=CARTESIAN_POINT('Ctrl Pts',(133.367858964113,-37.1397818812582,23.4928586971089));
#55817=CARTESIAN_POINT('Ctrl Pts',(130.056485792592,-38.9897305493931,23.2957792445405));
#55818=CARTESIAN_POINT('Ctrl Pts',(126.694067944094,-37.2342680553723,23.098699791972));
#55819=CARTESIAN_POINT('Ctrl Pts',(126.31913112674,-33.4597581880133,22.9016203394036));
#55820=CARTESIAN_POINT('Ctrl Pts',(129.27049556151,-31.0771230231173,22.7045408868351));
#55821=CARTESIAN_POINT('Ctrl Pts',(132.881093348709,-32.239485262215,22.5074614342667));
#55822=CARTESIAN_POINT('Ctrl Pts',(133.888125308583,-35.8964497120742,22.3103819816983));
#55823=CARTESIAN_POINT('Ctrl Pts',(131.381564003476,-38.743316898943,22.1133025291298));
#55824=CARTESIAN_POINT('Ctrl Pts',(127.626520822797,-38.207450248518,21.9162230765614));
#55825=CARTESIAN_POINT('Ctrl Pts',(126.016326326165,-34.7730979022514,21.7191436239929));
#55826=CARTESIAN_POINT('Ctrl Pts',(128.006069557745,-31.5437908203244,21.5220641714245));
#55827=CARTESIAN_POINT('Ctrl Pts',(131.797673587636,-31.4377661261477,21.324984718856));
#55828=CARTESIAN_POINT('Ctrl Pts',(133.964768809745,-34.550835455637,21.1279052662876));
#55829=CARTESIAN_POINT('Ctrl Pts',(132.549010115704,-38.0698025892216,20.9308258137191));
#55830=CARTESIAN_POINT('Ctrl Pts',(128.829780195416,-38.8146724753018,20.7337463611507));
#55831=CARTESIAN_POINT('Ctrl Pts',(126.168046135565,-36.1123264348889,20.5366669085822));
#55832=CARTESIAN_POINT('Ctrl Pts',(126.969144734657,-32.4048011832485,20.3395874560138));
#55833=CARTESIAN_POINT('Ctrl Pts',(130.5091449328,-31.0424866657829,20.1425080034454));
#55834=CARTESIAN_POINT('Ctrl Pts',(133.589044692203,-33.2564694210485,19.9454285508769));
#55835=CARTESIAN_POINT('Ctrl Pts',(133.425622193847,-37.0460335558426,19.7483490983085));
#55836=CARTESIAN_POINT('Ctrl Pts',(130.166557987812,-38.9866524370216,19.5512696457401));
#55837=CARTESIAN_POINT('Ctrl Pts',(126.75697974509,-37.3246423548653,19.3541901931716));
#55838=CARTESIAN_POINT('Ctrl Pts',(126.278031065997,-33.5619148736047,19.1571107406032));
#55839=CARTESIAN_POINT('Ctrl Pts',(129.162524195305,-31.0987484069462,18.9600312880347));
#55840=CARTESIAN_POINT('Ctrl Pts',(132.803822405259,-32.1610318275282,18.7629518354663));
#55841=CARTESIAN_POINT('Ctrl Pts',(133.911380504042,-35.7888245479408,18.5658723828978));
#55842=CARTESIAN_POINT('Ctrl Pts',(131.484334257128,-38.703755495549,18.3687929303294));
#55843=CARTESIAN_POINT('Ctrl Pts',(127.715927155011,-38.2717496145793,18.171713477761));
#55844=CARTESIAN_POINT('Ctrl Pts',(126.011591817358,-34.8830563622797,17.9746340251925));
#55845=CARTESIAN_POINT('Ctrl Pts',(127.911437163445,-31.6002406871,17.7775545726241));
#55846=CARTESIAN_POINT('Ctrl Pts',(131.698733465358,-31.3892839246133,17.5804751200556));
#55847=CARTESIAN_POINT('Ctrl Pts',(133.950778614665,-34.4420841751546,17.3833956674872));
#55848=CARTESIAN_POINT('Ctrl Pts',(132.632927369956,-37.9972978706467,17.1863162149187));
#55849=CARTESIAN_POINT('Ctrl Pts',(128.935134434648,-38.8475943936263,16.9892367623503));
#55850=CARTESIAN_POINT('Ctrl Pts',(126.201080798138,-36.2134083112296,16.7921573097818));
#55851=CARTESIAN_POINT('Ctrl Pts',(126.667056273216,-33.7394457916199,16.6607710080696));
#55852=CARTESIAN_POINT('Ctrl Pts',(127.370067526471,-32.8710163360532,16.5950778572134));
#55853=CARTESIAN_POINT('Ctrl Pts',(132.745392735114,-32.6424671496488,30.1323365993077));
#55854=CARTESIAN_POINT('Ctrl Pts',(133.524486192134,-33.5496341631874,30.066596771382));
#55855=CARTESIAN_POINT('Ctrl Pts',(134.098617984373,-36.1814801480512,29.9351637926001));
#55856=CARTESIAN_POINT('Ctrl Pts',(131.254878967113,-39.0810019880405,29.7380376629621));
#55857=CARTESIAN_POINT('Ctrl Pts',(127.276036445345,-38.2839554963636,29.5409582103937));
#55858=CARTESIAN_POINT('Ctrl Pts',(125.759557301321,-34.5231805052529,29.3438787578252));
#55859=CARTESIAN_POINT('Ctrl Pts',(128.074661087812,-31.1914224329392,29.1467993052568));
#55860=CARTESIAN_POINT('Ctrl Pts',(132.129829463554,-31.3022775847555,28.9497198526884));
#55861=CARTESIAN_POINT('Ctrl Pts',(134.260237831562,-34.7542266427015,28.7526404001199));
#55862=CARTESIAN_POINT('Ctrl Pts',(132.540828912276,-38.4284858473968,28.5555609475515));
#55863=CARTESIAN_POINT('Ctrl Pts',(128.525320648812,-39.0044132885975,28.358481494983));
#55864=CARTESIAN_POINT('Ctrl Pts',(125.842450342846,-35.961710573039,28.1614020424146));
#55865=CARTESIAN_POINT('Ctrl Pts',(126.916639805502,-32.0499122497264,27.9643225898461));
#55866=CARTESIAN_POINT('Ctrl Pts',(130.77718055129,-30.8040396619014,27.7672431372777));
#55867=CARTESIAN_POINT('Ctrl Pts',(133.935403176266,-33.3499369180767,27.5701636847093));
#55868=CARTESIAN_POINT('Ctrl Pts',(133.537309371604,-37.3869540726307,27.3730842321408));
#55869=CARTESIAN_POINT('Ctrl Pts',(129.942644867347,-39.2669443427457,27.1760047795724));
#55870=CARTESIAN_POINT('Ctrl Pts',(126.399810770048,-37.2910135029307,26.9789253270039));
#55871=CARTESIAN_POINT('Ctrl Pts',(126.110369858646,-33.2447556651743,26.7818458744355));
#55872=CARTESIAN_POINT('Ctrl Pts',(129.335882119334,-30.7846646188652,26.584766421867));
#55873=CARTESIAN_POINT('Ctrl Pts',(133.161539660835,-32.1338576240479,26.3876869692986));
#55874=CARTESIAN_POINT('Ctrl Pts',(134.130199665,-36.0731057028338,26.1906075167301));
#55875=CARTESIAN_POINT('Ctrl Pts',(131.366510378016,-39.0426172799742,25.9935280641617));
#55876=CARTESIAN_POINT('Ctrl Pts',(127.367942769692,-38.3589254006293,25.7964486115933));
#55877=CARTESIAN_POINT('Ctrl Pts',(125.747893809902,-34.6398638395882,25.5993691590248));
#55878=CARTESIAN_POINT('Ctrl Pts',(127.970357754733,-31.2462475496142,25.4022897064564));
#55879=CARTESIAN_POINT('Ctrl Pts',(132.026954284439,-31.2447954204569,25.2052102538879));
#55880=CARTESIAN_POINT('Ctrl Pts',(134.251847266385,-34.6368197031509,25.0081308013195));
#55881=CARTESIAN_POINT('Ctrl Pts',(132.634461326385,-38.3570401582626,24.8110513487511));
#55882=CARTESIAN_POINT('Ctrl Pts',(128.636384220719,-39.0435945779991,24.6139718961826));
#55883=CARTESIAN_POINT('Ctrl Pts',(125.870569667775,-36.0760623754797,24.4168924436142));
#55884=CARTESIAN_POINT('Ctrl Pts',(126.836409177391,-32.1361218231724,24.2198129910457));
#55885=CARTESIAN_POINT('Ctrl Pts',(130.661099810687,-30.7841902148048,24.0227335384773));
#55886=CARTESIAN_POINT('Ctrl Pts',(133.888372496271,-33.241971435139,23.8256540859088));
#55887=CARTESIAN_POINT('Ctrl Pts',(133.601828540075,-37.2884353328256,23.6285746333404));
#55888=CARTESIAN_POINT('Ctrl Pts',(130.060409934631,-39.2669023593734,23.431495180772));
#55889=CARTESIAN_POINT('Ctrl Pts',(126.464400511604,-37.3894855852837,23.2344157282035));
#55890=CARTESIAN_POINT('Ctrl Pts',(126.063416342178,-33.3527555707813,23.0373362756351));
#55891=CARTESIAN_POINT('Ctrl Pts',(129.21981593212,-30.8045956184337,22.8402568230666));
#55892=CARTESIAN_POINT('Ctrl Pts',(133.081246679441,-32.0477086856073,22.6431773704982));
#55893=CARTESIAN_POINT('Ctrl Pts',(134.158238469326,-35.958727248408,22.4460979179297));
#55894=CARTESIAN_POINT('Ctrl Pts',(131.477543065397,-39.0033700296909,22.2490184653613));
#55895=CARTESIAN_POINT('Ctrl Pts',(127.46163211381,-38.4302760207844,22.0519390127928));
#55896=CARTESIAN_POINT('Ctrl Pts',(125.739575295267,-34.7573347161559,21.8548595602244));
#55897=CARTESIAN_POINT('Ctrl Pts',(127.86754859679,-31.3036834391011,21.657780107656));
#55898=CARTESIAN_POINT('Ctrl Pts',(131.922560327698,-31.1902930704699,21.4607006550875));
#55899=CARTESIAN_POINT('Ctrl Pts',(134.240206494958,-34.5196314060906,21.2636212025191));
#55900=CARTESIAN_POINT('Ctrl Pts',(132.726093189031,-38.2830657982036,21.0665417499506));
#55901=CARTESIAN_POINT('Ctrl Pts',(128.748483491969,-39.079682771454,20.8694622973822));
#55902=CARTESIAN_POINT('Ctrl Pts',(125.901835278662,-36.1896012100724,20.6723828448137));
#55903=CARTESIAN_POINT('Ctrl Pts',(126.758587247308,-32.2245093203287,20.4753033922453));
#55904=CARTESIAN_POINT('Ctrl Pts',(130.544515898538,-30.7675530279628,20.2782239396769));
#55905=CARTESIAN_POINT('Ctrl Pts',(133.838380330569,-33.1353440667567,20.0811444871084));
#55906=CARTESIAN_POINT('Ctrl Pts',(133.66360465708,-37.1881741883823,19.88406503454));
#55907=CARTESIAN_POINT('Ctrl Pts',(130.178128989507,-39.2636104065015,19.6869855819715));
#55908=CARTESIAN_POINT('Ctrl Pts',(126.531682877863,-37.4861383058019,19.4899061294031));
#55909=CARTESIAN_POINT('Ctrl Pts',(126.019461006351,-33.4620092152014,19.2928266768347));
#55910=CARTESIAN_POINT('Ctrl Pts',(129.104343653605,-30.8277233460182,19.0957472242662));
#55911=CARTESIAN_POINT('Ctrl Pts',(132.998607622283,-31.9638049879963,18.8986677716978));
#55912=CARTESIAN_POINT('Ctrl Pts',(134.183109233691,-35.8436252230749,18.7015883191293));
#55913=CARTESIAN_POINT('Ctrl Pts',(131.587452903254,-38.9610602437561,18.5045088665609));
#55914=CARTESIAN_POINT('Ctrl Pts',(127.557249621093,-38.4990423480732,18.3074294139925));
#55915=CARTESIAN_POINT('Ctrl Pts',(125.734511873928,-34.8749321345075,18.110349961424));
#55916=CARTESIAN_POINT('Ctrl Pts',(127.766341966037,-31.3640549521016,17.9132705088556));
#55917=CARTESIAN_POINT('Ctrl Pts',(131.816746705461,-31.138442746857,17.7161910562871));
#55918=CARTESIAN_POINT('Ctrl Pts',(134.225244382692,-34.4033250316298,17.5191116037187));
#55919=CARTESIAN_POINT('Ctrl Pts',(132.815840284911,-38.2055240818087,17.3220321511502));
#55920=CARTESIAN_POINT('Ctrl Pts',(128.861156828271,-39.11489181859,17.1249526985818));
#55921=CARTESIAN_POINT('Ctrl Pts',(125.937164902537,-36.2977053768346,16.9278732460134));
#55922=CARTESIAN_POINT('Ctrl Pts',(126.435512304549,-33.651873438753,16.7964869443011));
#55923=CARTESIAN_POINT('Ctrl Pts',(127.187362670894,-32.7231130507938,16.7307937934449));
#55924=CARTESIAN_POINT('Ctrl Pts',(132.923729479057,-32.4893252232149,30.2680525355392));
#55925=CARTESIAN_POINT('Ctrl Pts',(133.753431720963,-33.4554204947541,30.2023127076135));
#55926=CARTESIAN_POINT('Ctrl Pts',(134.364858284588,-36.2582273907838,30.0708797288316));
#55927=CARTESIAN_POINT('Ctrl Pts',(131.336394091043,-39.3460979785953,29.8737535991936));
#55928=CARTESIAN_POINT('Ctrl Pts',(127.09909170999,-38.497276498852,29.6766741466252));
#55929=CARTESIAN_POINT('Ctrl Pts',(125.484104272656,-34.4922070000582,29.4795946940567));
#55930=CARTESIAN_POINT('Ctrl Pts',(127.949593854918,-30.9440227390151,29.2825152414883));
#55931=CARTESIAN_POINT('Ctrl Pts',(132.268180107098,-31.0620788812659,29.0854357889198));
#55932=CARTESIAN_POINT('Ctrl Pts',(134.536976723449,-34.7382615606466,28.8883563363514));
#55933=CARTESIAN_POINT('Ctrl Pts',(132.70587748596,-38.6511953325875,28.691276883783));
#55934=CARTESIAN_POINT('Ctrl Pts',(128.429527609628,-39.2645341879362,28.4941974312145));
#55935=CARTESIAN_POINT('Ctrl Pts',(125.572381926345,-36.0241819018289,28.2971179786461));
#55936=CARTESIAN_POINT('Ctrl Pts',(126.716349183886,-31.858278813459,28.1000385260776));
#55937=CARTESIAN_POINT('Ctrl Pts',(130.827665076582,-30.5314761430851,27.9029590735092));
#55938=CARTESIAN_POINT('Ctrl Pts',(134.191041278453,-33.2427512052388,27.7058796209408));
#55939=CARTESIAN_POINT('Ctrl Pts',(133.767087875637,-37.5420071591392,27.5088001683723));
#55940=CARTESIAN_POINT('Ctrl Pts',(129.93891916083,-39.5441188799051,27.3117207158039));
#55941=CARTESIAN_POINT('Ctrl Pts',(126.165947681302,-37.4398344287019,27.1146412632354));
#55942=CARTESIAN_POINT('Ctrl Pts',(125.857705106647,-33.1307375301746,26.917561810667));
#55943=CARTESIAN_POINT('Ctrl Pts',(129.292741981707,-30.5108425252575,26.7204823580985));
#55944=CARTESIAN_POINT('Ctrl Pts',(133.366908707584,-31.9476771579637,26.5234029055301));
#55945=CARTESIAN_POINT('Ctrl Pts',(134.398491465541,-36.142813098247,26.3263234529617));
#55946=CARTESIAN_POINT('Ctrl Pts',(131.455276917049,-39.3052198553734,26.1292440003932));
#55947=CARTESIAN_POINT('Ctrl Pts',(127.196968136327,-38.5771163397391,25.9321645478248));
#55948=CARTESIAN_POINT('Ctrl Pts',(125.471683137692,-34.6164699151406,25.7350850952563));
#55949=CARTESIAN_POINT('Ctrl Pts',(127.83851512808,-31.0024092160264,25.5380056426879));
#55950=CARTESIAN_POINT('Ctrl Pts',(132.158622305042,-31.0008627586579,25.3409261901194));
#55951=CARTESIAN_POINT('Ctrl Pts',(134.528041119285,-34.6132280360003,25.143846737551));
#55952=CARTESIAN_POINT('Ctrl Pts',(132.805592126357,-38.5751086347531,24.9467672849826));
#55953=CARTESIAN_POINT('Ctrl Pts',(128.547805710636,-39.3062606372654,24.7496878324141));
#55954=CARTESIAN_POINT('Ctrl Pts',(125.602327841979,-36.1459618320745,24.5526083798457));
#55955=CARTESIAN_POINT('Ctrl Pts',(126.630906890138,-31.9500884361906,24.3555289272772));
#55956=CARTESIAN_POINT('Ctrl Pts',(130.704043898852,-30.510337304595,24.1584494747088));
#55957=CARTESIAN_POINT('Ctrl Pts',(134.140955553463,-33.1277724405804,23.9613700221403));
#55958=CARTESIAN_POINT('Ctrl Pts',(133.835798116036,-37.4370887843932,23.7642905695719));
#55959=CARTESIAN_POINT('Ctrl Pts',(130.064334076669,-39.5440741693538,23.5672111170034));
#55960=CARTESIAN_POINT('Ctrl Pts',(126.234733079114,-37.5447031151951,23.370131664435));
#55961=CARTESIAN_POINT('Ctrl Pts',(125.807701557615,-33.2457529535492,23.1730522118666));
#55962=CARTESIAN_POINT('Ctrl Pts',(129.169136302732,-30.5320682137501,22.9759727592981));
#55963=CARTESIAN_POINT('Ctrl Pts',(133.281400010173,-31.8559321089998,22.7788933067297));
#55964=CARTESIAN_POINT('Ctrl Pts',(134.428351630069,-36.0210047847419,22.5818138541613));
#55965=CARTESIAN_POINT('Ctrl Pts',(131.573522127316,-39.2634231604387,22.3847344015928));
#55966=CARTESIAN_POINT('Ctrl Pts',(127.296743404824,-38.6531017930509,22.1876549490244));
#55967=CARTESIAN_POINT('Ctrl Pts',(125.462824264368,-34.7415715300603,21.9905754964559));
#55968=CARTESIAN_POINT('Ctrl Pts',(127.729027635835,-31.0635760578779,21.7934960438875));
#55969=CARTESIAN_POINT('Ctrl Pts',(132.047447067761,-30.9428200147922,21.596416591319));
#55970=CARTESIAN_POINT('Ctrl Pts',(134.515644180173,-34.4884273565441,21.3993371387506));
#55971=CARTESIAN_POINT('Ctrl Pts',(132.903176262356,-38.4963290071856,21.2022576861821));
#55972=CARTESIAN_POINT('Ctrl Pts',(128.667186788521,-39.3446930676061,21.0051782336137));
#55973=CARTESIAN_POINT('Ctrl Pts',(125.635624421759,-36.2668759852559,20.8080987810452));
#55974=CARTESIAN_POINT('Ctrl Pts',(126.548029759958,-32.044217457409,20.6110193284768));
#55975=CARTESIAN_POINT('Ctrl Pts',(130.579886864277,-30.4926193901429,20.4139398759084));
#55976=CARTESIAN_POINT('Ctrl Pts',(134.087715968934,-33.0142187124648,20.2168604233399));
#55977=CARTESIAN_POINT('Ctrl Pts',(133.901587120311,-37.3303148209218,20.0197809707715));
#55978=CARTESIAN_POINT('Ctrl Pts',(130.189699991202,-39.5405683759814,19.822701518203));
#55979=CARTESIAN_POINT('Ctrl Pts',(126.306386010636,-37.6476342567385,19.6256220656346));
#55980=CARTESIAN_POINT('Ctrl Pts',(125.760890946705,-33.362103556798,19.4285426130662));
#55981=CARTESIAN_POINT('Ctrl Pts',(129.046163111905,-30.5566982850902,19.2314631604977));
#55982=CARTESIAN_POINT('Ctrl Pts',(133.193392839307,-31.7665781484643,19.0343837079293));
#55983=CARTESIAN_POINT('Ctrl Pts',(134.45483796334,-35.898425898209,18.8373042553608));
#55984=CARTESIAN_POINT('Ctrl Pts',(131.690571549381,-39.2183649919633,18.6402248027924));
#55985=CARTESIAN_POINT('Ctrl Pts',(127.398572087175,-38.726335081567,18.443145350224));
#55986=CARTESIAN_POINT('Ctrl Pts',(125.4574319305,-34.8668079067353,18.2460658976555));
#55987=CARTESIAN_POINT('Ctrl Pts',(127.62124676863,-31.1278692171032,18.0489864450871));
#55988=CARTESIAN_POINT('Ctrl Pts',(131.934759945563,-30.8876015691007,17.8519069925186));
#55989=CARTESIAN_POINT('Ctrl Pts',(134.499710150719,-34.364565888105,17.6548275399502));
#55990=CARTESIAN_POINT('Ctrl Pts',(132.998753199867,-38.4137502929707,17.4577480873817));
#55991=CARTESIAN_POINT('Ctrl Pts',(128.787179221893,-39.3821892435537,17.2606686348133));
#55992=CARTESIAN_POINT('Ctrl Pts',(125.673249006936,-36.3820024424398,17.0635891822449));
#55993=CARTESIAN_POINT('Ctrl Pts',(126.203968335883,-33.5643010858862,16.9322028805325));
#55994=CARTESIAN_POINT('Ctrl Pts',(127.004657815318,-32.5752097655344,16.8665097296764));
#55995=CARTESIAN_POINT('Ctrl Pts',(133.102066223001,-32.3361832967811,30.4037684717707));
#55996=CARTESIAN_POINT('Ctrl Pts',(133.98237724979,-33.3612068263209,30.338028643845));
#55997=CARTESIAN_POINT('Ctrl Pts',(134.631098584803,-36.3349746335164,30.2065956650631));
#55998=CARTESIAN_POINT('Ctrl Pts',(131.417909214973,-39.61119396915,30.0094695354251));
#55999=CARTESIAN_POINT('Ctrl Pts',(126.922146974635,-38.7105975013405,29.8123900828567));
#56000=CARTESIAN_POINT('Ctrl Pts',(125.20865124399,-34.4612334948636,29.6153106302882));
#56001=CARTESIAN_POINT('Ctrl Pts',(127.824526622024,-30.696623045091,29.4182311777198));
#56002=CARTESIAN_POINT('Ctrl Pts',(132.406530750643,-30.8218801777763,29.2211517251513));
#56003=CARTESIAN_POINT('Ctrl Pts',(134.813715615336,-34.7222964785918,29.0240722725829));
#56004=CARTESIAN_POINT('Ctrl Pts',(132.870926059646,-38.8739048177783,28.8269928200145));
#56005=CARTESIAN_POINT('Ctrl Pts',(128.333734570443,-39.5246550872747,28.629913367446));
#56006=CARTESIAN_POINT('Ctrl Pts',(125.302313509846,-36.0866532306186,28.4328339148776));
#56007=CARTESIAN_POINT('Ctrl Pts',(126.516058562272,-31.6666453771916,28.2357544623091));
#56008=CARTESIAN_POINT('Ctrl Pts',(130.878149601875,-30.2589126242688,28.0386750097407));
#56009=CARTESIAN_POINT('Ctrl Pts',(134.446679380639,-33.1355654924012,27.8415955571722));
#56010=CARTESIAN_POINT('Ctrl Pts',(133.996866379668,-37.6970602456476,27.6445161046038));
#56011=CARTESIAN_POINT('Ctrl Pts',(129.935193454313,-39.8212934170647,27.4474366520353));
#56012=CARTESIAN_POINT('Ctrl Pts',(125.932084592557,-37.5886553544729,27.2503571994669));
#56013=CARTESIAN_POINT('Ctrl Pts',(125.605040354648,-33.0167193951749,27.0532777468985));
#56014=CARTESIAN_POINT('Ctrl Pts',(129.24960184408,-30.2370204316497,26.85619829433));
#56015=CARTESIAN_POINT('Ctrl Pts',(133.572277754333,-31.7614966918794,26.6591188417616));
#56016=CARTESIAN_POINT('Ctrl Pts',(134.666783266082,-36.2125204936603,26.4620393891931));
#56017=CARTESIAN_POINT('Ctrl Pts',(131.544043456082,-39.5678224307725,26.2649599366247));
#56018=CARTESIAN_POINT('Ctrl Pts',(127.025993502963,-38.7953072788489,26.0678804840562));
#56019=CARTESIAN_POINT('Ctrl Pts',(125.195472465481,-34.5930759906928,25.8708010314878));
#56020=CARTESIAN_POINT('Ctrl Pts',(127.706672501426,-30.7585708824386,25.6737215789194));
#56021=CARTESIAN_POINT('Ctrl Pts',(132.290290325646,-30.7569300968589,25.4766421263509));
#56022=CARTESIAN_POINT('Ctrl Pts',(134.804234972186,-34.5896363688495,25.2795626737825));
#56023=CARTESIAN_POINT('Ctrl Pts',(132.976722926327,-38.7931771112437,25.0824832212141));
#56024=CARTESIAN_POINT('Ctrl Pts',(128.459227200554,-39.5689266965317,24.8854037686456));
#56025=CARTESIAN_POINT('Ctrl Pts',(125.334086016183,-36.2158612886693,24.6883243160772));
#56026=CARTESIAN_POINT('Ctrl Pts',(126.425404602883,-31.7640550492089,24.4912448635087));
#56027=CARTESIAN_POINT('Ctrl Pts',(130.746987987015,-30.2364843943852,24.2941654109403));
#56028=CARTESIAN_POINT('Ctrl Pts',(134.393538610655,-33.013573446022,24.0970859583718));
#56029=CARTESIAN_POINT('Ctrl Pts',(134.069767691998,-37.5857422359606,23.9000065058034));
#56030=CARTESIAN_POINT('Ctrl Pts',(130.068258218707,-39.8212459793342,23.702927053235));
#56031=CARTESIAN_POINT('Ctrl Pts',(126.005065646623,-37.6999206451065,23.5058476006665));
#56032=CARTESIAN_POINT('Ctrl Pts',(125.551986773052,-33.1387503363173,23.308768148098));
#56033=CARTESIAN_POINT('Ctrl Pts',(129.118456673342,-30.2595408090666,23.1116886955297));
#56034=CARTESIAN_POINT('Ctrl Pts',(133.481553340905,-31.6641555323922,22.9146092429611));
#56035=CARTESIAN_POINT('Ctrl Pts',(134.698464790813,-36.0832823210757,22.7175297903928));
#56036=CARTESIAN_POINT('Ctrl Pts',(131.669501189237,-39.5234762911866,22.5204503378243));
#56037=CARTESIAN_POINT('Ctrl Pts',(127.131854695836,-38.8759275653174,22.3233708852559));
#56038=CARTESIAN_POINT('Ctrl Pts',(125.186073233471,-34.7258083439647,22.1262914326874));
#56039=CARTESIAN_POINT('Ctrl Pts',(127.590506674879,-30.8234686766545,21.929211980119));
#56040=CARTESIAN_POINT('Ctrl Pts',(132.172333807822,-30.6953469591144,21.7321325275505));
#56041=CARTESIAN_POINT('Ctrl Pts',(134.791081865386,-34.4572233069978,21.5350530749821));
#56042=CARTESIAN_POINT('Ctrl Pts',(133.080259335682,-38.7095922161676,21.3379736224136));
#56043=CARTESIAN_POINT('Ctrl Pts',(128.585890085073,-39.6097033637582,21.1408941698452));
#56044=CARTESIAN_POINT('Ctrl Pts',(125.369413564855,-36.3441507604394,20.9438147172767));
#56045=CARTESIAN_POINT('Ctrl Pts',(126.337472272608,-31.8639255944892,20.7467352647083));
#56046=CARTESIAN_POINT('Ctrl Pts',(130.615257830015,-30.2176857523228,20.5496558121399));
#56047=CARTESIAN_POINT('Ctrl Pts',(134.337051607298,-32.893093358173,20.3525763595714));
#56048=CARTESIAN_POINT('Ctrl Pts',(134.139569583543,-37.4724554534615,20.155496907003));
#56049=CARTESIAN_POINT('Ctrl Pts',(130.201270992896,-39.8175263454613,19.9584174544345));
#56050=CARTESIAN_POINT('Ctrl Pts',(126.08108914341,-37.8091302076751,19.7613380018661));
#56051=CARTESIAN_POINT('Ctrl Pts',(125.502320887058,-33.2621978983947,19.5642585492976));
#56052=CARTESIAN_POINT('Ctrl Pts',(128.987982570204,-30.2856732241622,19.3671790967292));
#56053=CARTESIAN_POINT('Ctrl Pts',(133.388178056331,-31.5693513089325,19.1700996441607));
#56054=CARTESIAN_POINT('Ctrl Pts',(134.726566692989,-35.953226573343,18.9730201915924));
#56055=CARTESIAN_POINT('Ctrl Pts',(131.793690195508,-39.4756697401704,18.7759407390239));
#56056=CARTESIAN_POINT('Ctrl Pts',(127.239894553259,-38.9536278150609,18.5788612864555));
#56057=CARTESIAN_POINT('Ctrl Pts',(125.18035198707,-34.8586836789633,18.381781833887));
#56058=CARTESIAN_POINT('Ctrl Pts',(127.476151571223,-30.8916834821048,18.1847023813186));
#56059=CARTESIAN_POINT('Ctrl Pts',(132.052773185665,-30.6367603913443,17.9876229287501));
#56060=CARTESIAN_POINT('Ctrl Pts',(134.774175918744,-34.3258067445803,17.7905434761817));
#56061=CARTESIAN_POINT('Ctrl Pts',(133.181666114823,-38.6219765041328,17.5934640236132));
#56062=CARTESIAN_POINT('Ctrl Pts',(128.713201615517,-39.6494866685174,17.3963845710448));
#56063=CARTESIAN_POINT('Ctrl Pts',(125.409333111335,-36.4662995080448,17.1993051184764));
#56064=CARTESIAN_POINT('Ctrl Pts',(125.972424367217,-33.4767287330193,17.067918816764));
#56065=CARTESIAN_POINT('Ctrl Pts',(126.821952959743,-32.4273064802751,17.0022256659079));
#56066=CARTESIAN_POINT('Ctrl Pts',(132.573234427015,-32.7934484719078,30.));
#56067=CARTESIAN_POINT('Ctrl Pts',(132.649853057503,-32.8663667566396,29.9999999999999));
#56068=CARTESIAN_POINT('Ctrl Pts',(132.722535071741,-32.9429224736587,29.9999999999998));
#56069=CARTESIAN_POINT('Ctrl Pts',(132.791284600853,-33.022699725554,29.9999999999998));
#56070=CARTESIAN_POINT('Ctrl Pts',(132.861753079838,-33.1044716543404,29.9999999999998));
#56071=CARTESIAN_POINT('Ctrl Pts',(132.928090363081,-33.1896286377168,30.));
#56072=CARTESIAN_POINT('Ctrl Pts',(132.990274682848,-33.2777711046078,30.));
#56073=CARTESIAN_POINT('Ctrl Pts',(133.054246634771,-33.3684474306573,30.));
#56074=CARTESIAN_POINT('Ctrl Pts',(133.113823916719,-33.462283857259,30.));
#56075=CARTESIAN_POINT('Ctrl Pts',(133.168948488249,-33.5588888786663,30.));
#56076=CARTESIAN_POINT('Ctrl Pts',(133.221605685532,-33.651169862074,30.));
#56077=CARTESIAN_POINT('Ctrl Pts',(133.270199903795,-33.7459780039061,30.));
#56078=CARTESIAN_POINT('Ctrl Pts',(133.314646378775,-33.8430003949785,30.));
#56079=CARTESIAN_POINT('Ctrl Pts',(133.321660120829,-33.8583107210449,30.));
#56080=CARTESIAN_POINT('Ctrl Pts',(133.328571263663,-33.8736779522171,29.9999999999999));
#56081=CARTESIAN_POINT('Ctrl Pts',(133.335376993632,-33.8890954660849,29.9999999999999));
#56082=CARTESIAN_POINT('Ctrl Pts',(133.381245007221,-33.9930036050855,30.));
#56083=CARTESIAN_POINT('Ctrl Pts',(133.422184804746,-34.0988655926642,30.));
#56084=CARTESIAN_POINT('Ctrl Pts',(133.458173581916,-34.2062509409393,30.));
#56085=CARTESIAN_POINT('Ctrl Pts',(133.494910039186,-34.3158672593755,30.));
#56086=CARTESIAN_POINT('Ctrl Pts',(133.52648809981,-34.4270715662737,30.));
#56087=CARTESIAN_POINT('Ctrl Pts',(133.552844216446,-34.5394441670278,30.));
#56088=CARTESIAN_POINT('Ctrl Pts',(133.57918140631,-34.651736071123,30.));
#56089=CARTESIAN_POINT('Ctrl Pts',(133.600304510595,-34.7651954321151,30.0000000000001));
#56090=CARTESIAN_POINT('Ctrl Pts',(133.616105145657,-34.8794295532343,30.));
#56091=CARTESIAN_POINT('Ctrl Pts',(133.629438458493,-34.9758256327184,29.9999999999999));
#56092=CARTESIAN_POINT('Ctrl Pts',(133.638981116824,-35.0727741182234,30.0000000000001));
#56093=CARTESIAN_POINT('Ctrl Pts',(133.644640126762,-35.1700467953132,30.));
#56094=CARTESIAN_POINT('Ctrl Pts',(133.645721269348,-35.1886305466821,30.));
#56095=CARTESIAN_POINT('Ctrl Pts',(133.646660581927,-35.207226141285,30.0000000000001));
#56096=CARTESIAN_POINT('Ctrl Pts',(133.647457301671,-35.2258319984673,30.0000000000001));
#56097=CARTESIAN_POINT('Ctrl Pts',(133.648146506942,-35.2419270619067,30.0000000000002));
#56098=CARTESIAN_POINT('Ctrl Pts',(133.64872875084,-35.2580246317189,30.0000000000001));
#56099=CARTESIAN_POINT('Ctrl Pts',(133.649203597933,-35.2741159296301,30.0000000000001));
#56100=CARTESIAN_POINT('Ctrl Pts',(133.652701975148,-35.3926665764815,30.0000000000001));
#56101=CARTESIAN_POINT('Ctrl Pts',(133.650380391952,-35.5110020020146,29.9999999999999));
#56102=CARTESIAN_POINT('Ctrl Pts',(133.642173844882,-35.6286939927366,29.9999999999999));
#56103=CARTESIAN_POINT('Ctrl Pts',(133.633997658714,-35.7459505707316,29.9999999999999));
#56104=CARTESIAN_POINT('Ctrl Pts',(133.619980289647,-35.8625693524084,30.));
#56105=CARTESIAN_POINT('Ctrl Pts',(133.600009193167,-35.9781441488548,29.9999999999999));
#56106=CARTESIAN_POINT('Ctrl Pts',(133.59650213025,-35.9984398839037,29.9999999999998));
#56107=CARTESIAN_POINT('Ctrl Pts',(133.592811339928,-36.0187034486169,30.0000000000002));
#56108=CARTESIAN_POINT('Ctrl Pts',(133.588936046823,-36.038932666806,30.0000000000002));
#56109=CARTESIAN_POINT('Ctrl Pts',(133.567332076941,-36.1517064386639,30.0000000000001));
#56110=CARTESIAN_POINT('Ctrl Pts',(133.539998383114,-36.2634130820552,30.0000000000001));
#56111=CARTESIAN_POINT('Ctrl Pts',(133.507233683019,-36.3737930037498,30.0000000000001));
#56112=CARTESIAN_POINT('Ctrl Pts',(133.486428152307,-36.4438840726162,30.0000000000002));
#56113=CARTESIAN_POINT('Ctrl Pts',(133.463431616385,-36.5134401519788,30.));
#56114=CARTESIAN_POINT('Ctrl Pts',(133.438309961509,-36.5823930508116,29.9999999999999));
#56115=CARTESIAN_POINT('Ctrl Pts',(133.432144353763,-36.5993161607454,29.9999999999998));
#56116=CARTESIAN_POINT('Ctrl Pts',(133.425850700818,-36.6162029277894,29.9999999999999));
#56117=CARTESIAN_POINT('Ctrl Pts',(133.419429906065,-36.6330523228395,29.9999999999999));
#56118=CARTESIAN_POINT('Ctrl Pts',(133.413621254329,-36.6482953373861,29.9999999999998));
#56119=CARTESIAN_POINT('Ctrl Pts',(133.407710252341,-36.6635031939445,30.0000000000001));
#56120=CARTESIAN_POINT('Ctrl Pts',(133.401700786121,-36.6786677684889,30.0000000000001));
#56121=CARTESIAN_POINT('Ctrl Pts',(133.358822804144,-36.786868119445,30.));
#56122=CARTESIAN_POINT('Ctrl Pts',(133.310892795036,-36.8929797564497,30.));
#56123=CARTESIAN_POINT('Ctrl Pts',(133.258267581598,-36.9967501880808,29.9999999999999));
#56124=CARTESIAN_POINT('Ctrl Pts',(133.2037780914,-37.1041967435974,29.9999999999999));
#56125=CARTESIAN_POINT('Ctrl Pts',(133.14425472734,-37.2091339535983,30.0000000000001));
#56126=CARTESIAN_POINT('Ctrl Pts',(133.080037568562,-37.3112779782923,30.0000000000001));
#56127=CARTESIAN_POINT('Ctrl Pts',(133.015111946839,-37.4145488864843,30.0000000000001));
#56128=CARTESIAN_POINT('Ctrl Pts',(132.945388009163,-37.5149653945738,30.0000000000001));
#56129=CARTESIAN_POINT('Ctrl Pts',(132.87116509564,-37.6122196498687,30.));
#56130=CARTESIAN_POINT('Ctrl Pts',(132.817181793609,-37.682953949941,30.));
#56131=CARTESIAN_POINT('Ctrl Pts',(132.760817487172,-37.7520152103035,30.0000000000001));
#56132=CARTESIAN_POINT('Ctrl Pts',(132.702172154835,-37.8192767143393,29.9999999999999));
#56133=CARTESIAN_POINT('Ctrl Pts',(132.682391535084,-37.8419635025653,29.9999999999999));
#56134=CARTESIAN_POINT('Ctrl Pts',(132.662351312549,-37.8644454683242,29.9999999999999));
#56135=CARTESIAN_POINT('Ctrl Pts',(132.642055030732,-37.8867175151918,30.));
#56136=CARTESIAN_POINT('Ctrl Pts',(132.629127618235,-37.9009033616246,30.));
#56137=CARTESIAN_POINT('Ctrl Pts',(132.616095858353,-37.9150044443019,29.9999999999998));
#56138=CARTESIAN_POINT('Ctrl Pts',(132.602971661464,-37.9290079434914,29.9999999999998));
#56139=CARTESIAN_POINT('Ctrl Pts',(132.517322557525,-38.0203954141101,29.9999999999999));
#56140=CARTESIAN_POINT('Ctrl Pts',(132.427632644473,-38.1077482657667,29.9999999999999));
#56141=CARTESIAN_POINT('Ctrl Pts',(132.334235165115,-38.1907540095518,29.9999999999999));
#56142=CARTESIAN_POINT('Ctrl Pts',(132.250200410151,-38.2654387589431,29.9999999999998));
#56143=CARTESIAN_POINT('Ctrl Pts',(132.163163235718,-38.3366044655783,30.0000000000001));
#56144=CARTESIAN_POINT('Ctrl Pts',(132.073335782034,-38.4040052793126,30.));
#56145=CARTESIAN_POINT('Ctrl Pts',(132.035647403083,-38.4322842442108,29.9999999999999));
#56146=CARTESIAN_POINT('Ctrl Pts',(131.997467518359,-38.4599002091719,30.));
#56147=CARTESIAN_POINT('Ctrl Pts',(131.958810486488,-38.4868338044422,30.0000000000001));
#56148=CARTESIAN_POINT('Ctrl Pts',(131.94120789347,-38.4990980961665,30.0000000000001));
#56149=CARTESIAN_POINT('Ctrl Pts',(131.923504399256,-38.5112222027607,29.9999999999999));
#56150=CARTESIAN_POINT('Ctrl Pts',(131.905707729789,-38.5231999316637,29.9999999999999));
#56151=CARTESIAN_POINT('Ctrl Pts',(131.800671774011,-38.5938924961189,29.9999999999999));
#56152=CARTESIAN_POINT('Ctrl Pts',(131.692537688031,-38.659393354725,29.9999999999999));
#56153=CARTESIAN_POINT('Ctrl Pts',(131.581620730744,-38.7193732400858,29.9999999999999));
#56154=CARTESIAN_POINT('Ctrl Pts',(131.471353175383,-38.7790019523351,29.9999999999999));
#56155=CARTESIAN_POINT('Ctrl Pts',(131.358334664968,-38.8331748755337,30.));
#56156=CARTESIAN_POINT('Ctrl Pts',(131.242839107679,-38.8815321227036,30.));
#56157=CARTESIAN_POINT('Ctrl Pts',(131.228328557671,-38.8876075966851,30.));
#56158=CARTESIAN_POINT('Ctrl Pts',(131.21377886806,-38.8935912160834,30.));
#56159=CARTESIAN_POINT('Ctrl Pts',(131.199190548796,-38.899482217298,30.));
#56160=CARTESIAN_POINT('Ctrl Pts',(131.153580177004,-38.9179004292087,30.));
#56161=CARTESIAN_POINT('Ctrl Pts',(131.107592245152,-38.935413389631,30.));
#56162=CARTESIAN_POINT('Ctrl Pts',(131.061251415332,-38.9520280711437,30.));
#56163=CARTESIAN_POINT('Ctrl Pts',(128.941097447709,-38.949361204357,29.9977747858503));
#56164=CARTESIAN_POINT('Ctrl Pts',(127.636979705122,-38.599701212612,29.9320816349942));
#56165=CARTESIAN_POINT('Ctrl Pts',(125.424202616686,-36.5120753779567,29.8006953332819));
#56166=CARTESIAN_POINT('Ctrl Pts',(126.226060557691,-31.9948456048335,29.6036158807134));
#56167=CARTESIAN_POINT('Ctrl Pts',(130.445077406051,-30.199627076779,29.406536428145));
#56168=CARTESIAN_POINT('Ctrl Pts',(134.258668325894,-32.7392435465971,29.2094569755765));
#56169=CARTESIAN_POINT('Ctrl Pts',(134.225374578973,-37.3233447428259,29.0123775230081));
#56170=CARTESIAN_POINT('Ctrl Pts',(130.372971341113,-39.8071763851411,28.8152980704396));
#56171=CARTESIAN_POINT('Ctrl Pts',(126.183888210242,-37.9472442087612,28.6182186178712));
#56172=CARTESIAN_POINT('Ctrl Pts',(125.443145605471,-33.4237977850877,28.4211391653028));
#56173=CARTESIAN_POINT('Ctrl Pts',(128.820393714243,-30.3248045440124,28.2240597127343));
#56174=CARTESIAN_POINT('Ctrl Pts',(133.263578832371,-31.4506188224813,28.0269802601659));
#56175=CARTESIAN_POINT('Ctrl Pts',(134.757576278224,-35.7839316709174,27.8299008075974));
#56176=CARTESIAN_POINT('Ctrl Pts',(131.952271604642,-39.4088174824048,27.632821355029));
#56177=CARTESIAN_POINT('Ctrl Pts',(127.382756745135,-39.0495791332309,27.4357419024605));
#56178=CARTESIAN_POINT('Ctrl Pts',(125.178371298366,-35.0308439142191,27.2386624498921));
#56179=CARTESIAN_POINT('Ctrl Pts',(127.33116187244,-30.9842369354514,27.0415829973237));
#56180=CARTESIAN_POINT('Ctrl Pts',(131.895708468177,-30.5665654892088,26.8445035447552));
#56181=CARTESIAN_POINT('Ctrl Pts',(134.747155050647,-34.1552686718858,26.6474240921868));
#56182=CARTESIAN_POINT('Ctrl Pts',(133.308726393028,-38.5073324998802,26.4503446396183));
#56183=CARTESIAN_POINT('Ctrl Pts',(128.880291597111,-39.6899152415161,26.2532651870499));
#56184=CARTESIAN_POINT('Ctrl Pts',(125.463706852098,-36.634348899534,26.0561857344814));
#56185=CARTESIAN_POINT('Ctrl Pts',(126.146447062293,-32.1018658487985,25.859106281913));
#56186=CARTESIAN_POINT('Ctrl Pts',(130.311538417948,-30.1883479294121,25.6620268293445));
#56187=CARTESIAN_POINT('Ctrl Pts',(134.195100967925,-32.6229893359297,25.4649473767761));
#56188=CARTESIAN_POINT('Ctrl Pts',(134.287664683484,-37.2056707337862,25.2678679242077));
#56189=CARTESIAN_POINT('Ctrl Pts',(130.505582250638,-39.7951473820333,25.0707884716392));
#56190=CARTESIAN_POINT('Ctrl Pts',(126.266618865874,-38.0513795460382,24.8737090190708));
#56191=CARTESIAN_POINT('Ctrl Pts',(125.40141063766,-33.5501628702343,24.6766295665024));
#56192=CARTESIAN_POINT('Ctrl Pts',(128.6918227481,-30.3591246402977,24.4795501139339));
#56193=CARTESIAN_POINT('Ctrl Pts',(133.164399119471,-31.3619194567416,24.2824706613655));
#56194=CARTESIAN_POINT('Ctrl Pts',(134.777393931214,-35.6523488733214,24.085391208797));
#56195=CARTESIAN_POINT('Ctrl Pts',(132.073187570514,-39.3532683266752,23.8883117562286));
#56196=CARTESIAN_POINT('Ctrl Pts',(127.49549789673,-39.1202573998797,23.6912323036602));
#56197=CARTESIAN_POINT('Ctrl Pts',(125.18105876756,-35.1638817404141,23.4941528510917));
#56198=CARTESIAN_POINT('Ctrl Pts',(127.221365978803,-31.0594106021052,23.2970733985233));
#56199=CARTESIAN_POINT('Ctrl Pts',(131.772649305235,-30.5159431016996,23.0999939459548));
#56200=CARTESIAN_POINT('Ctrl Pts',(134.72203758824,-34.0245960622412,22.9029144933864));
#56201=CARTESIAN_POINT('Ctrl Pts',(133.404248722819,-38.4146950756628,22.7058350408179));
#56202=CARTESIAN_POINT('Ctrl Pts',(129.010132724007,-39.7190268702816,22.5087555882495));
#56203=CARTESIAN_POINT('Ctrl Pts',(125.51053290411,-36.7589022205524,22.3116761356811));
#56204=CARTESIAN_POINT('Ctrl Pts',(126.067942593805,-32.2093053945169,22.1145966831126));
#56205=CARTESIAN_POINT('Ctrl Pts',(130.178645792201,-30.1815835062547,21.9175172305442));
#56206=CARTESIAN_POINT('Ctrl Pts',(134.127911639003,-32.5081337661877,21.7204377779757));
#56207=CARTESIAN_POINT('Ctrl Pts',(134.346895825177,-37.086515878837,21.5233583254073));
#56208=CARTESIAN_POINT('Ctrl Pts',(130.637708287566,-39.7793702476217,21.3262788728388));
#56209=CARTESIAN_POINT('Ctrl Pts',(126.352241086956,-38.1532375014412,21.1291994202704));
#56210=CARTESIAN_POINT('Ctrl Pts',(125.363154565577,-33.6776096448007,20.932119967702));
#56211=CARTESIAN_POINT('Ctrl Pts',(128.564259358348,-30.3969900486762,20.7350405151335));
#56212=CARTESIAN_POINT('Ctrl Pts',(133.062803979689,-31.2759855490205,20.5379610625651));
#56213=CARTESIAN_POINT('Ctrl Pts',(134.793575818518,-35.520271806098,20.3408816099966));
#56214=CARTESIAN_POINT('Ctrl Pts',(132.192523336302,-39.294402522867,20.1438021574282));
#56215=CARTESIAN_POINT('Ctrl Pts',(127.610147083839,-39.187798363185,19.9467227048597));
#56216=CARTESIAN_POINT('Ctrl Pts',(125.187415948436,-35.2967943807173,19.7496432522913));
#56217=CARTESIAN_POINT('Ctrl Pts',(127.113686487097,-31.1375856971393,19.5525637997228));
#56218=CARTESIAN_POINT('Ctrl Pts',(131.648239873017,-30.4687352753939,19.3554843471544));
#56219=CARTESIAN_POINT('Ctrl Pts',(134.693324263192,-33.8946671216466,19.158404894586));
#56220=CARTESIAN_POINT('Ctrl Pts',(133.49717767076,-38.3194554298236,18.9613254420175));
#56221=CARTESIAN_POINT('Ctrl Pts',(129.140729238591,-39.7445478885119,18.7642459894491));
#56222=CARTESIAN_POINT('Ctrl Pts',(125.560774958467,-36.8821090746942,18.5671665368806));
#56223=CARTESIAN_POINT('Ctrl Pts',(125.992439189035,-32.3188845814651,18.3700870843122));
#56224=CARTESIAN_POINT('Ctrl Pts',(130.045603765049,-30.1784591994005,18.1730076317438));
#56225=CARTESIAN_POINT('Ctrl Pts',(134.057606144223,-32.3952370556287,17.9759281791753));
#56226=CARTESIAN_POINT('Ctrl Pts',(134.40275932918,-36.9656456212823,17.7788487266069));
#56227=CARTESIAN_POINT('Ctrl Pts',(130.769466728782,-39.7602144993633,17.5817692740384));
#56228=CARTESIAN_POINT('Ctrl Pts',(126.440397046927,-38.2521535123727,17.38468982147));
#56229=CARTESIAN_POINT('Ctrl Pts',(125.32893397472,-33.8071813688381,17.1876103689015));
#56230=CARTESIAN_POINT('Ctrl Pts',(128.436718489661,-30.4360408883912,16.9905309163331));
#56231=CARTESIAN_POINT('Ctrl Pts',(132.961968787017,-31.197894221067,16.7934047948872));
#56232=CARTESIAN_POINT('Ctrl Pts',(134.185068371337,-33.9850287565488,16.6619718242975));
#56233=CARTESIAN_POINT('Ctrl Pts',(134.075375726175,-35.3317236383559,16.5962320045639));
#56234=CARTESIAN_POINT('Ctrl Pts',(129.001973251084,-38.7223143098011,30.1334903656045));
#56235=CARTESIAN_POINT('Ctrl Pts',(127.772828616367,-38.3927561044383,30.0677972147483));
#56236=CARTESIAN_POINT('Ctrl Pts',(125.687263028798,-36.4251468846801,29.9364109130361));
#56237=CARTESIAN_POINT('Ctrl Pts',(126.4430225387,-32.1676104996552,29.7393314604676));
#56238=CARTESIAN_POINT('Ctrl Pts',(130.419490117967,-30.4755982297153,29.5422520078992));
#56239=CARTESIAN_POINT('Ctrl Pts',(134.013839512243,-32.8692133583039,29.3451725553307));
#56240=CARTESIAN_POINT('Ctrl Pts',(133.982459806977,-37.189776760171,29.1480931027623));
#56241=CARTESIAN_POINT('Ctrl Pts',(130.351529396359,-39.5308141044197,28.9510136501938));
#56242=CARTESIAN_POINT('Ctrl Pts',(126.403274659419,-37.7778085429733,28.7539341976254));
#56243=CARTESIAN_POINT('Ctrl Pts',(125.705116994181,-33.5144128996771,28.5568547450569));
#56244=CARTESIAN_POINT('Ctrl Pts',(128.888208717764,-30.5935793039794,28.3597752924885));
#56245=CARTESIAN_POINT('Ctrl Pts',(133.075957239742,-31.654671055805,28.1626958399201));
#56246=CARTESIAN_POINT('Ctrl Pts',(134.484065484026,-35.7388638125433,27.9656163873516));
#56247=CARTESIAN_POINT('Ctrl Pts',(131.840036439958,-39.1553566652632,27.7685369347832));
#56248=CARTESIAN_POINT('Ctrl Pts',(127.533220813264,-38.8167707576779,27.5714574822147));
#56249=CARTESIAN_POINT('Ctrl Pts',(125.455564435879,-35.0290707122816,27.3743780296463));
#56250=CARTESIAN_POINT('Ctrl Pts',(127.484592105225,-31.2151012413225,27.1772985770779));
#56251=CARTESIAN_POINT('Ctrl Pts',(131.786725091269,-30.8214415275873,26.9802191245094));
#56252=CARTESIAN_POINT('Ctrl Pts',(134.474243367857,-34.2038318735932,26.783139671941));
#56253=CARTESIAN_POINT('Ctrl Pts',(133.118509288641,-38.3056976250062,26.5860602193725));
#56254=CARTESIAN_POINT('Ctrl Pts',(128.944663099876,-39.42029424809,26.3889807668041));
#56255=CARTESIAN_POINT('Ctrl Pts',(125.724496184533,-36.540390959741,26.1919013142356));
#56256=CARTESIAN_POINT('Ctrl Pts',(126.367985985233,-32.2684782007685,25.9948218616672));
#56257=CARTESIAN_POINT('Ctrl Pts',(130.293628222687,-30.4649675151582,25.7977424090988));
#56258=CARTESIAN_POINT('Ctrl Pts',(133.953926611407,-32.7596425468358,25.6006629565303));
#56259=CARTESIAN_POINT('Ctrl Pts',(134.041168883048,-37.0788677738628,25.4035835039619));
#56260=CARTESIAN_POINT('Ctrl Pts',(130.476516567858,-39.5194766429712,25.2065040513934));
#56261=CARTESIAN_POINT('Ctrl Pts',(126.481249169064,-37.87595718931,25.009424598825));
#56262=CARTESIAN_POINT('Ctrl Pts',(125.665781349791,-33.6335133162664,24.8123451462565));
#56263=CARTESIAN_POINT('Ctrl Pts',(128.767029235226,-30.625926354276,24.6152656936881));
#56264=CARTESIAN_POINT('Ctrl Pts',(132.982479321297,-31.5710709743541,24.4181862411197));
#56265=CARTESIAN_POINT('Ctrl Pts',(134.502743829583,-35.6148456473082,24.2211067885512));
#56266=CARTESIAN_POINT('Ctrl Pts',(131.954001004545,-39.1030010040384,24.0240273359828));
#56267=CARTESIAN_POINT('Ctrl Pts',(127.639480529752,-38.883385764441,23.8269478834143));
#56268=CARTESIAN_POINT('Ctrl Pts',(125.458097403749,-35.1544602572147,23.6298684308459));
#56269=CARTESIAN_POINT('Ctrl Pts',(127.381108325217,-31.2859532096857,23.4327889782775));
#56270=CARTESIAN_POINT('Ctrl Pts',(131.670740540991,-30.7737293970246,23.235709525709));
#56271=CARTESIAN_POINT('Ctrl Pts',(134.450569896401,-34.0806715700376,23.0386300731406));
#56272=CARTESIAN_POINT('Ctrl Pts',(133.208540085189,-38.2183858821837,22.8415506205721));
#56273=CARTESIAN_POINT('Ctrl Pts',(129.06703972223,-39.4477322631838,22.6444711680036));
#56274=CARTESIAN_POINT('Ctrl Pts',(125.768630229117,-36.6577837696589,22.4473917154353));
#56275=CARTESIAN_POINT('Ctrl Pts',(126.293994701247,-32.369741098177,22.2503122628668));
#56276=CARTESIAN_POINT('Ctrl Pts',(130.168375530697,-30.4585919754662,22.0532328102984));
#56277=CARTESIAN_POINT('Ctrl Pts',(133.890599965003,-32.6513899690925,21.8561533577299));
#56278=CARTESIAN_POINT('Ctrl Pts',(134.096994854616,-36.9665630747711,21.6590739051615));
#56279=CARTESIAN_POINT('Ctrl Pts',(130.601046741853,-39.5046065285022,21.461994452593));
#56280=CARTESIAN_POINT('Ctrl Pts',(126.561949009437,-37.9719593793719,21.2649150000246));
#56281=CARTESIAN_POINT('Ctrl Pts',(125.629724601071,-33.753633236466,21.0678355474561));
#56282=CARTESIAN_POINT('Ctrl Pts',(128.646799403992,-30.6616148983622,20.8707560948877));
#56283=CARTESIAN_POINT('Ctrl Pts',(132.886724837712,-31.4900773660575,20.6736766423193));
#56284=CARTESIAN_POINT('Ctrl Pts',(134.517995427894,-35.4903616277712,20.4765971897508));
#56285=CARTESIAN_POINT('Ctrl Pts',(132.066476213998,-39.0475193672533,20.2795177371824));
#56286=CARTESIAN_POINT('Ctrl Pts',(127.747538589701,-38.9470438299358,20.0824382846139));
#56287=CARTESIAN_POINT('Ctrl Pts',(125.464089113325,-35.2797318131331,19.8853588320455));
#56288=CARTESIAN_POINT('Ctrl Pts',(127.279619276201,-31.3596340557411,19.688279379477));
#56289=CARTESIAN_POINT('Ctrl Pts',(131.553483347775,-30.729235526168,19.4911999269086));
#56290=CARTESIAN_POINT('Ctrl Pts',(134.423507286734,-33.9582121823526,19.2941204743402));
#56291=CARTESIAN_POINT('Ctrl Pts',(133.296126592175,-38.1286215182213,19.0970410217717));
#56292=CARTESIAN_POINT('Ctrl Pts',(129.190128305394,-39.4717860902317,18.8999615692033));
#56293=CARTESIAN_POINT('Ctrl Pts',(125.8159838917,-36.7739075204394,18.7028821166348));
#56294=CARTESIAN_POINT('Ctrl Pts',(126.222831951255,-32.4730206298602,18.5058026640664));
#56295=CARTESIAN_POINT('Ctrl Pts',(130.042982026317,-30.455647283525,18.308723211498));
#56296=CARTESIAN_POINT('Ctrl Pts',(133.824336299632,-32.5449836366508,18.1116437589295));
#56297=CARTESIAN_POINT('Ctrl Pts',(134.149646792382,-36.8526415907527,17.9145643063611));
#56298=CARTESIAN_POINT('Ctrl Pts',(130.725230453043,-39.4865520350872,17.7174848537926));
#56299=CARTESIAN_POINT('Ctrl Pts',(126.645036925259,-38.0651887559485,17.5204054012242));
#56300=CARTESIAN_POINT('Ctrl Pts',(125.597471335683,-33.8757559438036,17.3233259486557));
#56301=CARTESIAN_POINT('Ctrl Pts',(128.526590799099,-30.6984207239018,17.1262464960873));
#56302=CARTESIAN_POINT('Ctrl Pts',(132.791686612239,-31.4164754713532,16.9291203746415));
#56303=CARTESIAN_POINT('Ctrl Pts',(133.944470784019,-34.0433789699035,16.7976874040518));
#56304=CARTESIAN_POINT('Ctrl Pts',(133.84108431678,-35.3126530043869,16.7319475843182));
#56305=CARTESIAN_POINT('Ctrl Pts',(129.06284905446,-38.4952674152452,30.2692059453588));
#56306=CARTESIAN_POINT('Ctrl Pts',(127.908677527612,-38.1858109962646,30.2035127945026));
#56307=CARTESIAN_POINT('Ctrl Pts',(125.95032344091,-36.3382183914036,30.0721264927903));
#56308=CARTESIAN_POINT('Ctrl Pts',(126.65998451971,-32.3403753944769,29.8750470402219));
#56309=CARTESIAN_POINT('Ctrl Pts',(130.393902829884,-30.7515693826514,29.6779675876535));
#56310=CARTESIAN_POINT('Ctrl Pts',(133.769010698594,-32.9991831700107,29.480888135085));
#56311=CARTESIAN_POINT('Ctrl Pts',(133.739545034979,-37.0562087775161,29.2838086825166));
#56312=CARTESIAN_POINT('Ctrl Pts',(130.330087451605,-39.2544518236982,29.0867292299481));
#56313=CARTESIAN_POINT('Ctrl Pts',(126.622661108597,-37.6083728771854,28.8896497773797));
#56314=CARTESIAN_POINT('Ctrl Pts',(125.967088382891,-33.6050280142665,28.6925703248112));
#56315=CARTESIAN_POINT('Ctrl Pts',(128.956023721286,-30.8623540639465,28.4954908722428));
#56316=CARTESIAN_POINT('Ctrl Pts',(132.888335647114,-31.8587232891287,28.2984114196744));
#56317=CARTESIAN_POINT('Ctrl Pts',(134.210554689826,-35.6937959541694,28.1013319671059));
#56318=CARTESIAN_POINT('Ctrl Pts',(131.727801275276,-38.9018958481215,27.9042525145375));
#56319=CARTESIAN_POINT('Ctrl Pts',(127.683684881391,-38.5839623821248,27.707173061969));
#56320=CARTESIAN_POINT('Ctrl Pts',(125.732757573393,-35.0272975103442,27.5100936094006));
#56321=CARTESIAN_POINT('Ctrl Pts',(127.638022338009,-31.4459655471936,27.3130141568322));
#56322=CARTESIAN_POINT('Ctrl Pts',(131.67774171436,-31.0763175659658,27.1159347042637));
#56323=CARTESIAN_POINT('Ctrl Pts',(134.201331685068,-34.2523950753005,26.9188552516953));
#56324=CARTESIAN_POINT('Ctrl Pts',(132.928292184253,-38.1040627501321,26.7217757991268));
#56325=CARTESIAN_POINT('Ctrl Pts',(129.00903460264,-39.1506732546641,26.5246963465584));
#56326=CARTESIAN_POINT('Ctrl Pts',(125.985285516968,-36.4464330199479,26.32761689399));
#56327=CARTESIAN_POINT('Ctrl Pts',(126.589524908172,-32.4350905527384,26.1305374414215));
#56328=CARTESIAN_POINT('Ctrl Pts',(130.275718027424,-30.7415871009042,25.9334579888531));
#56329=CARTESIAN_POINT('Ctrl Pts',(133.71275225489,-32.896295757742,25.7363785362846));
#56330=CARTESIAN_POINT('Ctrl Pts',(133.794673082611,-36.9520648139394,25.5392990837162));
#56331=CARTESIAN_POINT('Ctrl Pts',(130.447450885079,-39.2438059039089,25.3422196311477));
#56332=CARTESIAN_POINT('Ctrl Pts',(126.695879472254,-37.7005348325817,25.1451401785793));
#56333=CARTESIAN_POINT('Ctrl Pts',(125.930152061922,-33.7168637622985,24.9480607260108));
#56334=CARTESIAN_POINT('Ctrl Pts',(128.842235722353,-30.8927280682542,24.7509812734424));
#56335=CARTESIAN_POINT('Ctrl Pts',(132.800559523124,-31.7802224919666,24.553901820874));
#56336=CARTESIAN_POINT('Ctrl Pts',(134.228093727952,-35.5773424212951,24.3568223683055));
#56337=CARTESIAN_POINT('Ctrl Pts',(131.834814438577,-38.8527336814015,24.1597429157371));
#56338=CARTESIAN_POINT('Ctrl Pts',(127.783463162773,-38.6465141290025,23.9626634631686));
#56339=CARTESIAN_POINT('Ctrl Pts',(125.735136039938,-35.1450387740152,23.7655840106002));
#56340=CARTESIAN_POINT('Ctrl Pts',(127.540850671631,-31.5124958172661,23.5685045580317));
#56341=CARTESIAN_POINT('Ctrl Pts',(131.568831776746,-31.0315156923496,23.3714251054633));
#56342=CARTESIAN_POINT('Ctrl Pts',(134.179102204562,-34.1367470778341,23.1743456528949));
#56343=CARTESIAN_POINT('Ctrl Pts',(133.01283144756,-38.0220766887047,22.9772662003264));
#56344=CARTESIAN_POINT('Ctrl Pts',(129.123946720453,-39.1764376560859,22.780186747758));
#56345=CARTESIAN_POINT('Ctrl Pts',(126.026727554125,-36.5566653187652,22.5831072951895));
#56346=CARTESIAN_POINT('Ctrl Pts',(126.520046808689,-32.5301768018372,22.3860278426211));
#56347=CARTESIAN_POINT('Ctrl Pts',(130.158105269193,-30.7356004446776,22.1889483900526));
#56348=CARTESIAN_POINT('Ctrl Pts',(133.653288291002,-32.7946461719973,21.9918689374842));
#56349=CARTESIAN_POINT('Ctrl Pts',(133.847093884055,-36.8466102707053,21.7947894849158));
#56350=CARTESIAN_POINT('Ctrl Pts',(130.564385196142,-39.2298428093826,21.5977100323473));
#56351=CARTESIAN_POINT('Ctrl Pts',(126.771656931919,-37.7906812573025,21.4006305797789));
#56352=CARTESIAN_POINT('Ctrl Pts',(125.896294636564,-33.8296568281313,21.2035511272104));
#56353=CARTESIAN_POINT('Ctrl Pts',(128.729339449638,-30.926239748048,21.006471674642));
#56354=CARTESIAN_POINT('Ctrl Pts',(132.710645695734,-31.7041691830945,20.8093922220735));
#56355=CARTESIAN_POINT('Ctrl Pts',(134.24241503727,-35.4604514494443,20.6123127695051));
#56356=CARTESIAN_POINT('Ctrl Pts',(131.940429091694,-38.8006362116395,20.4152333169367));
#56357=CARTESIAN_POINT('Ctrl Pts',(127.884930095563,-38.7062892966865,20.2181538643682));
#56358=CARTESIAN_POINT('Ctrl Pts',(125.740762278213,-35.262669245549,20.0210744117998));
#56359=CARTESIAN_POINT('Ctrl Pts',(127.445552065305,-31.5816824143429,19.8239949592313));
#56360=CARTESIAN_POINT('Ctrl Pts',(131.458726822532,-30.9897357769423,19.6269155066629));
#56361=CARTESIAN_POINT('Ctrl Pts',(134.153690310275,-34.0217572430586,19.4298360540945));
#56362=CARTESIAN_POINT('Ctrl Pts',(133.09507551359,-37.9377876066188,19.232756601526));
#56363=CARTESIAN_POINT('Ctrl Pts',(129.239527372196,-39.1990242919515,19.0356771489576));
#56364=CARTESIAN_POINT('Ctrl Pts',(126.071192824932,-36.6657059661847,18.8385976963891));
#56365=CARTESIAN_POINT('Ctrl Pts',(126.453224713474,-32.6271566782553,18.6415182438207));
#56366=CARTESIAN_POINT('Ctrl Pts',(130.040360287586,-30.7328353676494,18.4444387912522));
#56367=CARTESIAN_POINT('Ctrl Pts',(133.59106645504,-32.694730217673,18.2473593386838));
#56368=CARTESIAN_POINT('Ctrl Pts',(133.896534255584,-36.7396375602231,18.0502798861154));
#56369=CARTESIAN_POINT('Ctrl Pts',(130.680994177302,-39.2128895708112,17.8532004335469));
#56370=CARTESIAN_POINT('Ctrl Pts',(126.849676803589,-37.8782239995245,17.6561209809785));
#56371=CARTESIAN_POINT('Ctrl Pts',(125.866008696645,-33.9443305187691,17.45904152841));
#56372=CARTESIAN_POINT('Ctrl Pts',(128.616463108536,-30.9608005594124,17.2619620758416));
#56373=CARTESIAN_POINT('Ctrl Pts',(132.62140443746,-31.6350567216393,17.0648359543957));
#56374=CARTESIAN_POINT('Ctrl Pts',(133.703873196701,-34.1017291832583,16.933402983806));
#56375=CARTESIAN_POINT('Ctrl Pts',(133.606792907386,-35.293582370418,16.8676631640724));
#56376=CARTESIAN_POINT('Ctrl Pts',(129.123724857835,-38.2682205206892,30.4049215251131));
#56377=CARTESIAN_POINT('Ctrl Pts',(128.044526438856,-37.9788658880908,30.3392283742569));
#56378=CARTESIAN_POINT('Ctrl Pts',(126.213383853024,-36.251289898127,30.2078420725446));
#56379=CARTESIAN_POINT('Ctrl Pts',(126.876946500719,-32.5131402892986,30.0107626199762));
#56380=CARTESIAN_POINT('Ctrl Pts',(130.368315541801,-31.0275405355875,29.8136831674077));
#56381=CARTESIAN_POINT('Ctrl Pts',(133.524181884943,-33.1291529817175,29.6166037148393));
#56382=CARTESIAN_POINT('Ctrl Pts',(133.496630262981,-36.9226407948612,29.4195242622709));
#56383=CARTESIAN_POINT('Ctrl Pts',(130.30864550685,-38.9780895429767,29.2224448097024));
#56384=CARTESIAN_POINT('Ctrl Pts',(126.842047557774,-37.4389372113975,29.025365357134));
#56385=CARTESIAN_POINT('Ctrl Pts',(126.2290597716,-33.6956431288561,28.8282859045656));
#56386=CARTESIAN_POINT('Ctrl Pts',(129.023838724806,-31.1311288239135,28.6312064519971));
#56387=CARTESIAN_POINT('Ctrl Pts',(132.700714054484,-32.0627755224524,28.4341269994287));
#56388=CARTESIAN_POINT('Ctrl Pts',(133.937043895626,-35.6487280957953,28.2370475468602));
#56389=CARTESIAN_POINT('Ctrl Pts',(131.615566110593,-38.6484350309798,28.0399680942918));
#56390=CARTESIAN_POINT('Ctrl Pts',(127.83414894952,-38.3511540065717,27.8428886417233));
#56391=CARTESIAN_POINT('Ctrl Pts',(126.009950710905,-35.0255243084067,27.6458091891549));
#56392=CARTESIAN_POINT('Ctrl Pts',(127.791452570794,-31.6768298530648,27.4487297365864));
#56393=CARTESIAN_POINT('Ctrl Pts',(131.568758337451,-31.3311936043443,27.251650284018));
#56394=CARTESIAN_POINT('Ctrl Pts',(133.928420002278,-34.3009582770079,27.0545708314495));
#56395=CARTESIAN_POINT('Ctrl Pts',(132.738075079866,-37.9024278752581,26.8574913788811));
#56396=CARTESIAN_POINT('Ctrl Pts',(129.073406105405,-38.8810522612381,26.6604119263127));
#56397=CARTESIAN_POINT('Ctrl Pts',(126.246074849402,-36.3524750801548,26.4633324737443));
#56398=CARTESIAN_POINT('Ctrl Pts',(126.811063831112,-32.6017029047084,26.2662530211758));
#56399=CARTESIAN_POINT('Ctrl Pts',(130.257807832163,-31.0182066866501,26.0691735686074));
#56400=CARTESIAN_POINT('Ctrl Pts',(133.471577898372,-33.0329489686482,25.8720941160389));
#56401=CARTESIAN_POINT('Ctrl Pts',(133.548177282174,-36.8252618540159,25.6750146634705));
#56402=CARTESIAN_POINT('Ctrl Pts',(130.418385202298,-38.9681351648467,25.477935210902));
#56403=CARTESIAN_POINT('Ctrl Pts',(126.910509775443,-37.5251124758535,25.2808557583336));
#56404=CARTESIAN_POINT('Ctrl Pts',(126.194522774053,-33.8002142083307,25.0837763057651));
#56405=CARTESIAN_POINT('Ctrl Pts',(128.917442209478,-31.1595297822324,24.8866968531967));
#56406=CARTESIAN_POINT('Ctrl Pts',(132.61863972495,-31.9893740095791,24.6896174006282));
#56407=CARTESIAN_POINT('Ctrl Pts',(133.953443626322,-35.5398391952819,24.4925379480598));
#56408=CARTESIAN_POINT('Ctrl Pts',(131.715627872607,-38.6024663587646,24.2954584954914));
#56409=CARTESIAN_POINT('Ctrl Pts',(127.927445795795,-38.4096424935639,24.0983790429229));
#56410=CARTESIAN_POINT('Ctrl Pts',(126.012174676128,-35.1356172908157,23.9012995903545));
#56411=CARTESIAN_POINT('Ctrl Pts',(127.700593018045,-31.7390384248466,23.704220137786));
#56412=CARTESIAN_POINT('Ctrl Pts',(131.466923012502,-31.2893019876745,23.5071406852176));
#56413=CARTESIAN_POINT('Ctrl Pts',(133.907634512722,-34.1928225856305,23.3100612326491));
#56414=CARTESIAN_POINT('Ctrl Pts',(132.81712280993,-37.8257674952256,23.1129817800807));
#56415=CARTESIAN_POINT('Ctrl Pts',(129.180853718675,-38.9051430489881,22.9159023275123));
#56416=CARTESIAN_POINT('Ctrl Pts',(126.284824879133,-36.4555468678715,22.7188228749439));
#56417=CARTESIAN_POINT('Ctrl Pts',(126.74609891613,-32.6906125054973,22.5217434223754));
#56418=CARTESIAN_POINT('Ctrl Pts',(130.147835007688,-31.012608913889,22.324663969807));
#56419=CARTESIAN_POINT('Ctrl Pts',(133.415976617003,-32.9379023749022,22.1275845172385));
#56420=CARTESIAN_POINT('Ctrl Pts',(133.597192913494,-36.7266574666393,21.9305050646701));
#56421=CARTESIAN_POINT('Ctrl Pts',(130.527723650431,-38.9550790902631,21.7334256121016));
#56422=CARTESIAN_POINT('Ctrl Pts',(126.981364854401,-37.609403135233,21.5363461595332));
#56423=CARTESIAN_POINT('Ctrl Pts',(126.162864672058,-33.9056804197966,21.3392667069647));
#56424=CARTESIAN_POINT('Ctrl Pts',(128.811879495282,-31.1908645977338,21.1421872543962));
#56425=CARTESIAN_POINT('Ctrl Pts',(132.534566553757,-31.9182610001316,20.9451078018278));
#56426=CARTESIAN_POINT('Ctrl Pts',(133.966834646645,-35.4305412711174,20.7480283492594));
#56427=CARTESIAN_POINT('Ctrl Pts',(131.814381969389,-38.5537530560258,20.550948896691));
#56428=CARTESIAN_POINT('Ctrl Pts',(128.022321601425,-38.4655347634374,20.3538694441225));
#56429=CARTESIAN_POINT('Ctrl Pts',(126.017435443101,-35.2456066779649,20.1567899915541));
#56430=CARTESIAN_POINT('Ctrl Pts',(127.61148485441,-31.8037307729446,19.9597105389856));
#56431=CARTESIAN_POINT('Ctrl Pts',(131.36397029729,-31.2502360277164,19.7626310864172));
#56432=CARTESIAN_POINT('Ctrl Pts',(133.883873333817,-34.0853023037645,19.5655516338488));
#56433=CARTESIAN_POINT('Ctrl Pts',(132.894024435006,-37.7469536950163,19.3684721812803));
#56434=CARTESIAN_POINT('Ctrl Pts',(129.288926438999,-38.9262624936712,19.1713927287119));
#56435=CARTESIAN_POINT('Ctrl Pts',(126.326401758165,-36.5575044119299,18.9743132761434));
#56436=CARTESIAN_POINT('Ctrl Pts',(126.683617475693,-32.7812927266503,18.777233823575));
#56437=CARTESIAN_POINT('Ctrl Pts',(130.037738548853,-31.0100234517737,18.5801543710065));
#56438=CARTESIAN_POINT('Ctrl Pts',(133.357796610448,-32.844476798695,18.3830749184381));
#56439=CARTESIAN_POINT('Ctrl Pts',(133.643421718785,-36.6266335296934,18.1859954658697));
#56440=CARTESIAN_POINT('Ctrl Pts',(130.636757901562,-38.9392271065351,17.9889160133012));
#56441=CARTESIAN_POINT('Ctrl Pts',(127.054316681922,-37.6912592431004,17.7918365607328));
#56442=CARTESIAN_POINT('Ctrl Pts',(126.134546057608,-34.0129050937345,17.5947571081642));
#56443=CARTESIAN_POINT('Ctrl Pts',(128.706335417974,-31.223180394923,17.3976776555959));
#56444=CARTESIAN_POINT('Ctrl Pts',(132.451122262682,-31.8536379719255,17.20055153415));
#56445=CARTESIAN_POINT('Ctrl Pts',(133.463275609383,-34.160079396613,17.0691185635602));
#56446=CARTESIAN_POINT('Ctrl Pts',(133.372501497992,-35.274511736449,17.0033787438267));
#56447=CARTESIAN_POINT('',(127.424194268159,-32.7919560716439,30.0017032878335));
#56448=CARTESIAN_POINT('Ctrl Pts',(127.426413829439,-32.7938587340794,30.0017032878335));
#56449=CARTESIAN_POINT('Ctrl Pts',(127.438461137846,-32.7798048805081,30.0011355252223));
#56450=CARTESIAN_POINT('Ctrl Pts',(127.450623566855,-32.7658497111731,30.0005677626112));
#56451=CARTESIAN_POINT('Ctrl Pts',(127.462899484434,-32.7519950986681,30.));
#56452=CARTESIAN_POINT('Ctrl Pts',(128.942095577027,-38.9456385074984,30.));
#56453=CARTESIAN_POINT('Ctrl Pts',(128.82630386935,-38.9038806817832,30.));
#56454=CARTESIAN_POINT('Ctrl Pts',(128.712884526443,-38.8565769348122,30.));
#56455=CARTESIAN_POINT('Ctrl Pts',(128.602063029409,-38.8040859693868,30.));
#56456=CARTESIAN_POINT('Ctrl Pts',(128.48644207688,-38.7493217261301,30.));
#56457=CARTESIAN_POINT('Ctrl Pts',(128.373648076022,-38.6889108098624,29.9999999999999));
#56458=CARTESIAN_POINT('Ctrl Pts',(128.263966932901,-38.6232096796844,29.9999999999999));
#56459=CARTESIAN_POINT('Ctrl Pts',(128.15428578978,-38.5575085495065,29.9999999999999));
#56460=CARTESIAN_POINT('Ctrl Pts',(128.047716901034,-38.4865164045163,30.));
#56461=CARTESIAN_POINT('Ctrl Pts',(127.944585645469,-38.4105498139686,30.));
#56462=CARTESIAN_POINT('Ctrl Pts',(127.85193017975,-38.3422997011609,30.0000000000001));
#56463=CARTESIAN_POINT('Ctrl Pts',(127.762049656311,-38.2700334897146,29.9999999999999));
#56464=CARTESIAN_POINT('Ctrl Pts',(127.675213227679,-38.1939612063097,29.9999999999999));
#56465=CARTESIAN_POINT('Ctrl Pts',(127.658100651142,-38.1789698853557,29.9999999999999));
#56466=CARTESIAN_POINT('Ctrl Pts',(127.641106400836,-38.1638307099299,30.0000000000001));
#56467=CARTESIAN_POINT('Ctrl Pts',(127.624232699747,-38.1485452275119,30.));
#56468=CARTESIAN_POINT('Ctrl Pts',(127.613106149663,-38.1384659517932,30.));
#56469=CARTESIAN_POINT('Ctrl Pts',(127.602033315642,-38.1283241907556,30.0000000000001));
#56470=CARTESIAN_POINT('Ctrl Pts',(127.59102153458,-38.1181267915428,30.0000000000001));
#56471=CARTESIAN_POINT('Ctrl Pts',(127.500544559117,-38.0343410866547,29.9999999999998));
#56472=CARTESIAN_POINT('Ctrl Pts',(127.414055491681,-37.9466844892944,30.0000000000001));
#56473=CARTESIAN_POINT('Ctrl Pts',(127.331810952627,-37.855473172009,30.0000000000001));
#56474=CARTESIAN_POINT('Ctrl Pts',(127.25026281251,-37.7650341791259,30.));
#56475=CARTESIAN_POINT('Ctrl Pts',(127.172887189515,-37.671099663786,29.9999999999999));
#56476=CARTESIAN_POINT('Ctrl Pts',(127.099976041161,-37.5739493940444,30.));
#56477=CARTESIAN_POINT('Ctrl Pts',(127.027475603359,-37.4773463745078,30.0000000000001));
#56478=CARTESIAN_POINT('Ctrl Pts',(126.959389056289,-37.3775630490853,30.0000000000001));
#56479=CARTESIAN_POINT('Ctrl Pts',(126.896051405949,-37.2748568041853,29.9999999999999));
#56480=CARTESIAN_POINT('Ctrl Pts',(126.843495295564,-37.1896335488993,29.9999999999998));
#56481=CARTESIAN_POINT('Ctrl Pts',(126.794209667284,-37.1023972880374,30.0000000000002));
#56482=CARTESIAN_POINT('Ctrl Pts',(126.748414412018,-37.0132907019563,30.0000000000001));
#56483=CARTESIAN_POINT('Ctrl Pts',(126.738572960238,-36.9941415965499,30.0000000000001));
#56484=CARTESIAN_POINT('Ctrl Pts',(126.728892803937,-36.9749061092015,29.9999999999999));
#56485=CARTESIAN_POINT('Ctrl Pts',(126.719376295068,-36.9555856509566,30.));
#56486=CARTESIAN_POINT('Ctrl Pts',(126.712231453978,-36.9410801630899,30.));
#56487=CARTESIAN_POINT('Ctrl Pts',(126.705179730846,-36.9265284390521,30.));
#56488=CARTESIAN_POINT('Ctrl Pts',(126.698226860057,-36.9119414822678,30.));
#56489=CARTESIAN_POINT('Ctrl Pts',(126.647942792783,-36.8064467106005,30.0000000000001));
#56490=CARTESIAN_POINT('Ctrl Pts',(126.602751084607,-36.6989610097156,30.0000000000001));
#56491=CARTESIAN_POINT('Ctrl Pts',(126.562915840835,-36.5897363849447,30.0000000000001));
#56492=CARTESIAN_POINT('Ctrl Pts',(126.523317774394,-36.4811620789004,30.0000000000001));
#56493=CARTESIAN_POINT('Ctrl Pts',(126.489012229666,-36.3708688756739,30.));
#56494=CARTESIAN_POINT('Ctrl Pts',(126.460308487673,-36.2590933458545,29.9999999999999));
#56495=CARTESIAN_POINT('Ctrl Pts',(126.452959393802,-36.2304751656402,29.9999999999998));
#56496=CARTESIAN_POINT('Ctrl Pts',(126.445977784055,-36.2017597851064,29.9999999999999));
#56497=CARTESIAN_POINT('Ctrl Pts',(126.439369421695,-36.1729511329457,29.9999999999999));
#56498=CARTESIAN_POINT('Ctrl Pts',(126.412872256441,-36.0574387600593,29.9999999999999));
#56499=CARTESIAN_POINT('Ctrl Pts',(126.392371897484,-35.9404260397136,30.));
#56500=CARTESIAN_POINT('Ctrl Pts',(126.377781991937,-35.8223498160256,29.9999999999999));
#56501=CARTESIAN_POINT('Ctrl Pts',(126.369641629914,-35.7564698002806,29.9999999999999));
#56502=CARTESIAN_POINT('Ctrl Pts',(126.363342135217,-35.6902588634788,30.0000000000001));
#56503=CARTESIAN_POINT('Ctrl Pts',(126.358875193738,-35.6237950595802,29.9999999999999));
#56504=CARTESIAN_POINT('Ctrl Pts',(126.357510944051,-35.6034963330169,29.9999999999998));
#56505=CARTESIAN_POINT('Ctrl Pts',(126.356317658871,-35.5831740353541,29.9999999999999));
#56506=CARTESIAN_POINT('Ctrl Pts',(126.355295185526,-35.5628304336442,30.));
#56507=CARTESIAN_POINT('Ctrl Pts',(126.35456734149,-35.5483489126842,30.0000000000001));
#56508=CARTESIAN_POINT('Ctrl Pts',(126.353926172819,-35.5338582350463,30.0000000000001));
#56509=CARTESIAN_POINT('Ctrl Pts',(126.353371824647,-35.5193686343449,30.0000000000001));
#56510=CARTESIAN_POINT('Ctrl Pts',(126.348947576412,-35.403727249526,30.0000000000001));
#56511=CARTESIAN_POINT('Ctrl Pts',(126.350040249793,-35.2879868021222,29.9999999999999));
#56512=CARTESIAN_POINT('Ctrl Pts',(126.356503368941,-35.1725471859202,30.0000000000001));
#56513=CARTESIAN_POINT('Ctrl Pts',(126.363113237002,-35.0544864454716,30.0000000000002));
#56514=CARTESIAN_POINT('Ctrl Pts',(126.375340363165,-34.9367393586674,30.0000000000002));
#56515=CARTESIAN_POINT('Ctrl Pts',(126.393082724363,-34.8197437025802,30.0000000000002));
#56516=CARTESIAN_POINT('Ctrl Pts',(126.410825085562,-34.702748046493,30.0000000000002));
#56517=CARTESIAN_POINT('Ctrl Pts',(126.434083043154,-34.5865028570309,30.));
#56518=CARTESIAN_POINT('Ctrl Pts',(126.462804329437,-34.4714705833518,29.9999999999999));
#56519=CARTESIAN_POINT('Ctrl Pts',(126.481403635652,-34.3969780811092,29.9999999999998));
#56520=CARTESIAN_POINT('Ctrl Pts',(126.502295031583,-34.3229947638336,30.0000000000002));
#56521=CARTESIAN_POINT('Ctrl Pts',(126.525474385826,-34.2496546116183,30.0000000000001));
#56522=CARTESIAN_POINT('Ctrl Pts',(126.53257453879,-34.2271895207573,30.));
#56523=CARTESIAN_POINT('Ctrl Pts',(126.539889419495,-34.2047848317409,30.0000000000002));
#56524=CARTESIAN_POINT('Ctrl Pts',(126.547419047006,-34.1824445482406,30.0000000000001));
#56525=CARTESIAN_POINT('Ctrl Pts',(126.553170483406,-34.1653801291155,30.0000000000001));
#56526=CARTESIAN_POINT('Ctrl Pts',(126.559046987838,-34.1483541612293,30.));
#56527=CARTESIAN_POINT('Ctrl Pts',(126.565044083677,-34.1313805413347,30.));
#56528=CARTESIAN_POINT('Ctrl Pts',(126.602641717811,-34.0249677095538,30.0000000000001));
#56529=CARTESIAN_POINT('Ctrl Pts',(126.645018327222,-33.9204820438248,29.9999999999998));
#56530=CARTESIAN_POINT('Ctrl Pts',(126.69210907066,-33.8183255357337,30.));
#56531=CARTESIAN_POINT('Ctrl Pts',(126.732414546534,-33.7308886772017,30.0000000000001));
#56532=CARTESIAN_POINT('Ctrl Pts',(126.776174342542,-33.6451582292905,29.9999999999999));
#56533=CARTESIAN_POINT('Ctrl Pts',(126.823370536012,-33.5614064352205,29.9999999999999));
#56534=CARTESIAN_POINT('Ctrl Pts',(126.844837231283,-33.5233128071232,29.9999999999999));
#56535=CARTESIAN_POINT('Ctrl Pts',(126.867015116863,-33.4856288122295,29.9999999999999));
#56536=CARTESIAN_POINT('Ctrl Pts',(126.889903809861,-33.448381667042,30.));
#56537=CARTESIAN_POINT('Ctrl Pts',(126.903889653885,-33.4256222738776,30.0000000000001));
#56538=CARTESIAN_POINT('Ctrl Pts',(126.9181432011,-33.4030226799343,29.9999999999998));
#56539=CARTESIAN_POINT('Ctrl Pts',(126.932649322486,-33.3806120942224,29.9999999999998));
#56540=CARTESIAN_POINT('Ctrl Pts',(126.991212030765,-33.2901382481445,29.9999999999998));
#56541=CARTESIAN_POINT('Ctrl Pts',(127.053930677688,-33.2026705753962,29.9999999999999));
#56542=CARTESIAN_POINT('Ctrl Pts',(127.120768947966,-33.1185902784384,30.));
#56543=CARTESIAN_POINT('Ctrl Pts',(127.187607218243,-33.0345099814805,30.));
#56544=CARTESIAN_POINT('Ctrl Pts',(127.258565397579,-32.9538164052713,29.9999999999999));
#56545=CARTESIAN_POINT('Ctrl Pts',(127.333638398083,-32.8769328424591,30.));
#56546=CARTESIAN_POINT('Ctrl Pts',(127.362444874375,-32.8474316301123,30.));
#56547=CARTESIAN_POINT('Ctrl Pts',(127.391857525546,-32.8184918975039,29.9999999999999));
#56548=CARTESIAN_POINT('Ctrl Pts',(127.421855683173,-32.7901223422051,29.9999999999999));
#56549=CARTESIAN_POINT('Origin',(-10.,-35.,17.));
#56550=CARTESIAN_POINT('Ctrl Pts',(-6.62123117139838,-35.2726284383003,
17.));
#56551=CARTESIAN_POINT('Ctrl Pts',(-6.60195936274602,-35.1678051036246,
17.));
#56552=CARTESIAN_POINT('Ctrl Pts',(-6.58807248374327,-35.0622614892112,
17.));
#56553=CARTESIAN_POINT('Ctrl Pts',(-6.57934242661586,-34.9563326165135,
17.));
#56554=CARTESIAN_POINT('Ctrl Pts',(-6.57037153216212,-34.8474814689544,
17.));
#56555=CARTESIAN_POINT('Ctrl Pts',(-6.56684579918875,-34.7382228961907,
17.));
#56556=CARTESIAN_POINT('Ctrl Pts',(-6.56856914163975,-34.6289004249964,
17.));
#56557=CARTESIAN_POINT('Ctrl Pts',(-6.56942711098046,-34.5744740232787,
17.));
#56558=CARTESIAN_POINT('Ctrl Pts',(-6.57158689612088,-34.5200315365156,
17.));
#56559=CARTESIAN_POINT('Ctrl Pts',(-6.57502897084565,-34.465614347352,17.));
#56560=CARTESIAN_POINT('Ctrl Pts',(-6.57632076661394,-34.4451918114384,
17.));
#56561=CARTESIAN_POINT('Ctrl Pts',(-6.57779265782301,-34.4247816698274,
17.));
#56562=CARTESIAN_POINT('Ctrl Pts',(-6.57944296507798,-34.4043890422814,
17.));
#56563=CARTESIAN_POINT('Ctrl Pts',(-6.58842189201816,-34.2934376347159,
17.));
#56564=CARTESIAN_POINT('Ctrl Pts',(-6.60267989553898,-34.1829782686288,
17.));
#56565=CARTESIAN_POINT('Ctrl Pts',(-6.62200581466125,-34.0733656510403,
17.));
#56566=CARTESIAN_POINT('Ctrl Pts',(-6.64170770786029,-33.9616205862218,
17.));
#56567=CARTESIAN_POINT('Ctrl Pts',(-6.66667661424612,-33.8507547385056,
17.));
#56568=CARTESIAN_POINT('Ctrl Pts',(-6.69674188079343,-33.7411363045331,
17.));
#56569=CARTESIAN_POINT('Ctrl Pts',(-6.70213413683576,-33.7214760543234,
17.));
#56570=CARTESIAN_POINT('Ctrl Pts',(-6.7076904628942,-33.7018559288903,17.));
#56571=CARTESIAN_POINT('Ctrl Pts',(-6.71341005038338,-33.6822780588274,
17.));
#56572=CARTESIAN_POINT('Ctrl Pts',(-6.7206963490438,-33.6573374125511,17.));
#56573=CARTESIAN_POINT('Ctrl Pts',(-6.72824940271889,-33.6324599742726,
17.));
#56574=CARTESIAN_POINT('Ctrl Pts',(-6.7360574985804,-33.6076813199021,17.));
#56575=CARTESIAN_POINT('Ctrl Pts',(-6.77081749559188,-33.4973719734054,
17.));
#56576=CARTESIAN_POINT('Ctrl Pts',(-6.81065448189253,-33.3889213989467,
17.));
#56577=CARTESIAN_POINT('Ctrl Pts',(-6.85534159827004,-33.2827019280528,
17.));
#56578=CARTESIAN_POINT('Ctrl Pts',(-6.90044356785989,-33.1754963678275,
17.));
#56579=CARTESIAN_POINT('Ctrl Pts',(-6.95048625969968,-33.0705626493514,
17.));
#56580=CARTESIAN_POINT('Ctrl Pts',(-7.00528986546843,-32.9682816440293,
17.));
#56581=CARTESIAN_POINT('Ctrl Pts',(-7.05981998464246,-32.8665110519083,
17.));
#56582=CARTESIAN_POINT('Ctrl Pts',(-7.11906386156907,-32.7673658768366,
17.));
#56583=CARTESIAN_POINT('Ctrl Pts',(-7.18289409730164,-32.671232657024,17.));
#56584=CARTESIAN_POINT('Ctrl Pts',(-7.22018368206598,-32.6150716886722,
17.));
#56585=CARTESIAN_POINT('Ctrl Pts',(-7.25903945429618,-32.5599389460292,
17.));
#56586=CARTESIAN_POINT('Ctrl Pts',(-7.29944343578837,-32.5059151540895,
17.));
#56587=CARTESIAN_POINT('Ctrl Pts',(-7.32106075068243,-32.4770108412222,
17.));
#56588=CARTESIAN_POINT('Ctrl Pts',(-7.34312134161498,-32.448424027476,17.));
#56589=CARTESIAN_POINT('Ctrl Pts',(-7.36562307324715,-32.4201675125236,
17.));
#56590=CARTESIAN_POINT('Ctrl Pts',(-7.37557070373355,-32.4076757908119,
17.));
#56591=CARTESIAN_POINT('Ctrl Pts',(-7.3856037462521,-32.39524973087,17.));
#56592=CARTESIAN_POINT('Ctrl Pts',(-7.39571409769092,-32.3828998151529,
17.));
#56593=CARTESIAN_POINT('Ctrl Pts',(-7.47117758841242,-32.2907202548503,
17.));
#56594=CARTESIAN_POINT('Ctrl Pts',(-7.55105817840693,-32.2026374053398,
17.));
#56595=CARTESIAN_POINT('Ctrl Pts',(-7.63516588800145,-32.1190387156275,
17.));
#56596=CARTESIAN_POINT('Ctrl Pts',(-7.65864346748547,-32.0957032224611,
17.));
#56597=CARTESIAN_POINT('Ctrl Pts',(-7.68245071568654,-32.0727172019008,
17.));
#56598=CARTESIAN_POINT('Ctrl Pts',(-7.70658419094811,-32.0500893063318,
17.));
#56599=CARTESIAN_POINT('Ctrl Pts',(-7.79064406788299,-31.9712735495372,
17.));
#56600=CARTESIAN_POINT('Ctrl Pts',(-7.87865820844732,-31.8968001233851,
17.));
#56601=CARTESIAN_POINT('Ctrl Pts',(-7.97020004902603,-31.8266803948519,
17.));
#56602=CARTESIAN_POINT('Ctrl Pts',(-8.06174188960474,-31.7565606663187,
17.));
#56603=CARTESIAN_POINT('Ctrl Pts',(-8.15681210589746,-31.6907943583393,
17.));
#56604=CARTESIAN_POINT('Ctrl Pts',(-8.2550244894812,-31.6294268457453,17.));
#56605=CARTESIAN_POINT('Ctrl Pts',(-8.31110600223239,-31.5943845953236,
17.));
#56606=CARTESIAN_POINT('Ctrl Pts',(-8.36821275697467,-31.5607772919423,
17.));
#56607=CARTESIAN_POINT('Ctrl Pts',(-8.4262774446775,-31.5286188972515,17.));
#56608=CARTESIAN_POINT('Ctrl Pts',(-8.44233628183896,-31.5197249129016,
17.));
#56609=CARTESIAN_POINT('Ctrl Pts',(-8.45846840796252,-31.5109417802214,
17.));
#56610=CARTESIAN_POINT('Ctrl Pts',(-8.47467243570209,-31.5022698523055,
17.));
#56611=CARTESIAN_POINT('Ctrl Pts',(-8.48766853586036,-31.495314714634,17.));
#56612=CARTESIAN_POINT('Ctrl Pts',(-8.50071001765182,-31.4884316194093,
17.));
#56613=CARTESIAN_POINT('Ctrl Pts',(-8.51378706273541,-31.4816253310382,
17.));
#56614=CARTESIAN_POINT('Ctrl Pts',(-8.61982624789618,-31.4264344780416,
17.));
#56615=CARTESIAN_POINT('Ctrl Pts',(-8.72835801098144,-31.3762061453459,
17.));
#56616=CARTESIAN_POINT('Ctrl Pts',(-8.83892749372354,-31.3309409256438,
17.));
#56617=CARTESIAN_POINT('Ctrl Pts',(-8.95138481870543,-31.2849028562219,
17.));
#56618=CARTESIAN_POINT('Ctrl Pts',(-9.06595070186539,-31.2439984397476,
17.));
#56619=CARTESIAN_POINT('Ctrl Pts',(-9.18218640297054,-31.208266008192,17.));
#56620=CARTESIAN_POINT('Ctrl Pts',(-9.29985863077184,-31.1720919688398,
17.));
#56621=CARTESIAN_POINT('Ctrl Pts',(-9.41924298093842,-31.1412181424403,
17.));
#56622=CARTESIAN_POINT('Ctrl Pts',(-9.53991371679841,-31.1157285615814,
17.));
#56623=CARTESIAN_POINT('Ctrl Pts',(-9.61457871346185,-31.0999568878925,
17.));
#56624=CARTESIAN_POINT('Ctrl Pts',(-9.68973674093548,-31.0862474736742,
17.));
#56625=CARTESIAN_POINT('Ctrl Pts',(-9.76529045541688,-31.0746295822446,
17.));
#56626=CARTESIAN_POINT('Ctrl Pts',(-9.80157333625044,-31.0690503652177,
17.));
#56627=CARTESIAN_POINT('Ctrl Pts',(-9.83794749841506,-31.0639535993401,
17.));
#56628=CARTESIAN_POINT('Ctrl Pts',(-9.87440228076019,-31.0593431503807,
17.));
#56629=CARTESIAN_POINT('Ctrl Pts',(-9.89072382555558,-31.0572789589529,
17.));
#56630=CARTESIAN_POINT('Ctrl Pts',(-9.90706204440871,-31.0553121984509,
17.));
#56631=CARTESIAN_POINT('Ctrl Pts',(-9.9234144236545,-31.0534434210371,17.));
#56632=CARTESIAN_POINT('Ctrl Pts',(-10.0491353854642,-31.0390758179906,
17.));
#56633=CARTESIAN_POINT('Ctrl Pts',(-10.1751595106833,-31.0305566396611,
17.));
#56634=CARTESIAN_POINT('Ctrl Pts',(-10.3010219327232,-31.0279204753263,
17.));
#56635=CARTESIAN_POINT('Ctrl Pts',(-10.4271451736567,-31.0252788481897,
17.));
#56636=CARTESIAN_POINT('Ctrl Pts',(-10.5531069280695,-31.0285443279939,
17.));
#56637=CARTESIAN_POINT('Ctrl Pts',(-10.6784621466317,-31.0377989166891,
17.));
#56638=CARTESIAN_POINT('Ctrl Pts',(-10.8015650460913,-31.04688722362,17.));
#56639=CARTESIAN_POINT('Ctrl Pts',(-10.924083889428,-31.061751209596,17.));
#56640=CARTESIAN_POINT('Ctrl Pts',(-11.0456058942539,-31.0825171502249,
17.));
#56641=CARTESIAN_POINT('Ctrl Pts',(-11.1383505538559,-31.0983655564268,
17.));
#56642=CARTESIAN_POINT('Ctrl Pts',(-11.2305148677362,-31.1176525692725,
17.));
#56643=CARTESIAN_POINT('Ctrl Pts',(-11.3219141163422,-31.1404548077392,
17.));
#56644=CARTESIAN_POINT('Ctrl Pts',(-11.3696276429971,-31.152358354316,17.));
#56645=CARTESIAN_POINT('Ctrl Pts',(-11.4171326273164,-31.165220183099,17.));
#56646=CARTESIAN_POINT('Ctrl Pts',(-11.4644130279462,-31.1790224515809,
17.));
#56647=CARTESIAN_POINT('Ctrl Pts',(-13.1750507821944,-32.4297320119321,
17.));
#56648=CARTESIAN_POINT('Ctrl Pts',(-13.2457830379296,-32.5339316716807,
17.));
#56649=CARTESIAN_POINT('Ctrl Pts',(-13.3111684320266,-32.6414695796738,
17.));
#56650=CARTESIAN_POINT('Ctrl Pts',(-13.3712014634247,-32.7519056634986,
17.));
#56651=CARTESIAN_POINT('Ctrl Pts',(-13.4312344948227,-32.8623417473234,
17.));
#56652=CARTESIAN_POINT('Ctrl Pts',(-13.4859151823647,-32.9756769087957,
17.));
#56653=CARTESIAN_POINT('Ctrl Pts',(-13.5351879905628,-33.0914857757907,
17.));
#56654=CARTESIAN_POINT('Ctrl Pts',(-13.5568745982239,-33.1424571239651,
17.));
#56655=CARTESIAN_POINT('Ctrl Pts',(-13.577512952621,-33.1939077821244,17.));
#56656=CARTESIAN_POINT('Ctrl Pts',(-13.5970952298849,-33.2458016998049,
17.));
#56657=CARTESIAN_POINT('Ctrl Pts',(-13.6073220395261,-33.2729032064631,
17.));
#56658=CARTESIAN_POINT('Ctrl Pts',(-13.6172620907691,-33.3001296513874,
17.));
#56659=CARTESIAN_POINT('Ctrl Pts',(-13.6269050370344,-33.3274493235186,
17.));
#56660=CARTESIAN_POINT('Ctrl Pts',(-13.6685917972946,-33.4455531261519,
17.));
#56661=CARTESIAN_POINT('Ctrl Pts',(-13.7047654844905,-33.5654872367405,
17.));
#56662=CARTESIAN_POINT('Ctrl Pts',(-13.7353853470909,-33.686824179545,17.));
#56663=CARTESIAN_POINT('Ctrl Pts',(-13.7610632945821,-33.7885778577618,
17.));
#56664=CARTESIAN_POINT('Ctrl Pts',(-13.7828345727888,-33.8913185884214,
17.));
#56665=CARTESIAN_POINT('Ctrl Pts',(-13.8006468889342,-33.9947943925399,
17.));
#56666=CARTESIAN_POINT('Ctrl Pts',(-13.8084972326622,-34.0403988284389,
17.));
#56667=CARTESIAN_POINT('Ctrl Pts',(-13.8155782548013,-34.0861460076211,
17.));
#56668=CARTESIAN_POINT('Ctrl Pts',(-13.8218838856489,-34.1320140579904,
17.));
#56669=CARTESIAN_POINT('Ctrl Pts',(-13.8245828861217,-34.151646969055,17.));
#56670=CARTESIAN_POINT('Ctrl Pts',(-13.8271398150965,-34.1713020216297,
17.));
#56671=CARTESIAN_POINT('Ctrl Pts',(-13.8295541419123,-34.1909774839374,
17.));
#56672=CARTESIAN_POINT('Ctrl Pts',(-13.8317972215008,-34.20925737364,17.));
#56673=CARTESIAN_POINT('Ctrl Pts',(-13.833916727226,-34.2275513035412,17.));
#56674=CARTESIAN_POINT('Ctrl Pts',(-13.835911424144,-34.2458481127575,17.));
#56675=CARTESIAN_POINT('Ctrl Pts',(-13.8491700107784,-34.3674655013118,
17.));
#56676=CARTESIAN_POINT('Ctrl Pts',(-13.8569344264697,-34.4893371723603,
17.));
#56677=CARTESIAN_POINT('Ctrl Pts',(-13.8591700411928,-34.611066101442,17.));
#56678=CARTESIAN_POINT('Ctrl Pts',(-13.8613878458839,-34.7318252766074,
17.));
#56679=CARTESIAN_POINT('Ctrl Pts',(-13.8581645033039,-34.8524448082591,
17.));
#56680=CARTESIAN_POINT('Ctrl Pts',(-13.8494158248468,-34.9725303958732,
17.));
#56681=CARTESIAN_POINT('Ctrl Pts',(-13.840878077774,-35.0897207097202,17.));
#56682=CARTESIAN_POINT('Ctrl Pts',(-13.8270780176714,-35.2064031908734,
17.));
#56683=CARTESIAN_POINT('Ctrl Pts',(-13.8078915167199,-35.3221939954455,
17.));
#56684=CARTESIAN_POINT('Ctrl Pts',(-13.7961959663632,-35.3927768072427,
17.));
#56685=CARTESIAN_POINT('Ctrl Pts',(-13.7824980530838,-35.4630279096876,
17.));
#56686=CARTESIAN_POINT('Ctrl Pts',(-13.7667614148585,-35.532855489557,17.));
#56687=CARTESIAN_POINT('Ctrl Pts',(-13.757216255672,-35.5752098574922,17.));
#56688=CARTESIAN_POINT('Ctrl Pts',(-13.7469209067431,-35.6174083281479,
17.));
#56689=CARTESIAN_POINT('Ctrl Pts',(-13.7358661344643,-35.6594295784058,
17.));
#56690=CARTESIAN_POINT('Ctrl Pts',(-13.7309267403395,-35.6782051362742,
17.));
#56691=CARTESIAN_POINT('Ctrl Pts',(-13.7258352371277,-35.6969467100214,
17.));
#56692=CARTESIAN_POINT('Ctrl Pts',(-13.7205966738498,-35.7156322006019,
17.));
#56693=CARTESIAN_POINT('Ctrl Pts',(-13.6893367538286,-35.8271335627347,
17.));
#56694=CARTESIAN_POINT('Ctrl Pts',(-13.6528018180032,-35.9368053180647,
17.));
#56695=CARTESIAN_POINT('Ctrl Pts',(-13.6109158237098,-36.0442928075802,
17.));
#56696=CARTESIAN_POINT('Ctrl Pts',(-13.5979435125947,-36.0775822442643,
17.));
#56697=CARTESIAN_POINT('Ctrl Pts',(-13.5844575975254,-36.1106620277172,
17.));
#56698=CARTESIAN_POINT('Ctrl Pts',(-13.5704548945751,-36.1435211813812,
17.));
#56699=CARTESIAN_POINT('Ctrl Pts',(-13.5245394274593,-36.2512677639423,
17.));
#56700=CARTESIAN_POINT('Ctrl Pts',(-13.4730705027225,-36.3566445855268,
17.));
#56701=CARTESIAN_POINT('Ctrl Pts',(-13.4163937309752,-36.4593820470852,
17.));
#56702=CARTESIAN_POINT('Ctrl Pts',(-13.3593202829442,-36.5628385600856,
17.));
#56703=CARTESIAN_POINT('Ctrl Pts',(-13.2969650692165,-36.6636192426463,
17.));
#56704=CARTESIAN_POINT('Ctrl Pts',(-13.2296453006718,-36.7614105285874,
17.));
#56705=CARTESIAN_POINT('Ctrl Pts',(-13.1959565268153,-36.8103481376796,
17.));
#56706=CARTESIAN_POINT('Ctrl Pts',(-13.1610239983712,-36.8585364607721,
17.));
#56707=CARTESIAN_POINT('Ctrl Pts',(-13.1248850662753,-36.9059319156406,
17.));
#56708=CARTESIAN_POINT('Ctrl Pts',(-13.1136839868388,-36.9206218974448,
17.));
#56709=CARTESIAN_POINT('Ctrl Pts',(-13.1023670038866,-36.9352356893667,
17.));
#56710=CARTESIAN_POINT('Ctrl Pts',(-13.0909352063088,-36.9497719323387,
17.));
#56711=CARTESIAN_POINT('Ctrl Pts',(-13.0810899908133,-36.9622907373281,
17.));
#56712=CARTESIAN_POINT('Ctrl Pts',(-13.0711625418207,-36.9747482535312,
17.));
#56713=CARTESIAN_POINT('Ctrl Pts',(-13.0611586777581,-36.9871376957437,
17.));
#56714=CARTESIAN_POINT('Ctrl Pts',(-12.9882938384087,-37.0773782978546,
17.));
#56715=CARTESIAN_POINT('Ctrl Pts',(-12.9112998416349,-37.1641103597806,
17.));
#56716=CARTESIAN_POINT('Ctrl Pts',(-12.8305219931231,-37.2470878105587,
17.));
#56717=CARTESIAN_POINT('Ctrl Pts',(-12.7496930685579,-37.3301177282046,
17.));
#56718=CARTESIAN_POINT('Ctrl Pts',(-12.6650746977764,-37.409388808979,17.));
#56719=CARTESIAN_POINT('Ctrl Pts',(-12.5769811318078,-37.4846132121967,
17.));
#56720=CARTESIAN_POINT('Ctrl Pts',(-12.4904409634934,-37.5585111461063,
17.));
#56721=CARTESIAN_POINT('Ctrl Pts',(-12.4005462848826,-37.6285042016323,
17.));
#56722=CARTESIAN_POINT('Ctrl Pts',(-12.3075763963486,-37.694273447211,17.));
#56723=CARTESIAN_POINT('Ctrl Pts',(-12.2551724160701,-37.731345345463,17.));
#56724=CARTESIAN_POINT('Ctrl Pts',(-12.2017911097264,-37.767074392327,17.));
#56725=CARTESIAN_POINT('Ctrl Pts',(-12.1474812222069,-37.8013962232141,
17.));
#56726=CARTESIAN_POINT('Ctrl Pts',(-12.1187449086064,-37.8195565056371,
17.));
#56727=CARTESIAN_POINT('Ctrl Pts',(-12.08974861503,-37.8373227245847,17.));
#56728=CARTESIAN_POINT('Ctrl Pts',(-12.0604995325634,-37.8546847045796,
17.));
#56729=CARTESIAN_POINT('Ctrl Pts',(-12.0426076402161,-37.8653051634387,
17.));
#56730=CARTESIAN_POINT('Ctrl Pts',(-12.024619808101,-37.8757749838419,17.));
#56731=CARTESIAN_POINT('Ctrl Pts',(-12.0065599568337,-37.8860794595539,
17.));
#56732=CARTESIAN_POINT('Ctrl Pts',(-11.9096687237166,-37.9413630465328,
17.));
#56733=CARTESIAN_POINT('Ctrl Pts',(-11.8105593158835,-37.9919798651834,
17.));
#56734=CARTESIAN_POINT('Ctrl Pts',(-11.7095166454714,-38.0376717971112,
17.));
#56735=CARTESIAN_POINT('Ctrl Pts',(-11.6099952290825,-38.0826758114,17.));
#56736=CARTESIAN_POINT('Ctrl Pts',(-11.5085976071889,-38.1229024009533,
17.));
#56737=CARTESIAN_POINT('Ctrl Pts',(-11.4055841475048,-38.1580565561197,
17.));
#56738=CARTESIAN_POINT('Ctrl Pts',(-11.3056451647854,-38.1921615217861,
17.));
#56739=CARTESIAN_POINT('Ctrl Pts',(-11.2041847596975,-38.2214924163805,
17.));
#56740=CARTESIAN_POINT('Ctrl Pts',(-11.101438968834,-38.2457313749553,17.));
#56741=CARTESIAN_POINT('Ctrl Pts',(-11.0378253219427,-38.2607385936338,
17.));
#56742=CARTESIAN_POINT('Ctrl Pts',(-10.9737189501175,-38.2737929603252,
17.));
#56743=CARTESIAN_POINT('Ctrl Pts',(-10.9091769854019,-38.2848089949374,
17.));
#56744=CARTESIAN_POINT('Ctrl Pts',(-10.8685412172475,-38.2917447154481,
17.));
#56745=CARTESIAN_POINT('Ctrl Pts',(-10.8277327929855,-38.2978722505483,
17.));
#56746=CARTESIAN_POINT('Ctrl Pts',(-10.7867735403064,-38.3031951868165,
17.));
#56747=CARTESIAN_POINT('Ctrl Pts',(-7.43281991866731,-32.7955655913445,
29.9966885573452));
#56748=CARTESIAN_POINT('Ctrl Pts',(-6.70433287707855,-33.6438343820474,
29.9309496672087));
#56749=CARTESIAN_POINT('Ctrl Pts',(-6.16680494687376,-36.1040434535625,
29.7995176262159));
#56750=CARTESIAN_POINT('Ctrl Pts',(-8.82688604484989,-38.8162402853805,
29.602392434367));
#56751=CARTESIAN_POINT('Ctrl Pts',(-12.5469213771536,-38.0704890626947,
29.4053129817986));
#56752=CARTESIAN_POINT('Ctrl Pts',(-13.9650986146378,-34.5542581135541,
29.2082335292301));
#56753=CARTESIAN_POINT('Ctrl Pts',(-11.8002655329401,-31.4387142292477,
29.0111540766617));
#56754=CARTESIAN_POINT('Ctrl Pts',(-8.00850995998504,-31.5424701940952,
28.8140746240932));
#56755=CARTESIAN_POINT('Ctrl Pts',(-6.01644574177587,-34.7701684626168,
28.6169951715248));
#56756=CARTESIAN_POINT('Ctrl Pts',(-7.62419332014188,-38.2058271295203,
28.4199157189564));
#56757=CARTESIAN_POINT('Ctrl Pts',(-11.378901931472,-38.7443323602222,28.2228362663879));
#56758=CARTESIAN_POINT('Ctrl Pts',(-13.8875297661741,-35.8992536493971,
28.0257568138195));
#56759=CARTESIAN_POINT('Ctrl Pts',(-12.8831047926849,-32.2415099196181,
27.828677361251));
#56760=CARTESIAN_POINT('Ctrl Pts',(-9.27329515907125,-31.0765558017924,
27.6315979086826));
#56761=CARTESIAN_POINT('Ctrl Pts',(-6.32018953277514,-33.4571031196912,
27.4345184561141));
#56762=CARTESIAN_POINT('Ctrl Pts',(-6.6924284169921,-37.2319287467791,27.2374390035457));
#56763=CARTESIAN_POINT('Ctrl Pts',(-10.0536300734982,-38.9898188142619,
27.0403595509773));
#56764=CARTESIAN_POINT('Ctrl Pts',(-13.3663676160112,-37.142219039571,26.8432800984088));
#56765=CARTESIAN_POINT('Ctrl Pts',(-13.6370101893174,-33.3587535440872,
26.6462006458404));
#56766=CARTESIAN_POINT('Ctrl Pts',(-10.6209853939007,-31.0584381780949,
26.4491211932719));
#56767=CARTESIAN_POINT('Ctrl Pts',(-7.04379296919064,-32.3200050661253,
26.2520417407035));
#56768=CARTESIAN_POINT('Ctrl Pts',(-6.13804456209019,-36.0034106733504,
26.0549622881351));
#56769=CARTESIAN_POINT('Ctrl Pts',(-8.72224042076868,-38.7800612666714,
25.8578828355666));
#56770=CARTESIAN_POINT('Ctrl Pts',(-12.4611129143278,-38.14077315272,25.6608033829982));
#56771=CARTESIAN_POINT('Ctrl Pts',(-13.9759444957377,-34.6632536150714,
25.4637239304297));
#56772=CARTESIAN_POINT('Ctrl Pts',(-11.8978229970468,-31.490042645999,25.2666444778613));
#56773=CARTESIAN_POINT('Ctrl Pts',(-8.10469038869652,-31.4886848277523,
25.0695650252928));
#56774=CARTESIAN_POINT('Ctrl Pts',(-6.02429761163027,-34.6604071871109,
24.8724855727244));
#56775=CARTESIAN_POINT('Ctrl Pts',(-7.53663912855336,-38.1390103497744,
24.6754061201559));
#56776=CARTESIAN_POINT('Ctrl Pts',(-11.2750529760013,-38.7809750948868,
24.4783266675875));
#56777=CARTESIAN_POINT('Ctrl Pts',(-13.861236071256,-36.0061753134915,24.2812472150191));
#56778=CARTESIAN_POINT('Ctrl Pts',(-12.958124975163,-32.3221222225917,24.0841677624506));
#56779=CARTESIAN_POINT('Ctrl Pts',(-9.38183666260023,-31.0579945652231,
23.8870883098822));
#56780=CARTESIAN_POINT('Ctrl Pts',(-6.36416577271778,-33.3561501798544,
23.6900088573138));
#56781=CARTESIAN_POINT('Ctrl Pts',(-6.63209954823897,-37.1398082405902,
23.4929294047453));
#56782=CARTESIAN_POINT('Ctrl Pts',(-9.94351351157651,-38.9897796976916,
23.2958499521769));
#56783=CARTESIAN_POINT('Ctrl Pts',(-13.305972780694,-37.2342955786512,23.0987704996084));
#56784=CARTESIAN_POINT('Ctrl Pts',(-13.6809142167823,-33.459739214237,22.90169104704));
#56785=CARTESIAN_POINT('Ctrl Pts',(-10.7295134250377,-31.0770746983652,
22.7046115944715));
#56786=CARTESIAN_POINT('Ctrl Pts',(-7.11887115996344,-32.2394512562663,
22.5075321419031));
#56787=CARTESIAN_POINT('Ctrl Pts',(-6.11182679476447,-35.8964607551567,
22.3104526893346));
#56788=CARTESIAN_POINT('Ctrl Pts',(-8.61841897744962,-38.7433630117707,
22.1133732367662));
#56789=CARTESIAN_POINT('Ctrl Pts',(-12.3735084153843,-38.2074897600872,
21.9162937841978));
#56790=CARTESIAN_POINT('Ctrl Pts',(-13.9837227475169,-34.7730951072122,
21.7192143316293));
#56791=CARTESIAN_POINT('Ctrl Pts',(-11.9939550048957,-31.5437482441223,
21.5221348790609));
#56792=CARTESIAN_POINT('Ctrl Pts',(-8.20230426734218,-31.4377222444328,
21.3250554264924));
#56793=CARTESIAN_POINT('Ctrl Pts',(-6.0351823494922,-34.5508299217764,21.127975973924));
#56794=CARTESIAN_POINT('Ctrl Pts',(-7.45095848371802,-38.0698404066318,
20.9308965213555));
#56795=CARTESIAN_POINT('Ctrl Pts',(-11.1702342203526,-38.814719464341,20.7338170687871));
#56796=CARTESIAN_POINT('Ctrl Pts',(-13.8320010687388,-36.112340142663,20.5367376162187));
#56797=CARTESIAN_POINT('Ctrl Pts',(-13.0308926023777,-32.4047692034324,
20.3396581636502));
#56798=CARTESIAN_POINT('Ctrl Pts',(-9.49084879340863,-31.0424379342625,
20.1425787110818));
#56799=CARTESIAN_POINT('Ctrl Pts',(-6.41091109924001,-33.2564479047973,
19.9454992585133));
#56800=CARTESIAN_POINT('Ctrl Pts',(-6.5743355988234,-37.0460588334994,19.7484198059449));
#56801=CARTESIAN_POINT('Ctrl Pts',(-9.8334399776528,-38.9867014077275,19.5513403533764));
#56802=CARTESIAN_POINT('Ctrl Pts',(-13.2430601681256,-37.3246712570463,
19.354260900808));
#56803=CARTESIAN_POINT('Ctrl Pts',(-13.7220148613169,-33.561896655278,19.1571814482396));
#56804=CARTESIAN_POINT('Ctrl Pts',(-10.8374859573864,-31.0987012965605,
18.9601019956711));
#56805=CARTESIAN_POINT('Ctrl Pts',(-7.1961434015981,-32.1609950784182,18.7630225431027));
#56806=CARTESIAN_POINT('Ctrl Pts',(-6.08857058207861,-35.7888375735615,
18.5659430905342));
#56807=CARTESIAN_POINT('Ctrl Pts',(-8.51564899808879,-38.7037950083057,
18.3688636379658));
#56808=CARTESIAN_POINT('Ctrl Pts',(-12.2840977384796,-38.2718011072648,
18.1717841853974));
#56809=CARTESIAN_POINT('Ctrl Pts',(-13.9884641375675,-34.8830346755273,
17.9747047328289));
#56810=CARTESIAN_POINT('Ctrl Pts',(-12.0885742245895,-31.6002349130302,
17.7776252802605));
#56811=CARTESIAN_POINT('Ctrl Pts',(-8.30127573310404,-31.3891762442465,
17.580545827692));
#56812=CARTESIAN_POINT('Ctrl Pts',(-6.04910953722514,-34.4421851523227,
17.3834663751236));
#56813=CARTESIAN_POINT('Ctrl Pts',(-7.36717415028043,-37.9971552563352,
17.1863869225551));
#56814=CARTESIAN_POINT('Ctrl Pts',(-11.0646063138124,-38.8479214732267,
16.9893074699867));
#56815=CARTESIAN_POINT('Ctrl Pts',(-13.7997685140726,-36.2127299742061,
16.7922280174183));
#56816=CARTESIAN_POINT('Ctrl Pts',(-13.3330643605671,-33.7394001666604,
16.660841715706));
#56817=CARTESIAN_POINT('Ctrl Pts',(-12.6300276622661,-32.8709392788408,
16.5951485648498));
#56818=CARTESIAN_POINT('Ctrl Pts',(-7.2545283688926,-32.642466854737,30.1323684526006));
#56819=CARTESIAN_POINT('Ctrl Pts',(-6.47544764882367,-33.5496482080684,
30.066629562464));
#56820=CARTESIAN_POINT('Ctrl Pts',(-5.90058821685929,-36.180719655511,29.9351975214714));
#56821=CARTESIAN_POINT('Ctrl Pts',(-8.74541287253645,-39.0812795008765,
29.7380723296225));
#56822=CARTESIAN_POINT('Ctrl Pts',(-12.7238059528751,-38.283735596327,29.5409928770541));
#56823=CARTESIAN_POINT('Ctrl Pts',(-14.2404760928887,-34.5233011844661,
29.3439134244856));
#56824=CARTESIAN_POINT('Ctrl Pts',(-11.9252946005181,-31.1913816934919,
29.1468339719172));
#56825=CARTESIAN_POINT('Ctrl Pts',(-7.87020028386335,-31.3023435461948,
28.9497545193487));
#56826=CARTESIAN_POINT('Ctrl Pts',(-5.73978651265714,-34.7542065823867,
28.7526750667803));
#56827=CARTESIAN_POINT('Ctrl Pts',(-7.45919271967868,-38.428472938978,28.5555956142119));
#56828=CARTESIAN_POINT('Ctrl Pts',(-11.474667150335,-39.0043775452991,28.3585161616434));
#56829=CARTESIAN_POINT('Ctrl Pts',(-14.1575200609129,-35.9617071281995,
28.161436709075));
#56830=CARTESIAN_POINT('Ctrl Pts',(-13.0833374235737,-32.0499318238524,
27.9643572565065));
#56831=CARTESIAN_POINT('Ctrl Pts',(-9.22282525504695,-30.8040712372542,
27.7672778039381));
#56832=CARTESIAN_POINT('Ctrl Pts',(-6.06462541561428,-33.3499483945774,
27.5701983513697));
#56833=CARTESIAN_POINT('Ctrl Pts',(-6.46271641984263,-37.3869369747346,
27.3731188988012));
#56834=CARTESIAN_POINT('Ctrl Pts',(-10.0573547007607,-39.2669131189769,
27.1760394462328));
#56835=CARTESIAN_POINT('Ctrl Pts',(-13.6001630181079,-37.2909968971508,
26.9789599936643));
#56836=CARTESIAN_POINT('Ctrl Pts',(-13.8896018122872,-33.2447684067318,
26.7818805410959));
#56837=CARTESIAN_POINT('Ctrl Pts',(-10.664113045549,-30.7846953382877,26.5848010885274));
#56838=CARTESIAN_POINT('Ctrl Pts',(-6.83848336243165,-32.1338784855931,
26.387721635959));
#56839=CARTESIAN_POINT('Ctrl Pts',(-5.86983041334672,-36.0730978937028,
26.1906421833905));
#56840=CARTESIAN_POINT('Ctrl Pts',(-8.63349957345641,-39.0425878367312,
25.9935627308221));
#56841=CARTESIAN_POINT('Ctrl Pts',(-12.6320380624531,-38.3589009408566,
25.7964832782536));
#56842=CARTESIAN_POINT('Ctrl Pts',(-14.2520752242043,-34.6398664614834,
25.5994038256852));
#56843=CARTESIAN_POINT('Ctrl Pts',(-12.0296274644475,-31.2462748866438,
25.4023243731168));
#56844=CARTESIAN_POINT('Ctrl Pts',(-7.97306047681017,-31.2448227674474,
25.2052449205483));
#56845=CARTESIAN_POINT('Ctrl Pts',(-5.74818369760461,-34.6368223481107,
25.0081654679799));
#56846=CARTESIAN_POINT('Ctrl Pts',(-7.3655578590241,-38.357015710633,24.8110860154114));
#56847=CARTESIAN_POINT('Ctrl Pts',(-11.3636058487777,-39.0435651306342,
24.614006562843));
#56848=CARTESIAN_POINT('Ctrl Pts',(-14.129400259735,-36.0760545390636,24.4169271102746));
#56849=CARTESIAN_POINT('Ctrl Pts',(-13.1635677838246,-32.1361426793127,
24.2198476577061));
#56850=CARTESIAN_POINT('Ctrl Pts',(-9.33890500375777,-30.7842209163476,
24.0227682051376));
#56851=CARTESIAN_POINT('Ctrl Pts',(-6.11165582072035,-33.2419842379472,
23.8256887525693));
#56852=CARTESIAN_POINT('Ctrl Pts',(-6.39819769016606,-37.288418667342,23.6286093000008));
#56853=CARTESIAN_POINT('Ctrl Pts',(-9.93959050530377,-39.2668712857472,
23.4315298474324));
#56854=CARTESIAN_POINT('Ctrl Pts',(-13.5355737404665,-37.3894681839036,
23.2344503948639));
#56855=CARTESIAN_POINT('Ctrl Pts',(-13.936554989734,-33.3527675668065,23.0373709422955));
#56856=CARTESIAN_POINT('Ctrl Pts',(-10.7801783862054,-30.8046261713746,
22.840291489727));
#56857=CARTESIAN_POINT('Ctrl Pts',(-6.91877575967346,-32.0477301856145,
22.6432120371586));
#56858=CARTESIAN_POINT('Ctrl Pts',(-5.84179181295901,-35.9587202664826,
22.4461325845901));
#56859=CARTESIAN_POINT('Ctrl Pts',(-8.52246769477921,-39.0033408752603,
22.2490531320217));
#56860=CARTESIAN_POINT('Ctrl Pts',(-12.5383494005802,-38.4302510398163,
22.0519736794533));
#56861=CARTESIAN_POINT('Ctrl Pts',(-14.2603936782757,-34.7573364834676,
21.8548942268848));
#56862=CARTESIAN_POINT('Ctrl Pts',(-12.132435873686,-31.303710357241,21.6578147743164));
#56863=CARTESIAN_POINT('Ctrl Pts',(-8.0774536732878,-31.1903208149863,21.4607353217479));
#56864=CARTESIAN_POINT('Ctrl Pts',(-5.75982438429787,-34.5196349035768,
21.2636558691795));
#56865=CARTESIAN_POINT('Ctrl Pts',(-7.27392666359651,-38.2830418908748,
21.066576416611));
#56866=CARTESIAN_POINT('Ctrl Pts',(-11.2515073940825,-39.0796530582867,
20.8694969640426));
#56867=CARTESIAN_POINT('Ctrl Pts',(-14.0981348761221,-36.1895925525558,
20.6724175114742));
#56868=CARTESIAN_POINT('Ctrl Pts',(-13.2413891480653,-32.2245295217257,
20.4753380589057));
#56869=CARTESIAN_POINT('Ctrl Pts',(-9.45548806497633,-30.7675838719546,
20.2782586063373));
#56870=CARTESIAN_POINT('Ctrl Pts',(-6.16164762643231,-33.1353576052008,
20.0811791537688));
#56871=CARTESIAN_POINT('Ctrl Pts',(-6.33642201436741,-37.1881583313131,
19.8840997012004));
#56872=CARTESIAN_POINT('Ctrl Pts',(-9.82187232615428,-39.2635792074742,
19.6870202486319));
#56873=CARTESIAN_POINT('Ctrl Pts',(-13.4682918250679,-37.4861204846052,
19.4899407960635));
#56874=CARTESIAN_POINT('Ctrl Pts',(-13.9805100883304,-33.4620198776685,
19.2928613434951));
#56875=CARTESIAN_POINT('Ctrl Pts',(-10.8956496484897,-30.8277547443384,
19.0957818909266));
#56876=CARTESIAN_POINT('Ctrl Pts',(-7.00141458537276,-31.9638251989198,
18.8987024383582));
#56877=CARTESIAN_POINT('Ctrl Pts',(-5.81692044821127,-35.8436226174832,
18.7016229857897));
#56878=CARTESIAN_POINT('Ctrl Pts',(-8.4125603045979,-38.9610248601888,18.5045435332213));
#56879=CARTESIAN_POINT('Ctrl Pts',(-12.4427291210584,-38.4990288324294,
18.3074640806529));
#56880=CARTESIAN_POINT('Ctrl Pts',(-14.2654643595148,-34.8749113930502,
18.1103846280844));
#56881=CARTESIAN_POINT('Ctrl Pts',(-12.2336264311057,-31.3641200449563,
17.913305175516));
#56882=CARTESIAN_POINT('Ctrl Pts',(-8.18329874177914,-31.138403278198,17.7162257229475));
#56883=CARTESIAN_POINT('Ctrl Pts',(-5.77471882006415,-34.4034447170867,
17.5191462703791));
#56884=CARTESIAN_POINT('Ctrl Pts',(-7.18432347905296,-38.205308731603,17.3220668178106));
#56885=CARTESIAN_POINT('Ctrl Pts',(-11.1385435926851,-39.1151609582406,
17.1249873652422));
#56886=CARTESIAN_POINT('Ctrl Pts',(-14.0636637593207,-36.2969544928254,
16.9279079126738));
#56887=CARTESIAN_POINT('Ctrl Pts',(-13.564546839987,-33.6518510696702,16.7965216109615));
#56888=CARTESIAN_POINT('Ctrl Pts',(-12.8126839984014,-32.7230752710526,
16.7308284601053));
#56889=CARTESIAN_POINT('Ctrl Pts',(-7.07623681911788,-32.4893681181295,
30.268048347856));
#56890=CARTESIAN_POINT('Ctrl Pts',(-6.24656242056877,-33.4554620340893,
30.2023094577194));
#56891=CARTESIAN_POINT('Ctrl Pts',(-5.63437148684482,-36.2573958574595,
30.0708774167267));
#56892=CARTESIAN_POINT('Ctrl Pts',(-8.663939700223,-39.3463187163724,29.8737522248779));
#56893=CARTESIAN_POINT('Ctrl Pts',(-12.9006905285965,-38.4969821299593,
29.6766727723095));
#56894=CARTESIAN_POINT('Ctrl Pts',(-14.5158535711396,-34.4923442553782,
29.479593319741));
#56895=CARTESIAN_POINT('Ctrl Pts',(-12.0503236680962,-30.9440491577359,
29.2825138671726));
#56896=CARTESIAN_POINT('Ctrl Pts',(-7.73189060774165,-31.0622168982944,
29.0854344146041));
#56897=CARTESIAN_POINT('Ctrl Pts',(-5.46312728353841,-34.7382447021567,
28.8883549620357));
#56898=CARTESIAN_POINT('Ctrl Pts',(-7.29419211921549,-38.6511187484357,
28.6912755094673));
#56899=CARTESIAN_POINT('Ctrl Pts',(-11.5704323691979,-39.2644227303759,
28.4941960568988));
#56900=CARTESIAN_POINT('Ctrl Pts',(-14.4275103556515,-36.0241606070019,
28.2971166043304));
#56901=CARTESIAN_POINT('Ctrl Pts',(-13.2835700544625,-31.8583537280866,
28.1000371517619));
#56902=CARTESIAN_POINT('Ctrl Pts',(-9.17235535102264,-30.5315866727159,
27.9029576991935));
#56903=CARTESIAN_POINT('Ctrl Pts',(-5.8090612984534,-33.2427936694637,27.7058782466251));
#56904=CARTESIAN_POINT('Ctrl Pts',(-6.23300442269314,-37.5419452026901,
27.5087987940566));
#56905=CARTESIAN_POINT('Ctrl Pts',(-10.0610793280231,-39.5440074236919,
27.3117193414882));
#56906=CARTESIAN_POINT('Ctrl Pts',(-13.8339584202047,-37.4397747547305,
27.1146398889197));
#56907=CARTESIAN_POINT('Ctrl Pts',(-14.1421934352571,-33.1307832693763,
26.9175604363513));
#56908=CARTESIAN_POINT('Ctrl Pts',(-10.7072406971973,-30.5109524984806,
26.7204809837828));
#56909=CARTESIAN_POINT('Ctrl Pts',(-6.63317375567267,-31.9477519050608,
26.5234015312144));
#56910=CARTESIAN_POINT('Ctrl Pts',(-5.60161626460324,-36.1427851140552,
26.3263220786459));
#56911=CARTESIAN_POINT('Ctrl Pts',(-8.54475872614412,-39.3051144067911,
26.1292426260775));
#56912=CARTESIAN_POINT('Ctrl Pts',(-12.8029632105785,-38.577028728993,25.9321631735091));
#56913=CARTESIAN_POINT('Ctrl Pts',(-14.5282059526709,-34.6164793078955,
25.7350837209406));
#56914=CARTESIAN_POINT('Ctrl Pts',(-12.1614319318481,-31.0025071272885,
25.5380042683722));
#56915=CARTESIAN_POINT('Ctrl Pts',(-7.84143056492381,-31.0009607071424,
25.3409248158037));
#56916=CARTESIAN_POINT('Ctrl Pts',(-5.47206978357895,-34.6132375091107,
25.1438453632353));
#56917=CARTESIAN_POINT('Ctrl Pts',(-7.19447658949484,-38.5750210714917,
24.9467659106668));
#56918=CARTESIAN_POINT('Ctrl Pts',(-11.452158721554,-39.3061551663815,24.7496864580984));
#56919=CARTESIAN_POINT('Ctrl Pts',(-14.3975644482142,-36.1459337646356,
24.55260700553));
#56920=CARTESIAN_POINT('Ctrl Pts',(-13.3690105924863,-31.9501631360336,
24.3555275529615));
#56921=CARTESIAN_POINT('Ctrl Pts',(-9.29597334491533,-30.5104472674722,
24.1584481003931));
#56922=CARTESIAN_POINT('Ctrl Pts',(-5.8591458687229,-33.1278182960401,23.9613686478246));
#56923=CARTESIAN_POINT('Ctrl Pts',(-6.16429583209316,-37.4370290940937,
23.7642891952562));
#56924=CARTESIAN_POINT('Ctrl Pts',(-9.93566749903101,-39.5439628738029,
23.5672097426877));
#56925=CARTESIAN_POINT('Ctrl Pts',(-13.7651747002391,-37.544640789156,23.3701302901193));
#56926=CARTESIAN_POINT('Ctrl Pts',(-14.1921957626856,-33.245795919376,23.1730508375509));
#56927=CARTESIAN_POINT('Ctrl Pts',(-10.8308433473732,-30.532177644384,22.9759713849824));
#56928=CARTESIAN_POINT('Ctrl Pts',(-6.71868035938346,-31.8560091149627,
22.778891932414));
#56929=CARTESIAN_POINT('Ctrl Pts',(-5.57175683115357,-36.0209797778084,
22.5818124798456));
#56930=CARTESIAN_POINT('Ctrl Pts',(-8.42651641210876,-39.2633187387499,
22.3847330272771));
#56931=CARTESIAN_POINT('Ctrl Pts',(-12.7031903857762,-38.6530123195454,
22.1876535747087));
#56932=CARTESIAN_POINT('Ctrl Pts',(-14.5370646090343,-34.7415778597228,
21.9905741221402));
#56933=CARTESIAN_POINT('Ctrl Pts',(-12.2709167424762,-31.0636724703596,
21.7934946695718));
#56934=CARTESIAN_POINT('Ctrl Pts',(-7.95260307923342,-30.9429193855399,
21.5964152170033));
#56935=CARTESIAN_POINT('Ctrl Pts',(-5.48446641910354,-34.4884398853772,
21.3993357644349));
#56936=CARTESIAN_POINT('Ctrl Pts',(-7.09689484347499,-38.496243375118,21.2022563118664));
#56937=CARTESIAN_POINT('Ctrl Pts',(-11.3327805678125,-39.3445866522322,
21.005176859298));
#56938=CARTESIAN_POINT('Ctrl Pts',(-14.3642686835055,-36.2668449624488,
20.8080974067296));
#56939=CARTESIAN_POINT('Ctrl Pts',(-13.451885693753,-32.0442898400189,20.6110179541611));
#56940=CARTESIAN_POINT('Ctrl Pts',(-9.420127336544,-30.4927298096469,20.4139385015927));
#56941=CARTESIAN_POINT('Ctrl Pts',(-5.91238415362461,-33.0142673056043,
20.2168590490242));
#56942=CARTESIAN_POINT('Ctrl Pts',(-6.09850842991144,-37.3302578291269,
20.0197795964558));
#56943=CARTESIAN_POINT('Ctrl Pts',(-9.81030467465576,-39.5404570072207,
19.8227001438873));
#56944=CARTESIAN_POINT('Ctrl Pts',(-13.6935234820103,-37.6475697121639,
19.6256206913189));
#56945=CARTESIAN_POINT('Ctrl Pts',(-14.2390053153439,-33.3621431000591,
19.4285412387505));
#56946=CARTESIAN_POINT('Ctrl Pts',(-10.9538133395929,-30.5568081921163,
19.231461786182));
#56947=CARTESIAN_POINT('Ctrl Pts',(-6.80668576914744,-31.7666553194215,
19.0343823336136));
#56948=CARTESIAN_POINT('Ctrl Pts',(-5.54527031434392,-35.8984076614049,
18.8373028810451));
#56949=CARTESIAN_POINT('Ctrl Pts',(-8.30947161110702,-39.2182547120721,
18.6402234284767));
#56950=CARTESIAN_POINT('Ctrl Pts',(-12.6013605036371,-38.7262565575938,
18.4431439759083));
#56951=CARTESIAN_POINT('Ctrl Pts',(-14.5424645814622,-34.8667881105732,
18.2460645233398));
#56952=CARTESIAN_POINT('Ctrl Pts',(-12.3786786376218,-31.1280051768823,
18.0489850707714));
#56953=CARTESIAN_POINT('Ctrl Pts',(-8.06532175045426,-30.8876303121494,
17.8519056182029));
#56954=CARTESIAN_POINT('Ctrl Pts',(-5.50032810290316,-34.3647042818508,
17.6548261656345));
#56955=CARTESIAN_POINT('Ctrl Pts',(-7.00147280782552,-38.4134622068707,
17.457746713066));
#56956=CARTESIAN_POINT('Ctrl Pts',(-11.2124808715576,-39.3824004432543,
17.2606672604976));
#56957=CARTESIAN_POINT('Ctrl Pts',(-14.3275590045687,-36.3811790114449,
17.0635878079291));
#56958=CARTESIAN_POINT('Ctrl Pts',(-13.796029319407,-33.5643019726801,16.9322015062168));
#56959=CARTESIAN_POINT('Ctrl Pts',(-12.9953403345368,-32.5752112632643,
16.8665083553607));
#56960=CARTESIAN_POINT('Ctrl Pts',(-6.89794526934316,-32.3362693815221,
30.4037282431115));
#56961=CARTESIAN_POINT('Ctrl Pts',(-6.01767719231387,-33.3612758601103,
30.3379893529749));
#56962=CARTESIAN_POINT('Ctrl Pts',(-5.36815475683035,-36.3340720594079,
30.2065573119822));
#56963=CARTESIAN_POINT('Ctrl Pts',(-8.58246652790955,-39.6113579318683,
30.0094321201333));
#56964=CARTESIAN_POINT('Ctrl Pts',(-13.077575104318,-38.7102286635917,29.8123526675649));
#56965=CARTESIAN_POINT('Ctrl Pts',(-14.7912310493905,-34.4613873262902,
29.6152732149964));
#56966=CARTESIAN_POINT('Ctrl Pts',(-12.1753527356742,-30.69671662198,29.418193762428));
#56967=CARTESIAN_POINT('Ctrl Pts',(-7.59358093161996,-30.822090250394,29.2211143098595));
#56968=CARTESIAN_POINT('Ctrl Pts',(-5.18646805441968,-34.7222828219266,
29.0240348572911));
#56969=CARTESIAN_POINT('Ctrl Pts',(-7.12919151875231,-38.8737645578935,
28.8269554047226));
#56970=CARTESIAN_POINT('Ctrl Pts',(-11.6661975880609,-39.5244679154526,
28.6298759521542));
#56971=CARTESIAN_POINT('Ctrl Pts',(-14.6975006503904,-36.0866140858044,
28.4327964995858));
#56972=CARTESIAN_POINT('Ctrl Pts',(-13.4838026853514,-31.6667756323208,
28.2357170470173));
#56973=CARTESIAN_POINT('Ctrl Pts',(-9.12188544699834,-30.2591021081778,
28.0386375944489));
#56974=CARTESIAN_POINT('Ctrl Pts',(-5.55349718129253,-33.1356389443498,
27.8415581418804));
#56975=CARTESIAN_POINT('Ctrl Pts',(-6.00329242554367,-37.6969534306456,
27.644478689312));
#56976=CARTESIAN_POINT('Ctrl Pts',(-10.0648039552855,-39.8211017284068,
27.4473992367436));
#56977=CARTESIAN_POINT('Ctrl Pts',(-14.0677538223015,-37.5885526123103,
27.2503197841751));
#56978=CARTESIAN_POINT('Ctrl Pts',(-14.394785058227,-33.0167981320208,27.0532403316067));
#56979=CARTESIAN_POINT('Ctrl Pts',(-10.7503683488455,-30.2372096586735,
26.8561608790382));
#56980=CARTESIAN_POINT('Ctrl Pts',(-6.42786414891367,-31.7616253245286,
26.6590814264698));
#56981=CARTESIAN_POINT('Ctrl Pts',(-5.33340211585977,-36.2124723344077,
26.4620019739013));
#56982=CARTESIAN_POINT('Ctrl Pts',(-8.45601787883186,-39.5676409768508,
26.2649225213329));
#56983=CARTESIAN_POINT('Ctrl Pts',(-12.9738883587037,-38.7951565171297,
26.0678430687645));
#56984=CARTESIAN_POINT('Ctrl Pts',(-14.8043366811376,-34.5930921543075,
25.870763616196));
#56985=CARTESIAN_POINT('Ctrl Pts',(-12.2932363992487,-30.7587393679332,
25.6736841636276));
#56986=CARTESIAN_POINT('Ctrl Pts',(-7.70980065303747,-30.7570986468375,
25.4766047110591));
#56987=CARTESIAN_POINT('Ctrl Pts',(-5.19595586955329,-34.5896526701106,
25.2795252584907));
#56988=CARTESIAN_POINT('Ctrl Pts',(-7.02339531996559,-38.7930264323505,
25.0824458059222));
#56989=CARTESIAN_POINT('Ctrl Pts',(-11.5407115943303,-39.5687452021288,
24.8853663533538));
#56990=CARTESIAN_POINT('Ctrl Pts',(-14.6657286366932,-36.2158129902076,
24.6882869007854));
#56991=CARTESIAN_POINT('Ctrl Pts',(-13.5744534011479,-31.7641835927545,
24.4912074482169));
#56992=CARTESIAN_POINT('Ctrl Pts',(-9.25304168607287,-30.2366736185969,
24.2941279956485));
#56993=CARTESIAN_POINT('Ctrl Pts',(-5.60663591672545,-33.0136523541329,
24.09704854308));
#56994=CARTESIAN_POINT('Ctrl Pts',(-5.93039397402027,-37.5856395208455,
23.8999690905116));
#56995=CARTESIAN_POINT('Ctrl Pts',(-9.93174449275826,-39.8210544618584,
23.7028896379431));
#56996=CARTESIAN_POINT('Ctrl Pts',(-13.9947756600116,-37.6998133944084,
23.5058101853747));
#56997=CARTESIAN_POINT('Ctrl Pts',(-14.4478365356373,-33.1388242719455,
23.3087307328062));
#56998=CARTESIAN_POINT('Ctrl Pts',(-10.881508308541,-30.2597291173932,23.1116512802378));
#56999=CARTESIAN_POINT('Ctrl Pts',(-6.51858495909347,-31.664288044311,22.9145718276693));
#57000=CARTESIAN_POINT('Ctrl Pts',(-5.30172184934813,-36.0832392891341,
22.717492375101));
#57001=CARTESIAN_POINT('Ctrl Pts',(-8.33056512943833,-39.5232966022396,
22.5204129225325));
#57002=CARTESIAN_POINT('Ctrl Pts',(-12.8680313709721,-38.8757735992743,
22.3233334699641));
#57003=CARTESIAN_POINT('Ctrl Pts',(-14.8137355397931,-34.7258192359782,
22.1262540173956));
#57004=CARTESIAN_POINT('Ctrl Pts',(-12.4093976112665,-30.8236345834782,
21.9291745648272));
#57005=CARTESIAN_POINT('Ctrl Pts',(-7.82775248517904,-30.6955179560935,
21.7320951122587));
#57006=CARTESIAN_POINT('Ctrl Pts',(-5.2091084539092,-34.4572448671776,21.5350156596903));
#57007=CARTESIAN_POINT('Ctrl Pts',(-6.91986302335349,-38.709444859361,21.3379362071218));
#57008=CARTESIAN_POINT('Ctrl Pts',(-11.4140537415424,-39.6095202461779,
21.1408567545534));
#57009=CARTESIAN_POINT('Ctrl Pts',(-14.6304024908889,-36.3440973723417,
20.943777301985));
#57010=CARTESIAN_POINT('Ctrl Pts',(-13.6623822394406,-31.8640501583123,
20.7466978494165));
#57011=CARTESIAN_POINT('Ctrl Pts',(-9.38476660811169,-30.2178757473391,
20.5496183968481));
#57012=CARTESIAN_POINT('Ctrl Pts',(-5.66312068081691,-32.8931770060079,
20.3525389442796));
#57013=CARTESIAN_POINT('Ctrl Pts',(-5.86059484545545,-37.4723573269407,
20.1554594917112));
#57014=CARTESIAN_POINT('Ctrl Pts',(-9.79873702315724,-39.8173348069675,
19.9583800391427));
#57015=CARTESIAN_POINT('Ctrl Pts',(-13.9187551389525,-37.8090189397228,
19.7613005865743));
#57016=CARTESIAN_POINT('Ctrl Pts',(-14.4975005423574,-33.2622663224496,
19.5642211340059));
#57017=CARTESIAN_POINT('Ctrl Pts',(-11.0119770306961,-30.2858616398942,
19.3671416814374));
#57018=CARTESIAN_POINT('Ctrl Pts',(-6.61195695292212,-31.5694854399232,
19.170062228869));
#57019=CARTESIAN_POINT('Ctrl Pts',(-5.27362018047655,-35.9531927053267,
18.9729827763005));
#57020=CARTESIAN_POINT('Ctrl Pts',(-8.20638291761613,-39.4754845639552,
18.7759033237321));
#57021=CARTESIAN_POINT('Ctrl Pts',(-12.7599918862159,-38.9534842827584,
18.5788238711636));
#57022=CARTESIAN_POINT('Ctrl Pts',(-14.8194648034095,-34.8586648280961,
18.3817444185952));
#57023=CARTESIAN_POINT('Ctrl Pts',(-12.523730844138,-30.8918903088085,18.1846649660268));
#57024=CARTESIAN_POINT('Ctrl Pts',(-7.94734475912938,-30.6368573461008,
17.9875855134583));
#57025=CARTESIAN_POINT('Ctrl Pts',(-5.22593738574218,-34.325963846615,17.7905060608899));
#57026=CARTESIAN_POINT('Ctrl Pts',(-6.81862213659804,-38.6216156821384,
17.5934266083214));
#57027=CARTESIAN_POINT('Ctrl Pts',(-11.2864181504302,-39.6496399282681,
17.396347155753));
#57028=CARTESIAN_POINT('Ctrl Pts',(-14.5914542498167,-36.4654035300642,
17.1992677031845));
#57029=CARTESIAN_POINT('Ctrl Pts',(-14.0275117988269,-33.4767528756898,
17.0678814014722));
#57030=CARTESIAN_POINT('Ctrl Pts',(-13.177996670672,-32.4273472554761,17.0021882506161));
#57031=CARTESIAN_POINT('Ctrl Pts',(-7.42676557298524,-32.7934484719077,
30.));
#57032=CARTESIAN_POINT('Ctrl Pts',(-7.348473680774,-32.8679592071175,30.));
#57033=CARTESIAN_POINT('Ctrl Pts',(-7.27428894791241,-32.9462643748986,
30.));
#57034=CARTESIAN_POINT('Ctrl Pts',(-7.20420784983133,-33.0279214358029,
30.));
#57035=CARTESIAN_POINT('Ctrl Pts',(-7.13363401900521,-33.1101526188153,
30.));
#57036=CARTESIAN_POINT('Ctrl Pts',(-7.06722139480313,-33.1957835701515,
30.));
#57037=CARTESIAN_POINT('Ctrl Pts',(-7.00499327507605,-33.2844116565263,
30.));
#57038=CARTESIAN_POINT('Ctrl Pts',(-6.94120691731623,-33.3752590555778,
30.));
#57039=CARTESIAN_POINT('Ctrl Pts',(-6.88181677124198,-33.4692561008207,
30.));
#57040=CARTESIAN_POINT('Ctrl Pts',(-6.82688246489709,-33.5660125152163,
30.));
#57041=CARTESIAN_POINT('Ctrl Pts',(-6.77575465411374,-33.6560645059748,
30.));
#57042=CARTESIAN_POINT('Ctrl Pts',(-6.72848667230412,-33.748507616239,30.));
#57043=CARTESIAN_POINT('Ctrl Pts',(-6.68515790161883,-33.8430529558883,
30.));
#57044=CARTESIAN_POINT('Ctrl Pts',(-6.67815310128406,-33.8583377474102,
30.));
#57045=CARTESIAN_POINT('Ctrl Pts',(-6.67125055154478,-33.8736792804882,
30.));
#57046=CARTESIAN_POINT('Ctrl Pts',(-6.66445311748837,-33.8890708261453,
30.));
#57047=CARTESIAN_POINT('Ctrl Pts',(-6.61779557045972,-33.9947183042054,
30.));
#57048=CARTESIAN_POINT('Ctrl Pts',(-6.5762333697332,-34.1023850035639,30.));
#57049=CARTESIAN_POINT('Ctrl Pts',(-6.53979147597588,-34.2116192879216,
30.));
#57050=CARTESIAN_POINT('Ctrl Pts',(-6.50328868698427,-34.3210361052559,
30.));
#57051=CARTESIAN_POINT('Ctrl Pts',(-6.47192296745121,-34.4320265565667,
30.));
#57052=CARTESIAN_POINT('Ctrl Pts',(-6.44575876679422,-34.5441747920789,
30.));
#57053=CARTESIAN_POINT('Ctrl Pts',(-6.41958697740395,-34.6563555553591,
30.));
#57054=CARTESIAN_POINT('Ctrl Pts',(-6.39861935723561,-34.7696956037716,
30.));
#57055=CARTESIAN_POINT('Ctrl Pts',(-6.38296523648734,-34.8838044926981,
30.));
#57056=CARTESIAN_POINT('Ctrl Pts',(-6.36739851537545,-34.9972762921604,
30.));
#57057=CARTESIAN_POINT('Ctrl Pts',(-6.35708579723688,-35.1115092190907,
30.));
#57058=CARTESIAN_POINT('Ctrl Pts',(-6.3521840433183,-35.2261322552398,30.));
#57059=CARTESIAN_POINT('Ctrl Pts',(-6.35142083329213,-35.2439792242782,
30.));
#57060=CARTESIAN_POINT('Ctrl Pts',(-6.35078926352373,-35.2618281998695,
30.));
#57061=CARTESIAN_POINT('Ctrl Pts',(-6.35028981819732,-35.2796697579982,
30.));
#57062=CARTESIAN_POINT('Ctrl Pts',(-6.34696896251305,-35.3982998393995,
30.));
#57063=CARTESIAN_POINT('Ctrl Pts',(-6.34948085220682,-35.5167089537285,
30.));
#57064=CARTESIAN_POINT('Ctrl Pts',(-6.3578921072129,-35.6344688667497,30.));
#57065=CARTESIAN_POINT('Ctrl Pts',(-6.36625711786001,-35.7515813458642,
30.));
#57066=CARTESIAN_POINT('Ctrl Pts',(-6.38045650012585,-35.8680526311929,
30.));
#57067=CARTESIAN_POINT('Ctrl Pts',(-6.40060399470209,-35.9834785326489,
30.));
#57068=CARTESIAN_POINT('Ctrl Pts',(-6.40380951972359,-36.0018431294897,
30.));
#57069=CARTESIAN_POINT('Ctrl Pts',(-6.4071657188688,-36.0201812828735,30.));
#57070=CARTESIAN_POINT('Ctrl Pts',(-6.41067317161291,-36.0384913817355,
30.));
#57071=CARTESIAN_POINT('Ctrl Pts',(-6.43232735026095,-36.1515335752435,
30.));
#57072=CARTESIAN_POINT('Ctrl Pts',(-6.45974222332004,-36.2635067659136,
30.));
#57073=CARTESIAN_POINT('Ctrl Pts',(-6.49261646094871,-36.3741489668983,
30.));
#57074=CARTESIAN_POINT('Ctrl Pts',(-6.51335838631696,-36.4439584116473,
30.));
#57075=CARTESIAN_POINT('Ctrl Pts',(-6.5362747620185,-36.5132379695589,30.));
#57076=CARTESIAN_POINT('Ctrl Pts',(-6.56130037757764,-36.5819201363282,
30.));
#57077=CARTESIAN_POINT('Ctrl Pts',(-6.56744767501135,-36.5987912381209,
30.));
#57078=CARTESIAN_POINT('Ctrl Pts',(-6.57372227837194,-36.6156262842334,
30.));
#57079=CARTESIAN_POINT('Ctrl Pts',(-6.58012329087647,-36.632424253444,30.));
#57080=CARTESIAN_POINT('Ctrl Pts',(-6.58592196118508,-36.6476415155939,
30.));
#57081=CARTESIAN_POINT('Ctrl Pts',(-6.5918227230537,-36.6628239282595,30.));
#57082=CARTESIAN_POINT('Ctrl Pts',(-6.59782163563458,-36.6779632135072,
30.));
#57083=CARTESIAN_POINT('Ctrl Pts',(-6.64115230666265,-36.787315596931,30.));
#57084=CARTESIAN_POINT('Ctrl Pts',(-6.68964474891968,-36.8945375462831,
30.));
#57085=CARTESIAN_POINT('Ctrl Pts',(-6.74293042168715,-36.9993679579068,
30.));
#57086=CARTESIAN_POINT('Ctrl Pts',(-6.79720023807432,-37.1061345031175,
30.));
#57087=CARTESIAN_POINT('Ctrl Pts',(-6.8564422422142,-37.2104210176384,30.));
#57088=CARTESIAN_POINT('Ctrl Pts',(-6.92032223600451,-37.3119481519295,
30.));
#57089=CARTESIAN_POINT('Ctrl Pts',(-6.98529990584252,-37.4152198684739,
30.));
#57090=CARTESIAN_POINT('Ctrl Pts',(-7.05507665614285,-37.5156373235829,
30.));
#57091=CARTESIAN_POINT('Ctrl Pts',(-7.12935272067387,-37.6128920097048,
30.));
#57092=CARTESIAN_POINT('Ctrl Pts',(-7.18304873196466,-37.6831998370926,
30.));
#57093=CARTESIAN_POINT('Ctrl Pts',(-7.23909729085682,-37.7518544742134,
30.));
#57094=CARTESIAN_POINT('Ctrl Pts',(-7.2974000200836,-37.8187312516186,30.));
#57095=CARTESIAN_POINT('Ctrl Pts',(-7.3176529320871,-37.8419625738196,30.));
#57096=CARTESIAN_POINT('Ctrl Pts',(-7.33817775201689,-37.8649790685653,
30.));
#57097=CARTESIAN_POINT('Ctrl Pts',(-7.35897141037825,-37.8877760628998,
30.));
#57098=CARTESIAN_POINT('Ctrl Pts',(-7.37199172460619,-37.9020508011171,
30.));
#57099=CARTESIAN_POINT('Ctrl Pts',(-7.38511665917092,-37.9162385040998,
30.));
#57100=CARTESIAN_POINT('Ctrl Pts',(-7.3983354919303,-37.9303276817975,30.));
#57101=CARTESIAN_POINT('Ctrl Pts',(-7.48411062168129,-38.0217503563337,
30.));
#57102=CARTESIAN_POINT('Ctrl Pts',(-7.57393021067795,-38.1091313263961,
30.));
#57103=CARTESIAN_POINT('Ctrl Pts',(-7.66746004992797,-38.1921567632245,
30.));
#57104=CARTESIAN_POINT('Ctrl Pts',(-7.73941550489948,-38.2560308501373,
30.));
#57105=CARTESIAN_POINT('Ctrl Pts',(-7.81356806356869,-38.3173268123056,
30.));
#57106=CARTESIAN_POINT('Ctrl Pts',(-7.88978351495984,-38.3758912604165,
30.));
#57107=CARTESIAN_POINT('Ctrl Pts',(-7.92789124065542,-38.405173484472,30.));
#57108=CARTESIAN_POINT('Ctrl Pts',(-7.96651491739015,-38.4337726638739,
30.));
#57109=CARTESIAN_POINT('Ctrl Pts',(-8.00563904546686,-38.4616684950285,
30.));
#57110=CARTESIAN_POINT('Ctrl Pts',(-8.02949698067293,-38.4786794027451,
30.));
#57111=CARTESIAN_POINT('Ctrl Pts',(-8.05354236869358,-38.4954296697472,
30.));
#57112=CARTESIAN_POINT('Ctrl Pts',(-8.07776857551838,-38.5119122904479,
30.));
#57113=CARTESIAN_POINT('Ctrl Pts',(-8.09327041768187,-38.5224591740931,
30.));
#57114=CARTESIAN_POINT('Ctrl Pts',(-8.1088447591175,-38.5328953980027,30.));
#57115=CARTESIAN_POINT('Ctrl Pts',(-8.12448498934949,-38.5432161517883,
30.));
#57116=CARTESIAN_POINT('Ctrl Pts',(-8.2313653964011,-38.613744932332,30.));
#57117=CARTESIAN_POINT('Ctrl Pts',(-8.34138274960732,-38.6789276717489,
30.));
#57118=CARTESIAN_POINT('Ctrl Pts',(-8.45421422908593,-38.7384194582944,
30.));
#57119=CARTESIAN_POINT('Ctrl Pts',(-8.56704570856451,-38.7979112448399,
30.));
#57120=CARTESIAN_POINT('Ctrl Pts',(-8.68269189967889,-38.8517129044718,
30.));
#57121=CARTESIAN_POINT('Ctrl Pts',(-8.80086736442083,-38.8994392928682,
30.));
#57122=CARTESIAN_POINT('Ctrl Pts',(-8.84648289711551,-38.9178615993515,
30.));
#57123=CARTESIAN_POINT('Ctrl Pts',(-8.89247562661289,-38.9353782311179,
30.));
#57124=CARTESIAN_POINT('Ctrl Pts',(-8.93882090860579,-38.9519961826432,
30.));
#57125=CARTESIAN_POINT('Ctrl Pts',(-11.0588859861567,-38.9492994180788,
29.9978117181351));
#57126=CARTESIAN_POINT('Ctrl Pts',(-12.3629833263098,-38.5996448966335,
29.932118567279));
#57127=CARTESIAN_POINT('Ctrl Pts',(-14.5759069292524,-36.5132512939394,
29.8007322655667));
#57128=CARTESIAN_POINT('Ctrl Pts',(-13.7737241750814,-31.9945004802153,
29.6036528129982));
#57129=CARTESIAN_POINT('Ctrl Pts',(-9.55494350084833,-30.2000838007241,
29.4065733604298));
#57130=CARTESIAN_POINT('Ctrl Pts',(-5.74151352522334,-32.7391832451362,
29.2094939078613));
#57131=CARTESIAN_POINT('Ctrl Pts',(-5.77477598136472,-37.3233360369277,
29.0124144552929));
#57132=CARTESIAN_POINT('Ctrl Pts',(-9.62705482091557,-39.8069425790181,
28.8153350027244));
#57133=CARTESIAN_POINT('Ctrl Pts',(-13.8159543550122,-37.9471529628393,
28.618255550156));
#57134=CARTESIAN_POINT('Ctrl Pts',(-14.5566802618819,-33.4238465177708,
28.4211760975876));
#57135=CARTESIAN_POINT('Ctrl Pts',(-11.1795571712635,-30.3249950720552,
28.2240966450191));
#57136=CARTESIAN_POINT('Ctrl Pts',(-6.73655089324582,-31.4507544203241,
28.0270171924506));
#57137=CARTESIAN_POINT('Ctrl Pts',(-5.24260955293931,-35.7839028674565,
27.8299377398823));
#57138=CARTESIAN_POINT('Ctrl Pts',(-8.04780553591408,-39.4086433897224,
27.6328582873138));
#57139=CARTESIAN_POINT('Ctrl Pts',(-12.617140242138,-39.0494207196498,27.4357788347454));
#57140=CARTESIAN_POINT('Ctrl Pts',(-14.8214395921059,-35.0308424199595,
27.2386993821769));
#57141=CARTESIAN_POINT('Ctrl Pts',(-12.6687332871507,-30.9843947121075,
27.0416199296085));
#57142=CARTESIAN_POINT('Ctrl Pts',(-8.10436598692081,-30.5667394360589,
26.84454047704));
#57143=CARTESIAN_POINT('Ctrl Pts',(-5.25303126404637,-34.1553018695318,
26.6474610244716));
#57144=CARTESIAN_POINT('Ctrl Pts',(-6.69140349521391,-38.5071948075579,
26.4503815719031));
#57145=CARTESIAN_POINT('Ctrl Pts',(-11.1196644450027,-39.6897311610149,
26.2533021193347));
#57146=CARTESIAN_POINT('Ctrl Pts',(-14.5361150902314,-36.6342847416972,
26.0562226667663));
#57147=CARTESIAN_POINT('Ctrl Pts',(-13.8534016741551,-32.1019796107692,
25.8591432141978));
#57148=CARTESIAN_POINT('Ctrl Pts',(-9.68847381165508,-30.1885367975724,
25.6620637616294));
#57149=CARTESIAN_POINT('Ctrl Pts',(-5.80506369999907,-32.6230826404,25.4649843090609));
#57150=CARTESIAN_POINT('Ctrl Pts',(-5.7125036185332,-37.205584155207,25.2679048564925));
#57151=CARTESIAN_POINT('Ctrl Pts',(-9.49443759462431,-39.794959160471,25.070825403924));
#57152=CARTESIAN_POINT('Ctrl Pts',(-13.7332345894671,-38.0512597715136,
24.8737459513556));
#57153=CARTESIAN_POINT('Ctrl Pts',(-14.598408855951,-33.550219780088,24.6766664987872));
#57154=CARTESIAN_POINT('Ctrl Pts',(-11.3081259026265,-30.3593068064588,
24.4795870462187));
#57155=CARTESIAN_POINT('Ctrl Pts',(-6.83572509125078,-31.3620622606893,
24.2825075936503));
#57156=CARTESIAN_POINT('Ctrl Pts',(-5.22279359367999,-35.6523232669585,
24.0854281410818));
#57157=CARTESIAN_POINT('Ctrl Pts',(-7.92689380738031,-39.3530974498007,
23.8883486885134));
#57158=CARTESIAN_POINT('Ctrl Pts',(-12.5044037951801,-39.1200956692727,
23.6912692359449));
#57159=CARTESIAN_POINT('Ctrl Pts',(-14.8187520767123,-35.1638753076392,
23.4941897833765));
#57160=CARTESIAN_POINT('Ctrl Pts',(-12.7785249527297,-31.0595652802824,
23.2971103308081));
#57161=CARTESIAN_POINT('Ctrl Pts',(-8.2274202757673,-30.5161191123635,23.1000308782396));
#57162=CARTESIAN_POINT('Ctrl Pts',(-5.27814776377262,-34.0246343493302,
22.9029514256712));
#57163=CARTESIAN_POINT('Ctrl Pts',(-6.59588490261864,-38.4145610401807,
22.7058719731027));
#57164=CARTESIAN_POINT('Ctrl Pts',(-10.989828421184,-39.7188416364419,22.5087925205343));
#57165=CARTESIAN_POINT('Ctrl Pts',(-14.4892908728541,-36.7588331791699,
22.3117130679658));
#57166=CARTESIAN_POINT('Ctrl Pts',(-13.9319030629373,-32.2094149363679,
22.1146336153974));
#57167=CARTESIAN_POINT('Ctrl Pts',(-9.8213612200649,-30.1817726414334,21.917554162829));
#57168=CARTESIAN_POINT('Ctrl Pts',(-5.8722503921224,-32.5082315781925,21.7204747102605));
#57169=CARTESIAN_POINT('Ctrl Pts',(-5.65327480142373,-37.0864339779578,
21.5233952576921));
#57170=CARTESIAN_POINT('Ctrl Pts',(-9.36231674438557,-39.7791826447939,
21.3263158051236));
#57171=CARTESIAN_POINT('Ctrl Pts',(-13.6476157286711,-38.1531137295354,
21.1292363525552));
#57172=CARTESIAN_POINT('Ctrl Pts',(-14.6366634274731,-33.6776615506337,
20.9321568999867));
#57173=CARTESIAN_POINT('Ctrl Pts',(-11.4356842831145,-30.3971707311702,
20.7350774474183));
#57174=CARTESIAN_POINT('Ctrl Pts',(-6.9373162471913,-31.2761317210392,20.5379979948499));
#57175=CARTESIAN_POINT('Ctrl Pts',(-5.20661233371697,-35.5202513937734,
20.3409185422814));
#57176=CARTESIAN_POINT('Ctrl Pts',(-7.80756274108455,-39.294233938127,20.143839089713));
#57177=CARTESIAN_POINT('Ctrl Pts',(-12.38975907867,-39.1876340166796,19.9467596371445));
#57178=CARTESIAN_POINT('Ctrl Pts',(-14.8123952029925,-35.2967826638352,
19.7496801845761));
#57179=CARTESIAN_POINT('Ctrl Pts',(-12.8862001060391,-31.1377374333175,
19.5526007320077));
#57180=CARTESIAN_POINT('Ctrl Pts',(-8.35182504074954,-30.4689129009811,
19.3555212794392));
#57181=CARTESIAN_POINT('Ctrl Pts',(-5.30685954432354,-33.8947109540756,
19.1584418268708));
#57182=CARTESIAN_POINT('Ctrl Pts',(-6.50296040670598,-38.3193243056809,
18.9613623743023));
#57183=CARTESIAN_POINT('Ctrl Pts',(-10.8592354868165,-39.7443631764007,
18.7642829217339));
#57184=CARTESIAN_POINT('Ctrl Pts',(-14.4390537541248,-36.8820324187471,
18.5672034691654));
#57185=CARTESIAN_POINT('Ctrl Pts',(-14.0073978409461,-32.3189948263819,
18.370124016597));
#57186=CARTESIAN_POINT('Ctrl Pts',(-9.95440880910246,-30.1786395849428,
18.1730445640285));
#57187=CARTESIAN_POINT('Ctrl Pts',(-5.94253267211965,-32.3953547057049,
17.9759651114601));
#57188=CARTESIAN_POINT('Ctrl Pts',(-5.59745211347252,-36.9655424623781,
17.7788856588917));
#57189=CARTESIAN_POINT('Ctrl Pts',(-9.23049091074666,-39.7600697589106,
17.5818062063232));
#57190=CARTESIAN_POINT('Ctrl Pts',(-13.5595986838708,-38.2519619715973,
17.3847267537548));
#57191=CARTESIAN_POINT('Ctrl Pts',(-14.6706288037252,-33.8073150519438,
17.1876473011863));
#57192=CARTESIAN_POINT('Ctrl Pts',(-11.5636788830593,-30.4361277555464,
16.9905678486179));
#57193=CARTESIAN_POINT('Ctrl Pts',(-7.03690775456509,-31.1981823891181,
16.7934426556376));
#57194=CARTESIAN_POINT('Ctrl Pts',(-5.81501521204634,-33.9850050967667,
16.6620106135137));
#57195=CARTESIAN_POINT('Ctrl Pts',(-5.92468338351297,-35.3316613902157,
16.5962717222458));
#57196=CARTESIAN_POINT('Ctrl Pts',(-10.9980261717899,-38.7223121573106,
30.1334916522396));
#57197=CARTESIAN_POINT('Ctrl Pts',(-12.2271700957341,-38.3927541425204,
30.0677985013834));
#57198=CARTESIAN_POINT('Ctrl Pts',(-14.3129051992123,-36.4262766866223,
29.9364121996711));
#57199=CARTESIAN_POINT('Ctrl Pts',(-13.5568281581637,-32.1672425367211,
29.7393327471027));
#57200=CARTESIAN_POINT('Ctrl Pts',(-9.58052326701321,-30.4759605359757,
29.5422532945342));
#57201=CARTESIAN_POINT('Ctrl Pts',(-5.986271412028,-32.8691244189901,29.3451738419658));
#57202=CARTESIAN_POINT('Ctrl Pts',(-6.01762209774973,-37.1898015471262,
29.1480943893974));
#57203=CARTESIAN_POINT('Ctrl Pts',(-9.6484899656477,-39.5306620003194,28.9510149368289));
#57204=CARTESIAN_POINT('Ctrl Pts',(-13.5966311448511,-37.7777643935561,
28.7539354842605));
#57205=CARTESIAN_POINT('Ctrl Pts',(-14.2947835907645,-33.5144364486947,
28.5568560316921));
#57206=CARTESIAN_POINT('Ctrl Pts',(-11.1117617415225,-30.5936924916062,
28.3597765791236));
#57207=CARTESIAN_POINT('Ctrl Pts',(-6.9241186856516,-31.6547484574022,28.1626971265552));
#57208=CARTESIAN_POINT('Ctrl Pts',(-5.51604210683472,-35.7388477967325,
27.9656176739867));
#57209=CARTESIAN_POINT('Ctrl Pts',(-8.16000854383523,-39.1552551856891,
27.7685382214183));
#57210=CARTESIAN_POINT('Ctrl Pts',(-12.4667192606622,-38.816678954707,27.5714587688498));
#57211=CARTESIAN_POINT('Ctrl Pts',(-14.5443257928935,-35.0290697419017,
27.3743793162814));
#57212=CARTESIAN_POINT('Ctrl Pts',(-12.5153469787341,-31.2151929241783,
27.177299863713));
#57213=CARTESIAN_POINT('Ctrl Pts',(-8.2133181646357,-30.8215425201386,26.9802204111445));
#57214=CARTESIAN_POINT('Ctrl Pts',(-5.52586482672684,-34.2038511676513,
26.7831409585761));
#57215=CARTESIAN_POINT('Ctrl Pts',(-6.88156614891665,-38.3056176522011,
26.5860615060077));
#57216=CARTESIAN_POINT('Ctrl Pts',(-11.0553113690653,-39.4201873464575,
26.3889820534392));
#57217=CARTESIAN_POINT('Ctrl Pts',(-14.2754004090027,-36.540353697843,26.1919026008708));
#57218=CARTESIAN_POINT('Ctrl Pts',(-13.6319261672203,-32.2685442695009,
25.9948231483023));
#57219=CARTESIAN_POINT('Ctrl Pts',(-9.70637888003917,-30.465077200563,25.7977436957339));
#57220=CARTESIAN_POINT('Ctrl Pts',(-6.04616901996426,-32.7596967340437,
25.6006642431654));
#57221=CARTESIAN_POINT('Ctrl Pts',(-5.9589288591031,-37.0788174928738,25.403584790597));
#57222=CARTESIAN_POINT('Ctrl Pts',(-9.52349495730953,-39.5193673326274,
25.2065053380285));
#57223=CARTESIAN_POINT('Ctrl Pts',(-13.5186657245719,-37.8758876297465,
25.0094258854601));
#57224=CARTESIAN_POINT('Ctrl Pts',(-14.3341138203995,-33.6335463669068,
24.8123464328917));
#57225=CARTESIAN_POINT('Ctrl Pts',(-11.2329409434872,-30.6260321479827,
24.6152669803232));
#57226=CARTESIAN_POINT('Ctrl Pts',(-7.01759281456559,-31.5711539083146,
24.4181875277548));
#57227=CARTESIAN_POINT('Ctrl Pts',(-5.49736507623987,-35.6148307763096,
24.2211080751863));
#57228=CARTESIAN_POINT('Ctrl Pts',(-8.04604625598683,-39.1029017666212,
24.0240286226179));
#57229=CARTESIAN_POINT('Ctrl Pts',(-12.3604623774382,-38.8832918387528,
23.8269491700494));
#57230=CARTESIAN_POINT('Ctrl Pts',(-14.5417927433158,-35.1544565213557,
23.629869717481));
#57231=CARTESIAN_POINT('Ctrl Pts',(-12.6188283328409,-31.2860430396466,
23.4327902649126));
#57232=CARTESIAN_POINT('Ctrl Pts',(-8.32929986845024,-30.7738316159119,
23.2357108123441));
#57233=CARTESIAN_POINT('Ctrl Pts',(-5.54953774751175,-34.0806938054149,
23.0386313597757));
#57234=CARTESIAN_POINT('Ctrl Pts',(-6.79153751830967,-38.2183080405503,
22.8415519072072));
#57235=CARTESIAN_POINT('Ctrl Pts',(-10.9329377126885,-39.4476246878987,
22.6444724546388));
#57236=CARTESIAN_POINT('Ctrl Pts',(-14.2312674286564,-36.6577436736085,
22.4473930020703));
#57237=CARTESIAN_POINT('Ctrl Pts',(-13.7059156633048,-32.3698047150298,
22.2503135495019));
#57238=CARTESIAN_POINT('Ctrl Pts',(-9.83162854169131,-30.4587018164847,
22.0532340969334));
#57239=CARTESIAN_POINT('Ctrl Pts',(-6.10949413523795,-32.651446773765,21.856154644365));
#57240=CARTESIAN_POINT('Ctrl Pts',(-5.90310423740425,-36.9665155105805,
21.6590751917966));
#57241=CARTESIAN_POINT('Ctrl Pts',(-9.39896779564977,-39.5044975772889,
21.4619957392281));
#57242=CARTESIAN_POINT('Ctrl Pts',(-13.4379678354787,-37.971887498604,21.2649162866597));
#57243=CARTESIAN_POINT('Ctrl Pts',(-14.3701696980567,-33.7536633804914,
21.0678368340912));
#57244=CARTESIAN_POINT('Ctrl Pts',(-11.35316786482,-30.6617198313809,20.8707573815228));
#57245=CARTESIAN_POINT('Ctrl Pts',(-7.11334498597645,-31.4901622542101,
20.6736779289544));
#57246=CARTESIAN_POINT('Ctrl Pts',(-5.48211383942423,-35.4903497767315,
20.4765984763859));
#57247=CARTESIAN_POINT('Ctrl Pts',(-7.93357378130328,-39.0474214543101,
20.2795190238175));
#57248=CARTESIAN_POINT('Ctrl Pts',(-12.2524069030715,-38.946948397809,20.082439571249));
#57249=CARTESIAN_POINT('Ctrl Pts',(-14.5358012329681,-35.2797249842885,
19.8853601186806));
#57250=CARTESIAN_POINT('Ctrl Pts',(-12.720314821905,-31.3597222229148,19.6882806661121));
#57251=CARTESIAN_POINT('Ctrl Pts',(-8.44655442934804,-30.7293385967893,
19.4912012135437));
#57252=CARTESIAN_POINT('Ctrl Pts',(-5.57659930919367,-33.9582377993036,
19.2941217609752));
#57253=CARTESIAN_POINT('Ctrl Pts',(-6.70395388783986,-38.1285450681538,
19.0970423084068));
#57254=CARTESIAN_POINT('Ctrl Pts',(-10.8098506494414,-39.4716793690978,
18.8999628558384));
#57255=CARTESIAN_POINT('Ctrl Pts',(-14.1839177045665,-36.7738619970635,
18.7028834032699));
#57256=CARTESIAN_POINT('Ctrl Pts',(-13.7770713545418,-32.4730864654405,
18.5058039507015));
#57257=CARTESIAN_POINT('Ctrl Pts',(-9.95702917753784,-30.4557488334288,
18.3087244981331));
#57258=CARTESIAN_POINT('Ctrl Pts',(-6.17573691847179,-32.5450575360141,
18.1116450455646));
#57259=CARTESIAN_POINT('Ctrl Pts',(-5.85048997648918,-36.8525722739401,
17.9145655929962));
#57260=CARTESIAN_POINT('Ctrl Pts',(-9.27471869441539,-39.4864832107005,
17.7174861404277));
#57261=CARTESIAN_POINT('Ctrl Pts',(-13.3550095987821,-38.0650544059981,
17.5204066878593));
#57262=CARTESIAN_POINT('Ctrl Pts',(-14.4021829033284,-33.8758650048999,
17.3233272352908));
#57263=CARTESIAN_POINT('Ctrl Pts',(-11.4738059337554,-30.6984377881871,
17.1262477827224));
#57264=CARTESIAN_POINT('Ctrl Pts',(-7.20721243926833,-31.4166930853403,
16.9291225897422));
#57265=CARTESIAN_POINT('Ctrl Pts',(-6.05554856563953,-34.0433422569536,
16.7976905476182));
#57266=CARTESIAN_POINT('Ctrl Pts',(-6.15891352349801,-35.3125990445948,
16.7319516563503));
#57267=CARTESIAN_POINT('Ctrl Pts',(-10.9371663574229,-38.4953248965424,
30.2691715863441));
#57268=CARTESIAN_POINT('Ctrl Pts',(-12.0913568651584,-38.1858633884072,
30.2034784354879));
#57269=CARTESIAN_POINT('Ctrl Pts',(-14.0499034691722,-36.3393020793051,
30.0720921337757));
#57270=CARTESIAN_POINT('Ctrl Pts',(-13.3399321412461,-32.3399845932268,
29.8750126812072));
#57271=CARTESIAN_POINT('Ctrl Pts',(-9.60610303317808,-30.7518372712273,
29.6779332286388));
#57272=CARTESIAN_POINT('Ctrl Pts',(-6.23102929883268,-32.9990655928438,
29.4808537760703));
#57273=CARTESIAN_POINT('Ctrl Pts',(-6.26046821413472,-37.0562670573248,
29.2837743235019));
#57274=CARTESIAN_POINT('Ctrl Pts',(-9.66992511037984,-39.2543814216206,
29.0866948709334));
#57275=CARTESIAN_POINT('Ctrl Pts',(-13.3773079346899,-37.6083758242728,
28.889615418365));
#57276=CARTESIAN_POINT('Ctrl Pts',(-14.032886919647,-33.6050263796185,28.6925359657965));
#57277=CARTESIAN_POINT('Ctrl Pts',(-11.0439663117815,-30.8623899111572,
28.4954565132281));
#57278=CARTESIAN_POINT('Ctrl Pts',(-7.11168647805739,-31.8587424944803,
28.2983770606597));
#57279=CARTESIAN_POINT('Ctrl Pts',(-5.78947466073016,-35.6937927260083,
28.1012976080912));
#57280=CARTESIAN_POINT('Ctrl Pts',(-8.27221155175637,-38.9018669816557,
27.9042181555228));
#57281=CARTESIAN_POINT('Ctrl Pts',(-12.3162982791864,-38.5839371897643,
27.7071387029544));
#57282=CARTESIAN_POINT('Ctrl Pts',(-14.267211993681,-35.0272970638439,27.5100592503859));
#57283=CARTESIAN_POINT('Ctrl Pts',(-12.3619606703174,-31.4459911362492,
27.3129797978175));
#57284=CARTESIAN_POINT('Ctrl Pts',(-8.32227034235058,-31.0763456042183,
27.115900345249));
#57285=CARTESIAN_POINT('Ctrl Pts',(-5.7986983894073,-34.2524004657706,26.9188208926806));
#57286=CARTESIAN_POINT('Ctrl Pts',(-7.07172880261939,-38.1040404968445,
26.7217414401122));
#57287=CARTESIAN_POINT('Ctrl Pts',(-10.990958293128,-39.1506435319003,26.5246619875437));
#57288=CARTESIAN_POINT('Ctrl Pts',(-14.0146857277741,-36.4464226539888,
26.3275825349753));
#57289=CARTESIAN_POINT('Ctrl Pts',(-13.4104506602856,-32.4351089282327,
26.1305030824068));
#57290=CARTESIAN_POINT('Ctrl Pts',(-9.72428394842326,-30.7416176035536,
25.9334236298383));
#57291=CARTESIAN_POINT('Ctrl Pts',(-6.28727433992944,-32.8963108276873,
25.7363441772699));
#57292=CARTESIAN_POINT('Ctrl Pts',(-6.205354099673,-36.9520508305407,25.5392647247015));
#57293=CARTESIAN_POINT('Ctrl Pts',(-9.55255231999473,-39.2437755047836,
25.342185272133));
#57294=CARTESIAN_POINT('Ctrl Pts',(-13.3040968596768,-37.7005154879794,
25.1451058195646));
#57295=CARTESIAN_POINT('Ctrl Pts',(-14.0698187848481,-33.7168729537256,
24.9480263669962));
#57296=CARTESIAN_POINT('Ctrl Pts',(-11.1577559843479,-30.8927574895067,
24.7509469144277));
#57297=CARTESIAN_POINT('Ctrl Pts',(-7.1994605378804,-31.7802455559398,24.5538674618593));
#57298=CARTESIAN_POINT('Ctrl Pts',(-5.77193655879976,-35.5773382856607,
24.3567880092908));
#57299=CARTESIAN_POINT('Ctrl Pts',(-8.1651987045933,-38.8527060834415,24.1597085567224));
#57300=CARTESIAN_POINT('Ctrl Pts',(-12.2165209596964,-38.6464880082329,
23.9626291041539));
#57301=CARTESIAN_POINT('Ctrl Pts',(-14.2648334099194,-35.1450377350721,
23.7655496515855));
#57302=CARTESIAN_POINT('Ctrl Pts',(-12.4591317129521,-31.5125207990106,
23.5684701990171));
#57303=CARTESIAN_POINT('Ctrl Pts',(-8.43117946113315,-31.0315441194603,
23.3713907464486));
#57304=CARTESIAN_POINT('Ctrl Pts',(-5.82092773125088,-34.1367532614996,
23.1743112938802));
#57305=CARTESIAN_POINT('Ctrl Pts',(-6.98719013400071,-38.02205504092,22.9772318413117));
#57306=CARTESIAN_POINT('Ctrl Pts',(-10.8760470041931,-39.1764077393554,
22.7801523887433));
#57307=CARTESIAN_POINT('Ctrl Pts',(-13.9732439844587,-36.5566541680469,
22.5830729361748));
#57308=CARTESIAN_POINT('Ctrl Pts',(-13.4799282636722,-32.5301944936914,
22.3859934836064));
#57309=CARTESIAN_POINT('Ctrl Pts',(-9.84189586331774,-30.7356309915362,
22.188914031038));
#57310=CARTESIAN_POINT('Ctrl Pts',(-6.34673787835349,-32.7946619693375,
21.9918345784695));
#57311=CARTESIAN_POINT('Ctrl Pts',(-6.15293367338478,-36.8465970432031,
21.7947551259011));
#57312=CARTESIAN_POINT('Ctrl Pts',(-9.43561884691396,-39.2298125097838,
21.5976756733326));
#57313=CARTESIAN_POINT('Ctrl Pts',(-13.2283199422864,-37.7906612676727,
21.4005962207642));
#57314=CARTESIAN_POINT('Ctrl Pts',(-14.1036759686402,-33.8296652103491,
21.2035167681957));
#57315=CARTESIAN_POINT('Ctrl Pts',(-11.2706514465257,-30.9262689315915,
21.0064373156273));
#57316=CARTESIAN_POINT('Ctrl Pts',(-7.28937372476156,-31.7041927873809,
20.8093578630588));
#57317=CARTESIAN_POINT('Ctrl Pts',(-5.75761534513151,-35.4604481596895,
20.6122784104904));
#57318=CARTESIAN_POINT('Ctrl Pts',(-8.05958482152201,-38.800608970493,20.415198957922));
#57319=CARTESIAN_POINT('Ctrl Pts',(-12.1150547274729,-38.7062627789383,
20.2181195053535));
#57320=CARTESIAN_POINT('Ctrl Pts',(-14.2592072629438,-35.2626673047419,
20.0210400527851));
#57321=CARTESIAN_POINT('Ctrl Pts',(-12.5544295377709,-31.581707012512,19.8239606002167));
#57322=CARTESIAN_POINT('Ctrl Pts',(-8.54128381794652,-30.9897642925976,
19.6268811476482));
#57323=CARTESIAN_POINT('Ctrl Pts',(-5.8463390740638,-34.0217646445317,19.4298016950797));
#57324=CARTESIAN_POINT('Ctrl Pts',(-6.90494736897375,-37.9377658306266,
19.2327222425113));
#57325=CARTESIAN_POINT('Ctrl Pts',(-10.7604658120663,-39.198995561795,19.0356427899429));
#57326=CARTESIAN_POINT('Ctrl Pts',(-13.9287816550082,-36.6656915753799,
18.8385633373744));
#57327=CARTESIAN_POINT('Ctrl Pts',(-13.5467448681375,-32.6271781044991,
18.641483884806));
#57328=CARTESIAN_POINT('Ctrl Pts',(-9.95964954597322,-30.7328580819148,
18.4444044322375));
#57329=CARTESIAN_POINT('Ctrl Pts',(-6.40894116482391,-32.6947603663233,
18.2473249796691));
#57330=CARTESIAN_POINT('Ctrl Pts',(-6.10352783950584,-36.739602085502,18.0502455271006));
#57331=CARTESIAN_POINT('Ctrl Pts',(-9.31894647808413,-39.2128966624903,
17.8531660745322));
#57332=CARTESIAN_POINT('Ctrl Pts',(-13.1504205136935,-37.878146840399,17.6560866219638));
#57333=CARTESIAN_POINT('Ctrl Pts',(-14.1337370029317,-33.944414957856,17.4590071693953));
#57334=CARTESIAN_POINT('Ctrl Pts',(-11.3839329844517,-30.9607478208279,
17.2619277168269));
#57335=CARTESIAN_POINT('Ctrl Pts',(-7.37751712397162,-31.6352037815626,
17.0648025238468));
#57336=CARTESIAN_POINT('Ctrl Pts',(-6.29608191923271,-34.1016794171405,
16.9333704817227));
#57337=CARTESIAN_POINT('Ctrl Pts',(-6.39314366348305,-35.293536698974,16.8676315904548));
#57338=CARTESIAN_POINT('Ctrl Pts',(-10.876306543056,-38.2683376357742,30.4048515204486));
#57339=CARTESIAN_POINT('Ctrl Pts',(-11.9555436345827,-37.978972634294,30.3391583695924));
#57340=CARTESIAN_POINT('Ctrl Pts',(-13.7869017391321,-36.2523274719879,
30.2077720678801));
#57341=CARTESIAN_POINT('Ctrl Pts',(-13.1230361243285,-32.5127266497326,
30.0106926153117));
#57342=CARTESIAN_POINT('Ctrl Pts',(-9.63168279934295,-31.0277140064789,
29.8136131627432));
#57343=CARTESIAN_POINT('Ctrl Pts',(-6.47578718563735,-33.1290067666977,
29.6165337101748));
#57344=CARTESIAN_POINT('Ctrl Pts',(-6.50331433051971,-36.9227325675234,
29.4194542576064));
#57345=CARTESIAN_POINT('Ctrl Pts',(-9.69136025511198,-38.9781008429219,
29.2223748050379));
#57346=CARTESIAN_POINT('Ctrl Pts',(-13.1579847245288,-37.4389872549895,
29.0252953524695));
#57347=CARTESIAN_POINT('Ctrl Pts',(-13.7709902485295,-33.6956163105424,
28.8282158999011));
#57348=CARTESIAN_POINT('Ctrl Pts',(-10.9761708820405,-31.1310873307082,
28.6311364473326));
#57349=CARTESIAN_POINT('Ctrl Pts',(-7.29925427046318,-32.0627365315584,
28.4340569947642));
#57350=CARTESIAN_POINT('Ctrl Pts',(-6.06290721462558,-35.6487376552842,
28.2369775421957));
#57351=CARTESIAN_POINT('Ctrl Pts',(-8.38441455967752,-38.6484787776224,
28.0398980896273));
#57352=CARTESIAN_POINT('Ctrl Pts',(-12.1658772977107,-38.3511954248215,
27.8428186370589));
#57353=CARTESIAN_POINT('Ctrl Pts',(-13.9900981944685,-35.0255243857861,
27.6457391844904));
#57354=CARTESIAN_POINT('Ctrl Pts',(-12.2085743619008,-31.67678934832,27.448659731922));
#57355=CARTESIAN_POINT('Ctrl Pts',(-8.43122252006548,-31.3311486882979,
27.2515802793535));
#57356=CARTESIAN_POINT('Ctrl Pts',(-6.07153195208776,-34.3009497638899,
27.0545008267851));
#57357=CARTESIAN_POINT('Ctrl Pts',(-7.26189145632214,-37.9024633414879,
26.8574213742166));
#57358=CARTESIAN_POINT('Ctrl Pts',(-10.9266052171908,-38.881099717343,26.6603419216482));
#57359=CARTESIAN_POINT('Ctrl Pts',(-13.7539710465455,-36.3524916101345,
26.4632624690798));
#57360=CARTESIAN_POINT('Ctrl Pts',(-13.188975153351,-32.6016735869645,26.2661830165113));
#57361=CARTESIAN_POINT('Ctrl Pts',(-9.74218901680736,-31.0181580065441,
26.0691035639429));
#57362=CARTESIAN_POINT('Ctrl Pts',(-6.52837965989463,-33.0329249213308,
25.8720241113744));
#57363=CARTESIAN_POINT('Ctrl Pts',(-6.4517793402429,-36.8252841682075,25.674944658806));
#57364=CARTESIAN_POINT('Ctrl Pts',(-9.58160968267994,-38.9681836769399,
25.4778652062375));
#57365=CARTESIAN_POINT('Ctrl Pts',(-13.0895279947817,-37.5251433462124,
25.2807857536691));
#57366=CARTESIAN_POINT('Ctrl Pts',(-13.8055237492966,-33.8001995405442,
25.0837063011006));
#57367=CARTESIAN_POINT('Ctrl Pts',(-11.0825710252086,-31.1594828310307,
24.8866268485322));
#57368=CARTESIAN_POINT('Ctrl Pts',(-7.3813282611952,-31.989337203565,24.6895473959638));
#57369=CARTESIAN_POINT('Ctrl Pts',(-6.04650804135964,-35.5398457950117,
24.4924679433953));
#57370=CARTESIAN_POINT('Ctrl Pts',(-8.2843511531998,-38.6025104002618,24.2953884908269));
#57371=CARTESIAN_POINT('Ctrl Pts',(-12.0725795419546,-38.409684177713,24.0983090382584));
#57372=CARTESIAN_POINT('Ctrl Pts',(-13.9878740765231,-35.1356189487886,
23.90122958569));
#57373=CARTESIAN_POINT('Ctrl Pts',(-12.2994350930632,-31.7389985583748,
23.7041501331215));
#57374=CARTESIAN_POINT('Ctrl Pts',(-8.53305905381608,-31.2892566230088,
23.5070706805531));
#57375=CARTESIAN_POINT('Ctrl Pts',(-6.09231771499001,-34.1928127175841,
23.3099912279846));
#57376=CARTESIAN_POINT('Ctrl Pts',(-7.18284274969174,-37.8258020412897,
23.1129117754162));
#57377=CARTESIAN_POINT('Ctrl Pts',(-10.8191562956977,-38.9051907908123,
22.9158323228478));
#57378=CARTESIAN_POINT('Ctrl Pts',(-13.7152205402609,-36.4555646624855,
22.7187528702793));
#57379=CARTESIAN_POINT('Ctrl Pts',(-13.2539408640396,-32.6905842723531,
22.5216734177109));
#57380=CARTESIAN_POINT('Ctrl Pts',(-9.85216318494415,-31.0125601665875,
22.3245939651425));
#57381=CARTESIAN_POINT('Ctrl Pts',(-6.58398162146904,-32.9378771649101,
22.127514512574));
#57382=CARTESIAN_POINT('Ctrl Pts',(-6.40276310936531,-36.7266785758257,
21.9304350600056));
#57383=CARTESIAN_POINT('Ctrl Pts',(-9.47226989817816,-38.9551274422788,
21.7333556074371));
#57384=CARTESIAN_POINT('Ctrl Pts',(-13.0186720490941,-37.6094350367414,
21.5362761548687));
#57385=CARTESIAN_POINT('Ctrl Pts',(-13.8371822392237,-33.9056670402069,
21.3391967023002));
#57386=CARTESIAN_POINT('Ctrl Pts',(-11.1881350282313,-31.1908180318022,
21.1421172497318));
#57387=CARTESIAN_POINT('Ctrl Pts',(-7.4654024635467,-31.9182233205518,20.9450377971633));
#57388=CARTESIAN_POINT('Ctrl Pts',(-6.03311685083878,-35.4305465426475,
20.7479583445949));
#57389=CARTESIAN_POINT('Ctrl Pts',(-8.18559586174073,-38.553796486676,20.5508788920265));
#57390=CARTESIAN_POINT('Ctrl Pts',(-11.9777025518743,-38.4655771600677,
20.353799439458));
#57391=CARTESIAN_POINT('Ctrl Pts',(-13.9826132929195,-35.2456096251953,
20.1567199868896));
#57392=CARTESIAN_POINT('Ctrl Pts',(-12.3885442536368,-31.8036918021093,
19.9596405343211));
#57393=CARTESIAN_POINT('Ctrl Pts',(-8.63601320654501,-31.2501899884059,
19.7625610817527));
#57394=CARTESIAN_POINT('Ctrl Pts',(-6.11607883893393,-34.0852914897597,
19.5654816291843));
#57395=CARTESIAN_POINT('Ctrl Pts',(-7.10594085010763,-37.7469865930994,
19.3684021766158));
#57396=CARTESIAN_POINT('Ctrl Pts',(-10.7110809746912,-38.9263117544921,
19.1713227240473));
#57397=CARTESIAN_POINT('Ctrl Pts',(-13.6736456054499,-36.5575211536964,
18.9742432714789));
#57398=CARTESIAN_POINT('Ctrl Pts',(-13.3164183817332,-32.7812697435577,
18.7771638189105));
#57399=CARTESIAN_POINT('Ctrl Pts',(-9.9622699144086,-31.0099673304008,18.5800843663421));
#57400=CARTESIAN_POINT('Ctrl Pts',(-6.64214541117603,-32.8444631966324,
18.3830049137736));
#57401=CARTESIAN_POINT('Ctrl Pts',(-6.3565657025225,-36.6266318970639,18.1859254612052));
#57402=CARTESIAN_POINT('Ctrl Pts',(-9.36317426175285,-38.9393101142802,
17.9888460086367));
#57403=CARTESIAN_POINT('Ctrl Pts',(-12.9458314286048,-37.6912392747999,
17.7917665560683));
#57404=CARTESIAN_POINT('Ctrl Pts',(-13.865291102535,-34.0129649108121,17.5946871034998));
#57405=CARTESIAN_POINT('Ctrl Pts',(-11.2940600351478,-31.2230578534687,
17.3976076509314));
#57406=CARTESIAN_POINT('Ctrl Pts',(-7.54782180867489,-31.8537144777848,
17.2004824579512));
#57407=CARTESIAN_POINT('Ctrl Pts',(-6.53661527282589,-34.1600165773275,
17.0690504158272));
#57408=CARTESIAN_POINT('Ctrl Pts',(-6.62737380346809,-35.2744743533532,
17.0033115245594));
#57409=CARTESIAN_POINT('',(-12.5757531795041,-32.7919405097392,30.0016970964046));
#57410=CARTESIAN_POINT('Ctrl Pts',(-12.5735562464391,-32.7938238264104,
30.0016970964046));
#57411=CARTESIAN_POINT('Ctrl Pts',(-12.5615843318249,-32.7798583072438,
30.0011313976031));
#57412=CARTESIAN_POINT('Ctrl Pts',(-12.5494987379337,-32.7659902394485,
30.0005656988015));
#57413=CARTESIAN_POINT('Ctrl Pts',(-12.5373010662035,-32.7522214606544,
30.));
#57414=CARTESIAN_POINT('Ctrl Pts',(-11.0579044229731,-38.9456385074984,
30.));
#57415=CARTESIAN_POINT('Ctrl Pts',(-11.1744096706663,-38.9036233586964,
30.));
#57416=CARTESIAN_POINT('Ctrl Pts',(-11.2885140055709,-38.8559987888831,
30.));
#57417=CARTESIAN_POINT('Ctrl Pts',(-11.3999875271948,-38.8031290833885,
30.));
#57418=CARTESIAN_POINT('Ctrl Pts',(-11.5131043589436,-38.7494799881242,
30.));
#57419=CARTESIAN_POINT('Ctrl Pts',(-11.6235128455776,-38.690429357792,30.));
#57420=CARTESIAN_POINT('Ctrl Pts',(-11.7309450457163,-38.6263105171745,
30.));
#57421=CARTESIAN_POINT('Ctrl Pts',(-11.8388142181791,-38.5619308780369,
30.));
#57422=CARTESIAN_POINT('Ctrl Pts',(-11.9436834175853,-38.4924410128984,
30.));
#57423=CARTESIAN_POINT('Ctrl Pts',(-12.0452448209239,-38.4181410778747,
30.));
#57424=CARTESIAN_POINT('Ctrl Pts',(-12.1415282742907,-38.3477023669682,
30.));
#57425=CARTESIAN_POINT('Ctrl Pts',(-12.2348389156493,-38.2729397397906,
30.));
#57426=CARTESIAN_POINT('Ctrl Pts',(-12.3248772751976,-38.1940868171024,
30.));
#57427=CARTESIAN_POINT('Ctrl Pts',(-12.3423412091291,-38.1787924221463,
30.));
#57428=CARTESIAN_POINT('Ctrl Pts',(-12.3596819162977,-38.1633440964326,
30.));
#57429=CARTESIAN_POINT('Ctrl Pts',(-12.3768970324285,-38.1477434784525,
30.));
#57430=CARTESIAN_POINT('Ctrl Pts',(-12.3882097974424,-38.1374916669666,
30.));
#57431=CARTESIAN_POINT('Ctrl Pts',(-12.3994663625361,-38.1271758271379,
30.));
#57432=CARTESIAN_POINT('Ctrl Pts',(-12.4106599136893,-38.1168023488082,
30.));
#57433=CARTESIAN_POINT('Ctrl Pts',(-12.5011105162613,-38.0329784261902,
30.));
#57434=CARTESIAN_POINT('Ctrl Pts',(-12.587570228655,-37.9452850315018,30.));
#57435=CARTESIAN_POINT('Ctrl Pts',(-12.6697818789516,-37.854037402353,30.));
#57436=CARTESIAN_POINT('Ctrl Pts',(-12.7516039958967,-37.7632221206229,
30.));
#57437=CARTESIAN_POINT('Ctrl Pts',(-12.8292186797432,-37.6688854688381,
30.));
#57438=CARTESIAN_POINT('Ctrl Pts',(-12.902329952052,-37.5713094616899,30.));
#57439=CARTESIAN_POINT('Ctrl Pts',(-12.973771793756,-37.4759615155162,30.));
#57440=CARTESIAN_POINT('Ctrl Pts',(-13.0409138149038,-37.3775197612551,
30.));
#57441=CARTESIAN_POINT('Ctrl Pts',(-13.1034339775746,-37.2762304601522,
30.));
#57442=CARTESIAN_POINT('Ctrl Pts',(-13.1564891880338,-37.1902753864973,
30.));
#57443=CARTESIAN_POINT('Ctrl Pts',(-13.2062154030788,-37.1022692102076,
30.));
#57444=CARTESIAN_POINT('Ctrl Pts',(-13.2523866301025,-37.012357944282,30.));
#57445=CARTESIAN_POINT('Ctrl Pts',(-13.2633295087652,-36.9910483942254,
30.));
#57446=CARTESIAN_POINT('Ctrl Pts',(-13.2740725700391,-36.9696318241106,
30.));
#57447=CARTESIAN_POINT('Ctrl Pts',(-13.2846125648802,-36.948110170831,30.));
#57448=CARTESIAN_POINT('Ctrl Pts',(-13.2922655181554,-36.9324835780826,
30.));
#57449=CARTESIAN_POINT('Ctrl Pts',(-13.2998074679507,-36.9168095952847,
30.));
#57450=CARTESIAN_POINT('Ctrl Pts',(-13.3072357732831,-36.9010928608241,
30.));
#57451=CARTESIAN_POINT('Ctrl Pts',(-13.3571186448737,-36.795551177783,30.));
#57452=CARTESIAN_POINT('Ctrl Pts',(-13.4019075471307,-36.6880280906304,
30.));
#57453=CARTESIAN_POINT('Ctrl Pts',(-13.4413371254717,-36.5787736678,30.));
#57454=CARTESIAN_POINT('Ctrl Pts',(-13.4805534288888,-36.4701102030702,
30.));
#57455=CARTESIAN_POINT('Ctrl Pts',(-13.5144685808348,-36.3597334673255,
30.));
#57456=CARTESIAN_POINT('Ctrl Pts',(-13.5427714797555,-36.2478788313556,
30.));
#57457=CARTESIAN_POINT('Ctrl Pts',(-13.5490241675936,-36.2231678600901,
30.));
#57458=CARTESIAN_POINT('Ctrl Pts',(-13.5550027386183,-36.1983847374895,
30.));
#57459=CARTESIAN_POINT('Ctrl Pts',(-13.5607034802902,-36.1735319763925,
30.));
#57460=CARTESIAN_POINT('Ctrl Pts',(-13.5872167898843,-36.0579454462257,
30.));
#57461=CARTESIAN_POINT('Ctrl Pts',(-13.6077246013846,-35.9408518074948,
30.));
#57462=CARTESIAN_POINT('Ctrl Pts',(-13.622313567663,-35.8226895292052,30.));
#57463=CARTESIAN_POINT('Ctrl Pts',(-13.6304386582349,-35.7568809451723,
30.));
#57464=CARTESIAN_POINT('Ctrl Pts',(-13.6367269390635,-35.6907410456955,
30.));
#57465=CARTESIAN_POINT('Ctrl Pts',(-13.6411867179029,-35.6243477453809,
30.));
#57466=CARTESIAN_POINT('Ctrl Pts',(-13.6425502406279,-35.6040488074671,
30.));
#57467=CARTESIAN_POINT('Ctrl Pts',(-13.6437428108378,-35.5837261979104,
30.));
#57468=CARTESIAN_POINT('Ctrl Pts',(-13.6447645818877,-35.5633821868984,
30.));
#57469=CARTESIAN_POINT('Ctrl Pts',(-13.6454919371615,-35.5489001522975,
30.));
#57470=CARTESIAN_POINT('Ctrl Pts',(-13.6461326209842,-35.5344089094296,
30.));
#57471=CARTESIAN_POINT('Ctrl Pts',(-13.6466864886703,-35.5199186950792,
30.));
#57472=CARTESIAN_POINT('Ctrl Pts',(-13.6511186439618,-35.4039652249222,
30.));
#57473=CARTESIAN_POINT('Ctrl Pts',(-13.6500048268794,-35.2879090483184,
30.));
#57474=CARTESIAN_POINT('Ctrl Pts',(-13.6434927288465,-35.172153928784,30.));
#57475=CARTESIAN_POINT('Ctrl Pts',(-13.6369459111642,-35.055781653741,30.));
#57476=CARTESIAN_POINT('Ctrl Pts',(-13.6249427915427,-34.939712732213,30.));
#57477=CARTESIAN_POINT('Ctrl Pts',(-13.6075814117316,-34.8243668994998,
30.));
#57478=CARTESIAN_POINT('Ctrl Pts',(-13.5904442763799,-34.710510905969,30.));
#57479=CARTESIAN_POINT('Ctrl Pts',(-13.568085985003,-34.5973586326097,30.));
#57480=CARTESIAN_POINT('Ctrl Pts',(-13.5405558990396,-34.4853357966022,
30.));
#57481=CARTESIAN_POINT('Ctrl Pts',(-13.5211239058209,-34.4062649577923,
30.));
#57482=CARTESIAN_POINT('Ctrl Pts',(-13.4991142948317,-34.327757263627,30.));
#57483=CARTESIAN_POINT('Ctrl Pts',(-13.474532315096,-34.2499724344563,30.));
#57484=CARTESIAN_POINT('Ctrl Pts',(-13.4674334198858,-34.2275093799274,
30.));
#57485=CARTESIAN_POINT('Ctrl Pts',(-13.4601199377529,-34.2051066720009,
30.));
#57486=CARTESIAN_POINT('Ctrl Pts',(-13.4525918509037,-34.1827683167229,
30.));
#57487=CARTESIAN_POINT('Ctrl Pts',(-13.4468393693237,-34.1656987770326,
30.));
#57488=CARTESIAN_POINT('Ctrl Pts',(-13.4409618009596,-34.1486676726928,
30.));
#57489=CARTESIAN_POINT('Ctrl Pts',(-13.4349636292873,-34.1316889240451,
30.));
#57490=CARTESIAN_POINT('Ctrl Pts',(-13.3973629896804,-34.0252545230712,
30.));
#57491=CARTESIAN_POINT('Ctrl Pts',(-13.3549838287623,-33.920747099218,30.));
#57492=CARTESIAN_POINT('Ctrl Pts',(-13.307891120105,-33.8185692933513,30.));
#57493=CARTESIAN_POINT('Ctrl Pts',(-13.267579990653,-33.7311055887387,30.));
#57494=CARTESIAN_POINT('Ctrl Pts',(-13.2238142902954,-33.6453489675918,
30.));
#57495=CARTESIAN_POINT('Ctrl Pts',(-13.1766120348928,-33.5615721686833,
30.));
#57496=CARTESIAN_POINT('Ctrl Pts',(-13.1583494816227,-33.5291589240236,
30.));
#57497=CARTESIAN_POINT('Ctrl Pts',(-13.1395722952297,-33.4970422713474,
30.));
#57498=CARTESIAN_POINT('Ctrl Pts',(-13.1202807524539,-33.4652389414177,
30.));
#57499=CARTESIAN_POINT('Ctrl Pts',(-13.1062080395183,-33.4420391829693,
30.));
#57500=CARTESIAN_POINT('Ctrl Pts',(-13.0918589518343,-33.4190020869106,
30.));
#57501=CARTESIAN_POINT('Ctrl Pts',(-13.0772443148201,-33.3961510770974,
30.));
#57502=CARTESIAN_POINT('Ctrl Pts',(-13.0739471956041,-33.3909957999949,
30.));
#57503=CARTESIAN_POINT('Ctrl Pts',(-13.0706366360367,-33.3858500994359,
30.));
#57504=CARTESIAN_POINT('Ctrl Pts',(-13.0673128268107,-33.3807143197486,
30.));
#57505=CARTESIAN_POINT('Ctrl Pts',(-13.0087456693047,-33.2902193492488,
30.));
#57506=CARTESIAN_POINT('Ctrl Pts',(-12.946022899502,-33.2027323003118,30.));
#57507=CARTESIAN_POINT('Ctrl Pts',(-12.879180959548,-33.1186350334298,30.));
#57508=CARTESIAN_POINT('Ctrl Pts',(-12.8123390195941,-33.0345377665478,
30.));
#57509=CARTESIAN_POINT('Ctrl Pts',(-12.7413776235882,-32.9538296256876,
30.));
#57510=CARTESIAN_POINT('Ctrl Pts',(-12.6663019920974,-32.8769345953137,
30.));
#57511=CARTESIAN_POINT('Ctrl Pts',(-12.6374947385807,-32.8474292206645,
30.));
#57512=CARTESIAN_POINT('Ctrl Pts',(-12.6080814062809,-32.8184857731937,
30.));
#57513=CARTESIAN_POINT('Ctrl Pts',(-12.5780826598067,-32.7901129261999,
30.));
#57514=CARTESIAN_POINT('Origin',(130.,35.,17.));
#57515=CARTESIAN_POINT('Ctrl Pts',(133.378768828602,34.7273715616999,17.));
#57516=CARTESIAN_POINT('Ctrl Pts',(133.398288233977,34.8335416259198,17.));
#57517=CARTESIAN_POINT('Ctrl Pts',(133.412279007432,34.9404514354858,17.0000000000001));
#57518=CARTESIAN_POINT('Ctrl Pts',(133.420978703021,35.0477528815053,17.0000000000001));
#57519=CARTESIAN_POINT('Ctrl Pts',(133.42967839861,35.1550543275247,17.0000000000002));
#57520=CARTESIAN_POINT('Ctrl Pts',(133.433086897826,35.2627480950217,17.0000000000003));
#57521=CARTESIAN_POINT('Ctrl Pts',(133.431392514054,35.3705051659232,17.0000000000002));
#57522=CARTESIAN_POINT('Ctrl Pts',(133.430532515791,35.425198143565,17.0000000000001));
#57523=CARTESIAN_POINT('Ctrl Pts',(133.428357163319,35.479907669662,17.0000000000001));
#57524=CARTESIAN_POINT('Ctrl Pts',(133.424886375688,35.5345917347118,17.0000000000001));
#57525=CARTESIAN_POINT('Ctrl Pts',(133.423593503532,35.5549616082467,17.0000000000001));
#57526=CARTESIAN_POINT('Ctrl Pts',(133.422121399213,35.5753190427029,17.));
#57527=CARTESIAN_POINT('Ctrl Pts',(133.420471724452,35.5956591262037,17.));
#57528=CARTESIAN_POINT('Ctrl Pts',(133.411386020314,35.7076836204683,17.));
#57529=CARTESIAN_POINT('Ctrl Pts',(133.396916614694,35.8192070065116,17.0000000000002));
#57530=CARTESIAN_POINT('Ctrl Pts',(133.377281468097,35.9298641207523,17.0000000000002));
#57531=CARTESIAN_POINT('Ctrl Pts',(133.36026028628,36.025789804401,17.0000000000001));
#57532=CARTESIAN_POINT('Ctrl Pts',(133.339356307749,36.1210651259812,17.));
#57533=CARTESIAN_POINT('Ctrl Pts',(133.314680099781,36.2154569772683,17.0000000000001));
#57534=CARTESIAN_POINT('Ctrl Pts',(133.305738302252,36.2496612935773,17.0000000000002));
#57535=CARTESIAN_POINT('Ctrl Pts',(133.296300907899,36.2837496130644,17.0000000000001));
#57536=CARTESIAN_POINT('Ctrl Pts',(133.286372264486,36.3177108224521,17.0000000000001));
#57537=CARTESIAN_POINT('Ctrl Pts',(133.27907397728,36.3426748230392,17.0000000000001));
#57538=CARTESIAN_POINT('Ctrl Pts',(133.271508428315,36.3675755235939,17.));
#57539=CARTESIAN_POINT('Ctrl Pts',(133.263687370245,36.3923772787486,17.));
#57540=CARTESIAN_POINT('Ctrl Pts',(133.229058695359,36.5021900314774,17.));
#57541=CARTESIAN_POINT('Ctrl Pts',(133.189398803451,36.6101610148702,16.9999999999999));
#57542=CARTESIAN_POINT('Ctrl Pts',(133.144932484444,36.7159227801683,17.));
#57543=CARTESIAN_POINT('Ctrl Pts',(133.099884875903,36.8230671246546,17.));
#57544=CARTESIAN_POINT('Ctrl Pts',(133.049904265293,36.9279449826529,17.));
#57545=CARTESIAN_POINT('Ctrl Pts',(132.995171184149,37.0301762722481,16.9999999999999));
#57546=CARTESIAN_POINT('Ctrl Pts',(132.940661033746,37.1319911683814,16.9999999999999));
#57547=CARTESIAN_POINT('Ctrl Pts',(132.881436812319,37.2311818991061,17.0000000000001));
#57548=CARTESIAN_POINT('Ctrl Pts',(132.817627108291,37.327361736492,17.0000000000001));
#57549=CARTESIAN_POINT('Ctrl Pts',(132.780025706327,37.3840380176536,17.0000000000001));
#57550=CARTESIAN_POINT('Ctrl Pts',(132.74083110084,37.4396685072474,17.0000000000001));
#57551=CARTESIAN_POINT('Ctrl Pts',(132.70006195955,37.4941703136841,16.9999999999999));
#57552=CARTESIAN_POINT('Ctrl Pts',(132.678439734566,37.5230757623517,16.9999999999999));
#57553=CARTESIAN_POINT('Ctrl Pts',(132.656374531928,37.5516636796183,16.9999999999999));
#57554=CARTESIAN_POINT('Ctrl Pts',(132.633868515218,37.579921261406,17.));
#57555=CARTESIAN_POINT('Ctrl Pts',(132.623918667431,37.592413860219,17.));
#57556=CARTESIAN_POINT('Ctrl Pts',(132.613883456604,37.6048407975903,17.0000000000001));
#57557=CARTESIAN_POINT('Ctrl Pts',(132.60377100071,37.6171915760467,17.0000000000001));
#57558=CARTESIAN_POINT('Ctrl Pts',(132.528292267067,37.7093770082662,17.));
#57559=CARTESIAN_POINT('Ctrl Pts',(132.448399939567,37.7974650775518,17.0000000000002));
#57560=CARTESIAN_POINT('Ctrl Pts',(132.364284930497,37.8810681553255,17.));
#57561=CARTESIAN_POINT('Ctrl Pts',(132.340799781667,37.9044103714878,17.));
#57562=CARTESIAN_POINT('Ctrl Pts',(132.316985154723,37.9274028855291,17.));
#57563=CARTESIAN_POINT('Ctrl Pts',(132.292844514065,37.9500370350214,17.));
#57564=CARTESIAN_POINT('Ctrl Pts',(132.208770395894,38.0288645270553,17.0000000000001));
#57565=CARTESIAN_POINT('Ctrl Pts',(132.12074560811,38.1033478921207,17.0000000000001));
#57566=CARTESIAN_POINT('Ctrl Pts',(132.029196142605,38.1734758687271,17.0000000000001));
#57567=CARTESIAN_POINT('Ctrl Pts',(131.937646677099,38.2436038453334,17.0000000000001));
#57568=CARTESIAN_POINT('Ctrl Pts',(131.842571858722,38.3093767105707,17.0000000000001));
#57569=CARTESIAN_POINT('Ctrl Pts',(131.744357347521,38.3707491714389,17.));
#57570=CARTESIAN_POINT('Ctrl Pts',(131.688282851896,38.4057891033832,16.9999999999999));
#57571=CARTESIAN_POINT('Ctrl Pts',(131.631184222155,38.4393939844899,17.));
#57572=CARTESIAN_POINT('Ctrl Pts',(131.573128638195,38.4715498712856,17.));
#57573=CARTESIAN_POINT('Ctrl Pts',(131.556944790657,38.4805137974726,17.));
#57574=CARTESIAN_POINT('Ctrl Pts',(131.540686561425,38.4893650974868,16.9999999999999));
#57575=CARTESIAN_POINT('Ctrl Pts',(131.524355368347,38.4981034100422,17.));
#57576=CARTESIAN_POINT('Ctrl Pts',(131.511360721652,38.5050564405907,17.0000000000001));
#57577=CARTESIAN_POINT('Ctrl Pts',(131.498320953668,38.5119373168649,17.));
#57578=CARTESIAN_POINT('Ctrl Pts',(131.485245644539,38.5187414041372,17.));
#57579=CARTESIAN_POINT('Ctrl Pts',(131.379199746276,38.5739252272921,17.));
#57580=CARTESIAN_POINT('Ctrl Pts',(131.270663835054,38.6241445793112,17.));
#57581=CARTESIAN_POINT('Ctrl Pts',(131.160092156422,38.6693989331698,17.));
#57582=CARTESIAN_POINT('Ctrl Pts',(131.047638905155,38.7154233698825,16.9999999999999));
#57583=CARTESIAN_POINT('Ctrl Pts',(130.93307935156,38.7563127793653,17.));
#57584=CARTESIAN_POINT('Ctrl Pts',(130.81685155244,38.7920288702004,17.));
#57585=CARTESIAN_POINT('Ctrl Pts',(130.699197470088,38.8281832491378,17.));
#57586=CARTESIAN_POINT('Ctrl Pts',(130.579833172242,38.8590369618314,17.));
#57587=CARTESIAN_POINT('Ctrl Pts',(130.459183611273,38.884506012631,17.));
#57588=CARTESIAN_POINT('Ctrl Pts',(130.384593215661,38.9002520009274,17.));
#57589=CARTESIAN_POINT('Ctrl Pts',(130.309511030868,38.9139389657507,17.));
#57590=CARTESIAN_POINT('Ctrl Pts',(130.234033981252,38.9255377255911,17.));
#57591=CARTESIAN_POINT('Ctrl Pts',(130.197793530202,38.9311068925151,17.));
#57592=CARTESIAN_POINT('Ctrl Pts',(130.16146201578,38.9361945229447,17.));
#57593=CARTESIAN_POINT('Ctrl Pts',(130.125050048296,38.9407967639506,17.));
#57594=CARTESIAN_POINT('Ctrl Pts',(130.107526906085,38.9430115776289,17.));
#57595=CARTESIAN_POINT('Ctrl Pts',(130.089983170934,38.9451141902373,17.));
#57596=CARTESIAN_POINT('Ctrl Pts',(130.072426243663,38.9471034374065,17.));
#57597=CARTESIAN_POINT('Ctrl Pts',(129.946714063481,38.9613469661689,17.));
#57598=CARTESIAN_POINT('Ctrl Pts',(129.820703192049,38.969740803944,17.));
#57599=CARTESIAN_POINT('Ctrl Pts',(129.694857535268,38.9722500045349,17.));
#57600=CARTESIAN_POINT('Ctrl Pts',(129.568768076596,38.9747640662221,17.));
#57601=CARTESIAN_POINT('Ctrl Pts',(129.442843586438,38.971370981313,17.));
#57602=CARTESIAN_POINT('Ctrl Pts',(129.317528116281,38.9619883570952,17.));
#57603=CARTESIAN_POINT('Ctrl Pts',(129.194473565428,38.9527750125059,17.));
#57604=CARTESIAN_POINT('Ctrl Pts',(129.072005379203,38.9377864472662,17.));
#57605=CARTESIAN_POINT('Ctrl Pts',(128.950535432686,38.916896007705,17.));
#57606=CARTESIAN_POINT('Ctrl Pts',(128.859101902848,38.90117124052,17.));
#57607=CARTESIAN_POINT('Ctrl Pts',(128.768233713755,38.8821015413518,17.0000000000001));
#57608=CARTESIAN_POINT('Ctrl Pts',(128.678107721738,38.859613353343,17.));
#57609=CARTESIAN_POINT('Ctrl Pts',(128.630400716805,38.8477095276847,17.));
#57610=CARTESIAN_POINT('Ctrl Pts',(128.582901718775,38.8348475473756,16.9999999999999));
#57611=CARTESIAN_POINT('Ctrl Pts',(128.535626794907,38.8210452480852,17.));
#57612=CARTESIAN_POINT('Ctrl Pts',(126.824949217806,37.5702679880679,17.));
#57613=CARTESIAN_POINT('Ctrl Pts',(126.754722583789,37.4668131880797,17.0000000000002));
#57614=CARTESIAN_POINT('Ctrl Pts',(126.689770370388,37.3600639476932,17.0000000000001));
#57615=CARTESIAN_POINT('Ctrl Pts',(126.630097099889,37.2504517185812,17.));
#57616=CARTESIAN_POINT('Ctrl Pts',(126.569576179664,37.1392824644374,16.9999999999999));
#57617=CARTESIAN_POINT('Ctrl Pts',(126.514485103446,37.0251674270994,17.0000000000002));
#57618=CARTESIAN_POINT('Ctrl Pts',(126.464879687316,36.9085416396813,17.));
#57619=CARTESIAN_POINT('Ctrl Pts',(126.443235336355,36.8576542634462,16.9999999999998));
#57620=CARTESIAN_POINT('Ctrl Pts',(126.422636031133,36.8062887679583,17.));
#57621=CARTESIAN_POINT('Ctrl Pts',(126.403089494403,36.7544810720487,17.));
#57622=CARTESIAN_POINT('Ctrl Pts',(126.392820972199,36.7272645639194,17.0000000000001));
#57623=CARTESIAN_POINT('Ctrl Pts',(126.38284168639,36.6999218975391,16.9999999999999));
#57624=CARTESIAN_POINT('Ctrl Pts',(126.373162067941,36.6724850908568,16.9999999999999));
#57625=CARTESIAN_POINT('Ctrl Pts',(126.331490348817,36.5543669121558,16.9999999999999));
#57626=CARTESIAN_POINT('Ctrl Pts',(126.295333444097,36.4344165564152,16.9999999999998));
#57627=CARTESIAN_POINT('Ctrl Pts',(126.264731412048,36.3130621740795,17.));
#57628=CARTESIAN_POINT('Ctrl Pts',(126.239068026807,36.2112923223389,17.0000000000001));
#57629=CARTESIAN_POINT('Ctrl Pts',(126.217312167367,36.1085345475138,16.9999999999999));
#57630=CARTESIAN_POINT('Ctrl Pts',(126.199515719586,36.0050412373779,16.9999999999998));
#57631=CARTESIAN_POINT('Ctrl Pts',(126.191672794255,35.9594315565208,16.9999999999998));
#57632=CARTESIAN_POINT('Ctrl Pts',(126.184599194475,35.9136790581849,17.0000000000001));
#57633=CARTESIAN_POINT('Ctrl Pts',(126.178300953791,35.8678056462447,17.));
#57634=CARTESIAN_POINT('Ctrl Pts',(126.175607684965,35.8481891475192,17.));
#57635=CARTESIAN_POINT('Ctrl Pts',(126.173056211163,35.828550541702,16.9999999999998));
#57636=CARTESIAN_POINT('Ctrl Pts',(126.170647058657,35.8088915581212,16.9999999999999));
#57637=CARTESIAN_POINT('Ctrl Pts',(126.168408509338,35.7906247177321,16.9999999999999));
#57638=CARTESIAN_POINT('Ctrl Pts',(126.166293315633,35.7723438132087,17.0000000000001));
#57639=CARTESIAN_POINT('Ctrl Pts',(126.164302713477,35.7540600423693,17.0000000000001));
#57640=CARTESIAN_POINT('Ctrl Pts',(126.151059358918,35.6324192317109,17.));
#57641=CARTESIAN_POINT('Ctrl Pts',(126.143310499907,35.510523911799,16.9999999999999));
#57642=CARTESIAN_POINT('Ctrl Pts',(126.141090098496,35.3887717903632,17.));
#57643=CARTESIAN_POINT('Ctrl Pts',(126.138887312408,35.267985576692,17.));
#57644=CARTESIAN_POINT('Ctrl Pts',(126.142125699594,35.1473394639188,16.9999999999999));
#57645=CARTESIAN_POINT('Ctrl Pts',(126.150888803704,35.0272284639509,17.));
#57646=CARTESIAN_POINT('Ctrl Pts',(126.15944062651,34.9100133794443,17.0000000000001));
#57647=CARTESIAN_POINT('Ctrl Pts',(126.173254171156,34.7933072394163,16.9999999999999));
#57648=CARTESIAN_POINT('Ctrl Pts',(126.192452956354,34.6774945709228,17.));
#57649=CARTESIAN_POINT('Ctrl Pts',(126.204155767891,34.6068998005225,17.));
#57650=CARTESIAN_POINT('Ctrl Pts',(126.217860418479,34.5366373940648,17.));
#57651=CARTESIAN_POINT('Ctrl Pts',(126.233603126139,34.4667993207977,17.));
#57652=CARTESIAN_POINT('Ctrl Pts',(126.243156003279,34.4244206812378,17.));
#57653=CARTESIAN_POINT('Ctrl Pts',(126.253459458477,34.3821983693281,17.));
#57654=CARTESIAN_POINT('Ctrl Pts',(126.264522704234,34.3401537713521,16.9999999999999));
#57655=CARTESIAN_POINT('Ctrl Pts',(126.269462731949,34.3213797620011,16.9999999999999));
#57656=CARTESIAN_POINT('Ctrl Pts',(126.27455474766,34.3026397937225,16.9999999999999));
#57657=CARTESIAN_POINT('Ctrl Pts',(126.279793700241,34.2839559596265,16.9999999999999));
#57658=CARTESIAN_POINT('Ctrl Pts',(126.311063324684,34.1724381578618,16.9999999999998));
#57659=CARTESIAN_POINT('Ctrl Pts',(126.347606076099,34.0627526620742,16.9999999999999));
#57660=CARTESIAN_POINT('Ctrl Pts',(126.389497418337,33.9552547881673,16.9999999999998));
#57661=CARTESIAN_POINT('Ctrl Pts',(126.402467602738,33.9219718429867,16.9999999999998));
#57662=CARTESIAN_POINT('Ctrl Pts',(126.415950855001,33.8888987507312,16.9999999999999));
#57663=CARTESIAN_POINT('Ctrl Pts',(126.429950338727,33.8560464984648,16.9999999999999));
#57664=CARTESIAN_POINT('Ctrl Pts',(126.475866889916,33.7482952304651,16.9999999999998));
#57665=CARTESIAN_POINT('Ctrl Pts',(126.527333732362,33.6429171859707,17.));
#57666=CARTESIAN_POINT('Ctrl Pts',(126.584005799438,33.5401814510135,17.));
#57667=CARTESIAN_POINT('Ctrl Pts',(126.641108069226,33.4366658399347,17.));
#57668=CARTESIAN_POINT('Ctrl Pts',(126.703495652404,33.3358321983157,16.9999999999999));
#57669=CARTESIAN_POINT('Ctrl Pts',(126.770851333061,33.2379941517966,16.9999999999999));
#57670=CARTESIAN_POINT('Ctrl Pts',(126.804494181508,33.1891259562828,16.9999999999999));
#57671=CARTESIAN_POINT('Ctrl Pts',(126.839376958759,33.1410057578031,16.9999999999999));
#57672=CARTESIAN_POINT('Ctrl Pts',(126.875462529273,33.0936769067577,17.));
#57673=CARTESIAN_POINT('Ctrl Pts',(126.886664671689,33.0789844819944,17.));
#57674=CARTESIAN_POINT('Ctrl Pts',(126.897982734747,33.0643683404368,17.));
#57675=CARTESIAN_POINT('Ctrl Pts',(126.909415630747,33.0498298403455,16.9999999999999));
#57676=CARTESIAN_POINT('Ctrl Pts',(126.919261036269,33.0373100527876,16.9999999999999));
#57677=CARTESIAN_POINT('Ctrl Pts',(126.929188667834,33.0248516240596,17.0000000000002));
#57678=CARTESIAN_POINT('Ctrl Pts',(126.939192716546,33.0124613276602,17.0000000000002));
#57679=CARTESIAN_POINT('Ctrl Pts',(127.011948576822,32.922351143313,17.));
#57680=CARTESIAN_POINT('Ctrl Pts',(127.088821101316,32.8357421178869,17.0000000000001));
#57681=CARTESIAN_POINT('Ctrl Pts',(127.169466870983,32.7528788149574,17.0000000000001));
#57682=CARTESIAN_POINT('Ctrl Pts',(127.249991207905,32.6701402838339,17.0000000000001));
#57683=CARTESIAN_POINT('Ctrl Pts',(127.334278242301,32.5911357022543,17.0000000000001));
#57684=CARTESIAN_POINT('Ctrl Pts',(127.422017428112,32.5161493067951,17.));
#57685=CARTESIAN_POINT('Ctrl Pts',(127.509023135241,32.4417897797291,16.9999999999999));
#57686=CARTESIAN_POINT('Ctrl Pts',(127.599424292657,32.3713811155938,17.0000000000001));
#57687=CARTESIAN_POINT('Ctrl Pts',(127.692937081477,32.3052474021187,17.0000000000001));
#57688=CARTESIAN_POINT('Ctrl Pts',(127.745229281574,32.2682655366242,17.0000000000001));
#57689=CARTESIAN_POINT('Ctrl Pts',(127.79849477284,32.2326213384267,17.));
#57690=CARTESIAN_POINT('Ctrl Pts',(127.852685200275,32.1983787022165,17.));
#57691=CARTESIAN_POINT('Ctrl Pts',(127.881422505441,32.1802197554612,17.0000000000001));
#57692=CARTESIAN_POINT('Ctrl Pts',(127.91041993099,32.1624550478516,16.9999999999999));
#57693=CARTESIAN_POINT('Ctrl Pts',(127.939670295583,32.1450947484183,16.9999999999999));
#57694=CARTESIAN_POINT('Ctrl Pts',(127.95623701152,32.1352622846765,16.9999999999999));
#57695=CARTESIAN_POINT('Ctrl Pts',(127.972886663471,32.1255586278457,17.));
#57696=CARTESIAN_POINT('Ctrl Pts',(127.98959836262,32.1159965954256,17.));
#57697=CARTESIAN_POINT('Ctrl Pts',(128.086647842483,32.060467216604,17.));
#57698=CARTESIAN_POINT('Ctrl Pts',(128.1859309852,32.0096238875741,17.));
#57699=CARTESIAN_POINT('Ctrl Pts',(128.287161065264,31.9637255550784,17.));
#57700=CARTESIAN_POINT('Ctrl Pts',(128.385832953704,31.9189871221864,16.9999999999999));
#57701=CARTESIAN_POINT('Ctrl Pts',(128.486355341507,31.8789467189593,17.));
#57702=CARTESIAN_POINT('Ctrl Pts',(128.588474407863,31.8438911608433,17.));
#57703=CARTESIAN_POINT('Ctrl Pts',(128.688986058153,31.8093873984823,17.));
#57704=CARTESIAN_POINT('Ctrl Pts',(128.791045115042,31.77971256302,17.));
#57705=CARTESIAN_POINT('Ctrl Pts',(128.894411452207,31.7551894334429,17.));
#57706=CARTESIAN_POINT('Ctrl Pts',(128.959370158269,31.7397783159591,16.9999999999999));
#57707=CARTESIAN_POINT('Ctrl Pts',(129.024845149963,31.7264027373315,17.));
#57708=CARTESIAN_POINT('Ctrl Pts',(129.090775656524,31.7151536247108,17.));
#57709=CARTESIAN_POINT('Ctrl Pts',(129.131408312752,31.7082208503425,17.));
#57710=CARTESIAN_POINT('Ctrl Pts',(129.172213968367,31.7020959537143,17.));
#57711=CARTESIAN_POINT('Ctrl Pts',(129.213170778782,31.6967753652515,17.));
#57712=CARTESIAN_POINT('Ctrl Pts',(132.567055762672,37.2043908438416,29.9966205380558));
#57713=CARTESIAN_POINT('Ctrl Pts',(133.295540430453,36.3561521436381,29.9308807084033));
#57714=CARTESIAN_POINT('Ctrl Pts',(133.83237619187,33.895265814678,29.7994477278945));
#57715=CARTESIAN_POINT('Ctrl Pts',(131.173364181338,31.1840944667917,29.6023215965296));
#57716=CARTESIAN_POINT('Ctrl Pts',(127.452981029627,31.9293652704744,29.4052421439611));
#57717=CARTESIAN_POINT('Ctrl Pts',(126.035010474348,35.4458461447659,29.2081626913928));
#57718=CARTESIAN_POINT('Ctrl Pts',(128.199728311344,38.5611777251301,29.0110832388244));
#57719=CARTESIAN_POINT('Ctrl Pts',(131.991478805662,38.4575237094584,28.814003786256));
#57720=CARTESIAN_POINT('Ctrl Pts',(133.983498870357,35.2298082435239,28.6169243336875));
#57721=CARTESIAN_POINT('Ctrl Pts',(132.375780304869,31.7942237028353,28.4198448811191));
#57722=CARTESIAN_POINT('Ctrl Pts',(128.621113708042,31.2557076608804,28.2227654285506));
#57723=CARTESIAN_POINT('Ctrl Pts',(126.112518820413,34.1007607740198,28.0256859759822));
#57724=CARTESIAN_POINT('Ctrl Pts',(127.116930471706,37.7584542688539,27.8286065234137));
#57725=CARTESIAN_POINT('Ctrl Pts',(130.726696014798,38.9233967594309,27.6315270708453));
#57726=CARTESIAN_POINT('Ctrl Pts',(133.679765016802,36.5428773444799,27.4344476182769));
#57727=CARTESIAN_POINT('Ctrl Pts',(133.307530816144,32.7680990489065,27.2373681657084));
#57728=CARTESIAN_POINT('Ctrl Pts',(129.946370574694,31.0102302563085,27.04028871314));
#57729=CARTESIAN_POINT('Ctrl Pts',(126.633673911154,32.8578074562423,26.8432092605715));
#57730=CARTESIAN_POINT('Ctrl Pts',(126.363034667212,36.6412261742564,26.646129808003));
#57731=CARTESIAN_POINT('Ctrl Pts',(129.379022266619,38.941513226243,26.4490503554346));
#57732=CARTESIAN_POINT('Ctrl Pts',(132.956170568106,37.6799618681735,26.2519709028662));
#57733=CARTESIAN_POINT('Ctrl Pts',(133.861907804393,33.9966017081917,26.0548914502976));
#57734=CARTESIAN_POINT('Ctrl Pts',(131.277743819111,31.2199853542158,25.8578119977293));
#57735=CARTESIAN_POINT('Ctrl Pts',(127.538917441336,31.8592655873322,25.6607325451609));
#57736=CARTESIAN_POINT('Ctrl Pts',(126.024104543952,35.3367422307258,25.4636530925924));
#57737=CARTESIAN_POINT('Ctrl Pts',(128.102200410904,38.5099140622057,25.2665736400239));
#57738=CARTESIAN_POINT('Ctrl Pts',(131.895286234357,38.5112718631302,25.0694941874556));
#57739=CARTESIAN_POINT('Ctrl Pts',(133.975653351649,35.3395886244166,24.8724147348871));
#57740=CARTESIAN_POINT('Ctrl Pts',(132.4633304881,31.8610283670508,24.6753352823186));
#57741=CARTESIAN_POINT('Ctrl Pts',(128.724962750633,31.2190715400751,24.4782558297502));
#57742=CARTESIAN_POINT('Ctrl Pts',(126.138811553627,33.9938370967647,24.2811763771818));
#57743=CARTESIAN_POINT('Ctrl Pts',(127.041911510654,37.6778447481953,24.0840969246132));
#57744=CARTESIAN_POINT('Ctrl Pts',(130.618155712909,38.9419568136729,23.8870174720449));
#57745=CARTESIAN_POINT('Ctrl Pts',(133.635789382529,36.6438295447349,23.6899380194764));
#57746=CARTESIAN_POINT('Ctrl Pts',(133.36785891173,32.8602181520236,23.492858566908));
#57747=CARTESIAN_POINT('Ctrl Pts',(130.056485791714,31.0102695126623,23.2957791143395));
#57748=CARTESIAN_POINT('Ctrl Pts',(126.694067995515,32.765731979379,23.0986996617711));
#57749=CARTESIAN_POINT('Ctrl Pts',(126.319131183993,36.54024178803,22.9016202092026));
#57750=CARTESIAN_POINT('Ctrl Pts',(129.270495572856,38.922876915867,22.7045407566343));
#57751=CARTESIAN_POINT('Ctrl Pts',(132.881093303896,37.7605146948486,22.5074613040658));
#57752=CARTESIAN_POINT('Ctrl Pts',(133.888125248107,34.103550301869,22.3103818514974));
#57753=CARTESIAN_POINT('Ctrl Pts',(131.381563981988,31.2566831592799,22.1133023989289));
#57754=CARTESIAN_POINT('Ctrl Pts',(127.626520859714,31.7925498013699,21.9162229463605));
#57755=CARTESIAN_POINT('Ctrl Pts',(126.016326388125,35.2269020942195,21.719143493792));
#57756=CARTESIAN_POINT('Ctrl Pts',(128.006069588758,38.4562091259181,21.5220640412236));
#57757=CARTESIAN_POINT('Ctrl Pts',(131.797673559676,38.5622338184465,21.3249845886551));
#57758=CARTESIAN_POINT('Ctrl Pts',(133.964768748078,35.4491645373762,21.1279051360867));
#57759=CARTESIAN_POINT('Ctrl Pts',(132.549010076058,31.930197458527,20.9308256835183));
#57760=CARTESIAN_POINT('Ctrl Pts',(128.829780213618,31.1853275840279,20.7337462309498));
#57761=CARTESIAN_POINT('Ctrl Pts',(126.168046195167,33.8876735824175,20.5366667783814));
#57762=CARTESIAN_POINT('Ctrl Pts',(126.9691447818,37.5951987763752,20.3395873258129));
#57763=CARTESIAN_POINT('Ctrl Pts',(130.509144924881,38.9575132726843,20.1425078732445));
#57764=CARTESIAN_POINT('Ctrl Pts',(133.589044636381,36.7435305517908,19.9454284206759));
#57765=CARTESIAN_POINT('Ctrl Pts',(133.425622140562,32.9539664760638,19.7483489681076));
#57766=CARTESIAN_POINT('Ctrl Pts',(130.166557985232,31.0133476248247,19.5512695155392));
#57767=CARTESIAN_POINT('Ctrl Pts',(126.756979795506,32.6753576816052,19.3541900629707));
#57768=CARTESIAN_POINT('Ctrl Pts',(126.278031123947,36.4380851034208,19.1571106104022));
#57769=CARTESIAN_POINT('Ctrl Pts',(129.162524208194,38.9012515335436,18.9600311578338));
#57770=CARTESIAN_POINT('Ctrl Pts',(132.803822361966,37.8389681260754,18.7629517052654));
#57771=CARTESIAN_POINT('Ctrl Pts',(133.911380442483,34.2111754685922,18.5658722526969));
#57772=CARTESIAN_POINT('Ctrl Pts',(131.484334235672,31.296244554003,18.3687928001285));
#57773=CARTESIAN_POINT('Ctrl Pts',(127.715927186878,31.7282504513906,18.1717133475601));
#57774=CARTESIAN_POINT('Ctrl Pts',(126.011591887548,35.1169436079755,17.9746338949916));
#57775=CARTESIAN_POINT('Ctrl Pts',(127.911437177851,38.3997593110105,17.7775544424232));
#57776=CARTESIAN_POINT('Ctrl Pts',(131.698733478907,38.6107159277045,17.5804749898547));
#57777=CARTESIAN_POINT('Ctrl Pts',(133.950778465968,35.5579159759099,17.3833955372863));
#57778=CARTESIAN_POINT('Ctrl Pts',(132.632927527639,32.0027018980742,17.1863160847178));
#57779=CARTESIAN_POINT('Ctrl Pts',(128.935134083485,31.1524060608917,16.9892366321493));
#57780=CARTESIAN_POINT('Ctrl Pts',(126.201082349571,33.7865904288514,16.792157179581));
#57781=CARTESIAN_POINT('Ctrl Pts',(126.667056495351,36.2605541243663,16.6607708778687));
#57782=CARTESIAN_POINT('Ctrl Pts',(127.37006770175,37.1289835220537,16.5950777270125));
#57783=CARTESIAN_POINT('Ctrl Pts',(132.745392601518,37.3575328598391,30.1323365495442));
#57784=CARTESIAN_POINT('Ctrl Pts',(133.524486085317,36.4503658688749,30.0665967198915));
#57785=CARTESIAN_POINT('Ctrl Pts',(134.098616553793,33.8185184353491,29.9351637393829));
#57786=CARTESIAN_POINT('Ctrl Pts',(131.254879379394,30.9189983438223,29.738037608018));
#57787=CARTESIAN_POINT('Ctrl Pts',(127.276036173865,31.7160441191073,29.5409581554496));
#57788=CARTESIAN_POINT('Ctrl Pts',(125.759557284609,35.4768196799831,29.3438787028811));
#57789=CARTESIAN_POINT('Ctrl Pts',(128.074661000111,38.8085775624481,29.1467992503127));
#57790=CARTESIAN_POINT('Ctrl Pts',(132.129829534149,38.6977225619917,28.9497197977443));
#57791=CARTESIAN_POINT('Ctrl Pts',(134.260237929328,35.2457733332921,28.7526403451758));
#57792=CARTESIAN_POINT('Ctrl Pts',(132.540828978734,31.5715140838237,28.5555608926074));
#57793=CARTESIAN_POINT('Ctrl Pts',(128.525320610746,30.9955866034469,28.3584814400389));
#57794=CARTESIAN_POINT('Ctrl Pts',(125.842450240398,34.038289407694,28.1614019874705));
#57795=CARTESIAN_POINT('Ctrl Pts',(126.916639728775,37.9500878210208,27.964322534902));
#57796=CARTESIAN_POINT('Ctrl Pts',(130.777180570673,39.1959604433965,27.7672430823336));
#57797=CARTESIAN_POINT('Ctrl Pts',(133.935403273804,36.6500631221882,27.5701636297652));
#57798=CARTESIAN_POINT('Ctrl Pts',(133.537309459333,32.6130458685179,27.3730841771967));
#57799=CARTESIAN_POINT('Ctrl Pts',(129.942644865919,30.7330555512775,27.1760047246283));
#57800=CARTESIAN_POINT('Ctrl Pts',(126.399810680779,32.7089864403492,26.9789252720598));
#57801=CARTESIAN_POINT('Ctrl Pts',(126.110369762197,36.7552443783039,26.7818458194914));
#57802=CARTESIAN_POINT('Ctrl Pts',(129.335882102866,39.2153354856822,26.5847663669229));
#57803=CARTESIAN_POINT('Ctrl Pts',(133.161539739229,37.86614244701,26.3876869143545));
#57804=CARTESIAN_POINT('Ctrl Pts',(134.130199767414,33.9268942705633,26.190607461786));
#57805=CARTESIAN_POINT('Ctrl Pts',(131.366510411901,30.9573826197811,25.9935280092176));
#57806=CARTESIAN_POINT('Ctrl Pts',(127.367942704426,31.6410745160834,25.7964485566492));
#57807=CARTESIAN_POINT('Ctrl Pts',(125.747893704466,35.360136169341,25.5993691040807));
#57808=CARTESIAN_POINT('Ctrl Pts',(127.970357704405,38.753752543465,25.4022896515123));
#57809=CARTESIAN_POINT('Ctrl Pts',(132.0269543347,38.7552046726578,25.2052101989438));
#57810=CARTESIAN_POINT('Ctrl Pts',(134.251847371815,35.3631803058548,25.0081307463754));
#57811=CARTESIAN_POINT('Ctrl Pts',(132.63446139171,31.6429597584955,24.8110512938069));
#57812=CARTESIAN_POINT('Ctrl Pts',(128.636384186906,30.956405321735,24.6139718412385));
#57813=CARTESIAN_POINT('Ctrl Pts',(125.870569565381,33.923937597838,24.41689238867));
#57814=CARTESIAN_POINT('Ctrl Pts',(126.836409098946,37.8638782478409,24.2198129361016));
#57815=CARTESIAN_POINT('Ctrl Pts',(130.661099827081,39.2158098897313,24.0227334835332));
#57816=CARTESIAN_POINT('Ctrl Pts',(133.888372592688,36.7580286084536,23.8256540309647));
#57817=CARTESIAN_POINT('Ctrl Pts',(133.601828629387,32.7115646104299,23.6285745783963));
#57818=CARTESIAN_POINT('Ctrl Pts',(130.060409936129,30.7330975348234,23.4314951258278));
#57819=CARTESIAN_POINT('Ctrl Pts',(126.464400423935,32.610514355466,23.2344156732594));
#57820=CARTESIAN_POINT('Ctrl Pts',(126.063416244566,36.647244470064,23.0373362206909));
#57821=CARTESIAN_POINT('Ctrl Pts',(129.219815912774,39.1954044855965,22.8402567681225));
#57822=CARTESIAN_POINT('Ctrl Pts',(133.081246755844,37.9522913875984,22.6431773155541));
#57823=CARTESIAN_POINT('Ctrl Pts',(134.158238572435,34.0412727278192,22.4460978629857));
#57824=CARTESIAN_POINT('Ctrl Pts',(131.477543102034,30.9966298710407,22.2490184104172));
#57825=CARTESIAN_POINT('Ctrl Pts',(127.461632050868,31.5697238941575,22.0519389578488));
#57826=CARTESIAN_POINT('Ctrl Pts',(125.739575189624,35.2426652898614,21.8548595052803));
#57827=CARTESIAN_POINT('Ctrl Pts',(127.867548543914,38.6963166525534,21.6577800527119));
#57828=CARTESIAN_POINT('Ctrl Pts',(131.922560375371,38.8097070239969,21.4607006001434));
#57829=CARTESIAN_POINT('Ctrl Pts',(134.2402066001,35.4803686058201,21.263621147575));
#57830=CARTESIAN_POINT('Ctrl Pts',(132.726093256627,31.7169341203904,21.0665416950066));
#57831=CARTESIAN_POINT('Ctrl Pts',(128.748483460936,30.9203171273822,20.8694622424381));
#57832=CARTESIAN_POINT('Ctrl Pts',(125.901835177042,33.8103987604358,20.6723827898697));
#57833=CARTESIAN_POINT('Ctrl Pts',(126.758587166934,37.7754907484812,20.4753033373012));
#57834=CARTESIAN_POINT('Ctrl Pts',(130.54451591204,39.2324470770089,20.2782238847328));
#57835=CARTESIAN_POINT('Ctrl Pts',(133.838380425747,36.8646559794346,20.0811444321643));
#57836=CARTESIAN_POINT('Ctrl Pts',(133.663604747919,32.8118257574478,19.8840649795959));
#57837=CARTESIAN_POINT('Ctrl Pts',(130.178128993934,30.7363894876046,19.6869855270274));
#57838=CARTESIAN_POINT('Ctrl Pts',(126.531682791835,32.5138616328864,19.489906074459));
#57839=CARTESIAN_POINT('Ctrl Pts',(126.019460907712,36.537990822286,19.2928266218906));
#57840=CARTESIAN_POINT('Ctrl Pts',(129.104343631249,39.1722767586888,19.0957471693221));
#57841=CARTESIAN_POINT('Ctrl Pts',(132.998607696976,38.0361950848947,18.8986677167537));
#57842=CARTESIAN_POINT('Ctrl Pts',(134.183109336644,34.1563747605664,18.7015882641852));
#57843=CARTESIAN_POINT('Ctrl Pts',(131.587452944362,31.0389396494094,18.5045088116168));
#57844=CARTESIAN_POINT('Ctrl Pts',(127.55724955661,31.5009575812933,18.3074293590484));
#57845=CARTESIAN_POINT('Ctrl Pts',(125.734511776882,35.1250678387278,18.1103499064799));
#57846=CARTESIAN_POINT('Ctrl Pts',(127.766341891317,38.6359451925881,17.9132704539115));
#57847=CARTESIAN_POINT('Ctrl Pts',(131.816746793257,38.8615572510151,17.716191001343));
#57848=CARTESIAN_POINT('Ctrl Pts',(134.225244394153,35.5966751540052,17.5191115487746));
#57849=CARTESIAN_POINT('Ctrl Pts',(132.815840567169,31.794475541502,17.3220320962061));
#57850=CARTESIAN_POINT('Ctrl Pts',(128.86115640676,30.8851085014681,17.1249526436377));
#57851=CARTESIAN_POINT('Ctrl Pts',(125.937166397815,33.7022932233556,16.9278731910693));
#57852=CARTESIAN_POINT('Ctrl Pts',(126.435512398289,36.3481265257936,16.796486889357));
#57853=CARTESIAN_POINT('Ctrl Pts',(127.187362744862,37.2768868893281,16.7307937385008));
#57854=CARTESIAN_POINT('Ctrl Pts',(132.923729440365,37.5106748758366,30.2680525610325));
#57855=CARTESIAN_POINT('Ctrl Pts',(133.753431740182,36.5445795941117,30.2023127313799));
#57856=CARTESIAN_POINT('Ctrl Pts',(134.364856915716,33.7417710560202,30.0708797508712));
#57857=CARTESIAN_POINT('Ctrl Pts',(131.336394577451,30.653902220853,29.8737536195064));
#57858=CARTESIAN_POINT('Ctrl Pts',(127.099091318103,31.5027229677401,29.676674166938));
#57859=CARTESIAN_POINT('Ctrl Pts',(125.484104094871,35.5077932152003,29.4795947143695));
#57860=CARTESIAN_POINT('Ctrl Pts',(127.949593688879,39.0559773997662,29.2825152618011));
#57861=CARTESIAN_POINT('Ctrl Pts',(132.268180262635,38.937921414525,29.0854358092327));
#57862=CARTESIAN_POINT('Ctrl Pts',(134.536976988299,35.2617384230603,28.8883563566642));
#57863=CARTESIAN_POINT('Ctrl Pts',(132.705877652598,31.3488044648121,28.6912769040958));
#57864=CARTESIAN_POINT('Ctrl Pts',(128.42952751345,30.7354655460134,28.4941974515273));
#57865=CARTESIAN_POINT('Ctrl Pts',(125.572381660382,33.9758180413684,28.2971179989589));
#57866=CARTESIAN_POINT('Ctrl Pts',(126.716348985843,38.1417213731875,28.1000385463904));
#57867=CARTESIAN_POINT('Ctrl Pts',(130.827665126547,39.4685241273619,27.902959093822));
#57868=CARTESIAN_POINT('Ctrl Pts',(134.191041530805,36.7572488998967,27.7058796412536));
#57869=CARTESIAN_POINT('Ctrl Pts',(133.767088102523,32.4579926881293,27.5088001886851));
#57870=CARTESIAN_POINT('Ctrl Pts',(129.938919157145,30.4558808462466,27.3117207361167));
#57871=CARTESIAN_POINT('Ctrl Pts',(126.165947450404,32.5601654244561,27.1146412835482));
#57872=CARTESIAN_POINT('Ctrl Pts',(125.857704857182,36.8692625823514,26.9175618309798));
#57873=CARTESIAN_POINT('Ctrl Pts',(129.292741939113,39.4891577451213,26.7204823784113));
#57874=CARTESIAN_POINT('Ctrl Pts',(133.366908910353,38.0523230258466,26.5234029258429));
#57875=CARTESIAN_POINT('Ctrl Pts',(134.398491730435,33.8571868329348,26.3263234732744));
#57876=CARTESIAN_POINT('Ctrl Pts',(131.455277004692,30.6947798853466,26.129244020706));
#57877=CARTESIAN_POINT('Ctrl Pts',(127.196967967518,31.4228834448347,25.9321645681376));
#57878=CARTESIAN_POINT('Ctrl Pts',(125.471682864979,35.3835301079562,25.7350851155691));
#57879=CARTESIAN_POINT('Ctrl Pts',(127.838514997906,38.9975910247243,25.5380056630007));
#57880=CARTESIAN_POINT('Ctrl Pts',(132.158622435042,38.9991374821854,25.3409262104322));
#57881=CARTESIAN_POINT('Ctrl Pts',(134.528041391981,35.3867719872929,25.1438467578638));
#57882=CARTESIAN_POINT('Ctrl Pts',(132.80559229532,31.42489114994,24.9467673052954));
#57883=CARTESIAN_POINT('Ctrl Pts',(128.547805623179,30.693739103395,24.7496878527269));
#57884=CARTESIAN_POINT('Ctrl Pts',(125.602327577135,33.8540380989111,24.5526084001585));
#57885=CARTESIAN_POINT('Ctrl Pts',(126.630906687238,38.0499117474868,24.35552894759));
#57886=CARTESIAN_POINT('Ctrl Pts',(130.704043941251,39.4896629657897,24.1584494950216));
#57887=CARTESIAN_POINT('Ctrl Pts',(134.140955802847,36.8722276721723,23.9613700424531));
#57888=CARTESIAN_POINT('Ctrl Pts',(133.835798347043,32.5629110688361,23.7642905898847));
#57889=CARTESIAN_POINT('Ctrl Pts',(130.064334080544,30.4559255569845,23.5672111373162));
#57890=CARTESIAN_POINT('Ctrl Pts',(126.234732852354,32.455296731553,23.3701316847478));
#57891=CARTESIAN_POINT('Ctrl Pts',(125.807701305139,36.7542471520982,23.1730522321794));
#57892=CARTESIAN_POINT('Ctrl Pts',(129.169136252694,39.467932055326,22.9759727796109));
#57893=CARTESIAN_POINT('Ctrl Pts',(133.281400207792,38.1440680803481,22.7788933270425));
#57894=CARTESIAN_POINT('Ctrl Pts',(134.428351896762,33.9789951537694,22.581813874474));
#57895=CARTESIAN_POINT('Ctrl Pts',(131.573522222081,30.7365765828016,22.3847344219056));
#57896=CARTESIAN_POINT('Ctrl Pts',(127.296743242023,31.3468979869451,22.1876549693372));
#57897=CARTESIAN_POINT('Ctrl Pts',(125.462823991122,35.2584284855033,21.9905755167687));
#57898=CARTESIAN_POINT('Ctrl Pts',(127.729027499068,38.9364241791886,21.7934960642003));
#57899=CARTESIAN_POINT('Ctrl Pts',(132.047447191065,39.0571802295473,21.5964166116318));
#57900=CARTESIAN_POINT('Ctrl Pts',(134.515644452122,35.5115726742641,21.3993371590634));
#57901=CARTESIAN_POINT('Ctrl Pts',(132.903176437197,31.5036707822537,21.202257706495));
#57902=CARTESIAN_POINT('Ctrl Pts',(128.667186708253,30.6553066707365,21.0051782539265));
#57903=CARTESIAN_POINT('Ctrl Pts',(125.635624158919,33.7331239384541,20.8080988013581));
#57904=CARTESIAN_POINT('Ctrl Pts',(126.548029552068,37.9557827205871,20.6110193487896));
#57905=CARTESIAN_POINT('Ctrl Pts',(130.579886899199,39.5073808813335,20.4139398962212));
#57906=CARTESIAN_POINT('Ctrl Pts',(134.087716215113,36.9857814070785,20.2168604436527));
#57907=CARTESIAN_POINT('Ctrl Pts',(133.901587355275,32.6696850388319,20.0197809910843));
#57908=CARTESIAN_POINT('Ctrl Pts',(130.189700002638,30.4594313503844,19.8227015385158));
#57909=CARTESIAN_POINT('Ctrl Pts',(126.306385788164,32.3523655841678,19.6256220859474));
#57910=CARTESIAN_POINT('Ctrl Pts',(125.760890691477,36.6378965411511,19.428542633379));
#57911=CARTESIAN_POINT('Ctrl Pts',(129.046163054305,39.443301983834,19.2314631808105));
#57912=CARTESIAN_POINT('Ctrl Pts',(133.193393031986,38.2334220437139,19.0343837282421));
#57913=CARTESIAN_POINT('Ctrl Pts',(134.454838230805,34.1015740525406,18.8373042756736));
#57914=CARTESIAN_POINT('Ctrl Pts',(131.690571653052,30.7816347448159,18.6402248231052));
#57915=CARTESIAN_POINT('Ctrl Pts',(127.398571926341,31.273664711196,18.4431453705367));
#57916=CARTESIAN_POINT('Ctrl Pts',(125.457431666217,35.1331920694799,18.2460659179683));
#57917=CARTESIAN_POINT('Ctrl Pts',(127.621246604782,38.8721310741658,18.0489864653999));
#57918=CARTESIAN_POINT('Ctrl Pts',(131.934760107606,39.1123985743256,17.8519070128314));
#57919=CARTESIAN_POINT('Ctrl Pts',(134.499710322339,35.6354343321004,17.654827560263));
#57920=CARTESIAN_POINT('Ctrl Pts',(132.998753606699,31.5862491849297,17.4577481076945));
#57921=CARTESIAN_POINT('Ctrl Pts',(128.787178730035,30.6178109420444,17.2606686551261));
#57922=CARTESIAN_POINT('Ctrl Pts',(125.673250446058,33.6179960178598,17.0635892025576));
#57923=CARTESIAN_POINT('Ctrl Pts',(126.203968301227,36.4356989272208,16.9322029008454));
#57924=CARTESIAN_POINT('Ctrl Pts',(127.004657787973,37.4247902566023,16.8665097499892));
#57925=CARTESIAN_POINT('Ctrl Pts',(133.102066279211,37.6638168918341,30.4037685725209));
#57926=CARTESIAN_POINT('Ctrl Pts',(133.982377395047,36.6387933193483,30.3380287428683));
#57927=CARTESIAN_POINT('Ctrl Pts',(134.631097277639,33.6650236766912,30.2065957623595));
#57928=CARTESIAN_POINT('Ctrl Pts',(131.417909775507,30.3888060978836,30.0094696309947));
#57929=CARTESIAN_POINT('Ctrl Pts',(126.922146462341,31.289401816373,29.8123901784262));
#57930=CARTESIAN_POINT('Ctrl Pts',(125.208650905131,35.5387667504174,29.6153107258578));
#57931=CARTESIAN_POINT('Ctrl Pts',(127.824526377647,39.3033772370842,29.4182312732893));
#57932=CARTESIAN_POINT('Ctrl Pts',(132.406530991122,39.1781202670583,29.221151820721));
#57933=CARTESIAN_POINT('Ctrl Pts',(134.813716047271,35.2777035128283,29.0240723681525));
#57934=CARTESIAN_POINT('Ctrl Pts',(132.870926326462,31.1260948458003,28.8269929155841));
#57935=CARTESIAN_POINT('Ctrl Pts',(128.333734416155,30.4753444885799,28.6299134630156));
#57936=CARTESIAN_POINT('Ctrl Pts',(125.302313080367,33.9133466750426,28.4328340104471));
#57937=CARTESIAN_POINT('Ctrl Pts',(126.516058242912,38.3333549253541,28.2357545578788));
#57938=CARTESIAN_POINT('Ctrl Pts',(130.87814968242,39.7410878113275,28.0386751053102));
#57939=CARTESIAN_POINT('Ctrl Pts',(134.446679787807,36.8644346776051,27.8415956527419));
#57940=CARTESIAN_POINT('Ctrl Pts',(133.996866745713,32.3029395077406,27.6445162001734));
#57941=CARTESIAN_POINT('Ctrl Pts',(129.935193448372,30.1787061412156,27.447436747605));
#57942=CARTESIAN_POINT('Ctrl Pts',(125.932084220027,32.4113444085631,27.2503572950365));
#57943=CARTESIAN_POINT('Ctrl Pts',(125.605039952166,36.9832807863989,27.0532778424681));
#57944=CARTESIAN_POINT('Ctrl Pts',(129.249601775359,39.7629800045605,26.8561983898996));
#57945=CARTESIAN_POINT('Ctrl Pts',(133.572278081476,38.2385036046833,26.6591189373312));
#57946=CARTESIAN_POINT('Ctrl Pts',(134.666783693457,33.7874793953062,26.4620394847627));
#57947=CARTESIAN_POINT('Ctrl Pts',(131.544043597482,30.4321771509119,26.2649600321943));
#57948=CARTESIAN_POINT('Ctrl Pts',(127.025993230609,31.204692373586,26.0678805796259));
#57949=CARTESIAN_POINT('Ctrl Pts',(125.195472025492,35.4069240465715,25.8708011270574));
#57950=CARTESIAN_POINT('Ctrl Pts',(127.706672291407,39.2414295059836,25.673721674489));
#57951=CARTESIAN_POINT('Ctrl Pts',(132.290290535385,39.2430702917129,25.4766422219205));
#57952=CARTESIAN_POINT('Ctrl Pts',(134.804235412148,35.410363668731,25.2795627693521));
#57953=CARTESIAN_POINT('Ctrl Pts',(132.976723198929,31.2068225413846,25.0824833167836));
#57954=CARTESIAN_POINT('Ctrl Pts',(128.459227059453,30.4310728850549,24.8854038642152));
#57955=CARTESIAN_POINT('Ctrl Pts',(125.334085588889,33.7841385999844,24.6883244116468));
#57956=CARTESIAN_POINT('Ctrl Pts',(126.425404275529,38.2359452471325,24.4912449590783));
#57957=CARTESIAN_POINT('Ctrl Pts',(130.746988055422,39.7635160418482,24.2941655065099));
#57958=CARTESIAN_POINT('Ctrl Pts',(134.393539013006,36.9864267358912,24.0970860539414));
#57959=CARTESIAN_POINT('Ctrl Pts',(134.0697680647,32.4142575272423,23.900006601373));
#57960=CARTESIAN_POINT('Ctrl Pts',(130.068258224959,30.1787535791456,23.7029271488045));
#57961=CARTESIAN_POINT('Ctrl Pts',(126.005065280775,32.3000791076401,23.5058476962361));
#57962=CARTESIAN_POINT('Ctrl Pts',(125.551986365712,36.8612498341322,23.3087682436676));
#57963=CARTESIAN_POINT('Ctrl Pts',(129.118456592612,39.7404596250554,23.1116887910992));
#57964=CARTESIAN_POINT('Ctrl Pts',(133.481553659739,38.3358447730979,22.9146093385308));
#57965=CARTESIAN_POINT('Ctrl Pts',(134.698465221089,33.9167175797195,22.7175298859623));
#57966=CARTESIAN_POINT('Ctrl Pts',(131.669501342127,30.4765232945625,22.5204504333939));
#57967=CARTESIAN_POINT('Ctrl Pts',(127.131854433178,31.1240720797326,22.3233709808255));
#57968=CARTESIAN_POINT('Ctrl Pts',(125.186072792621,35.2741916811453,22.126291528257));
#57969=CARTESIAN_POINT('Ctrl Pts',(127.590506454223,39.1765317058238,21.9292120756886));
#57970=CARTESIAN_POINT('Ctrl Pts',(132.17233400676,39.3046534350976,21.7321326231201));
#57971=CARTESIAN_POINT('Ctrl Pts',(134.791082304144,35.5427767427079,21.5350531705517));
#57972=CARTESIAN_POINT('Ctrl Pts',(133.080259617766,31.2904074441171,21.3379737179832));
#57973=CARTESIAN_POINT('Ctrl Pts',(128.585889955571,30.3902962140908,21.1408942654148));
#57974=CARTESIAN_POINT('Ctrl Pts',(125.369413140795,33.6558491164725,20.9438148128464));
#57975=CARTESIAN_POINT('Ctrl Pts',(126.337471937201,38.136074692693,20.7467353602779));
#57976=CARTESIAN_POINT('Ctrl Pts',(130.615257886358,39.7823146856582,20.5496559077095));
#57977=CARTESIAN_POINT('Ctrl Pts',(134.33705200448,37.1069068347224,20.352576455141));
#57978=CARTESIAN_POINT('Ctrl Pts',(134.139569962632,32.5275443202159,20.1554970025726));
#57979=CARTESIAN_POINT('Ctrl Pts',(130.201271011341,30.1824732131642,19.9584175500041));
#57980=CARTESIAN_POINT('Ctrl Pts',(126.081088784494,32.1908695354491,19.7613380974357));
#57981=CARTESIAN_POINT('Ctrl Pts',(125.502320475242,36.7378022600163,19.5642586448672));
#57982=CARTESIAN_POINT('Ctrl Pts',(128.987982477359,39.7143272089792,19.3671791922988));
#57983=CARTESIAN_POINT('Ctrl Pts',(133.388178366997,38.4306490025331,19.1700997397304));
#57984=CARTESIAN_POINT('Ctrl Pts',(134.726567124965,34.0467733445149,18.9730202871619));
#57985=CARTESIAN_POINT('Ctrl Pts',(131.793690361742,30.5243298402222,18.7759408345935));
#57986=CARTESIAN_POINT('Ctrl Pts',(127.239894296073,31.0463718410988,18.5788613820251));
#57987=CARTESIAN_POINT('Ctrl Pts',(125.180351555551,35.1413163002321,18.3817819294566));
#57988=CARTESIAN_POINT('Ctrl Pts',(127.476151318247,39.1083169557435,18.1847024768882));
#57989=CARTESIAN_POINT('Ctrl Pts',(132.052773421955,39.3632398976362,17.9876230243197));
#57990=CARTESIAN_POINT('Ctrl Pts',(134.774176250524,35.6741935101957,17.7905435717513));
#57991=CARTESIAN_POINT('Ctrl Pts',(133.181666646227,31.3780228283574,17.5934641191828));
#57992=CARTESIAN_POINT('Ctrl Pts',(128.713201053309,30.3505133826207,17.3963846666144));
#57993=CARTESIAN_POINT('Ctrl Pts',(125.409334494302,33.533698812364,17.199305214046));
#57994=CARTESIAN_POINT('Ctrl Pts',(125.972424204166,36.5232713286481,17.0679189123336));
#57995=CARTESIAN_POINT('Ctrl Pts',(126.821952831084,37.5726936238766,17.0022257614775));
#57996=CARTESIAN_POINT('Ctrl Pts',(132.573234427015,37.2065515280923,30.));
#57997=CARTESIAN_POINT('Ctrl Pts',(132.649853019674,37.1336332793624,29.9999999999999));
#57998=CARTESIAN_POINT('Ctrl Pts',(132.722534994398,37.0570775958444,29.9999999999998));
#57999=CARTESIAN_POINT('Ctrl Pts',(132.791284483358,36.977300375456,30.));
#58000=CARTESIAN_POINT('Ctrl Pts',(132.861752925125,36.895528474395,30.0000000000001));
#58001=CARTESIAN_POINT('Ctrl Pts',(132.928090170014,36.8103715162712,30.));
#58002=CARTESIAN_POINT('Ctrl Pts',(132.990274451397,36.722229072783,30.));
#58003=CARTESIAN_POINT('Ctrl Pts',(133.053778947546,36.6322153050177,30.0000000000001));
#58004=CARTESIAN_POINT('Ctrl Pts',(133.112952713737,36.5390874001683,30.0000000000001));
#58005=CARTESIAN_POINT('Ctrl Pts',(133.167739109377,36.4432284799637,30.0000000000002));
#58006=CARTESIAN_POINT('Ctrl Pts',(133.220861751636,36.3502806036549,30.0000000000002));
#58007=CARTESIAN_POINT('Ctrl Pts',(133.269859583631,36.2547642631004,29.9999999999999));
#58008=CARTESIAN_POINT('Ctrl Pts',(133.314646019766,36.1569996980181,30.));
#58009=CARTESIAN_POINT('Ctrl Pts',(133.321659778676,36.1416893239718,30.));
#58010=CARTESIAN_POINT('Ctrl Pts',(133.328570937711,36.1263220445087,30.));
#58011=CARTESIAN_POINT('Ctrl Pts',(133.335376683319,36.110904481846,30.));
#58012=CARTESIAN_POINT('Ctrl Pts',(133.381298957067,36.0068733331781,29.9999999999998));
#58013=CARTESIAN_POINT('Ctrl Pts',(133.422281347888,35.9008837141508,29.9999999999999));
#58014=CARTESIAN_POINT('Ctrl Pts',(133.458300951026,35.7933676203473,29.9999999999999));
#58015=CARTESIAN_POINT('Ctrl Pts',(133.494921707518,35.6840571241977,30.));
#58016=CARTESIAN_POINT('Ctrl Pts',(133.526413089524,35.5731680825438,29.9999999999999));
#58017=CARTESIAN_POINT('Ctrl Pts',(133.552712099049,35.4611166522047,30.));
#58018=CARTESIAN_POINT('Ctrl Pts',(133.579063193468,35.3488433052603,30.0000000000001));
#58019=CARTESIAN_POINT('Ctrl Pts',(133.600201707779,35.2354021361399,30.0000000000001));
#58020=CARTESIAN_POINT('Ctrl Pts',(133.616019384666,35.1211857228107,30.0000000000001));
#58021=CARTESIAN_POINT('Ctrl Pts',(133.629397241759,35.0245867806253,30.));
#58022=CARTESIAN_POINT('Ctrl Pts',(133.638968470452,34.9274325880293,30.));
#58023=CARTESIAN_POINT('Ctrl Pts',(133.644639510987,34.8299528255702,30.));
#58024=CARTESIAN_POINT('Ctrl Pts',(133.645720632867,34.8113693745521,30.));
#58025=CARTESIAN_POINT('Ctrl Pts',(133.646659929478,34.7927740807523,29.9999999999998));
#58026=CARTESIAN_POINT('Ctrl Pts',(133.647456638038,34.7741685247524,29.9999999999998));
#58027=CARTESIAN_POINT('Ctrl Pts',(133.648145835737,34.7580736727038,29.9999999999998));
#58028=CARTESIAN_POINT('Ctrl Pts',(133.648728075031,34.7419763134874,29.9999999999998));
#58029=CARTESIAN_POINT('Ctrl Pts',(133.649202920447,34.725885226351,29.9999999999998));
#58030=CARTESIAN_POINT('Ctrl Pts',(133.652701331799,34.6073345568996,29.9999999999999));
#58031=CARTESIAN_POINT('Ctrl Pts',(133.650379787513,34.4889991098537,30.));
#58032=CARTESIAN_POINT('Ctrl Pts',(133.642173285556,34.3713070999481,30.));
#58033=CARTESIAN_POINT('Ctrl Pts',(133.63399714229,34.2540504735288,29.9999999999999));
#58034=CARTESIAN_POINT('Ctrl Pts',(133.619979819363,34.1374316460575,30.0000000000001));
#58035=CARTESIAN_POINT('Ctrl Pts',(133.600008773635,34.0218568079166,29.9999999999999));
#58036=CARTESIAN_POINT('Ctrl Pts',(133.596501616631,34.0015604694782,29.9999999999998));
#58037=CARTESIAN_POINT('Ctrl Pts',(133.592810721572,33.9812963033916,29.9999999999998));
#58038=CARTESIAN_POINT('Ctrl Pts',(133.58893531302,33.9610664860445,29.9999999999998));
#58039=CARTESIAN_POINT('Ctrl Pts',(133.567331333046,33.848292680912,29.9999999999999));
#58040=CARTESIAN_POINT('Ctrl Pts',(133.539997632525,33.736586010492,29.9999999999997));
#58041=CARTESIAN_POINT('Ctrl Pts',(133.50723292845,33.6262060673214,29.9999999999999));
#58042=CARTESIAN_POINT('Ctrl Pts',(133.486427399802,33.556115000282,29.9999999999999));
#58043=CARTESIAN_POINT('Ctrl Pts',(133.463430868005,33.4865589247505,30.));
#58044=CARTESIAN_POINT('Ctrl Pts',(133.438309219098,33.4176060315415,29.9999999999998));
#58045=CARTESIAN_POINT('Ctrl Pts',(133.432143579052,33.4006828303125,29.9999999999997));
#58046=CARTESIAN_POINT('Ctrl Pts',(133.425849892516,33.3837959724792,29.9999999999997));
#58047=CARTESIAN_POINT('Ctrl Pts',(133.419429062893,33.36694648716,29.9999999999998));
#58048=CARTESIAN_POINT('Ctrl Pts',(133.413620392469,33.3517034246926,29.9999999999998));
#58049=CARTESIAN_POINT('Ctrl Pts',(133.407709371309,33.3364955207696,30.));
#58050=CARTESIAN_POINT('Ctrl Pts',(133.401699885338,33.3213308991472,29.9999999999999));
#58051=CARTESIAN_POINT('Ctrl Pts',(133.358585042201,33.2125328612307,29.9999999999998));
#58052=CARTESIAN_POINT('Ctrl Pts',(133.310362255848,33.1058466822621,29.9999999999999));
#58053=CARTESIAN_POINT('Ctrl Pts',(133.257394148206,33.0015290590835,29.9999999999999));
#58054=CARTESIAN_POINT('Ctrl Pts',(133.20269552755,32.8938032906528,29.9999999999999));
#58055=CARTESIAN_POINT('Ctrl Pts',(133.14293630787,32.7886026856914,30.0000000000001));
#58056=CARTESIAN_POINT('Ctrl Pts',(133.078459117678,32.6862135768433,30.));
#58057=CARTESIAN_POINT('Ctrl Pts',(133.013981927485,32.5838244679953,29.9999999999999));
#58058=CARTESIAN_POINT('Ctrl Pts',(132.944786300179,32.4842461433536,29.9999999999999));
#58059=CARTESIAN_POINT('Ctrl Pts',(132.871164169375,32.387779114913,29.9999999999999));
#58060=CARTESIAN_POINT('Ctrl Pts',(132.817180895344,32.3170448672846,29.9999999999998));
#58061=CARTESIAN_POINT('Ctrl Pts',(132.760816619589,32.2479836595213,29.9999999999998));
#58062=CARTESIAN_POINT('Ctrl Pts',(132.702171320135,32.1807222077868,30.));
#58063=CARTESIAN_POINT('Ctrl Pts',(132.682391185113,32.1580359804248,30.0000000000001));
#58064=CARTESIAN_POINT('Ctrl Pts',(132.662351459987,32.1355545656877,30.));
#58065=CARTESIAN_POINT('Ctrl Pts',(132.64205568799,32.1132830596148,29.9999999999999));
#58066=CARTESIAN_POINT('Ctrl Pts',(132.629127996341,32.099096894973,29.9999999999999));
#58067=CARTESIAN_POINT('Ctrl Pts',(132.616095952342,32.0849954975785,30.));
#58068=CARTESIAN_POINT('Ctrl Pts',(132.602971467161,32.0709916880355,30.));
#58069=CARTESIAN_POINT('Ctrl Pts',(132.51706134301,31.9793256912457,30.));
#58070=CARTESIAN_POINT('Ctrl Pts',(132.42708576349,31.8917189352439,30.0000000000001));
#58071=CARTESIAN_POINT('Ctrl Pts',(132.333380954484,31.8084868081493,30.));
#58072=CARTESIAN_POINT('Ctrl Pts',(132.249610606485,31.7340788420559,30.));
#58073=CARTESIAN_POINT('Ctrl Pts',(132.162858888468,31.6631669226728,30.));
#58074=CARTESIAN_POINT('Ctrl Pts',(132.073335746272,31.595994443417,29.9999999999999));
#58075=CARTESIAN_POINT('Ctrl Pts',(132.035647395435,31.5677154989709,29.9999999999998));
#58076=CARTESIAN_POINT('Ctrl Pts',(131.997467538981,31.5400995537595,30.0000000000001));
#58077=CARTESIAN_POINT('Ctrl Pts',(131.958810535468,31.5131659774618,30.));
#58078=CARTESIAN_POINT('Ctrl Pts',(131.941207933923,31.5009016794395,30.));
#58079=CARTESIAN_POINT('Ctrl Pts',(131.923504430989,31.4887775667498,29.9999999999999));
#58080=CARTESIAN_POINT('Ctrl Pts',(131.905707752497,31.4767998318809,29.9999999999999));
#58081=CARTESIAN_POINT('Ctrl Pts',(131.800671830913,31.4061072910769,30.));
#58082=CARTESIAN_POINT('Ctrl Pts',(131.692537776855,31.3406064541469,29.9999999999999));
#58083=CARTESIAN_POINT('Ctrl Pts',(131.581620848268,31.2806265875096,30.));
#58084=CARTESIAN_POINT('Ctrl Pts',(131.47135331977,31.2209978929718,30.));
#58085=CARTESIAN_POINT('Ctrl Pts',(131.35833483295,31.1668249847331,29.9999999999999));
#58086=CARTESIAN_POINT('Ctrl Pts',(131.242839295058,31.1184677488179,29.9999999999999));
#58087=CARTESIAN_POINT('Ctrl Pts',(131.228328688645,31.1123922516138,29.9999999999999));
#58088=CARTESIAN_POINT('Ctrl Pts',(131.213778942246,31.1064086096793,30.));
#58089=CARTESIAN_POINT('Ctrl Pts',(131.199190565814,31.1005175866223,30.));
#58090=CARTESIAN_POINT('Ctrl Pts',(131.153580206964,31.0820993838236,30.0000000000001));
#58091=CARTESIAN_POINT('Ctrl Pts',(131.107592287516,31.0645864316864,29.9999999999999));
#58092=CARTESIAN_POINT('Ctrl Pts',(131.061251469589,31.0479717576683,30.));
#58093=CARTESIAN_POINT('Ctrl Pts',(128.941097384543,31.0506385600526,29.9977746450279));
#58094=CARTESIAN_POINT('Ctrl Pts',(127.636979564161,31.4002985726558,29.9320814941718));
#58095=CARTESIAN_POINT('Ctrl Pts',(125.424202813788,33.4879278405674,29.8006951924595));
#58096=CARTESIAN_POINT('Ctrl Pts',(126.226059929022,38.0051538371624,29.603615739891));
#58097=CARTESIAN_POINT('Ctrl Pts',(130.44507746161,39.800374185406,29.4065362873226));
#58098=CARTESIAN_POINT('Ctrl Pts',(134.258668943317,37.2607564345166,29.2094568347541));
#58099=CARTESIAN_POINT('Ctrl Pts',(134.225375111656,32.6766551184777,29.0123773821857));
#58100=CARTESIAN_POINT('Ctrl Pts',(130.372971419078,30.1928228717204,28.8152979296172));
#58101=CARTESIAN_POINT('Ctrl Pts',(126.183887676755,32.0527554421128,28.6182184770488));
#58102=CARTESIAN_POINT('Ctrl Pts',(125.443145000095,36.5762024021472,28.4211390244803));
#58103=CARTESIAN_POINT('Ctrl Pts',(128.820393548648,39.6751961014325,28.2240595719119));
#58104=CARTESIAN_POINT('Ctrl Pts',(133.26357927699,38.5493816503394,28.0269801193435));
#58105=CARTESIAN_POINT('Ctrl Pts',(134.757576919438,34.216068226713,27.829900666775));
#58106=CARTESIAN_POINT('Ctrl Pts',(131.952271869581,30.5911819197693,27.6328212142066));
#58107=CARTESIAN_POINT('Ctrl Pts',(127.382756390785,30.9504203203026,27.4357417616381));
#58108=CARTESIAN_POINT('Ctrl Pts',(125.178370646884,34.9691560811274,27.2386623090697));
#58109=CARTESIAN_POINT('Ctrl Pts',(127.331161511516,39.015763607638,27.0415828565013));
#58110=CARTESIAN_POINT('Ctrl Pts',(131.895708724517,39.4334351099692,26.8445034039328));
#58111=CARTESIAN_POINT('Ctrl Pts',(134.747155692316,35.8447314423668,26.6474239513644));
#58112=CARTESIAN_POINT('Ctrl Pts',(133.308726840317,31.4926670259735,26.4503444987959));
#58113=CARTESIAN_POINT('Ctrl Pts',(128.88029144574,30.3100841245265,26.2532650462275));
#58114=CARTESIAN_POINT('Ctrl Pts',(125.463706238897,33.3656508795297,26.056185593659));
#58115=CARTESIAN_POINT('Ctrl Pts',(126.146446541373,37.8981345429696,25.8591061410906));
#58116=CARTESIAN_POINT('Ctrl Pts',(130.311538460064,39.8116527210156,25.6620266885222));
#58117=CARTESIAN_POINT('Ctrl Pts',(134.19510153501,37.3770109853911,25.4649472359537));
#58118=CARTESIAN_POINT('Ctrl Pts',(134.287665263084,32.7943289680552,25.2678677833853));
#58119=CARTESIAN_POINT('Ctrl Pts',(130.505582318982,30.2048519697683,25.0707883308168));
#58120=CARTESIAN_POINT('Ctrl Pts',(126.266618361204,31.9486200414821,24.8737088782484));
#58121=CARTESIAN_POINT('Ctrl Pts',(125.401410016033,36.4498373257519,24.6766294256799));
#58122=CARTESIAN_POINT('Ctrl Pts',(128.691822571263,39.6408759870467,24.4795499731115));
#58123=CARTESIAN_POINT('Ctrl Pts',(133.164399547228,38.6380810350471,24.2824705205431));
#58124=CARTESIAN_POINT('Ctrl Pts',(134.777394577013,34.3476510384955,24.0853910679746));
#58125=CARTESIAN_POINT('Ctrl Pts',(132.073187850764,30.6467310848586,23.8883116154062));
#58126=CARTESIAN_POINT('Ctrl Pts',(127.495497558176,30.8797420431519,23.6912321628377));
#58127=CARTESIAN_POINT('Ctrl Pts',(125.181058116145,34.8361182374327,23.4941527102693));
#58128=CARTESIAN_POINT('Ctrl Pts',(127.221365603193,38.9405899305759,23.2970732577009));
#58129=CARTESIAN_POINT('Ctrl Pts',(131.772649544859,39.4840575044465,23.0999938051324));
#58130=CARTESIAN_POINT('Ctrl Pts',(134.722038226556,35.9754040696121,22.902914352564));
#58131=CARTESIAN_POINT('Ctrl Pts',(133.404249182998,31.5853044627455,22.7058348999955));
#58132=CARTESIAN_POINT('Ctrl Pts',(129.010132590199,30.2809724918095,22.5087554474271));
#58133=CARTESIAN_POINT('Ctrl Pts',(125.510532297232,33.2410975416826,22.3116759948586));
#58134=CARTESIAN_POINT('Ctrl Pts',(126.067942062277,37.7906949827236,22.1145965422902));
#58135=CARTESIAN_POINT('Ctrl Pts',(130.17864581635,39.8184171450895,21.9175170897218));
#58136=CARTESIAN_POINT('Ctrl Pts',(134.127912197006,37.4918665706579,21.7204376371533));
#58137=CARTESIAN_POINT('Ctrl Pts',(134.346896412782,32.9134838391122,21.5233581845849));
#58138=CARTESIAN_POINT('Ctrl Pts',(130.63770837377,30.2206291063118,21.3262787320164));
#58139=CARTESIAN_POINT('Ctrl Pts',(126.352240593858,31.8467620723114,21.129199279448));
#58140=CARTESIAN_POINT('Ctrl Pts',(125.363153938779,36.3223905339553,20.9321198268796));
#58141=CARTESIAN_POINT('Ctrl Pts',(128.564259164265,39.6030105735538,20.7350403743111));
#58142=CARTESIAN_POINT('Ctrl Pts',(133.062804393718,38.7240149543763,20.5379609217427));
#58143=CARTESIAN_POINT('Ctrl Pts',(134.793576466494,34.4797281235888,20.3408814691742));
#58144=CARTESIAN_POINT('Ctrl Pts',(132.192523632706,30.7055968965927,20.1438020166058));
#58145=CARTESIAN_POINT('Ctrl Pts',(127.610146760738,30.8122010707778,19.9467225640373));
#58146=CARTESIAN_POINT('Ctrl Pts',(125.187415297971,34.7032055790439,19.7496431114689));
#58147=CARTESIAN_POINT('Ctrl Pts',(127.113686096751,38.8624148252036,19.5525636589004));
#58148=CARTESIAN_POINT('Ctrl Pts',(131.64824009618,39.531265336693,19.355484206332));
#58149=CARTESIAN_POINT('Ctrl Pts',(134.693324896921,36.1053330286121,19.1584047537636));
#58150=CARTESIAN_POINT('Ctrl Pts',(133.497178144898,31.680544119862,18.9613253011951));
#58151=CARTESIAN_POINT('Ctrl Pts',(129.140729119686,30.2554514731342,18.7642458486267));
#58152=CARTESIAN_POINT('Ctrl Pts',(125.560774363793,33.117890665288,18.5671663960582));
#58153=CARTESIAN_POINT('Ctrl Pts',(125.992438636684,37.6811157912653,18.3700869434898));
#58154=CARTESIAN_POINT('Ctrl Pts',(130.045603791983,39.8215414336961,18.1730074909214));
#58155=CARTESIAN_POINT('Ctrl Pts',(134.057606652229,37.6047633296345,17.9759280383529));
#58156=CARTESIAN_POINT('Ctrl Pts',(134.40276000298,33.0343540557215,17.7788485857845));
#58157=CARTESIAN_POINT('Ctrl Pts',(130.76946668054,30.2397849523119,17.581769133216));
#58158=CARTESIAN_POINT('Ctrl Pts',(126.440396857374,31.7478458997171,17.3846896806476));
#58159=CARTESIAN_POINT('Ctrl Pts',(125.328932767176,36.1928190026923,17.1876102280791));
#58160=CARTESIAN_POINT('Ctrl Pts',(128.436719226379,39.5639595163822,16.9905307755107));
#58161=CARTESIAN_POINT('Ctrl Pts',(132.961965747045,38.80210666434,16.793404651506));
#58162=CARTESIAN_POINT('Ctrl Pts',(134.185068670941,36.0149711949963,16.6619716783574));
#58163=CARTESIAN_POINT('Ctrl Pts',(134.075375956471,34.6682761845988,16.5962318560649));
#58164=CARTESIAN_POINT('Ctrl Pts',(129.001973237821,31.2776856407296,30.1334903360346));
#58165=CARTESIAN_POINT('Ctrl Pts',(127.772828586768,31.6072438504722,30.0677971851784));
#58166=CARTESIAN_POINT('Ctrl Pts',(125.68726341452,33.5748562148862,29.9364108834662));
#58167=CARTESIAN_POINT('Ctrl Pts',(126.443022111084,37.8323888431025,29.7393314308977));
#58168=CARTESIAN_POINT('Ctrl Pts',(130.419490150884,39.5244027501432,29.5422519783293));
#58169=CARTESIAN_POINT('Ctrl Pts',(134.013839908078,37.1307865251062,29.3451725257608));
#58170=CARTESIAN_POINT('Ctrl Pts',(133.982460124397,32.8102232106304,29.1480930731924));
#58171=CARTESIAN_POINT('Ctrl Pts',(130.351529453544,30.4691854052259,28.9510136206239));
#58172=CARTESIAN_POINT('Ctrl Pts',(126.403274323357,32.2221912567589,28.7539341680555));
#58173=CARTESIAN_POINT('Ctrl Pts',(125.705116622731,36.4855872079176,28.5568547154871));
#58174=CARTESIAN_POINT('Ctrl Pts',(128.888208613234,39.406421100065,28.3597752629186));
#58175=CARTESIAN_POINT('Ctrl Pts',(133.075957516191,38.3453292347345,28.1626958103502));
#58176=CARTESIAN_POINT('Ctrl Pts',(134.484065880482,34.2611361252281,27.9656163577817));
#58177=CARTESIAN_POINT('Ctrl Pts',(131.840036604358,30.8446429639338,27.7685369052133));
#58178=CARTESIAN_POINT('Ctrl Pts',(127.533220593652,31.1832289042281,27.5714574526448));
#58179=CARTESIAN_POINT('Ctrl Pts',(125.455564032542,34.9709292846803,27.3743780000764));
#58180=CARTESIAN_POINT('Ctrl Pts',(127.484591881671,38.7848990950663,27.177298547508));
#58181=CARTESIAN_POINT('Ctrl Pts',(131.786725250034,39.1785588434143,26.9802190949395));
#58182=CARTESIAN_POINT('Ctrl Pts',(134.474243765198,35.7961681971786,26.7831396423711));
#58183=CARTESIAN_POINT('Ctrl Pts',(133.118509565632,31.6943020813675,26.5860601898026));
#58184=CARTESIAN_POINT('Ctrl Pts',(128.944663006135,30.5797053593359,26.3889807372342));
#58185=CARTESIAN_POINT('Ctrl Pts',(125.724495804809,33.4596089034412,26.1919012846657));
#58186=CARTESIAN_POINT('Ctrl Pts',(126.367985662651,37.7315220418359,25.9948218320973));
#58187=CARTESIAN_POINT('Ctrl Pts',(130.293628248766,39.5350328876198,25.7977423795289));
#58188=CARTESIAN_POINT('Ctrl Pts',(133.953926962576,37.240357652143,25.6006629269604));
#58189=CARTESIAN_POINT('Ctrl Pts',(134.041169241965,32.9211320415018,25.403583474392));
#58190=CARTESIAN_POINT('Ctrl Pts',(130.47651661018,30.4805229556309,25.2065040218235));
#58191=CARTESIAN_POINT('Ctrl Pts',(126.481248856545,32.1240425552611,25.0094245692551));
#58192=CARTESIAN_POINT('Ctrl Pts',(125.665780964847,36.3664868050984,24.8123451166866));
#58193=CARTESIAN_POINT('Ctrl Pts',(128.767029125719,39.3740740342083,24.6152656641182));
#58194=CARTESIAN_POINT('Ctrl Pts',(132.982479586188,38.428929330187,24.4181862115498));
#58195=CARTESIAN_POINT('Ctrl Pts',(134.502744229496,34.3851542980842,24.2211067589813));
#58196=CARTESIAN_POINT('Ctrl Pts',(131.95400117809,30.8969986315528,24.0240273064129));
#58197=CARTESIAN_POINT('Ctrl Pts',(127.639480320101,31.1166138906552,23.8269478538444));
#58198=CARTESIAN_POINT('Ctrl Pts',(125.45809700036,34.8455397290669,23.629868401276));
#58199=CARTESIAN_POINT('Ctrl Pts',(127.38110809262,38.7140471201781,23.4327889487075));
#58200=CARTESIAN_POINT('Ctrl Pts',(131.670740689378,39.2262709783325,23.2357094961391));
#58201=CARTESIAN_POINT('Ctrl Pts',(134.450570291679,35.9193285116128,23.0386300435706));
#58202=CARTESIAN_POINT('Ctrl Pts',(133.208540370156,31.7816138319748,22.8415505910022));
#58203=CARTESIAN_POINT('Ctrl Pts',(129.067039639369,30.5522673417899,22.6444711384338));
#58204=CARTESIAN_POINT('Ctrl Pts',(125.768629853308,33.3422160831047,22.4473916858653));
#58205=CARTESIAN_POINT('Ctrl Pts',(126.293994372097,37.6302591354298,22.2503122332969));
#58206=CARTESIAN_POINT('Ctrl Pts',(130.168375545651,39.54140842788,22.0532327807285));
#58207=CARTESIAN_POINT('Ctrl Pts',(133.890600310547,37.3486102394997,21.85615332816));
#58208=CARTESIAN_POINT('Ctrl Pts',(134.096995218492,33.0334367505684,21.6590738755916));
#58209=CARTESIAN_POINT('Ctrl Pts',(130.601046795236,30.4953930714198,21.4619944230231));
#58210=CARTESIAN_POINT('Ctrl Pts',(126.561948704086,32.028040356674,21.2649149704547));
#58211=CARTESIAN_POINT('Ctrl Pts',(125.629724212925,36.2463668742282,21.0678355178862));
#58212=CARTESIAN_POINT('Ctrl Pts',(128.646799283805,39.3383854869563,20.8707560653178));
#58213=CARTESIAN_POINT('Ctrl Pts',(132.886725094102,38.5099229456693,20.6736766127494));
#58214=CARTESIAN_POINT('Ctrl Pts',(134.51799582915,34.5096383286925,20.4765971601809));
#58215=CARTESIAN_POINT('Ctrl Pts',(132.066476397554,30.9524802732359,20.2795177076125));
#58216=CARTESIAN_POINT('Ctrl Pts',(127.747538389606,31.0529558195643,20.082438255044));
#58217=CARTESIAN_POINT('Ctrl Pts',(125.464088710552,34.7202681619105,19.8853588024756));
#58218=CARTESIAN_POINT('Ctrl Pts',(127.279619034421,38.6403662677949,19.6882793499071));
#58219=CARTESIAN_POINT('Ctrl Pts',(131.553483486084,39.2707648527254,19.4911998973387));
#58220=CARTESIAN_POINT('Ctrl Pts',(134.423507678942,36.0417879109675,19.2941204447703));
#58221=CARTESIAN_POINT('Ctrl Pts',(133.296126886236,31.8713782024045,19.0970409922018));
#58222=CARTESIAN_POINT('Ctrl Pts',(129.190128230872,30.5282135154378,18.8999615396334));
#58223=CARTESIAN_POINT('Ctrl Pts',(125.815983525196,33.2260923167344,18.7028820870649));
#58224=CARTESIAN_POINT('Ctrl Pts',(126.222831605778,37.5269796042843,18.5058026344965));
#58225=CARTESIAN_POINT('Ctrl Pts',(130.04298204971,39.5443531024862,18.3087231819281));
#58226=CARTESIAN_POINT('Ctrl Pts',(133.824336601125,37.4550166126422,18.1116437293596));
#58227=CARTESIAN_POINT('Ctrl Pts',(134.149647235057,33.1473581907137,17.9145642767912));
#58228=CARTESIAN_POINT('Ctrl Pts',(130.725230373951,30.5134476561202,17.7174848242227));
#58229=CARTESIAN_POINT('Ctrl Pts',(126.645036902149,31.9348108320508,17.5204053716543));
#58230=CARTESIAN_POINT('Ctrl Pts',(125.597470401674,36.1242443542447,17.3233259190859));
#58231=CARTESIAN_POINT('Ctrl Pts',(128.526591561774,39.3015794581679,17.1262464665174));
#58232=CARTESIAN_POINT('Ctrl Pts',(132.791683617603,38.5835251970098,16.9291203425127));
#58233=CARTESIAN_POINT('Ctrl Pts',(133.944470883522,35.9566209400755,16.7976873693641));
#58234=CARTESIAN_POINT('Ctrl Pts',(133.841084355752,34.6873468432416,16.7319475470716));
#58235=CARTESIAN_POINT('Ctrl Pts',(129.062849091099,31.5047327214066,30.2692060270413));
#58236=CARTESIAN_POINT('Ctrl Pts',(127.908677609375,31.8141891282886,30.2035128761852));
#58237=CARTESIAN_POINT('Ctrl Pts',(125.950324015252,33.661784589205,30.072126574473));
#58238=CARTESIAN_POINT('Ctrl Pts',(126.659984293147,37.6596238490425,29.8750471219045));
#58239=CARTESIAN_POINT('Ctrl Pts',(130.393902840157,39.2484313148805,29.6779676693361));
#58240=CARTESIAN_POINT('Ctrl Pts',(133.76901087284,37.0008166156958,29.4808882167676));
#58241=CARTESIAN_POINT('Ctrl Pts',(133.739545137138,32.9437913027832,29.2838087641992));
#58242=CARTESIAN_POINT('Ctrl Pts',(130.330087488009,30.7455479387316,29.0867293116307));
#58243=CARTESIAN_POINT('Ctrl Pts',(126.622660969959,32.3916270714049,28.8896498590623));
#58244=CARTESIAN_POINT('Ctrl Pts',(125.967088245366,36.3949720136881,28.6925704064939));
#58245=CARTESIAN_POINT('Ctrl Pts',(128.956023677822,39.1376460986974,28.4954909539254));
#58246=CARTESIAN_POINT('Ctrl Pts',(132.888335755391,38.1412768191297,28.298411501357));
#58247=CARTESIAN_POINT('Ctrl Pts',(134.210554841525,34.3062040237431,28.1013320487885));
#58248=CARTESIAN_POINT('Ctrl Pts',(131.727801339134,31.0981040080983,27.9042525962201));
#58249=CARTESIAN_POINT('Ctrl Pts',(127.683684796518,31.4160374881537,27.7071731436516));
#58250=CARTESIAN_POINT('Ctrl Pts',(125.732757418202,34.972702488233,27.5100936910832));
#58251=CARTESIAN_POINT('Ctrl Pts',(127.638022251826,38.5540345824945,27.3130142385148));
#58252=CARTESIAN_POINT('Ctrl Pts',(131.67774177555,38.9236825768594,27.1159347859463));
#58253=CARTESIAN_POINT('Ctrl Pts',(134.201331838081,35.7476049519903,26.9188553333779));
#58254=CARTESIAN_POINT('Ctrl Pts',(132.928292290948,31.8959371367615,26.7217758808094));
#58255=CARTESIAN_POINT('Ctrl Pts',(129.00903456653,30.8493265941452,26.524696428241));
#58256=CARTESIAN_POINT('Ctrl Pts',(125.985285370721,33.5535669273527,26.3276169756725));
#58257=CARTESIAN_POINT('Ctrl Pts',(126.589524783929,37.5649095407024,26.1305375231041));
#58258=CARTESIAN_POINT('Ctrl Pts',(130.27571803747,39.2584130542239,25.9334580705357));
#58259=CARTESIAN_POINT('Ctrl Pts',(133.712752390142,37.103704318895,25.7363786179672));
#58260=CARTESIAN_POINT('Ctrl Pts',(133.794673220847,33.0479351149484,25.5392991653988));
#58261=CARTESIAN_POINT('Ctrl Pts',(130.447450901378,30.7561939414936,25.3422197128302));
#58262=CARTESIAN_POINT('Ctrl Pts',(126.695879351888,32.2994650690403,25.1451402602619));
#58263=CARTESIAN_POINT('Ctrl Pts',(125.930151913661,36.2831362844449,24.9480608076934));
#58264=CARTESIAN_POINT('Ctrl Pts',(128.842235680176,39.1072720813698,24.750981355125));
#58265=CARTESIAN_POINT('Ctrl Pts',(132.800559625146,38.2197776253269,24.5539019025566));
#58266=CARTESIAN_POINT('Ctrl Pts',(134.228093881978,34.4226575576729,24.3568224499881));
#58267=CARTESIAN_POINT('Ctrl Pts',(131.834814505417,31.1472661782472,24.1597429974197));
#58268=CARTESIAN_POINT('Ctrl Pts',(127.783463082027,31.3534857381584,23.9626635448512));
#58269=CARTESIAN_POINT('Ctrl Pts',(125.735135884574,34.8549612207012,23.7655840922828));
#58270=CARTESIAN_POINT('Ctrl Pts',(127.540850582046,38.4875043097803,23.5685046397144));
#58271=CARTESIAN_POINT('Ctrl Pts',(131.568831833898,38.9684844522186,23.3714251871459));
#58272=CARTESIAN_POINT('Ctrl Pts',(134.179102356802,35.8632529536134,23.1743457345775));
#58273=CARTESIAN_POINT('Ctrl Pts',(133.012831557314,31.977923201204,22.977266282009));
#58274=CARTESIAN_POINT('Ctrl Pts',(129.123946688539,30.8235621917705,22.7801868294405));
#58275=CARTESIAN_POINT('Ctrl Pts',(126.026727409382,33.4433346245269,22.5831073768721));
#58276=CARTESIAN_POINT('Ctrl Pts',(126.520046681916,37.4698232881361,22.3860279243037));
#58277=CARTESIAN_POINT('Ctrl Pts',(130.158105274952,39.2643997106705,22.1889484717353));
#58278=CARTESIAN_POINT('Ctrl Pts',(133.653288424089,37.2053539083415,21.9918690191668));
#58279=CARTESIAN_POINT('Ctrl Pts',(133.847094024202,33.1533896620248,21.7947895665984));
#58280=CARTESIAN_POINT('Ctrl Pts',(130.564385216702,30.7701570365278,21.5977101140299));
#58281=CARTESIAN_POINT('Ctrl Pts',(126.771656814313,32.2093186410366,21.4006306614615));
#58282=CARTESIAN_POINT('Ctrl Pts',(125.896294487071,36.1703432145012,21.203551208893));
#58283=CARTESIAN_POINT('Ctrl Pts',(128.729339403346,39.0737604003589,21.0064717563246));
#58284=CARTESIAN_POINT('Ctrl Pts',(132.710645794485,38.2958309369622,20.8093923037562));
#58285=CARTESIAN_POINT('Ctrl Pts',(134.242415191807,34.5395485337962,20.6123128511877));
#58286=CARTESIAN_POINT('Ctrl Pts',(131.940429162402,31.1993636498791,20.4152333986193));
#58287=CARTESIAN_POINT('Ctrl Pts',(127.884930018473,31.2937105683511,20.2181539460508));
#58288=CARTESIAN_POINT('Ctrl Pts',(125.740762123133,34.7373307447771,20.0210744934824));
#58289=CARTESIAN_POINT('Ctrl Pts',(127.44555197209,38.4183177103862,19.8239950409139));
#58290=CARTESIAN_POINT('Ctrl Pts',(131.458726875989,39.0102643687579,19.6269155883455));
#58291=CARTESIAN_POINT('Ctrl Pts',(134.153690460965,35.978242793323,19.429836135777));
#58292=CARTESIAN_POINT('Ctrl Pts',(133.095075627576,32.0622122849472,19.2327566832086));
#58293=CARTESIAN_POINT('Ctrl Pts',(129.239527342058,30.8009755577414,19.0356772306402));
#58294=CARTESIAN_POINT('Ctrl Pts',(126.071192686599,33.3342939681808,18.8385977780717));
#58295=CARTESIAN_POINT('Ctrl Pts',(126.453224574871,37.3728434173031,18.6415183255033));
#58296=CARTESIAN_POINT('Ctrl Pts',(130.040360307437,39.2671647712763,18.4444388729348));
#58297=CARTESIAN_POINT('Ctrl Pts',(133.591066550021,37.3052698956499,18.2473594203664));
#58298=CARTESIAN_POINT('Ctrl Pts',(133.896534467132,33.260362325706,18.050279967798));
#58299=CARTESIAN_POINT('Ctrl Pts',(130.680994067359,30.7871103599285,17.8532005152295));
#58300=CARTESIAN_POINT('Ctrl Pts',(126.849676946924,32.1217757643844,17.6561210626611));
#58301=CARTESIAN_POINT('Ctrl Pts',(125.866008036171,36.055669705797,17.4590416100926));
#58302=CARTESIAN_POINT('Ctrl Pts',(128.61646389717,39.0391993999536,17.2619621575242));
#58303=CARTESIAN_POINT('Ctrl Pts',(132.621401488161,38.3649437296796,17.0648360335194));
#58304=CARTESIAN_POINT('Ctrl Pts',(133.703873096103,35.8982706851548,16.9334030603708));
#58305=CARTESIAN_POINT('Ctrl Pts',(133.606792755035,34.7064175018843,16.8676632380784));
#58306=CARTESIAN_POINT('Ctrl Pts',(129.123724944377,31.7317798020836,30.4049217180481));
#58307=CARTESIAN_POINT('Ctrl Pts',(128.044526631981,32.021134406105,30.3392285671919));
#58308=CARTESIAN_POINT('Ctrl Pts',(126.213384615984,33.7487129635239,30.2078422654796));
#58309=CARTESIAN_POINT('Ctrl Pts',(126.876946475209,37.4868588549827,30.0107628129112));
#58310=CARTESIAN_POINT('Ctrl Pts',(130.368315529432,38.9724598796177,29.8136833603428));
#58311=CARTESIAN_POINT('Ctrl Pts',(133.524181837602,36.8708467062855,29.6166039077743));
#58312=CARTESIAN_POINT('Ctrl Pts',(133.496630149878,33.077359394936,29.4195244552059));
#58313=CARTESIAN_POINT('Ctrl Pts',(130.308645522475,31.0219104722371,29.2224450026374));
#58314=CARTESIAN_POINT('Ctrl Pts',(126.842047616561,32.5610628860511,29.025365550069));
#58315=CARTESIAN_POINT('Ctrl Pts',(126.229059868002,36.3043568194586,28.8282860975006));
#58316=CARTESIAN_POINT('Ctrl Pts',(129.023838742409,38.8688710973299,28.6312066449321));
#58317=CARTESIAN_POINT('Ctrl Pts',(132.70071399459,37.9372244035248,28.4341271923637));
#58318=CARTESIAN_POINT('Ctrl Pts',(133.937043802569,34.3512719222581,28.2370477397952));
#58319=CARTESIAN_POINT('Ctrl Pts',(131.615566073911,31.351565052263,28.0399682872268));
#58320=CARTESIAN_POINT('Ctrl Pts',(127.834148999385,31.6488460720792,27.8428888346583));
#58321=CARTESIAN_POINT('Ctrl Pts',(126.009950803862,34.9744756917859,27.6458093820899));
#58322=CARTESIAN_POINT('Ctrl Pts',(127.791452621982,38.3231700699227,27.4487299295215));
#58323=CARTESIAN_POINT('Ctrl Pts',(131.568758301068,38.6688063103047,27.251650476953));
#58324=CARTESIAN_POINT('Ctrl Pts',(133.928419910963,35.6990417068019,27.0545710243846));
#58325=CARTESIAN_POINT('Ctrl Pts',(132.738075016263,32.0975721921556,26.8574915718161));
#58326=CARTESIAN_POINT('Ctrl Pts',(129.073406126925,31.1189478289545,26.6604121192477));
#58327=CARTESIAN_POINT('Ctrl Pts',(126.246074936632,33.6475249512642,26.4633326666792));
#58328=CARTESIAN_POINT('Ctrl Pts',(126.811063905207,37.3982970395687,26.2662532141108));
#58329=CARTESIAN_POINT('Ctrl Pts',(130.257807826173,38.9817932208281,26.0691737615424));
#58330=CARTESIAN_POINT('Ctrl Pts',(133.471577817707,36.9670509856468,25.8720943089739));
#58331=CARTESIAN_POINT('Ctrl Pts',(133.54817719973,33.174738188395,25.6750148564055));
#58332=CARTESIAN_POINT('Ctrl Pts',(130.418385192576,31.0318649273562,25.477935403837));
#58333=CARTESIAN_POINT('Ctrl Pts',(126.910509847231,32.4748875828193,25.2808559512686));
#58334=CARTESIAN_POINT('Ctrl Pts',(126.194522862476,36.1997857637913,25.0837764987001));
#58335=CARTESIAN_POINT('Ctrl Pts',(128.917442234633,38.8404701285314,24.8866970461317));
#58336=CARTESIAN_POINT('Ctrl Pts',(132.618639664104,38.0106259204668,24.6896175935632));
#58337=CARTESIAN_POINT('Ctrl Pts',(133.953443534461,34.4601608172618,24.4925381409948));
#58338=CARTESIAN_POINT('Ctrl Pts',(131.715627832744,31.3975337249415,24.2954586884264));
#58339=CARTESIAN_POINT('Ctrl Pts',(127.927445843952,31.5903575856617,24.0983792358579));
#58340=CARTESIAN_POINT('Ctrl Pts',(126.012174768787,34.8643827123355,23.9012997832895));
#58341=CARTESIAN_POINT('Ctrl Pts',(127.700593071473,38.2609614993825,23.704220330721));
#58342=CARTESIAN_POINT('Ctrl Pts',(131.466922978418,38.7106979261046,23.5071408781526));
#58343=CARTESIAN_POINT('Ctrl Pts',(133.907634421926,35.8071773956141,23.3100614255842));
#58344=CARTESIAN_POINT('Ctrl Pts',(132.817122744472,32.1742325704332,23.1129819730157));
#58345=CARTESIAN_POINT('Ctrl Pts',(129.180853737708,31.0948570417509,22.9159025204473));
#58346=CARTESIAN_POINT('Ctrl Pts',(126.284824965458,33.5444531659491,22.7188230678788));
#58347=CARTESIAN_POINT('Ctrl Pts',(126.746098991737,37.3093874408423,22.5217436153104));
#58348=CARTESIAN_POINT('Ctrl Pts',(130.147835004252,38.987390993461,22.324664162742));
#58349=CARTESIAN_POINT('Ctrl Pts',(133.415976537629,37.0620975771833,22.1275847101735));
#58350=CARTESIAN_POINT('Ctrl Pts',(133.59719282991,33.273342573481,21.9305052576051));
#58351=CARTESIAN_POINT('Ctrl Pts',(130.527723638169,31.0449210016357,21.7334258050366));
#58352=CARTESIAN_POINT('Ctrl Pts',(126.981364924541,32.3905969253993,21.5363463524682));
#58353=CARTESIAN_POINT('Ctrl Pts',(126.162864761217,36.0943195547742,21.3392668998997));
#58354=CARTESIAN_POINT('Ctrl Pts',(128.811879522886,38.8091353137614,21.1421874473313));
#58355=CARTESIAN_POINT('Ctrl Pts',(132.534566494868,38.0817389282551,20.9451079947628));
#58356=CARTESIAN_POINT('Ctrl Pts',(133.966834554464,34.5694587389,20.7480285421944));
#58357=CARTESIAN_POINT('Ctrl Pts',(131.81438192725,31.4462470265224,20.550949089626));
#58358=CARTESIAN_POINT('Ctrl Pts',(128.022321647341,31.5344653171377,20.3538696370575));
#58359=CARTESIAN_POINT('Ctrl Pts',(126.017435535714,34.7543933276437,20.1567901844891));
#58360=CARTESIAN_POINT('Ctrl Pts',(127.61148490976,38.1962691529774,19.9597107319206));
#58361=CARTESIAN_POINT('Ctrl Pts',(131.363970265893,38.7497638847903,19.7626312793522));
#58362=CARTESIAN_POINT('Ctrl Pts',(133.883873242987,35.9146976756785,19.5655518267837));
#58363=CARTESIAN_POINT('Ctrl Pts',(132.894024368916,32.2530463674897,19.3684723742153));
#58364=CARTESIAN_POINT('Ctrl Pts',(129.288926453244,31.073737600045,19.1713929216469));
#58365=CARTESIAN_POINT('Ctrl Pts',(126.326401848002,33.4424956196272,18.9743134690784));
#58366=CARTESIAN_POINT('Ctrl Pts',(126.683617543965,37.218707230322,18.77723401651));
#58367=CARTESIAN_POINT('Ctrl Pts',(130.037738565164,38.9899764400662,18.5801545639415));
#58368=CARTESIAN_POINT('Ctrl Pts',(133.357796498917,37.1555231786576,18.3830751113731));
#58369=CARTESIAN_POINT('Ctrl Pts',(133.643421699208,33.3733664606983,18.1859956588046));
#58370=CARTESIAN_POINT('Ctrl Pts',(130.636757760769,31.0607730637369,17.9889162062362));
#58371=CARTESIAN_POINT('Ctrl Pts',(127.054316991698,32.3087406967181,17.7918367536678));
#58372=CARTESIAN_POINT('Ctrl Pts',(126.134545670668,35.9870950573493,17.5947573010993));
#58373=CARTESIAN_POINT('Ctrl Pts',(128.706336232565,38.7768193417394,17.3976778485309));
#58374=CARTESIAN_POINT('Ctrl Pts',(132.451119358719,38.1463622623494,17.2005517245261));
#58375=CARTESIAN_POINT('Ctrl Pts',(133.463275308683,35.839920430234,17.0691187513775));
#58376=CARTESIAN_POINT('Ctrl Pts',(133.372501154318,34.7254881605269,17.0033789290851));
#58377=CARTESIAN_POINT('',(127.424194198253,37.2080440111198,30.0017033528262));
#58378=CARTESIAN_POINT('Ctrl Pts',(127.426413840714,37.2061412790735,30.0017033528262));
#58379=CARTESIAN_POINT('Ctrl Pts',(127.438461580037,37.220195635187,30.0011355685508));
#58380=CARTESIAN_POINT('Ctrl Pts',(127.450624448196,37.234151300005,30.0005677842754));
#58381=CARTESIAN_POINT('Ctrl Pts',(127.462900812983,37.2480064007332,30.));
#58382=CARTESIAN_POINT('Ctrl Pts',(128.942095577027,31.0543614925016,30.));
#58383=CARTESIAN_POINT('Ctrl Pts',(128.825609397642,31.0963697647221,30.));
#58384=CARTESIAN_POINT('Ctrl Pts',(128.7115241043,31.1439906471432,30.0000000000001));
#58385=CARTESIAN_POINT('Ctrl Pts',(128.600069328297,31.1968590882299,30.0000000000001));
#58386=CARTESIAN_POINT('Ctrl Pts',(128.486962920038,31.2505109791227,30.0000000000001));
#58387=CARTESIAN_POINT('Ctrl Pts',(128.376564964256,31.309567722175,30.0000000000001));
#58388=CARTESIAN_POINT('Ctrl Pts',(128.269143169485,31.3736951260073,30.0000000000001));
#58389=CARTESIAN_POINT('Ctrl Pts',(128.161272060922,31.4380907559205,30.0000000000001));
#58390=CARTESIAN_POINT('Ctrl Pts',(128.056401487506,31.5076002570416,30.));
#58391=CARTESIAN_POINT('Ctrl Pts',(127.954839131891,31.581922498923,30.));
#58392=CARTESIAN_POINT('Ctrl Pts',(127.858557800154,31.6523801442061,30.));
#58393=CARTESIAN_POINT('Ctrl Pts',(127.765249473048,31.7271638358833,30.));
#58394=CARTESIAN_POINT('Ctrl Pts',(127.675213472941,31.8060391429531,30.));
#58395=CARTESIAN_POINT('Ctrl Pts',(127.65810181963,31.8210296679401,30.));
#58396=CARTESIAN_POINT('Ctrl Pts',(127.641108479803,31.8361680316025,30.0000000000001));
#58397=CARTESIAN_POINT('Ctrl Pts',(127.624235676082,31.8514526866952,30.));
#58398=CARTESIAN_POINT('Ctrl Pts',(127.613109396249,31.8615317080905,29.9999999999999));
#58399=CARTESIAN_POINT('Ctrl Pts',(127.602036828276,31.8716732131105,30.));
#58400=CARTESIAN_POINT('Ctrl Pts',(127.591025310482,31.8818703533532,30.));
#58401=CARTESIAN_POINT('Ctrl Pts',(127.50054824138,31.9656560202932,30.));
#58402=CARTESIAN_POINT('Ctrl Pts',(127.414059076834,32.0533125866699,30.));
#58403=CARTESIAN_POINT('Ctrl Pts',(127.331814436228,32.1445238770439,30.0000000000001));
#58404=CARTESIAN_POINT('Ctrl Pts',(127.250266160805,32.2349628816326,30.0000000000002));
#58405=CARTESIAN_POINT('Ctrl Pts',(127.172890401673,32.3288974156517,29.9999999999999));
#58406=CARTESIAN_POINT('Ctrl Pts',(127.099979115674,32.4260477080103,30.));
#58407=CARTESIAN_POINT('Ctrl Pts',(127.027478544049,32.5226507459768,30.0000000000001));
#58408=CARTESIAN_POINT('Ctrl Pts',(126.959391861292,32.6224340934605,29.9999999999998));
#58409=CARTESIAN_POINT('Ctrl Pts',(126.896054072652,32.7251403611992,29.9999999999999));
#58410=CARTESIAN_POINT('Ctrl Pts',(126.84349765552,32.8103639467586,29.9999999999999));
#58411=CARTESIAN_POINT('Ctrl Pts',(126.794211742569,32.8976005531388,30.0000000000002));
#58412=CARTESIAN_POINT('Ctrl Pts',(126.748416226718,32.9867074968054,30.));
#58413=CARTESIAN_POINT('Ctrl Pts',(126.738576987573,33.0058522648458,29.9999999999999));
#58414=CARTESIAN_POINT('Ctrl Pts',(126.728898970669,33.0250833755648,29.9999999999999));
#58415=CARTESIAN_POINT('Ctrl Pts',(126.719384526347,33.0443994188612,30.));
#58416=CARTESIAN_POINT('Ctrl Pts',(126.712239720925,33.0589046664819,30.0000000000001));
#58417=CARTESIAN_POINT('Ctrl Pts',(126.705188026154,33.0734561576526,30.0000000000002));
#58418=CARTESIAN_POINT('Ctrl Pts',(126.69823518144,33.0880428789924,30.0000000000002));
#58419=CARTESIAN_POINT('Ctrl Pts',(126.647578219101,33.1943186587582,29.9999999999999));
#58420=CARTESIAN_POINT('Ctrl Pts',(126.602089235897,33.3026149502714,30.0000000000002));
#58421=CARTESIAN_POINT('Ctrl Pts',(126.562038428248,33.4126741616684,30.0000000000001));
#58422=CARTESIAN_POINT('Ctrl Pts',(126.522813048182,33.5204651064788,30.));
#58423=CARTESIAN_POINT('Ctrl Pts',(126.488803776214,33.6299476902416,30.0000000000001));
#58424=CARTESIAN_POINT('Ctrl Pts',(126.460313221096,33.7408906127765,30.0000000000002));
#58425=CARTESIAN_POINT('Ctrl Pts',(126.452962461272,33.7695146523725,30.0000000000002));
#58426=CARTESIAN_POINT('Ctrl Pts',(126.445979335698,33.798235932397,30.0000000000002));
#58427=CARTESIAN_POINT('Ctrl Pts',(126.43936961117,33.8270505216889,30.0000000000001));
#58428=CARTESIAN_POINT('Ctrl Pts',(126.412872443509,33.942562900497,30.));
#58429=CARTESIAN_POINT('Ctrl Pts',(126.392372079654,34.0595756139416,30.0000000000003));
#58430=CARTESIAN_POINT('Ctrl Pts',(126.377782167101,34.1776518198943,30.0000000000002));
#58431=CARTESIAN_POINT('Ctrl Pts',(126.369641800959,34.243531827449,30.0000000000002));
#58432=CARTESIAN_POINT('Ctrl Pts',(126.363342301581,34.3097427527037,30.0000000000003));
#58433=CARTESIAN_POINT('Ctrl Pts',(126.358875354926,34.3762065420342,30.0000000000001));
#58434=CARTESIAN_POINT('Ctrl Pts',(126.357511103473,34.3965052668978,30.0000000000001));
#58435=CARTESIAN_POINT('Ctrl Pts',(126.356317816527,34.4168275625855,30.));
#58436=CARTESIAN_POINT('Ctrl Pts',(126.355295341418,34.4371711620536,29.9999999999999));
#58437=CARTESIAN_POINT('Ctrl Pts',(126.354567496136,34.4516526812134,29.9999999999999));
#58438=CARTESIAN_POINT('Ctrl Pts',(126.353926326219,34.4661433569147,30.));
#58439=CARTESIAN_POINT('Ctrl Pts',(126.3533719768,34.4806329555477,30.));
#58440=CARTESIAN_POINT('Ctrl Pts',(126.348947719107,34.5962743110845,30.0000000000001));
#58441=CARTESIAN_POINT('Ctrl Pts',(126.350040381804,34.7120147207867,29.9999999999999));
#58442=CARTESIAN_POINT('Ctrl Pts',(126.356503489409,34.8274542927884,30.));
#58443=CARTESIAN_POINT('Ctrl Pts',(126.363113345688,34.9455149884253,30.0000000000001));
#58444=CARTESIAN_POINT('Ctrl Pts',(126.375340459208,35.0632620236151,30.0000000000001));
#58445=CARTESIAN_POINT('Ctrl Pts',(126.393082807289,35.1802576232764,30.0000000000001));
#58446=CARTESIAN_POINT('Ctrl Pts',(126.41082515537,35.2972532229377,30.0000000000001));
#58447=CARTESIAN_POINT('Ctrl Pts',(126.43408309937,35.4134983511588,30.0000000000001));
#58448=CARTESIAN_POINT('Ctrl Pts',(126.462804371977,35.5285305607672,30.0000000000002));
#58449=CARTESIAN_POINT('Ctrl Pts',(126.481403668795,35.6030230193498,30.0000000000002));
#58450=CARTESIAN_POINT('Ctrl Pts',(126.502295055159,35.6770062918083,30.0000000000003));
#58451=CARTESIAN_POINT('Ctrl Pts',(126.525474399776,35.7503463986096,30.0000000000001));
#58452=CARTESIAN_POINT('Ctrl Pts',(126.532574556592,35.7728114970735,30.));
#58453=CARTESIAN_POINT('Ctrl Pts',(126.539889441554,35.7952161935211,30.0000000000002));
#58454=CARTESIAN_POINT('Ctrl Pts',(126.547419073731,35.8175564842859,30.0000000000002));
#58455=CARTESIAN_POINT('Ctrl Pts',(126.553170507578,35.8346208908098,30.0000000000002));
#58456=CARTESIAN_POINT('Ctrl Pts',(126.559047009417,35.8516468460435,30.));
#58457=CARTESIAN_POINT('Ctrl Pts',(126.56504410264,35.8686204532914,30.));
#58458=CARTESIAN_POINT('Ctrl Pts',(126.60289081843,35.9757382294415,29.9999999999999));
#58459=CARTESIAN_POINT('Ctrl Pts',(126.645579997457,36.0809032528098,29.9999999999999));
#58460=CARTESIAN_POINT('Ctrl Pts',(126.693045639272,36.1837053875735,29.9999999999999));
#58461=CARTESIAN_POINT('Ctrl Pts',(126.733092203321,36.2704391199489,30.));
#58462=CARTESIAN_POINT('Ctrl Pts',(126.776539630878,36.3554907358829,30.0000000000001));
#58463=CARTESIAN_POINT('Ctrl Pts',(126.823370488022,36.4385941868589,30.));
#58464=CARTESIAN_POINT('Ctrl Pts',(126.844837183414,36.4766877981435,29.9999999999999));
#58465=CARTESIAN_POINT('Ctrl Pts',(126.867015069518,36.5143717765041,30.0000000000001));
#58466=CARTESIAN_POINT('Ctrl Pts',(126.889903763462,36.5516189055333,30.));
#58467=CARTESIAN_POINT('Ctrl Pts',(126.903889590876,36.574378260852,30.));
#58468=CARTESIAN_POINT('Ctrl Pts',(126.918143120974,36.5969778174688,30.));
#58469=CARTESIAN_POINT('Ctrl Pts',(126.932649224775,36.6193883664837,30.));
#58470=CARTESIAN_POINT('Ctrl Pts',(126.991211921456,36.7098621561641,30.0000000000001));
#58471=CARTESIAN_POINT('Ctrl Pts',(127.053930557615,36.7973297766238,30.0000000000001));
#58472=CARTESIAN_POINT('Ctrl Pts',(127.120768818292,36.8814100270898,30.0000000000001));
#58473=CARTESIAN_POINT('Ctrl Pts',(127.187607078969,36.9654902775559,30.0000000000001));
#58474=CARTESIAN_POINT('Ctrl Pts',(127.258565249867,37.0461838130672,30.));
#58475=CARTESIAN_POINT('Ctrl Pts',(127.333638243439,37.1230673427468,30.0000000000001));
#58476=CARTESIAN_POINT('Ctrl Pts',(127.362444717677,37.1525685430013,30.0000000000001));
#58477=CARTESIAN_POINT('Ctrl Pts',(127.391857367042,37.1815082646089,30.));
#58478=CARTESIAN_POINT('Ctrl Pts',(127.421855523101,37.2098778099405,30.));
#58479=CARTESIAN_POINT('Origin',(-10.,35.,17.));
#58480=CARTESIAN_POINT('Ctrl Pts',(-6.62123117139838,34.7273715616997,17.));
#58481=CARTESIAN_POINT('Ctrl Pts',(-6.60195934569834,34.8321949891012,17.));
#58482=CARTESIAN_POINT('Ctrl Pts',(-6.58807244351625,34.9377386945817,17.));
#58483=CARTESIAN_POINT('Ctrl Pts',(-6.5793423594526,35.0436676563277,17.));
#58484=CARTESIAN_POINT('Ctrl Pts',(-6.57037143927326,35.1525188716857,17.));
#58485=CARTESIAN_POINT('Ctrl Pts',(-6.5668456742337,35.261777509942,17.));
#58486=CARTESIAN_POINT('Ctrl Pts',(-6.56856898097211,35.3711000441821,17.));
#58487=CARTESIAN_POINT('Ctrl Pts',(-6.56942692580178,35.4255260502596,17.));
#58488=CARTESIAN_POINT('Ctrl Pts',(-6.57158666510304,35.4799681405241,17.));
#58489=CARTESIAN_POINT('Ctrl Pts',(-6.57502867344059,35.5343849332849,17.));
#58490=CARTESIAN_POINT('Ctrl Pts',(-6.57632046539286,35.5548076539941,17.));
#58491=CARTESIAN_POINT('Ctrl Pts',(-6.57779235581878,35.5752179805597,17.));
#58492=CARTESIAN_POINT('Ctrl Pts',(-6.57944266526219,35.5956107924917,17.));
#58493=CARTESIAN_POINT('Ctrl Pts',(-6.58842152809188,35.7065622639138,17.));
#58494=CARTESIAN_POINT('Ctrl Pts',(-6.60267946638345,35.8170216916155,17.));
#58495=CARTESIAN_POINT('Ctrl Pts',(-6.62200532182683,35.9266343683881,17.));
#58496=CARTESIAN_POINT('Ctrl Pts',(-6.641707143771,36.038379457599,17.));
#58497=CARTESIAN_POINT('Ctrl Pts',(-6.66667597712323,36.1492453277495,17.));
#58498=CARTESIAN_POINT('Ctrl Pts',(-6.69674117187053,36.2588637823476,17.));
#58499=CARTESIAN_POINT('Ctrl Pts',(-6.70213341047965,36.2785240196461,17.));
#58500=CARTESIAN_POINT('Ctrl Pts',(-6.70768971886736,36.2981441321776,17.));
#58501=CARTESIAN_POINT('Ctrl Pts',(-6.71340928846767,36.3177219893546,17.));
#58502=CARTESIAN_POINT('Ctrl Pts',(-6.72069554508889,36.3426625533225,17.));
#58503=CARTESIAN_POINT('Ctrl Pts',(-6.72824855494793,36.367539909623,17.));
#58504=CARTESIAN_POINT('Ctrl Pts',(-6.73605660535735,36.392318482591,17.));
#58505=CARTESIAN_POINT('Ctrl Pts',(-6.77081652375714,36.5026278593585,17.));
#58506=CARTESIAN_POINT('Ctrl Pts',(-6.81065343512221,36.6110784621336,17.));
#58507=CARTESIAN_POINT('Ctrl Pts',(-6.85534048320785,36.7172979594713,17.));
#58508=CARTESIAN_POINT('Ctrl Pts',(-6.90044237101414,36.8245035158237,17.));
#58509=CARTESIAN_POINT('Ctrl Pts',(-6.95048498501844,36.9294372298153,17.));
#58510=CARTESIAN_POINT('Ctrl Pts',(-7.0052885201046,37.0317182304336,17.));
#58511=CARTESIAN_POINT('Ctrl Pts',(-7.05981854622386,37.1334887754623,17.));
#58512=CARTESIAN_POINT('Ctrl Pts',(-7.11906233324677,37.2326339054117,17.));
#58513=CARTESIAN_POINT('Ctrl Pts',(-7.18289248555842,37.328767082928,17.));
#58514=CARTESIAN_POINT('Ctrl Pts',(-7.22018203267521,37.3849280432681,17.));
#58515=CARTESIAN_POINT('Ctrl Pts',(-7.25903777040094,37.4400607782531,17.));
#58516=CARTESIAN_POINT('Ctrl Pts',(-7.29944172118395,37.4940845629917,17.));
#58517=CARTESIAN_POINT('Ctrl Pts',(-7.3210590200253,37.522988872511,17.));
#58518=CARTESIAN_POINT('Ctrl Pts',(-7.34311959600719,37.5515756830289,17.));
#58519=CARTESIAN_POINT('Ctrl Pts',(-7.36562131389244,37.5798321948882,17.));
#58520=CARTESIAN_POINT('Ctrl Pts',(-7.37556893692007,37.5923239134976,17.));
#58521=CARTESIAN_POINT('Ctrl Pts',(-7.38560197216116,37.6047499703436,17.));
#58522=CARTESIAN_POINT('Ctrl Pts',(-7.39571231655314,37.6170998830206,17.));
#58523=CARTESIAN_POINT('Ctrl Pts',(-7.47117575693862,37.7092794233932,17.));
#58524=CARTESIAN_POINT('Ctrl Pts',(-7.55105630936717,37.7973622554539,17.));
#58525=CARTESIAN_POINT('Ctrl Pts',(-7.63516399751822,37.8809609308377,17.));
#58526=CARTESIAN_POINT('Ctrl Pts',(-7.65864155501132,37.904296404096,17.));
#58527=CARTESIAN_POINT('Ctrl Pts',(-7.68244878202814,37.9272824054679,17.));
#58528=CARTESIAN_POINT('Ctrl Pts',(-7.70658223699224,37.9499102825999,17.));
#58529=CARTESIAN_POINT('Ctrl Pts',(-7.78963819592032,38.0277847533917,17.));
#58530=CARTESIAN_POINT('Ctrl Pts',(-7.87655463462689,38.1014199334542,17.));
#58531=CARTESIAN_POINT('Ctrl Pts',(-7.96691983219225,38.1708050440767,17.));
#58532=CARTESIAN_POINT('Ctrl Pts',(-8.05961255392386,38.2419772976049,17.));
#58533=CARTESIAN_POINT('Ctrl Pts',(-8.15593450042321,38.3086781586375,17.));
#58534=CARTESIAN_POINT('Ctrl Pts',(-8.25548340140922,38.3708605803994,17.));
#58535=CARTESIAN_POINT('Ctrl Pts',(-8.31141688788464,38.4057989836583,17.));
#58536=CARTESIAN_POINT('Ctrl Pts',(-8.3683698237762,38.4393102584732,17.));
#58537=CARTESIAN_POINT('Ctrl Pts',(-8.4262754553306,38.4713805519023,17.));
#58538=CARTESIAN_POINT('Ctrl Pts',(-8.44233384032758,38.4802742830477,17.));
#58539=CARTESIAN_POINT('Ctrl Pts',(-8.45846551033602,38.4890571689273,17.));
#58540=CARTESIAN_POINT('Ctrl Pts',(-8.47466907811928,38.4977288564759,17.));
#58541=CARTESIAN_POINT('Ctrl Pts',(-8.48766521757792,38.504684019822,17.));
#58542=CARTESIAN_POINT('Ctrl Pts',(-8.50070673982194,38.5115671407453,17.));
#58543=CARTESIAN_POINT('Ctrl Pts',(-8.51378382562772,38.5183734543627,17.));
#58544=CARTESIAN_POINT('Ctrl Pts',(-8.61982299463778,38.5735643318048,17.));
#58545=CARTESIAN_POINT('Ctrl Pts',(-8.7283547505616,38.6237926959064,17.));
#58546=CARTESIAN_POINT('Ctrl Pts',(-8.83892423282891,38.6690579537086,17.));
#58547=CARTESIAN_POINT('Ctrl Pts',(-8.9513815803523,38.7150960713069,17.));
#58548=CARTESIAN_POINT('Ctrl Pts',(-9.06594749383451,38.7560005407811,17.));
#58549=CARTESIAN_POINT('Ctrl Pts',(-9.18218323047418,38.7917330299808,17.));
#58550=CARTESIAN_POINT('Ctrl Pts',(-9.29985553091803,38.827907138962,17.));
#58551=CARTESIAN_POINT('Ctrl Pts',(-9.41923996013768,38.8587810364494,17.));
#58552=CARTESIAN_POINT('Ctrl Pts',(-9.53991077851995,38.8842706896853,17.));
#58553=CARTESIAN_POINT('Ctrl Pts',(-9.61457604005369,38.900042453321,17.));
#58554=CARTESIAN_POINT('Ctrl Pts',(-9.68973433655139,38.9137519461733,17.));
#58555=CARTESIAN_POINT('Ctrl Pts',(-9.7652883226987,38.9253699046292,17.));
#58556=CARTESIAN_POINT('Ctrl Pts',(-9.80157135144814,38.9309491565279,17.));
#58557=CARTESIAN_POINT('Ctrl Pts',(-9.83794566222605,38.936045954135,17.));
#58558=CARTESIAN_POINT('Ctrl Pts',(-9.87440059370104,38.9406564316365,17.));
#58559=CARTESIAN_POINT('Ctrl Pts',(-9.89072243089403,38.9427206643786,17.));
#58560=CARTESIAN_POINT('Ctrl Pts',(-9.90706094261734,38.9446874628517,17.));
#58561=CARTESIAN_POINT('Ctrl Pts',(-9.92341361539116,38.9465562749007,17.));
#58562=CARTESIAN_POINT('Ctrl Pts',(-10.049134669734,38.9609238969046,17.));
#58563=CARTESIAN_POINT('Ctrl Pts',(-10.1751588854043,38.9694430949161,17.));
#58564=CARTESIAN_POINT('Ctrl Pts',(-10.3010213929365,38.9720792792337,17.));
#58565=CARTESIAN_POINT('Ctrl Pts',(-10.4271447298256,38.9747209266099,17.));
#58566=CARTESIAN_POINT('Ctrl Pts',(-10.5531065751926,38.9714554663851,17.));
#58567=CARTESIAN_POINT('Ctrl Pts',(-10.6784618767559,38.9622008961875,17.));
#58568=CARTESIAN_POINT('Ctrl Pts',(-10.8015648493969,38.9531126080367,17.));
#58569=CARTESIAN_POINT('Ctrl Pts',(-10.9240837583291,38.938248640579,17.));
#58570=CARTESIAN_POINT('Ctrl Pts',(-11.0456058184429,38.9174827178352,17.));
#58571=CARTESIAN_POINT('Ctrl Pts',(-11.1383506190094,38.9016343084053,17.));
#58572=CARTESIAN_POINT('Ctrl Pts',(-11.2305150666145,38.8823472846425,17.));
#58573=CARTESIAN_POINT('Ctrl Pts',(-11.3219144398766,38.8595450271519,17.));
#58574=CARTESIAN_POINT('Ctrl Pts',(-11.3696279828065,38.8476414828184,17.));
#58575=CARTESIAN_POINT('Ctrl Pts',(-11.4171329813549,38.8347796560283,17.));
#58576=CARTESIAN_POINT('Ctrl Pts',(-11.464413394279,38.8209773893083,17.));
#58577=CARTESIAN_POINT('Ctrl Pts',(-13.1750507821943,37.570267988068,17.));
#58578=CARTESIAN_POINT('Ctrl Pts',(-13.2457830638452,37.4660682901415,17.));
#58579=CARTESIAN_POINT('Ctrl Pts',(-13.3111684943071,37.3585303558788,17.));
#58580=CARTESIAN_POINT('Ctrl Pts',(-13.3712015697569,37.2480942554894,17.));
#58581=CARTESIAN_POINT('Ctrl Pts',(-13.4312346452066,37.1376581551,17.));
#58582=CARTESIAN_POINT('Ctrl Pts',(-13.4859153844916,37.0243229867705,17.));
#58583=CARTESIAN_POINT('Ctrl Pts',(-13.5351882493577,36.908514120475,17.));
#58584=CARTESIAN_POINT('Ctrl Pts',(-13.5568750177871,36.8575424533667,17.));
#58585=CARTESIAN_POINT('Ctrl Pts',(-13.5775135207773,36.8060914717338,17.));
#58586=CARTESIAN_POINT('Ctrl Pts',(-13.5970959340666,36.7541972265355,17.));
#58587=CARTESIAN_POINT('Ctrl Pts',(-13.6073225862103,36.727096154463,17.));
#58588=CARTESIAN_POINT('Ctrl Pts',(-13.6172624893017,36.6998701487207,17.));
#58589=CARTESIAN_POINT('Ctrl Pts',(-13.6269052970792,36.6725509192079,17.));
#58590=CARTESIAN_POINT('Ctrl Pts',(-13.6685921142032,36.5544471727738,17.));
#58591=CARTESIAN_POINT('Ctrl Pts',(-13.7047658650663,36.4345131254237,17.));
#58592=CARTESIAN_POINT('Ctrl Pts',(-13.7353857954243,36.3131762502625,17.));
#58593=CARTESIAN_POINT('Ctrl Pts',(-13.7610637989098,36.2114226320506,17.));
#58594=CARTESIAN_POINT('Ctrl Pts',(-13.7828351362415,36.1086819645596,17.));
#58595=CARTESIAN_POINT('Ctrl Pts',(-13.8006475130466,36.0052062251963,17.));
#58596=CARTESIAN_POINT('Ctrl Pts',(-13.8084978850862,35.9596018086737,17.));
#58597=CARTESIAN_POINT('Ctrl Pts',(-13.8155789355258,35.9138546491184,17.));
#58598=CARTESIAN_POINT('Ctrl Pts',(-13.821884594521,35.8679866185036,17.));
#58599=CARTESIAN_POINT('Ctrl Pts',(-13.8245836173036,35.8483536412497,17.));
#58600=CARTESIAN_POINT('Ctrl Pts',(-13.8271405674798,35.8286985223403,17.));
#58601=CARTESIAN_POINT('Ctrl Pts',(-13.8295549143713,35.8090229935632,17.));
#58602=CARTESIAN_POINT('Ctrl Pts',(-13.8317980116041,35.7907430503162,17.));
#58603=CARTESIAN_POINT('Ctrl Pts',(-13.8339175340875,35.7724490669597,17.));
#58604=CARTESIAN_POINT('Ctrl Pts',(-13.8359122468823,35.7541522042298,17.));
#58605=CARTESIAN_POINT('Ctrl Pts',(-13.8491708905682,35.6325349046639,17.));
#58606=CARTESIAN_POINT('Ctrl Pts',(-13.8569353644682,35.5106633232552,17.));
#58607=CARTESIAN_POINT('Ctrl Pts',(-13.8591710359411,35.3889344818084,17.));
#58608=CARTESIAN_POINT('Ctrl Pts',(-13.8613888966442,35.2681754091286,17.));
#58609=CARTESIAN_POINT('Ctrl Pts',(-13.8581656100447,35.1475559779588,17.));
#58610=CARTESIAN_POINT('Ctrl Pts',(-13.8494169850101,35.0274704860568,17.));
#58611=CARTESIAN_POINT('Ctrl Pts',(-13.8408792900479,34.9102802652854,17.));
#58612=CARTESIAN_POINT('Ctrl Pts',(-13.8270792795936,34.7935978726728,17.));
#58613=CARTESIAN_POINT('Ctrl Pts',(-13.8078928234413,34.6778071494505,17.));
#58614=CARTESIAN_POINT('Ctrl Pts',(-13.7961972995813,34.607224382343,17.));
#58615=CARTESIAN_POINT('Ctrl Pts',(-13.7824994107177,34.5369733219596,17.));
#58616=CARTESIAN_POINT('Ctrl Pts',(-13.7667627942638,34.4671457809156,17.));
#58617=CARTESIAN_POINT('Ctrl Pts',(-13.7572176645193,34.4247915085752,17.));
#58618=CARTESIAN_POINT('Ctrl Pts',(-13.7469223466112,34.3825931317931,17.));
#58619=CARTESIAN_POINT('Ctrl Pts',(-13.7358676068506,34.340571973438,17.));
#58620=CARTESIAN_POINT('Ctrl Pts',(-13.7309282145613,34.3217964083807,17.));
#58621=CARTESIAN_POINT('Ctrl Pts',(-13.7258367127005,34.3030548272173,17.));
#58622=CARTESIAN_POINT('Ctrl Pts',(-13.7205981502818,34.2843693290194,17.));
#58623=CARTESIAN_POINT('Ctrl Pts',(-13.689338264928,34.1728680267999,17.));
#58624=CARTESIAN_POINT('Ctrl Pts',(-13.6528033562578,34.0631963206846,17.));
#58625=CARTESIAN_POINT('Ctrl Pts',(-13.6109173793413,33.9557088671316,17.));
#58626=CARTESIAN_POINT('Ctrl Pts',(-13.5979450581991,33.9224194020434,17.));
#58627=CARTESIAN_POINT('Ctrl Pts',(-13.5844591309443,33.8893395894124,17.));
#58628=CARTESIAN_POINT('Ctrl Pts',(-13.5704564135702,33.8564804057572,17.));
#58629=CARTESIAN_POINT('Ctrl Pts',(-13.5243066910341,33.7481841252616,17.));
#58630=CARTESIAN_POINT('Ctrl Pts',(-13.4725467214683,33.6422818048275,17.));
#58631=CARTESIAN_POINT('Ctrl Pts',(-13.4155273320418,33.539047281335,17.));
#58632=CARTESIAN_POINT('Ctrl Pts',(-13.3586530947265,33.4360755580789,17.));
#58633=CARTESIAN_POINT('Ctrl Pts',(-13.2965453659658,33.3357575270244,17.));
#58634=CARTESIAN_POINT('Ctrl Pts',(-13.2295170803124,33.2384027306936,17.));
#58635=CARTESIAN_POINT('Ctrl Pts',(-13.1958682827822,33.1895297541822,17.));
#58636=CARTESIAN_POINT('Ctrl Pts',(-13.1609789634487,33.1414041960367,17.));
#58637=CARTESIAN_POINT('Ctrl Pts',(-13.1248863292235,33.0940694733039,17.));
#58638=CARTESIAN_POINT('Ctrl Pts',(-13.1136852563331,33.0793795042573,17.));
#58639=CARTESIAN_POINT('Ctrl Pts',(-13.1023682800586,33.06476572469,17.));
#58640=CARTESIAN_POINT('Ctrl Pts',(-13.090936489294,33.0502294936717,17.));
#58641=CARTESIAN_POINT('Ctrl Pts',(-13.0810912756462,33.0377106938654,17.));
#58642=CARTESIAN_POINT('Ctrl Pts',(-13.0711638284922,33.0252531825434,17.));
#58643=CARTESIAN_POINT('Ctrl Pts',(-13.0611599663059,33.0128637449684,17.));
#58644=CARTESIAN_POINT('Ctrl Pts',(-12.9882950661098,32.9226230843549,17.));
#58645=CARTESIAN_POINT('Ctrl Pts',(-12.9113010014507,32.8358909574534,17.));
#58646=CARTESIAN_POINT('Ctrl Pts',(-12.8305230803461,32.7529134373871,17.));
#58647=CARTESIAN_POINT('Ctrl Pts',(-12.7496940850864,32.6698834524061,17.));
#58648=CARTESIAN_POINT('Ctrl Pts',(-12.6650756390752,32.5906122997939,17.));
#58649=CARTESIAN_POINT('Ctrl Pts',(-12.5769819956178,32.5153878223483,17.));
#58650=CARTESIAN_POINT('Ctrl Pts',(-12.4904417698574,32.4414898314677,17.));
#58651=CARTESIAN_POINT('Ctrl Pts',(-12.4005470330641,32.371496714977,17.));
#58652=CARTESIAN_POINT('Ctrl Pts',(-12.3075770876119,32.3057274062505,17.));
#58653=CARTESIAN_POINT('Ctrl Pts',(-12.2551730571484,32.2686554595983,17.));
#58654=CARTESIAN_POINT('Ctrl Pts',(-12.2017917003474,32.2329263645682,17.));
#58655=CARTESIAN_POINT('Ctrl Pts',(-12.1474817625173,32.198604486143,17.));
#58656=CARTESIAN_POINT('Ctrl Pts',(-12.1187454577522,32.1804442009734,17.));
#58657=CARTESIAN_POINT('Ctrl Pts',(-12.0897491736939,32.1626779784828,17.));
#58658=CARTESIAN_POINT('Ctrl Pts',(-12.0605001014649,32.1453159941706,17.));
#58659=CARTESIAN_POINT('Ctrl Pts',(-12.0439204100942,32.1354744395659,17.));
#58660=CARTESIAN_POINT('Ctrl Pts',(-12.0272576783142,32.1257618412,17.));
#58661=CARTESIAN_POINT('Ctrl Pts',(-12.0105328383307,32.1161910461162,17.));
#58662=CARTESIAN_POINT('Ctrl Pts',(-11.9136863575601,32.0607706162074,17.));
#58663=CARTESIAN_POINT('Ctrl Pts',(-11.8146169520547,32.0100152898296,17.));
#58664=CARTESIAN_POINT('Ctrl Pts',(-11.7136099215379,31.9641826653935,17.));
#58665=CARTESIAN_POINT('Ctrl Pts',(-11.6141161250821,31.9190366811649,17.));
#58666=CARTESIAN_POINT('Ctrl Pts',(-11.512741606946,31.8786667193764,17.));
#58667=CARTESIAN_POINT('Ctrl Pts',(-11.4097470166284,31.8433673104104,17.));
#58668=CARTESIAN_POINT('Ctrl Pts',(-11.3098310001791,31.8091230232492,17.));
#58669=CARTESIAN_POINT('Ctrl Pts',(-11.2083897167571,31.7796505908842,17.));
#58670=CARTESIAN_POINT('Ctrl Pts',(-11.1056593067708,31.7552673702842,17.));
#58671=CARTESIAN_POINT('Ctrl Pts',(-11.0406608290356,31.7398398817588,17.));
#58672=CARTESIAN_POINT('Ctrl Pts',(-10.9751462807458,31.7264506838377,17.));
#58673=CARTESIAN_POINT('Ctrl Pts',(-10.9091766549683,31.7151909620675,17.));
#58674=CARTESIAN_POINT('Ctrl Pts',(-10.8685408754868,31.708255231184,17.));
#58675=CARTESIAN_POINT('Ctrl Pts',(-10.8277324413485,31.7021276870367,17.));
#58676=CARTESIAN_POINT('Ctrl Pts',(-10.7867731801703,31.6968047429727,17.));
#58677=CARTESIAN_POINT('Ctrl Pts',(-7.43281944318039,37.2044345752726,29.9966888174997));
#58678=CARTESIAN_POINT('Ctrl Pts',(-6.70433239249398,36.3561656695364,29.9309499309566));
#58679=CARTESIAN_POINT('Ctrl Pts',(-6.16680179062131,33.8959591706789,29.7995178935572));
#58680=CARTESIAN_POINT('Ctrl Pts',(-8.82688724400274,31.1837581319228,29.6023927053017));
#58681=CARTESIAN_POINT('Ctrl Pts',(-12.5469209189557,31.9295115870956,29.4053132527333));
#58682=CARTESIAN_POINT('Ctrl Pts',(-13.9650991559566,35.445741398928,29.2082338001648));
#58683=CARTESIAN_POINT('Ctrl Pts',(-11.8002654955171,38.5612862953215,29.0111543475964));
#58684=CARTESIAN_POINT('Ctrl Pts',(-8.00850991085725,38.4575298371214,28.8140748950279));
#58685=CARTESIAN_POINT('Ctrl Pts',(-6.01644546373737,35.2298316539741,28.6169954424595));
#58686=CARTESIAN_POINT('Ctrl Pts',(-7.62419319279026,31.7941726174109,28.419915989891));
#58687=CARTESIAN_POINT('Ctrl Pts',(-11.3789020069552,31.255667443897,28.2228365373226));
#58688=CARTESIAN_POINT('Ctrl Pts',(-13.8875300071254,34.1007462780832,28.0257570847542));
#58689=CARTESIAN_POINT('Ctrl Pts',(-12.8831049662547,37.7584902581075,27.8286776321857));
#58690=CARTESIAN_POINT('Ctrl Pts',(-9.27329511580484,38.9234444319071,27.6315981796173));
#58691=CARTESIAN_POINT('Ctrl Pts',(-6.32018930815337,36.5428969771351,27.4345187270488));
#58692=CARTESIAN_POINT('Ctrl Pts',(-6.69242821576807,32.7680711157438,27.2374392744804));
#58693=CARTESIAN_POINT('Ctrl Pts',(-10.0536300766488,31.0101809435409,27.0403598219119));
#58694=CARTESIAN_POINT('Ctrl Pts',(-13.3663678211108,32.8577808295107,26.8432803693435));
#58695=CARTESIAN_POINT('Ctrl Pts',(-13.6370104108175,36.6412465561122,26.6462009167751));
#58696=CARTESIAN_POINT('Ctrl Pts',(-10.6209854317379,38.9415620618598,26.4491214642066));
#58697=CARTESIAN_POINT('Ctrl Pts',(-7.04379278912358,37.6799950971764,26.2520420116382));
#58698=CARTESIAN_POINT('Ctrl Pts',(-6.13804432686434,33.9965892654983,26.0549625590698));
#58699=CARTESIAN_POINT('Ctrl Pts',(-8.72224034293969,31.2199385031057,25.8578831065013));
#58700=CARTESIAN_POINT('Ctrl Pts',(-12.4611130642332,31.8592266559683,25.6608036539329));
#58701=CARTESIAN_POINT('Ctrl Pts',(-13.9759447379094,35.3367464054446,25.4637242013644));
#58702=CARTESIAN_POINT('Ctrl Pts',(-11.8978231126421,38.5099575677875,25.266644748796));
#58703=CARTESIAN_POINT('Ctrl Pts',(-8.10469027325444,38.5113153861208,25.0695652962275));
#58704=CARTESIAN_POINT('Ctrl Pts',(-6.02429736947304,35.3395928335728,24.8724858436591));
#58705=CARTESIAN_POINT('Ctrl Pts',(-7.53663897851176,31.8609894590311,24.6754063910907));
#58706=CARTESIAN_POINT('Ctrl Pts',(-11.275053053664,31.2190246748164,24.4783269385222));
#58707=CARTESIAN_POINT('Ctrl Pts',(-13.8612363064412,33.9938246252232,24.2812474859537));
#58708=CARTESIAN_POINT('Ctrl Pts',(-12.9581251553404,37.6778779405159,24.0841680333854));
#58709=CARTESIAN_POINT('Ctrl Pts',(-9.38183662494831,38.9420056748818,23.8870885808168));
#58710=CARTESIAN_POINT('Ctrl Pts',(-6.36416555126165,36.6438499202713,23.6900091282485));
#58711=CARTESIAN_POINT('Ctrl Pts',(-6.63209934310249,32.8601916290756,23.49292967568));
#58712=CARTESIAN_POINT('Ctrl Pts',(-9.94351350813597,31.0102200592936,23.2958502231116));
#58713=CARTESIAN_POINT('Ctrl Pts',(-13.3059729820585,32.7657042852594,23.0987707705431));
#58714=CARTESIAN_POINT('Ctrl Pts',(-13.6809144409843,36.5402608795793,22.9016913179747));
#58715=CARTESIAN_POINT('Ctrl Pts',(-10.7295134694718,38.9229255405774,22.7046118654062));
#58716=CARTESIAN_POINT('Ctrl Pts',(-7.11887098447587,37.7605489118768,22.5075324128378));
#58717=CARTESIAN_POINT('Ctrl Pts',(-6.11182655793853,34.1035391902405,22.3104529602694));
#58718=CARTESIAN_POINT('Ctrl Pts',(-8.61841889329849,31.2566367602235,22.1133735077009));
#58719=CARTESIAN_POINT('Ctrl Pts',(-12.3735085599531,31.7925100445471,21.9162940551325));
#58720=CARTESIAN_POINT('Ctrl Pts',(-13.9837229901626,35.2269049066077,21.719214602564));
#58721=CARTESIAN_POINT('Ctrl Pts',(-11.9939551263463,38.4562519663969,21.5221351499956));
#58722=CARTESIAN_POINT('Ctrl Pts',(-8.20230415784552,38.5622779725406,21.3250556974271));
#58723=CARTESIAN_POINT('Ctrl Pts',(-6.0351821079984,35.4491701055871,21.1279762448587));
#58724=CARTESIAN_POINT('Ctrl Pts',(-7.45095832845666,31.930159406377,20.9308967922902));
#58725=CARTESIAN_POINT('Ctrl Pts',(-11.1702342916329,31.1852803033251,20.7338173397218));
#58726=CARTESIAN_POINT('Ctrl Pts',(-13.8320013021391,33.887659789551,20.5367378871533));
#58727=CARTESIAN_POINT('Ctrl Pts',(-13.0308927869956,37.5952309547061,20.3396584345849));
#58728=CARTESIAN_POINT('Ctrl Pts',(-9.49084876237968,38.9575623066672,20.1425789820165));
#58729=CARTESIAN_POINT('Ctrl Pts',(-6.41091088066521,36.7435522016327,19.945499529448));
#58730=CARTESIAN_POINT('Ctrl Pts',(-6.57433539009964,32.9539410414412,19.7484200768796));
#58731=CARTESIAN_POINT('Ctrl Pts',(-9.83343996764695,31.0132983502615,19.5513406243111));
#58732=CARTESIAN_POINT('Ctrl Pts',(-13.2430603653772,32.6753285998351,19.3542611717427));
#58733=CARTESIAN_POINT('Ctrl Pts',(-13.7220150885897,36.4381034351505,19.1571817191743));
#58734=CARTESIAN_POINT('Ctrl Pts',(-10.8374860072516,38.9012989358204,18.9601022666058));
#58735=CARTESIAN_POINT('Ctrl Pts',(-7.19614323312918,37.83900510415,18.7630228140374));
#58736=CARTESIAN_POINT('Ctrl Pts',(-6.08857033917078,34.2111623607691,18.5659433614689));
#58737=CARTESIAN_POINT('Ctrl Pts',(-8.51564891709047,31.296204798029,18.3688639089005));
#58738=CARTESIAN_POINT('Ctrl Pts',(-12.2840978586159,31.7281986361625,18.1717844563321));
#58739=CARTESIAN_POINT('Ctrl Pts',(-13.9884644187953,35.1169654331458,17.9747050037636));
#58740=CARTESIAN_POINT('Ctrl Pts',(-12.0885742745814,38.3997651167831,17.7776255511952));
#58741=CARTESIAN_POINT('Ctrl Pts',(-8.30127578536255,38.6108242790529,17.5805460986267));
#58742=CARTESIAN_POINT('Ctrl Pts',(-6.0491089823217,35.5578143756796,17.3834666460583));
#58743=CARTESIAN_POINT('Ctrl Pts',(-7.36717462669024,32.002845380223,17.1863871934898));
#58744=CARTESIAN_POINT('Ctrl Pts',(-11.0646050703342,31.1520769786589,16.9893077409214));
#58745=CARTESIAN_POINT('Ctrl Pts',(-13.7997717921734,33.78727260672,16.7922282883529));
#58746=CARTESIAN_POINT('Ctrl Pts',(-13.3330648228068,36.2606000081635,16.6608419866407));
#58747=CARTESIAN_POINT('Ctrl Pts',(-12.6300280270065,37.1290610164239,16.5951488357845));
#58748=CARTESIAN_POINT('Ctrl Pts',(-7.25452804718548,37.3575331630446,30.1323685894149));
#58749=CARTESIAN_POINT('Ctrl Pts',(-6.47544737039588,36.4503517484157,30.0666297028717));
#58750=CARTESIAN_POINT('Ctrl Pts',(-5.90058512032913,33.8192832313211,29.9351976654724));
#58751=CARTESIAN_POINT('Ctrl Pts',(-8.74541424033318,30.9187190841993,29.7380724772169));
#58752=CARTESIAN_POINT('Ctrl Pts',(-12.7238052775268,31.7162653220174,29.5409930246485));
#58753=CARTESIAN_POINT('Ctrl Pts',(-14.2404763832793,35.4766982617231,29.34391357208));
#58754=CARTESIAN_POINT('Ctrl Pts',(-11.9252944294986,38.8086186083696,29.1468341195116));
#58755=CARTESIAN_POINT('Ctrl Pts',(-7.87020037623567,38.6976562356004,28.9497546669431));
#58756=CARTESIAN_POINT('Ctrl Pts',(-5.73978650517466,35.2457935255776,28.7526752143747));
#58757=CARTESIAN_POINT('Ctrl Pts',(-7.45919275635956,31.5715270236516,28.5555957618062));
#58758=CARTESIAN_POINT('Ctrl Pts',(-11.4746671307238,30.995622517675,28.3585163092378));
#58759=CARTESIAN_POINT('Ctrl Pts',(-14.1575200357198,34.038292859679,28.1614368566694));
#58760=CARTESIAN_POINT('Ctrl Pts',(-13.0833373994071,37.9500681654932,27.9643574041009));
#58761=CARTESIAN_POINT('Ctrl Pts',(-9.2228252616548,39.1959287271839,27.7672779515325));
#58762=CARTESIAN_POINT('Ctrl Pts',(-6.06462544315624,36.6500515967036,27.570198498964));
#58763=CARTESIAN_POINT('Ctrl Pts',(-6.46271644532108,32.6130630406483,27.3731190463956));
#58764=CARTESIAN_POINT('Ctrl Pts',(-10.0573547002275,30.733086912327,27.1760395938271));
#58765=CARTESIAN_POINT('Ctrl Pts',(-13.6001629924959,32.7090031187187,26.9789601412587));
#58766=CARTESIAN_POINT('Ctrl Pts',(-13.8896017845213,36.7552315810001,26.7818806886903));
#58767=CARTESIAN_POINT('Ctrl Pts',(-10.6641130408276,39.2153046315217,26.5848012361218));
#58768=CARTESIAN_POINT('Ctrl Pts',(-6.83848338496921,37.8661214940384,26.3877217835534));
#58769=CARTESIAN_POINT('Ctrl Pts',(-5.86983044280201,33.9269021139128,26.190642330985));
#58770=CARTESIAN_POINT('Ctrl Pts',(-8.63349958319917,30.9574121921154,25.9935628784165));
#58771=CARTESIAN_POINT('Ctrl Pts',(-12.6320380436851,31.6410990830854,25.7964834258481));
#58772=CARTESIAN_POINT('Ctrl Pts',(-14.2520751938827,35.3601335359538,25.5994039732796));
#58773=CARTESIAN_POINT('Ctrl Pts',(-12.0296274499745,38.753725086586,25.4023245207112));
#58774=CARTESIAN_POINT('Ctrl Pts',(-7.97306049126402,38.7551772057762,25.2052450681427));
#58775=CARTESIAN_POINT('Ctrl Pts',(-5.74818372792402,35.3631776492987,25.0081656155743));
#58776=CARTESIAN_POINT('Ctrl Pts',(-7.36555787781011,31.6429843133059,24.8110861630058));
#58777=CARTESIAN_POINT('Ctrl Pts',(-11.363605839054,30.9564348982,24.6140067104374));
#58778=CARTESIAN_POINT('Ctrl Pts',(-14.1294002302886,33.9239454686098,24.416927257869));
#58779=CARTESIAN_POINT('Ctrl Pts',(-13.1635677612655,37.8638573002654,24.2198478053005));
#58780=CARTESIAN_POINT('Ctrl Pts',(-9.338905008472,39.21577905359,24.0227683527321));
#58781=CARTESIAN_POINT('Ctrl Pts',(-6.11165584844781,36.7580157495165,23.8256889001636));
#58782=CARTESIAN_POINT('Ctrl Pts',(-6.39819771585024,32.7115813489765,23.6286094475952));
#58783=CARTESIAN_POINT('Ctrl Pts',(-9.93959050573454,30.7331287446795,23.4315299950267));
#58784=CARTESIAN_POINT('Ctrl Pts',(-13.5355737152546,32.6105318331355,23.2344505424584));
#58785=CARTESIAN_POINT('Ctrl Pts',(-13.9365549616627,36.6472324214472,23.0373710898898));
#58786=CARTESIAN_POINT('Ctrl Pts',(-10.780178380642,39.1953737987086,22.8402916373215));
#58787=CARTESIAN_POINT('Ctrl Pts',(-6.91877578164541,37.952269793333,22.643212184753));
#58788=CARTESIAN_POINT('Ctrl Pts',(-5.84179184261089,34.0412797403541,22.4461327321845));
#58789=CARTESIAN_POINT('Ctrl Pts',(-8.52246770531536,30.9966591532869,22.2490532796161));
#58790=CARTESIAN_POINT('Ctrl Pts',(-12.5383493824794,31.569748984645,22.0519738270477));
#58791=CARTESIAN_POINT('Ctrl Pts',(-14.260393647895,35.2426635148013,21.8548943744792));
#58792=CARTESIAN_POINT('Ctrl Pts',(-12.1324358584799,38.6962896164025,21.6578149219108));
#58793=CARTESIAN_POINT('Ctrl Pts',(-8.07745368699706,38.8096791578444,21.4607354693423));
#58794=CARTESIAN_POINT('Ctrl Pts',(-5.75982441453476,35.480365093003,21.2636560167739));
#58795=CARTESIAN_POINT('Ctrl Pts',(-7.27392668303485,31.7169581325262,21.0665765642054));
#58796=CARTESIAN_POINT('Ctrl Pts',(-11.2515073851604,30.9203469708242,20.869497111637));
#58797=CARTESIAN_POINT('Ctrl Pts',(-14.0981348468943,33.8104074558905,20.6724176590685));
#58798=CARTESIAN_POINT('Ctrl Pts',(-13.2413891249602,37.775470458552,20.4753382065001));
#58799=CARTESIAN_POINT('Ctrl Pts',(-9.45548806884112,39.2324160977332,20.2782587539317));
#58800=CARTESIAN_POINT('Ctrl Pts',(-6.16164765383978,36.86464238175,20.0811793013632));
#58801=CARTESIAN_POINT('Ctrl Pts',(-6.33642204041841,32.8118416838248,19.8840998487948));
#58802=CARTESIAN_POINT('Ctrl Pts',(-9.82187232757338,30.736420823802,19.6870203962264));
#58803=CARTESIAN_POINT('Ctrl Pts',(-13.4682918000352,32.5138795314929,19.4899409436579));
#58804=CARTESIAN_POINT('Ctrl Pts',(-13.9805100605527,36.5379801143958,19.2928614910895));
#58805=CARTESIAN_POINT('Ctrl Pts',(-10.8956496408777,39.172245220301,19.095782038521));
#58806=CARTESIAN_POINT('Ctrl Pts',(-7.00141460922806,38.0361747897458,18.8987025859526));
#58807=CARTESIAN_POINT('Ctrl Pts',(-5.81692047305108,34.1563773696868,18.7016231333842));
#58808=CARTESIAN_POINT('Ctrl Pts',(-8.41256032598399,31.0389752022047,18.5045436808157));
#58809=CARTESIAN_POINT('Ctrl Pts',(-12.4427290833343,31.5009711312537,18.3074642282473));
#58810=CARTESIAN_POINT('Ctrl Pts',(-14.2654643700508,35.1250887146591,18.1103847756788));
#58811=CARTESIAN_POINT('Ctrl Pts',(-12.233626332593,38.6358797395415,17.9133053231104));
#58812=CARTESIAN_POINT('Ctrl Pts',(-8.18329892127581,38.8615970187009,17.7162258705419));
#58813=CARTESIAN_POINT('Ctrl Pts',(-5.77471851411159,35.5965547375453,17.5191464179735));
#58814=CARTESIAN_POINT('Ctrl Pts',(-7.18432418012883,31.7946921672543,17.322066965405));
#58815=CARTESIAN_POINT('Ctrl Pts',(-11.1385421853802,30.8848376661246,17.1249875128366));
#58816=CARTESIAN_POINT('Ctrl Pts',(-14.0636669885939,33.7030483555917,16.9279080602682));
#58817=CARTESIAN_POINT('Ctrl Pts',(-13.5645470917968,36.3481490255669,16.7965217585559));
#58818=CARTESIAN_POINT('Ctrl Pts',(-12.8126841970975,37.2769248897959,16.7308286076997));
#58819=CARTESIAN_POINT('Ctrl Pts',(-7.07623665119056,37.5106317508166,30.2680483613301));
#58820=CARTESIAN_POINT('Ctrl Pts',(-6.24656234829778,36.544537827295,30.2023094747869));
#58821=CARTESIAN_POINT('Ctrl Pts',(-5.63436845003696,33.7426072919634,30.0708774373876));
#58822=CARTESIAN_POINT('Ctrl Pts',(-8.66394123666363,30.6536800364758,29.8737522491321));
#58823=CARTESIAN_POINT('Ctrl Pts',(-12.9006896360979,31.5030190569393,29.6766727965637));
#58824=CARTESIAN_POINT('Ctrl Pts',(-14.515853610602,35.5076551245181,29.4795933439952));
#58825=CARTESIAN_POINT('Ctrl Pts',(-12.0503233634801,39.0559509214177,29.2825138914268));
#58826=CARTESIAN_POINT('Ctrl Pts',(-7.73189084161409,38.9377826340795,29.0854344388583));
#58827=CARTESIAN_POINT('Ctrl Pts',(-5.46312754661196,35.2617553971811,28.8883549862899));
#58828=CARTESIAN_POINT('Ctrl Pts',(-7.29419231992886,31.3488814298923,28.6912755337214));
#58829=CARTESIAN_POINT('Ctrl Pts',(-11.5704322544924,30.7355775914529,28.494196081153));
#58830=CARTESIAN_POINT('Ctrl Pts',(-14.4275100643141,33.9758394412748,28.2971166285846));
#58831=CARTESIAN_POINT('Ctrl Pts',(-13.2835698325594,38.1416460728787,28.1000371760161));
#58832=CARTESIAN_POINT('Ctrl Pts',(-9.17235540750479,39.4684130224607,27.9029577234477));
#58833=CARTESIAN_POINT('Ctrl Pts',(-5.80906157815909,36.7572062162722,27.7058782708792));
#58834=CARTESIAN_POINT('Ctrl Pts',(-6.23300467487411,32.4580549655527,27.5087988183108));
#58835=CARTESIAN_POINT('Ctrl Pts',(-10.0610793238064,30.4559928811131,27.3117193657423));
#58836=CARTESIAN_POINT('Ctrl Pts',(-13.8339581638812,32.5602254079266,27.1146399131739));
#58837=CARTESIAN_POINT('Ctrl Pts',(-14.1421931582251,36.8692166058882,26.9175604606055));
#58838=CARTESIAN_POINT('Ctrl Pts',(-10.7072406499173,39.4890472011835,26.7204810080371));
#58839=CARTESIAN_POINT('Ctrl Pts',(-6.63317398081481,38.0522478909004,26.5234015554685));
#58840=CARTESIAN_POINT('Ctrl Pts',(-5.60161655873972,33.8572149623272,26.3263221029002));
#58841=CARTESIAN_POINT('Ctrl Pts',(-8.54475882345865,30.6948858811251,26.1292426503317));
#58842=CARTESIAN_POINT('Ctrl Pts',(-12.8029630231369,31.4229715102027,25.9321631977633));
#58843=CARTESIAN_POINT('Ctrl Pts',(-14.5282056498561,35.383520666463,25.7350837451948));
#58844=CARTESIAN_POINT('Ctrl Pts',(-12.161431787307,38.9974926053846,25.5380042926264));
#58845=CARTESIAN_POINT('Ctrl Pts',(-7.8414307092736,38.9990390254316,25.3409248400579));
#58846=CARTESIAN_POINT('Ctrl Pts',(-5.47207008637501,35.3867624650245,25.1438453874895));
#58847=CARTESIAN_POINT('Ctrl Pts',(-7.19447677710844,31.4249791675809,24.946765934921));
#58848=CARTESIAN_POINT('Ctrl Pts',(-11.4521586244438,30.6938451215836,24.7496864823526));
#58849=CARTESIAN_POINT('Ctrl Pts',(-14.3975641541361,33.8540663119965,24.5526070297842));
#58850=CARTESIAN_POINT('Ctrl Pts',(-13.3690103671906,38.0498366600148,24.3555275772157));
#58851=CARTESIAN_POINT('Ctrl Pts',(-9.29597339199564,39.4895524322982,24.1584481246473));
#58852=CARTESIAN_POINT('Ctrl Pts',(-5.859146145634,36.8721815787616,23.9613686720789));
#58853=CARTESIAN_POINT('Ctrl Pts',(-6.16429608859798,32.5629710688776,23.7642892195104));
#58854=CARTESIAN_POINT('Ctrl Pts',(-9.93566750333314,30.4560374300653,23.5672097669419));
#58855=CARTESIAN_POINT('Ctrl Pts',(-13.7651744484508,32.4553593810116,23.3701303143735));
#58856=CARTESIAN_POINT('Ctrl Pts',(-14.1921954823411,36.7542039633153,23.1730508618051));
#58857=CARTESIAN_POINT('Ctrl Pts',(-10.8308432918122,39.4678220568397,22.9759714092366));
#58858=CARTESIAN_POINT('Ctrl Pts',(-6.71868057881495,38.1439906747893,22.7788919566682));
#58859=CARTESIAN_POINT('Ctrl Pts',(-5.57175712728321,33.9790202904677,22.5818125040997));
#58860=CARTESIAN_POINT('Ctrl Pts',(-8.42651651733225,30.7366815463504,22.3847330515313));
#58861=CARTESIAN_POINT('Ctrl Pts',(-12.7031902050059,31.3469879247428,22.1876535989628));
#58862=CARTESIAN_POINT('Ctrl Pts',(-14.5370643056275,35.2584221229949,21.9905741463944));
#58863=CARTESIAN_POINT('Ctrl Pts',(-12.2709165906135,38.9363272664081,21.793494693826));
#58864=CARTESIAN_POINT('Ctrl Pts',(-7.95260321614858,39.0570803431483,21.5964152412575));
#58865=CARTESIAN_POINT('Ctrl Pts',(-5.48446672107112,35.5115600804189,21.3993357886891));
#58866=CARTESIAN_POINT('Ctrl Pts',(-7.09689503761302,31.5037568586754,21.2022563361206));
#58867=CARTESIAN_POINT('Ctrl Pts',(-11.3327804786878,30.6554136383235,21.0051768835522));
#58868=CARTESIAN_POINT('Ctrl Pts',(-14.3642683916493,33.7331551222299,20.8080974309837));
#58869=CARTESIAN_POINT('Ctrl Pts',(-13.4518854629247,37.9557099623979,20.6110179784153));
#58870=CARTESIAN_POINT('Ctrl Pts',(-9.42012737530255,39.5072698887991,20.4139385258469));
#58871=CARTESIAN_POINT('Ctrl Pts',(-5.91238442701437,36.9857325618673,20.2168590732784));
#58872=CARTESIAN_POINT('Ctrl Pts',(-6.09850869073715,32.6697423262084,20.01977962071));
#58873=CARTESIAN_POINT('Ctrl Pts',(-9.8103046874998,30.4595432973425,19.8227001681415));
#58874=CARTESIAN_POINT('Ctrl Pts',(-13.6935232346933,32.3524304631507,19.6256207155731));
#58875=CARTESIAN_POINT('Ctrl Pts',(-14.2390050325155,36.637856793641,19.4285412630047));
#58876=CARTESIAN_POINT('Ctrl Pts',(-10.9538132745039,39.4431915047816,19.2314618104362));
#58877=CARTESIAN_POINT('Ctrl Pts',(-6.80668598532695,38.2333444753415,19.0343823578678));
#58878=CARTESIAN_POINT('Ctrl Pts',(-5.54527060693137,34.1015923786047,18.8373029052994));
#58879=CARTESIAN_POINT('Ctrl Pts',(-8.3094717348775,30.7817456063805,18.6402234527309));
#58880=CARTESIAN_POINT('Ctrl Pts',(-12.6013603080527,31.2737436263448,18.4431440001625));
#58881=CARTESIAN_POINT('Ctrl Pts',(-14.5424643213063,35.1332119961725,18.246064547594));
#58882=CARTESIAN_POINT('Ctrl Pts',(-12.3786783906047,38.8719943622999,18.0489850950256));
#58883=CARTESIAN_POINT('Ctrl Pts',(-8.06532205718906,39.112369758349,17.8519056424571));
#58884=CARTESIAN_POINT('Ctrl Pts',(-5.50032804590148,35.635295099411,17.6548261898887));
#58885=CARTESIAN_POINT('Ctrl Pts',(-7.00147373356744,31.5865389542858,17.4577467373202));
#58886=CARTESIAN_POINT('Ctrl Pts',(-11.212479300426,30.6175983535903,17.2606672847518));
#58887=CARTESIAN_POINT('Ctrl Pts',(-14.3275621850144,33.6188241044634,17.0635878321833));
#58888=CARTESIAN_POINT('Ctrl Pts',(-13.7960293607869,36.4356980429703,16.932201530471));
#58889=CARTESIAN_POINT('Ctrl Pts',(-12.9953403671885,37.424788763168,16.8665083796149));
#58890=CARTESIAN_POINT('Ctrl Pts',(-6.89794525519566,37.6637303385885,30.4037281332453));
#58891=CARTESIAN_POINT('Ctrl Pts',(-6.01767732619968,36.6387239061743,30.3379892467021));
#58892=CARTESIAN_POINT('Ctrl Pts',(-5.36815177974479,33.6659313526057,30.2065572093028));
#58893=CARTESIAN_POINT('Ctrl Pts',(-8.58246823299407,30.3886409887524,30.0094320210473));
#58894=CARTESIAN_POINT('Ctrl Pts',(-13.077573994669,31.2897727918613,29.8123525684789));
#58895=CARTESIAN_POINT('Ctrl Pts',(-14.7912308379247,35.5386119873131,29.6152731159104));
#58896=CARTESIAN_POINT('Ctrl Pts',(-12.1753522974616,39.303283234466,29.418193663342));
#58897=CARTESIAN_POINT('Ctrl Pts',(-7.59358130699251,39.1779090325584,29.2211142107735));
#58898=CARTESIAN_POINT('Ctrl Pts',(-5.18646858804926,35.2777172687847,29.0240347582051));
#58899=CARTESIAN_POINT('Ctrl Pts',(-7.12919188349817,31.1262358361329,28.8269553056366));
#58900=CARTESIAN_POINT('Ctrl Pts',(-11.6661973782611,30.4755326652309,28.6298758530682));
#58901=CARTESIAN_POINT('Ctrl Pts',(-14.6975000929084,33.9133860228706,28.4327964004997));
#58902=CARTESIAN_POINT('Ctrl Pts',(-13.4838022657118,38.3332239802643,28.2357169479313));
#58903=CARTESIAN_POINT('Ctrl Pts',(-9.12188555335475,39.7408973177375,28.0386374953629));
#58904=CARTESIAN_POINT('Ctrl Pts',(-5.55349771316196,36.8643608358407,27.8415580427944));
#58905=CARTESIAN_POINT('Ctrl Pts',(-6.00329290442712,32.3030468904572,27.644478590226));
#58906=CARTESIAN_POINT('Ctrl Pts',(-10.0648039473853,30.178898849899,27.4473991376575));
#58907=CARTESIAN_POINT('Ctrl Pts',(-14.0677533352663,32.4114476971345,27.2503196850891));
#58908=CARTESIAN_POINT('Ctrl Pts',(-14.3947845319289,36.9832016307762,27.0532402325207));
#58909=CARTESIAN_POINT('Ctrl Pts',(-10.7503682590069,39.7627897708452,26.8561607799522));
#58910=CARTESIAN_POINT('Ctrl Pts',(-6.42786457666041,38.2383742877625,26.6590813273838));
#58911=CARTESIAN_POINT('Ctrl Pts',(-5.3334026746774,33.7875278107416,26.4620018748153));
#58912=CARTESIAN_POINT('Ctrl Pts',(-8.45601806371814,30.4323595701348,26.2649224222469));
#58913=CARTESIAN_POINT('Ctrl Pts',(-12.9738880025887,31.2048439373198,26.0678429696785));
#58914=CARTESIAN_POINT('Ctrl Pts',(-14.8043361058294,35.4069077969722,25.87076351711));
#58915=CARTESIAN_POINT('Ctrl Pts',(-12.2932361246394,39.241260124183,25.6736840645416));
#58916=CARTESIAN_POINT('Ctrl Pts',(-7.70980092728317,39.2429008450869,25.4766046119731));
#58917=CARTESIAN_POINT('Ctrl Pts',(-5.19595644482599,35.4103472807504,25.2795251594047));
#58918=CARTESIAN_POINT('Ctrl Pts',(-7.02339567640677,31.2069740218558,25.0824457068363));
#58919=CARTESIAN_POINT('Ctrl Pts',(-11.5407114098338,30.431255344967,24.8853662542678));
#58920=CARTESIAN_POINT('Ctrl Pts',(-14.6657280779835,33.7841871553832,24.6882868016994));
#58921=CARTESIAN_POINT('Ctrl Pts',(-13.5744529731157,38.2358160197642,24.4912073491309));
#58922=CARTESIAN_POINT('Ctrl Pts',(-9.25304177551932,39.7633258110065,24.2941278965625));
#58923=CARTESIAN_POINT('Ctrl Pts',(-5.60663644282017,36.9863474080067,24.097048443994));
#58924=CARTESIAN_POINT('Ctrl Pts',(-5.93039446134574,32.4143607887785,23.8999689914256));
#58925=CARTESIAN_POINT('Ctrl Pts',(-9.93174450093171,30.1789461154511,23.7028895388571));
#58926=CARTESIAN_POINT('Ctrl Pts',(-13.994775181647,32.3001869288876,23.5058100862887));
#58927=CARTESIAN_POINT('Ctrl Pts',(-14.4478360030196,36.8611755051832,23.3087306337203));
#58928=CARTESIAN_POINT('Ctrl Pts',(-10.8815082029825,39.7402703149709,23.1116511811518));
#58929=CARTESIAN_POINT('Ctrl Pts',(-6.51858537598449,38.3357115562455,22.9145717285834));
#58930=CARTESIAN_POINT('Ctrl Pts',(-5.30172241195556,33.9167608405812,22.7174922760149));
#58931=CARTESIAN_POINT('Ctrl Pts',(-8.33056532934912,30.4767039394141,22.5204128234465));
#58932=CARTESIAN_POINT('Ctrl Pts',(-12.8680310275323,31.1242268648406,22.323333370878));
#58933=CARTESIAN_POINT('Ctrl Pts',(-14.8137349633598,35.2741807311886,22.1262539183096));
#58934=CARTESIAN_POINT('Ctrl Pts',(-12.409397322747,39.1763649164138,21.9291744657412));
#58935=CARTESIAN_POINT('Ctrl Pts',(-7.82775274530012,39.3044815284521,21.7320950131727));
#58936=CARTESIAN_POINT('Ctrl Pts',(-5.20910902760746,35.5427550678348,21.5350155606043));
#58937=CARTESIAN_POINT('Ctrl Pts',(-6.91986339219122,31.2905555848246,21.3379361080358));
#58938=CARTESIAN_POINT('Ctrl Pts',(-11.4140535722153,30.3904803058226,21.1408566554674));
#58939=CARTESIAN_POINT('Ctrl Pts',(-14.6304019364044,33.6559027885695,20.9437772028989));
#58940=CARTESIAN_POINT('Ctrl Pts',(-13.6623818008893,38.1359494662436,20.7466977503305));
#58941=CARTESIAN_POINT('Ctrl Pts',(-9.384766681764,39.7821236798649,20.549618297762));
#58942=CARTESIAN_POINT('Ctrl Pts',(-5.66312120018892,37.1068227419848,20.3525388451936));
#58943=CARTESIAN_POINT('Ctrl Pts',(-5.86059534105592,32.5276429685921,20.1554593926252));
#58944=CARTESIAN_POINT('Ctrl Pts',(-9.79873704742623,30.182665770883,19.9583799400567));
#58945=CARTESIAN_POINT('Ctrl Pts',(-13.9187546693514,32.1909813948084,19.7613004874883));
#58946=CARTESIAN_POINT('Ctrl Pts',(-14.4975000044784,36.7377334728862,19.5642210349199));
#58947=CARTESIAN_POINT('Ctrl Pts',(-11.0119769081301,39.714137789262,19.3671415823514));
#58948=CARTESIAN_POINT('Ctrl Pts',(-6.61195736142583,38.4305141609372,19.170062129783));
#58949=CARTESIAN_POINT('Ctrl Pts',(-5.27362074081168,34.0468073875224,18.9729826772145));
#58950=CARTESIAN_POINT('Ctrl Pts',(-8.20638314377102,30.5245160105561,18.7759032246461));
#58951=CARTESIAN_POINT('Ctrl Pts',(-12.7599915327711,31.046516121436,18.5788237720777));
#58952=CARTESIAN_POINT('Ctrl Pts',(-14.8194642725618,35.1413352776858,18.3817443195092));
#58953=CARTESIAN_POINT('Ctrl Pts',(-12.5237304486164,39.1081089850583,18.1846648669408));
#58954=CARTESIAN_POINT('Ctrl Pts',(-7.9473451931023,39.3631424979969,17.9875854143723));
#58955=CARTESIAN_POINT('Ctrl Pts',(-5.22593757769137,35.6740354612769,17.7905059618039));
#58956=CARTESIAN_POINT('Ctrl Pts',(-6.81862328700602,31.3783857413171,17.5934265092354));
#58957=CARTESIAN_POINT('Ctrl Pts',(-11.2864164154719,30.350359041056,17.396347056667));
#58958=CARTESIAN_POINT('Ctrl Pts',(-14.5914573814348,33.5345998533351,17.1992676040985));
#58959=CARTESIAN_POINT('Ctrl Pts',(-14.027511629777,36.5232470603737,17.0678813023862));
#58960=CARTESIAN_POINT('Ctrl Pts',(-13.1779965372794,37.5726526365399,17.0021881515301));
#58961=CARTESIAN_POINT('Ctrl Pts',(-7.42676557298524,37.2065515280923,30.));
#58962=CARTESIAN_POINT('Ctrl Pts',(-7.34847363574758,37.1320407500307,30.));
#58963=CARTESIAN_POINT('Ctrl Pts',(-7.27428885024511,37.0537355480842,30.));
#58964=CARTESIAN_POINT('Ctrl Pts',(-7.20420769434694,36.9720784599283,30.));
#58965=CARTESIAN_POINT('Ctrl Pts',(-7.13363378334808,36.889847223898,30.));
#58966=CARTESIAN_POINT('Ctrl Pts',(-7.06722107630683,36.8042162244444,30.));
#58967=CARTESIAN_POINT('Ctrl Pts',(-7.00499287349493,36.7155880934709,30.));
#58968=CARTESIAN_POINT('Ctrl Pts',(-6.94120645481753,36.6247406832387,30.));
#58969=CARTESIAN_POINT('Ctrl Pts',(-6.88181624422247,36.5307436329052,30.));
#58970=CARTESIAN_POINT('Ctrl Pts',(-6.8268818722938,36.4339872175739,30.));
#58971=CARTESIAN_POINT('Ctrl Pts',(-6.77575400980664,36.3439352423875,30.));
#58972=CARTESIAN_POINT('Ctrl Pts',(-6.72848597396037,36.2514921521688,30.));
#58973=CARTESIAN_POINT('Ctrl Pts',(-6.68515714892584,36.1569468353438,30.));
#58974=CARTESIAN_POINT('Ctrl Pts',(-6.67815238204425,36.1416621396804,30.));
#58975=CARTESIAN_POINT('Ctrl Pts',(-6.67124986444939,36.1263207030674,30.));
#58976=CARTESIAN_POINT('Ctrl Pts',(-6.664452461429,36.1109292548971,30.));
#58977=CARTESIAN_POINT('Ctrl Pts',(-6.61833776570796,36.0065111489012,30.));
#58978=CARTESIAN_POINT('Ctrl Pts',(-6.57720059468109,35.9001204628048,30.));
#58979=CARTESIAN_POINT('Ctrl Pts',(-6.54106484244435,35.7921934874974,30.));
#58980=CARTESIAN_POINT('Ctrl Pts',(-6.50446358285172,35.6828761771951,30.));
#58981=CARTESIAN_POINT('Ctrl Pts',(-6.47299300143779,35.571982021054,30.));
#58982=CARTESIAN_POINT('Ctrl Pts',(-6.44671693976219,35.4599265310262,30.));
#58983=CARTESIAN_POINT('Ctrl Pts',(-6.42039387087784,35.3476705765652,30.));
#58984=CARTESIAN_POINT('Ctrl Pts',(-6.39928354477019,35.2342483047979,30.));
#58985=CARTESIAN_POINT('Ctrl Pts',(-6.38349503862451,35.1200514719229,30.));
#58986=CARTESIAN_POINT('Ctrl Pts',(-6.37020038024279,35.0238924137234,30.));
#58987=CARTESIAN_POINT('Ctrl Pts',(-6.36067977039915,34.9271834452265,30.));
#58988=CARTESIAN_POINT('Ctrl Pts',(-6.35502598487487,34.8301507851366,30.));
#58989=CARTESIAN_POINT('Ctrl Pts',(-6.35382226773603,34.8094920821356,30.));
#58990=CARTESIAN_POINT('Ctrl Pts',(-6.35279385607806,34.7888170008357,30.));
#58991=CARTESIAN_POINT('Ctrl Pts',(-6.35194202070525,34.7681330554352,30.));
#58992=CARTESIAN_POINT('Ctrl Pts',(-6.35128574764422,34.7521976803671,30.));
#58993=CARTESIAN_POINT('Ctrl Pts',(-6.35073447381912,34.7362615104886,30.));
#58994=CARTESIAN_POINT('Ctrl Pts',(-6.35028852693944,34.7203312537507,30.));
#58995=CARTESIAN_POINT('Ctrl Pts',(-6.34696763355239,34.6017012404777,30.));
#58996=CARTESIAN_POINT('Ctrl Pts',(-6.34947949264528,34.4832921867427,30.));
#58997=CARTESIAN_POINT('Ctrl Pts',(-6.3578907267476,34.3655323240003,30.));
#58998=CARTESIAN_POINT('Ctrl Pts',(-6.36625571653258,34.2484198959146,30.));
#58999=CARTESIAN_POINT('Ctrl Pts',(-6.38045508742067,34.1319486514061,30.));
#59000=CARTESIAN_POINT('Ctrl Pts',(-6.40060258265579,34.0165227778237,30.));
#59001=CARTESIAN_POINT('Ctrl Pts',(-6.40380809020162,33.998158286137,30.));
#59002=CARTESIAN_POINT('Ctrl Pts',(-6.40716427052324,33.9798202372895,30.));
#59003=CARTESIAN_POINT('Ctrl Pts',(-6.4106717030966,33.9615102423084,30.));
#59004=CARTESIAN_POINT('Ctrl Pts',(-6.43232586871275,33.8484681080808,30.));
#59005=CARTESIAN_POINT('Ctrl Pts',(-6.45974073675761,33.7364949627291,30.));
#59006=CARTESIAN_POINT('Ctrl Pts',(-6.49261497570932,33.6258527948074,30.));
#59007=CARTESIAN_POINT('Ctrl Pts',(-6.5133569109009,33.5560433406674,30.));
#59008=CARTESIAN_POINT('Ctrl Pts',(-6.53627330083344,33.4867637689423,30.));
#59009=CARTESIAN_POINT('Ctrl Pts',(-6.56129893452937,33.4180815844293,30.));
#59010=CARTESIAN_POINT('Ctrl Pts',(-6.56744615902576,33.4012106906796,30.));
#59011=CARTESIAN_POINT('Ctrl Pts',(-6.57372068647934,33.384375851465,30.));
#59012=CARTESIAN_POINT('Ctrl Pts',(-6.5801216201336,33.3675780879759,30.));
#59013=CARTESIAN_POINT('Ctrl Pts',(-6.58592025317676,33.3523609225308,30.));
#59014=CARTESIAN_POINT('Ctrl Pts',(-6.59182097681593,33.3371786053701,30.));
#59015=CARTESIAN_POINT('Ctrl Pts',(-6.59781984998277,33.3220394150435,30.));
#59016=CARTESIAN_POINT('Ctrl Pts',(-6.64115049854471,33.2126870554737,30.));
#59017=CARTESIAN_POINT('Ctrl Pts',(-6.68964292214754,33.1054651171024,30.));
#59018=CARTESIAN_POINT('Ctrl Pts',(-6.74292857838681,33.0006347052758,30.));
#59019=CARTESIAN_POINT('Ctrl Pts',(-6.7971983889184,32.8938681382613,30.));
#59020=CARTESIAN_POINT('Ctrl Pts',(-6.85644039141944,32.7895815913385,30.));
#59021=CARTESIAN_POINT('Ctrl Pts',(-6.92032038581974,32.6880544158277,30.));
#59022=CARTESIAN_POINT('Ctrl Pts',(-6.9852980783428,32.5847826222873,30.));
#59023=CARTESIAN_POINT('Ctrl Pts',(-7.05507485691378,32.484365082995,30.));
#59024=CARTESIAN_POINT('Ctrl Pts',(-7.12935095295689,32.3871103075363,30.));
#59025=CARTESIAN_POINT('Ctrl Pts',(-7.18304703332837,32.3168023549413,30.));
#59026=CARTESIAN_POINT('Ctrl Pts',(-7.23909566705282,32.2481475927666,30.));
#59027=CARTESIAN_POINT('Ctrl Pts',(-7.29739847574476,32.1812706915235,30.));
#59028=CARTESIAN_POINT('Ctrl Pts',(-7.31474064201097,32.1613781620425,30.));
#59029=CARTESIAN_POINT('Ctrl Pts',(-7.33228232709857,32.1416429873077,30.));
#59030=CARTESIAN_POINT('Ctrl Pts',(-7.35002113254827,32.1220685998336,30.));
#59031=CARTESIAN_POINT('Ctrl Pts',(-7.36801595625955,32.1022117017549,30.));
#59032=CARTESIAN_POINT('Ctrl Pts',(-7.38621564046034,32.0825183614633,30.));
#59033=CARTESIAN_POINT('Ctrl Pts',(-7.40459523086067,32.0630154735846,30.));
#59034=CARTESIAN_POINT('Ctrl Pts',(-7.49052313537484,31.971835950489,30.));
#59035=CARTESIAN_POINT('Ctrl Pts',(-7.58048269396152,31.884701382044,30.));
#59036=CARTESIAN_POINT('Ctrl Pts',(-7.6741413572269,31.8019256291752,30.));
#59037=CARTESIAN_POINT('Ctrl Pts',(-7.7679471631547,31.7190198312658,30.));
#59038=CARTESIAN_POINT('Ctrl Pts',(-7.86546422372204,31.6404857796622,30.));
#59039=CARTESIAN_POINT('Ctrl Pts',(-7.96640243919652,31.5666660266351,30.));
#59040=CARTESIAN_POINT('Ctrl Pts',(-7.99169676439379,31.5481673754526,30.));
#59041=CARTESIAN_POINT('Ctrl Pts',(-8.01720611984243,31.5299649311879,30.));
#59042=CARTESIAN_POINT('Ctrl Pts',(-8.04292631309347,31.512064441274,30.));
#59043=CARTESIAN_POINT('Ctrl Pts',(-8.06988678062553,31.4933007573303,30.));
#59044=CARTESIAN_POINT('Ctrl Pts',(-8.0970847011253,31.4748651824742,30.));
#59045=CARTESIAN_POINT('Ctrl Pts',(-8.12448495777706,31.4567841571235,30.));
#59046=CARTESIAN_POINT('Ctrl Pts',(-8.23136544948198,31.3862552965884,30.));
#59047=CARTESIAN_POINT('Ctrl Pts',(-8.34138288217212,31.3210724845241,30.));
#59048=CARTESIAN_POINT('Ctrl Pts',(-8.45421443341316,31.2615806352042,30.));
#59049=CARTESIAN_POINT('Ctrl Pts',(-8.56704598465418,31.2020887858843,30.));
#59050=CARTESIAN_POINT('Ctrl Pts',(-8.68269223981398,31.1482870733463,30.0000000000001));
#59051=CARTESIAN_POINT('Ctrl Pts',(-8.80086775832496,31.1005606444914,30.0000000000001));
#59052=CARTESIAN_POINT('Ctrl Pts',(-8.84648330399997,31.0821383255308,30.0000000000001));
#59053=CARTESIAN_POINT('Ctrl Pts',(-8.89247604481757,31.064621682834,30.));
#59054=CARTESIAN_POINT('Ctrl Pts',(-8.93882133655981,31.0480037218324,30.));
#59055=CARTESIAN_POINT('Ctrl Pts',(-11.0588859455903,31.0507007332205,29.9978118085731));
#59056=CARTESIAN_POINT('Ctrl Pts',(-12.3629832357829,31.4003552412704,29.932118657717));
#59057=CARTESIAN_POINT('Ctrl Pts',(-14.5759074258155,33.4867445316354,29.8007323560046));
#59058=CARTESIAN_POINT('Ctrl Pts',(-13.7737234475427,38.005501208821,29.6036529034362));
#59059=CARTESIAN_POINT('Ctrl Pts',(-9.55494358652074,39.7999145328719,29.4065734508678));
#59060=CARTESIAN_POINT('Ctrl Pts',(-5.74151403809183,37.2608171620003,29.2094939982993));
#59061=CARTESIAN_POINT('Ctrl Pts',(-5.77477638536515,32.6766638459004,29.0124145457309));
#59062=CARTESIAN_POINT('Ctrl Pts',(-9.62705490761888,30.1930581540609,28.8153350931624));
#59063=CARTESIAN_POINT('Ctrl Pts',(-13.8159539064568,32.0528472439456,28.618255640594));
#59064=CARTESIAN_POINT('Ctrl Pts',(-14.5566797841821,36.5761533733236,28.4211761880255));
#59065=CARTESIAN_POINT('Ctrl Pts',(-11.1795570301019,39.6750043826236,28.2240967354571));
#59066=CARTESIAN_POINT('Ctrl Pts',(-6.73655125706319,38.5492452105912,28.0270172828887));
#59067=CARTESIAN_POINT('Ctrl Pts',(-5.24261006855395,34.2160972081087,27.8299378303202));
#59068=CARTESIAN_POINT('Ctrl Pts',(-8.04780575158656,30.5913570973815,27.6328583777518));
#59069=CARTESIAN_POINT('Ctrl Pts',(-12.6171399548574,30.9505797199039,27.4357789251833));
#59070=CARTESIAN_POINT('Ctrl Pts',(-14.8214390660459,34.9691575849492,27.2386994726149));
#59071=CARTESIAN_POINT('Ctrl Pts',(-12.6687329951577,39.0156048483263,27.0416200200464));
#59072=CARTESIAN_POINT('Ctrl Pts',(-8.10436619426024,39.4332600799899,26.844540567478));
#59073=CARTESIAN_POINT('Ctrl Pts',(-5.25303178258637,35.8446980379474,26.6474611149096));
#59074=CARTESIAN_POINT('Ctrl Pts',(-6.69140385677929,31.4928055757625,26.4503816623411));
#59075=CARTESIAN_POINT('Ctrl Pts',(-11.1196643226323,30.3102693513275,26.2533022097727));
#59076=CARTESIAN_POINT('Ctrl Pts',(-14.5361145946286,33.3657154368998,26.0562227572043));
#59077=CARTESIAN_POINT('Ctrl Pts',(-13.8534012531181,37.8980200725724,25.8591433046358));
#59078=CARTESIAN_POINT('Ctrl Pts',(-9.68847384569797,39.8114626767306,25.6620638520674));
#59079=CARTESIAN_POINT('Ctrl Pts',(-5.80506415833992,37.3769170998905,25.4649843994989));
#59080=CARTESIAN_POINT('Ctrl Pts',(-5.71250408699149,32.7944160857802,25.2679049469305));
#59081=CARTESIAN_POINT('Ctrl Pts',(-9.49443764986189,30.2050413634305,25.070825494362));
#59082=CARTESIAN_POINT('Ctrl Pts',(-13.7332341815699,31.9487405618712,24.8737460417936));
#59083=CARTESIAN_POINT('Ctrl Pts',(-14.5984083535233,36.449780061507,24.6766665892252));
#59084=CARTESIAN_POINT('Ctrl Pts',(-11.3081257596992,39.6406926864939,24.4795871366567));
#59085=CARTESIAN_POINT('Ctrl Pts',(-6.83572543698307,38.6379373418252,24.2825076840883));
#59086=CARTESIAN_POINT('Ctrl Pts',(-5.22279411564314,34.347676804315,24.0854282315198));
#59087=CARTESIAN_POINT('Ctrl Pts',(-7.9268940338903,30.6469030258237,23.8883487789514));
#59088=CARTESIAN_POINT('Ctrl Pts',(-12.5044035215461,30.8799047808937,23.6912693263829));
#59089=CARTESIAN_POINT('Ctrl Pts',(-14.8187515502098,34.836124710266,23.4941898738145));
#59090=CARTESIAN_POINT('Ctrl Pts',(-12.7785246491449,38.9404342891812,23.297110421246));
#59091=CARTESIAN_POINT('Ctrl Pts',(-8.22742046944141,39.4838803977224,23.1000309686776));
#59092=CARTESIAN_POINT('Ctrl Pts',(-5.27814827968767,35.9753655441003,22.9029515161092));
#59093=CARTESIAN_POINT('Ctrl Pts',(-6.5958852745562,31.5854393328981,22.7058720635407));
#59094=CARTESIAN_POINT('Ctrl Pts',(-10.9898283130341,30.2811588791444,22.5087926109723));
#59095=CARTESIAN_POINT('Ctrl Pts',(-14.4892903823489,33.241167013002,22.3117131584039));
#59096=CARTESIAN_POINT('Ctrl Pts',(-13.9319026333332,37.7905847587297,22.1146337058354));
#59097=CARTESIAN_POINT('Ctrl Pts',(-9.82136123958291,39.8182268321212,21.917554253267));
#59098=CARTESIAN_POINT('Ctrl Pts',(-5.8722508431256,37.4917681495545,21.7204748006985));
#59099=CARTESIAN_POINT('Ctrl Pts',(-5.65327527635101,32.9135662500072,21.5233953481301));
#59100=CARTESIAN_POINT('Ctrl Pts',(-9.36231681406144,30.2208178773872,21.3263158955616));
#59101=CARTESIAN_POINT('Ctrl Pts',(-13.6476153301248,31.8468866149734,21.1292364429932));
#59102=CARTESIAN_POINT('Ctrl Pts',(-14.6366629208727,36.322338304894,20.9321569904247));
#59103=CARTESIAN_POINT('Ctrl Pts',(-11.435684126237,39.6028287659043,20.7350775378563));
#59104=CARTESIAN_POINT('Ctrl Pts',(-6.93731658184864,38.7238678721151,20.5379980852879));
#59105=CARTESIAN_POINT('Ctrl Pts',(-5.20661285740024,34.4797486630162,20.3409186327194));
#59106=CARTESIAN_POINT('Ctrl Pts',(-7.8075629807243,30.7057665311668,20.143839180151));
#59107=CARTESIAN_POINT('Ctrl Pts',(-12.3897588173874,30.8123664406772,19.9467597275825));
#59108=CARTESIAN_POINT('Ctrl Pts',(-14.8123946775176,34.7032173689442,19.7496802750141));
#59109=CARTESIAN_POINT('Ctrl Pts',(-12.886199790056,38.8622621440323,19.5526008224457));
#59110=CARTESIAN_POINT('Ctrl Pts',(-8.35182522203339,39.5310866051571,19.3555213698772));
#59111=CARTESIAN_POINT('Ctrl Pts',(-5.30686005482489,36.1052889229368,19.1584419173088));
#59112=CARTESIAN_POINT('Ctrl Pts',(-6.50296079309576,31.6806760610448,18.9613624647403));
#59113=CARTESIAN_POINT('Ctrl Pts',(-10.859235384841,30.2556373346469,18.7642830121719));
#59114=CARTESIAN_POINT('Ctrl Pts',(-14.4390532842977,33.1179677999974,18.5672035596034));
#59115=CARTESIAN_POINT('Ctrl Pts',(-14.007397374698,37.6810048575257,18.370124107035));
#59116=CARTESIAN_POINT('Ctrl Pts',(-9.95440886694127,39.8213599285263,18.1730446544665));
#59117=CARTESIAN_POINT('Ctrl Pts',(-5.94253301752884,37.6046449412306,17.9759652018981));
#59118=CARTESIAN_POINT('Ctrl Pts',(-5.59745277486287,33.0344578654708,17.7788857493297));
#59119=CARTESIAN_POINT('Ctrl Pts',(-9.23049066470893,30.2399305822798,17.5818062967612));
#59120=CARTESIAN_POINT('Ctrl Pts',(-13.5595988951335,31.7480386482111,17.3847268441928));
#59121=CARTESIAN_POINT('Ctrl Pts',(-14.670627205324,36.1926844691458,17.1876473916243));
#59122=CARTESIAN_POINT('Ctrl Pts',(-11.5636807183284,39.5638721263731,16.9905679390559));
#59123=CARTESIAN_POINT('Ctrl Pts',(-7.03690372967489,38.8018166892409,16.7934427493524));
#59124=CARTESIAN_POINT('Ctrl Pts',(-5.81501543623371,36.0149950038524,16.6620107105051));
#59125=CARTESIAN_POINT('Ctrl Pts',(-5.92468352323803,34.6683388238581,16.5962718225139));
#59126=CARTESIAN_POINT('Ctrl Pts',(-10.9980261816851,31.2776878057835,30.1334916301794));
#59127=CARTESIAN_POINT('Ctrl Pts',(-12.227170117816,31.6072458238412,30.0677984793232));
#59128=CARTESIAN_POINT('Ctrl Pts',(-14.312905875226,33.5737193100963,29.9364121776109));
#59129=CARTESIAN_POINT('Ctrl Pts',(-13.5568276439693,37.8327591918477,29.7393327250425));
#59130=CARTESIAN_POINT('Ctrl Pts',(-9.58052332753221,39.5240381115701,29.5422532724741));
#59131=CARTESIAN_POINT('Ctrl Pts',(-5.98627170185645,37.1308760675081,29.3451738199056));
#59132=CARTESIAN_POINT('Ctrl Pts',(-6.01762228647917,32.8101982368328,29.1480943673372));
#59133=CARTESIAN_POINT('Ctrl Pts',(-9.6484900304161,30.4693384721336,28.9510149147687));
#59134=CARTESIAN_POINT('Ctrl Pts',(-13.5966308955247,32.2222356673857,28.7539354622003));
#59135=CARTESIAN_POINT('Ctrl Pts',(-14.2947833476373,36.4855635203007,28.5568560096318));
#59136=CARTESIAN_POINT('Ctrl Pts',(-11.111761662089,39.4063072069101,28.3597765570634));
#59137=CARTESIAN_POINT('Ctrl Pts',(-6.92411888022353,38.3452513560518,28.162697104495));
#59138=CARTESIAN_POINT('Ctrl Pts',(-5.51604237657456,34.2611522388586,27.9656176519265));
#59139=CARTESIAN_POINT('Ctrl Pts',(-8.16000865837793,30.8447450730304,27.7685381993581));
#59140=CARTESIAN_POINT('Ctrl Pts',(-12.4667191088512,31.1833212755231,27.5714587467896));
#59141=CARTESIAN_POINT('Ctrl Pts',(-14.5443255162198,34.9709302613231,27.3743792942212));
#59142=CARTESIAN_POINT('Ctrl Pts',(-12.5153468248265,38.7848068440426,27.1772998416527));
#59143=CARTESIAN_POINT('Ctrl Pts',(-8.21331827389517,39.1784572252324,26.9802203890843));
#59144=CARTESIAN_POINT('Ctrl Pts',(-5.5258650996976,35.7961487835401,26.7831409365158));
#59145=CARTESIAN_POINT('Ctrl Pts',(-6.88156633931391,31.6943825496736,26.5860614839474));
#59146=CARTESIAN_POINT('Ctrl Pts',(-11.0553113046209,30.5798129232734,26.388982031379));
#59147=CARTESIAN_POINT('Ctrl Pts',(-14.2754001480669,33.4596463962052,26.1919025788106));
#59148=CARTESIAN_POINT('Ctrl Pts',(-13.6319259455329,37.7314555637656,25.9948231262421));
#59149=CARTESIAN_POINT('Ctrl Pts',(-9.70637889796551,39.5349225226521,25.7977436736737));
#59150=CARTESIAN_POINT('Ctrl Pts',(-6.0461692612876,37.2403031292128,25.6006642211052));
#59151=CARTESIAN_POINT('Ctrl Pts',(-5.9589291057552,32.9211826340111,25.4035847685368));
#59152=CARTESIAN_POINT('Ctrl Pts',(-9.52349498639276,30.4806329432155,25.2065053159683));
#59153=CARTESIAN_POINT('Ctrl Pts',(-13.5186655098071,32.1241125457867,25.0094258633998));
#59154=CARTESIAN_POINT('Ctrl Pts',(-14.3341135558625,36.3664535496901,24.8123464108315));
#59155=CARTESIAN_POINT('Ctrl Pts',(-11.2329408682335,39.373967585048,24.615266958263));
#59156=CARTESIAN_POINT('Ctrl Pts',(-7.01759299659966,38.4288458824024,24.4181875056946));
#59157=CARTESIAN_POINT('Ctrl Pts',(-5.49736535106264,34.3851692612172,24.2211080531261));
#59158=CARTESIAN_POINT('Ctrl Pts',(-8.04604637524828,30.8970984838035,24.0240286005577));
#59159=CARTESIAN_POINT('Ctrl Pts',(-12.3604622333652,31.1167083982678,23.8269491479892));
#59160=CARTESIAN_POINT('Ctrl Pts',(-14.5417924661031,34.8455434880719,23.6298696954208));
#59161=CARTESIAN_POINT('Ctrl Pts',(-12.6188281729981,38.7139567336685,23.4327902428523));
#59162=CARTESIAN_POINT('Ctrl Pts',(-8.32929997042302,39.2261681261397,23.2357107902839));
#59163=CARTESIAN_POINT('Ctrl Pts',(-5.54953801915008,35.9193061384744,23.0386313377155));
#59164=CARTESIAN_POINT('Ctrl Pts',(-6.7915377141413,31.7816921558822,22.841551885147));
#59165=CARTESIAN_POINT('Ctrl Pts',(-10.9329376557458,30.5523755835666,22.6444724325786));
#59166=CARTESIAN_POINT('Ctrl Pts',(-14.2312671703968,33.3422564275734,22.4473929800101));
#59167=CARTESIAN_POINT('Ctrl Pts',(-13.7059154371107,37.6301951244339,22.2503135274417));
#59168=CARTESIAN_POINT('Ctrl Pts',(-9.83162855196778,39.5412979063323,22.0532340748733));
#59169=CARTESIAN_POINT('Ctrl Pts',(-6.10949437269923,37.3485530828893,21.8561546223048));
#59170=CARTESIAN_POINT('Ctrl Pts',(-5.9031044874614,33.0334846094467,21.6590751697364));
#59171=CARTESIAN_POINT('Ctrl Pts',(-9.3989678323361,30.4955026976495,21.4619957171679));
#59172=CARTESIAN_POINT('Ctrl Pts',(-13.4379676256357,32.0281126827842,21.2649162645995));
#59173=CARTESIAN_POINT('Ctrl Pts',(-14.3701694313254,36.2463365434447,21.067836812031));
#59174=CARTESIAN_POINT('Ctrl Pts',(-11.3531677822158,39.3382799038139,20.8707573594626));
#59175=CARTESIAN_POINT('Ctrl Pts',(-7.11334516218977,38.5098375315904,20.6736779068942));
#59176=CARTESIAN_POINT('Ctrl Pts',(-5.48211411513276,34.509650253147,20.4765984543257));
#59177=CARTESIAN_POINT('Ctrl Pts',(-7.93357390751589,30.9525787928234,20.2795190017573));
#59178=CARTESIAN_POINT('Ctrl Pts',(-12.2524067654289,31.0530518429187,20.0824395491888));
#59179=CARTESIAN_POINT('Ctrl Pts',(-14.5358009564349,34.7202750331171,19.8853600966204));
#59180=CARTESIAN_POINT('Ctrl Pts',(-12.7203146552709,38.6402775542801,19.6882806440519));
#59181=CARTESIAN_POINT('Ctrl Pts',(-8.44655452529733,39.2706611436872,19.4912011914835));
#59182=CARTESIAN_POINT('Ctrl Pts',(-5.57659957703449,36.0417621350167,19.2941217389151));
#59183=CARTESIAN_POINT('Ctrl Pts',(-6.70395409306934,31.8714551266196,19.0970422863466));
#59184=CARTESIAN_POINT('Ctrl Pts',(-10.8098505923823,30.5283208969295,18.8999628337782));
#59185=CARTESIAN_POINT('Ctrl Pts',(-14.1839174635131,33.2261381235637,18.7028833812097));
#59186=CARTESIAN_POINT('Ctrl Pts',(-13.7770710972414,37.5269133584954,18.5058039286413));
#59187=CARTESIAN_POINT('Ctrl Pts',(-9.95702922998006,39.5442509271512,18.3087244760728));
#59188=CARTESIAN_POINT('Ctrl Pts',(-6.17573705960266,37.4549422496039,18.1116450235044));
#59189=CARTESIAN_POINT('Ctrl Pts',(-5.85049039975504,33.1474279457251,17.914565570936));
#59190=CARTESIAN_POINT('Ctrl Pts',(-9.27471842754193,30.5135168945186,17.7174861183675));
#59191=CARTESIAN_POINT('Ctrl Pts',(-13.3550099596984,31.9349460303737,17.5204066657991));
#59192=CARTESIAN_POINT('Ctrl Pts',(-14.4021816090919,36.1241345979269,17.3233272132306));
#59193=CARTESIAN_POINT('Ctrl Pts',(-11.4738077346166,39.3015623079627,17.1262477606622));
#59194=CARTESIAN_POINT('Ctrl Pts',(-7.20720851102714,38.583306218796,16.9291225709587));
#59195=CARTESIAN_POINT('Ctrl Pts',(-6.05554858671976,35.9566578840173,16.7976905321114));
#59196=CARTESIAN_POINT('Ctrl Pts',(-6.15891346995523,34.6874011421,16.7319516441202));
#59197=CARTESIAN_POINT('Ctrl Pts',(-10.9371664177797,31.5046748783465,30.2691714517856));
#59198=CARTESIAN_POINT('Ctrl Pts',(-12.0913569998491,31.8141364064121,30.2034783009294));
#59199=CARTESIAN_POINT('Ctrl Pts',(-14.0499043246364,33.6606940885572,30.0720919992171));
#59200=CARTESIAN_POINT('Ctrl Pts',(-13.3399318403958,37.6600171748744,29.8750125466487));
#59201=CARTESIAN_POINT('Ctrl Pts',(-9.60610306854369,39.2481616902682,29.6779330940803));
#59202=CARTESIAN_POINT('Ctrl Pts',(-6.23102936562104,37.0009349730159,29.4808536415118));
#59203=CARTESIAN_POINT('Ctrl Pts',(-6.2604681875932,32.943732627765,29.2837741889434));
#59204=CARTESIAN_POINT('Ctrl Pts',(-9.6699251532133,30.7456187902063,29.0866947363749));
#59205=CARTESIAN_POINT('Ctrl Pts',(-13.3773078845926,32.3916240908258,28.8896152838065));
#59206=CARTESIAN_POINT('Ctrl Pts',(-14.0328869110925,36.3949736672779,28.6925358312381));
#59207=CARTESIAN_POINT('Ctrl Pts',(-11.0439662940763,39.1376100311967,28.4954563786696));
#59208=CARTESIAN_POINT('Ctrl Pts',(-7.11168650338384,38.1412575015122,28.2983769261012));
#59209=CARTESIAN_POINT('Ctrl Pts',(-5.78947468459519,34.3062072696085,28.1012974735327));
#59210=CARTESIAN_POINT('Ctrl Pts',(-8.27221156516931,31.0981330486793,27.9042180209643));
#59211=CARTESIAN_POINT('Ctrl Pts',(-12.316298262845,31.4160628311424,27.7071385683959));
#59212=CARTESIAN_POINT('Ctrl Pts',(-14.2672119663938,34.9727029376968,27.5100591158274));
#59213=CARTESIAN_POINT('Ctrl Pts',(-12.3619606544954,38.5540088397591,27.312979663259));
#59214=CARTESIAN_POINT('Ctrl Pts',(-8.32227035353011,38.9236543704749,27.1159002106905));
#59215=CARTESIAN_POINT('Ctrl Pts',(-5.7986984168088,35.7475995291328,26.9188207581221));
#59216=CARTESIAN_POINT('Ctrl Pts',(-7.07172882184853,31.8959595235848,26.7217413055536));
#59217=CARTESIAN_POINT('Ctrl Pts',(-10.9909582866094,30.8493564952194,26.5246618529852));
#59218=CARTESIAN_POINT('Ctrl Pts',(-14.0146857015052,33.5535773555107,26.3275824004167));
#59219=CARTESIAN_POINT('Ctrl Pts',(-13.4104506379478,37.5648910549589,26.1305029478483));
#59220=CARTESIAN_POINT('Ctrl Pts',(-9.72428395023304,39.2583823685737,25.9334234952798));
#59221=CARTESIAN_POINT('Ctrl Pts',(-6.28727436423529,37.1036891585352,25.7363440427114));
#59222=CARTESIAN_POINT('Ctrl Pts',(-6.20535412451891,33.0479491822421,25.539264590143));
#59223=CARTESIAN_POINT('Ctrl Pts',(-9.55255232292363,30.7562245230005,25.3421851375745));
#59224=CARTESIAN_POINT('Ctrl Pts',(-13.3040968380443,32.2994845297022,25.1451056850062));
#59225=CARTESIAN_POINT('Ctrl Pts',(-14.0698187582016,36.2831270378733,24.9480262324377));
#59226=CARTESIAN_POINT('Ctrl Pts',(-11.1577559767678,39.1072424836022,24.7509467798692));
#59227=CARTESIAN_POINT('Ctrl Pts',(-7.19946055621625,38.2197544229795,24.5538673273008));
#59228=CARTESIAN_POINT('Ctrl Pts',(-5.77193658648213,34.4226617181194,24.3567878747323));
#59229=CARTESIAN_POINT('Ctrl Pts',(-8.16519871660625,31.1472939417833,24.1597084221639));
#59230=CARTESIAN_POINT('Ctrl Pts',(-12.2165209451842,31.3535120156418,23.9626289695954));
#59231=CARTESIAN_POINT('Ctrl Pts',(-14.2648333819964,34.8549622658775,23.765549517027));
#59232=CARTESIAN_POINT('Ctrl Pts',(-12.4591316968514,38.4874791781558,23.5684700644586));
#59233=CARTESIAN_POINT('Ctrl Pts',(-8.43117947140467,38.968455854557,23.3713906118901));
#59234=CARTESIAN_POINT('Ctrl Pts',(-5.82092775861246,35.8632467328487,23.1743111593217));
#59235=CARTESIAN_POINT('Ctrl Pts',(-6.98719015372643,31.9779449788662,22.9772317067532));
#59236=CARTESIAN_POINT('Ctrl Pts',(-10.8760469984575,30.8235922879887,22.7801522541848));
#59237=CARTESIAN_POINT('Ctrl Pts',(-13.9732439584446,33.4433458421448,22.5830728016163));
#59238=CARTESIAN_POINT('Ctrl Pts',(-13.4799282408882,37.4698054901383,22.3859933490479));
#59239=CARTESIAN_POINT('Ctrl Pts',(-9.84189586435265,39.2643689805436,22.1889138964794));
#59240=CARTESIAN_POINT('Ctrl Pts',(-6.34673790227287,37.205338016224,21.991834443911));
#59241=CARTESIAN_POINT('Ctrl Pts',(-6.15293369857177,33.1534029688861,21.7947549913426));
#59242=CARTESIAN_POINT('Ctrl Pts',(-9.43561885061076,30.7701875179118,21.5976755387741));
#59243=CARTESIAN_POINT('Ctrl Pts',(-13.2283199211465,32.2093387505949,21.4005960862057));
#59244=CARTESIAN_POINT('Ctrl Pts',(-14.1036759417782,36.1703347819953,21.2035166336372));
#59245=CARTESIAN_POINT('Ctrl Pts',(-11.2706514381948,39.0737310417233,21.0064371810688));
#59246=CARTESIAN_POINT('Ctrl Pts',(-7.2893737425309,38.2958071910657,20.8093577285003));
#59247=CARTESIAN_POINT('Ctrl Pts',(-5.75761537286527,34.5395518432776,20.6122782759319));
#59248=CARTESIAN_POINT('Ctrl Pts',(-8.05958483430744,31.19939105448,20.4151988233635));
#59249=CARTESIAN_POINT('Ctrl Pts',(-12.1150547134704,31.2937372451604,20.218119370795));
#59250=CARTESIAN_POINT('Ctrl Pts',(-14.2592072353523,34.7373326972899,20.0210399182266));
#59251=CARTESIAN_POINT('Ctrl Pts',(-12.5544295204857,38.4182929645279,19.8239604656581));
#59252=CARTESIAN_POINT('Ctrl Pts',(-8.54128382856128,39.0102356822172,19.6268810130897));
#59253=CARTESIAN_POINT('Ctrl Pts',(-5.84633909924408,35.9782353470966,19.4298015605213));
#59254=CARTESIAN_POINT('Ctrl Pts',(-6.90494739304291,32.0622341921945,19.2327221079528));
#59255=CARTESIAN_POINT('Ctrl Pts',(-10.7604657999234,30.8010044592122,19.0356426553844));
#59256=CARTESIAN_POINT('Ctrl Pts',(-13.9287816427284,33.3343084471301,18.8385632028159));
#59257=CARTESIAN_POINT('Ctrl Pts',(-13.5467448197848,37.3728218594653,18.6414837502475));
#59258=CARTESIAN_POINT('Ctrl Pts',(-9.95964959301886,39.2671419257761,18.444404297679));
#59259=CARTESIAN_POINT('Ctrl Pts',(-6.40894110167649,37.3052395579773,18.2473248451106));
#59260=CARTESIAN_POINT('Ctrl Pts',(-6.10352802464721,33.2603980259793,18.0502453925421));
#59261=CARTESIAN_POINT('Ctrl Pts',(-9.31894619037493,30.7871032067572,17.8531659399737));
#59262=CARTESIAN_POINT('Ctrl Pts',(-13.1504210242633,32.1218534125364,17.6560864874053));
#59263=CARTESIAN_POINT('Ctrl Pts',(-14.1337360128598,36.0555847267079,17.4590070348368));
#59264=CARTESIAN_POINT('Ctrl Pts',(-11.3839347509046,39.0392524895524,17.2619275822684));
#59265=CARTESIAN_POINT('Ctrl Pts',(-7.3775132923794,38.3647957483509,17.064802392565));
#59266=CARTESIAN_POINT('Ctrl Pts',(-6.2960817372058,35.8983207641823,16.9333703537176));
#59267=CARTESIAN_POINT('Ctrl Pts',(-6.39314341667241,34.7064634603417,16.8676314657265));
#59268=CARTESIAN_POINT('Ctrl Pts',(-10.8763066538745,31.7316619509095,30.4048512733919));
#59269=CARTESIAN_POINT('Ctrl Pts',(-11.9555438818821,32.021026988983,30.3391581225357));
#59270=CARTESIAN_POINT('Ctrl Pts',(-13.7869027740469,33.7476688670181,30.2077718208234));
#59271=CARTESIAN_POINT('Ctrl Pts',(-13.1230360368224,37.487275157901,30.010692368255));
#59272=CARTESIAN_POINT('Ctrl Pts',(-9.63168280955517,38.9722852689663,29.8136129156865));
#59273=CARTESIAN_POINT('Ctrl Pts',(-6.47578702938564,36.8709938785236,29.6165334631181));
#59274=CARTESIAN_POINT('Ctrl Pts',(-6.50331408870724,33.0772670186974,29.4194540105497));
#59275=CARTESIAN_POINT('Ctrl Pts',(-9.6913602760105,31.0218991082791,29.2223745579812));
#59276=CARTESIAN_POINT('Ctrl Pts',(-13.1579848736605,32.5610125142658,29.0252951054128));
#59277=CARTESIAN_POINT('Ctrl Pts',(-13.7709904745478,36.3043838142549,28.8282156528444));
#59278=CARTESIAN_POINT('Ctrl Pts',(-10.9761709260635,38.8689128554832,28.6311362002759));
#59279=CARTESIAN_POINT('Ctrl Pts',(-7.29925412654417,37.9372636469728,28.4340567477075));
#59280=CARTESIAN_POINT('Ctrl Pts',(-6.0629069926158,34.3512623003585,28.236977295139));
#59281=CARTESIAN_POINT('Ctrl Pts',(-8.38441447196068,31.3515210243283,28.0398978425706));
#59282=CARTESIAN_POINT('Ctrl Pts',(-12.1658774168387,31.6488043867616,27.8428183900021));
#59283=CARTESIAN_POINT('Ctrl Pts',(-13.9900984165678,34.9744756140705,27.6457389374337));
#59284=CARTESIAN_POINT('Ctrl Pts',(-12.2085744841641,38.3232108354754,27.4486594848652));
#59285=CARTESIAN_POINT('Ctrl Pts',(-8.43122243316505,38.6688515157174,27.2515800322968));
#59286=CARTESIAN_POINT('Ctrl Pts',(-6.07153173392002,35.6990502747255,27.0545005797284));
#59287=CARTESIAN_POINT('Ctrl Pts',(-7.26189130438314,32.097536497496,26.8574211271599));
#59288=CARTESIAN_POINT('Ctrl Pts',(-10.9266052685981,31.1189000671652,26.6603416745915));
#59289=CARTESIAN_POINT('Ctrl Pts',(-13.7539712549434,33.6475083148162,26.463262222023));
#59290=CARTESIAN_POINT('Ctrl Pts',(-13.1889753303626,37.398326546152,26.2661827694546));
#59291=CARTESIAN_POINT('Ctrl Pts',(-9.74218900250058,38.9818422144952,26.0691033168861));
#59292=CARTESIAN_POINT('Ctrl Pts',(-6.52837946718296,36.9670751878574,25.8720238643177));
#59293=CARTESIAN_POINT('Ctrl Pts',(-6.45177914328262,33.1747157304732,25.6749444117493));
#59294=CARTESIAN_POINT('Ctrl Pts',(-9.58160965945451,31.0318161027855,25.4778649591808));
#59295=CARTESIAN_POINT('Ctrl Pts',(-13.0895281662815,32.4748565136177,25.2807855066124));
#59296=CARTESIAN_POINT('Ctrl Pts',(-13.8055239605408,36.1998005260564,25.0837060540439));
#59297=CARTESIAN_POINT('Ctrl Pts',(-11.0825710853022,38.8405173821563,24.8866266014755));
#59298=CARTESIAN_POINT('Ctrl Pts',(-7.38132811583285,38.0106629635567,24.6895471489071));
#59299=CARTESIAN_POINT('Ctrl Pts',(-6.04650782190161,34.4601541750215,24.4924676963386));
#59300=CARTESIAN_POINT('Ctrl Pts',(-8.28435105796425,31.3974893997631,24.2953882437702));
#59301=CARTESIAN_POINT('Ctrl Pts',(-12.0725796570033,31.5903156330156,24.0983087912017));
#59302=CARTESIAN_POINT('Ctrl Pts',(-13.9878742978896,34.8643810436833,23.9012293386333));
#59303=CARTESIAN_POINT('Ctrl Pts',(-12.2994352207047,38.2610016226431,23.7041498860648));
#59304=CARTESIAN_POINT('Ctrl Pts',(-8.53305897238628,38.7107435829743,23.5070704334964));
#59305=CARTESIAN_POINT('Ctrl Pts',(-6.09231749807485,35.8071873272227,23.309990980928));
#59306=CARTESIAN_POINT('Ctrl Pts',(-7.18284259331154,32.1741978018502,23.1129115283595));
#59307=CARTESIAN_POINT('Ctrl Pts',(-10.819156341169,31.0948089924109,22.9158320757911));
#59308=CARTESIAN_POINT('Ctrl Pts',(-13.7152207464925,33.5444352567162,22.7187526232226));
#59309=CARTESIAN_POINT('Ctrl Pts',(-13.2539410446657,37.3094158558426,22.5216731706542));
#59310=CARTESIAN_POINT('Ctrl Pts',(-9.85216317673751,38.9874400547548,22.3245937180858));
#59311=CARTESIAN_POINT('Ctrl Pts',(-6.5839814318465,37.0621229495586,22.1275142655173));
#59312=CARTESIAN_POINT('Ctrl Pts',(-6.40276290968217,33.2733213283256,21.9304348129489));
#59313=CARTESIAN_POINT('Ctrl Pts',(-9.47226986888541,31.0448723381741,21.7333553603804));
#59314=CARTESIAN_POINT('Ctrl Pts',(-13.0186722166574,32.3905648184057,21.536275907812));
#59315=CARTESIAN_POINT('Ctrl Pts',(-13.8371824522311,36.094333020546,21.3391964552435));
#59316=CARTESIAN_POINT('Ctrl Pts',(-11.1881350941738,38.8091821796328,21.1421170026751));
#59317=CARTESIAN_POINT('Ctrl Pts',(-7.46540232287201,38.081776850541,20.9450375501066));
#59318=CARTESIAN_POINT('Ctrl Pts',(-6.0331166305978,34.5694534334084,20.7479580975382));
#59319=CARTESIAN_POINT('Ctrl Pts',(-8.185595761099,31.4462033161365,20.5508786449698));
#59320=CARTESIAN_POINT('Ctrl Pts',(-11.9777026615119,31.534422647402,20.3537991924013));
#59321=CARTESIAN_POINT('Ctrl Pts',(-13.9826135142697,34.7543903614628,20.1567197398329));
#59322=CARTESIAN_POINT('Ctrl Pts',(-12.3885443857005,38.1963083747756,19.9596402872644));
#59323=CARTESIAN_POINT('Ctrl Pts',(-8.63601313182522,38.7498102207472,19.762560834696));
#59324=CARTESIAN_POINT('Ctrl Pts',(-6.11607862145368,35.9147085591765,19.5654813821276));
#59325=CARTESIAN_POINT('Ctrl Pts',(-7.1059406930165,32.2530132577694,19.3684019295591));
#59326=CARTESIAN_POINT('Ctrl Pts',(-10.7110810074646,31.0736880214948,19.1713224769907));
#59327=CARTESIAN_POINT('Ctrl Pts',(-13.6736458219438,33.4424787706964,18.9742430244222));
#59328=CARTESIAN_POINT('Ctrl Pts',(-13.3164185423282,37.218730360435,18.7771635718538));
#59329=CARTESIAN_POINT('Ctrl Pts',(-9.96226995605767,38.990032924401,18.5800841192853));
#59330=CARTESIAN_POINT('Ctrl Pts',(-6.64214514375032,37.1555368663507,18.3830046667169));
#59331=CARTESIAN_POINT('Ctrl Pts',(-6.35656564953937,33.3733681062335,18.1859252141485));
#59332=CARTESIAN_POINT('Ctrl Pts',(-9.36317395320792,31.0606895189958,17.98884576158));
#59333=CARTESIAN_POINT('Ctrl Pts',(-12.9458320888283,32.308760794699,17.7917663090116));
#59334=CARTESIAN_POINT('Ctrl Pts',(-13.8652904166277,35.987034855489,17.5946868564431));
#59335=CARTESIAN_POINT('Ctrl Pts',(-11.2940617671928,38.776942671142,17.3976074038747));
#59336=CARTESIAN_POINT('Ctrl Pts',(-7.54781807373163,38.146285277906,17.2004822141713));
#59337=CARTESIAN_POINT('Ctrl Pts',(-6.53661488769183,35.8399836443472,17.0690501753239));
#59338=CARTESIAN_POINT('Ctrl Pts',(-6.62737336338959,34.7255257785834,17.0033112873327));
#59339=CARTESIAN_POINT('',(-12.5757516043532,37.208058672647,30.0016980799398));
#59340=CARTESIAN_POINT('Ctrl Pts',(-12.5735559834512,37.206176480371,30.0016980799398));
#59341=CARTESIAN_POINT('Ctrl Pts',(-12.5615840841705,37.2201419782817,30.0011320532932));
#59342=CARTESIAN_POINT('Ctrl Pts',(-12.5494985059473,37.2340100250842,30.0005660266466));
#59343=CARTESIAN_POINT('Ctrl Pts',(-12.5373008502128,37.2477787831567,30.));
#59344=CARTESIAN_POINT('Ctrl Pts',(-11.0579044229731,31.0543614925016,30.));
#59345=CARTESIAN_POINT('Ctrl Pts',(-11.1744097379893,31.0963766655822,30.));
#59346=CARTESIAN_POINT('Ctrl Pts',(-11.2885141402515,31.1440012484697,30.));
#59347=CARTESIAN_POINT('Ctrl Pts',(-11.3999877282899,31.1968709585829,30.));
#59348=CARTESIAN_POINT('Ctrl Pts',(-11.5131045963172,31.2505200437767,30.));
#59349=CARTESIAN_POINT('Ctrl Pts',(-11.6235131197498,31.3095706523587,30.));
#59350=CARTESIAN_POINT('Ctrl Pts',(-11.7309453563639,31.3736894626584,30.));
#59351=CARTESIAN_POINT('Ctrl Pts',(-11.8388145215838,31.4380690451737,30.));
#59352=CARTESIAN_POINT('Ctrl Pts',(-11.94368371586,31.507558840894,30.));
#59353=CARTESIAN_POINT('Ctrl Pts',(-12.045245115667,31.5818586971976,30.));
#59354=CARTESIAN_POINT('Ctrl Pts',(-12.141528578336,31.6522973427294,30.));
#59355=CARTESIAN_POINT('Ctrl Pts',(-12.2348392296536,31.7270598973032,30.));
#59356=CARTESIAN_POINT('Ctrl Pts',(-12.3248775992634,31.8059127430533,30.));
#59357=CARTESIAN_POINT('Ctrl Pts',(-12.3423428346842,31.8212082611818,30.));
#59358=CARTESIAN_POINT('Ctrl Pts',(-12.3596848250068,31.8366577328144,30.));
#59359=CARTESIAN_POINT('Ctrl Pts',(-12.3769012054219,31.8522595191162,30.));
#59360=CARTESIAN_POINT('Ctrl Pts',(-12.3882150003473,31.8625122787807,30.));
#59361=CARTESIAN_POINT('Ctrl Pts',(-12.399472582474,31.8728290762095,30.));
#59362=CARTESIAN_POINT('Ctrl Pts',(-12.4106671396558,31.8832035231787,30.));
#59363=CARTESIAN_POINT('Ctrl Pts',(-12.5011175434017,31.9670275549618,30.));
#59364=CARTESIAN_POINT('Ctrl Pts',(-12.587577051358,32.0547210466236,30.));
#59365=CARTESIAN_POINT('Ctrl Pts',(-12.6697884900426,32.1459687647768,30.));
#59366=CARTESIAN_POINT('Ctrl Pts',(-12.7516103599846,32.2367840946956,30.));
#59367=CARTESIAN_POINT('Ctrl Pts',(-12.8292247934612,32.3311207836379,30.));
#59368=CARTESIAN_POINT('Ctrl Pts',(-12.9023358107026,32.428696821173,30.));
#59369=CARTESIAN_POINT('Ctrl Pts',(-12.9737773812525,32.5240447677968,30.));
#59370=CARTESIAN_POINT('Ctrl Pts',(-13.0409191293949,32.6224865141385,30.));
#59371=CARTESIAN_POINT('Ctrl Pts',(-13.1034390161676,32.7237758029549,30.));
#59372=CARTESIAN_POINT('Ctrl Pts',(-13.1564936425993,32.8097302993092,30.));
#59373=CARTESIAN_POINT('Ctrl Pts',(-13.2062193154101,32.8977358680952,30.));
#59374=CARTESIAN_POINT('Ctrl Pts',(-13.2523900459045,32.9876465015809,30.));
#59375=CARTESIAN_POINT('Ctrl Pts',(-13.2633342592225,33.0089587299534,30.));
#59376=CARTESIAN_POINT('Ctrl Pts',(-13.2740786046814,33.0303780053924,30.));
#59377=CARTESIAN_POINT('Ctrl Pts',(-13.284619831996,33.0519023903029,30.));
#59378=CARTESIAN_POINT('Ctrl Pts',(-13.2922709150539,33.0675253203285,30.));
#59379=CARTESIAN_POINT('Ctrl Pts',(-13.2998110412698,33.0831956068833,30.));
#59380=CARTESIAN_POINT('Ctrl Pts',(-13.3072375789992,33.0989086300593,30.));
#59381=CARTESIAN_POINT('Ctrl Pts',(-13.3571203304174,33.2044502508889,30.));
#59382=CARTESIAN_POINT('Ctrl Pts',(-13.4019091124834,33.3119732815046,30.));
#59383=CARTESIAN_POINT('Ctrl Pts',(-13.4413385699665,33.4212276569007,30.));
#59384=CARTESIAN_POINT('Ctrl Pts',(-13.480554760447,33.5298910945909,30.));
#59385=CARTESIAN_POINT('Ctrl Pts',(-13.5144697968334,33.6402678129294,30.));
#59386=CARTESIAN_POINT('Ctrl Pts',(-13.5427725767595,33.752122444386,30.));
#59387=CARTESIAN_POINT('Ctrl Pts',(-13.5490249649288,33.7768323342352,30.));
#59388=CARTESIAN_POINT('Ctrl Pts',(-13.5550032600854,33.8016143697398,30.));
#59389=CARTESIAN_POINT('Ctrl Pts',(-13.5607037501708,33.8264660384264,30.));
#59390=CARTESIAN_POINT('Ctrl Pts',(-13.5872170560123,33.9420525726855,30.));
#59391=CARTESIAN_POINT('Ctrl Pts',(-13.6077248602857,34.0591462330772,30.));
#59392=CARTESIAN_POINT('Ctrl Pts',(-13.6223138164184,34.1773085476865,30.));
#59393=CARTESIAN_POINT('Ctrl Pts',(-13.6304389010778,34.2431171498245,30.));
#59394=CARTESIAN_POINT('Ctrl Pts',(-13.6367271752067,34.3092570719329,30.));
#59395=CARTESIAN_POINT('Ctrl Pts',(-13.6411869466529,34.3756503989149,30.));
#59396=CARTESIAN_POINT('Ctrl Pts',(-13.6425504665288,34.3959493362173,30.));
#59397=CARTESIAN_POINT('Ctrl Pts',(-13.6437430339725,34.4162719455193,30.));
#59398=CARTESIAN_POINT('Ctrl Pts',(-13.6447648023415,34.4366159566223,30.));
#59399=CARTESIAN_POINT('Ctrl Pts',(-13.6454921557764,34.4510979926728,30.));
#59400=CARTESIAN_POINT('Ctrl Pts',(-13.6461328377877,34.4655892371793,30.));
#59401=CARTESIAN_POINT('Ctrl Pts',(-13.6466867036911,34.4800794533411,30.));
#59402=CARTESIAN_POINT('Ctrl Pts',(-13.6511188462219,34.5960329773438,30.));
#59403=CARTESIAN_POINT('Ctrl Pts',(-13.6500050144421,34.7120892190283,30.));
#59404=CARTESIAN_POINT('Ctrl Pts',(-13.6434929003203,34.8278444120361,30.));
#59405=CARTESIAN_POINT('Ctrl Pts',(-13.6369460662828,34.9442167641516,30.));
#59406=CARTESIAN_POINT('Ctrl Pts',(-13.6249429285982,35.0602857712229,30.));
#59407=CARTESIAN_POINT('Ctrl Pts',(-13.6075815295661,35.1756316950981,30.));
#59408=CARTESIAN_POINT('Ctrl Pts',(-13.5904443779721,35.2894877604727,30.));
#59409=CARTESIAN_POINT('Ctrl Pts',(-13.5680860708864,35.4026401113781,30.));
#59410=CARTESIAN_POINT('Ctrl Pts',(-13.5405559702548,35.514663028091,30.));
#59411=CARTESIAN_POINT('Ctrl Pts',(-13.5211239632378,35.5937339378838,30.));
#59412=CARTESIAN_POINT('Ctrl Pts',(-13.4991143380556,35.6722417044066,30.));
#59413=CARTESIAN_POINT('Ctrl Pts',(-13.4745323439232,35.7500266063154,30.));
#59414=CARTESIAN_POINT('Ctrl Pts',(-13.4674334526882,35.7724896561152,30.));
#59415=CARTESIAN_POINT('Ctrl Pts',(-13.4601199750053,35.7948923594824,30.));
#59416=CARTESIAN_POINT('Ctrl Pts',(-13.4525918930855,35.8172307103604,30.));
#59417=CARTESIAN_POINT('Ctrl Pts',(-13.4468394074071,35.8343002700268,30.));
#59418=CARTESIAN_POINT('Ctrl Pts',(-13.4409618348628,35.8513313943885,30.));
#59419=CARTESIAN_POINT('Ctrl Pts',(-13.4349636589554,35.8683101630108,30.));
#59420=CARTESIAN_POINT('Ctrl Pts',(-13.3973630090629,35.9747446431643,30.));
#59421=CARTESIAN_POINT('Ctrl Pts',(-13.3549838397234,36.0792521464373,30.));
#59422=CARTESIAN_POINT('Ctrl Pts',(-13.3078911250007,36.1814300295353,30.));
#59423=CARTESIAN_POINT('Ctrl Pts',(-13.2675799744265,36.2688938348217,30.));
#59424=CARTESIAN_POINT('Ctrl Pts',(-13.2238142519443,36.3546505536924,30.));
#59425=CARTESIAN_POINT('Ctrl Pts',(-13.1766119737641,36.4384274454971,30.));
#59426=CARTESIAN_POINT('Ctrl Pts',(-13.1551452588006,36.4765276119769,30.));
#59427=CARTESIAN_POINT('Ctrl Pts',(-13.132967502798,36.514218007177,30.));
#59428=CARTESIAN_POINT('Ctrl Pts',(-13.110079097282,36.5514713768243,30.));
#59429=CARTESIAN_POINT('Ctrl Pts',(-13.0960864911787,36.5742458652932,30.));
#59430=CARTESIAN_POINT('Ctrl Pts',(-13.0818259721494,36.5968603357343,30.));
#59431=CARTESIAN_POINT('Ctrl Pts',(-13.0673126858154,36.6192855347161,30.));
#59432=CARTESIAN_POINT('Ctrl Pts',(-13.0087455119247,36.7097805816736,30.));
#59433=CARTESIAN_POINT('Ctrl Pts',(-12.9460227269703,36.7972676999888,30.));
#59434=CARTESIAN_POINT('Ctrl Pts',(-12.8791807735713,36.8813650266868,30.));
#59435=CARTESIAN_POINT('Ctrl Pts',(-12.8123388201723,36.9654623533848,30.));
#59436=CARTESIAN_POINT('Ctrl Pts',(-12.7413774124275,37.0461705445025,30.));
#59437=CARTESIAN_POINT('Ctrl Pts',(-12.6663017713996,37.1230656129614,30.));
#59438=CARTESIAN_POINT('Ctrl Pts',(-12.6374945150854,37.1525710013412,30.));
#59439=CARTESIAN_POINT('Ctrl Pts',(-12.6080811803488,37.1815144607823,30.));
#59440=CARTESIAN_POINT('Ctrl Pts',(-12.5780824317837,37.2098873180834,30.));
#59441=CARTESIAN_POINT('Origin',(130.,-35.,16.));
#59442=CARTESIAN_POINT('Origin',(-10.,-35.,16.));
#59443=CARTESIAN_POINT('Origin',(-10.,35.,16.));
#59444=CARTESIAN_POINT('Origin',(130.,35.,16.));
#59445=CARTESIAN_POINT('Origin',(140.,-60.,20.));
#59446=CARTESIAN_POINT('',(135.5,-60.,30.));
#59447=CARTESIAN_POINT('Origin',(140.,-60.,30.));
#59448=CARTESIAN_POINT('',(135.5,-60.,10.));
#59449=CARTESIAN_POINT('',(135.5,-60.,20.));
#59450=CARTESIAN_POINT('Origin',(140.,-60.,10.));
#59451=CARTESIAN_POINT('Origin',(-20.,-60.,20.));
#59452=CARTESIAN_POINT('',(-24.5,-60.,30.));
#59453=CARTESIAN_POINT('Origin',(-20.,-60.,30.));
#59454=CARTESIAN_POINT('',(-24.5,-60.,10.));
#59455=CARTESIAN_POINT('',(-24.5,-60.,20.));
#59456=CARTESIAN_POINT('Origin',(-20.,-60.,10.));
#59457=CARTESIAN_POINT('Origin',(-20.,60.,20.));
#59458=CARTESIAN_POINT('',(-24.5,60.,30.));
#59459=CARTESIAN_POINT('Origin',(-20.,60.,30.));
#59460=CARTESIAN_POINT('',(-24.5,60.,10.));
#59461=CARTESIAN_POINT('',(-24.5,60.,20.));
#59462=CARTESIAN_POINT('Origin',(-20.,60.,10.));
#59463=CARTESIAN_POINT('Origin',(140.,60.,20.));
#59464=CARTESIAN_POINT('',(135.5,60.,30.));
#59465=CARTESIAN_POINT('Origin',(140.,60.,30.));
#59466=CARTESIAN_POINT('',(135.5,60.,10.));
#59467=CARTESIAN_POINT('',(135.5,60.,20.));
#59468=CARTESIAN_POINT('Origin',(140.,60.,10.));
#59469=CARTESIAN_POINT('Origin',(160.,75.,10.));
#59470=CARTESIAN_POINT('',(165.,75.,10.));
#59471=CARTESIAN_POINT('',(-45.,75.,10.));
#59472=CARTESIAN_POINT('',(110.,75.,10.));
#59473=CARTESIAN_POINT('',(-45.,75.,30.));
#59474=CARTESIAN_POINT('',(-45.,75.,10.));
#59475=CARTESIAN_POINT('',(165.,75.,30.));
#59476=CARTESIAN_POINT('',(110.,75.,30.));
#59477=CARTESIAN_POINT('',(165.,75.,10.));
#59478=CARTESIAN_POINT('Origin',(165.,-70.,10.));
#59479=CARTESIAN_POINT('',(165.,-75.,10.));
#59480=CARTESIAN_POINT('',(165.,-35.,10.));
#59481=CARTESIAN_POINT('',(165.,-75.,30.));
#59482=CARTESIAN_POINT('',(165.,-35.,30.));
#59483=CARTESIAN_POINT('',(165.,-75.,10.));
#59484=CARTESIAN_POINT('Origin',(-40.,-75.,10.));
#59485=CARTESIAN_POINT('',(-45.,-75.,10.));
#59486=CARTESIAN_POINT('',(10.,-75.,10.));
#59487=CARTESIAN_POINT('',(-45.,-75.,30.));
#59488=CARTESIAN_POINT('',(10.,-75.,30.));
#59489=CARTESIAN_POINT('',(-45.,-75.,10.));
#59490=CARTESIAN_POINT('Origin',(-45.,70.,10.));
#59491=CARTESIAN_POINT('',(-45.,35.,10.));
#59492=CARTESIAN_POINT('',(-45.,35.,30.));
#59493=CARTESIAN_POINT('Origin',(60.,0.,30.));
#59494=CARTESIAN_POINT('Origin',(60.,0.,10.));
#59495=CARTESIAN_POINT('',(0.,0.,0.));
#59496=CARTESIAN_POINT('Origin',(80.,9.,141.545925280538));
#59497=CARTESIAN_POINT('',(81.252039109102,10.6292316077768,129.106054344332));
#59498=CARTESIAN_POINT('',(81.2492121323183,10.6255440252465,129.047846840803));
#59499=CARTESIAN_POINT('',(81.252039109102,10.6292316077768,141.545925280538));
#59500=CARTESIAN_POINT('',(81.8174278887596,9.95862058795898,129.));
#59501=CARTESIAN_POINT('Ctrl Pts',(81.2492121323183,10.6255440252465,129.047846840803));
#59502=CARTESIAN_POINT('Ctrl Pts',(81.4831295089877,10.4461916147052,129.031897893869));
#59503=CARTESIAN_POINT('Ctrl Pts',(81.6801942454166,10.2187988626804,129.015948946934));
#59504=CARTESIAN_POINT('Ctrl Pts',(81.8174278887596,9.95862058795898,129.));
#59505=CARTESIAN_POINT('',(82.0533682613732,8.92465847303635,129.000000008565));
#59506=CARTESIAN_POINT('Origin',(80.,9.,129.));
#59507=CARTESIAN_POINT('Ctrl Pts',(81.252039109102,10.6292316077768,129.106054344332));
#59508=CARTESIAN_POINT('Ctrl Pts',(81.3081324428432,10.5861247546636,129.102199429059));
#59509=CARTESIAN_POINT('Ctrl Pts',(81.3621028162874,10.5400362316538,129.098344513787));
#59510=CARTESIAN_POINT('Ctrl Pts',(81.4136152532126,10.49120403647,129.094489598514));
#59511=CARTESIAN_POINT('Ctrl Pts',(81.4662254566598,10.4413311926145,129.090552532266));
#59512=CARTESIAN_POINT('Ctrl Pts',(81.5162712916801,10.3885966287696,129.086615466018));
#59513=CARTESIAN_POINT('Ctrl Pts',(81.5634291489626,10.3332992382335,129.08267839977));
#59514=CARTESIAN_POINT('Ctrl Pts',(81.6094921147899,10.2792857194398,129.078832742684));
#59515=CARTESIAN_POINT('Ctrl Pts',(81.6527994239459,10.2228274898001,129.074987085598));
#59516=CARTESIAN_POINT('Ctrl Pts',(81.6930862822707,10.164240698175,129.071141428511));
#59517=CARTESIAN_POINT('Ctrl Pts',(81.7333526428636,10.1056837151871,129.067297728074));
#59518=CARTESIAN_POINT('Ctrl Pts',(81.7706013247367,10.0450007212822,129.063454027637));
#59519=CARTESIAN_POINT('Ctrl Pts',(81.8046092461277,9.98253907367099,129.0596103272));
#59520=CARTESIAN_POINT('Ctrl Pts',(81.83861143105,9.92008796211362,129.055767275119));
#59521=CARTESIAN_POINT('Ctrl Pts',(81.8693737075422,9.85585922244642,129.051924223039));
#59522=CARTESIAN_POINT('Ctrl Pts',(81.896718484156,9.79022563509474,129.048081170959));
#59523=CARTESIAN_POINT('Ctrl Pts',(81.9252281299942,9.72179610074859,129.044074407426));
#59524=CARTESIAN_POINT('Ctrl Pts',(81.9500223238438,9.65183985848909,129.040067643893));
#59525=CARTESIAN_POINT('Ctrl Pts',(81.9709559793998,9.58080124807728,129.03606088036));
#59526=CARTESIAN_POINT('Ctrl Pts',(81.9910609207249,9.51257488931614,129.03221273518));
#59527=CARTESIAN_POINT('Ctrl Pts',(82.0076051816575,9.44335075661424,129.02836459));
#59528=CARTESIAN_POINT('Ctrl Pts',(82.0205121917149,9.37353453070845,129.02451644482));
#59529=CARTESIAN_POINT('Ctrl Pts',(82.0334283357576,9.30366889751318,129.020665576398));
#59530=CARTESIAN_POINT('Ctrl Pts',(82.0427020466773,9.23321082209362,129.016814707977));
#59531=CARTESIAN_POINT('Ctrl Pts',(82.0483086039853,9.16257129309895,129.012963839556));
#59532=CARTESIAN_POINT('Ctrl Pts',(82.053924244546,9.09181732013021,129.009106732295));
#59533=CARTESIAN_POINT('Ctrl Pts',(82.0558608740505,9.02088179457733,129.005249625034));
#59534=CARTESIAN_POINT('Ctrl Pts',(82.054145810819,8.95017480160856,129.001392517773));
#59535=CARTESIAN_POINT('Ctrl Pts',(82.0539394176871,8.94166582219882,129.000928348037));
#59536=CARTESIAN_POINT('Ctrl Pts',(82.0536802019389,8.93316014380039,129.000464178301));
#59537=CARTESIAN_POINT('Ctrl Pts',(82.0533682613732,8.92465847303635,129.000000008565));
#59538=CARTESIAN_POINT('Origin',(80.,9.,141.545925280538));
#59539=CARTESIAN_POINT('',(81.252039109102,10.6292316077768,129.806138766482));
#59540=CARTESIAN_POINT('',(81.252039109102,10.6292316077768,129.74786511009));
#59541=CARTESIAN_POINT('',(81.252039109102,10.6292316077768,141.545925280538));
#59542=CARTESIAN_POINT('',(77.945443344794,8.99850140731331,129.295925300345));
#59543=CARTESIAN_POINT('Ctrl Pts',(81.252039109102,10.6292316077768,129.74786511009));
#59544=CARTESIAN_POINT('Ctrl Pts',(81.3085193333677,10.5858274353228,129.744007244423));
#59545=CARTESIAN_POINT('Ctrl Pts',(81.3627900115786,10.5394443174509,129.740149378756));
#59546=CARTESIAN_POINT('Ctrl Pts',(81.4145261411931,10.4903400143529,129.736291513089));
#59547=CARTESIAN_POINT('Ctrl Pts',(81.4662398767985,10.4412569660766,129.732435317301));
#59548=CARTESIAN_POINT('Ctrl Pts',(81.515420889261,10.3894554040803,129.728579121513));
#59549=CARTESIAN_POINT('Ctrl Pts',(81.5617787889323,10.3352320311246,129.724722925726));
#59550=CARTESIAN_POINT('Ctrl Pts',(81.6081321155176,10.2810140071633,129.720867110342));
#59551=CARTESIAN_POINT('Ctrl Pts',(81.6516625677301,10.2243750165204,129.717011294957));
#59552=CARTESIAN_POINT('Ctrl Pts',(81.692119193999,10.1656458277711,129.713155479573));
#59553=CARTESIAN_POINT('Ctrl Pts',(81.7326518785676,10.1068062283758,129.709292415271));
#59554=CARTESIAN_POINT('Ctrl Pts',(81.7700988932371,10.0458689678327,129.705429350969));
#59555=CARTESIAN_POINT('Ctrl Pts',(81.8042518602189,9.98319519292799,129.701566286667));
#59556=CARTESIAN_POINT('Ctrl Pts',(81.8383883906004,9.92055158066739,129.69770508152));
#59557=CARTESIAN_POINT('Ctrl Pts',(81.8692338507331,9.85617357356739,129.693843876372));
#59558=CARTESIAN_POINT('Ctrl Pts',(81.8966275623393,9.79044383246044,129.689982671225));
#59559=CARTESIAN_POINT('Ctrl Pts',(81.9240726458304,9.72459082727232,129.686114225095));
#59560=CARTESIAN_POINT('Ctrl Pts',(81.9480528801327,9.6573814808109,129.682245778965));
#59561=CARTESIAN_POINT('Ctrl Pts',(81.9684568154499,9.58921585875539,129.678377332835));
#59562=CARTESIAN_POINT('Ctrl Pts',(81.9888137843977,9.52120714230307,129.674517791206));
#59563=CARTESIAN_POINT('Ctrl Pts',(82.0056108658398,9.45224703112079,129.670658249578));
#59564=CARTESIAN_POINT('Ctrl Pts',(82.0187884999237,9.3827408458422,129.666798707949));
#59565=CARTESIAN_POINT('Ctrl Pts',(82.0319999872495,9.313056099701,129.662929251187));
#59566=CARTESIAN_POINT('Ctrl Pts',(82.0416249737109,9.24255035252164,129.659059794426));
#59567=CARTESIAN_POINT('Ctrl Pts',(82.0475698214487,9.17162572299227,129.655190337664));
#59568=CARTESIAN_POINT('Ctrl Pts',(82.0535058266289,9.10080658903576,129.651326636456));
#59569=CARTESIAN_POINT('Ctrl Pts',(82.0557725185925,9.02957028953356,129.647462935249));
#59570=CARTESIAN_POINT('Ctrl Pts',(82.054327394704,8.95832845252654,129.643599234042));
#59571=CARTESIAN_POINT('Ctrl Pts',(82.0528839614273,8.88716995944365,129.639740052875));
#59572=CARTESIAN_POINT('Ctrl Pts',(82.0477373475193,8.81600642494071,129.635880871709));
#59573=CARTESIAN_POINT('Ctrl Pts',(82.0388970300604,8.74525215739669,129.632021690542));
#59574=CARTESIAN_POINT('Ctrl Pts',(82.0300622648841,8.67454232804085,129.628164933187));
#59575=CARTESIAN_POINT('Ctrl Pts',(82.0175384588747,8.60424173644822,129.624308175832));
#59576=CARTESIAN_POINT('Ctrl Pts',(82.0013870241082,8.53476076881736,129.620451418478));
#59577=CARTESIAN_POINT('Ctrl Pts',(81.9852403338186,8.46530021119049,129.616595794043));
#59578=CARTESIAN_POINT('Ctrl Pts',(81.9654682402386,8.3966592723316,129.612740169609));
#59579=CARTESIAN_POINT('Ctrl Pts',(81.9421831510885,8.3292376202201,129.608884545175));
#59580=CARTESIAN_POINT('Ctrl Pts',(81.9188971176168,8.26181323383866,129.605028764377));
#59581=CARTESIAN_POINT('Ctrl Pts',(81.8920979663439,8.1956086907147,129.601172983579));
#59582=CARTESIAN_POINT('Ctrl Pts',(81.8619472520006,8.13100633301075,129.597317202781));
#59583=CARTESIAN_POINT('Ctrl Pts',(81.8317649374834,8.06633626726792,129.59345738084));
#59584=CARTESIAN_POINT('Ctrl Pts',(81.7982242536195,8.00327218000733,129.5895975589));
#59585=CARTESIAN_POINT('Ctrl Pts',(81.7615336137239,7.94217350656126,129.585737736959));
#59586=CARTESIAN_POINT('Ctrl Pts',(81.7248221654374,7.8810401821776,129.581875725994));
#59587=CARTESIAN_POINT('Ctrl Pts',(81.6849574763693,7.82187489349001,129.578013715029));
#59588=CARTESIAN_POINT('Ctrl Pts',(81.6421908386299,7.76500736357659,129.574151704065));
#59589=CARTESIAN_POINT('Ctrl Pts',(81.5993493728494,7.70804033353673,129.570282935807));
#59590=CARTESIAN_POINT('Ctrl Pts',(81.5535961328667,7.65337946154818,129.566414167549));
#59591=CARTESIAN_POINT('Ctrl Pts',(81.5052216848136,7.60132017885905,129.562545399291));
#59592=CARTESIAN_POINT('Ctrl Pts',(81.4765470131007,7.57046126675146,129.560252129513));
#59593=CARTESIAN_POINT('Ctrl Pts',(81.4469520253758,7.54051576286219,129.557958859736));
#59594=CARTESIAN_POINT('Ctrl Pts',(81.416502734468,7.51153852392995,129.555665589958));
#59595=CARTESIAN_POINT('Ctrl Pts',(81.3651794217435,7.46269640474508,129.551800205955));
#59596=CARTESIAN_POINT('Ctrl Pts',(81.3112252599378,7.41641511917265,129.547934821953));
#59597=CARTESIAN_POINT('Ctrl Pts',(81.2549263703187,7.37299128226715,129.544069437951));
#59598=CARTESIAN_POINT('Ctrl Pts',(81.1987115926323,7.32963232164728,129.540209828927));
#59599=CARTESIAN_POINT('Ctrl Pts',(81.1401594225051,7.28912263103086,129.536350219904));
#59600=CARTESIAN_POINT('Ctrl Pts',(81.0795917608502,7.25172107705769,129.532490610881));
#59601=CARTESIAN_POINT('Ctrl Pts',(81.019095173482,7.21436341265691,129.52863553099));
#59602=CARTESIAN_POINT('Ctrl Pts',(80.9565882043631,7.18010689512892,129.524780451099));
#59603=CARTESIAN_POINT('Ctrl Pts',(80.8924232503983,7.14916821276258,129.520925371209));
#59604=CARTESIAN_POINT('Ctrl Pts',(80.8282986965517,7.118249010289,129.517072718588));
#59605=CARTESIAN_POINT('Ctrl Pts',(80.7625186662802,7.09064370965583,129.513220065967));
#59606=CARTESIAN_POINT('Ctrl Pts',(80.6954604719183,7.06652326248824,129.509367413347));
#59607=CARTESIAN_POINT('Ctrl Pts',(80.6284219527023,7.04240989235757,129.50551589111));
#59608=CARTESIAN_POINT('Ctrl Pts',(80.5601064716975,7.02177951062841,129.501664368873));
#59609=CARTESIAN_POINT('Ctrl Pts',(80.4909100257795,7.00475442386427,129.497812846637));
#59610=CARTESIAN_POINT('Ctrl Pts',(80.421710617344,6.98772860820264,129.493961159504));
#59611=CARTESIAN_POINT('Ctrl Pts',(80.3516306423667,6.97430850810218,129.490109472372));
#59612=CARTESIAN_POINT('Ctrl Pts',(80.2810782143665,6.96456574660134,129.486257785239));
#59613=CARTESIAN_POINT('Ctrl Pts',(80.2104510098597,6.9548126590254,129.482402015814));
#59614=CARTESIAN_POINT('Ctrl Pts',(80.139350835998,6.9487447569335,129.478546246388));
#59615=CARTESIAN_POINT('Ctrl Pts',(80.068191985698,6.9463818720155,129.474690476962));
#59616=CARTESIAN_POINT('Ctrl Pts',(79.9969924228888,6.944017635207,129.470832501513));
#59617=CARTESIAN_POINT('Ctrl Pts',(79.9257346037539,6.94536262570084,129.466974526065));
#59618=CARTESIAN_POINT('Ctrl Pts',(79.8548310998208,6.95038453535285,129.463116550616));
#59619=CARTESIAN_POINT('Ctrl Pts',(79.7838021060318,6.95541533312298,129.459251747059));
#59620=CARTESIAN_POINT('Ctrl Pts',(79.7131291626912,6.96413598279352,129.455386943503));
#59621=CARTESIAN_POINT('Ctrl Pts',(79.6432173161427,6.97646258275278,129.451522139946));
#59622=CARTESIAN_POINT('Ctrl Pts',(79.6010710950756,6.98389364962538,129.449192250619));
#59623=CARTESIAN_POINT('Ctrl Pts',(79.5592012548522,6.99263422302007,129.446862361293));
#59624=CARTESIAN_POINT('Ctrl Pts',(79.5176937420075,7.00265720618587,129.444532471966));
#59625=CARTESIAN_POINT('Ctrl Pts',(79.4486461888338,7.01933039172912,129.440656711986));
#59626=CARTESIAN_POINT('Ctrl Pts',(79.3803311134737,7.03962034190895,129.436780952005));
#59627=CARTESIAN_POINT('Ctrl Pts',(79.3131544745362,7.06344615704848,129.432905192025));
#59628=CARTESIAN_POINT('Ctrl Pts',(79.2460780170999,7.08723644040247,129.429035212022));
#59629=CARTESIAN_POINT('Ctrl Pts',(79.1801370782105,7.11455196023636,129.425165232019));
#59630=CARTESIAN_POINT('Ctrl Pts',(79.115725168422,7.14526131632033,129.421295252016));
#59631=CARTESIAN_POINT('Ctrl Pts',(79.0513895933296,7.17593427867882,129.417429858334));
#59632=CARTESIAN_POINT('Ctrl Pts',(78.9885798822686,7.20999287981601,129.413564464653));
#59633=CARTESIAN_POINT('Ctrl Pts',(78.9276705405346,7.24725726563691,129.409699070972));
#59634=CARTESIAN_POINT('Ctrl Pts',(78.8668000929382,7.28449785599208,129.405836145568));
#59635=CARTESIAN_POINT('Ctrl Pts',(78.8078280186592,7.32493991718004,129.401973220164));
#59636=CARTESIAN_POINT('Ctrl Pts',(78.7511038510315,7.36835789108281,129.398110294761));
#59637=CARTESIAN_POINT('Ctrl Pts',(78.6943971038458,7.41176253098132,129.394248555692));
#59638=CARTESIAN_POINT('Ctrl Pts',(78.6399372767077,7.45814097500666,129.390386816623));
#59639=CARTESIAN_POINT('Ctrl Pts',(78.5880431440327,7.50722560331881,129.386525077554));
#59640=CARTESIAN_POINT('Ctrl Pts',(78.5361477488554,7.55631142578241,129.382663244536));
#59641=CARTESIAN_POINT('Ctrl Pts',(78.4868185221684,7.60810322910186,129.378801411517));
#59642=CARTESIAN_POINT('Ctrl Pts',(78.4403382347849,7.66229572003898,129.374939578498));
#59643=CARTESIAN_POINT('Ctrl Pts',(78.39381094995,7.71654300644102,129.371073840678));
#59644=CARTESIAN_POINT('Ctrl Pts',(78.3501386708224,7.77319545824749,129.367208102857));
#59645=CARTESIAN_POINT('Ctrl Pts',(78.3095640209211,7.8319144880893,129.363342365037));
#59646=CARTESIAN_POINT('Ctrl Pts',(78.2689671120395,7.89066573079638,129.359474506498));
#59647=CARTESIAN_POINT('Ctrl Pts',(78.2314714702368,7.95148539676405,129.35560664796));
#59648=CARTESIAN_POINT('Ctrl Pts',(78.1972750294098,8.01400799044285,129.351738789422));
#59649=CARTESIAN_POINT('Ctrl Pts',(78.1630203529657,8.07663705841363,129.347864344024));
#59650=CARTESIAN_POINT('Ctrl Pts',(78.132076305444,8.14097440811675,129.343989898627));
#59651=CARTESIAN_POINT('Ctrl Pts',(78.1045934316036,8.20663280696784,129.34011545323));
#59652=CARTESIAN_POINT('Ctrl Pts',(78.0887135064689,8.24457099582957,129.337876753478));
#59653=CARTESIAN_POINT('Ctrl Pts',(78.0739882366105,8.28294990542073,129.335638053726));
#59654=CARTESIAN_POINT('Ctrl Pts',(78.0604390140864,8.32169273598019,129.333399353975));
#59655=CARTESIAN_POINT('Ctrl Pts',(78.033260828792,8.39940640744042,129.328908779215));
#59656=CARTESIAN_POINT('Ctrl Pts',(78.010731418976,8.47882922479276,129.324418204456));
#59657=CARTESIAN_POINT('Ctrl Pts',(77.993036431149,8.55943809083774,129.319927629697));
#59658=CARTESIAN_POINT('Ctrl Pts',(77.9754996204933,8.63932638659772,129.315477196611));
#59659=CARTESIAN_POINT('Ctrl Pts',(77.9627112748633,8.72037946475493,129.311026763524));
#59660=CARTESIAN_POINT('Ctrl Pts',(77.9548055650093,8.80206747214528,129.306576330438));
#59661=CARTESIAN_POINT('Ctrl Pts',(77.9484987679612,8.86723425582204,129.303025987867));
#59662=CARTESIAN_POINT('Ctrl Pts',(77.9452984670482,8.93280468883457,129.299475645296));
#59663=CARTESIAN_POINT('Ctrl Pts',(77.9452505466197,8.99850122269098,129.295925302724));
#59664=CARTESIAN_POINT('Ctrl Pts',(77.9470482356371,8.99850294414681,129.295925280538));
#59665=CARTESIAN_POINT('Ctrl Pts',(77.9500644391936,9.45244375993743,129.271372265686));
#59666=CARTESIAN_POINT('Ctrl Pts',(78.321762223559,10.5960398895428,129.209774878171));
#59667=CARTESIAN_POINT('Ctrl Pts',(79.9094066588576,11.2849415874619,129.127082064926));
#59668=CARTESIAN_POINT('Ctrl Pts',(80.939813231773,10.8627706880183,129.068942266533));
#59669=CARTESIAN_POINT('Ctrl Pts',(81.2492121323183,10.6255440252465,129.047846840803));
#59670=CARTESIAN_POINT('',(77.9452508134379,9.00182833865366,129.354074719499));
#59671=CARTESIAN_POINT('Ctrl Pts',(77.9452508134385,9.00182833933565,129.354074719462));
#59672=CARTESIAN_POINT('Ctrl Pts',(77.9453406304354,9.10276769878956,129.348594607972));
#59673=CARTESIAN_POINT('Ctrl Pts',(77.9528718856253,9.2033869237755,129.343114496482));
#59674=CARTESIAN_POINT('Ctrl Pts',(77.9676835434894,9.3027992455346,129.337634384992));
#59675=CARTESIAN_POINT('Ctrl Pts',(77.9734618754717,9.34158203430287,129.335496480932));
#59676=CARTESIAN_POINT('Ctrl Pts',(77.9803477636373,9.38018147547678,129.333358576871));
#59677=CARTESIAN_POINT('Ctrl Pts',(77.9883298389047,9.41854596576566,129.331220672811));
#59678=CARTESIAN_POINT('Ctrl Pts',(78.0027616204826,9.48790987498085,129.327355291515));
#59679=CARTESIAN_POINT('Ctrl Pts',(78.0208138006321,9.556663936971,129.32348991022));
#59680=CARTESIAN_POINT('Ctrl Pts',(78.0424197606568,9.62440144861534,129.319624528925));
#59681=CARTESIAN_POINT('Ctrl Pts',(78.0639934408006,9.69203775860952,129.315764922612));
#59682=CARTESIAN_POINT('Ctrl Pts',(78.0891102156646,9.75866007280167,129.3119053163));
#59683=CARTESIAN_POINT('Ctrl Pts',(78.1176525675056,9.82387238446372,129.308045709988));
#59684=CARTESIAN_POINT('Ctrl Pts',(78.1461614258055,9.88900817155401,129.3041906328));
#59685=CARTESIAN_POINT('Ctrl Pts',(78.1780876826902,9.95273679869852,129.300335555613));
#59686=CARTESIAN_POINT('Ctrl Pts',(78.2132647473922,10.0146796044016,129.296480478426));
#59687=CARTESIAN_POINT('Ctrl Pts',(78.2484196636299,10.0765834091808,129.292627828503));
#59688=CARTESIAN_POINT('Ctrl Pts',(78.2868210873334,10.1367032008444,129.28877517858));
#59689=CARTESIAN_POINT('Ctrl Pts',(78.3282559207096,10.1946837639549,129.284922528658));
#59690=CARTESIAN_POINT('Ctrl Pts',(78.3696785970312,10.2526473154639,129.281071009109));
#59691=CARTESIAN_POINT('Ctrl Pts',(78.4141326333405,10.3084724885383,129.277219489561));
#59692=CARTESIAN_POINT('Ctrl Pts',(78.4613618953665,10.3618334499747,129.273367970013));
#59693=CARTESIAN_POINT('Ctrl Pts',(78.5085931795893,10.4151966961464,129.269516285555));
#59694=CARTESIAN_POINT('Ctrl Pts',(78.5585996011231,10.4660951581404,129.265664601098));
#59695=CARTESIAN_POINT('Ctrl Pts',(78.6110862317618,10.5142377973418,129.261812916641));
#59696=CARTESIAN_POINT('Ctrl Pts',(78.6636284920416,10.5624314620654,129.257957149852));
#59697=CARTESIAN_POINT('Ctrl Pts',(78.7186558493627,10.607863143692,129.254101383063));
#59698=CARTESIAN_POINT('Ctrl Pts',(78.7758388347598,10.6502808864002,129.250245616274));
#59699=CARTESIAN_POINT('Ctrl Pts',(78.8330545368563,10.6927228980151,129.246387643445));
#59700=CARTESIAN_POINT('Ctrl Pts',(78.8924279161816,10.7321472689681,129.242529670616));
#59701=CARTESIAN_POINT('Ctrl Pts',(78.9536012630827,10.7683459067382,129.238671697787));
#59702=CARTESIAN_POINT('Ctrl Pts',(79.0148828797013,10.804608611892,129.234806896795));
#59703=CARTESIAN_POINT('Ctrl Pts',(79.0779703927226,10.8376339598158,129.230942095802));
#59704=CARTESIAN_POINT('Ctrl Pts',(79.1424829361018,10.8672605730383,129.227077294809));
#59705=CARTESIAN_POINT('Ctrl Pts',(79.1813746242017,10.8851211151989,129.224747381479));
#59706=CARTESIAN_POINT('Ctrl Pts',(79.2207838360795,10.9017473816217,129.222417468149));
#59707=CARTESIAN_POINT('Ctrl Pts',(79.2606244670148,10.9171127728235,129.220087554819));
#59708=CARTESIAN_POINT('Ctrl Pts',(79.3268985097602,10.942672774495,129.216211793517));
#59709=CARTESIAN_POINT('Ctrl Pts',(79.3946272743244,10.9648414181532,129.212336032215));
#59710=CARTESIAN_POINT('Ctrl Pts',(79.4634308512325,10.9834543380403,129.208460270913));
#59711=CARTESIAN_POINT('Ctrl Pts',(79.5321318201631,11.0020395001545,129.204590289601));
#59712=CARTESIAN_POINT('Ctrl Pts',(79.6019039559843,11.017079339933,129.20072030829));
#59713=CARTESIAN_POINT('Ctrl Pts',(79.6723488634407,11.0284581078276,129.196850326978));
#59714=CARTESIAN_POINT('Ctrl Pts',(79.7427102860479,11.0398233906491,129.192984932014));
#59715=CARTESIAN_POINT('Ctrl Pts',(79.8137424208771,11.0475361441803,129.189119537049));
#59716=CARTESIAN_POINT('Ctrl Pts',(79.8850349442187,11.0515312813723,129.185254142085));
#59717=CARTESIAN_POINT('Ctrl Pts',(79.9562819428734,11.0555238674221,129.181391215415));
#59718=CARTESIAN_POINT('Ctrl Pts',(80.027788518058,11.0558035205452,129.177528288744));
#59719=CARTESIAN_POINT('Ctrl Pts',(80.0991388891969,11.0523569482789,129.173665362074));
#59720=CARTESIAN_POINT('Ctrl Pts',(80.1704673477443,11.0489114344981,129.169803621756));
#59721=CARTESIAN_POINT('Ctrl Pts',(80.2416392143741,11.0417419908114,129.165941881439));
#59722=CARTESIAN_POINT('Ctrl Pts',(80.3122400830185,11.0308874151603,129.162080141122));
#59723=CARTESIAN_POINT('Ctrl Pts',(80.3828426689081,11.0200325754903,129.158218306874));
#59724=CARTESIAN_POINT('Ctrl Pts',(80.4528737512294,11.0054925015909,129.154356472627));
#59725=CARTESIAN_POINT('Ctrl Pts',(80.5219271081132,10.9873574555969,129.150494638379));
#59726=CARTESIAN_POINT('Ctrl Pts',(80.5910502859759,10.9692040729612,129.146628899368));
#59727=CARTESIAN_POINT('Ctrl Pts',(80.6591932958107,10.9474485848929,129.142763160356));
#59728=CARTESIAN_POINT('Ctrl Pts',(80.7259639989441,10.9222314727257,129.138897421345));
#59729=CARTESIAN_POINT('Ctrl Pts',(80.7927713316841,10.8970005267533,129.135029561635));
#59730=CARTESIAN_POINT('Ctrl Pts',(80.8582044152026,10.8683043698804,129.131161701926));
#59731=CARTESIAN_POINT('Ctrl Pts',(80.9218925622573,10.8363310339246,129.127293842217));
#59732=CARTESIAN_POINT('Ctrl Pts',(80.9856891677658,10.804303248613,129.123419395692));
#59733=CARTESIAN_POINT('Ctrl Pts',(81.0477344828468,10.7689873806112,129.119544949167));
#59734=CARTESIAN_POINT('Ctrl Pts',(81.1076844332874,10.7306162944896,129.115670502641));
#59735=CARTESIAN_POINT('Ctrl Pts',(81.1423240314956,10.7084451501216,129.113431814037));
#59736=CARTESIAN_POINT('Ctrl Pts',(81.1762646277231,10.6852547759275,129.111193125432));
#59737=CARTESIAN_POINT('Ctrl Pts',(81.2094449454566,10.6610961701266,129.108954436827));
#59738=CARTESIAN_POINT('Ctrl Pts',(81.2237726773633,10.6506641414181,129.107987739329));
#59739=CARTESIAN_POINT('Ctrl Pts',(81.2379725780439,10.6400415177553,129.10702104183));
#59740=CARTESIAN_POINT('Ctrl Pts',(81.252039109102,10.6292316077768,129.106054344332));
#59741=CARTESIAN_POINT('Ctrl Pts',(81.252039109102,10.6292316077768,129.806138766482));
#59742=CARTESIAN_POINT('Ctrl Pts',(81.3085776991369,10.5857825821384,129.802277188624));
#59743=CARTESIAN_POINT('Ctrl Pts',(81.3628020004145,10.5394254826911,129.798415610767));
#59744=CARTESIAN_POINT('Ctrl Pts',(81.4144129894673,10.490447401865,129.794554032909));
#59745=CARTESIAN_POINT('Ctrl Pts',(81.4661146701134,10.441383256031,129.79068566943));
#59746=CARTESIAN_POINT('Ctrl Pts',(81.5151935348951,10.3896892853797,129.78681730595));
#59747=CARTESIAN_POINT('Ctrl Pts',(81.5613890748026,10.335687732813,129.782948942471));
#59748=CARTESIAN_POINT('Ctrl Pts',(81.5900328636082,10.3022037845792,129.780550343239));
#59749=CARTESIAN_POINT('Ctrl Pts',(81.6175689177519,10.2678332878201,129.778151744008));
#59750=CARTESIAN_POINT('Ctrl Pts',(81.6439435865611,10.2326585280217,129.775753144776));
#59751=CARTESIAN_POINT('Ctrl Pts',(81.6864883341909,10.1759184305673,129.77188398533));
#59752=CARTESIAN_POINT('Ctrl Pts',(81.7261753858345,10.1168620335078,129.768014825883));
#59753=CARTESIAN_POINT('Ctrl Pts',(81.7627435644833,10.0558090207858,129.764145666437));
#59754=CARTESIAN_POINT('Ctrl Pts',(81.7992572695089,9.99484695541022,129.760282270666));
#59755=CARTESIAN_POINT('Ctrl Pts',(81.8326610761952,9.93189459151865,129.756418874895));
#59756=CARTESIAN_POINT('Ctrl Pts',(81.8627355219774,9.86730267938221,129.752555479125));
#59757=CARTESIAN_POINT('Ctrl Pts',(81.8927747004109,9.80278651213253,129.748696613836));
#59758=CARTESIAN_POINT('Ctrl Pts',(81.9194920690401,9.73663505389883,129.744837748547));
#59759=CARTESIAN_POINT('Ctrl Pts',(81.9427136477607,9.66922436096161,129.740978883258));
#59760=CARTESIAN_POINT('Ctrl Pts',(81.965920603033,9.60185611891828,129.737122448033));
#59761=CARTESIAN_POINT('Ctrl Pts',(81.9856359781547,9.53323067363172,129.733266012808));
#59762=CARTESIAN_POINT('Ctrl Pts',(82.0017341442023,9.46374344031431,129.729409577583));
#59763=CARTESIAN_POINT('Ctrl Pts',(82.0178275571484,9.39427672361183,129.725554280999));
#59764=CARTESIAN_POINT('Ctrl Pts',(82.0303057717423,9.32394919700083,129.721698984414));
#59765=CARTESIAN_POINT('Ctrl Pts',(82.039093661386,9.25316911856549,129.71784368783));
#59766=CARTESIAN_POINT('Ctrl Pts',(82.0478818956115,9.18238626477412,129.713988240076));
#59767=CARTESIAN_POINT('Ctrl Pts',(82.0529794599358,9.11115130625805,129.710132792321));
#59768=CARTESIAN_POINT('Ctrl Pts',(82.0543629815708,9.03987859640918,129.706277344567));
#59769=CARTESIAN_POINT('Ctrl Pts',(82.0557479513842,8.96853128302626,129.702417861186));
#59770=CARTESIAN_POINT('Ctrl Pts',(82.0534111085149,8.89714662609191,129.698558377806));
#59771=CARTESIAN_POINT('Ctrl Pts',(82.0473812380801,8.8261390542485,129.694698894425));
#59772=CARTESIAN_POINT('Ctrl Pts',(82.041347953272,8.75509127484793,129.690837225638));
#59773=CARTESIAN_POINT('Ctrl Pts',(82.0316175443434,8.68442148704298,129.686975556851));
#59774=CARTESIAN_POINT('Ctrl Pts',(82.0182703789565,8.61453633124921,129.683113888064));
#59775=CARTESIAN_POINT('Ctrl Pts',(82.0048998647885,8.54452892229111,129.67924546389));
#59776=CARTESIAN_POINT('Ctrl Pts',(81.9879000781151,8.47530935765307,129.675377039717));
#59777=CARTESIAN_POINT('Ctrl Pts',(81.9674017498609,8.40727078936132,129.671508615544));
#59778=CARTESIAN_POINT('Ctrl Pts',(81.9552344738799,8.36688485995832,129.669212419291));
#59779=CARTESIAN_POINT('Ctrl Pts',(81.9418354981883,8.32691469877441,129.666916223038));
#59780=CARTESIAN_POINT('Ctrl Pts',(81.9272400716739,8.28743893690832,129.664620026785));
#59781=CARTESIAN_POINT('Ctrl Pts',(81.9026497162947,8.2209302252788,129.66075139836));
#59782=CARTESIAN_POINT('Ctrl Pts',(81.8745642826625,8.15556547524259,129.656882769936));
#59783=CARTESIAN_POINT('Ctrl Pts',(81.8431105948871,8.09173742920077,129.653014141511));
#59784=CARTESIAN_POINT('Ctrl Pts',(81.8117037846444,8.02800451036091,129.649151278762));
#59785=CARTESIAN_POINT('Ctrl Pts',(81.7769388976484,7.96580418176457,129.645288416013));
#59786=CARTESIAN_POINT('Ctrl Pts',(81.7389914861927,7.90551099893629,129.641425553264));
#59787=CARTESIAN_POINT('Ctrl Pts',(81.7010885844062,7.84528853581008,129.637567221384));
#59788=CARTESIAN_POINT('Ctrl Pts',(81.6600108304285,7.78696918439063,129.633708889504));
#59789=CARTESIAN_POINT('Ctrl Pts',(81.6159797094141,7.73090302133297,129.629850557624));
#59790=CARTESIAN_POINT('Ctrl Pts',(81.5719763196151,7.67487216927354,129.625994655757));
#59791=CARTESIAN_POINT('Ctrl Pts',(81.5250235524811,7.62109207141463,129.622138753891));
#59792=CARTESIAN_POINT('Ctrl Pts',(81.475385385291,7.56988268754986,129.618282852024));
#59793=CARTESIAN_POINT('Ctrl Pts',(81.4257618654248,7.51868841464652,129.614428087965));
#59794=CARTESIAN_POINT('Ctrl Pts',(81.3734548566607,7.47006369848698,129.610573323905));
#59795=CARTESIAN_POINT('Ctrl Pts',(81.3187665200082,7.42429303859968,129.606718559846));
#59796=CARTESIAN_POINT('Ctrl Pts',(81.2640760157143,7.37852056453442,129.602863642998));
#59797=CARTESIAN_POINT('Ctrl Pts',(81.20700437018,7.33560268150686,129.599008726149));
#59798=CARTESIAN_POINT('Ctrl Pts',(81.1478869368393,7.29578371597568,129.595153809301));
#59799=CARTESIAN_POINT('Ctrl Pts',(81.08870752091,7.25592300163336,129.591294850706));
#59800=CARTESIAN_POINT('Ctrl Pts',(81.0274784392499,7.21916796272987,129.587435892111));
#59801=CARTESIAN_POINT('Ctrl Pts',(80.9645633986281,7.18571914728537,129.583576933515));
#59802=CARTESIAN_POINT('Ctrl Pts',(80.901612684589,7.15225136604917,129.579715786854));
#59803=CARTESIAN_POINT('Ctrl Pts',(80.8369745491523,7.12209374562773,129.575854640193));
#59804=CARTESIAN_POINT('Ctrl Pts',(80.7710341310293,7.09539927247522,129.571993493532));
#59805=CARTESIAN_POINT('Ctrl Pts',(80.7049781762283,7.0686580269358,129.568125581612));
#59806=CARTESIAN_POINT('Ctrl Pts',(80.637615842551,7.04539220205611,129.564257669691));
#59807=CARTESIAN_POINT('Ctrl Pts',(80.569348250249,7.02570515564711,129.56038975777));
#59808=CARTESIAN_POINT('Ctrl Pts',(80.5287371152381,7.01399369384332,129.558088808111));
#59809=CARTESIAN_POINT('Ctrl Pts',(80.4878058559495,7.00354773124927,129.555787858452));
#59810=CARTESIAN_POINT('Ctrl Pts',(80.4466401967145,6.99438037076347,129.553486908793));
#59811=CARTESIAN_POINT('Ctrl Pts',(80.3774071820531,6.9789625682865,129.549617137619));
#59812=CARTESIAN_POINT('Ctrl Pts',(80.307239509545,6.96710365544103,129.545747366445));
#59813=CARTESIAN_POINT('Ctrl Pts',(80.2365361422388,6.95891004217972,129.541877595271));
#59814=CARTESIAN_POINT('Ctrl Pts',(80.16593814403,6.95072863984509,129.538013591209));
#59815=CARTESIAN_POINT('Ctrl Pts',(80.0948065141796,6.94620174973747,129.534149587148));
#59816=CARTESIAN_POINT('Ctrl Pts',(80.0235513509058,6.94538497611584,129.530285583086));
#59817=CARTESIAN_POINT('Ctrl Pts',(79.9523798796856,6.94456916182766,129.526426117453));
#59818=CARTESIAN_POINT('Ctrl Pts',(79.8810856464657,6.94745481361333,129.52256665182));
#59819=CARTESIAN_POINT('Ctrl Pts',(79.810083084742,6.954045668203,129.518707186187));
#59820=CARTESIAN_POINT('Ctrl Pts',(79.7391253248915,6.96063236403242,129.514850155836));
#59821=CARTESIAN_POINT('Ctrl Pts',(79.6684593537717,6.97091957938468,129.510993125485));
#59822=CARTESIAN_POINT('Ctrl Pts',(79.5984973427476,6.98485901765677,129.507136095134));
#59823=CARTESIAN_POINT('Ctrl Pts',(79.5285560950896,6.99879431897429,129.503280209475));
#59824=CARTESIAN_POINT('Ctrl Pts',(79.4593188687309,7.01637959649254,129.499424323816));
#59825=CARTESIAN_POINT('Ctrl Pts',(79.3911887511958,7.03751524188606,129.495568438157));
#59826=CARTESIAN_POINT('Ctrl Pts',(79.3230560843437,7.05865167814072,129.491712408217));
#59827=CARTESIAN_POINT('Ctrl Pts',(79.2560310717025,7.08333860004452,129.487856378277));
#59828=CARTESIAN_POINT('Ctrl Pts',(79.1905010544802,7.11142672376675,129.484000348336));
#59829=CARTESIAN_POINT('Ctrl Pts',(79.1249027002981,7.1395441387522,129.480140297196));
#59830=CARTESIAN_POINT('Ctrl Pts',(79.0608029009693,7.17106964428378,129.476280246055));
#59831=CARTESIAN_POINT('Ctrl Pts',(78.9985675987183,7.20580639055781,129.472420194914));
#59832=CARTESIAN_POINT('Ctrl Pts',(78.9362971787157,7.2405627378683,129.468557965647));
#59833=CARTESIAN_POINT('Ctrl Pts',(78.8758937615436,7.27853367462545,129.46469573638));
#59834=CARTESIAN_POINT('Ctrl Pts',(78.8176949647001,7.31947854342635,129.460833507114));
#59835=CARTESIAN_POINT('Ctrl Pts',(78.7593946368001,7.36049484284114,129.456964539972));
#59836=CARTESIAN_POINT('Ctrl Pts',(78.7033069902807,7.40449513291138,129.45309557283));
#59837=CARTESIAN_POINT('Ctrl Pts',(78.6497366239544,7.45119840592477,129.449226605688));
#59838=CARTESIAN_POINT('Ctrl Pts',(78.6180159090372,7.47885289684122,129.446935667393));
#59839=CARTESIAN_POINT('Ctrl Pts',(78.587177113685,7.5074543877569,129.444644729097));
#59840=CARTESIAN_POINT('Ctrl Pts',(78.5572770043333,7.53693885285868,129.442353790802));
#59841=CARTESIAN_POINT('Ctrl Pts',(78.507519198505,7.58600497071898,129.43854136117));
#59842=CARTESIAN_POINT('Ctrl Pts',(78.4601566137214,7.63772181533481,129.434728931539));
#59843=CARTESIAN_POINT('Ctrl Pts',(78.4154907258652,7.69182267154611,129.430916501907));
#59844=CARTESIAN_POINT('Ctrl Pts',(78.3708843294308,7.74585146970567,129.42710915013));
#59845=CARTESIAN_POINT('Ctrl Pts',(78.3289678286292,7.80225760548264,129.423301798352));
#59846=CARTESIAN_POINT('Ctrl Pts',(78.2900066810319,7.86073689975305,129.419494446575));
#59847=CARTESIAN_POINT('Ctrl Pts',(78.2510835039569,7.91915920162234,129.415690805344));
#59848=CARTESIAN_POINT('Ctrl Pts',(78.2151102469513,7.97965024231591,129.411887164112));
#59849=CARTESIAN_POINT('Ctrl Pts',(78.1823115521101,8.04187356319355,129.408083522881));
#59850=CARTESIAN_POINT('Ctrl Pts',(78.1495331090737,8.10405846380596,129.404282230237));
#59851=CARTESIAN_POINT('Ctrl Pts',(78.1199255730656,8.16797308076684,129.400480937593));
#59852=CARTESIAN_POINT('Ctrl Pts',(78.0936687399069,8.23325448205287,129.396679644949));
#59853=CARTESIAN_POINT('Ctrl Pts',(78.0674080110329,8.29854556911333,129.392877788309));
#59854=CARTESIAN_POINT('Ctrl Pts',(78.0444991802892,8.36520338671441,129.389075931669));
#59855=CARTESIAN_POINT('Ctrl Pts',(78.0250741653868,8.43284436855716,129.385274075029));
#59856=CARTESIAN_POINT('Ctrl Pts',(78.0056484149394,8.50048791168432,129.381472074428));
#59857=CARTESIAN_POINT('Ctrl Pts',(77.9897068701602,8.56911420800702,129.377670073827));
#59858=CARTESIAN_POINT('Ctrl Pts',(77.9773310505391,8.63832627495641,129.373868073226));
#59859=CARTESIAN_POINT('Ctrl Pts',(77.9649417654702,8.70761364774499,129.370061935878));
#59860=CARTESIAN_POINT('Ctrl Pts',(77.9561260270523,8.77748756743294,129.36625579853));
#59861=CARTESIAN_POINT('Ctrl Pts',(77.9509137023551,8.84754375282076,129.362449661181));
#59862=CARTESIAN_POINT('Ctrl Pts',(77.9470906737942,8.89892712073455,129.359658013954));
#59863=CARTESIAN_POINT('Ctrl Pts',(77.9452050593912,8.9504083842497,129.356866366726));
#59864=CARTESIAN_POINT('Ctrl Pts',(77.9452508134379,9.00182833865365,129.354074719499));
#59865=CARTESIAN_POINT('Origin',(80.,9.,141.545925280538));
#59866=CARTESIAN_POINT('',(81.252039109102,10.6292316077768,130.506052881431));
#59867=CARTESIAN_POINT('',(81.252039109102,10.6292316077768,130.447945712677));
#59868=CARTESIAN_POINT('',(81.252039109102,10.6292316077768,141.545925280538));
#59869=CARTESIAN_POINT('',(77.9452500565798,8.99951780232932,129.995925280508));
#59870=CARTESIAN_POINT('Ctrl Pts',(81.252039109102,10.6292316077768,130.447945712677));
#59871=CARTESIAN_POINT('Ctrl Pts',(81.2676313183556,10.6172492378733,130.446873986415));
#59872=CARTESIAN_POINT('Ctrl Pts',(81.283043563841,10.6050491142855,130.445802260153));
#59873=CARTESIAN_POINT('Ctrl Pts',(81.2982695699005,10.5926373367375,130.44473053389));
#59874=CARTESIAN_POINT('Ctrl Pts',(81.3532376874634,10.5478289973244,130.440861444718));
#59875=CARTESIAN_POINT('Ctrl Pts',(81.4059909767705,10.5000838098986,130.436992355545));
#59876=CARTESIAN_POINT('Ctrl Pts',(81.4561988948284,10.4496490406993,130.433123266372));
#59877=CARTESIAN_POINT('Ctrl Pts',(81.5063320051152,10.3992894172703,130.429259941986));
#59878=CARTESIAN_POINT('Ctrl Pts',(81.5539269322296,10.3462485080518,130.4253966176));
#59879=CARTESIAN_POINT('Ctrl Pts',(81.5986861256879,10.2908137875127,130.421533293214));
#59880=CARTESIAN_POINT('Ctrl Pts',(81.643392815583,10.2354440931756,130.417674500597));
#59881=CARTESIAN_POINT('Ctrl Pts',(81.6852700754498,10.177686541274,130.413815707979));
#59882=CARTESIAN_POINT('Ctrl Pts',(81.7240583933976,10.1178641324666,130.409956915362));
#59883=CARTESIAN_POINT('Ctrl Pts',(81.7628222769504,10.0580794083137,130.40610055356));
#59884=CARTESIAN_POINT('Ctrl Pts',(81.7985008154704,9.99623281453984,130.402244191758));
#59885=CARTESIAN_POINT('Ctrl Pts',(81.830876753814,9.93267779797929,130.398387829957));
#59886=CARTESIAN_POINT('Ctrl Pts',(81.8632431273927,9.86914155736234,130.394532607433));
#59887=CARTESIAN_POINT('Ctrl Pts',(81.8923086174108,9.80389832857846,130.39067738491));
#59888=CARTESIAN_POINT('Ctrl Pts',(81.9179018844489,9.73732619926814,130.386822162386));
#59889=CARTESIAN_POINT('Ctrl Pts',(81.9434961515718,9.67075146857944,130.382966789215));
#59890=CARTESIAN_POINT('Ctrl Pts',(81.9656177540764,9.60284818848602,130.379111416045));
#59891=CARTESIAN_POINT('Ctrl Pts',(81.9841441098762,9.53401284042958,130.375256042874));
#59892=CARTESIAN_POINT('Ctrl Pts',(82.0026898569072,9.46510544354896,130.371396634348));
#59893=CARTESIAN_POINT('Ctrl Pts',(82.0176327187617,9.39526450127846,130.367537225822));
#59894=CARTESIAN_POINT('Ctrl Pts',(82.0289007144248,9.32489914359176,130.363677817295));
#59895=CARTESIAN_POINT('Ctrl Pts',(82.0401750898638,9.25449394605857,130.359816223628));
#59896=CARTESIAN_POINT('Ctrl Pts',(82.0477704054185,9.18356422528882,130.35595462996));
#59897=CARTESIAN_POINT('Ctrl Pts',(82.0516666187131,9.11252398925642,130.352093036293));
#59898=CARTESIAN_POINT('Ctrl Pts',(82.0555696483686,9.04135946950529,130.348224686831));
#59899=CARTESIAN_POINT('Ctrl Pts',(82.0557606538919,8.97008453440691,130.34435633737));
#59900=CARTESIAN_POINT('Ctrl Pts',(82.0522717225443,8.89911224383035,130.340487987908));
#59901=CARTESIAN_POINT('Ctrl Pts',(82.05020014715,8.85697199049934,130.338191130572));
#59902=CARTESIAN_POINT('Ctrl Pts',(82.0468322168767,8.81493833801628,130.335894273235));
#59903=CARTESIAN_POINT('Ctrl Pts',(82.0421831982151,8.7730961714123,130.333597415899));
#59904=CARTESIAN_POINT('Ctrl Pts',(82.0343518468839,8.70261232718845,130.32972832049));
#59905=CARTESIAN_POINT('Ctrl Pts',(82.0228518584094,8.63239635192647,130.325859225081));
#59906=CARTESIAN_POINT('Ctrl Pts',(82.0077116911561,8.56286005936857,130.321990129672));
#59907=CARTESIAN_POINT('Ctrl Pts',(81.9925940814525,8.49342736991812,130.318126798884));
#59908=CARTESIAN_POINT('Ctrl Pts',(81.973847161083,8.4246728238438,130.314263468095));
#59909=CARTESIAN_POINT('Ctrl Pts',(81.9515510631405,8.35700232468914,130.310400137306));
#59910=CARTESIAN_POINT('Ctrl Pts',(81.9292811177576,8.28941120071327,130.306541338072));
#59911=CARTESIAN_POINT('Ctrl Pts',(81.9034704153359,8.22290205707025,130.302682538838));
#59912=CARTESIAN_POINT('Ctrl Pts',(81.8742495670342,8.15786810832739,130.298823739604));
#59913=CARTESIAN_POINT('Ctrl Pts',(81.8450471251758,8.09287512498284,130.294967371059));
#59914=CARTESIAN_POINT('Ctrl Pts',(81.8124389978158,8.02935593500499,130.291111002513));
#59915=CARTESIAN_POINT('Ctrl Pts',(81.7766042941104,7.96768476488599,130.287254633967));
#59916=CARTESIAN_POINT('Ctrl Pts',(81.7407801758834,7.90603181227041,130.283399404582));
#59917=CARTESIAN_POINT('Ctrl Pts',(81.7017316174486,7.84622621554188,130.279544175198));
#59918=CARTESIAN_POINT('Ctrl Pts',(81.6596833332211,7.78861699040805,130.275688945813));
#59919=CARTESIAN_POINT('Ctrl Pts',(81.6176334047604,7.7310055125544,130.271833565676));
#59920=CARTESIAN_POINT('Ctrl Pts',(81.5725838057957,7.67559096789019,130.267978185538));
#59921=CARTESIAN_POINT('Ctrl Pts',(81.5248011489136,7.62269138579189,130.264122805401));
#59922=CARTESIAN_POINT('Ctrl Pts',(81.4769684774253,7.56973643314834,130.260263389797));
#59923=CARTESIAN_POINT('Ctrl Pts',(81.426397363668,7.51930205923476,130.256403974193));
#59924=CARTESIAN_POINT('Ctrl Pts',(81.3733924916258,7.4716706420258,130.252544558589));
#59925=CARTESIAN_POINT('Ctrl Pts',(81.3203576080414,7.42401225574343,130.24868295777));
#59926=CARTESIAN_POINT('Ctrl Pts',(81.2648866009189,7.37916029105891,130.244821356952));
#59927=CARTESIAN_POINT('Ctrl Pts',(81.2073164228308,7.33735613625078,130.240959756133));
#59928=CARTESIAN_POINT('Ctrl Pts',(81.1496455263141,7.29547884550793,130.237091399484));
#59929=CARTESIAN_POINT('Ctrl Pts',(81.0898685341668,7.25666027500702,130.233223042835));
#59930=CARTESIAN_POINT('Ctrl Pts',(81.0283498764503,7.22109750292359,130.229354686186));
#59931=CARTESIAN_POINT('Ctrl Pts',(80.9918238201664,7.19998248086451,130.227057890093));
#59932=CARTESIAN_POINT('Ctrl Pts',(80.9546842397429,7.1800143268547,130.224761094));
#59933=CARTESIAN_POINT('Ctrl Pts',(80.9170107235692,7.16122625226509,130.222464297907));
#59934=CARTESIAN_POINT('Ctrl Pts',(80.8535484472579,7.12957712306075,130.218595269394));
#59935=CARTESIAN_POINT('Ctrl Pts',(80.7883214520981,7.10115529781342,130.21472624088));
#59936=CARTESIAN_POINT('Ctrl Pts',(80.7216911370353,7.07616022880679,130.210857212366));
#59937=CARTESIAN_POINT('Ctrl Pts',(80.6551601004848,7.05120240220646,130.206993948667));
#59938=CARTESIAN_POINT('Ctrl Pts',(80.5872303456127,7.02966136615534,130.203130684968));
#59939=CARTESIAN_POINT('Ctrl Pts',(80.5182863343939,7.01168995423737,130.199267421268));
#59940=CARTESIAN_POINT('Ctrl Pts',(80.4494231929077,6.99373962237048,130.195408689088));
#59941=CARTESIAN_POINT('Ctrl Pts',(80.379548626026,6.97935071961538,130.191549956908));
#59942=CARTESIAN_POINT('Ctrl Pts',(80.3090638144979,6.96862678932009,130.187691224728));
#59943=CARTESIAN_POINT('Ctrl Pts',(80.2386234016157,6.95790961406854,130.183834923177));
#59944=CARTESIAN_POINT('Ctrl Pts',(80.1675739858566,6.9508529039936,130.179978621627));
#59945=CARTESIAN_POINT('Ctrl Pts',(80.0963271004719,6.94750915904244,130.176122320077));
#59946=CARTESIAN_POINT('Ctrl Pts',(80.0251012587066,6.94416640170632,130.172267157531));
#59947=CARTESIAN_POINT('Ctrl Pts',(79.9536785481068,6.94453445506637,130.168411994985));
#59948=CARTESIAN_POINT('Ctrl Pts',(79.8824740573168,6.94861383077285,130.16455683244));
#59949=CARTESIAN_POINT('Ctrl Pts',(79.8112667774319,6.95269336626935,130.160701518887));
#59950=CARTESIAN_POINT('Ctrl Pts',(79.740278219204,6.96048448274595,130.156846205334));
#59951=CARTESIAN_POINT('Ctrl Pts',(79.6699201635377,6.97193568542291,130.15299089178));
#59952=CARTESIAN_POINT('Ctrl Pts',(79.5994884466511,6.98339887691275,130.149131541915));
#59953=CARTESIAN_POINT('Ctrl Pts',(79.5296890305112,6.99852972577124,130.145272192049));
#59954=CARTESIAN_POINT('Ctrl Pts',(79.4609243933277,7.01722541553738,130.141412842183));
#59955=CARTESIAN_POINT('Ctrl Pts',(79.3921208139723,7.03593169287869,130.137551306725));
#59956=CARTESIAN_POINT('Ctrl Pts',(79.3243536418541,7.05820667817763,130.133689771267));
#59957=CARTESIAN_POINT('Ctrl Pts',(79.2580084198717,7.08389821316334,130.129828235809));
#59958=CARTESIAN_POINT('Ctrl Pts',(79.1915471032066,7.1096347046736,130.125959943215));
#59959=CARTESIAN_POINT('Ctrl Pts',(79.1265131478625,7.13879948321254,130.12209165062));
#59960=CARTESIAN_POINT('Ctrl Pts',(79.0632697732558,7.17119327297723,130.118223358025));
#59961=CARTESIAN_POINT('Ctrl Pts',(79.025709308585,7.1904320597051,130.115925965322));
#59962=CARTESIAN_POINT('Ctrl Pts',(78.9887799235412,7.21080892047137,130.113628572619));
#59963=CARTESIAN_POINT('Ctrl Pts',(78.9525527429518,7.23227496306631,130.111331179916));
#59964=CARTESIAN_POINT('Ctrl Pts',(78.8915407851485,7.26842697003174,130.107462029063));
#59965=CARTESIAN_POINT('Ctrl Pts',(78.8322831878937,7.30781216979145,130.103592878211));
#59966=CARTESIAN_POINT('Ctrl Pts',(78.7751435465107,7.3502350983108,130.099723727359));
#59967=CARTESIAN_POINT('Ctrl Pts',(78.7180890438663,7.392594816167,130.095860341587));
#59968=CARTESIAN_POINT('Ctrl Pts',(78.6631466197984,7.43798299107895,130.091996955814));
#59969=CARTESIAN_POINT('Ctrl Pts',(78.6106532113617,7.48615949869204,130.088133570042));
#59970=CARTESIAN_POINT('Ctrl Pts',(78.5582213877529,7.53427948602916,130.084274716762));
#59971=CARTESIAN_POINT('Ctrl Pts',(78.5082332288406,7.58518098138821,130.080415863482));
#59972=CARTESIAN_POINT('Ctrl Pts',(78.4609933282997,7.63858308113869,130.076557010202));
#59973=CARTESIAN_POINT('Ctrl Pts',(78.4137831915473,7.69195153456925,130.072700588216));
#59974=CARTESIAN_POINT('Ctrl Pts',(78.3693181988724,7.74781710360056,130.06884416623));
#59975=CARTESIAN_POINT('Ctrl Pts',(78.3278656752727,7.80586250265354,130.064987744243));
#59976=CARTESIAN_POINT('Ctrl Pts',(78.2864254037727,7.8638907452598,130.061132462098));
#59977=CARTESIAN_POINT('Ctrl Pts',(78.24799611582,7.9240971436945,130.057277179952));
#59978=CARTESIAN_POINT('Ctrl Pts',(78.2128033876072,7.98613322810559,130.053421897807));
#59979=CARTESIAN_POINT('Ctrl Pts',(78.1776092901316,8.04817172618856,130.049566465662));
#59980=CARTESIAN_POINT('Ctrl Pts',(78.1456522401799,8.11203962798427,130.045711033517));
#59981=CARTESIAN_POINT('Ctrl Pts',(78.1171123277082,8.17736303509301,130.041855601371));
#59982=CARTESIAN_POINT('Ctrl Pts',(78.0885425536903,8.24275479062207,130.037996135256));
#59983=CARTESIAN_POINT('Ctrl Pts',(78.0633972492933,8.30960464548333,130.03413666914));
#59984=CARTESIAN_POINT('Ctrl Pts',(78.0418083419939,8.37751868058912,130.030277203025));
#59985=CARTESIAN_POINT('Ctrl Pts',(78.0202072154328,8.44547115485051,130.026415552462));
#59986=CARTESIAN_POINT('Ctrl Pts',(78.0021666159711,8.5144885382013,130.022553901899));
#59987=CARTESIAN_POINT('Ctrl Pts',(77.9877678323499,8.58416437625648,130.018692251336));
#59988=CARTESIAN_POINT('Ctrl Pts',(77.9733438650333,8.65396207843101,130.014823846687));
#59989=CARTESIAN_POINT('Ctrl Pts',(77.9625745040558,8.72442005426722,130.010955442038));
#59990=CARTESIAN_POINT('Ctrl Pts',(77.9554893455248,8.79512504731584,130.007087037388));
#59991=CARTESIAN_POINT('Ctrl Pts',(77.9512835218753,8.83709626512267,130.004790712234));
#59992=CARTESIAN_POINT('Ctrl Pts',(77.9483749151369,8.87915447197554,130.002494387079));
#59993=CARTESIAN_POINT('Ctrl Pts',(77.9467610336869,8.92121351820568,130.000198061924));
#59994=CARTESIAN_POINT('Ctrl Pts',(77.9457600484671,8.94729999663671,129.998773801462));
#59995=CARTESIAN_POINT('Ctrl Pts',(77.9452561844405,8.97340567540233,129.997349541));
#59996=CARTESIAN_POINT('Ctrl Pts',(77.9452500565799,8.99951780177073,129.995925280538));
#59997=CARTESIAN_POINT('Ctrl Pts',(77.9452500565798,8.99951780232931,129.995925280508));
#59998=CARTESIAN_POINT('Ctrl Pts',(77.9452335129583,9.07001379864739,129.992080145153));
#59999=CARTESIAN_POINT('Ctrl Pts',(77.9488491930074,9.14065511061305,129.988235009798));
#60000=CARTESIAN_POINT('Ctrl Pts',(77.9561158549005,9.2110335611009,129.984389874443));
#60001=CARTESIAN_POINT('Ctrl Pts',(77.9636220280264,9.28373170523678,129.980418002338));
#60002=CARTESIAN_POINT('Ctrl Pts',(77.975024177992,9.35614883199943,129.976446130233));
#60003=CARTESIAN_POINT('Ctrl Pts',(77.9902844919774,9.4278330741228,129.972474258129));
#60004=CARTESIAN_POINT('Ctrl Pts',(78.0050192001863,9.49704832040622,129.968639187857));
#60005=CARTESIAN_POINT('Ctrl Pts',(78.02335052537,9.56557981566392,129.964804117585));
#60006=CARTESIAN_POINT('Ctrl Pts',(78.0451918512736,9.63302659041542,129.960969047313));
#60007=CARTESIAN_POINT('Ctrl Pts',(78.0670205775869,9.70043445719311,129.957136189376));
#60008=CARTESIAN_POINT('Ctrl Pts',(78.0923551372306,9.76675837705386,129.953303331438));
#60009=CARTESIAN_POINT('Ctrl Pts',(78.1210586664692,9.83161110361127,129.949470473501));
#60010=CARTESIAN_POINT('Ctrl Pts',(78.1497555410476,9.89644879463568,129.945638504178));
#60011=CARTESIAN_POINT('Ctrl Pts',(78.1818196352711,9.95981551941986,129.941806534854));
#60012=CARTESIAN_POINT('Ctrl Pts',(78.2170660925413,10.0213443318167,129.937974565531));
#60013=CARTESIAN_POINT('Ctrl Pts',(78.2523165391549,10.0828801083052,129.934142162489));
#60014=CARTESIAN_POINT('Ctrl Pts',(78.2907498162761,10.1425771338496,129.930309759448));
#60015=CARTESIAN_POINT('Ctrl Pts',(78.3321362084666,10.200094969322,129.926477356406));
#60016=CARTESIAN_POINT('Ctrl Pts',(78.373567411324,10.2576750816064,129.922640803871));
#60017=CARTESIAN_POINT('Ctrl Pts',(78.4179578187722,10.3130708973975,129.918804251337));
#60018=CARTESIAN_POINT('Ctrl Pts',(78.4650362908378,10.3659736359297,129.914967698802));
#60019=CARTESIAN_POINT('Ctrl Pts',(78.5121454499549,10.4189108579316,129.911128645497));
#60020=CARTESIAN_POINT('Ctrl Pts',(78.5619458123617,10.4693514211948,129.907289592191));
#60021=CARTESIAN_POINT('Ctrl Pts',(78.6141300837946,10.5170241058919,129.903450538885));
#60022=CARTESIAN_POINT('Ctrl Pts',(78.6664000026858,10.5647750334034,129.899605184732));
#60023=CARTESIAN_POINT('Ctrl Pts',(78.7210612535677,10.6097487117794,129.895759830578));
#60024=CARTESIAN_POINT('Ctrl Pts',(78.7777751229153,10.6517154453281,129.891914476425));
#60025=CARTESIAN_POINT('Ctrl Pts',(78.7917840634903,10.6620816834842,129.890964632261));
#60026=CARTESIAN_POINT('Ctrl Pts',(78.8059181176275,10.6722646699556,129.890014788096));
#60027=CARTESIAN_POINT('Ctrl Pts',(78.820171946148,10.6822613726303,129.889064943932));
#60028=CARTESIAN_POINT('Ctrl Pts',(78.8782264933528,10.7229770334427,129.885196315038));
#60029=CARTESIAN_POINT('Ctrl Pts',(78.938505015448,10.7607638442889,129.881327686144));
#60030=CARTESIAN_POINT('Ctrl Pts',(79.0006798143163,10.7953709168261,129.87745905725));
#60031=CARTESIAN_POINT('Ctrl Pts',(79.0627619499484,10.8299264121425,129.873596194031));
#60032=CARTESIAN_POINT('Ctrl Pts',(79.1267343314652,10.8613113414234,129.869733330812));
#60033=CARTESIAN_POINT('Ctrl Pts',(79.192239527078,10.8893174907582,129.865870467592));
#60034=CARTESIAN_POINT('Ctrl Pts',(79.2576678896478,10.9172907908258,129.862012135243));
#60035=CARTESIAN_POINT('Ctrl Pts',(79.32462505052,10.9418929927971,129.858153802894));
#60036=CARTESIAN_POINT('Ctrl Pts',(79.3927297221528,10.9629621423103,129.854295470545));
#60037=CARTESIAN_POINT('Ctrl Pts',(79.4607915008078,10.9840180222703,129.850439568211));
#60038=CARTESIAN_POINT('Ctrl Pts',(79.5299988932787,11.0015451211287,129.846583665877));
#60039=CARTESIAN_POINT('Ctrl Pts',(79.599952793044,11.0154304241791,129.842727763542));
#60040=CARTESIAN_POINT('Ctrl Pts',(79.6698860506518,11.0293116299224,129.838872999017));
#60041=CARTESIAN_POINT('Ctrl Pts',(79.7405649018862,11.0395530787255,129.835018234491));
#60042=CARTESIAN_POINT('Ctrl Pts',(79.8115790040935,11.0460926398386,129.831163469965));
#60043=CARTESIAN_POINT('Ctrl Pts',(79.8825959209901,11.0526324601514,129.827308552654));
#60044=CARTESIAN_POINT('Ctrl Pts',(79.9539476311761,11.0554700591059,129.823453635342));
#60045=CARTESIAN_POINT('Ctrl Pts',(80.0252193417206,11.0545952271197,129.81959871803));
#60046=CARTESIAN_POINT('Ctrl Pts',(80.0965657780592,11.0537194779041,129.815739758978));
#60047=CARTESIAN_POINT('Ctrl Pts',(80.1678315604504,11.0491235337427,129.811880799926));
#60048=CARTESIAN_POINT('Ctrl Pts',(80.2386034764512,11.0408493191623,129.808021840873));
#60049=CARTESIAN_POINT('Ctrl Pts',(80.3094155207289,11.0325704130321,129.804160693759));
#60050=CARTESIAN_POINT('Ctrl Pts',(80.3797326619261,11.0206091662598,129.800299546644));
#60051=CARTESIAN_POINT('Ctrl Pts',(80.4491511126179,11.0050588122382,129.796438399529));
#60052=CARTESIAN_POINT('Ctrl Pts',(80.5186911937878,10.9894812119013,129.792570487164));
#60053=CARTESIAN_POINT('Ctrl Pts',(80.5873289725487,10.9703020797991,129.7887025748));
#60054=CARTESIAN_POINT('Ctrl Pts',(80.6546757450919,10.9476645582051,129.784834662435));
#60055=CARTESIAN_POINT('Ctrl Pts',(80.6947390243179,10.9341979388801,129.782533716937));
#60056=CARTESIAN_POINT('Ctrl Pts',(80.7343458013838,10.9195083881302,129.780232771439));
#60057=CARTESIAN_POINT('Ctrl Pts',(80.7734181170445,10.903633887786,129.777931825941));
#60058=CARTESIAN_POINT('Ctrl Pts',(80.8391271583217,10.8769372822551,129.774062259468));
#60059=CARTESIAN_POINT('Ctrl Pts',(80.903580819736,10.8467822905527,129.770192692995));
#60060=CARTESIAN_POINT('Ctrl Pts',(80.9663904970254,10.8133082941847,129.766323126522));
#60061=CARTESIAN_POINT('Ctrl Pts',(81.0291002039768,10.779887576338,129.762459719002));
#60062=CARTESIAN_POINT('Ctrl Pts',(81.0901706983107,10.74315857112,129.758596311482));
#60063=CARTESIAN_POINT('Ctrl Pts',(81.1492332216771,10.7033087109193,129.754732903962));
#60064=CARTESIAN_POINT('Ctrl Pts',(81.1842307580926,10.6796956504872,129.752443639338));
#60065=CARTESIAN_POINT('Ctrl Pts',(81.218523639527,10.6549877240144,129.750154374714));
#60066=CARTESIAN_POINT('Ctrl Pts',(81.252039109102,10.6292316077768,129.74786511009));
#60067=CARTESIAN_POINT('',(77.9452500005989,8.99995038927704,130.054074719503));
#60068=CARTESIAN_POINT('Ctrl Pts',(77.9452500005989,8.99995039003008,130.054074719462));
#60069=CARTESIAN_POINT('Ctrl Pts',(77.9452481959203,9.07469672239711,130.050044138511));
#60070=CARTESIAN_POINT('Ctrl Pts',(77.9493293030444,9.14936770606286,130.04601355756));
#60071=CARTESIAN_POINT('Ctrl Pts',(77.9574429752524,9.22351367554211,130.041982976609));
#60072=CARTESIAN_POINT('Ctrl Pts',(77.965578494409,9.2978592911421,130.037941542879));
#60073=CARTESIAN_POINT('Ctrl Pts',(77.9777682288688,9.37167665110889,130.033900109149));
#60074=CARTESIAN_POINT('Ctrl Pts',(77.9939102839952,9.44452403066627,130.029858675418));
#60075=CARTESIAN_POINT('Ctrl Pts',(78.0100750993415,9.51747412467749,130.025811543286));
#60076=CARTESIAN_POINT('Ctrl Pts',(78.0302032317879,9.58945110973448,130.021764411154));
#60077=CARTESIAN_POINT('Ctrl Pts',(78.0541430533931,9.66002901893903,130.017717279021));
#60078=CARTESIAN_POINT('Ctrl Pts',(78.0781473934775,9.73079713755454,130.013659239756));
#60079=CARTESIAN_POINT('Ctrl Pts',(78.1059837999931,9.80015825502306,130.009601200491));
#60080=CARTESIAN_POINT('Ctrl Pts',(78.1374525208473,9.8677064310018,130.005543161226));
#60081=CARTESIAN_POINT('Ctrl Pts',(78.1569006444202,9.90945217845837,130.003035234404));
#60082=CARTESIAN_POINT('Ctrl Pts',(78.1777351870459,9.95050597400759,130.000527307582));
#60083=CARTESIAN_POINT('Ctrl Pts',(78.1999006273473,9.99077737715166,129.99801938076));
#60084=CARTESIAN_POINT('Ctrl Pts',(78.2340956916408,10.0529048693632,129.994150352319));
#60085=CARTESIAN_POINT('Ctrl Pts',(78.2715778611207,10.1133817065652,129.990281323878));
#60086=CARTESIAN_POINT('Ctrl Pts',(78.3121633370003,10.1718382830126,129.986412295437));
#60087=CARTESIAN_POINT('Ctrl Pts',(78.3526883409194,10.2302077597351,129.982549031811));
#60088=CARTESIAN_POINT('Ctrl Pts',(78.3963071981439,10.2865625550009,129.978685768185));
#60089=CARTESIAN_POINT('Ctrl Pts',(78.4427906247499,10.3405582882267,129.974822504558));
#60090=CARTESIAN_POINT('Ctrl Pts',(78.4892195273723,10.394490685707,129.970963772451));
#60091=CARTESIAN_POINT('Ctrl Pts',(78.5385060097335,10.44606915121,129.967105040343));
#60092=CARTESIAN_POINT('Ctrl Pts',(78.5903790012833,10.4949803351472,129.963246308236));
#60093=CARTESIAN_POINT('Ctrl Pts',(78.642219317844,10.5438607097489,129.959390006758));
#60094=CARTESIAN_POINT('Ctrl Pts',(78.6966425585689,10.5900768036493,129.95553370528));
#60095=CARTESIAN_POINT('Ctrl Pts',(78.7533401052594,10.6333513612647,129.951677403802));
#60096=CARTESIAN_POINT('Ctrl Pts',(78.8100209056556,10.6766131372252,129.947822241329));
#60097=CARTESIAN_POINT('Ctrl Pts',(78.8689742924639,10.7169348071598,129.943967078855));
#60098=CARTESIAN_POINT('Ctrl Pts',(78.9298591529066,10.7540798527668,129.940111916382));
#60099=CARTESIAN_POINT('Ctrl Pts',(78.9907463982287,10.791226353357,129.9362566029));
#60100=CARTESIAN_POINT('Ctrl Pts',(79.0535648515318,10.8251957314521,129.932401289419));
#60101=CARTESIAN_POINT('Ctrl Pts',(79.1179465399631,10.8557961246152,129.928545975937));
#60102=CARTESIAN_POINT('Ctrl Pts',(79.182395632689,10.8864285548058,129.924686626142));
#60103=CARTESIAN_POINT('Ctrl Pts',(79.2484107879555,10.9136847501106,129.920827276347));
#60104=CARTESIAN_POINT('Ctrl Pts',(79.3156024930666,10.9374203506218,129.916967926552));
#60105=CARTESIAN_POINT('Ctrl Pts',(79.3828322495905,10.9611693928685,129.913106391164));
#60106=CARTESIAN_POINT('Ctrl Pts',(79.451239416256,10.9813937335869,129.909244855777));
#60107=CARTESIAN_POINT('Ctrl Pts',(79.520420344357,10.9979992283265,129.905383320389));
#60108=CARTESIAN_POINT('Ctrl Pts',(79.5897223292526,11.0146337803225,129.901515027863));
#60109=CARTESIAN_POINT('Ctrl Pts',(79.6598003010311,11.0276367547423,129.897646735336));
#60110=CARTESIAN_POINT('Ctrl Pts',(79.7302421718041,11.0369654578876,129.89377844281));
#60111=CARTESIAN_POINT('Ctrl Pts',(79.7720778613746,11.0425058094512,129.891481049463));
#60112=CARTESIAN_POINT('Ctrl Pts',(79.8140418210399,11.0467511619059,129.889183656115));
#60113=CARTESIAN_POINT('Ctrl Pts',(79.8560477423787,11.049701273363,129.886886262768));
#60114=CARTESIAN_POINT('Ctrl Pts',(79.9267744983491,11.0546684733781,129.883018065774));
#60115=CARTESIAN_POINT('Ctrl Pts',(79.9978971266534,11.0559803693969,129.87914986878));
#60116=CARTESIAN_POINT('Ctrl Pts',(80.0690057026482,11.0535909464891,129.875281671786));
#60117=CARTESIAN_POINT('Ctrl Pts',(80.1400164914646,11.0512048094708,129.871418794264));
#60118=CARTESIAN_POINT('Ctrl Pts',(80.2110127852759,11.0451274670466,129.867555916742));
#60119=CARTESIAN_POINT('Ctrl Pts',(80.2815810425782,11.0353647532962,129.86369303922));
#60120=CARTESIAN_POINT('Ctrl Pts',(80.3520758688713,11.0256121983049,129.859834181281));
#60121=CARTESIAN_POINT('Ctrl Pts',(80.422143063926,11.0121819488409,129.855975323343));
#60122=CARTESIAN_POINT('Ctrl Pts',(80.4913723260528,10.9951317750188,129.852116465404));
#60123=CARTESIAN_POINT('Ctrl Pts',(80.5605648373335,10.9780906524026,129.848259655968));
#60124=CARTESIAN_POINT('Ctrl Pts',(80.6289198260969,10.9574335277133,129.844402846531));
#60125=CARTESIAN_POINT('Ctrl Pts',(80.6960368287023,10.9332693282598,129.840546037095));
#60126=CARTESIAN_POINT('Ctrl Pts',(80.7631293959301,10.9091139262989,129.836690631812));
#60127=CARTESIAN_POINT('Ctrl Pts',(80.8289844162549,10.881454152868,129.832835226529));
#60128=CARTESIAN_POINT('Ctrl Pts',(80.8932181094343,10.850448316349,129.828979821247));
#60129=CARTESIAN_POINT('Ctrl Pts',(80.9574849801847,10.8194264648961,129.825122424595));
#60130=CARTESIAN_POINT('Ctrl Pts',(81.0201284102717,10.7850553046203,129.821265027943));
#60131=CARTESIAN_POINT('Ctrl Pts',(81.0807870582173,10.7475402419659,129.817407631292));
#60132=CARTESIAN_POINT('Ctrl Pts',(81.1398557484067,10.711008507606,129.813651343022));
#60133=CARTESIAN_POINT('Ctrl Pts',(81.1970420974188,10.6714959544679,129.809895054752));
#60134=CARTESIAN_POINT('Ctrl Pts',(81.252039109102,10.6292316077768,129.806138766482));
#60135=CARTESIAN_POINT('Ctrl Pts',(81.252039109102,10.6292316077768,130.506052881431));
#60136=CARTESIAN_POINT('Ctrl Pts',(81.3085807231097,10.5857802582625,130.50219771152));
#60137=CARTESIAN_POINT('Ctrl Pts',(81.3628732049477,10.5393702223445,130.498342541608));
#60138=CARTESIAN_POINT('Ctrl Pts',(81.4145999473004,10.4902699593019,130.494487371696));
#60139=CARTESIAN_POINT('Ctrl Pts',(81.4663306408243,10.441165945713,130.490631907306));
#60140=CARTESIAN_POINT('Ctrl Pts',(81.5154948550975,10.3893716331966,130.486776442915));
#60141=CARTESIAN_POINT('Ctrl Pts',(81.561812210644,10.3351929378121,130.482920978525));
#60142=CARTESIAN_POINT('Ctrl Pts',(81.6081791199772,10.280956277989,130.479061389268));
#60143=CARTESIAN_POINT('Ctrl Pts',(81.6516927756994,10.2243305140825,130.475201800012));
#60144=CARTESIAN_POINT('Ctrl Pts',(81.6921131545386,10.1656545949541,130.471342210756));
#60145=CARTESIAN_POINT('Ctrl Pts',(81.7325577712789,10.1069434910705,130.467480307115));
#60146=CARTESIAN_POINT('Ctrl Pts',(81.7699051651171,10.0461801991002,130.463618403473));
#60147=CARTESIAN_POINT('Ctrl Pts',(81.803960185088,9.98373025424512,130.459756499831));
#60148=CARTESIAN_POINT('Ctrl Pts',(81.8380736276579,9.9211731742867,130.455887970957));
#60149=CARTESIAN_POINT('Ctrl Pts',(81.8688832130284,9.85692410394344,130.452019442082));
#60150=CARTESIAN_POINT('Ctrl Pts',(81.896241347074,9.79136989843372,130.448150913207));
#60151=CARTESIAN_POINT('Ctrl Pts',(81.9094401496965,9.75974358144321,130.446284559713));
#60152=CARTESIAN_POINT('Ctrl Pts',(81.921836354179,9.72781373601789,130.44441820622));
#60153=CARTESIAN_POINT('Ctrl Pts',(81.9334175758377,9.69562492763128,130.442551852726));
#60154=CARTESIAN_POINT('Ctrl Pts',(81.9574262793351,9.62889521816968,130.438682768015));
#60155=CARTESIAN_POINT('Ctrl Pts',(81.9780233007368,9.56079040286018,130.434813683304));
#60156=CARTESIAN_POINT('Ctrl Pts',(81.9950528338149,9.49169274225609,130.430944598593));
#60157=CARTESIAN_POINT('Ctrl Pts',(82.0120569938088,9.4226980334326,130.42708127861));
#60158=CARTESIAN_POINT('Ctrl Pts',(82.025504101033,9.35271388348272,130.423217958626));
#60159=CARTESIAN_POINT('Ctrl Pts',(82.0352873460187,9.28214000360805,130.419354638642));
#60160=CARTESIAN_POINT('Ctrl Pts',(82.0450591152943,9.21164890663373,130.415495850318));
#60161=CARTESIAN_POINT('Ctrl Pts',(82.0511754926331,9.14056993263242,130.411637061995));
#60162=CARTESIAN_POINT('Ctrl Pts',(82.0535805762484,9.06931363037274,130.407778273671));
#60163=CARTESIAN_POINT('Ctrl Pts',(82.0559841448415,8.99810221423524,130.403921916095));
#60164=CARTESIAN_POINT('Ctrl Pts',(82.0546810415938,8.92671417581581,130.400065558518));
#60165=CARTESIAN_POINT('Ctrl Pts',(82.0496672687178,8.85556437403794,130.396209200941));
#60166=CARTESIAN_POINT('Ctrl Pts',(82.0446549769562,8.78443559056478,130.392353982568));
#60167=CARTESIAN_POINT('Ctrl Pts',(82.0359342258887,8.71354538833167,130.388498764195));
#60168=CARTESIAN_POINT('Ctrl Pts',(82.0235530649906,8.64330607565128,130.384643545822));
#60169=CARTESIAN_POINT('Ctrl Pts',(82.0111714200269,8.57306401682869,130.380788176721));
#60170=CARTESIAN_POINT('Ctrl Pts',(81.9951291676038,8.50347337610662,130.376932807621));
#60171=CARTESIAN_POINT('Ctrl Pts',(81.9755256196588,8.43493709326139,130.37307743852));
#60172=CARTESIAN_POINT('Ctrl Pts',(81.9559015522231,8.36632907189102,130.369218033915));
#60173=CARTESIAN_POINT('Ctrl Pts',(81.9327088818243,8.2987780794815,130.36535862931));
#60174=CARTESIAN_POINT('Ctrl Pts',(81.9060968015639,8.23267181364955,130.361499224705));
#60175=CARTESIAN_POINT('Ctrl Pts',(81.8794696533747,8.16652811803004,130.35763763488));
#60176=CARTESIAN_POINT('Ctrl Pts',(81.8494194458972,8.10183121818607,130.353776045056));
#60177=CARTESIAN_POINT('Ctrl Pts',(81.8161423944517,8.03894622128876,130.349914455231));
#60178=CARTESIAN_POINT('Ctrl Pts',(81.7828071238814,7.97595120534435,130.346046109448));
#60179=CARTESIAN_POINT('Ctrl Pts',(81.746233987383,7.91477483837574,130.342177763665));
#60180=CARTESIAN_POINT('Ctrl Pts',(81.7066633832417,7.85575454608636,130.338309417882));
#60181=CARTESIAN_POINT('Ctrl Pts',(81.6831676816,7.82071026994933,130.336012523499));
#60182=CARTESIAN_POINT('Ctrl Pts',(81.6586159997449,7.78642554225776,130.333715629117));
#60183=CARTESIAN_POINT('Ctrl Pts',(81.6330651749068,7.75296523825247,130.331418734734));
#60184=CARTESIAN_POINT('Ctrl Pts',(81.5900252788846,7.6966019695759,130.327549658255));
#60185=CARTESIAN_POINT('Ctrl Pts',(81.5439796920784,7.64235912550215,130.323680581776));
#60186=CARTESIAN_POINT('Ctrl Pts',(81.495165056335,7.59057493394831,130.319811505297));
#60187=CARTESIAN_POINT('Ctrl Pts',(81.4464231521381,7.53886789844155,130.315948193563));
#60188=CARTESIAN_POINT('Ctrl Pts',(81.3949207190144,7.48961259455697,130.312084881829));
#60189=CARTESIAN_POINT('Ctrl Pts',(81.3409356346372,7.44311555141037,130.308221570095));
#60190=CARTESIAN_POINT('Ctrl Pts',(81.2870138745101,7.39667304907682,130.304362790007));
#60191=CARTESIAN_POINT('Ctrl Pts',(81.2306156139143,7.35298269631473,130.300504009919));
#60192=CARTESIAN_POINT('Ctrl Pts',(81.1720554469248,7.3123141311743,130.296645229832));
#60193=CARTESIAN_POINT('Ctrl Pts',(81.1135321683292,7.27167118409694,130.292788880478));
#60194=CARTESIAN_POINT('Ctrl Pts',(81.052850083258,7.23404652458339,130.288932531125));
#60195=CARTESIAN_POINT('Ctrl Pts',(80.9903555586582,7.19966852220633,130.285076181771));
#60196=CARTESIAN_POINT('Ctrl Pts',(80.9278794951522,7.16530067520734,130.281220971596));
#60197=CARTESIAN_POINT('Ctrl Pts',(80.8635924804399,7.1341778153307,130.277365761421));
#60198=CARTESIAN_POINT('Ctrl Pts',(80.7978669680663,7.10648320214244,130.273510551246));
#60199=CARTESIAN_POINT('Ctrl Pts',(80.7321388853924,7.07878750591246,130.269655190307));
#60200=CARTESIAN_POINT('Ctrl Pts',(80.6649726418922,7.05452050914529,130.265799829368));
#60201=CARTESIAN_POINT('Ctrl Pts',(80.5967606240574,7.03381732281188,130.261944468429));
#60202=CARTESIAN_POINT('Ctrl Pts',(80.528477204978,7.01309246532262,130.258085071874));
#60203=CARTESIAN_POINT('Ctrl Pts',(80.4591462921572,6.99593900642655,130.254225675318));
#60204=CARTESIAN_POINT('Ctrl Pts',(80.389174521208,6.98244188323049,130.250366278762));
#60205=CARTESIAN_POINT('Ctrl Pts',(80.3191631307887,6.96893711768293,130.246504696936));
#60206=CARTESIAN_POINT('Ctrl Pts',(80.2485106412491,6.95909287621989,130.242643115109));
#60207=CARTESIAN_POINT('Ctrl Pts',(80.177630213097,6.95294233840492,130.238781533283));
#60208=CARTESIAN_POINT('Ctrl Pts',(80.1066257743388,6.9467810397644,130.234913195331));
#60209=CARTESIAN_POINT('Ctrl Pts',(80.0353930864115,6.94432636389211,130.231044857378));
#60210=CARTESIAN_POINT('Ctrl Pts',(79.9643460176259,6.9455593568952,130.227176519426));
#60211=CARTESIAN_POINT('Ctrl Pts',(79.9221592143221,6.94629149172054,130.224879551865));
#60212=CARTESIAN_POINT('Ctrl Pts',(79.8800377932647,6.94832283725827,130.222582584304));
#60213=CARTESIAN_POINT('Ctrl Pts',(79.8380670940032,6.95164082825901,130.220285616743));
#60214=CARTESIAN_POINT('Ctrl Pts',(79.7673702408721,6.95722976355429,130.216416527565));
#60215=CARTESIAN_POINT('Ctrl Pts',(79.6968246045509,6.96649397761275,130.212547438387));
#60216=CARTESIAN_POINT('Ctrl Pts',(79.6268426934916,6.97941810680701,130.208678349209));
#60217=CARTESIAN_POINT('Ctrl Pts',(79.5569650526557,6.9923229795703,130.204815024817));
#60218=CARTESIAN_POINT('Ctrl Pts',(79.4876499436599,7.0088768556617,130.200951700426));
#60219=CARTESIAN_POINT('Ctrl Pts',(79.4193056091046,7.02901253507726,130.197088376034));
#60220=CARTESIAN_POINT('Ctrl Pts',(79.3510414440278,7.04912459487707,130.193229583412));
#60221=CARTESIAN_POINT('Ctrl Pts',(79.2837462551835,7.07280997570245,130.189370790789));
#60222=CARTESIAN_POINT('Ctrl Pts',(79.217817205908,7.09995062192413,130.185511998166));
#60223=CARTESIAN_POINT('Ctrl Pts',(79.1519296881186,7.12707417110922,130.181655636359));
#60224=CARTESIAN_POINT('Ctrl Pts',(79.0874070506485,7.15764848282999,130.177799274552));
#60225=CARTESIAN_POINT('Ctrl Pts',(79.0246290187541,7.19150642482661,130.173942912745));
#60226=CARTESIAN_POINT('Ctrl Pts',(78.9618695332617,7.22535436423186,130.170087690217));
#60227=CARTESIAN_POINT('Ctrl Pts',(78.9008540574504,7.2624837775702,130.166232467688));
#60228=CARTESIAN_POINT('Ctrl Pts',(78.8419385670213,7.30268114959286,130.162377245159));
#60229=CARTESIAN_POINT('Ctrl Pts',(78.783020774407,7.3428800923705,130.158521871984));
#60230=CARTESIAN_POINT('Ctrl Pts',(78.726203530129,7.3861469562388,130.154666498808));
#60231=CARTESIAN_POINT('Ctrl Pts',(78.6718131699329,7.43222536474902,130.150811125632));
#60232=CARTESIAN_POINT('Ctrl Pts',(78.6173658802461,7.47835200276759,130.146951717101));
#60233=CARTESIAN_POINT('Ctrl Pts',(78.5653509168195,7.52729574525971,130.14309230857));
#60234=CARTESIAN_POINT('Ctrl Pts',(78.5160601911565,7.57876103127255,130.139232900039));
#60235=CARTESIAN_POINT('Ctrl Pts',(78.4667415577998,7.63025545618356,130.135371306367));
#60236=CARTESIAN_POINT('Ctrl Pts',(78.4201505501253,7.68427389861833,130.131509712695));
#60237=CARTESIAN_POINT('Ctrl Pts',(78.3765391354799,7.74048724346613,130.127648119023));
#60238=CARTESIAN_POINT('Ctrl Pts',(78.3328514233877,7.79679893262852,130.123779769557));
#60239=CARTESIAN_POINT('Ctrl Pts',(78.2921539891894,7.85531279183206,130.11991142009));
#60240=CARTESIAN_POINT('Ctrl Pts',(78.2546553851637,7.91567083504972,130.116043070624));
#60241=CARTESIAN_POINT('Ctrl Pts',(78.2323903486635,7.95150881009529,130.113746213333));
#60242=CARTESIAN_POINT('Ctrl Pts',(78.2112521766875,7.98799645884686,130.111449356042));
#60243=CARTESIAN_POINT('Ctrl Pts',(78.1912765943839,8.02505528132276,130.109152498751));
#60244=CARTESIAN_POINT('Ctrl Pts',(78.1558306636805,8.09081478877886,130.105076810587));
#60245=CARTESIAN_POINT('Ctrl Pts',(78.1239212018672,8.15860872697479,130.101001122422));
#60246=CARTESIAN_POINT('Ctrl Pts',(78.0957732939045,8.22804260849929,130.096925434258));
#60247=CARTESIAN_POINT('Ctrl Pts',(78.0677085507005,8.29727134326781,130.092861787969));
#60248=CARTESIAN_POINT('Ctrl Pts',(78.0433833815485,8.36812999422939,130.088798141681));
#60249=CARTESIAN_POINT('Ctrl Pts',(78.0229762169732,8.4402013541938,130.084734495393));
#60250=CARTESIAN_POINT('Ctrl Pts',(78.0026057685371,8.5121430448907,130.080678160331));
#60251=CARTESIAN_POINT('Ctrl Pts',(77.9861394179251,8.58529271403991,130.076621825269));
#60252=CARTESIAN_POINT('Ctrl Pts',(77.9737071027707,8.65921464653235,130.072565490207));
#60253=CARTESIAN_POINT('Ctrl Pts',(77.9613030306111,8.73296864757114,130.068518370086));
#60254=CARTESIAN_POINT('Ctrl Pts',(77.9529148138812,8.80749101628244,130.064471249965));
#60255=CARTESIAN_POINT('Ctrl Pts',(77.9486218581135,8.88233402577495,130.060424129845));
#60256=CARTESIAN_POINT('Ctrl Pts',(77.9463768265079,8.92147370735203,130.058307659731));
#60257=CARTESIAN_POINT('Ctrl Pts',(77.9452509482554,8.96070086656248,130.056191189617));
#60258=CARTESIAN_POINT('Ctrl Pts',(77.9452500005989,8.99995038927706,130.054074719503));
#60259=CARTESIAN_POINT('Origin',(80.,9.,141.545925280538));
#60260=CARTESIAN_POINT('',(81.252039109102,10.6292316077768,131.206019331793));
#60261=CARTESIAN_POINT('',(81.252039109102,10.6292316077768,131.147979658073));
#60262=CARTESIAN_POINT('',(81.252039109102,10.6292316077768,141.545925280538));
#60263=CARTESIAN_POINT('',(77.9452508472645,9.00186596700246,130.695925280507));
#60264=CARTESIAN_POINT('Ctrl Pts',(81.252039109102,10.6292316077768,131.147979658073));
#60265=CARTESIAN_POINT('Ctrl Pts',(81.3086037731427,10.5857625446712,131.144119415786));
#60266=CARTESIAN_POINT('Ctrl Pts',(81.3628640477792,10.5393734651264,131.1402591735));
#60267=CARTESIAN_POINT('Ctrl Pts',(81.4145173023013,10.4903484035588,131.136398931214));
#60268=CARTESIAN_POINT('Ctrl Pts',(81.4662067786891,10.4412889631469,131.132535981931));
#60269=CARTESIAN_POINT('Ctrl Pts',(81.5152852644682,10.3895902156041,131.128673032648));
#60270=CARTESIAN_POINT('Ctrl Pts',(81.5614888507507,10.3355710881422,131.124810083366));
#60271=CARTESIAN_POINT('Ctrl Pts',(81.6077671726066,10.2814645832537,131.120940885656));
#60272=CARTESIAN_POINT('Ctrl Pts',(81.65116102721,10.2250305980703,131.117071687946));
#60273=CARTESIAN_POINT('Ctrl Pts',(81.6914490135609,10.1666181024756,131.113202490237));
#60274=CARTESIAN_POINT('Ctrl Pts',(81.6972565748548,10.1581978715527,131.112644740771));
#60275=CARTESIAN_POINT('Ctrl Pts',(81.7029996753843,10.1497365699715,131.112086991305));
#60276=CARTESIAN_POINT('Ctrl Pts',(81.7086777314092,10.1412352836669,131.11152924184));
#60277=CARTESIAN_POINT('Ctrl Pts',(81.7480661499276,10.0822622440483,131.107660158956));
#60278=CARTESIAN_POINT('Ctrl Pts',(81.7844750515846,10.0211321362282,131.103791076072));
#60279=CARTESIAN_POINT('Ctrl Pts',(81.8176610664462,9.95817838110956,131.099921993188));
#60280=CARTESIAN_POINT('Ctrl Pts',(81.8507976357946,9.89531842395793,131.096058675046));
#60281=CARTESIAN_POINT('Ctrl Pts',(81.8807206253813,9.83064063919304,131.092195356903));
#60282=CARTESIAN_POINT('Ctrl Pts',(81.9072300095337,9.76450719632596,131.088332038761));
#60283=CARTESIAN_POINT('Ctrl Pts',(81.9337082981801,9.69845132798336,131.08447325229));
#60284=CARTESIAN_POINT('Ctrl Pts',(81.9567807551403,9.63094364190379,131.080614465819));
#60285=CARTESIAN_POINT('Ctrl Pts',(81.9762941479208,9.56236909889694,131.076755679349));
#60286=CARTESIAN_POINT('Ctrl Pts',(81.9957952486906,9.49383775283796,131.072899323631));
#60287=CARTESIAN_POINT('Ctrl Pts',(82.0117416006339,9.42424134930235,131.069042967914));
#60288=CARTESIAN_POINT('Ctrl Pts',(82.0240293050706,9.35398154572728,131.065186612197));
#60289=CARTESIAN_POINT('Ctrl Pts',(82.0363133795937,9.2837424976172,131.061331395686));
#60290=CARTESIAN_POINT('Ctrl Pts',(82.0449408686595,9.21284091679222,131.057476179176));
#60291=CARTESIAN_POINT('Ctrl Pts',(82.0498590005134,9.14168853346027,131.053620962666));
#60292=CARTESIAN_POINT('Ctrl Pts',(82.0547773246505,9.07053336829956,131.049765595429));
#60293=CARTESIAN_POINT('Ctrl Pts',(82.0559859723494,8.99912786594283,131.045910228192));
#60294=CARTESIAN_POINT('Ctrl Pts',(82.0534841808734,8.92788702333957,131.042054860955));
#60295=CARTESIAN_POINT('Ctrl Pts',(82.0509797707049,8.85657161103036,131.038195458202));
#60296=CARTESIAN_POINT('Ctrl Pts',(82.0447571854772,8.78542168900987,131.034336055448));
#60297=CARTESIAN_POINT('Ctrl Pts',(82.0348677469965,8.71484948758009,131.030476652695));
#60298=CARTESIAN_POINT('Ctrl Pts',(82.0249727090403,8.64423732763135,131.026615064718));
#60299=CARTESIAN_POINT('Ctrl Pts',(82.0114067771825,8.5742040165918,131.022753476741));
#60300=CARTESIAN_POINT('Ctrl Pts',(81.994272354764,8.50515119730975,131.018891888764));
#60301=CARTESIAN_POINT('Ctrl Pts',(81.9771079550668,8.43597756767561,131.015023544803));
#60302=CARTESIAN_POINT('Ctrl Pts',(81.9563627415185,8.36778831955185,131.011155200841));
#60303=CARTESIAN_POINT('Ctrl Pts',(81.9321886708897,8.30096888296347,131.007286856879));
#60304=CARTESIAN_POINT('Ctrl Pts',(81.9178348053741,8.26129342981564,131.004989945869));
#60305=CARTESIAN_POINT('Ctrl Pts',(81.902272970537,8.22210053979701,131.002693034859));
#60306=CARTESIAN_POINT('Ctrl Pts',(81.8855426871364,8.18346687912466,131.000396123848));
#60307=CARTESIAN_POINT('Ctrl Pts',(81.8573609872113,8.11838954564444,130.996527040743));
#60308=CARTESIAN_POINT('Ctrl Pts',(81.8257510312571,8.0546454517863,130.992657957638));
#60309=CARTESIAN_POINT('Ctrl Pts',(81.7908609381909,7.99261990164489,130.988788874533));
#60310=CARTESIAN_POINT('Ctrl Pts',(81.7560228296071,7.93068676645084,130.984925556166));
#60311=CARTESIAN_POINT('Ctrl Pts',(81.7179145211702,7.87046751231053,130.9810622378));
#60312=CARTESIAN_POINT('Ctrl Pts',(81.6767317935264,7.81232662104522,130.977198919434));
#60313=CARTESIAN_POINT('Ctrl Pts',(81.6355973731938,7.75425392900539,130.973340132738));
#60314=CARTESIAN_POINT('Ctrl Pts',(81.591395976397,7.69825515179778,130.969481346042));
#60315=CARTESIAN_POINT('Ctrl Pts',(81.5443679112032,7.6446678202943,130.965622559345));
#60316=CARTESIAN_POINT('Ctrl Pts',(81.4973694702354,7.59111424487264,130.961766203401));
#60317=CARTESIAN_POINT('Ctrl Pts',(81.4475482132096,7.53996946567178,130.957909847457));
#60318=CARTESIAN_POINT('Ctrl Pts',(81.3951852332696,7.49153862251418,130.954053491512));
#60319=CARTESIAN_POINT('Ctrl Pts',(81.3428377218772,7.44312208631166,130.950198274774));
#60320=CARTESIAN_POINT('Ctrl Pts',(81.2879503346523,7.39741822417739,130.946343058036));
#60321=CARTESIAN_POINT('Ctrl Pts',(81.2308403574428,7.3546946857832,130.942487841298));
#60322=CARTESIAN_POINT('Ctrl Pts',(81.1737281474099,7.31196947703082,130.938632473833));
#60323=CARTESIAN_POINT('Ctrl Pts',(81.1143935651727,7.27222511258728,130.934777106368));
#60324=CARTESIAN_POINT('Ctrl Pts',(81.0531848497429,7.23568731944361,130.930921738902));
#60325=CARTESIAN_POINT('Ctrl Pts',(80.991912065521,7.19911128121911,130.927062335922));
#60326=CARTESIAN_POINT('Ctrl Pts',(80.9287616500761,7.1657487639317,130.923202932941));
#60327=CARTESIAN_POINT('Ctrl Pts',(80.8641077676973,7.1357802360491,130.91934352996));
#60328=CARTESIAN_POINT('Ctrl Pts',(80.7994172778011,7.10579473975922,130.915481941755));
#60329=CARTESIAN_POINT('Ctrl Pts',(80.7332220773407,7.07920723953435,130.911620353551));
#60330=CARTESIAN_POINT('Ctrl Pts',(80.6659151413543,7.05614954612885,130.907758765347));
#60331=CARTESIAN_POINT('Ctrl Pts',(80.598490449554,7.03305151249074,130.903890421161));
#60332=CARTESIAN_POINT('Ctrl Pts',(80.5299506062292,7.01349574859718,130.900022076975));
#60333=CARTESIAN_POINT('Ctrl Pts',(80.4607018422944,6.99756364021062,130.896153732788));
#60334=CARTESIAN_POINT('Ctrl Pts',(80.4195839634618,6.98810362294875,130.893856823811));
#60335=CARTESIAN_POINT('Ctrl Pts',(80.3782163235637,6.97992019115943,130.891559914834));
#60336=CARTESIAN_POINT('Ctrl Pts',(80.3366847674717,6.97302172437578,130.889263005857));
#60337=CARTESIAN_POINT('Ctrl Pts',(80.2667259651543,6.96140144044177,130.885393923737));
#60338=CARTESIAN_POINT('Ctrl Pts',(80.1960278428692,6.95338446885016,130.881524841618));
#60339=CARTESIAN_POINT('Ctrl Pts',(80.1249944439213,6.94905535143223,130.877655759498));
#60340=CARTESIAN_POINT('Ctrl Pts',(80.0540668812148,6.94473268418453,130.873792442119));
#60341=CARTESIAN_POINT('Ctrl Pts',(79.9828055143632,6.94408699355418,130.86992912474));
#60342=CARTESIAN_POINT('Ctrl Pts',(79.9116227439901,6.94715148558883,130.866065807361));
#60343=CARTESIAN_POINT('Ctrl Pts',(79.8405234709305,6.9502123829776,130.862207021649));
#60344=CARTESIAN_POINT('Ctrl Pts',(79.7695030942002,6.95697479761317,130.858348235937));
#60345=CARTESIAN_POINT('Ctrl Pts',(79.6989755228482,6.96741990891982,130.854489450225));
#60346=CARTESIAN_POINT('Ctrl Pts',(79.6284923786564,6.97785844057792,130.850633095263));
#60347=CARTESIAN_POINT('Ctrl Pts',(79.5585019033587,6.99197499540708,130.846776740301));
#60348=CARTESIAN_POINT('Ctrl Pts',(79.4894129142435,7.00969891967103,130.842920385339));
#60349=CARTESIAN_POINT('Ctrl Pts',(79.4203443346471,7.02741760812577,130.83906516958));
#60350=CARTESIAN_POINT('Ctrl Pts',(79.3521771828293,7.04874142975738,130.83520995382));
#60351=CARTESIAN_POINT('Ctrl Pts',(79.2853084095778,7.07354899022068,130.831354738061));
#60352=CARTESIAN_POINT('Ctrl Pts',(79.2184370218765,7.09835752061536,130.827499371569));
#60353=CARTESIAN_POINT('Ctrl Pts',(79.152864568212,7.12664988923231,130.823644005078));
#60354=CARTESIAN_POINT('Ctrl Pts',(79.0889695671289,7.15825595891212,130.819788638586));
#60355=CARTESIAN_POINT('Ctrl Pts',(79.0250076851929,7.18989511163228,130.815929236565));
#60356=CARTESIAN_POINT('Ctrl Pts',(78.9627271972069,7.22485467359619,130.812069834543));
#60357=CARTESIAN_POINT('Ctrl Pts',(78.9024826598933,7.26291817962851,130.808210432521));
#60358=CARTESIAN_POINT('Ctrl Pts',(78.8422040115549,7.3010032375767,130.80434884527));
#60359=CARTESIAN_POINT('Ctrl Pts',(78.7839640055023,7.34219545755186,130.800487258018));
#60360=CARTESIAN_POINT('Ctrl Pts',(78.7280865220779,7.38623617986394,130.796625670767));
#60361=CARTESIAN_POINT('Ctrl Pts',(78.6721112787374,7.43035395320006,130.792757327513));
#60362=CARTESIAN_POINT('Ctrl Pts',(78.6185071757931,7.4773298584405,130.788888984258));
#60363=CARTESIAN_POINT('Ctrl Pts',(78.5675629196051,7.52686674967611,130.785020641004));
#60364=CARTESIAN_POINT('Ctrl Pts',(78.5373135966484,7.55628041734706,130.782723723291));
#60365=CARTESIAN_POINT('Ctrl Pts',(78.5080013169371,7.58659631930302,130.780426805578));
#60366=CARTESIAN_POINT('Ctrl Pts',(78.4796796815665,7.61774687851383,130.778129887865));
#60367=CARTESIAN_POINT('Ctrl Pts',(78.432491033337,7.66964899368187,130.774302833369));
#60368=CARTESIAN_POINT('Ctrl Pts',(78.3878608320637,7.72408325904773,130.770475778874));
#60369=CARTESIAN_POINT('Ctrl Pts',(78.3460767383815,7.78076441686718,130.766648724378));
#60370=CARTESIAN_POINT('Ctrl Pts',(78.3043498473889,7.83736797782163,130.762826909144));
#60371=CARTESIAN_POINT('Ctrl Pts',(78.2654616325524,7.89621193790445,130.759005093911));
#60372=CARTESIAN_POINT('Ctrl Pts',(78.2296616569897,7.95697568879366,130.755183278677));
#60373=CARTESIAN_POINT('Ctrl Pts',(78.1938980883631,8.01767764573017,130.751365350054));
#60374=CARTESIAN_POINT('Ctrl Pts',(78.1612167818413,8.08029509593303,130.747547421432));
#60375=CARTESIAN_POINT('Ctrl Pts',(78.131824742173,8.14447748799764,130.743729492809));
#60376=CARTESIAN_POINT('Ctrl Pts',(78.1011566443136,8.21144636470353,130.739745808453));
#60377=CARTESIAN_POINT('Ctrl Pts',(78.0740702736719,8.28011871133061,130.735762124097));
#60378=CARTESIAN_POINT('Ctrl Pts',(78.0507474289291,8.35006771377833,130.731778439741));
#60379=CARTESIAN_POINT('Ctrl Pts',(78.0284112294451,8.41705760671818,130.727963280423));
#60380=CARTESIAN_POINT('Ctrl Pts',(78.0095266831971,8.48521779437095,130.724148121104));
#60381=CARTESIAN_POINT('Ctrl Pts',(77.9942033860812,8.55415528926336,130.720332961786));
#60382=CARTESIAN_POINT('Ctrl Pts',(77.9788799282579,8.62309350715724,130.716517762455));
#60383=CARTESIAN_POINT('Ctrl Pts',(77.9671178912865,8.69280856095067,130.712702563123));
#60384=CARTESIAN_POINT('Ctrl Pts',(77.9589758110982,8.76289702064792,130.708887363792));
#60385=CARTESIAN_POINT('Ctrl Pts',(77.9508281238068,8.83303374727478,130.705069537096));
#60386=CARTESIAN_POINT('Ctrl Pts',(77.9463054071717,8.90354389752152,130.701251710401));
#60387=CARTESIAN_POINT('Ctrl Pts',(77.945414248457,8.97402016057328,130.697433883705));
#60388=CARTESIAN_POINT('Ctrl Pts',(77.9452968688616,8.98330299101405,130.696931015982));
#60389=CARTESIAN_POINT('Ctrl Pts',(77.9452424192121,8.99258523549095,130.69642814826));
#60390=CARTESIAN_POINT('Ctrl Pts',(77.945250847264,9.00186596643237,130.695925280538));
#60391=CARTESIAN_POINT('Ctrl Pts',(77.9452508472645,9.00186596700247,130.695925280507));
#60392=CARTESIAN_POINT('Ctrl Pts',(77.9453334654876,9.09284277613626,130.69099578723));
#60393=CARTESIAN_POINT('Ctrl Pts',(77.9514620741529,9.1835503686496,130.686066293953));
#60394=CARTESIAN_POINT('Ctrl Pts',(77.9635073127509,9.27330403817156,130.681136800675));
#60395=CARTESIAN_POINT('Ctrl Pts',(77.9750243886588,9.35912216593073,130.676423457075));
#60396=CARTESIAN_POINT('Ctrl Pts',(77.9919501516287,9.4440686242144,130.671710113474));
#60397=CARTESIAN_POINT('Ctrl Pts',(78.0141316039583,9.52756447577781,130.666996769874));
#60398=CARTESIAN_POINT('Ctrl Pts',(78.0323398920129,9.59610446558729,130.663127685167));
#60399=CARTESIAN_POINT('Ctrl Pts',(78.0541363781817,9.66383493390369,130.659258600461));
#60400=CARTESIAN_POINT('Ctrl Pts',(78.0794317853549,9.73035285677203,130.655389515754));
#60401=CARTESIAN_POINT('Ctrl Pts',(78.1046895037382,9.79677167152922,130.651526195775));
#60402=CARTESIAN_POINT('Ctrl Pts',(78.1334356237984,9.86198107658305,130.647662875795));
#60403=CARTESIAN_POINT('Ctrl Pts',(78.1655306436492,9.92559156387147,130.643799555816));
#60404=CARTESIAN_POINT('Ctrl Pts',(78.1975880161602,9.98912743629294,130.639940767497));
#60405=CARTESIAN_POINT('Ctrl Pts',(78.2329862678671,10.0510676847769,130.636081979177));
#60406=CARTESIAN_POINT('Ctrl Pts',(78.2715378618458,10.1110428432186,130.632223190858));
#60407=CARTESIAN_POINT('Ctrl Pts',(78.3100651712137,10.1709802218119,130.628366833286));
#60408=CARTESIAN_POINT('Ctrl Pts',(78.3517416198771,10.2289545585805,130.624510475713));
#60409=CARTESIAN_POINT('Ctrl Pts',(78.396334529133,10.2846223647629,130.620654118141));
#60410=CARTESIAN_POINT('Ctrl Pts',(78.4409142652341,10.3402737261642,130.616798899772));
#60411=CARTESIAN_POINT('Ctrl Pts',(78.4884084479691,10.3936195307578,130.612943681403));
#60412=CARTESIAN_POINT('Ctrl Pts',(78.5385430413457,10.444347991483,130.609088463034));
#60413=CARTESIAN_POINT('Ctrl Pts',(78.5886795948317,10.495078435536,130.605233093938));
#60414=CARTESIAN_POINT('Ctrl Pts',(78.6414564208742,10.5431909885896,130.601377724842));
#60415=CARTESIAN_POINT('Ctrl Pts',(78.6965626496331,10.5884107265341,130.597522355746));
#60416=CARTESIAN_POINT('Ctrl Pts',(78.7517265593669,10.6336777970331,130.593662951145));
#60417=CARTESIAN_POINT('Ctrl Pts',(78.8092243627905,10.6760456991132,130.589803546544));
#60418=CARTESIAN_POINT('Ctrl Pts',(78.8687128331584,10.7152804169113,130.585944141943));
#60419=CARTESIAN_POINT('Ctrl Pts',(78.9282349862763,10.7545373496561,130.582082552123));
#60420=CARTESIAN_POINT('Ctrl Pts',(78.9897496309988,10.7906573204859,130.578220962303));
#60421=CARTESIAN_POINT('Ctrl Pts',(79.0528877147299,10.8234516394987,130.574359372483));
#60422=CARTESIAN_POINT('Ctrl Pts',(79.116136260292,10.8563033330834,130.570491026704));
#60423=CARTESIAN_POINT('Ctrl Pts',(79.1810134731886,10.8858175571895,130.566622680925));
#60424=CARTESIAN_POINT('Ctrl Pts',(79.2471297059274,10.9118535202267,130.562754335146));
#60425=CARTESIAN_POINT('Ctrl Pts',(79.2863873149451,10.9273128048073,130.560457440725));
#60426=CARTESIAN_POINT('Ctrl Pts',(79.3260814287917,10.9415467438447,130.558160546303));
#60427=CARTESIAN_POINT('Ctrl Pts',(79.3661283994795,10.9545343068244,130.555863651882));
#60428=CARTESIAN_POINT('Ctrl Pts',(79.4335880972922,10.9764120433645,130.551994500211));
#60429=CARTESIAN_POINT('Ctrl Pts',(79.5023139049624,10.9948360288297,130.548125348539));
#60430=CARTESIAN_POINT('Ctrl Pts',(79.5719187855566,11.0096626673003,130.544256196868));
#60431=CARTESIAN_POINT('Ctrl Pts',(79.6441103183262,11.0250402923731,130.540243260027));
#60432=CARTESIAN_POINT('Ctrl Pts',(79.7172470800184,11.0365476894604,130.536230323185));
#60433=CARTESIAN_POINT('Ctrl Pts',(79.790877229805,11.044080534002,130.532217386344));
#60434=CARTESIAN_POINT('Ctrl Pts',(79.8616761606652,11.0513237263822,130.528358754536));
#60435=CARTESIAN_POINT('Ctrl Pts',(79.9329306946829,11.0548923739865,130.524500122729));
#60436=CARTESIAN_POINT('Ctrl Pts',(80.0042284951781,11.0547456490594,130.520641490921));
#60437=CARTESIAN_POINT('Ctrl Pts',(80.075481736293,11.0545990158318,130.516785270664));
#60438=CARTESIAN_POINT('Ctrl Pts',(80.1467777055784,11.0507416184974,130.512929050407));
#60439=CARTESIAN_POINT('Ctrl Pts',(80.2177016825888,11.0431846563387,130.509072830149));
#60440=CARTESIAN_POINT('Ctrl Pts',(80.2886050592828,11.0356298891474,130.505217729956));
#60441=CARTESIAN_POINT('Ctrl Pts',(80.3591361755064,11.0243777424631,130.501362629762));
#60442=CARTESIAN_POINT('Ctrl Pts',(80.4288847878984,11.0094913289709,130.497507529568));
#60443=CARTESIAN_POINT('Ctrl Pts',(80.498636472752,10.9946042597248,130.493652259555));
#60444=CARTESIAN_POINT('Ctrl Pts',(80.567605110909,10.9760827099337,130.489796989542));
#60445=CARTESIAN_POINT('Ctrl Pts',(80.6353917190606,10.9540406663755,130.485941719529));
#60446=CARTESIAN_POINT('Ctrl Pts',(80.7032436169625,10.9319773926723,130.482082736252));
#60447=CARTESIAN_POINT('Ctrl Pts',(80.7699107506148,10.906387010034,130.478223752974));
#60448=CARTESIAN_POINT('Ctrl Pts',(80.8350113136356,10.8774327334423,130.474364769697));
#60449=CARTESIAN_POINT('Ctrl Pts',(80.9001492852494,10.8484618189184,130.47050356894));
#60450=CARTESIAN_POINT('Ctrl Pts',(80.9637184615834,10.8161233831014,130.466642368184));
#60451=CARTESIAN_POINT('Ctrl Pts',(81.0253613348939,10.780626770383,130.462781167427));
#60452=CARTESIAN_POINT('Ctrl Pts',(81.0870986717551,10.7450757614968,130.45891404964));
#60453=CARTESIAN_POINT('Ctrl Pts',(81.1469034091337,10.7063571836609,130.455046931854));
#60454=CARTESIAN_POINT('Ctrl Pts',(81.2044475334767,10.6647233108244,130.451179814067));
#60455=CARTESIAN_POINT('Ctrl Pts',(81.2204890699024,10.6531170643956,130.450101780271));
#60456=CARTESIAN_POINT('Ctrl Pts',(81.2363551335118,10.6412844986803,130.449023746474));
#60457=CARTESIAN_POINT('Ctrl Pts',(81.252039109102,10.6292316077768,130.447945712677));
#60458=CARTESIAN_POINT('',(77.9452507933687,8.99819435662442,130.754074719418));
#60459=CARTESIAN_POINT('Ctrl Pts',(77.9452507933687,8.99819435662443,130.754074719418));
#60460=CARTESIAN_POINT('Ctrl Pts',(77.9451892124666,9.06827093509326,130.750269075961));
#60461=CARTESIAN_POINT('Ctrl Pts',(77.9487167666399,9.13846487636557,130.746463432503));
#60462=CARTESIAN_POINT('Ctrl Pts',(77.955842851978,9.20837254303459,130.742657789045));
#60463=CARTESIAN_POINT('Ctrl Pts',(77.9629627689955,9.27821969781131,130.738855439743));
#60464=CARTESIAN_POINT('Ctrl Pts',(77.9736749941454,9.34778057278129,130.73505309044));
#60465=CARTESIAN_POINT('Ctrl Pts',(77.9879368904968,9.41665286015621,130.731250741137));
#60466=CARTESIAN_POINT('Ctrl Pts',(78.0021915378848,9.48549014147856,130.727450324473));
#60467=CARTESIAN_POINT('Ctrl Pts',(78.019992177926,9.55363903911737,130.723649907809));
#60468=CARTESIAN_POINT('Ctrl Pts',(78.0412447589067,9.62070562103915,130.719849491145));
#60469=CARTESIAN_POINT('Ctrl Pts',(78.0624941303669,9.6877620747055,130.716049648412));
#60470=CARTESIAN_POINT('Ctrl Pts',(78.0871942556541,9.75373605967473,130.712249805679));
#60471=CARTESIAN_POINT('Ctrl Pts',(78.1152012631751,9.81824891332844,130.708449962946));
#60472=CARTESIAN_POINT('Ctrl Pts',(78.1432332471189,9.88281929902329,130.704646731543));
#60473=CARTESIAN_POINT('Ctrl Pts',(78.17457780405,9.94592548974653,130.700843500141));
#60474=CARTESIAN_POINT('Ctrl Pts',(78.2090433737487,10.0072099708535,130.697040268739));
#60475=CARTESIAN_POINT('Ctrl Pts',(78.2435240046636,10.0685212328558,130.693235375351));
#60476=CARTESIAN_POINT('Ctrl Pts',(78.2811280946731,10.12800877667,130.689430481963));
#60477=CARTESIAN_POINT('Ctrl Pts',(78.3216202127085,10.1853433477737,130.685625588575));
#60478=CARTESIAN_POINT('Ctrl Pts',(78.3621848365102,10.2427805829813,130.68181388209));
#60479=CARTESIAN_POINT('Ctrl Pts',(78.4056475047835,10.2980567525532,130.678002175606));
#60480=CARTESIAN_POINT('Ctrl Pts',(78.4517323843278,10.3508756244602,130.674190469121));
#60481=CARTESIAN_POINT('Ctrl Pts',(78.4895041823488,10.3941666947873,130.671066342317));
#60482=CARTESIAN_POINT('Ctrl Pts',(78.5290366712771,10.4358076062443,130.667942215513));
#60483=CARTESIAN_POINT('Ctrl Pts',(78.5701610020028,10.4756551095383,130.664818088709));
#60484=CARTESIAN_POINT('Ctrl Pts',(78.621091525187,10.5250043428154,130.660949006591));
#60485=CARTESIAN_POINT('Ctrl Pts',(78.6746796484828,10.5718104253932,130.657079924472));
#60486=CARTESIAN_POINT('Ctrl Pts',(78.730641139085,10.6157740079344,130.653210842354));
#60487=CARTESIAN_POINT('Ctrl Pts',(78.7865192498416,10.6596720869182,130.649347524977));
#60488=CARTESIAN_POINT('Ctrl Pts',(78.8447633297575,10.7007357749319,130.645484207599));
#60489=CARTESIAN_POINT('Ctrl Pts',(78.9050530730826,10.7387031919606,130.641620890221));
#60490=CARTESIAN_POINT('Ctrl Pts',(78.9652720966034,10.77662607325,130.637762104511));
#60491=CARTESIAN_POINT('Ctrl Pts',(79.0275316081242,10.8114596401715,130.6339033188));
#60492=CARTESIAN_POINT('Ctrl Pts',(79.0914804691145,10.8429839458063,130.63004453309));
#60493=CARTESIAN_POINT('Ctrl Pts',(79.1553890470463,10.8744883934572,130.626188178129));
#60494=CARTESIAN_POINT('Ctrl Pts',(79.2209844284724,10.9026875013314,130.622331823169));
#60495=CARTESIAN_POINT('Ctrl Pts',(79.2878901806696,10.9274068505931,130.618475468208));
#60496=CARTESIAN_POINT('Ctrl Pts',(79.3547761682962,10.9521188975332,130.61462025245));
#60497=CARTESIAN_POINT('Ctrl Pts',(79.4229713027732,10.9733530583668,130.610765036692));
#60498=CARTESIAN_POINT('Ctrl Pts',(79.4920800507304,10.9909833971266,130.606909820934));
#60499=CARTESIAN_POINT('Ctrl Pts',(79.5611915007165,11.0086144252013,130.603054454444));
#60500=CARTESIAN_POINT('Ctrl Pts',(79.6312161638495,11.02264123351,130.599199087954));
#60501=CARTESIAN_POINT('Ctrl Pts',(79.7017459426531,11.0329884603155,130.595343721464));
#60502=CARTESIAN_POINT('Ctrl Pts',(79.7723495471349,11.0433465178801,130.591484319443));
#60503=CARTESIAN_POINT('Ctrl Pts',(79.8434588411079,11.0500172347658,130.587624917423));
#60504=CARTESIAN_POINT('Ctrl Pts',(79.9146590844894,11.0529769824915,130.583765515403));
#60505=CARTESIAN_POINT('Ctrl Pts',(79.98589964212,11.0559384060542,130.579903928153));
#60506=CARTESIAN_POINT('Ctrl Pts',(80.0572307656864,11.0551846827794,130.576042340903));
#60507=CARTESIAN_POINT('Ctrl Pts',(80.1282389462027,11.0507443368633,130.572180753653));
#60508=CARTESIAN_POINT('Ctrl Pts',(80.1993713584019,11.0462962223825,130.5683124104));
#60509=CARTESIAN_POINT('Ctrl Pts',(80.2701792167571,11.0381486634102,130.564444067147));
#60510=CARTESIAN_POINT('Ctrl Pts',(80.34025605182,11.0263818449887,130.560575723893));
#60511=CARTESIAN_POINT('Ctrl Pts',(80.3818657834461,11.0193950260753,130.558278806168));
#60512=CARTESIAN_POINT('Ctrl Pts',(80.4232179920287,11.0111331547442,130.555981888443));
#60513=CARTESIAN_POINT('Ctrl Pts',(80.4642301545072,11.0016213243634,130.553684970717));
#60514=CARTESIAN_POINT('Ctrl Pts',(80.5351039376409,10.9851837760149,130.549715629943));
#60515=CARTESIAN_POINT('Ctrl Pts',(80.6052460381132,10.9649442735024,130.54574628917));
#60516=CARTESIAN_POINT('Ctrl Pts',(80.6742185437271,10.9409860684185,130.541776948396));
#60517=CARTESIAN_POINT('Ctrl Pts',(80.7413369799038,10.9176718906237,130.537914308594));
#60518=CARTESIAN_POINT('Ctrl Pts',(80.8073474054342,10.8908365645804,130.534051668793));
#60519=CARTESIAN_POINT('Ctrl Pts',(80.8718566420438,10.860608383896,130.530189028991));
#60520=CARTESIAN_POINT('Ctrl Pts',(80.9390388686133,10.829127675237,130.526166337731));
#60521=CARTESIAN_POINT('Ctrl Pts',(81.0045922542099,10.793966910179,130.522143646471));
#60522=CARTESIAN_POINT('Ctrl Pts',(81.0680928093577,10.7553276939359,130.518120955211));
#60523=CARTESIAN_POINT('Ctrl Pts',(81.1315933645054,10.7166884776928,130.514098263951));
#60524=CARTESIAN_POINT('Ctrl Pts',(81.1930405534724,10.6745710786514,130.510075572691));
#60525=CARTESIAN_POINT('Ctrl Pts',(81.252039109102,10.6292316077768,130.506052881431));
#60526=CARTESIAN_POINT('Ctrl Pts',(81.252039109102,10.6292316077768,131.206019331793));
#60527=CARTESIAN_POINT('Ctrl Pts',(81.3108254747807,10.5840552015738,131.201991466329));
#60528=CARTESIAN_POINT('Ctrl Pts',(81.3672518669379,10.5356251954291,131.197963600866));
#60529=CARTESIAN_POINT('Ctrl Pts',(81.4209427311286,10.4842234728479,131.193935735403));
#60530=CARTESIAN_POINT('Ctrl Pts',(81.4723686485046,10.4349901297404,131.190077785272));
#60531=CARTESIAN_POINT('Ctrl Pts',(81.52128479453,10.3830311202787,131.186219835142));
#60532=CARTESIAN_POINT('Ctrl Pts',(81.5673942489599,10.3286357028274,131.182361885011));
#60533=CARTESIAN_POINT('Ctrl Pts',(81.613479121098,10.2742692851558,131.178505991666));
#60534=CARTESIAN_POINT('Ctrl Pts',(81.6567599571315,10.217469406789,131.174650098321));
#60535=CARTESIAN_POINT('Ctrl Pts',(81.6969781573811,10.1585606138099,131.170794204976));
#60536=CARTESIAN_POINT('Ctrl Pts',(81.7371883696808,10.0996635210183,131.16693907747));
#60537=CARTESIAN_POINT('Ctrl Pts',(81.7743368805687,10.0386587466771,131.163083949965));
#60538=CARTESIAN_POINT('Ctrl Pts',(81.8082077324642,9.97590079350147,131.159228822459));
#60539=CARTESIAN_POINT('Ctrl Pts',(81.8420831870339,9.91313431221403,131.155373171084));
#60540=CARTESIAN_POINT('Ctrl Pts',(81.8726798700234,9.84861460785023,131.151517519709));
#60541=CARTESIAN_POINT('Ctrl Pts',(81.8998280279057,9.78272027371457,131.147661868334));
#60542=CARTESIAN_POINT('Ctrl Pts',(81.9270062096907,9.71675306520279,131.143801952888));
#60543=CARTESIAN_POINT('Ctrl Pts',(81.9507280723322,9.64940864383426,131.139942037441));
#60544=CARTESIAN_POINT('Ctrl Pts',(81.9708725883272,9.58108416178778,131.136082121994));
#60545=CARTESIAN_POINT('Ctrl Pts',(81.9910302587801,9.51271506355261,131.132219686005));
#60546=CARTESIAN_POINT('Ctrl Pts',(82.0076058219315,9.44336510344808,131.128357250016));
#60547=CARTESIAN_POINT('Ctrl Pts',(82.02052920906,9.37344246924429,131.124494814027));
#60548=CARTESIAN_POINT('Ctrl Pts',(82.0334740888014,9.30340354818092,131.120625954503));
#60549=CARTESIAN_POINT('Ctrl Pts',(82.0427546122951,9.23279053365593,131.116757094978));
#60550=CARTESIAN_POINT('Ctrl Pts',(82.0483525477548,9.16201667385336,131.112888235454));
#60551=CARTESIAN_POINT('Ctrl Pts',(82.0500587934809,9.14044486462523,131.111709010527));
#60552=CARTESIAN_POINT('Ctrl Pts',(82.0514232841471,9.11885810558639,131.110529785601));
#60553=CARTESIAN_POINT('Ctrl Pts',(82.0524464644487,9.09726804753776,131.109350560675));
#60554=CARTESIAN_POINT('Ctrl Pts',(82.0558035588435,9.02643022673454,131.105481477794));
#60555=CARTESIAN_POINT('Ctrl Pts',(82.055495594845,8.95527965835121,131.101612394913));
#60556=CARTESIAN_POINT('Ctrl Pts',(82.0514858739565,8.88422750129229,131.097743312031));
#60557=CARTESIAN_POINT('Ctrl Pts',(82.0474821273519,8.81328120840016,131.09387999389));
#60558=CARTESIAN_POINT('Ctrl Pts',(82.0397875989872,8.74243351684024,131.090016675749));
#60559=CARTESIAN_POINT('Ctrl Pts',(82.0284175513193,8.67209788045864,131.086153357608));
#60560=CARTESIAN_POINT('Ctrl Pts',(82.0170608407127,8.60184474774972,131.082294571138));
#60561=CARTESIAN_POINT('Ctrl Pts',(82.002037251815,8.53210295437389,131.078435784668));
#60562=CARTESIAN_POINT('Ctrl Pts',(81.9834138929847,8.46328136643552,131.074576998197));
#60563=CARTESIAN_POINT('Ctrl Pts',(81.9648022655047,8.39450313105044,131.070720642479));
#60564=CARTESIAN_POINT('Ctrl Pts',(81.9425954935482,8.32664441887198,131.066864286761));
#60565=CARTESIAN_POINT('Ctrl Pts',(81.9169115671849,8.26010297602124,131.063007931044));
#60566=CARTESIAN_POINT('Ctrl Pts',(81.8912352281108,8.19358119017946,131.059152714532));
#60567=CARTESIAN_POINT('Ctrl Pts',(81.8620839487106,8.1283763540738,131.05529749802));
#60568=CARTESIAN_POINT('Ctrl Pts',(81.8296247232406,8.06486849341557,131.051442281508));
#60569=CARTESIAN_POINT('Ctrl Pts',(81.7971642287126,8.00135814979139,131.047586914269));
#60570=CARTESIAN_POINT('Ctrl Pts',(81.7613957543905,7.93954534489364,131.04373154703));
#60571=CARTESIAN_POINT('Ctrl Pts',(81.7225325466121,7.87978609705021,131.039876179791));
#60572=CARTESIAN_POINT('Ctrl Pts',(81.6836286596568,7.81996429757617,131.036016777034));
#60573=CARTESIAN_POINT('Ctrl Pts',(81.6416238381762,7.76220075414289,131.032157374277));
#60574=CARTESIAN_POINT('Ctrl Pts',(81.5967745355487,7.7068222685481,131.02829797152));
#60575=CARTESIAN_POINT('Ctrl Pts',(81.5518998388958,7.65141242722229,131.024436383539));
#60576=CARTESIAN_POINT('Ctrl Pts',(81.5041777800879,7.5983906932835,131.020574795558));
#60577=CARTESIAN_POINT('Ctrl Pts',(81.453903128989,7.54804846705679,131.016713207578));
#60578=CARTESIAN_POINT('Ctrl Pts',(81.4035405205947,7.4976181653097,131.012844863611));
#60579=CARTESIAN_POINT('Ctrl Pts',(81.3506167645328,7.44987705627581,131.008976519644));
#60580=CARTESIAN_POINT('Ctrl Pts',(81.2954607382095,7.40507710585823,131.005108175677));
#60581=CARTESIAN_POINT('Ctrl Pts',(81.2627106817143,7.37847618833455,131.002811264679));
#60582=CARTESIAN_POINT('Ctrl Pts',(81.22917419994,7.35291141379814,131.000514353682));
#60583=CARTESIAN_POINT('Ctrl Pts',(81.1949246752979,7.32842811017166,130.998217442684));
#60584=CARTESIAN_POINT('Ctrl Pts',(81.1372323025217,7.28718666538178,130.994348359918));
#60585=CARTESIAN_POINT('Ctrl Pts',(81.0772893247036,7.24885472904751,130.990479277153));
#60586=CARTESIAN_POINT('Ctrl Pts',(81.0154212654727,7.21368613728555,130.986610194388));
#60587=CARTESIAN_POINT('Ctrl Pts',(80.9536453865656,7.17856994497192,130.982746876363));
#60588=CARTESIAN_POINT('Ctrl Pts',(80.8899505385721,7.14660797971772,130.978883558338));
#60589=CARTESIAN_POINT('Ctrl Pts',(80.8246923557782,7.11801166825588,130.975020240312));
#60590=CARTESIAN_POINT('Ctrl Pts',(80.7595107208011,7.08944890025352,130.971161453958));
#60591=CARTESIAN_POINT('Ctrl Pts',(80.6927698363328,7.06424413818421,130.967302667603));
#60592=CARTESIAN_POINT('Ctrl Pts',(80.6248496025437,7.04256276302381,130.963443881248));
#60593=CARTESIAN_POINT('Ctrl Pts',(80.5569721535164,7.02089504553831,130.959587525645));
#60594=CARTESIAN_POINT('Ctrl Pts',(80.4879172907597,7.00274645893529,130.955731170043));
#60595=CARTESIAN_POINT('Ctrl Pts',(80.4180831694177,6.98823360552234,130.95187481444));
#60596=CARTESIAN_POINT('Ctrl Pts',(80.3482696777666,6.97372503934997,130.948019598043));
#60597=CARTESIAN_POINT('Ctrl Pts',(80.2776778599043,6.96285017290605,130.944164381646));
#60598=CARTESIAN_POINT('Ctrl Pts',(80.2067175623795,6.95567482725867,130.940309165249));
#60599=CARTESIAN_POINT('Ctrl Pts',(80.1357544905088,6.94849920107567,130.936453798124));
#60600=CARTESIAN_POINT('Ctrl Pts',(80.0644233939133,6.94502342953479,130.932598430999));
#60601=CARTESIAN_POINT('Ctrl Pts',(79.9931390359637,6.94526145466814,130.928743063873));
#60602=CARTESIAN_POINT('Ctrl Pts',(79.9217800627019,6.94549972894899,130.924883661229));
#60603=CARTESIAN_POINT('Ctrl Pts',(79.8504684125221,6.94945955826817,130.921024258584));
#60604=CARTESIAN_POINT('Ctrl Pts',(79.7796177376698,6.95710273852301,130.91716485594));
#60605=CARTESIAN_POINT('Ctrl Pts',(79.7087269465955,6.96475024640798,130.91330326807));
#60606=CARTESIAN_POINT('Ctrl Pts',(79.6382981302733,6.97608517967534,130.909441680201));
#60607=CARTESIAN_POINT('Ctrl Pts',(79.5687359811075,6.99101794221335,130.905580092331));
#60608=CARTESIAN_POINT('Ctrl Pts',(79.4990521304315,7.00597683016258,130.901711748473));
#60609=CARTESIAN_POINT('Ctrl Pts',(79.4302384433347,7.02454598799566,130.897843404615));
#60610=CARTESIAN_POINT('Ctrl Pts',(79.3626849813179,7.04658577627215,130.893975060758));
#60611=CARTESIAN_POINT('Ctrl Pts',(79.3225736663156,7.05967237263228,130.891678148736));
#60612=CARTESIAN_POINT('Ctrl Pts',(79.2829063081009,7.07398165553897,130.889381236714));
#60613=CARTESIAN_POINT('Ctrl Pts',(79.2437607894417,7.08947655892053,130.887084324692));
#60614=CARTESIAN_POINT('Ctrl Pts',(79.177821278139,7.11557728236622,130.883215241808));
#60615=CARTESIAN_POINT('Ctrl Pts',(79.1131054573439,7.14514687385421,130.879346158925));
#60616=CARTESIAN_POINT('Ctrl Pts',(79.0500031408005,7.17804952591704,130.875477076041));
#60617=CARTESIAN_POINT('Ctrl Pts',(78.9869948435733,7.21090315466317,130.871613757898));
#60618=CARTESIAN_POINT('Ctrl Pts',(78.9255957058782,7.24707976365544,130.867750439756));
#60619=CARTESIAN_POINT('Ctrl Pts',(78.8661762433599,7.28639524645307,130.863887121613));
#60620=CARTESIAN_POINT('Ctrl Pts',(78.8068264798676,7.32566461219179,130.860028335142));
#60621=CARTESIAN_POINT('Ctrl Pts',(78.7494521821217,7.36806527148104,130.856169548672));
#60622=CARTESIAN_POINT('Ctrl Pts',(78.694398342541,7.41336775699586,130.852310762201));
#60623=CARTESIAN_POINT('Ctrl Pts',(78.6393791828537,7.45864170525735,130.848454406484));
#60624=CARTESIAN_POINT('Ctrl Pts',(78.5866779555281,7.50681354520323,130.844598050767));
#60625=CARTESIAN_POINT('Ctrl Pts',(78.5366085735487,7.55761201631153,130.840741695049));
#60626=CARTESIAN_POINT('Ctrl Pts',(78.4865539825771,7.60839548103162,130.836886478539));
#60627=CARTESIAN_POINT('Ctrl Pts',(78.4391300342729,7.66180369068438,130.833031262028));
#60628=CARTESIAN_POINT('Ctrl Pts',(78.3946143198094,7.71752801966709,130.829176045518));
#60629=CARTESIAN_POINT('Ctrl Pts',(78.350096864925,7.77325452729132,130.825320678281));
#60630=CARTESIAN_POINT('Ctrl Pts',(78.3084881711032,7.8312969531067,130.821465311044));
#60631=CARTESIAN_POINT('Ctrl Pts',(78.270024911011,7.89131440255697,130.817609943807));
#60632=CARTESIAN_POINT('Ctrl Pts',(78.2315213903901,7.95139467388565,130.813750541054));
#60633=CARTESIAN_POINT('Ctrl Pts',(78.1961701385391,8.01345368582609,130.8098911383));
#60634=CARTESIAN_POINT('Ctrl Pts',(78.1641634157805,8.07712319427703,130.806031735547));
#60635=CARTESIAN_POINT('Ctrl Pts',(78.1321385705713,8.14082875288952,130.80217014757));
#60636=CARTESIAN_POINT('Ctrl Pts',(78.1034622195977,8.20614617826129,130.798308559593));
#60637=CARTESIAN_POINT('Ctrl Pts',(78.0782785874146,8.27268687973425,130.794446971617));
#60638=CARTESIAN_POINT('Ctrl Pts',(78.0530508955754,8.3393439965202,130.790578627655));
#60639=CARTESIAN_POINT('Ctrl Pts',(78.0313282706822,8.40722819948842,130.786710283693));
#60640=CARTESIAN_POINT('Ctrl Pts',(78.0132049587206,8.47593604736861,130.782841939732));
#60641=CARTESIAN_POINT('Ctrl Pts',(78.002443859087,8.51673278464356,130.780545028721));
#60642=CARTESIAN_POINT('Ctrl Pts',(77.9929507711793,8.55781969999827,130.778248117711));
#60643=CARTESIAN_POINT('Ctrl Pts',(77.9847367966347,8.5991112577513,130.775951206701));
#60644=CARTESIAN_POINT('Ctrl Pts',(77.9647646110808,8.69951121014636,130.770366293739));
#60645=CARTESIAN_POINT('Ctrl Pts',(77.9522903129537,8.80144853340686,130.764781380778));
#60646=CARTESIAN_POINT('Ctrl Pts',(77.9474937711074,8.90400133929624,130.759196467816));
#60647=CARTESIAN_POINT('Ctrl Pts',(77.9460275184564,8.93535065893526,130.757489218365));
#60648=CARTESIAN_POINT('Ctrl Pts',(77.945278419186,8.96675730674471,130.755781968913));
#60649=CARTESIAN_POINT('Ctrl Pts',(77.9452507933694,8.99819435581925,130.754074719462));
#60650=CARTESIAN_POINT('Origin',(80.,9.,141.545925280538));
#60651=CARTESIAN_POINT('',(81.252039109102,10.6292316077769,131.906140964271));
#60652=CARTESIAN_POINT('',(81.252039109102,10.6292316077768,131.847886939688));
#60653=CARTESIAN_POINT('',(81.252039109102,10.6292316077768,141.545925280538));
#60654=CARTESIAN_POINT('',(77.9452501035681,8.99934760960447,131.39592528057));
#60655=CARTESIAN_POINT('Ctrl Pts',(81.252039109102,10.6292316077768,131.847886939688));
#60656=CARTESIAN_POINT('Ctrl Pts',(81.3085634809923,10.585793508561,131.844031409931));
#60657=CARTESIAN_POINT('Ctrl Pts',(81.3628520463242,10.5393893355674,131.840175880174));
#60658=CARTESIAN_POINT('Ctrl Pts',(81.4145852345703,10.4902839248397,131.836320350417));
#60659=CARTESIAN_POINT('Ctrl Pts',(81.4663133117732,10.4411833655407,131.832465201571));
#60660=CARTESIAN_POINT('Ctrl Pts',(81.5154861617407,10.3893824337431,131.828610052726));
#60661=CARTESIAN_POINT('Ctrl Pts',(81.5618198975157,10.3351839462127,131.82475490388));
#60662=CARTESIAN_POINT('Ctrl Pts',(81.6083190581177,10.2807919544186,131.82088599104));
#60663=CARTESIAN_POINT('Ctrl Pts',(81.65195846601,10.2239856221613,131.817017078199));
#60664=CARTESIAN_POINT('Ctrl Pts',(81.6924922182366,10.1651041385681,131.813148165358));
#60665=CARTESIAN_POINT('Ctrl Pts',(81.7329383898611,10.106349879214,131.809287612012));
#60666=CARTESIAN_POINT('Ctrl Pts',(81.7702920860257,10.0455298612198,131.805427058667));
#60667=CARTESIAN_POINT('Ctrl Pts',(81.8043538914048,9.98300793337198,131.801566505321));
#60668=CARTESIAN_POINT('Ctrl Pts',(81.8385263309912,9.92028293161642,131.797693412732));
#60669=CARTESIAN_POINT('Ctrl Pts',(81.8693852587684,9.85584539410209,131.793820320144));
#60670=CARTESIAN_POINT('Ctrl Pts',(81.8967778289509,9.79008317922887,131.789947227555));
#60671=CARTESIAN_POINT('Ctrl Pts',(81.9241703991334,9.72432096435564,131.786074134966));
#60672=CARTESIAN_POINT('Ctrl Pts',(81.9480965075822,9.65723455181734,131.782201042378));
#60673=CARTESIAN_POINT('Ctrl Pts',(81.9684540117227,9.58922522538739,131.778327949789));
#60674=CARTESIAN_POINT('Ctrl Pts',(81.9887904401114,9.52128630776972,131.774458866942));
#60675=CARTESIAN_POINT('Ctrl Pts',(82.0056453207932,9.45216025530351,131.770589784096));
#60676=CARTESIAN_POINT('Ctrl Pts',(82.0188839110768,9.38223725105644,131.766720701249));
#60677=CARTESIAN_POINT('Ctrl Pts',(82.0321027765212,9.31241842859865,131.762857383143));
#60678=CARTESIAN_POINT('Ctrl Pts',(82.0417159571495,9.24180548476804,131.758994065037));
#60679=CARTESIAN_POINT('Ctrl Pts',(82.0476385852172,9.17080335719701,131.75513074693));
#60680=CARTESIAN_POINT('Ctrl Pts',(82.0535542660444,9.0998845150946,131.751271960495));
#60681=CARTESIAN_POINT('Ctrl Pts',(82.0557879530187,9.02857787779235,131.747413174059));
#60682=CARTESIAN_POINT('Ctrl Pts',(82.0543062010364,8.9572964300878,131.743554387624));
#60683=CARTESIAN_POINT('Ctrl Pts',(82.0528253824493,8.88605988446865,131.739698031941));
#60684=CARTESIAN_POINT('Ctrl Pts',(82.0476337784021,8.81484898149624,131.735841676258));
#60685=CARTESIAN_POINT('Ctrl Pts',(82.0387500055476,8.74407818111861,131.731985320575));
#60686=CARTESIAN_POINT('Ctrl Pts',(82.0298688570486,8.67332828714428,131.728130104098));
#60687=CARTESIAN_POINT('Ctrl Pts',(82.0172977655639,8.60301871939521,131.724274887621));
#60688=CARTESIAN_POINT('Ctrl Pts',(82.0011071786636,8.53355855458501,131.720419671144));
#60689=CARTESIAN_POINT('Ctrl Pts',(81.9849159587599,8.46409567409016,131.71656430394));
#60690=CARTESIAN_POINT('Ctrl Pts',(81.9651050749096,8.3954827350673,131.712708936735));
#60691=CARTESIAN_POINT('Ctrl Pts',(81.9417956504084,8.32811666596407,131.708853569531));
#60692=CARTESIAN_POINT('Ctrl Pts',(81.918461827296,8.26068008295663,131.704994166808));
#60693=CARTESIAN_POINT('Ctrl Pts',(81.8916223124959,8.19449343522535,131.701134764086));
#60694=CARTESIAN_POINT('Ctrl Pts',(81.8614472056873,8.1299357133298,131.697275361363));
#60695=CARTESIAN_POINT('Ctrl Pts',(81.8312550134963,8.06534143834507,131.693413773417));
#60696=CARTESIAN_POINT('Ctrl Pts',(81.7977236980523,8.00237835420563,131.68955218547));
#60697=CARTESIAN_POINT('Ctrl Pts',(81.7610690802565,7.94140033201186,131.685690597524));
#60698=CARTESIAN_POINT('Ctrl Pts',(81.724350333893,7.88031562658267,131.68182225359));
#60699=CARTESIAN_POINT('Ctrl Pts',(81.6844976471958,7.82122331979352,131.677953909657));
#60700=CARTESIAN_POINT('Ctrl Pts',(81.641769449805,7.7644472345598,131.674085565724));
#60701=CARTESIAN_POINT('Ctrl Pts',(81.6163986757773,7.73073522898493,131.671788654415));
#60702=CARTESIAN_POINT('Ctrl Pts',(81.5900148690261,7.69783920296017,131.669491743107));
#60703=CARTESIAN_POINT('Ctrl Pts',(81.5626783192383,7.66582083921145,131.667194831798));
#60704=CARTESIAN_POINT('Ctrl Pts',(81.5166306657679,7.61188680108156,131.663325748947));
#60705=CARTESIAN_POINT('Ctrl Pts',(81.4676973380779,7.56023384777018,131.659456666095));
#60706=CARTESIAN_POINT('Ctrl Pts',(81.4161330600869,7.51118680868661,131.655587583244));
#60707=CARTESIAN_POINT('Ctrl Pts',(81.3646456102985,7.46221284724508,131.651724265133));
#60708=CARTESIAN_POINT('Ctrl Pts',(81.3105353403875,7.41583742508861,131.647860947022));
#60709=CARTESIAN_POINT('Ctrl Pts',(81.2540964212598,7.37235147261969,131.643997628911));
#60710=CARTESIAN_POINT('Ctrl Pts',(81.1977237049623,7.32891652915604,131.640138842471));
#60711=CARTESIAN_POINT('Ctrl Pts',(81.1390281480815,7.28836461804355,131.636280056031));
#60712=CARTESIAN_POINT('Ctrl Pts',(81.0783385728415,7.25094783244693,131.632421269591));
#60713=CARTESIAN_POINT('Ctrl Pts',(81.0176872275837,7.21355461668153,131.628564913903));
#60714=CARTESIAN_POINT('Ctrl Pts',(80.955044768553,7.1792928626006,131.624708558215));
#60715=CARTESIAN_POINT('Ctrl Pts',(80.8907694945681,7.14837172465776,131.620852202528));
#60716=CARTESIAN_POINT('Ctrl Pts',(80.826513208143,7.11745972112878,131.616996986046));
#60717=CARTESIAN_POINT('Ctrl Pts',(80.7606255018848,7.08988658504439,131.613141769564));
#60718=CARTESIAN_POINT('Ctrl Pts',(80.6934882640487,7.06581500622956,131.609286553083));
#60719=CARTESIAN_POINT('Ctrl Pts',(80.6263484013477,7.04174248628813,131.605431185874));
#60720=CARTESIAN_POINT('Ctrl Pts',(80.5579593681003,7.02117195729456,131.601575818665));
#60721=CARTESIAN_POINT('Ctrl Pts',(80.4887203319175,7.00421694574024,131.597720451456));
#60722=CARTESIAN_POINT('Ctrl Pts',(80.4194088213454,6.98724418691246,131.593861048729));
#60723=CARTESIAN_POINT('Ctrl Pts',(80.3492460045637,6.97389461593553,131.590001646001));
#60724=CARTESIAN_POINT('Ctrl Pts',(80.278642542797,6.96423088346354,131.586142243274));
#60725=CARTESIAN_POINT('Ctrl Pts',(80.207999104796,6.95456167931038,131.582280655323));
#60726=CARTESIAN_POINT('Ctrl Pts',(80.1369150094421,6.948582508874,131.578419067372));
#60727=CARTESIAN_POINT('Ctrl Pts',(80.0658046125619,6.94630398659744,131.574557479421));
#60728=CARTESIAN_POINT('Ctrl Pts',(79.9945698054951,6.94402147796453,131.570689135483));
#60729=CARTESIAN_POINT('Ctrl Pts',(79.9233090908698,6.94545253409038,131.566820791545));
#60730=CARTESIAN_POINT('Ctrl Pts',(79.8524346901804,6.95055567486261,131.562952447607));
#60731=CARTESIAN_POINT('Ctrl Pts',(79.8103515114051,6.95358577294237,131.56065553634));
#60732=CARTESIAN_POINT('Ctrl Pts',(79.7684044150234,6.95790952452471,131.558358625073));
#60733=CARTESIAN_POINT('Ctrl Pts',(79.7266779226685,6.96350973374701,131.556061713806));
#60734=CARTESIAN_POINT('Ctrl Pts',(79.65639081242,6.97294312967386,131.552192630968));
#60735=CARTESIAN_POINT('Ctrl Pts',(79.5864549840656,6.98603809145479,131.54832354813));
#60736=CARTESIAN_POINT('Ctrl Pts',(79.5172814947748,7.00275679818075,131.544454465292));
#60737=CARTESIAN_POINT('Ctrl Pts',(79.4482110705333,7.01945059486749,131.540591147194));
#60738=CARTESIAN_POINT('Ctrl Pts',(79.3799011990709,7.03975730604368,131.536727829097));
#60739=CARTESIAN_POINT('Ctrl Pts',(79.3127558531502,7.06358758392726,131.532864510999));
#60740=CARTESIAN_POINT('Ctrl Pts',(79.2456892686935,7.08738990890437,131.529005724572));
#60741=CARTESIAN_POINT('Ctrl Pts',(79.1797849520477,7.11470742907931,131.525146938145));
#60742=CARTESIAN_POINT('Ctrl Pts',(79.1154330417206,7.14540062039794,131.521288151718));
#60743=CARTESIAN_POINT('Ctrl Pts',(79.0511216683776,7.176074477257,131.517431796044));
#60744=CARTESIAN_POINT('Ctrl Pts',(78.9883611986377,7.21011957783073,131.513575440369));
#60745=CARTESIAN_POINT('Ctrl Pts',(78.9275216843021,7.24734834469085,131.509719084695));
#60746=CARTESIAN_POINT('Ctrl Pts',(78.8667001425676,7.2845661138009,131.505863868226));
#60747=CARTESIAN_POINT('Ctrl Pts',(78.8077988437883,7.32496542865309,131.502008651758));
#60748=CARTESIAN_POINT('Ctrl Pts',(78.7511615977401,7.36831369205322,131.498153435289));
#60749=CARTESIAN_POINT('Ctrl Pts',(78.6945221373438,7.41166365024171,131.494298068093));
#60750=CARTESIAN_POINT('Ctrl Pts',(78.6401472898425,7.45796248888234,131.490442700897));
#60751=CARTESIAN_POINT('Ctrl Pts',(78.5883489332518,7.50693642859771,131.486587333701));
#60752=CARTESIAN_POINT('Ctrl Pts',(78.5364963579042,7.55596163067553,131.482727930987));
#60753=CARTESIAN_POINT('Ctrl Pts',(78.4872260107637,7.60766718903243,131.478868528272));
#60754=CARTESIAN_POINT('Ctrl Pts',(78.4408132612819,7.66174207407326,131.475009125558));
#60755=CARTESIAN_POINT('Ctrl Pts',(78.3943742325358,7.71584757673993,131.471147537619));
#60756=CARTESIAN_POINT('Ctrl Pts',(78.3507963192765,7.77232469188178,131.467285949681));
#60757=CARTESIAN_POINT('Ctrl Pts',(78.310313177493,7.8308310625293,131.463424361742));
#60758=CARTESIAN_POINT('Ctrl Pts',(78.2697592089995,7.88943979217287,131.459556017817));
#60759=CARTESIAN_POINT('Ctrl Pts',(78.2323110773245,7.95008445204625,131.455687673892));
#60760=CARTESIAN_POINT('Ctrl Pts',(78.1981575144778,8.01239622324165,131.451819329966));
#60761=CARTESIAN_POINT('Ctrl Pts',(78.1778781109865,8.04939516112711,131.449522418582));
#60762=CARTESIAN_POINT('Ctrl Pts',(78.1587593571232,8.08698142395406,131.447225507198));
#60763=CARTESIAN_POINT('Ctrl Pts',(78.1408326489501,8.12507467559231,131.444928595814));
#60764=CARTESIAN_POINT('Ctrl Pts',(78.108155478463,8.19451183416958,131.440741738743));
#60765=CARTESIAN_POINT('Ctrl Pts',(78.0793295383059,8.26587225791199,131.436554881671));
#60766=CARTESIAN_POINT('Ctrl Pts',(78.0545656017949,8.33872655823763,131.432368024599));
#60767=CARTESIAN_POINT('Ctrl Pts',(78.0298638437669,8.41139793248148,131.42819168009));
#60768=CARTESIAN_POINT('Ctrl Pts',(78.0092039024862,8.48555538334085,131.42401533558));
#60769=CARTESIAN_POINT('Ctrl Pts',(77.9927491649578,8.56074876468895,131.419838991071));
#60770=CARTESIAN_POINT('Ctrl Pts',(77.9763607882817,8.63563889617533,131.415679489478));
#60771=CARTESIAN_POINT('Ctrl Pts',(77.9641439076397,8.7115562901603,131.411519987886));
#60772=CARTESIAN_POINT('Ctrl Pts',(77.9562120164597,8.7880371710974,131.407360486294));
#60773=CARTESIAN_POINT('Ctrl Pts',(77.9489432924382,8.8581236616763,131.403548751052));
#60774=CARTESIAN_POINT('Ctrl Pts',(77.9452725398498,8.92868294650349,131.399737015811));
#60775=CARTESIAN_POINT('Ctrl Pts',(77.9452501035681,8.99934760960448,131.39592528057));
#60776=CARTESIAN_POINT('Ctrl Pts',(77.9452501035679,8.99934761019358,131.395925280538));
#60777=CARTESIAN_POINT('Ctrl Pts',(77.9452268384226,9.07262290424563,131.391972724785));
#60778=CARTESIAN_POINT('Ctrl Pts',(77.9491275646018,9.14586509410072,131.388020169032));
#60779=CARTESIAN_POINT('Ctrl Pts',(77.956915517632,9.21863979602808,131.384067613279));
#60780=CARTESIAN_POINT('Ctrl Pts',(77.964709560304,9.29147140274994,131.3801119669));
#60781=CARTESIAN_POINT('Ctrl Pts',(77.9763968270618,9.36383434707673,131.376156320522));
#60782=CARTESIAN_POINT('Ctrl Pts',(77.9918890690414,9.4353022529972,131.372200674143));
#60783=CARTESIAN_POINT('Ctrl Pts',(78.0074099266823,9.5069021670158,131.368237721305));
#60784=CARTESIAN_POINT('Ctrl Pts',(78.0267496922357,9.57760330200735,131.364274768467));
#60785=CARTESIAN_POINT('Ctrl Pts',(78.0497697059516,9.64699255225699,131.360311815629));
#60786=CARTESIAN_POINT('Ctrl Pts',(78.072814378403,9.71645613135731,131.356344617728));
#60787=CARTESIAN_POINT('Ctrl Pts',(78.0995469862578,9.78460460843077,131.352377419827));
#60788=CARTESIAN_POINT('Ctrl Pts',(78.1297809942066,9.85104549400674,131.348410221926));
#60789=CARTESIAN_POINT('Ctrl Pts',(78.160077328869,9.91762334594345,131.344434845737));
#60790=CARTESIAN_POINT('Ctrl Pts',(78.1938892656041,9.98248618042066,131.340459469549));
#60791=CARTESIAN_POINT('Ctrl Pts',(78.2309848912312,10.045267002946,131.336484093361));
#60792=CARTESIAN_POINT('Ctrl Pts',(78.2393476952132,10.0594202542724,131.335587888181));
#60793=CARTESIAN_POINT('Ctrl Pts',(78.2478772169349,10.0734678168532,131.334691683002));
#60794=CARTESIAN_POINT('Ctrl Pts',(78.2565705111979,10.0874057108896,131.333795477822));
#60795=CARTESIAN_POINT('Ctrl Pts',(78.2941010642334,10.1475781674418,131.329926394941));
#60796=CARTESIAN_POINT('Ctrl Pts',(78.3348239566212,10.2059232122907,131.32605731206));
#60797=CARTESIAN_POINT('Ctrl Pts',(78.3785355099976,10.2620818001069,131.322188229179));
#60798=CARTESIAN_POINT('Ctrl Pts',(78.4221819353415,10.3181567144309,131.318324911038));
#60799=CARTESIAN_POINT('Ctrl Pts',(78.4688078867301,10.372051257967,131.314461592897));
#60800=CARTESIAN_POINT('Ctrl Pts',(78.5181656434058,10.4234340526055,131.310598274756));
#60801=CARTESIAN_POINT('Ctrl Pts',(78.5674655034532,10.474756575247,131.306739488286));
#60802=CARTESIAN_POINT('Ctrl Pts',(78.6194904688571,10.523572852667,131.302880701816));
#60803=CARTESIAN_POINT('Ctrl Pts',(78.6739527858832,10.569584769432,131.299021915345));
#60804=CARTESIAN_POINT('Ctrl Pts',(78.7283807956436,10.6155677020639,131.295165559628));
#60805=CARTESIAN_POINT('Ctrl Pts',(78.7852427407071,10.6587494660693,131.29130920391));
#60806=CARTESIAN_POINT('Ctrl Pts',(78.8442153428553,10.6988700329363,131.287452848192));
#60807=CARTESIAN_POINT('Ctrl Pts',(78.903170523906,10.7389787477859,131.28359763168));
#60808=CARTESIAN_POINT('Ctrl Pts',(78.9642347227752,10.7760277876989,131.279742415169));
#60809=CARTESIAN_POINT('Ctrl Pts',(79.0270544352387,10.8097995719171,131.275887198657));
#60810=CARTESIAN_POINT('Ctrl Pts',(79.0898766037636,10.8435726765103,131.272031831418));
#60811=CARTESIAN_POINT('Ctrl Pts',(79.1544539932342,10.8740680429386,131.268176464179));
#60812=CARTESIAN_POINT('Ctrl Pts',(79.2204087129387,10.9011141437689,131.26432109694));
#60813=CARTESIAN_POINT('Ctrl Pts',(79.2864324692427,10.9281885544887,131.260461694183));
#60814=CARTESIAN_POINT('Ctrl Pts',(79.3538359833336,10.9518063076746,131.256602291426));
#60815=CARTESIAN_POINT('Ctrl Pts',(79.4222224454108,10.9718444816752,131.252742888669));
#60816=CARTESIAN_POINT('Ctrl Pts',(79.4906476284368,10.9918940014464,131.248881300689));
#60817=CARTESIAN_POINT('Ctrl Pts',(79.5600563944854,11.0083597951441,131.245019712708));
#60818=CARTESIAN_POINT('Ctrl Pts',(79.6300405549925,11.0211698522266,131.241158124727));
#60819=CARTESIAN_POINT('Ctrl Pts',(79.7001471552846,11.0340023209609,131.23728978076));
#60820=CARTESIAN_POINT('Ctrl Pts',(79.7708306779828,11.0431662211242,131.233421436794));
#60821=CARTESIAN_POINT('Ctrl Pts',(79.8416773114418,11.0486413763242,131.229553092827));
#60822=CARTESIAN_POINT('Ctrl Pts',(79.8837439976024,11.0518923654572,131.227256181828));
#60823=CARTESIAN_POINT('Ctrl Pts',(79.9258681602445,11.0538438341146,131.22495927083));
#60824=CARTESIAN_POINT('Ctrl Pts',(79.9679636615187,11.0545002398434,131.222662359831));
#60825=CARTESIAN_POINT('Ctrl Pts',(80.0388583887734,11.0556057191395,131.21879403961));
#60826=CARTESIAN_POINT('Ctrl Pts',(80.1099492315853,11.0530395060358,131.21492571939));
#60827=CARTESIAN_POINT('Ctrl Pts',(80.1808243171346,11.0467779871869,131.211057399169));
#60828=CARTESIAN_POINT('Ctrl Pts',(80.2516008675047,11.040525173511,131.20719445694));
#60829=CARTESIAN_POINT('Ctrl Pts',(80.3221617761546,11.0305872888518,131.203331514711));
#60830=CARTESIAN_POINT('Ctrl Pts',(80.3920944026495,11.0169926975354,131.199468572483));
#60831=CARTESIAN_POINT('Ctrl Pts',(80.4619532083301,11.0034124566566,131.195609707972));
#60832=CARTESIAN_POINT('Ctrl Pts',(80.5311845737788,10.9861832627287,131.191750843461));
#60833=CARTESIAN_POINT('Ctrl Pts',(80.5993819433257,10.9653851654358,131.18789197895));
#60834=CARTESIAN_POINT('Ctrl Pts',(80.6675362532769,10.9446001999934,131.184035550914));
#60835=CARTESIAN_POINT('Ctrl Pts',(80.7346573990156,10.92025094335,131.180179122878));
#60836=CARTESIAN_POINT('Ctrl Pts',(80.8003515559622,10.8924679520058,131.176322694841));
#60837=CARTESIAN_POINT('Ctrl Pts',(80.86602140742,10.8646952397977,131.172467693604));
#60838=CARTESIAN_POINT('Ctrl Pts',(80.9302648728577,10.8334915082904,131.168612692367));
#60839=CARTESIAN_POINT('Ctrl Pts',(80.9927074781201,10.7990356931935,131.16475769113));
#60840=CARTESIAN_POINT('Ctrl Pts',(81.0551657820457,10.764571215578,131.160901720709));
#60841=CARTESIAN_POINT('Ctrl Pts',(81.1158218958457,10.7268532559481,131.157045750288));
#60842=CARTESIAN_POINT('Ctrl Pts',(81.174326582638,10.6861063548335,131.153189779867));
#60843=CARTESIAN_POINT('Ctrl Pts',(81.2006767626129,10.6677541810734,131.151453072602));
#60844=CARTESIAN_POINT('Ctrl Pts',(81.2265908973889,10.6487881620257,131.149716365337));
#60845=CARTESIAN_POINT('Ctrl Pts',(81.252039109102,10.6292316077768,131.147979658073));
#60846=CARTESIAN_POINT('',(77.9452503396332,9.00118140704016,131.454074719514));
#60847=CARTESIAN_POINT('Ctrl Pts',(77.9452503396338,9.00118140798793,131.454074719462));
#60848=CARTESIAN_POINT('Ctrl Pts',(77.9452901831621,9.07047878642176,131.450299784525));
#60849=CARTESIAN_POINT('Ctrl Pts',(77.9488353855608,9.13967381098879,131.446524849588));
#60850=CARTESIAN_POINT('Ctrl Pts',(77.955856695627,9.20850830603872,131.44274991465));
#60851=CARTESIAN_POINT('Ctrl Pts',(77.9630531190943,9.27905955229594,131.438880831799));
#60852=CARTESIAN_POINT('Ctrl Pts',(77.9739204176304,9.34937597973054,131.435011748947));
#60853=CARTESIAN_POINT('Ctrl Pts',(77.9884338439667,9.41904553738384,131.431142666096));
#60854=CARTESIAN_POINT('Ctrl Pts',(78.0029256460216,9.48861129087124,131.427279347985));
#60855=CARTESIAN_POINT('Ctrl Pts',(78.0210526941545,9.5575316160017,131.423416029874));
#60856=CARTESIAN_POINT('Ctrl Pts',(78.0427385152251,9.62539990623353,131.419552711764));
#60857=CARTESIAN_POINT('Ctrl Pts',(78.064398898836,9.69318858698713,131.415693925323));
#60858=CARTESIAN_POINT('Ctrl Pts',(78.0896096163955,9.7599272235673,131.411835138883));
#60859=CARTESIAN_POINT('Ctrl Pts',(78.1182436044463,9.82522144318533,131.407976352443));
#60860=CARTESIAN_POINT('Ctrl Pts',(78.1468595551843,9.89047453223283,131.404119996755));
#60861=CARTESIAN_POINT('Ctrl Pts',(78.1788943034939,9.95428456566709,131.400263641067));
#60862=CARTESIAN_POINT('Ctrl Pts',(78.2141721188591,10.01627572117,131.39640728538));
#60863=CARTESIAN_POINT('Ctrl Pts',(78.2494395128043,10.0782485638648,131.392552068898));
#60864=CARTESIAN_POINT('Ctrl Pts',(78.2879478317042,10.1384031733724,131.388696852417));
#60865=CARTESIAN_POINT('Ctrl Pts',(78.3294755145786,10.1963885264025,131.384841635935));
#60866=CARTESIAN_POINT('Ctrl Pts',(78.371004821061,10.2543761464861,131.380986268726));
#60867=CARTESIAN_POINT('Ctrl Pts',(78.4155534412464,10.3101939480482,131.377130901517));
#60868=CARTESIAN_POINT('Ctrl Pts',(78.4628576386396,10.3635215155659,131.373275534308));
#60869=CARTESIAN_POINT('Ctrl Pts',(78.5102113506275,10.4169049025044,131.369416131581));
#60870=CARTESIAN_POINT('Ctrl Pts',(78.5603260745845,10.4677924878938,131.365556728853));
#60871=CARTESIAN_POINT('Ctrl Pts',(78.6128996831301,10.5158991633481,131.361697326126));
#60872=CARTESIAN_POINT('Ctrl Pts',(78.6655030592655,10.5640330771796,131.357835738175));
#60873=CARTESIAN_POINT('Ctrl Pts',(78.7205677163487,10.6093826376158,131.353974150224));
#60874=CARTESIAN_POINT('Ctrl Pts',(78.7777588906698,10.6517034337808,131.350112562272));
#60875=CARTESIAN_POINT('Ctrl Pts',(78.8350501229989,10.6940982716946,131.346244218335));
#60876=CARTESIAN_POINT('Ctrl Pts',(78.8944748953416,10.7334534975559,131.342375874397));
#60877=CARTESIAN_POINT('Ctrl Pts',(78.9556705686791,10.7695687614153,131.338507530459));
#60878=CARTESIAN_POINT('Ctrl Pts',(78.9920067977846,10.7910129653963,131.336210619192));
#60879=CARTESIAN_POINT('Ctrl Pts',(79.0289669160085,10.8113157578957,131.333913707925));
#60880=CARTESIAN_POINT('Ctrl Pts',(79.066471624849,10.8304432073375,131.331616796658));
#60881=CARTESIAN_POINT('Ctrl Pts',(79.1296472587565,10.8626628613723,131.32774771382));
#60882=CARTESIAN_POINT('Ctrl Pts',(79.1946166239922,10.8916711307533,131.323878630982));
#60883=CARTESIAN_POINT('Ctrl Pts',(79.2610201204873,10.9172653181486,131.320009548144));
#60884=CARTESIAN_POINT('Ctrl Pts',(79.3273246790844,10.9428213714811,131.316146230047));
#60885=CARTESIAN_POINT('Ctrl Pts',(79.3950586778971,10.9649732667228,131.312282911949));
#60886=CARTESIAN_POINT('Ctrl Pts',(79.4638390357964,10.9835647161019,131.308419593851));
#60887=CARTESIAN_POINT('Ctrl Pts',(79.5325387143634,11.0021343577183,131.304560807424));
#60888=CARTESIAN_POINT('Ctrl Pts',(79.6022818473495,11.017151723076,131.300702020997));
#60889=CARTESIAN_POINT('Ctrl Pts',(79.6726681924137,11.0285096623488,131.296843234571));
#60890=CARTESIAN_POINT('Ctrl Pts',(79.7430101992425,11.0398604469528,131.292986878896));
#60891=CARTESIAN_POINT('Ctrl Pts',(79.81399413584,11.0475563016886,131.289130523221));
#60892=CARTESIAN_POINT('Ctrl Pts',(79.8852089486743,11.0515410249458,131.285274167547));
#60893=CARTESIAN_POINT('Ctrl Pts',(79.9564027239408,11.0555245710759,131.281418951078));
#60894=CARTESIAN_POINT('Ctrl Pts',(80.0278267552817,11.0557991350738,131.27756373461));
#60895=CARTESIAN_POINT('Ctrl Pts',(80.0990659661064,11.0523604695227,131.273708518141));
#60896=CARTESIAN_POINT('Ctrl Pts',(80.1703079621725,11.04892166953,131.269853150945));
#60897=CARTESIAN_POINT('Ctrl Pts',(80.2413646382644,11.0417693773813,131.265997783749));
#60898=CARTESIAN_POINT('Ctrl Pts',(80.3118237572204,11.030951379756,131.262142416554));
#60899=CARTESIAN_POINT('Ctrl Pts',(80.3823566276638,11.0201220586367,131.258283013839));
#60900=CARTESIAN_POINT('Ctrl Pts',(80.452290211234,11.0056194464126,131.254423611125));
#60901=CARTESIAN_POINT('Ctrl Pts',(80.521221111002,10.9875427331119,131.250564208411));
#60902=CARTESIAN_POINT('Ctrl Pts',(80.5901910399885,10.9694557846337,131.246702620472));
#60903=CARTESIAN_POINT('Ctrl Pts',(80.6581566919459,10.9477908541529,131.242841032534));
#60904=CARTESIAN_POINT('Ctrl Pts',(80.7247311599672,10.9226966240862,131.238979444595));
#60905=CARTESIAN_POINT('Ctrl Pts',(80.7914221024105,10.8975584907631,131.23511110067));
#60906=CARTESIAN_POINT('Ctrl Pts',(80.856716556353,10.8689792741642,131.231242756744));
#60907=CARTESIAN_POINT('Ctrl Pts',(80.9202495129103,10.8371549734544,131.227374412819));
#60908=CARTESIAN_POINT('Ctrl Pts',(80.9579735555502,10.8182586188377,131.225077501435));
#60909=CARTESIAN_POINT('Ctrl Pts',(80.9950770457667,10.7982190350941,131.222780590051));
#60910=CARTESIAN_POINT('Ctrl Pts',(81.0314884665628,10.7770844397068,131.220483678667));
#60911=CARTESIAN_POINT('Ctrl Pts',(81.0928208329716,10.7414847646637,131.216614699991));
#60912=CARTESIAN_POINT('Ctrl Pts',(81.1524281864628,10.7026364999002,131.212745721315));
#60913=CARTESIAN_POINT('Ctrl Pts',(81.2099452235117,10.6607318021286,131.208876742639));
#60914=CARTESIAN_POINT('Ctrl Pts',(81.2241048436853,10.6504156482657,131.207924272357));
#60915=CARTESIAN_POINT('Ctrl Pts',(81.2381378835472,10.6399144830512,131.206971802075));
#60916=CARTESIAN_POINT('Ctrl Pts',(81.252039109102,10.6292316077768,131.206019331793));
#60917=CARTESIAN_POINT('Ctrl Pts',(81.252039109102,10.6292316077769,131.906140964271));
#60918=CARTESIAN_POINT('Ctrl Pts',(81.3085547227941,10.5858002390999,131.902272668994));
#60919=CARTESIAN_POINT('Ctrl Pts',(81.3627348175322,10.539480934796,131.898404373717));
#60920=CARTESIAN_POINT('Ctrl Pts',(81.4142868161189,10.4905671283952,131.89453607844));
#60921=CARTESIAN_POINT('Ctrl Pts',(81.4465096501982,10.4599933095123,131.892118181165));
#60922=CARTESIAN_POINT('Ctrl Pts',(81.4777064486786,10.4284065658194,131.889700283891));
#60923=CARTESIAN_POINT('Ctrl Pts',(81.5078138187366,10.395885042017,131.887282386616));
#60924=CARTESIAN_POINT('Ctrl Pts',(81.555991179404,10.3438445888436,131.883413303769));
#60925=CARTESIAN_POINT('Ctrl Pts',(81.6015655640656,10.28920510133,131.879544220922));
#60926=CARTESIAN_POINT('Ctrl Pts',(81.6442441695773,10.2322575515334,131.875675138076));
#60927=CARTESIAN_POINT('Ctrl Pts',(81.6868591860952,10.1753948507458,131.871811819969));
#60928=CARTESIAN_POINT('Ctrl Pts',(81.726586698802,10.1162312993567,131.867948501863));
#60929=CARTESIAN_POINT('Ctrl Pts',(81.7631721851422,10.0550930802734,131.864085183757));
#60930=CARTESIAN_POINT('Ctrl Pts',(81.799714756721,9.99402657629762,131.860226397321));
#60931=CARTESIAN_POINT('Ctrl Pts',(81.8331223745403,9.93099042037825,131.856367610885));
#60932=CARTESIAN_POINT('Ctrl Pts',(81.8631831399907,9.86634066587836,131.852508824449));
#60933=CARTESIAN_POINT('Ctrl Pts',(81.893224969363,9.80173163598326,131.848652468766));
#60934=CARTESIAN_POINT('Ctrl Pts',(81.9199239248086,9.73551146357781,131.844796113083));
#60935=CARTESIAN_POINT('Ctrl Pts',(81.943114199668,9.66806045351347,131.8409397574));
#60936=CARTESIAN_POINT('Ctrl Pts',(81.966297623888,9.60062936915292,131.837084540923));
#60937=CARTESIAN_POINT('Ctrl Pts',(81.9859742674043,9.53196862812393,131.833229324446));
#60938=CARTESIAN_POINT('Ctrl Pts',(82.0020272285704,9.46247652758042,131.829374107968));
#60939=CARTESIAN_POINT('Ctrl Pts',(82.0180808173592,9.39298171010365,131.825518740764));
#60940=CARTESIAN_POINT('Ctrl Pts',(82.0305103353282,9.32265594239479,131.821663373559));
#60941=CARTESIAN_POINT('Ctrl Pts',(82.0392497279014,9.25190893146906,131.817808006355));
#60942=CARTESIAN_POINT('Ctrl Pts',(82.0479982682356,9.18108786771468,131.813948603632));
#60943=CARTESIAN_POINT('Ctrl Pts',(82.0530489129702,9.10984516366102,131.810089200909));
#60944=CARTESIAN_POINT('Ctrl Pts',(82.054387478561,9.03859598984201,131.806229798187));
#60945=CARTESIAN_POINT('Ctrl Pts',(82.0557268020581,8.96730647418111,131.80236821024));
#60946=CARTESIAN_POINT('Ctrl Pts',(82.0533498785534,8.89601096720569,131.798506622293));
#60947=CARTESIAN_POINT('Ctrl Pts',(82.0472946356544,8.82512222176385,131.794645034346));
#60948=CARTESIAN_POINT('Ctrl Pts',(82.0412287988908,8.75410945392093,131.790776690413));
#60949=CARTESIAN_POINT('Ctrl Pts',(82.0314718608921,8.68350534979087,131.786908346479));
#60950=CARTESIAN_POINT('Ctrl Pts',(82.0181132365228,8.61371444879264,131.783040002546));
#60951=CARTESIAN_POINT('Ctrl Pts',(82.0101812697977,8.57227462017489,131.780743091239));
#60952=CARTESIAN_POINT('Ctrl Pts',(82.0009804488128,8.53112126457092,131.778446179932));
#60953=CARTESIAN_POINT('Ctrl Pts',(81.9905377382802,8.49033631188563,131.776149268625));
#60954=CARTESIAN_POINT('Ctrl Pts',(81.9729472844919,8.42163519992567,131.772280185777));
#60955=CARTESIAN_POINT('Ctrl Pts',(81.9517614930238,8.35371126913166,131.76841110293));
#60956=CARTESIAN_POINT('Ctrl Pts',(81.9270660084627,8.28696833062777,131.764542020082));
#60957=CARTESIAN_POINT('Ctrl Pts',(81.9024073189419,8.22032483577358,131.760678701975));
#60958=CARTESIAN_POINT('Ctrl Pts',(81.8742494834812,8.15485929229784,131.756815383868));
#60959=CARTESIAN_POINT('Ctrl Pts',(81.8427284911056,8.09096244820819,131.752952065761));
#60960=CARTESIAN_POINT('Ctrl Pts',(81.8112444728419,8.02714055509204,131.749093279325));
#60961=CARTESIAN_POINT('Ctrl Pts',(81.776405347604,7.96488413987531,131.745234492889));
#60962=CARTESIAN_POINT('Ctrl Pts',(81.7383953179642,7.90456434192598,131.741375706452));
#60963=CARTESIAN_POINT('Ctrl Pts',(81.700409231856,7.84428254102631,131.737519350769));
#60964=CARTESIAN_POINT('Ctrl Pts',(81.6592564626002,7.78593534709736,131.733662995085));
#60965=CARTESIAN_POINT('Ctrl Pts',(81.6151665866135,7.72986832966531,131.729806639401));
#60966=CARTESIAN_POINT('Ctrl Pts',(81.5710897352177,7.67381787499165,131.725951422923));
#60967=CARTESIAN_POINT('Ctrl Pts',(81.5240777997389,7.62004664120675,131.722096206445));
#60968=CARTESIAN_POINT('Ctrl Pts',(81.4744019976384,7.5688688697887,131.718240989968));
#60969=CARTESIAN_POINT('Ctrl Pts',(81.4247242533627,7.5176890974729,131.714385622762));
#60970=CARTESIAN_POINT('Ctrl Pts',(81.3723827756188,7.46910333587675,131.710530255557));
#60971=CARTESIAN_POINT('Ctrl Pts',(81.3176859461205,7.42338929665673,131.706674888352));
#60972=CARTESIAN_POINT('Ctrl Pts',(81.2629318639569,7.37762740730336,131.702815485629));
#60973=CARTESIAN_POINT('Ctrl Pts',(81.2058178820311,7.33474355296152,131.698956082905));
#60974=CARTESIAN_POINT('Ctrl Pts',(81.1466851059665,7.29497483002314,131.695096680182));
#60975=CARTESIAN_POINT('Ctrl Pts',(81.0875188484596,7.25518358972147,131.691235092235));
#60976=CARTESIAN_POINT('Ctrl Pts',(81.026331938212,7.21851124188097,131.687373504287));
#60977=CARTESIAN_POINT('Ctrl Pts',(80.9634917137323,7.18514979128601,131.68351191634));
#60978=CARTESIAN_POINT('Ctrl Pts',(80.9005415480276,7.15172997363754,131.679643572406));
#60979=CARTESIAN_POINT('Ctrl Pts',(80.8359327335557,7.12163282338651,131.675775228472));
#60980=CARTESIAN_POINT('Ctrl Pts',(80.7700536341266,7.09500263436707,131.671906884538));
#60981=CARTESIAN_POINT('Ctrl Pts',(80.7309365208099,7.07919039451337,131.669609973236));
#60982=CARTESIAN_POINT('Ctrl Pts',(80.6913718813705,7.06459953841317,131.667313061935));
#60983=CARTESIAN_POINT('Ctrl Pts',(80.6514431729601,7.05125184928793,131.665016150633));
#60984=CARTESIAN_POINT('Ctrl Pts',(80.5841843803937,7.02876804027297,131.661147067787));
#60985=CARTESIAN_POINT('Ctrl Pts',(80.5156284830307,7.00972632113528,131.657277984941));
#60986=CARTESIAN_POINT('Ctrl Pts',(80.4461611878916,6.99427375823141,131.653408902095));
#60987=CARTESIAN_POINT('Ctrl Pts',(80.3767973955577,6.9788442188756,131.64954558399));
#60988=CARTESIAN_POINT('Ctrl Pts',(80.3065253712456,6.96699332541082,131.645682265884));
#60989=CARTESIAN_POINT('Ctrl Pts',(80.2357471530522,6.9588187629885,131.641818947779));
#60990=CARTESIAN_POINT('Ctrl Pts',(80.1650519576813,6.95065378932474,131.637960161344));
#60991=CARTESIAN_POINT('Ctrl Pts',(80.093852228081,6.94615663641099,131.634101374909));
#60992=CARTESIAN_POINT('Ctrl Pts',(80.0225596785607,6.9453738482626,131.630242588474));
#60993=CARTESIAN_POINT('Ctrl Pts',(79.9513120381188,6.94459155321334,131.626386232792));
#60994=CARTESIAN_POINT('Ctrl Pts',(79.8799721783654,6.94751898616858,131.622529877109));
#60995=CARTESIAN_POINT('Ctrl Pts',(79.8089549414203,6.95415070249731,131.618673521427));
#60996=CARTESIAN_POINT('Ctrl Pts',(79.7379586836779,6.96078045975063,131.614818304951));
#60997=CARTESIAN_POINT('Ctrl Pts',(79.6672853429502,6.97111228278093,131.610963088474));
#60998=CARTESIAN_POINT('Ctrl Pts',(79.5973460269105,6.98508875122122,131.607107871998));
#60999=CARTESIAN_POINT('Ctrl Pts',(79.5274039764526,6.99906576609965,131.603252504794));
#61000=CARTESIAN_POINT('Ctrl Pts',(79.458196483592,7.01668761193721,131.599397137591));
#61001=CARTESIAN_POINT('Ctrl Pts',(79.3901241232495,7.03784583239292,131.595541770387));
#61002=CARTESIAN_POINT('Ctrl Pts',(79.3219805097079,7.05902619973599,131.591682367665));
#61003=CARTESIAN_POINT('Ctrl Pts',(79.2549748653884,7.08375018647811,131.587822964943));
#61004=CARTESIAN_POINT('Ctrl Pts',(79.1894913917896,7.11185981491924,131.583963562221));
#61005=CARTESIAN_POINT('Ctrl Pts',(79.1239708409334,7.13998535925287,131.580101974275));
#61006=CARTESIAN_POINT('Ctrl Pts',(79.0599746125178,7.17150014668207,131.576240386329));
#61007=CARTESIAN_POINT('Ctrl Pts',(78.9978632532908,7.20619970359154,131.572378798383));
#61008=CARTESIAN_POINT('Ctrl Pts',(78.9356432280141,7.24095996861979,131.568510454451));
#61009=CARTESIAN_POINT('Ctrl Pts',(78.8753150670732,7.27891586874659,131.564642110518));
#61010=CARTESIAN_POINT('Ctrl Pts',(78.8172106373783,7.31981938882486,131.560773766585));
#61011=CARTESIAN_POINT('Ctrl Pts',(78.7827098989949,7.34410672203832,131.558476855271));
#61012=CARTESIAN_POINT('Ctrl Pts',(78.7489925561506,7.36943249127378,131.556179943956));
#61013=CARTESIAN_POINT('Ctrl Pts',(78.7161221751678,7.39573839620713,131.553883032642));
#61014=CARTESIAN_POINT('Ctrl Pts',(78.661450898684,7.43949138472648,131.550062721779));
#61015=CARTESIAN_POINT('Ctrl Pts',(78.6088985784268,7.48613870942767,131.546242410916));
#61016=CARTESIAN_POINT('Ctrl Pts',(78.5587935921189,7.53544489609219,131.542422100053));
#61017=CARTESIAN_POINT('Ctrl Pts',(78.5087739526717,7.58466709653985,131.538608296557));
#61018=CARTESIAN_POINT('Ctrl Pts',(78.4611937228877,7.63653881976069,131.534794493061));
#61019=CARTESIAN_POINT('Ctrl Pts',(78.4163489115398,7.69078390152009,131.530980689565));
#61020=CARTESIAN_POINT('Ctrl Pts',(78.3715467866424,7.7449773489896,131.527170516316));
#61021=CARTESIAN_POINT('Ctrl Pts',(78.3294752360328,7.80153929492881,131.523360343067));
#61022=CARTESIAN_POINT('Ctrl Pts',(78.2903930042301,7.86015725535729,131.519550169818));
#61023=CARTESIAN_POINT('Ctrl Pts',(78.251334107591,7.91874021625701,131.515742271541));
#61024=CARTESIAN_POINT('Ctrl Pts',(78.215261266858,7.97937634294027,131.511934373265));
#61025=CARTESIAN_POINT('Ctrl Pts',(78.1823913627715,8.04172216744194,131.508126474989));
#61026=CARTESIAN_POINT('Ctrl Pts',(78.1495294250013,8.10405288187323,131.504319499591));
#61027=CARTESIAN_POINT('Ctrl Pts',(78.1198691151503,8.16809202988376,131.500512524193));
#61028=CARTESIAN_POINT('Ctrl Pts',(78.0935816345596,8.23347108442563,131.496705548795));
#61029=CARTESIAN_POINT('Ctrl Pts',(78.0672753510514,8.29889690331867,131.492895850343));
#61030=CARTESIAN_POINT('Ctrl Pts',(78.0443469047301,8.36566407997194,131.48908615189));
#61031=CARTESIAN_POINT('Ctrl Pts',(78.0249190681297,8.43338472041204,131.485276453437));
#61032=CARTESIAN_POINT('Ctrl Pts',(78.005484315325,8.50112946903271,131.481465398753));
#61033=CARTESIAN_POINT('Ctrl Pts',(77.9895527685954,8.56982787082582,131.477654344068));
#61034=CARTESIAN_POINT('Ctrl Pts',(77.9771963820947,8.63908022236322,131.473843289384));
#61035=CARTESIAN_POINT('Ctrl Pts',(77.9648204879244,8.7084419061882,131.470026217989));
#61036=CARTESIAN_POINT('Ctrl Pts',(77.95603108832,8.77835879022988,131.466209146595));
#61037=CARTESIAN_POINT('Ctrl Pts',(77.9508483050221,8.84842528750064,131.4623920752));
#61038=CARTESIAN_POINT('Ctrl Pts',(77.947083896162,8.89931665763151,131.459619623304));
#61039=CARTESIAN_POINT('Ctrl Pts',(77.9452210770952,8.95028684822795,131.456847171409));
#61040=CARTESIAN_POINT('Ctrl Pts',(77.9452503396332,9.00118140704017,131.454074719514));
#61041=CARTESIAN_POINT('Origin',(80.,9.,141.545925280538));
#61042=CARTESIAN_POINT('',(81.252039109102,10.6292316077768,132.606087908811));
#61043=CARTESIAN_POINT('',(81.252039109102,10.6292316077768,132.547886797676));
#61044=CARTESIAN_POINT('',(81.252039109102,10.6292316077768,141.545925280538));
#61045=CARTESIAN_POINT('',(77.9452505617457,8.99848062725763,132.095925280492));
#61046=CARTESIAN_POINT('Ctrl Pts',(81.252039109102,10.6292316077768,132.547886797676));
#61047=CARTESIAN_POINT('Ctrl Pts',(81.3083538591921,10.5859545996489,132.544022016983));
#61048=CARTESIAN_POINT('Ctrl Pts',(81.3625154590115,10.5396826637711,132.540157236291));
#61049=CARTESIAN_POINT('Ctrl Pts',(81.4141896908426,10.4906592772376,132.536292455599));
#61050=CARTESIAN_POINT('Ctrl Pts',(81.4657959228315,10.4417004022107,132.5324327607));
#61051=CARTESIAN_POINT('Ctrl Pts',(81.5149209386215,10.3899976014555,132.528573065801));
#61052=CARTESIAN_POINT('Ctrl Pts',(81.5612632568425,10.3358347971713,132.524713370902));
#61053=CARTESIAN_POINT('Ctrl Pts',(81.607572059914,10.281711163877,132.520856467367));
#61054=CARTESIAN_POINT('Ctrl Pts',(81.6511018428738,10.2251314243555,132.516999563831));
#61055=CARTESIAN_POINT('Ctrl Pts',(81.6915887013729,10.1664155468304,132.513142660296));
#61056=CARTESIAN_POINT('Ctrl Pts',(81.7320598230887,10.1077224915017,132.509287255895));
#61057=CARTESIAN_POINT('Ctrl Pts',(81.769490092302,10.0468953456498,132.505431851494));
#61058=CARTESIAN_POINT('Ctrl Pts',(81.8036576212695,9.98428489155141,132.501576447094));
#61059=CARTESIAN_POINT('Ctrl Pts',(81.8378232990749,9.92167782962407,132.497721251575));
#61060=CARTESIAN_POINT('Ctrl Pts',(81.8687263563342,9.8572880784718,132.493866056056));
#61061=CARTESIAN_POINT('Ctrl Pts',(81.8961906147685,9.79149144970981,132.490010860537));
#61062=CARTESIAN_POINT('Ctrl Pts',(81.9236819784045,9.72562988451821,132.486151860224));
#61063=CARTESIAN_POINT('Ctrl Pts',(81.947727576468,9.65835911760964,132.482292859911));
#61064=CARTESIAN_POINT('Ctrl Pts',(81.9681995647198,9.5900746020095,132.478433859598));
#61065=CARTESIAN_POINT('Ctrl Pts',(81.9886814319893,9.52175713485006,132.474572997076));
#61066=CARTESIAN_POINT('Ctrl Pts',(82.0055861388274,9.4524254171311,132.470712134553));
#61067=CARTESIAN_POINT('Ctrl Pts',(82.0188366080988,9.38248700932207,132.466851272031));
#61068=CARTESIAN_POINT('Ctrl Pts',(82.0321114362183,9.31242003104405,132.462983311936));
#61069=CARTESIAN_POINT('Ctrl Pts',(82.0417185395784,9.24174461693172,132.459115351841));
#61070=CARTESIAN_POINT('Ctrl Pts',(82.0476326157001,9.17087490635356,132.455247391746));
#61071=CARTESIAN_POINT('Ctrl Pts',(82.0527907860587,9.10906338534611,132.451873813743));
#61072=CARTESIAN_POINT('Ctrl Pts',(82.0551404635228,9.04710432326967,132.448500235741));
#61073=CARTESIAN_POINT('Ctrl Pts',(82.0546972072604,8.98527081210231,132.445126657738));
#61074=CARTESIAN_POINT('Ctrl Pts',(82.0541888463451,8.91435531015297,132.441257574891));
#61075=CARTESIAN_POINT('Ctrl Pts',(82.0500038297876,8.84332726097794,132.437388492044));
#61076=CARTESIAN_POINT('Ctrl Pts',(82.0421279206532,8.77259921242762,132.433519409197));
#61077=CARTESIAN_POINT('Ctrl Pts',(82.0342637462307,8.70197654514227,132.429656091091));
#61078=CARTESIAN_POINT('Ctrl Pts',(82.0227196484063,8.63165347009274,132.425792772985));
#61079=CARTESIAN_POINT('Ctrl Pts',(82.0075333990489,8.56204199493211,132.421929454878));
#61080=CARTESIAN_POINT('Ctrl Pts',(81.9923649631562,8.49251217400505,132.418070668442));
#61081=CARTESIAN_POINT('Ctrl Pts',(81.9735629648897,8.42369276727413,132.414211882007));
#61082=CARTESIAN_POINT('Ctrl Pts',(81.9512166949536,8.35598837600995,132.410353095571));
#61083=CARTESIAN_POINT('Ctrl Pts',(81.928884501529,8.28832663354772,132.406496739888));
#61084=CARTESIAN_POINT('Ctrl Pts',(81.9030126178372,8.22177897326064,132.402640384204));
#61085=CARTESIAN_POINT('Ctrl Pts',(81.8737405346709,8.15673612004825,132.398784028521));
#61086=CARTESIAN_POINT('Ctrl Pts',(81.844477098771,8.091712481146,132.394928812044));
#61087=CARTESIAN_POINT('Ctrl Pts',(81.8118156567701,8.02819320954054,132.391073595567));
#61088=CARTESIAN_POINT('Ctrl Pts',(81.7759436651095,7.96654866546242,132.38721837909));
#61089=CARTESIAN_POINT('Ctrl Pts',(81.7400702709613,7.90490171126702,132.383363011885));
#61090=CARTESIAN_POINT('Ctrl Pts',(81.7009863241764,7.84513004887886,132.37950764468));
#61091=CARTESIAN_POINT('Ctrl Pts',(81.6589241562072,7.78757754621083,132.375652277476));
#61092=CARTESIAN_POINT('Ctrl Pts',(81.616817960618,7.72996480176631,132.371792874753));
#61093=CARTESIAN_POINT('Ctrl Pts',(81.5717276080722,7.67457624698685,132.36793347203));
#61094=CARTESIAN_POINT('Ctrl Pts',(81.5239269806332,7.62172422200847,132.364074069307));
#61095=CARTESIAN_POINT('Ctrl Pts',(81.4760992881035,7.56884227179838,132.360212481361));
#61096=CARTESIAN_POINT('Ctrl Pts',(81.4255586101456,7.51850005341321,132.356350893414));
#61097=CARTESIAN_POINT('Ctrl Pts',(81.3726151590845,7.47097246998247,132.352489305467));
#61098=CARTESIAN_POINT('Ctrl Pts',(81.319579081558,7.42336173534094,132.348620961533));
#61099=CARTESIAN_POINT('Ctrl Pts',(81.2641322160707,7.37857577250758,132.3447526176));
#61100=CARTESIAN_POINT('Ctrl Pts',(81.2066166827356,7.33684825002526,132.340884273666));
#61101=CARTESIAN_POINT('Ctrl Pts',(81.1724656141924,7.31207164798752,132.33858736236));
#61102=CARTESIAN_POINT('Ctrl Pts',(81.1375857558046,7.28837250744841,132.336290451053));
#61103=CARTESIAN_POINT('Ctrl Pts',(81.1020528512102,7.26579208984635,132.333993539747));
#61104=CARTESIAN_POINT('Ctrl Pts',(81.0421986673426,7.22775600801214,132.3301244569));
#61105=CARTESIAN_POINT('Ctrl Pts',(80.9802557831634,7.19274776279809,132.326255374053));
#61106=CARTESIAN_POINT('Ctrl Pts',(80.9165630719347,7.16100307295918,132.322386291206));
#61107=CARTESIAN_POINT('Ctrl Pts',(80.8529652596692,7.12930568112495,132.318522973099));
#61108=CARTESIAN_POINT('Ctrl Pts',(80.7876232267179,7.100862407597,132.314659654993));
#61109=CARTESIAN_POINT('Ctrl Pts',(80.7209036010567,7.07586498382168,132.310796336886));
#61110=CARTESIAN_POINT('Ctrl Pts',(80.6542622374906,7.05089688201483,132.306937550451));
#61111=CARTESIAN_POINT('Ctrl Pts',(80.5862469436659,7.02936677082744,132.303078764015));
#61112=CARTESIAN_POINT('Ctrl Pts',(80.517246068014,7.01141908195213,132.299219977579));
#61113=CARTESIAN_POINT('Ctrl Pts',(80.448288657854,6.99348269880476,132.295363621895));
#61114=CARTESIAN_POINT('Ctrl Pts',(80.3783473666403,6.97912438278268,132.291507266212));
#61115=CARTESIAN_POINT('Ctrl Pts',(80.3078261123458,6.96843886455315,132.287650910529));
#61116=CARTESIAN_POINT('Ctrl Pts',(80.237325690736,6.95775650293271,132.283795694051));
#61117=CARTESIAN_POINT('Ctrl Pts',(80.1662461262162,6.95074485785234,132.279940477574));
#61118=CARTESIAN_POINT('Ctrl Pts',(80.0950002433514,6.94744731705537,132.276085261097));
#61119=CARTESIAN_POINT('Ctrl Pts',(80.0237515749856,6.94414964733442,132.272229893892));
#61120=CARTESIAN_POINT('Ctrl Pts',(79.9523370607304,6.94456639045237,132.268374526687));
#61121=CARTESIAN_POINT('Ctrl Pts',(79.8811716074013,6.94868886425964,132.264519159483));
#61122=CARTESIAN_POINT('Ctrl Pts',(79.8099316632486,6.95281565317284,132.26065975676));
#61123=CARTESIAN_POINT('Ctrl Pts',(79.738941786399,6.96065588775716,132.256800354037));
#61124=CARTESIAN_POINT('Ctrl Pts',(79.6686129323736,6.97214887777481,132.252940951314));
#61125=CARTESIAN_POINT('Ctrl Pts',(79.5982442575986,6.98364837521368,132.249079363367));
#61126=CARTESIAN_POINT('Ctrl Pts',(79.5285378256331,6.99880464201056,132.24521777542));
#61127=CARTESIAN_POINT('Ctrl Pts',(79.4598928447495,7.01750616057775,132.241356187473));
#61128=CARTESIAN_POINT('Ctrl Pts',(79.3911277670113,7.036240398122,132.23748784354));
#61129=CARTESIAN_POINT('Ctrl Pts',(79.3234283095602,7.05853211901331,132.233619499606));
#61130=CARTESIAN_POINT('Ctrl Pts',(79.2571763442846,7.08422063404745,132.229751155673));
#61131=CARTESIAN_POINT('Ctrl Pts',(79.2178378338805,7.09947373501935,132.227454244367));
#61132=CARTESIAN_POINT('Ctrl Pts',(79.1790092532518,7.11592351035826,132.225157333061));
#61133=CARTESIAN_POINT('Ctrl Pts',(79.1407663493563,7.13352870472071,132.222860421755));
#61134=CARTESIAN_POINT('Ctrl Pts',(79.0763472474524,7.16318416218213,132.218991338908));
#61135=CARTESIAN_POINT('Ctrl Pts',(79.013339061303,7.19623664486004,132.215122256061));
#61136=CARTESIAN_POINT('Ctrl Pts',(78.9521236242196,7.23252930333163,132.211253173215));
#61137=CARTESIAN_POINT('Ctrl Pts',(78.8909993950846,7.26876788755209,132.207389855108));
#61138=CARTESIAN_POINT('Ctrl Pts',(78.8316630274031,7.30823681899428,132.203526537002));
#61139=CARTESIAN_POINT('Ctrl Pts',(78.7744744529044,7.35073207273163,132.199663218896));
#61140=CARTESIAN_POINT('Ctrl Pts',(78.7173529605816,7.39317747955271,132.19580443246));
#61141=CARTESIAN_POINT('Ctrl Pts',(78.6623746451652,7.4386418690834,132.191945646024));
#61142=CARTESIAN_POINT('Ctrl Pts',(78.6098714810442,7.48687731386848,132.188086859588));
#61143=CARTESIAN_POINT('Ctrl Pts',(78.5574013900668,7.53508237386029,132.184230503905));
#61144=CARTESIAN_POINT('Ctrl Pts',(78.5074037139143,7.58605469806288,132.180374148222));
#61145=CARTESIAN_POINT('Ctrl Pts',(78.4601771161135,7.63950632167599,132.176517792539));
#61146=CARTESIAN_POINT('Ctrl Pts',(78.4129644695226,7.69294215514429,132.172662576062));
#61147=CARTESIAN_POINT('Ctrl Pts',(78.3685215975986,7.74885547014025,132.168807359585));
#61148=CARTESIAN_POINT('Ctrl Pts',(78.3271088597398,7.80692297174955,132.164952143108));
#61149=CARTESIAN_POINT('Ctrl Pts',(78.2856945027668,7.86499274362452,132.161096775903));
#61150=CARTESIAN_POINT('Ctrl Pts',(78.2473107953371,7.9252164725418,132.157241408699));
#61151=CARTESIAN_POINT('Ctrl Pts',(78.2121754805812,7.98724087253438,132.153386041494));
#61152=CARTESIAN_POINT('Ctrl Pts',(78.1770033887317,8.04933019516052,132.149526638771));
#61153=CARTESIAN_POINT('Ctrl Pts',(78.1450867170065,8.11322352782564,132.145667236049));
#61154=CARTESIAN_POINT('Ctrl Pts',(78.1165973717164,8.17854269601251,132.141807833326));
#61155=CARTESIAN_POINT('Ctrl Pts',(78.0880918955352,8.24389884842555,132.137946245379));
#61156=CARTESIAN_POINT('Ctrl Pts',(78.063017779716,8.310681988484,132.134084657432));
#61157=CARTESIAN_POINT('Ctrl Pts',(78.0414978573552,8.37849624316854,132.130223069485));
#61158=CARTESIAN_POINT('Ctrl Pts',(78.0199402851188,8.44642914132239,132.126354725552));
#61159=CARTESIAN_POINT('Ctrl Pts',(78.001949443788,8.51539628558163,132.122486381619));
#61160=CARTESIAN_POINT('Ctrl Pts',(77.9875974528441,8.58498969807929,132.118618037685));
#61161=CARTESIAN_POINT('Ctrl Pts',(77.9790756536327,8.626312263712,132.116321126378));
#61162=CARTESIAN_POINT('Ctrl Pts',(77.9718357960167,8.66785547309974,132.114024215071));
#61163=CARTESIAN_POINT('Ctrl Pts',(77.9658843036767,8.70953331263113,132.111727303764));
#61164=CARTESIAN_POINT('Ctrl Pts',(77.9522361754433,8.80511009672412,132.106459962688));
#61165=CARTESIAN_POINT('Ctrl Pts',(77.9453221472454,8.90167081914922,132.101192621613));
#61166=CARTESIAN_POINT('Ctrl Pts',(77.9452505617463,8.99848062641328,132.095925280538));
#61167=CARTESIAN_POINT('Ctrl Pts',(77.9452505617457,8.99848062725764,132.095925280492));
#61168=CARTESIAN_POINT('Ctrl Pts',(77.9451965787833,9.07148539992385,132.091953151545));
#61169=CARTESIAN_POINT('Ctrl Pts',(77.9490383631329,9.14463767470539,132.087981022599));
#61170=CARTESIAN_POINT('Ctrl Pts',(77.9567917436018,9.21748007606708,132.084008893652));
#61171=CARTESIAN_POINT('Ctrl Pts',(77.9642163077101,9.28723327351193,132.080205220386));
#61172=CARTESIAN_POINT('Ctrl Pts',(77.9752273595376,9.35670178529796,132.07640154712));
#61173=CARTESIAN_POINT('Ctrl Pts',(77.989785708765,9.42548333200558,132.072597873854));
#61174=CARTESIAN_POINT('Ctrl Pts',(78.0043341072357,9.49421786593538,132.068796800431));
#61175=CARTESIAN_POINT('Ctrl Pts',(78.0224248939572,9.56226587652216,132.064995727008));
#61176=CARTESIAN_POINT('Ctrl Pts',(78.0439673846338,9.62923284253429,132.061194653586));
#61177=CARTESIAN_POINT('Ctrl Pts',(78.0655028484982,9.69617796500439,132.057394820012));
#61178=CARTESIAN_POINT('Ctrl Pts',(78.0904876294811,9.76204226555299,132.053594986438));
#61179=CARTESIAN_POINT('Ctrl Pts',(78.1187810484405,9.82644589586581,132.049795152864));
#61180=CARTESIAN_POINT('Ctrl Pts',(78.1470753477332,9.8908515300601,132.04599520106));
#61181=CARTESIAN_POINT('Ctrl Pts',(78.1786782846807,9.95379594626292,132.042195249257));
#61182=CARTESIAN_POINT('Ctrl Pts',(78.2134016340244,10.0149206083204,132.038395297453));
#61183=CARTESIAN_POINT('Ctrl Pts',(78.2481601793031,10.076107226948,132.03459149398));
#61184=CARTESIAN_POINT('Ctrl Pts',(78.2860451976125,10.1354699758928,132.030787690508));
#61185=CARTESIAN_POINT('Ctrl Pts',(78.3268238180268,10.1926772516391,132.026983887035));
#61186=CARTESIAN_POINT('Ctrl Pts',(78.3676269245136,10.2499188782657,132.023177799517));
#61187=CARTESIAN_POINT('Ctrl Pts',(78.4113267751392,10.3050020670922,132.019371711999));
#61188=CARTESIAN_POINT('Ctrl Pts',(78.4576505098364,10.3576286726097,132.015565624481));
#61189=CARTESIAN_POINT('Ctrl Pts',(78.5040502056944,10.4103415746677,132.011753295782));
#61190=CARTESIAN_POINT('Ctrl Pts',(78.5530820149242,10.4605895045058,132.007940967083));
#61191=CARTESIAN_POINT('Ctrl Pts',(78.6044374301093,10.5081122889294,132.004128638384));
#61192=CARTESIAN_POINT('Ctrl Pts',(78.6203081568687,10.5227985907287,132.002950487513));
#61193=CARTESIAN_POINT('Ctrl Pts',(78.6364005734968,10.5372249326002,132.001772336643));
#61194=CARTESIAN_POINT('Ctrl Pts',(78.6527050052885,10.5513844654777,132.000594185772));
#61195=CARTESIAN_POINT('Ctrl Pts',(78.7062492490403,10.5978847967674,131.996725102925));
#61196=CARTESIAN_POINT('Ctrl Pts',(78.7623085494613,10.6417009236037,131.992856020077));
#61197=CARTESIAN_POINT('Ctrl Pts',(78.820582782277,10.6825494313804,131.98898693723));
#61198=CARTESIAN_POINT('Ctrl Pts',(78.8787701893921,10.7233370769178,131.985123619123));
#61199=CARTESIAN_POINT('Ctrl Pts',(78.9391655836706,10.7611656035921,131.981260301016));
#61200=CARTESIAN_POINT('Ctrl Pts',(79.0014348634834,10.7957909763203,131.977396982909));
#61201=CARTESIAN_POINT('Ctrl Pts',(79.0636311014549,10.8303757334996,131.973538196473));
#61202=CARTESIAN_POINT('Ctrl Pts',(79.1276964363556,10.8617645650649,131.969679410036));
#61203=CARTESIAN_POINT('Ctrl Pts',(79.1932682648415,10.8897569870193,131.9658206236));
#61204=CARTESIAN_POINT('Ctrl Pts',(79.2587987878836,10.9177317758004,131.961964267916));
#61205=CARTESIAN_POINT('Ctrl Pts',(79.325833476029,10.9423142094072,131.958107912232));
#61206=CARTESIAN_POINT('Ctrl Pts',(79.3939869504902,10.963350642734,131.954251556549));
#61207=CARTESIAN_POINT('Ctrl Pts',(79.4621202917326,10.9843808616877,131.950396340071));
#61208=CARTESIAN_POINT('Ctrl Pts',(79.5313712992336,11.001867016792,131.946541123593));
#61209=CARTESIAN_POINT('Ctrl Pts',(79.6013381641291,11.0157049146936,131.942685907115));
#61210=CARTESIAN_POINT('Ctrl Pts',(79.6713077645197,11.0295433536157,131.93883053991));
#61211=CARTESIAN_POINT('Ctrl Pts',(79.7419928008916,11.0397331600597,131.934975172705));
#61212=CARTESIAN_POINT('Ctrl Pts',(79.8129816751027,11.0462213244546,131.9311198055));
#61213=CARTESIAN_POINT('Ctrl Pts',(79.8840448553073,11.0527162801883,131.927260402777));
#61214=CARTESIAN_POINT('Ctrl Pts',(79.9554120234629,11.0555018149779,131.923401000053));
#61215=CARTESIAN_POINT('Ctrl Pts',(80.0266677680113,11.054576937632,131.91954159733));
#61216=CARTESIAN_POINT('Ctrl Pts',(80.097963858122,11.0536515366133,131.915680009382));
#61217=CARTESIAN_POINT('Ctrl Pts',(80.169147914051,11.0490115728982,131.911818421435));
#61218=CARTESIAN_POINT('Ctrl Pts',(80.2398085956789,11.0407080633786,131.907956833487));
#61219=CARTESIAN_POINT('Ctrl Pts',(80.3105929007018,11.0323900265716,131.904088489553));
#61220=CARTESIAN_POINT('Ctrl Pts',(80.3808515242716,11.0203957289771,131.90022014562));
#61221=CARTESIAN_POINT('Ctrl Pts',(80.4501829707135,11.0048273879263,131.896351801686));
#61222=CARTESIAN_POINT('Ctrl Pts',(80.491349988332,10.9955833550492,131.894054890384));
#61223=CARTESIAN_POINT('Ctrl Pts',(80.5321903805207,10.9850802059216,131.891757979082));
#61224=CARTESIAN_POINT('Ctrl Pts',(80.5726231150621,10.9733474936251,131.889461067781));
#61225=CARTESIAN_POINT('Ctrl Pts',(80.6407129225893,10.9535892919824,131.885593007651));
#61226=CARTESIAN_POINT('Ctrl Pts',(80.7079122298131,10.9302641370807,131.881724947521));
#61227=CARTESIAN_POINT('Ctrl Pts',(80.7738204657355,10.9034703699582,131.877856887391));
#61228=CARTESIAN_POINT('Ctrl Pts',(80.8396428369133,10.8767115095501,131.87399386654));
#61229=CARTESIAN_POINT('Ctrl Pts',(80.9041770261002,10.8464931786054,131.870130845689));
#61230=CARTESIAN_POINT('Ctrl Pts',(80.96703688535,10.8129636579018,131.866267824838));
#61231=CARTESIAN_POINT('Ctrl Pts',(81.0298266373822,10.7794715324681,131.86240911239));
#61232=CARTESIAN_POINT('Ctrl Pts',(81.0909453409541,10.7426757775587,131.858550399943));
#61233=CARTESIAN_POINT('Ctrl Pts',(81.1500279067695,10.702772261975,131.854691687496));
#61234=CARTESIAN_POINT('Ctrl Pts',(81.1847581408959,10.6793159611261,131.852423438227));
#61235=CARTESIAN_POINT('Ctrl Pts',(81.2187852183793,10.6547867047415,131.850155188957));
#61236=CARTESIAN_POINT('Ctrl Pts',(81.252039109102,10.6292316077768,131.847886939688));
#61237=CARTESIAN_POINT('',(77.945250271645,9.00105656286654,132.154074719416));
#61238=CARTESIAN_POINT('Ctrl Pts',(77.945250271645,9.00105656286652,132.154074719416));
#61239=CARTESIAN_POINT('Ctrl Pts',(77.945290872253,9.08001456044151,132.14981310901));
#61240=CARTESIAN_POINT('Ctrl Pts',(77.9498868100455,9.15881521208162,132.145551498605));
#61241=CARTESIAN_POINT('Ctrl Pts',(77.9589591217713,9.23695927054993,132.141289888199));
#61242=CARTESIAN_POINT('Ctrl Pts',(77.9680642943238,9.31538637466667,132.137012841811));
#61243=CARTESIAN_POINT('Ctrl Pts',(77.9816781914328,9.39315183738754,132.132735795423));
#61244=CARTESIAN_POINT('Ctrl Pts',(77.9996710506677,9.46976766274754,132.128458749035));
#61245=CARTESIAN_POINT('Ctrl Pts',(78.0177509651587,9.5467541801807,132.124161008917));
#61246=CARTESIAN_POINT('Ctrl Pts',(78.0402521766353,9.62257963403658,132.1198632688));
#61247=CARTESIAN_POINT('Ctrl Pts',(78.0669947748148,9.69676994905539,132.115565528682));
#61248=CARTESIAN_POINT('Ctrl Pts',(78.0794747989849,9.73139249838321,132.113559893321));
#61249=CARTESIAN_POINT('Ctrl Pts',(78.092877854504,9.76565926600136,132.11155425796));
#61250=CARTESIAN_POINT('Ctrl Pts',(78.1071822245978,9.79952387808082,132.109548622599));
#61251=CARTESIAN_POINT('Ctrl Pts',(78.1347768681956,9.86485229833167,132.105679539752));
#61252=CARTESIAN_POINT('Ctrl Pts',(78.1658116320374,9.92887839899923,132.101810456905));
#61253=CARTESIAN_POINT('Ctrl Pts',(78.2001418722774,9.9912155580755,132.097941374058));
#61254=CARTESIAN_POINT('Ctrl Pts',(78.2344209621716,10.0534598378936,132.094078055952));
#61255=CARTESIAN_POINT('Ctrl Pts',(78.2719855496265,10.1140197491266,132.090214737845));
#61256=CARTESIAN_POINT('Ctrl Pts',(78.3126431435276,10.1725290620772,132.086351419739));
#61257=CARTESIAN_POINT('Ctrl Pts',(78.3532530460867,10.2309697436262,132.082492633303));
#61258=CARTESIAN_POINT('Ctrl Pts',(78.3969484726027,10.2873642077462,132.078633846867));
#61259=CARTESIAN_POINT('Ctrl Pts',(78.4434921636946,10.3413727736987,132.074775060431));
#61260=CARTESIAN_POINT('Ctrl Pts',(78.4900065356741,10.3953473182149,132.070918704748));
#61261=CARTESIAN_POINT('Ctrl Pts',(78.5393652961919,10.4469385792557,132.067062349065));
#61262=CARTESIAN_POINT('Ctrl Pts',(78.5912901108146,10.4958388986155,132.063205993381));
#61263=CARTESIAN_POINT('Ctrl Pts',(78.6431995863272,10.5447247723314,132.059350776904));
#61264=CARTESIAN_POINT('Ctrl Pts',(78.6976732575757,10.59092094966,132.055495560427));
#61265=CARTESIAN_POINT('Ctrl Pts',(78.754396261352,10.6341569351706,132.051640343949));
#61266=CARTESIAN_POINT('Ctrl Pts',(78.8111214828281,10.6773946110789,132.047784976745));
#61267=CARTESIAN_POINT('Ctrl Pts',(78.8700958237476,10.7176715726603,132.04392960954));
#61268=CARTESIAN_POINT('Ctrl Pts',(78.9309730915489,10.7547589667836,132.040074242335));
#61269=CARTESIAN_POINT('Ctrl Pts',(78.9919140812491,10.7918851812953,132.036214839613));
#61270=CARTESIAN_POINT('Ctrl Pts',(79.0547615582919,10.8258149104839,132.03235543689));
#61271=CARTESIAN_POINT('Ctrl Pts',(79.1191429984107,10.8563643244932,132.028496034167));
#61272=CARTESIAN_POINT('Ctrl Pts',(79.1835608918065,10.8869310358206,132.02463444622));
#61273=CARTESIAN_POINT('Ctrl Pts',(79.2495140279323,10.9141134366664,132.020772858273));
#61274=CARTESIAN_POINT('Ctrl Pts',(79.3166106344549,10.9377761835568,132.016911270326));
#61275=CARTESIAN_POINT('Ctrl Pts',(79.3838246288955,10.961480329271,132.013042926392));
#61276=CARTESIAN_POINT('Ctrl Pts',(79.4521856218031,10.981652389358,132.009174582459));
#61277=CARTESIAN_POINT('Ctrl Pts',(79.5212881315139,10.9982073239458,132.005306238525));
#61278=CARTESIAN_POINT('Ctrl Pts',(79.5623192131717,11.0080371676917,132.00300932722));
#61279=CARTESIAN_POINT('Ctrl Pts',(79.6036115398423,11.0165927238093,132.000712415914));
#61280=CARTESIAN_POINT('Ctrl Pts',(79.6450793453087,11.023864840194,131.998415504608));
#61281=CARTESIAN_POINT('Ctrl Pts',(79.7149081391765,11.0361105597419,131.994547671615));
#61282=CARTESIAN_POINT('Ctrl Pts',(79.7855081655636,11.0447620939113,131.990679838623));
#61283=CARTESIAN_POINT('Ctrl Pts',(79.8564765514179,11.04973134391,131.98681200563));
#61284=CARTESIAN_POINT('Ctrl Pts',(79.9273493904378,11.0546939036607,131.982949380016));
#61285=CARTESIAN_POINT('Ctrl Pts',(79.9985891252934,11.0559839786253,131.979086754401));
#61286=CARTESIAN_POINT('Ctrl Pts',(80.069783895318,11.0535646496895,131.975224128786));
#61287=CARTESIAN_POINT('Ctrl Pts',(80.1409066359359,11.0511477684451,131.97136541108));
#61288=CARTESIAN_POINT('Ctrl Pts',(80.2119840191092,11.0450289459532,131.967506693374));
#61289=CARTESIAN_POINT('Ctrl Pts',(80.2826020050072,11.0352232480163,131.963647975667));
#61290=CARTESIAN_POINT('Ctrl Pts',(80.3531721706576,11.0254241901852,131.959791870961));
#61291=CARTESIAN_POINT('Ctrl Pts',(80.4232830766721,11.011943279796,131.955935766256));
#61292=CARTESIAN_POINT('Ctrl Pts',(80.4925253618703,10.9948474453989,131.95207966155));
#61293=CARTESIAN_POINT('Ctrl Pts',(80.5617703013114,10.9777509556725,131.948223409029));
#61294=CARTESIAN_POINT('Ctrl Pts',(80.6301460772591,10.9570393630094,131.944367156508));
#61295=CARTESIAN_POINT('Ctrl Pts',(80.6972543344538,10.9328305553217,131.940510903988));
#61296=CARTESIAN_POINT('Ctrl Pts',(80.7643590610101,10.9086230212858,131.936654854349));
#61297=CARTESIAN_POINT('Ctrl Pts',(80.830195946503,10.8809188100334,131.93279880471));
#61298=CARTESIAN_POINT('Ctrl Pts',(80.8943847491103,10.8498847215594,131.928942755071));
#61299=CARTESIAN_POINT('Ctrl Pts',(80.9586397009917,10.8188186511455,131.925082731609));
#61300=CARTESIAN_POINT('Ctrl Pts',(81.0212427411801,10.7844160658132,131.921222708148));
#61301=CARTESIAN_POINT('Ctrl Pts',(81.0818372046246,10.7468903300408,131.917362684687));
#61302=CARTESIAN_POINT('Ctrl Pts',(81.1405565478585,10.7105258433588,131.913622111215));
#61303=CARTESIAN_POINT('Ctrl Pts',(81.1973895050298,10.671228977131,131.909881537743));
#61304=CARTESIAN_POINT('Ctrl Pts',(81.252039109102,10.6292316077769,131.906140964271));
#61305=CARTESIAN_POINT('Ctrl Pts',(81.252039109102,10.6292316077768,132.606087908811));
#61306=CARTESIAN_POINT('Ctrl Pts',(81.3085934766705,10.5857704573497,132.602232450677));
#61307=CARTESIAN_POINT('Ctrl Pts',(81.3628750366858,10.5393667122732,132.598376992543));
#61308=CARTESIAN_POINT('Ctrl Pts',(81.4145730936508,10.4902954489695,132.594521534409));
#61309=CARTESIAN_POINT('Ctrl Pts',(81.4663263957117,10.4411717475896,132.590661956291));
#61310=CARTESIAN_POINT('Ctrl Pts',(81.5154903318637,10.389375174002,132.586802378173));
#61311=CARTESIAN_POINT('Ctrl Pts',(81.5617909040319,10.3352178603446,132.582942800055));
#61312=CARTESIAN_POINT('Ctrl Pts',(81.6081191546343,10.281028171501,132.579080914685));
#61313=CARTESIAN_POINT('Ctrl Pts',(81.651580338457,10.2244753190296,132.575219029315));
#61314=CARTESIAN_POINT('Ctrl Pts',(81.6919423182945,10.1659025491285,132.571357143945));
#61315=CARTESIAN_POINT('Ctrl Pts',(81.732373615701,10.1072291864904,132.567488626183));
#61316=CARTESIAN_POINT('Ctrl Pts',(81.7696948311514,10.0465293960011,132.56362010842));
#61317=CARTESIAN_POINT('Ctrl Pts',(81.8037189047984,9.98417258393685,132.559751590658));
#61318=CARTESIAN_POINT('Ctrl Pts',(81.8203431338944,9.95370492329718,132.557861425294));
#61319=CARTESIAN_POINT('Ctrl Pts',(81.8361809518681,9.92284200712804,132.55597125993));
#61320=CARTESIAN_POINT('Ctrl Pts',(81.8512147628781,9.89162854608986,132.554081094566));
#61321=CARTESIAN_POINT('Ctrl Pts',(81.8819882927564,9.82773600578652,132.550212011719));
#61322=CARTESIAN_POINT('Ctrl Pts',(81.9095104472027,9.76212328485629,132.546342928872));
#61323=CARTESIAN_POINT('Ctrl Pts',(81.933586765323,9.6951545033067,132.542473846025));
#61324=CARTESIAN_POINT('Ctrl Pts',(81.9576272109301,9.62828550190184,132.538610527919));
#61325=CARTESIAN_POINT('Ctrl Pts',(81.9782318482965,9.5600649038539,132.534747209812));
#61326=CARTESIAN_POINT('Ctrl Pts',(81.9952531484607,9.49087924793937,132.530883891706));
#61327=CARTESIAN_POINT('Ctrl Pts',(82.0122544826464,9.42177474677252,132.52702510527));
#61328=CARTESIAN_POINT('Ctrl Pts',(82.0256807132235,9.35170790572679,132.523166318834));
#61329=CARTESIAN_POINT('Ctrl Pts',(82.0354338270114,9.28108130204246,132.519307532398));
#61330=CARTESIAN_POINT('Ctrl Pts',(82.0451807970527,9.2104991879396,132.515451176715));
#61331=CARTESIAN_POINT('Ctrl Pts',(82.0512591745402,9.13935849084858,132.511594821032));
#61332=CARTESIAN_POINT('Ctrl Pts',(82.053622127359,9.06807143689828,132.507738465349));
#61333=CARTESIAN_POINT('Ctrl Pts',(82.0559843821379,8.99680544185754,132.503883248871));
#61334=CARTESIAN_POINT('Ctrl Pts',(82.0546333751518,8.92539366104356,132.500028032394));
#61335=CARTESIAN_POINT('Ctrl Pts',(82.0495743065814,8.85425116020526,132.496172815917));
#61336=CARTESIAN_POINT('Ctrl Pts',(82.0445150402164,8.78310587790798,132.492317448712));
#61337=CARTESIAN_POINT('Ctrl Pts',(82.0357474610953,8.7122303808916,132.488462081508));
#61338=CARTESIAN_POINT('Ctrl Pts',(82.0233287253964,8.6420357119965,132.484606714303));
#61339=CARTESIAN_POINT('Ctrl Pts',(82.0108969906676,8.57176756842425,132.48074731158));
#61340=CARTESIAN_POINT('Ctrl Pts',(81.9948065550643,8.50218215489968,132.476887908857));
#61341=CARTESIAN_POINT('Ctrl Pts',(81.9751657636099,8.43368050646001,132.473028506135));
#61342=CARTESIAN_POINT('Ctrl Pts',(81.955513851385,8.36514007184891,132.469166918188));
#61343=CARTESIAN_POINT('Ctrl Pts',(81.932307739648,8.29768508346071,132.465305330241));
#61344=CARTESIAN_POINT('Ctrl Pts',(81.9057048777047,8.23169896421214,132.461443742294));
#61345=CARTESIAN_POINT('Ctrl Pts',(81.8790554731008,8.16559739988277,132.45757539836));
#61346=CARTESIAN_POINT('Ctrl Pts',(81.848997658377,8.10097027606216,132.453707054427));
#61347=CARTESIAN_POINT('Ctrl Pts',(81.8157356889673,8.0381780464605,132.449838710493));
#61348=CARTESIAN_POINT('Ctrl Pts',(81.7959856887279,8.00089382752599,132.447541799187));
#61349=CARTESIAN_POINT('Ctrl Pts',(81.7751068783498,7.96425601836013,132.44524488788));
#61350=CARTESIAN_POINT('Ctrl Pts',(81.7531490904374,7.92833502007459,132.442947976574));
#61351=CARTESIAN_POINT('Ctrl Pts',(81.7161618108982,7.86782710323811,132.439078893727));
#61352=CARTESIAN_POINT('Ctrl Pts',(81.6759658686668,7.80911778233093,132.43520981088));
#61353=CARTESIAN_POINT('Ctrl Pts',(81.6327617012439,7.75256792190871,132.431340728033));
#61354=CARTESIAN_POINT('Ctrl Pts',(81.5896219058757,7.69610231795813,132.427477409927));
#61355=CARTESIAN_POINT('Ctrl Pts',(81.5434830746862,7.64179017073909,132.42361409182));
#61356=CARTESIAN_POINT('Ctrl Pts',(81.4945899348819,7.58996507523763,132.419750773714));
#61357=CARTESIAN_POINT('Ctrl Pts',(81.4457541467119,7.53820077055332,132.415891987278));
#61358=CARTESIAN_POINT('Ctrl Pts',(81.3941707991377,7.48891807445518,132.412033200842));
#61359=CARTESIAN_POINT('Ctrl Pts',(81.3401249501949,7.44241768103089,132.408174414406));
#61360=CARTESIAN_POINT('Ctrl Pts',(81.2861131461738,7.39594657944474,132.404318058723));
#61361=CARTESIAN_POINT('Ctrl Pts',(81.2296422857038,7.3522546193917,132.40046170304));
#61362=CARTESIAN_POINT('Ctrl Pts',(81.1710332927737,7.31160472942042,132.396605347356));
#61363=CARTESIAN_POINT('Ctrl Pts',(81.112441613527,7.27096684783369,132.392750130879));
#61364=CARTESIAN_POINT('Ctrl Pts',(81.0517134547249,7.23336952894758,132.388894914402));
#61365=CARTESIAN_POINT('Ctrl Pts',(80.9892003473081,7.19903352741216,132.385039697925));
#61366=CARTESIAN_POINT('Ctrl Pts',(80.9266847958158,7.16469618344176,132.38118433072));
#61367=CARTESIAN_POINT('Ctrl Pts',(80.8623845840016,7.13362064190744,132.377328963515));
#61368=CARTESIAN_POINT('Ctrl Pts',(80.7966760429388,7.10598182556042,132.373473596311));
#61369=CARTESIAN_POINT('Ctrl Pts',(80.7308987229513,7.07831407890945,132.369614193588));
#61370=CARTESIAN_POINT('Ctrl Pts',(80.6637105797082,7.05409042722656,132.365754790865));
#61371=CARTESIAN_POINT('Ctrl Pts',(80.5955073002181,7.03343735978563,132.361895388142));
#61372=CARTESIAN_POINT('Ctrl Pts',(80.5272654034953,7.01277259841565,132.358033800195));
#61373=CARTESIAN_POINT('Ctrl Pts',(80.458007698179,6.99568256229063,132.354172212249));
#61374=CARTESIAN_POINT('Ctrl Pts',(80.3881417079493,6.98224293408492,132.350310624302));
#61375=CARTESIAN_POINT('Ctrl Pts',(80.3181534846654,6.96877979276795,132.346442280368));
#61376=CARTESIAN_POINT('Ctrl Pts',(80.2475553330518,6.95897987705045,132.342573936435));
#61377=CARTESIAN_POINT('Ctrl Pts',(80.1767608663212,6.95286708818471,132.338705592501));
#61378=CARTESIAN_POINT('Ctrl Pts',(80.1347251492656,6.94923749006711,132.336408681195));
#61379=CARTESIAN_POINT('Ctrl Pts',(80.0926202580339,6.94690684262272,132.334111769889));
#61380=CARTESIAN_POINT('Ctrl Pts',(80.0505323671528,6.94587146400963,132.331814858582));
#61381=CARTESIAN_POINT('Ctrl Pts',(79.9796364922357,6.94412739769725,132.327945775735));
#61382=CARTESIAN_POINT('Ctrl Pts',(79.9085113617539,6.9460545580838,132.324076692888));
#61383=CARTESIAN_POINT('Ctrl Pts',(79.8375688633129,6.95168027682821,132.320207610042));
#61384=CARTESIAN_POINT('Ctrl Pts',(79.7667320656567,6.95729761353225,132.316344291935));
#61385=CARTESIAN_POINT('Ctrl Pts',(79.696077840223,6.96660253198248,132.312480973829));
#61386=CARTESIAN_POINT('Ctrl Pts',(79.6260191864149,6.97957036411307,132.308617655722));
#61387=CARTESIAN_POINT('Ctrl Pts',(79.5560427113805,6.99252298498158,132.304758869287));
#61388=CARTESIAN_POINT('Ctrl Pts',(79.486660895656,7.00912989704807,132.300900082851));
#61389=CARTESIAN_POINT('Ctrl Pts',(79.4182809721592,7.02931470418336,132.297041296415));
#61390=CARTESIAN_POINT('Ctrl Pts',(79.349944123,7.04948679637026,132.293184940732));
#61391=CARTESIAN_POINT('Ctrl Pts',(79.2826083787462,7.07323217489448,132.289328585049));
#61392=CARTESIAN_POINT('Ctrl Pts',(79.2166686972246,7.10042382816793,132.285472229365));
#61393=CARTESIAN_POINT('Ctrl Pts',(79.150748494945,7.12760744875476,132.281617012888));
#61394=CARTESIAN_POINT('Ctrl Pts',(79.0862239854998,7.15823513785706,132.277761796411));
#61395=CARTESIAN_POINT('Ctrl Pts',(79.0234712956366,7.19213129568149,132.273906579934));
#61396=CARTESIAN_POINT('Ctrl Pts',(78.9607161523311,7.22602877874419,132.270051212729));
#61397=CARTESIAN_POINT('Ctrl Pts',(78.8997333925084,7.26319475142531,132.266195845525));
#61398=CARTESIAN_POINT('Ctrl Pts',(78.8408740891257,7.30340792020011,132.26234047832));
#61399=CARTESIAN_POINT('Ctrl Pts',(78.7819531761023,7.34366318119709,132.258481075597));
#61400=CARTESIAN_POINT('Ctrl Pts',(78.7251605584152,7.38697173080948,132.254621672874));
#61401=CARTESIAN_POINT('Ctrl Pts',(78.6708171167339,7.43306974458579,132.250762270152));
#61402=CARTESIAN_POINT('Ctrl Pts',(78.616442905369,7.47919385941963,132.246900682205));
#61403=CARTESIAN_POINT('Ctrl Pts',(78.5645209843359,7.52811024927646,132.243039094258));
#61404=CARTESIAN_POINT('Ctrl Pts',(78.5153359699768,7.57951758882584,132.239177506311));
#61405=CARTESIAN_POINT('Ctrl Pts',(78.4660649046721,7.6310148673584,132.235309162378));
#61406=CARTESIAN_POINT('Ctrl Pts',(78.4195406232418,7.68501142832933,132.231440818444));
#61407=CARTESIAN_POINT('Ctrl Pts',(78.3760075415854,7.74117274516616,132.227572474511));
#61408=CARTESIAN_POINT('Ctrl Pts',(78.35015885047,7.77451971892297,132.225275563204));
#61409=CARTESIAN_POINT('Ctrl Pts',(78.3253639320698,7.80862933347536,132.222978651898));
#61410=CARTESIAN_POINT('Ctrl Pts',(78.3016664325151,7.84342719379448,132.220681740591));
#61411=CARTESIAN_POINT('Ctrl Pts',(78.2611561583561,7.90291325300599,132.216755228997));
#61412=CARTESIAN_POINT('Ctrl Pts',(78.22369963522,7.96464047795975,132.212828717404));
#61413=CARTESIAN_POINT('Ctrl Pts',(78.1895485268499,8.02826802776241,132.20890220581));
#61414=CARTESIAN_POINT('Ctrl Pts',(78.155452465025,8.09179301934779,132.204982023173));
#61415=CARTESIAN_POINT('Ctrl Pts',(78.124651456215,8.15721184504486,132.201061840536));
#61416=CARTESIAN_POINT('Ctrl Pts',(78.0973541022693,8.22415455769291,132.1971416579));
#61417=CARTESIAN_POINT('Ctrl Pts',(78.0700989505562,8.29099377562381,132.19322753594));
#61418=CARTESIAN_POINT('Ctrl Pts',(78.0463368576601,8.3593517657761,132.189313413981));
#61419=CARTESIAN_POINT('Ctrl Pts',(78.0262298521907,8.4288354299182,132.185399292022));
#61420=CARTESIAN_POINT('Ctrl Pts',(78.0061411816452,8.49825573416795,132.181488739223));
#61421=CARTESIAN_POINT('Ctrl Pts',(77.9897011084489,8.56879922704156,132.177578186424));
#61422=CARTESIAN_POINT('Ctrl Pts',(77.9770226384295,8.64005534165216,132.173667633625));
#61423=CARTESIAN_POINT('Ctrl Pts',(77.9643515390461,8.71127003147841,132.169759354229));
#61424=CARTESIAN_POINT('Ctrl Pts',(77.9554377814962,8.78319606135745,132.165851074832));
#61425=CARTESIAN_POINT('Ctrl Pts',(77.950343495397,8.85541170296763,132.161942795435));
#61426=CARTESIAN_POINT('Ctrl Pts',(77.9469249211356,8.9038727687336,132.159320103444));
#61427=CARTESIAN_POINT('Ctrl Pts',(77.9452252851269,8.9524640140981,132.156697411453));
#61428=CARTESIAN_POINT('Ctrl Pts',(77.9452502716446,9.00105656201739,132.154074719462));
#61429=CARTESIAN_POINT('Origin',(80.,9.,141.545925280538));
#61430=CARTESIAN_POINT('',(81.252039109102,10.6292316077768,133.306011340678));
#61431=CARTESIAN_POINT('',(81.252039109102,10.6292316077768,133.247993489861));
#61432=CARTESIAN_POINT('',(81.252039109102,10.6292316077768,141.545925280538));
#61433=CARTESIAN_POINT('',(77.9452506345969,9.00161489178516,132.795925280579));
#61434=CARTESIAN_POINT('Ctrl Pts',(81.252039109102,10.6292316077768,133.247993489861));
#61435=CARTESIAN_POINT('Ctrl Pts',(81.3085458565354,10.5858070526816,133.244130559018));
#61436=CARTESIAN_POINT('Ctrl Pts',(81.3627300216765,10.5394860857007,133.240267628176));
#61437=CARTESIAN_POINT('Ctrl Pts',(81.4142959510654,10.4905584608797,133.236404697333));
#61438=CARTESIAN_POINT('Ctrl Pts',(81.4659453705785,10.4415516175995,133.232535512039));
#61439=CARTESIAN_POINT('Ctrl Pts',(81.5149677678158,10.3899300517469,133.228666326745));
#61440=CARTESIAN_POINT('Ctrl Pts',(81.5611066388145,10.3360178235148,133.224797141451));
#61441=CARTESIAN_POINT('Ctrl Pts',(81.5680176291622,10.3279424874507,133.224217588861));
#61442=CARTESIAN_POINT('Ctrl Pts',(81.5748640032644,10.3198158116359,133.22363803627));
#61443=CARTESIAN_POINT('Ctrl Pts',(81.5816449834367,10.3116389399791,133.223058483679));
#61444=CARTESIAN_POINT('Ctrl Pts',(81.6269146871559,10.2570502893934,133.219189400832));
#61445=CARTESIAN_POINT('Ctrl Pts',(81.6694436428746,10.200008321872,133.215320317985));
#61446=CARTESIAN_POINT('Ctrl Pts',(81.7089553397542,10.1408195340305,133.211451235138));
#61447=CARTESIAN_POINT('Ctrl Pts',(81.7484081661761,10.0817189345309,133.207587917032));
#61448=CARTESIAN_POINT('Ctrl Pts',(81.7848523898166,10.0204782646923,133.203724598926));
#61449=CARTESIAN_POINT('Ctrl Pts',(81.8180516424326,9.95743709346783,133.199861280819));
#61450=CARTESIAN_POINT('Ctrl Pts',(81.851211952338,9.8944698695129,133.196002494383));
#61451=CARTESIAN_POINT('Ctrl Pts',(81.88113462666,9.82970676703115,133.192143707948));
#61452=CARTESIAN_POINT('Ctrl Pts',(81.9076274856163,9.76351485815351,133.188284921512));
#61453=CARTESIAN_POINT('Ctrl Pts',(81.9341036560141,9.69736464532483,133.184428565829));
#61454=CARTESIAN_POINT('Ctrl Pts',(81.9571541174251,9.62978786170638,133.180572210145));
#61455=CARTESIAN_POINT('Ctrl Pts',(81.9766340351604,9.56117328299337,133.176715854462));
#61456=CARTESIAN_POINT('Ctrl Pts',(81.9961081983329,9.49257897371396,133.172860637985));
#61457=CARTESIAN_POINT('Ctrl Pts',(82.0120137792494,9.422947945037,133.169005421508));
#61458=CARTESIAN_POINT('Ctrl Pts',(82.0242557560879,9.35268427303351,133.16515020503));
#61459=CARTESIAN_POINT('Ctrl Pts',(82.036498211551,9.28241785393061,133.161294837826));
#61460=CARTESIAN_POINT('Ctrl Pts',(82.0450766973487,9.21151922134589,133.157439470621));
#61461=CARTESIAN_POINT('Ctrl Pts',(82.0499475849728,9.1404010732302,133.153584103417));
#61462=CARTESIAN_POINT('Ctrl Pts',(82.054823571088,9.06920848380641,133.149724700694));
#61463=CARTESIAN_POINT('Ctrl Pts',(82.055984178733,8.99779640581406,133.145865297971));
#61464=CARTESIAN_POINT('Ctrl Pts',(82.0534378710938,8.92658016577487,133.142005895248));
#61465=CARTESIAN_POINT('Ctrl Pts',(82.0508901217152,8.85532360254116,133.138144307301));
#61466=CARTESIAN_POINT('Ctrl Pts',(82.0446313214623,8.78426358213725,133.134282719354));
#61467=CARTESIAN_POINT('Ctrl Pts',(82.0347218354742,8.71381017707747,133.130421131407));
#61468=CARTESIAN_POINT('Ctrl Pts',(82.0247950124852,8.64323351126023,133.126552787474));
#61469=CARTESIAN_POINT('Ctrl Pts',(82.0112048445784,8.57326605671479,133.122684443541));
#61470=CARTESIAN_POINT('Ctrl Pts',(81.9940626600268,8.50430687881827,133.118816099607));
#61471=CARTESIAN_POINT('Ctrl Pts',(81.9838841241492,8.46336090345577,133.116519188301));
#61472=CARTESIAN_POINT('Ctrl Pts',(81.972454231622,8.42277012445263,133.114222276994));
#61473=CARTESIAN_POINT('Ctrl Pts',(81.9598043720399,8.38261488045671,133.111925365688));
#61474=CARTESIAN_POINT('Ctrl Pts',(81.9384960374133,8.31497449516047,133.108056282841));
#61475=CARTESIAN_POINT('Ctrl Pts',(81.9136400623008,8.24830607209196,133.104187199994));
#61476=CARTESIAN_POINT('Ctrl Pts',(81.8853439706103,8.1830081548855,133.100318117147));
#61477=CARTESIAN_POINT('Ctrl Pts',(81.8570900386851,8.1178075283191,133.096454799041));
#61478=CARTESIAN_POINT('Ctrl Pts',(81.8254063559397,8.05397379643129,133.092591480934));
#61479=CARTESIAN_POINT('Ctrl Pts',(81.7904500040001,7.99188971551923,133.088728162828));
#61480=CARTESIAN_POINT('Ctrl Pts',(81.755534655848,7.92987845921018,133.084869376392));
#61481=CARTESIAN_POINT('Ctrl Pts',(81.7173545009174,7.86961319847797,133.081010589956));
#61482=CARTESIAN_POINT('Ctrl Pts',(81.6761136941158,7.81145448261441,133.07715180352));
#61483=CARTESIAN_POINT('Ctrl Pts',(81.6348988659985,7.75333240247726,133.073295447837));
#61484=CARTESIAN_POINT('Ctrl Pts',(81.5906274914358,7.69731462985278,133.069439092154));
#61485=CARTESIAN_POINT('Ctrl Pts',(81.5435476382642,7.64373370944009,133.065582736471));
#61486=CARTESIAN_POINT('Ctrl Pts',(81.4964816929526,7.59016861736779,133.061727519993));
#61487=CARTESIAN_POINT('Ctrl Pts',(81.4466092365961,7.5390393130905,133.057872303516));
#61488=CARTESIAN_POINT('Ctrl Pts',(81.3942182089018,7.49064479049277,133.054017087039));
#61489=CARTESIAN_POINT('Ctrl Pts',(81.341825132875,7.44224837581396,133.050161719834));
#61490=CARTESIAN_POINT('Ctrl Pts',(81.2869136483497,7.39658728309613,133.04630635263));
#61491=CARTESIAN_POINT('Ctrl Pts',(81.229806813281,7.35392200533889,133.042450985425));
#61492=CARTESIAN_POINT('Ctrl Pts',(81.1726402029284,7.31121206867012,133.038591582702));
#61493=CARTESIAN_POINT('Ctrl Pts',(81.1132740448049,7.27150449807019,133.034732179979));
#61494=CARTESIAN_POINT('Ctrl Pts',(81.052061858725,7.23501744826862,133.030872777257));
#61495=CARTESIAN_POINT('Ctrl Pts',(80.9908150138244,7.19850973921284,133.02701118931));
#61496=CARTESIAN_POINT('Ctrl Pts',(80.9277204900948,7.16522640771259,133.023149601363));
#61497=CARTESIAN_POINT('Ctrl Pts',(80.8631555438834,7.13533915427942,133.019288013416));
#61498=CARTESIAN_POINT('Ctrl Pts',(80.7984776389843,7.1053996120251,133.015419669482));
#61499=CARTESIAN_POINT('Ctrl Pts',(80.7323246264365,7.07886819121591,133.011551325549));
#61500=CARTESIAN_POINT('Ctrl Pts',(80.6650921565278,7.05586780649431,133.007682981615));
#61501=CARTESIAN_POINT('Ctrl Pts',(80.6251714506782,7.04221083994012,133.005386070309));
#61502=CARTESIAN_POINT('Ctrl Pts',(80.5848704458188,7.02979783101441,133.003089159003));
#61503=CARTESIAN_POINT('Ctrl Pts',(80.5442736622037,7.0186459823819,133.000792247696));
#61504=CARTESIAN_POINT('Ctrl Pts',(80.4758895157695,6.99986100529781,132.996923164849));
#61505=CARTESIAN_POINT('Ctrl Pts',(80.4063977765704,6.98458369151803,132.993054082002));
#61506=CARTESIAN_POINT('Ctrl Pts',(80.3361915931481,6.97293986887499,132.989184999155));
#61507=CARTESIAN_POINT('Ctrl Pts',(80.2660900134378,6.96131339494699,132.985321681049));
#61508=CARTESIAN_POINT('Ctrl Pts',(80.1952765778126,6.95330974490485,132.981458362943));
#61509=CARTESIAN_POINT('Ctrl Pts',(80.1241580504811,6.94900454876157,132.977595044836));
#61510=CARTESIAN_POINT('Ctrl Pts',(80.0531229451549,6.94470440261171,132.9737362584));
#61511=CARTESIAN_POINT('Ctrl Pts',(79.9817839415205,6.94409412226872,132.969877471965));
#61512=CARTESIAN_POINT('Ctrl Pts',(79.9105546785681,6.94719774528233,132.966018685529));
#61513=CARTESIAN_POINT('Ctrl Pts',(79.8393702848284,6.95029941324102,132.962162329846));
#61514=CARTESIAN_POINT('Ctrl Pts',(79.7682959787961,6.95711032195449,132.958305974162));
#61515=CARTESIAN_POINT('Ctrl Pts',(79.6977456893852,6.96760242712831,132.954449618479));
#61516=CARTESIAN_POINT('Ctrl Pts',(79.6272162412362,6.97809143282919,132.950594402002));
#61517=CARTESIAN_POINT('Ctrl Pts',(79.557210982625,6.99225940465597,132.946739185525));
#61518=CARTESIAN_POINT('Ctrl Pts',(79.4881372810345,7.01002660333531,132.942883969047));
#61519=CARTESIAN_POINT('Ctrl Pts',(79.4190608788688,7.02779449665898,132.939028601843));
#61520=CARTESIAN_POINT('Ctrl Pts',(79.3509165759529,7.04916177306653,132.935173234638));
#61521=CARTESIAN_POINT('Ctrl Pts',(79.2840984413495,7.07399830716018,132.931317867434));
#61522=CARTESIAN_POINT('Ctrl Pts',(79.2172103663797,7.09886083833244,132.927458464711));
#61523=CARTESIAN_POINT('Ctrl Pts',(79.1516516870314,7.12719970661276,132.923599061988));
#61524=CARTESIAN_POINT('Ctrl Pts',(79.0877974244993,7.15883623114352,132.919739659265));
#61525=CARTESIAN_POINT('Ctrl Pts',(79.023907007182,7.19049066852297,132.915878071318));
#61526=CARTESIAN_POINT('Ctrl Pts',(78.9617233514694,7.2254462409346,132.912016483371));
#61527=CARTESIAN_POINT('Ctrl Pts',(78.9015953250588,7.26347912982095,132.908154895425));
#61528=CARTESIAN_POINT('Ctrl Pts',(78.8413621025109,7.30157855860964,132.904286551491));
#61529=CARTESIAN_POINT('Ctrl Pts',(78.783192086163,7.34276577212785,132.900418207558));
#61530=CARTESIAN_POINT('Ctrl Pts',(78.7274031336019,7.38677503796476,132.896549863624));
#61531=CARTESIAN_POINT('Ctrl Pts',(78.6942772590376,7.41290647354205,132.894252952318));
#61532=CARTESIAN_POINT('Ctrl Pts',(78.6619902077257,7.44003210903366,132.891956041011));
#61533=CARTESIAN_POINT('Ctrl Pts',(78.6306022743162,7.46809026656532,132.889659129705));
#61534=CARTESIAN_POINT('Ctrl Pts',(78.5772314750466,7.51579924676339,132.885753552658));
#61535=CARTESIAN_POINT('Ctrl Pts',(78.5262345230156,7.56641041597008,132.881847975611));
#61536=CARTESIAN_POINT('Ctrl Pts',(78.477949149806,7.6196526625796,132.877942398564));
#61537=CARTESIAN_POINT('Ctrl Pts',(78.4309056772215,7.67152551769528,132.874137273026));
#61538=CARTESIAN_POINT('Ctrl Pts',(78.3864363620088,7.72589535691467,132.870332147487));
#61539=CARTESIAN_POINT('Ctrl Pts',(78.3448201620119,7.78247083549608,132.866527021949));
#61540=CARTESIAN_POINT('Ctrl Pts',(78.3032434930467,7.83899257329763,132.862725510881));
#61541=CARTESIAN_POINT('Ctrl Pts',(78.2645148635039,7.89771539628927,132.858923999814));
#61542=CARTESIAN_POINT('Ctrl Pts',(78.2288739527535,7.95831382496211,132.855122488746));
#61543=CARTESIAN_POINT('Ctrl Pts',(78.1932541443471,8.0188763743923,132.851323228485));
#61544=CARTESIAN_POINT('Ctrl Pts',(78.1607186828807,8.08131189584067,132.847523968224));
#61545=CARTESIAN_POINT('Ctrl Pts',(78.1314636677262,8.14526639385559,132.843724707962));
#61546=CARTESIAN_POINT('Ctrl Pts',(78.100791622899,8.21231866573619,132.839741422347));
#61547=CARTESIAN_POINT('Ctrl Pts',(78.0737261978919,8.28104029941798,132.835758136732));
#61548=CARTESIAN_POINT('Ctrl Pts',(78.0504379098928,8.35099674937886,132.831774851116));
#61549=CARTESIAN_POINT('Ctrl Pts',(78.0282173314799,8.4177458715944,132.827974189155));
#61550=CARTESIAN_POINT('Ctrl Pts',(78.009435232024,8.48561853618905,132.824173527193));
#61551=CARTESIAN_POINT('Ctrl Pts',(77.9941886715372,8.55422149321622,132.820372865231));
#61552=CARTESIAN_POINT('Ctrl Pts',(77.9789361563187,8.6228512439721,132.816570718874));
#61553=CARTESIAN_POINT('Ctrl Pts',(77.9672220126629,8.69221136049643,132.812768572516));
#61554=CARTESIAN_POINT('Ctrl Pts',(77.9590918603005,8.76190017259942,132.808966426159));
#61555=CARTESIAN_POINT('Ctrl Pts',(77.950951700675,8.83167476344796,132.805159599806));
#61556=CARTESIAN_POINT('Ctrl Pts',(77.9464043599199,8.9017783571423,132.801352773453));
#61557=CARTESIAN_POINT('Ctrl Pts',(77.9454434209989,8.97180733812918,132.797545947101));
#61558=CARTESIAN_POINT('Ctrl Pts',(77.9453070553061,8.98174506705064,132.797005724927));
#61559=CARTESIAN_POINT('Ctrl Pts',(77.9452428274764,8.99168129996617,132.796465502753));
#61560=CARTESIAN_POINT('Ctrl Pts',(77.9452506345969,9.00161489178516,132.795925280579));
#61561=CARTESIAN_POINT('Ctrl Pts',(77.9452506345975,9.0016148925345,132.795925280538));
#61562=CARTESIAN_POINT('Ctrl Pts',(77.9453344508848,9.1082606658194,132.790125524263));
#61563=CARTESIAN_POINT('Ctrl Pts',(77.9537227446016,9.21458734448351,132.784325767988));
#61564=CARTESIAN_POINT('Ctrl Pts',(77.9702575839437,9.3195986341677,132.778526011713));
#61565=CARTESIAN_POINT('Ctrl Pts',(77.9812881618236,9.38965285030926,132.774656928866));
#61566=CARTESIAN_POINT('Ctrl Pts',(77.9959713625728,9.45927254399561,132.770787846019));
#61567=CARTESIAN_POINT('Ctrl Pts',(78.0142600200556,9.52804762526732,132.766918763172));
#61568=CARTESIAN_POINT('Ctrl Pts',(78.0325214283509,9.59672023509799,132.763055445066));
#61569=CARTESIAN_POINT('Ctrl Pts',(78.0543775063823,9.66455026482023,132.759192126959));
#61570=CARTESIAN_POINT('Ctrl Pts',(78.0797297357173,9.73113587971839,132.755328808853));
#61571=CARTESIAN_POINT('Ctrl Pts',(78.105052226897,9.79764338971588,132.751470022417));
#61572=CARTESIAN_POINT('Ctrl Pts',(78.1338625514211,9.86290893255779,132.747611235981));
#61573=CARTESIAN_POINT('Ctrl Pts',(78.1660123424271,9.92654564613423,132.743752449546));
#61574=CARTESIAN_POINT('Ctrl Pts',(78.1981418814222,9.9901422732474,132.739896093862));
#61575=CARTESIAN_POINT('Ctrl Pts',(78.2336064948162,10.0521116741827,132.736039738179));
#61576=CARTESIAN_POINT('Ctrl Pts',(78.2722102319607,10.1120881619543,132.732183382496));
#61577=CARTESIAN_POINT('Ctrl Pts',(78.3108025651747,10.1720469320708,132.728328166018));
#61578=CARTESIAN_POINT('Ctrl Pts',(78.3525319183583,10.2300135495482,132.724472949541));
#61579=CARTESIAN_POINT('Ctrl Pts',(78.3971579299853,10.2856495872091,132.720617733064));
#61580=CARTESIAN_POINT('Ctrl Pts',(78.4417856863558,10.3412878000726,132.716762365859));
#61581=CARTESIAN_POINT('Ctrl Pts',(78.4893100203429,10.3945948746504,132.712906998655));
#61582=CARTESIAN_POINT('Ctrl Pts',(78.5394501256207,10.4452652444969,132.70905163145));
#61583=CARTESIAN_POINT('Ctrl Pts',(78.5896427139162,10.4959886524034,132.705192228727));
#61584=CARTESIAN_POINT('Ctrl Pts',(78.6424561967735,10.5440695001681,132.701332826004));
#61585=CARTESIAN_POINT('Ctrl Pts',(78.6975733581752,10.5892395682102,132.697473423282));
#61586=CARTESIAN_POINT('Ctrl Pts',(78.7527217273466,10.6344352118997,132.693611835335));
#61587=CARTESIAN_POINT('Ctrl Pts',(78.8101759802012,10.6767165069286,132.689750247388));
#61588=CARTESIAN_POINT('Ctrl Pts',(78.8695885307946,10.7158576493371,132.685888659441));
#61589=CARTESIAN_POINT('Ctrl Pts',(78.9291050257748,10.7550672705773,132.682020315507));
#61590=CARTESIAN_POINT('Ctrl Pts',(78.990586239659,10.7911255248144,132.678151971574));
#61591=CARTESIAN_POINT('Ctrl Pts',(79.0536591538181,10.8238521226645,132.674283627641));
#61592=CARTESIAN_POINT('Ctrl Pts',(79.0911100351655,10.8432842346785,132.671986716334));
#61593=CARTESIAN_POINT('Ctrl Pts',(79.1291216747157,10.8615426311578,132.669689805028));
#61594=CARTESIAN_POINT('Ctrl Pts',(79.1676130426291,10.8785977525002,132.667392893721));
#61595=CARTESIAN_POINT('Ctrl Pts',(79.2324506752055,10.9073266273387,132.663523810874));
#61596=CARTESIAN_POINT('Ctrl Pts',(79.2989043618557,10.9327511364559,132.659654728027));
#61597=CARTESIAN_POINT('Ctrl Pts',(79.3666039904561,10.954688480959,132.65578564518));
#61598=CARTESIAN_POINT('Ctrl Pts',(79.4342027499863,10.9765931399129,132.651922327074));
#61599=CARTESIAN_POINT('Ctrl Pts',(79.5030433082192,10.995020799049,132.648059008968));
#61600=CARTESIAN_POINT('Ctrl Pts',(79.5727346360594,11.0098362797195,132.644195690861));
#61601=CARTESIAN_POINT('Ctrl Pts',(79.642344215999,11.0246343818369,132.640336904425));
#61602=CARTESIAN_POINT('Ctrl Pts',(79.7128021104158,11.0358286212486,132.63647811799));
#61603=CARTESIAN_POINT('Ctrl Pts',(79.7837028323885,11.0433338194684,132.632619331554));
#61604=CARTESIAN_POINT('Ctrl Pts',(79.8545588921052,11.0508342899636,132.628762975871));
#61605=CARTESIAN_POINT('Ctrl Pts',(79.9258567440054,11.0546502786843,132.624906620187));
#61606=CARTESIAN_POINT('Ctrl Pts',(79.9971828825806,11.0547480688273,132.621050264504));
#61607=CARTESIAN_POINT('Ctrl Pts',(80.0684879507002,11.0548458300821,132.617195048027));
#61608=CARTESIAN_POINT('Ctrl Pts',(80.1398208033875,11.0512275727087,132.61333983155));
#61609=CARTESIAN_POINT('Ctrl Pts',(80.2107667494145,11.0439116761351,132.609484615072));
#61610=CARTESIAN_POINT('Ctrl Pts',(80.2817154692159,11.0365954935317,132.605629247868));
#61611=CARTESIAN_POINT('Ctrl Pts',(80.3522767693298,11.0255814367308,132.601773880663));
#61612=CARTESIAN_POINT('Ctrl Pts',(80.4220416294529,11.0109396871882,132.597918513458));
#61613=CARTESIAN_POINT('Ctrl Pts',(80.4918795143607,10.9962826117265,132.594059110736));
#61614=CARTESIAN_POINT('Ctrl Pts',(80.560918818715,10.9779903634344,132.590199708013));
#61615=CARTESIAN_POINT('Ctrl Pts',(80.628762150649,10.9561839689588,132.58634030529));
#61616=CARTESIAN_POINT('Ctrl Pts',(80.6966438960105,10.9343652275313,132.582478717343));
#61617=CARTESIAN_POINT('Ctrl Pts',(80.7633278665926,10.9090285515885,132.578617129396));
#61618=CARTESIAN_POINT('Ctrl Pts',(80.8284358332439,10.8803434879557,132.574755541449));
#61619=CARTESIAN_POINT('Ctrl Pts',(80.8936577086166,10.8516082387759,132.570887197516));
#61620=CARTESIAN_POINT('Ctrl Pts',(80.9572976411981,10.8195131248122,132.567018853582));
#61621=CARTESIAN_POINT('Ctrl Pts',(81.0190018459501,10.7842737459399,132.563150509649));
#61622=CARTESIAN_POINT('Ctrl Pts',(81.0556400270381,10.7633496168672,132.560853598343));
#61623=CARTESIAN_POINT('Ctrl Pts',(81.0915962750952,10.7413177760724,132.558556687036));
#61624=CARTESIAN_POINT('Ctrl Pts',(81.1268018071315,10.7182302668575,132.55625977573));
#61625=CARTESIAN_POINT('Ctrl Pts',(81.1695802906112,10.690176476035,132.553468783045));
#61626=CARTESIAN_POINT('Ctrl Pts',(81.2113708104195,10.660484561751,132.55067779036));
#61627=CARTESIAN_POINT('Ctrl Pts',(81.252039109102,10.6292316077768,132.547886797676));
#61628=CARTESIAN_POINT('',(77.9452507493435,8.99824517046231,132.854074719498));
#61629=CARTESIAN_POINT('Ctrl Pts',(77.945250749343,8.99824517113454,132.854074719462));
#61630=CARTESIAN_POINT('Ctrl Pts',(77.9451902335234,9.0691038384727,132.850240467841));
#61631=CARTESIAN_POINT('Ctrl Pts',(77.9487993838056,9.14002687651476,132.846406216221));
#61632=CARTESIAN_POINT('Ctrl Pts',(77.9560714877068,9.21060341672155,132.8425719646));
#61633=CARTESIAN_POINT('Ctrl Pts',(77.9633409049725,9.28115388284672,132.838739129521));
#61634=CARTESIAN_POINT('Ctrl Pts',(77.9742705404255,9.35135761627535,132.834906294442));
#61635=CARTESIAN_POINT('Ctrl Pts',(77.988801718831,9.42080760012499,132.831073459363));
#61636=CARTESIAN_POINT('Ctrl Pts',(78.0033325301936,9.4902558297379,132.827240721097));
#61637=CARTESIAN_POINT('Ctrl Pts',(78.0214646012843,9.5589498665225,132.823407982832));
#61638=CARTESIAN_POINT('Ctrl Pts',(78.0430882613477,9.62649342344899,132.819575244566));
#61639=CARTESIAN_POINT('Ctrl Pts',(78.0647340638349,9.69410614433997,132.815738581613));
#61640=CARTESIAN_POINT('Ctrl Pts',(78.0898784440369,9.76056556353255,132.811901918659));
#61641=CARTESIAN_POINT('Ctrl Pts',(78.1183622815559,9.82549201027531,132.808065255706));
#61642=CARTESIAN_POINT('Ctrl Pts',(78.1468610721474,9.89045254125519,132.804226578632));
#61643=CARTESIAN_POINT('Ctrl Pts',(78.1787025884923,9.95387805807839,132.800387901557));
#61644=CARTESIAN_POINT('Ctrl Pts',(78.2136813665789,10.0154128728713,132.796549224483));
#61645=CARTESIAN_POINT('Ctrl Pts',(78.2487243400171,10.0770606203989,132.792703502416));
#61646=CARTESIAN_POINT('Ctrl Pts',(78.2869158076442,10.1368103218298,132.788857780349));
#61647=CARTESIAN_POINT('Ctrl Pts',(78.3280069113271,10.1943352435268,132.785012058282));
#61648=CARTESIAN_POINT('Ctrl Pts',(78.3588674553705,10.2375380348978,132.782123815704));
#61649=CARTESIAN_POINT('Ctrl Pts',(78.3913626087631,10.2794865660436,132.779235573126));
#61650=CARTESIAN_POINT('Ctrl Pts',(78.4253729722414,10.3200557889544,132.776347330549));
#61651=CARTESIAN_POINT('Ctrl Pts',(78.4709331737856,10.3744022229021,132.772478247702));
#61652=CARTESIAN_POINT('Ctrl Pts',(78.5193994699275,10.4264936451473,132.768609164855));
#61653=CARTESIAN_POINT('Ctrl Pts',(78.5705200716174,10.4760029460849,132.764740082008));
#61654=CARTESIAN_POINT('Ctrl Pts',(78.6215645061603,10.5254384806333,132.760876763902));
#61655=CARTESIAN_POINT('Ctrl Pts',(78.6752550500033,10.5722991953193,132.757013445795));
#61656=CARTESIAN_POINT('Ctrl Pts',(78.7313001635045,10.6162915230169,132.753150127689));
#61657=CARTESIAN_POINT('Ctrl Pts',(78.7872795361092,10.6602322477311,132.749291341253));
#61658=CARTESIAN_POINT('Ctrl Pts',(78.8456076120167,10.7013109702352,132.745432554817));
#61659=CARTESIAN_POINT('Ctrl Pts',(78.9059578520073,10.73927264709,132.741573768381));
#61660=CARTESIAN_POINT('Ctrl Pts',(78.966270075772,10.777210410872,132.737717412698));
#61661=CARTESIAN_POINT('Ctrl Pts',(79.0286015261645,10.8120347665365,132.733861057015));
#61662=CARTESIAN_POINT('Ctrl Pts',(79.0925958019739,10.8435333422275,132.730004701331));
#61663=CARTESIAN_POINT('Ctrl Pts',(79.1565711732334,10.8750226129239,132.726149484854));
#61664=CARTESIAN_POINT('Ctrl Pts',(79.2222079591012,10.9031878397086,132.722294268377));
#61665=CARTESIAN_POINT('Ctrl Pts',(79.2891257515502,10.9278629010879,132.7184390519));
#61666=CARTESIAN_POINT('Ctrl Pts',(79.3560461602849,10.9525389271883,132.714583684695));
#61667=CARTESIAN_POINT('Ctrl Pts',(79.4242472184884,10.9737243509719,132.710728317491));
#61668=CARTESIAN_POINT('Ctrl Pts',(79.4933307968446,10.9913020567141,132.706872950286));
#61669=CARTESIAN_POINT('Ctrl Pts',(79.5624866868691,11.0088981615211,132.703013547563));
#61670=CARTESIAN_POINT('Ctrl Pts',(79.6325264693269,11.0228788899197,132.69915414484));
#61671=CARTESIAN_POINT('Ctrl Pts',(79.7030400637026,11.0331778964799,132.695294742118));
#61672=CARTESIAN_POINT('Ctrl Pts',(79.7735935834293,11.0434827344185,132.691433154171));
#61673=CARTESIAN_POINT('Ctrl Pts',(79.8446209652123,11.0501016555882,132.687571566224));
#61674=CARTESIAN_POINT('Ctrl Pts',(79.9157079655849,11.0530203153973,132.683709978277));
#61675=CARTESIAN_POINT('Ctrl Pts',(79.9869193352128,11.0559440815064,132.679841634343));
#61676=CARTESIAN_POINT('Ctrl Pts',(80.0581900457709,11.0551546666323,132.67597329041));
#61677=CARTESIAN_POINT('Ctrl Pts',(80.1291075190145,11.0506898378433,132.672104946476));
#61678=CARTESIAN_POINT('Ctrl Pts',(80.1712162737992,11.048038750995,132.66980803517));
#61679=CARTESIAN_POINT('Ctrl Pts',(80.2132005988816,11.0440928378389,132.667511123864));
#61680=CARTESIAN_POINT('Ctrl Pts',(80.2549758212296,11.0388685325661,132.665214212557));
#61681=CARTESIAN_POINT('Ctrl Pts',(80.3253420978994,11.030068701241,132.661345290086));
#61682=CARTESIAN_POINT('Ctrl Pts',(80.3953900995657,11.0176045939,132.657476367615));
#61683=CARTESIAN_POINT('Ctrl Pts',(80.4647084963187,11.0015103237179,132.653607445144));
#61684=CARTESIAN_POINT('Ctrl Pts',(80.5356580112831,10.9850373422783,132.649647483783));
#61685=CARTESIAN_POINT('Ctrl Pts',(80.6058426316095,10.9647611560803,132.645687522422));
#61686=CARTESIAN_POINT('Ctrl Pts',(80.6748265776872,10.9407747557475,132.641727561061));
#61687=CARTESIAN_POINT('Ctrl Pts',(80.7420453187134,10.9174021346699,132.637868929708));
#61688=CARTESIAN_POINT('Ctrl Pts',(80.8081236063342,10.890507073603,132.634010298355));
#61689=CARTESIAN_POINT('Ctrl Pts',(80.8726704982589,10.8602268044431,132.630151667001));
#61690=CARTESIAN_POINT('Ctrl Pts',(80.9397599511857,10.8287537678361,132.626141040636));
#61691=CARTESIAN_POINT('Ctrl Pts',(81.0051943248821,10.793623421345,132.622130414271));
#61692=CARTESIAN_POINT('Ctrl Pts',(81.0685566242506,10.7550453849602,132.618119787906));
#61693=CARTESIAN_POINT('Ctrl Pts',(81.1319189236191,10.7164673485754,132.614109161541));
#61694=CARTESIAN_POINT('Ctrl Pts',(81.1932086330005,10.6744419121526,132.610098535176));
#61695=CARTESIAN_POINT('Ctrl Pts',(81.252039109102,10.6292316077768,132.606087908811));
#61696=CARTESIAN_POINT('Ctrl Pts',(81.252039109102,10.6292316077768,133.306011340678));
#61697=CARTESIAN_POINT('Ctrl Pts',(81.3084857783771,10.5858532218103,133.30215326156));
#61698=CARTESIAN_POINT('Ctrl Pts',(81.362733635988,10.539493193464,133.298295182442));
#61699=CARTESIAN_POINT('Ctrl Pts',(81.4144559732381,10.4904066097113,133.294437103324));
#61700=CARTESIAN_POINT('Ctrl Pts',(81.4661499193566,10.4413469702873,133.29058114196));
#61701=CARTESIAN_POINT('Ctrl Pts',(81.5153207440633,10.3895640788887,133.286725180597));
#61702=CARTESIAN_POINT('Ctrl Pts',(81.5616759642891,10.3353522924913,133.282869219233));
#61703=CARTESIAN_POINT('Ctrl Pts',(81.6080212459527,10.2811521291042,133.279014084588));
#61704=CARTESIAN_POINT('Ctrl Pts',(81.651551806428,10.2245244740596,133.275158949943));
#61705=CARTESIAN_POINT('Ctrl Pts',(81.6920142683062,10.1657981293296,133.271303815298));
#61706=CARTESIAN_POINT('Ctrl Pts',(81.7324815899134,10.1070647312935,133.267448217634));
#61707=CARTESIAN_POINT('Ctrl Pts',(81.7698798079035,10.04623254463,133.263592619969));
#61708=CARTESIAN_POINT('Ctrl Pts',(81.8039988342832,9.98365937620945,133.259737022305));
#61709=CARTESIAN_POINT('Ctrl Pts',(81.838155271222,9.92101759805821,133.255877197085));
#61710=CARTESIAN_POINT('Ctrl Pts',(81.8690251097147,9.85663145659424,133.252017371865));
#61711=CARTESIAN_POINT('Ctrl Pts',(81.896444661964,9.79088254918685,133.248157546646));
#61712=CARTESIAN_POINT('Ctrl Pts',(81.9238817311998,9.72509163807652,133.244295255576));
#61713=CARTESIAN_POINT('Ctrl Pts',(81.9478639650014,9.65793668596684,133.240432964506));
#61714=CARTESIAN_POINT('Ctrl Pts',(81.9682771234689,9.58981584221602,133.236570673436));
#61715=CARTESIAN_POINT('Ctrl Pts',(81.9887245103614,9.521580774633,133.232701906145));
#61716=CARTESIAN_POINT('Ctrl Pts',(82.0055907665823,9.45237705514605,133.228833138853));
#61717=CARTESIAN_POINT('Ctrl Pts',(82.018812624733,9.38261357623391,133.224964371562));
#61718=CARTESIAN_POINT('Ctrl Pts',(82.0234657513813,9.35806193613155,133.223602848546));
#61719=CARTESIAN_POINT('Ctrl Pts',(82.0276679804636,9.33344101299941,133.222241325531));
#61720=CARTESIAN_POINT('Ctrl Pts',(82.0314180869268,9.30876871377533,133.220879802515));
#61721=CARTESIAN_POINT('Ctrl Pts',(82.0420748826077,9.23865666378814,133.217010719668));
#61722=CARTESIAN_POINT('Ctrl Pts',(82.0491185350753,9.16785493292545,133.213141636821));
#61723=CARTESIAN_POINT('Ctrl Pts',(82.0524700687833,9.09676868940202,133.209272553974));
#61724=CARTESIAN_POINT('Ctrl Pts',(82.0558166088733,9.02578836083628,133.205409235868));
#61725=CARTESIAN_POINT('Ctrl Pts',(82.0554819269895,8.95452484234985,133.201545917761));
#61726=CARTESIAN_POINT('Ctrl Pts',(82.0514384934808,8.88339095247258,133.197682599655));
#61727=CARTESIAN_POINT('Ctrl Pts',(82.0473998029181,8.81234050262067,133.193823813219));
#61728=CARTESIAN_POINT('Ctrl Pts',(82.0396610294617,8.74141986199301,133.189965026783));
#61729=CARTESIAN_POINT('Ctrl Pts',(82.0282466859118,8.67104264168789,133.186106240347));
#61730=CARTESIAN_POINT('Ctrl Pts',(82.0168395325614,8.600709753871,133.182249884664));
#61731=CARTESIAN_POINT('Ctrl Pts',(82.0017614803032,8.53092008561283,133.178393528981));
#61732=CARTESIAN_POINT('Ctrl Pts',(81.9830888001473,8.46208144368299,133.174537173298));
#61733=CARTESIAN_POINT('Ctrl Pts',(81.9644216360882,8.3932631373773,133.17068195682));
#61734=CARTESIAN_POINT('Ctrl Pts',(81.9421620793813,8.3253957682363,133.166826740343));
#61735=CARTESIAN_POINT('Ctrl Pts',(81.9164369736019,8.25887457963469,133.162971523866));
#61736=CARTESIAN_POINT('Ctrl Pts',(81.8907108620478,8.19235079025377,133.159116156661));
#61737=CARTESIAN_POINT('Ctrl Pts',(81.8615191096896,8.12717373819403,133.155260789457));
#61738=CARTESIAN_POINT('Ctrl Pts',(81.8290370447406,8.06371956579946,133.151405422252));
#61739=CARTESIAN_POINT('Ctrl Pts',(81.7965209799269,8.00019897418937,133.147546019529));
#61740=CARTESIAN_POINT('Ctrl Pts',(81.7607079492153,7.9384052955115,133.143686616806));
#61741=CARTESIAN_POINT('Ctrl Pts',(81.72181927482,7.87869007524317,133.139827214084));
#61742=CARTESIAN_POINT('Ctrl Pts',(81.6829085813518,7.81894104374798,133.135965626137));
#61743=CARTESIAN_POINT('Ctrl Pts',(81.6409190635816,7.76127320628335,133.13210403819));
#61744=CARTESIAN_POINT('Ctrl Pts',(81.5961138122485,7.70600685440395,133.128242450243));
#61745=CARTESIAN_POINT('Ctrl Pts',(81.5512301725223,7.65064381206106,133.124374106309));
#61746=CARTESIAN_POINT('Ctrl Pts',(81.5035212891501,7.59769100470694,133.120505762376));
#61747=CARTESIAN_POINT('Ctrl Pts',(81.4532882515802,7.54743302380963,133.116637418442));
#61748=CARTESIAN_POINT('Ctrl Pts',(81.4234613194524,7.51759128105174,133.114340507136));
#61749=CARTESIAN_POINT('Ctrl Pts',(81.3927451338705,7.48869889924349,133.11204359583));
#61750=CARTESIAN_POINT('Ctrl Pts',(81.3612080022365,7.46080854434957,133.109746684523));
#61751=CARTESIAN_POINT('Ctrl Pts',(81.3080845861496,7.41382802167435,133.105877601676));
#61752=CARTESIAN_POINT('Ctrl Pts',(81.2524220485732,7.36950895079296,133.102008518829));
#61753=CARTESIAN_POINT('Ctrl Pts',(81.1945179499444,7.32813743694031,133.098139435982));
#61754=CARTESIAN_POINT('Ctrl Pts',(81.1367001255347,7.28682756457992,133.094276117876));
#61755=CARTESIAN_POINT('Ctrl Pts',(81.0766477615526,7.24845681192626,133.09041279977));
#61756=CARTESIAN_POINT('Ctrl Pts',(81.0146927489589,7.21327221219623,133.086549481663));
#61757=CARTESIAN_POINT('Ctrl Pts',(80.9528104095714,7.17812888398821,133.082690695227));
#61758=CARTESIAN_POINT('Ctrl Pts',(80.8890302750623,7.14616452377802,133.078831908792));
#61759=CARTESIAN_POINT('Ctrl Pts',(80.8237131290571,7.1175828720714,133.074973122356));
#61760=CARTESIAN_POINT('Ctrl Pts',(80.7584371280644,7.08901922470956,133.071116766673));
#61761=CARTESIAN_POINT('Ctrl Pts',(80.6916264804664,7.0638342525433,133.067260410989));
#61762=CARTESIAN_POINT('Ctrl Pts',(80.6236651661146,7.04218506414032,133.063404055306));
#61763=CARTESIAN_POINT('Ctrl Pts',(80.5557239282157,7.02054227112442,133.059548838829));
#61764=CARTESIAN_POINT('Ctrl Pts',(80.4866331610091,7.0024333356039,133.055693622352));
#61765=CARTESIAN_POINT('Ctrl Pts',(80.4167937189867,6.98796606432365,133.051838405874));
#61766=CARTESIAN_POINT('Ctrl Pts',(80.3469515464508,6.97349822741634,133.04798303867));
#61767=CARTESIAN_POINT('Ctrl Pts',(80.2763611171164,6.96267243380358,133.044127671465));
#61768=CARTESIAN_POINT('Ctrl Pts',(80.2054335351811,6.95554539665881,133.040272304261));
#61769=CARTESIAN_POINT('Ctrl Pts',(80.1344317114086,6.94841089944959,133.036412901538));
#61770=CARTESIAN_POINT('Ctrl Pts',(80.0630925148932,6.94498293593645,133.032553498815));
#61771=CARTESIAN_POINT('Ctrl Pts',(79.9918313314325,6.94526623735486,133.028694096092));
#61772=CARTESIAN_POINT('Ctrl Pts',(79.92052979933,6.94554969918076,133.024832508145));
#61773=CARTESIAN_POINT('Ctrl Pts',(79.849306853463,6.94954858182793,133.020970920198));
#61774=CARTESIAN_POINT('Ctrl Pts',(79.7785742766004,6.95721557389994,133.017109332251));
#61775=CARTESIAN_POINT('Ctrl Pts',(79.7077179505592,6.96489597964939,133.013240988318));
#61776=CARTESIAN_POINT('Ctrl Pts',(79.6373541861038,6.97625723006333,133.009372644385));
#61777=CARTESIAN_POINT('Ctrl Pts',(79.5678853829316,6.99120072674848,133.005504300451));
#61778=CARTESIAN_POINT('Ctrl Pts',(79.526636806746,7.00007374504374,133.003207389145));
#61779=CARTESIAN_POINT('Ctrl Pts',(79.4857035065237,7.01020876927607,133.000910477838));
#61780=CARTESIAN_POINT('Ctrl Pts',(79.4451667772744,7.02157697712044,132.998613566532));
#61781=CARTESIAN_POINT('Ctrl Pts',(79.3768837907397,7.04072640524487,132.994744483685));
#61782=CARTESIAN_POINT('Ctrl Pts',(79.3094596083654,7.06345255239703,132.990875400838));
#61783=CARTESIAN_POINT('Ctrl Pts',(79.243295987548,7.08966060606,132.987006317991));
#61784=CARTESIAN_POINT('Ctrl Pts',(79.177230947226,7.11582961103004,132.983142999885));
#61785=CARTESIAN_POINT('Ctrl Pts',(79.1124231883001,7.145470047296,132.979279681778));
#61786=CARTESIAN_POINT('Ctrl Pts',(79.049260262673,7.17843706823856,132.975416363672));
#61787=CARTESIAN_POINT('Ctrl Pts',(78.9861714271333,7.21136541887825,132.971557577236));
#61788=CARTESIAN_POINT('Ctrl Pts',(78.9247240210359,7.24761237965476,132.9676987908));
#61789=CARTESIAN_POINT('Ctrl Pts',(78.8652848954572,7.28698534915129,132.963840004364));
#61790=CARTESIAN_POINT('Ctrl Pts',(78.805883212169,7.32633351656419,132.959983648681));
#61791=CARTESIAN_POINT('Ctrl Pts',(78.7484877035544,7.36880351828716,132.956127292998));
#61792=CARTESIAN_POINT('Ctrl Pts',(78.6934386248325,7.41415797274114,132.952270937315));
#61793=CARTESIAN_POINT('Ctrl Pts',(78.6384058081597,7.45949902903517,132.948415720837));
#61794=CARTESIAN_POINT('Ctrl Pts',(78.5857184199867,7.50772253768425,132.94456050436));
#61795=CARTESIAN_POINT('Ctrl Pts',(78.5356844479136,7.55855019982731,132.940705287883));
#61796=CARTESIAN_POINT('Ctrl Pts',(78.4856485196619,7.60937984917983,132.936849920678));
#61797=CARTESIAN_POINT('Ctrl Pts',(78.4382665526904,7.66281350642767,132.932994553474));
#61798=CARTESIAN_POINT('Ctrl Pts',(78.3938091684385,7.71853654944516,132.929139186269));
#61799=CARTESIAN_POINT('Ctrl Pts',(78.3493052494283,7.77431791929373,132.925279783546));
#61800=CARTESIAN_POINT('Ctrl Pts',(78.3077323276436,7.83239307807583,132.921420380823));
#61801=CARTESIAN_POINT('Ctrl Pts',(78.2693196750335,7.89241561257217,132.917560978101));
#61802=CARTESIAN_POINT('Ctrl Pts',(78.2308852728778,7.95247213229911,132.913699390154));
#61803=CARTESIAN_POINT('Ctrl Pts',(78.1956149422791,8.01447780026488,132.909837802207));
#61804=CARTESIAN_POINT('Ctrl Pts',(78.1636922782386,8.07806100337411,132.90597621426));
#61805=CARTESIAN_POINT('Ctrl Pts',(78.1317137643532,8.14175544757624,132.902107870326));
#61806=CARTESIAN_POINT('Ctrl Pts',(78.1030948055349,8.20703249220501,132.898239526393));
#61807=CARTESIAN_POINT('Ctrl Pts',(78.0779708196889,8.27350059013615,132.894371182459));
#61808=CARTESIAN_POINT('Ctrl Pts',(78.063052919899,8.31296743390215,132.892074271153));
#61809=CARTESIAN_POINT('Ctrl Pts',(78.049366272519,8.35285389108696,132.889777359846));
#61810=CARTESIAN_POINT('Ctrl Pts',(78.0369307557736,8.39307603040213,132.88748044854));
#61811=CARTESIAN_POINT('Ctrl Pts',(78.0114354604796,8.47553945674731,132.88277132119));
#61812=CARTESIAN_POINT('Ctrl Pts',(77.9911203973394,8.55967521235693,132.878062193839));
#61813=CARTESIAN_POINT('Ctrl Pts',(77.9761678835397,8.64489279522422,132.873353066489));
#61814=CARTESIAN_POINT('Ctrl Pts',(77.9614177985701,8.7289566927755,132.868707691839));
#61815=CARTESIAN_POINT('Ctrl Pts',(77.9518860944981,8.81407332549794,132.86406231719));
#61816=CARTESIAN_POINT('Ctrl Pts',(77.9477016670827,8.89965501903518,132.859416942541));
#61817=CARTESIAN_POINT('Ctrl Pts',(77.946097623904,8.93246159401252,132.857636201526));
#61818=CARTESIAN_POINT('Ctrl Pts',(77.945278854709,8.96533628820413,132.855855460512));
#61819=CARTESIAN_POINT('Ctrl Pts',(77.9452507493435,8.99824517046232,132.854074719498));
#61820=CARTESIAN_POINT('Origin',(80.,9.,141.545925280538));
#61821=CARTESIAN_POINT('',(81.252039109102,10.6292316077768,134.006113615495));
#61822=CARTESIAN_POINT('',(81.252039109102,10.6292316077769,133.947919788944));
#61823=CARTESIAN_POINT('',(81.252039109102,10.6292316077768,141.545925280538));
#61824=CARTESIAN_POINT('',(77.94525006034,9.00049796301154,133.495925280488));
#61825=CARTESIAN_POINT('Ctrl Pts',(81.252039109102,10.6292316077769,133.947919788944));
#61826=CARTESIAN_POINT('Ctrl Pts',(81.3085900087084,10.5857731224245,133.944064641676));
#61827=CARTESIAN_POINT('Ctrl Pts',(81.3628803139282,10.539363224955,133.940209494408));
#61828=CARTESIAN_POINT('Ctrl Pts',(81.414596167302,10.4902735473578,133.936354347139));
#61829=CARTESIAN_POINT('Ctrl Pts',(81.466575160351,10.4409340925459,133.93247958418));
#61830=CARTESIAN_POINT('Ctrl Pts',(81.5159530592672,10.3888878396507,133.928604821221));
#61831=CARTESIAN_POINT('Ctrl Pts',(81.5624487554031,10.3344479942055,133.924730058262));
#61832=CARTESIAN_POINT('Ctrl Pts',(81.6087738167075,10.2802079378727,133.920869515318));
#61833=CARTESIAN_POINT('Ctrl Pts',(81.6522375312,10.2235922431463,133.917008972375));
#61834=CARTESIAN_POINT('Ctrl Pts',(81.6926037665952,10.1649420808812,133.913148429431));
#61835=CARTESIAN_POINT('Ctrl Pts',(81.7331930309163,10.1059678685141,133.909266556464));
#61836=CARTESIAN_POINT('Ctrl Pts',(81.7706502268193,10.0449370632542,133.905384683497));
#61837=CARTESIAN_POINT('Ctrl Pts',(81.8047817870842,9.9822221049789,133.90150281053));
#61838=CARTESIAN_POINT('Ctrl Pts',(81.8389133473491,9.91950714670365,133.897620937563));
#61839=CARTESIAN_POINT('Ctrl Pts',(81.8697191169326,9.85510850704433,133.893739064596));
#61840=CARTESIAN_POINT('Ctrl Pts',(81.897055014379,9.78941740221469,133.889857191629));
#61841=CARTESIAN_POINT('Ctrl Pts',(81.9243008446298,9.72394273855361,133.885988108782));
#61842=CARTESIAN_POINT('Ctrl Pts',(81.9482063861373,9.65692764160921,133.882119025935));
#61843=CARTESIAN_POINT('Ctrl Pts',(81.9685973105308,9.58874628786168,133.878249943088));
#61844=CARTESIAN_POINT('Ctrl Pts',(81.9889578534638,9.52066652093102,133.874386624982));
#61845=CARTESIAN_POINT('Ctrl Pts',(82.0058140357402,9.45142440803659,133.870523306875));
#61846=CARTESIAN_POINT('Ctrl Pts',(82.0190396129381,9.3814139534503,133.866659988769));
#61847=CARTESIAN_POINT('Ctrl Pts',(82.0322496765392,9.31148562110013,133.862801202333));
#61848=CARTESIAN_POINT('Ctrl Pts',(82.0418375045425,9.24079121229842,133.858942415897));
#61849=CARTESIAN_POINT('Ctrl Pts',(82.0477271687752,9.16973804747254,133.855083629461));
#61850=CARTESIAN_POINT('Ctrl Pts',(82.0536131229513,9.09872964093042,133.851227273778));
#61851=CARTESIAN_POINT('Ctrl Pts',(82.0558054951567,9.0273634097031,133.847370918095));
#61852=CARTESIAN_POINT('Ctrl Pts',(82.0542799880628,8.95605351954021,133.843514562412));
#61853=CARTESIAN_POINT('Ctrl Pts',(82.0527549316189,8.88476469503292,133.839659345934));
#61854=CARTESIAN_POINT('Ctrl Pts',(82.047514186688,8.8135326639551,133.835804129457));
#61855=CARTESIAN_POINT('Ctrl Pts',(82.0385855656644,8.74277159183953,133.83194891298));
#61856=CARTESIAN_POINT('Ctrl Pts',(82.0296565955584,8.67200775317777,133.828093545775));
#61857=CARTESIAN_POINT('Ctrl Pts',(82.0170395260989,8.60171539172073,133.824238178571));
#61858=CARTESIAN_POINT('Ctrl Pts',(82.0008138292302,8.53230182461196,133.820382811366));
#61859=CARTESIAN_POINT('Ctrl Pts',(81.9845711484813,8.46281560042647,133.816523408643));
#61860=CARTESIAN_POINT('Ctrl Pts',(81.9647124108874,8.3942104808327,133.81266400592));
#61861=CARTESIAN_POINT('Ctrl Pts',(81.9413676557692,8.32688100039217,133.808804603198));
#61862=CARTESIAN_POINT('Ctrl Pts',(81.9180096826674,8.25951339747097,133.804943015251));
#61863=CARTESIAN_POINT('Ctrl Pts',(81.8911619457095,8.19342332181168,133.801081427304));
#61864=CARTESIAN_POINT('Ctrl Pts',(81.8610025557139,8.12898504598001,133.797219839357));
#61865=CARTESIAN_POINT('Ctrl Pts',(81.8307904007844,8.06443403307509,133.793351495423));
#61866=CARTESIAN_POINT('Ctrl Pts',(81.7972552538553,8.00154101852065,133.78948315149));
#61867=CARTESIAN_POINT('Ctrl Pts',(81.7606207105567,7.9406547890047,133.785614807556));
#61868=CARTESIAN_POINT('Ctrl Pts',(81.7388681729964,7.90450229807125,133.78331789625));
#61869=CARTESIAN_POINT('Ctrl Pts',(81.7160237303533,7.8690567733382,133.781020984944));
#61870=CARTESIAN_POINT('Ctrl Pts',(81.6921409778437,7.83438579555573,133.778724073637));
#61871=CARTESIAN_POINT('Ctrl Pts',(81.6519111492852,7.77598350329134,133.77485499079));
#61872=CARTESIAN_POINT('Ctrl Pts',(81.6085754448932,7.71955199739188,133.770985907943));
#61873=CARTESIAN_POINT('Ctrl Pts',(81.5623536704282,7.66544068284709,133.767116825096));
#61874=CARTESIAN_POINT('Ctrl Pts',(81.516200764102,7.61140999146239,133.76325350699));
#61875=CARTESIAN_POINT('Ctrl Pts',(81.4671706362288,7.55969299580559,133.759390188884));
#61876=CARTESIAN_POINT('Ctrl Pts',(81.4155258303404,7.51060945815445,133.755526870777));
#61877=CARTESIAN_POINT('Ctrl Pts',(81.3639416037894,7.46158349547399,133.751668084341));
#61878=CARTESIAN_POINT('Ctrl Pts',(81.3097491417681,7.41518518794331,133.747809297906));
#61879=CARTESIAN_POINT('Ctrl Pts',(81.253249465694,7.37169924791589,133.74395051147));
#61880=CARTESIAN_POINT('Ctrl Pts',(81.1967853802729,7.328240700842,133.740094155787));
#61881=CARTESIAN_POINT('Ctrl Pts',(81.1380173483258,7.28769117708969,133.736237800103));
#61882=CARTESIAN_POINT('Ctrl Pts',(81.0772801458058,7.25029572500016,133.73238144442));
#61883=CARTESIAN_POINT('Ctrl Pts',(81.0165608856637,7.21291131990172,133.728526227943));
#61884=CARTESIAN_POINT('Ctrl Pts',(80.953874023249,7.17867939124625,133.724671011466));
#61885=CARTESIAN_POINT('Ctrl Pts',(80.8895825976207,7.14780120815545,133.720815794988));
#61886=CARTESIAN_POINT('Ctrl Pts',(80.8252886583898,7.11692181781997,133.716960427784));
#61887=CARTESIAN_POINT('Ctrl Pts',(80.7593904702457,7.08939664170252,133.713105060579));
#61888=CARTESIAN_POINT('Ctrl Pts',(80.6922733378124,7.06537983359678,133.709249693375));
#61889=CARTESIAN_POINT('Ctrl Pts',(80.6250859520435,7.04133788644204,133.705390290652));
#61890=CARTESIAN_POINT('Ctrl Pts',(80.5566775333176,7.02081180204424,133.701530887929));
#61891=CARTESIAN_POINT('Ctrl Pts',(80.4874500739385,7.00390631785045,133.697671485206));
#61892=CARTESIAN_POINT('Ctrl Pts',(80.418183417428,6.98699126163868,133.693809897259));
#61893=CARTESIAN_POINT('Ctrl Pts',(80.3480972745903,6.97370097712113,133.689948309312));
#61894=CARTESIAN_POINT('Ctrl Pts',(80.2776026879906,6.96408882558192,133.686086721365));
#61895=CARTESIAN_POINT('Ctrl Pts',(80.2069847685848,6.95445985723907,133.682218377432));
#61896=CARTESIAN_POINT('Ctrl Pts',(80.1359574629714,6.94852191006832,133.678350033499));
#61897=CARTESIAN_POINT('Ctrl Pts',(80.0649350722534,6.94627630902026,133.674481689565));
#61898=CARTESIAN_POINT('Ctrl Pts',(80.0227640204915,6.94494293574069,133.672184778259));
#61899=CARTESIAN_POINT('Ctrl Pts',(79.9805946865909,6.94491035259303,133.669887866952));
#61900=CARTESIAN_POINT('Ctrl Pts',(79.938512916366,6.94617018693218,133.667590955646));
#61901=CARTESIAN_POINT('Ctrl Pts',(79.8676273515256,6.94829234263664,133.663721872799));
#61902=CARTESIAN_POINT('Ctrl Pts',(79.7967129435705,6.9540927631037,133.659852789952));
#61903=CARTESIAN_POINT('Ctrl Pts',(79.7261824575087,6.96357629263357,133.655983707105));
#61904=CARTESIAN_POINT('Ctrl Pts',(79.6557570583536,6.97304569217743,133.652120388999));
#61905=CARTESIAN_POINT('Ctrl Pts',(79.5857149231673,6.98618724374451,133.648257070892));
#61906=CARTESIAN_POINT('Ctrl Pts',(79.5164670932613,7.00295380859611,133.644393752786));
#61907=CARTESIAN_POINT('Ctrl Pts',(79.4473004910331,7.01970070627358,133.64053496635));
#61908=CARTESIAN_POINT('Ctrl Pts',(79.3789268132236,7.04006405728557,133.636676179914));
#61909=CARTESIAN_POINT('Ctrl Pts',(79.3117485241913,7.0639453859596,133.632817393478));
#61910=CARTESIAN_POINT('Ctrl Pts',(79.2446125525552,7.08781167114769,133.628961037795));
#61911=CARTESIAN_POINT('Ctrl Pts',(79.1786709323809,7.11519137502217,133.625104682112));
#61912=CARTESIAN_POINT('Ctrl Pts',(79.1143111127741,7.14593615062896,133.621248326428));
#61913=CARTESIAN_POINT('Ctrl Pts',(79.0499703057024,7.17667184392122,133.617393109951));
#61914=CARTESIAN_POINT('Ctrl Pts',(78.9872108096165,7.21077042614907,133.613537893474));
#61915=CARTESIAN_POINT('Ctrl Pts',(78.9263986226043,7.24803606060112,133.609682676997));
#61916=CARTESIAN_POINT('Ctrl Pts',(78.8655840580174,7.28530315202802,133.605827309792));
#61917=CARTESIAN_POINT('Ctrl Pts',(78.8067173667056,7.32573728581333,133.601971942588));
#61918=CARTESIAN_POINT('Ctrl Pts',(78.7501370400154,7.36909836478144,133.598116575383));
#61919=CARTESIAN_POINT('Ctrl Pts',(78.6934974891518,7.41250483097526,133.59425717266));
#61920=CARTESIAN_POINT('Ctrl Pts',(78.6391494666409,7.45884406211309,133.590397769937));
#61921=CARTESIAN_POINT('Ctrl Pts',(78.5873989985908,7.50783513869356,133.586538367214));
#61922=CARTESIAN_POINT('Ctrl Pts',(78.5356192290193,7.55685395440631,133.582676779267));
#61923=CARTESIAN_POINT('Ctrl Pts',(78.4864402767907,7.6085272525214,133.578815191321));
#61924=CARTESIAN_POINT('Ctrl Pts',(78.440129913883,7.66253864469385,133.574953603374));
#61925=CARTESIAN_POINT('Ctrl Pts',(78.3937385293354,7.71664453173299,133.57108525944));
#61926=CARTESIAN_POINT('Ctrl Pts',(78.3502260507425,7.77309629491194,133.567216915507));
#61927=CARTESIAN_POINT('Ctrl Pts',(78.3098183000043,7.83154658479699,133.563348571573));
#61928=CARTESIAN_POINT('Ctrl Pts',(78.2858253404497,7.86625268487792,133.561051660267));
#61929=CARTESIAN_POINT('Ctrl Pts',(78.2629261494462,7.90166286469492,133.55875474896));
#61930=CARTESIAN_POINT('Ctrl Pts',(78.2411602539381,7.93770046118201,133.556457837654));
#61931=CARTESIAN_POINT('Ctrl Pts',(78.2033015192916,8.00038282599411,133.552462681304));
#61932=CARTESIAN_POINT('Ctrl Pts',(78.1687336620035,8.06519667391206,133.548467524953));
#61933=CARTESIAN_POINT('Ctrl Pts',(78.1376942678544,8.13177484342032,133.544472368603));
#61934=CARTESIAN_POINT('Ctrl Pts',(78.1062630365256,8.19919348687753,133.540426777931));
#61935=CARTESIAN_POINT('Ctrl Pts',(78.078450290962,8.26842096575299,133.536381187259));
#61936=CARTESIAN_POINT('Ctrl Pts',(78.0544569760338,8.33904621614173,133.532335596587));
#61937=CARTESIAN_POINT('Ctrl Pts',(78.0308540830866,8.40852224433065,133.528355836231));
#61938=CARTESIAN_POINT('Ctrl Pts',(78.0109474205576,8.47935046530343,133.524376075876));
#61939=CARTESIAN_POINT('Ctrl Pts',(77.9948811787214,8.55111685813086,133.520396315521));
#61940=CARTESIAN_POINT('Ctrl Pts',(77.9784163026598,8.62466391259056,133.51631780969));
#61941=CARTESIAN_POINT('Ctrl Pts',(77.9659851790174,8.69919589123697,133.51223930386));
#61942=CARTESIAN_POINT('Ctrl Pts',(77.9576890084772,8.77424930475158,133.508160798029));
#61943=CARTESIAN_POINT('Ctrl Pts',(77.9493928379371,8.84930271826618,133.504082292199));
#61944=CARTESIAN_POINT('Ctrl Pts',(77.9452317338588,8.92487707367048,133.500003786368));
#61945=CARTESIAN_POINT('Ctrl Pts',(77.9452500603398,9.00049796209039,133.495925280538));
#61946=CARTESIAN_POINT('Ctrl Pts',(77.94525006034,9.00049796301154,133.495925280488));
#61947=CARTESIAN_POINT('Ctrl Pts',(77.9452690078821,9.07868140246824,133.491708567086));
#61948=CARTESIAN_POINT('Ctrl Pts',(77.9497549266111,9.15674554238997,133.487491853684));
#61949=CARTESIAN_POINT('Ctrl Pts',(77.9586394355346,9.23418925753617,133.483275140282));
#61950=CARTESIAN_POINT('Ctrl Pts',(77.9673566235425,9.31017448426939,133.479137839749));
#61951=CARTESIAN_POINT('Ctrl Pts',(77.9803079746392,9.38556211302273,133.475000539217));
#61952=CARTESIAN_POINT('Ctrl Pts',(77.9973777224886,9.45989300507289,133.470863238684));
#61953=CARTESIAN_POINT('Ctrl Pts',(78.0149389348737,9.5363639988792,133.466606818847));
#61954=CARTESIAN_POINT('Ctrl Pts',(78.0368591598541,9.61171606121349,133.46235039901));
#61955=CARTESIAN_POINT('Ctrl Pts',(78.0629590532119,9.68547059234245,133.458093979173));
#61956=CARTESIAN_POINT('Ctrl Pts',(78.0890589465697,9.7592251234714,133.453837559336));
#61957=CARTESIAN_POINT('Ctrl Pts',(78.119338266365,9.8313817685356,133.4495811395));
#61958=CARTESIAN_POINT('Ctrl Pts',(78.153566954364,9.90148908506049,133.445324719663));
#61959=CARTESIAN_POINT('Ctrl Pts',(78.1846808093608,9.96521658991371,133.441455636816));
#61960=CARTESIAN_POINT('Ctrl Pts',(78.2191586994745,10.0274562334421,133.437586553969));
#61961=CARTESIAN_POINT('Ctrl Pts',(78.2568351259753,10.0878298508804,133.433717471122));
#61962=CARTESIAN_POINT('Ctrl Pts',(78.2944554164797,10.1481135146398,133.429854153016));
#61963=CARTESIAN_POINT('Ctrl Pts',(78.3352645285795,10.2065362623385,133.425990834909));
#61964=CARTESIAN_POINT('Ctrl Pts',(78.3790502987058,10.2627428987622,133.422127516803));
#61965=CARTESIAN_POINT('Ctrl Pts',(78.4227847081407,10.318883604823,133.418268730367));
#61966=CARTESIAN_POINT('Ctrl Pts',(78.4694885429769,10.3728129817268,133.414409943931));
#61967=CARTESIAN_POINT('Ctrl Pts',(78.5189063847538,10.4242047835114,133.410551157495));
#61968=CARTESIAN_POINT('Ctrl Pts',(78.5682930969139,10.4755642122293,133.406694801812));
#61969=CARTESIAN_POINT('Ctrl Pts',(78.6203900882308,10.5243888878679,133.402838446129));
#61970=CARTESIAN_POINT('Ctrl Pts',(78.6749026713719,10.5703867778871,133.398982090445));
#61971=CARTESIAN_POINT('Ctrl Pts',(78.7293991509501,10.6163710796691,133.395126873968));
#61972=CARTESIAN_POINT('Ctrl Pts',(78.7863094346104,10.6595299405508,133.391271657491));
#61973=CARTESIAN_POINT('Ctrl Pts',(78.8453043857994,10.6996104262583,133.387416441014));
#61974=CARTESIAN_POINT('Ctrl Pts',(78.9043016435144,10.7396924789928,133.383561073809));
#61975=CARTESIAN_POINT('Ctrl Pts',(78.9653833275151,10.776695646433,133.379705706604));
#61976=CARTESIAN_POINT('Ctrl Pts',(79.0281912878431,10.8104102820841,133.3758503394));
#61977=CARTESIAN_POINT('Ctrl Pts',(79.0910649909787,10.8441602077653,133.371990936677));
#61978=CARTESIAN_POINT('Ctrl Pts',(79.1556681486066,10.8746145000374,133.368131533954));
#61979=CARTESIAN_POINT('Ctrl Pts',(79.2216187718393,10.9016099037781,133.364272131231));
#61980=CARTESIAN_POINT('Ctrl Pts',(79.287606736833,10.9286205925285,133.360410543285));
#61981=CARTESIAN_POINT('Ctrl Pts',(79.3549432274509,10.9521683336448,133.356548955338));
#61982=CARTESIAN_POINT('Ctrl Pts',(79.4232296777173,10.9721393352991,133.352687367391));
#61983=CARTESIAN_POINT('Ctrl Pts',(79.4916355975762,10.9921452769366,133.348819023457));
#61984=CARTESIAN_POINT('Ctrl Pts',(79.560994322419,11.0085618736447,133.344950679524));
#61985=CARTESIAN_POINT('Ctrl Pts',(79.6308963387208,11.0213263095627,133.34108233559));
#61986=CARTESIAN_POINT('Ctrl Pts',(79.6724021443957,11.0289054642823,133.338785424284));
#61987=CARTESIAN_POINT('Ctrl Pts',(79.7140993616816,11.0351979879306,133.336488512977));
#61988=CARTESIAN_POINT('Ctrl Pts',(79.7559018530524,11.040199416027,133.334191601671));
#61989=CARTESIAN_POINT('Ctrl Pts',(79.8262968740995,11.0486217761438,133.330323623604));
#61990=CARTESIAN_POINT('Ctrl Pts',(79.897266151478,11.0534129893788,133.326455645537));
#61991=CARTESIAN_POINT('Ctrl Pts',(79.9684025636869,11.0545070368627,133.322587667471));
#61992=CARTESIAN_POINT('Ctrl Pts',(80.0394421231409,11.0555995947928,133.318724955685));
#61993=CARTESIAN_POINT('Ctrl Pts',(80.110647884865,11.0530049645083,133.314862243899));
#61994=CARTESIAN_POINT('Ctrl Pts',(80.1816065604028,11.0467087285979,133.310999532113));
#61995=CARTESIAN_POINT('Ctrl Pts',(80.2524923697582,11.0404189581784,133.307140786876));
#61996=CARTESIAN_POINT('Ctrl Pts',(80.323131115117,11.0304351676684,133.303282041639));
#61997=CARTESIAN_POINT('Ctrl Pts',(80.3931101843538,11.0167949686216,133.299423296402));
#61998=CARTESIAN_POINT('Ctrl Pts',(80.4630408059897,11.0031642128973,133.295567222635));
#61999=CARTESIAN_POINT('Ctrl Pts',(80.5323121827189,10.9858821674517,133.291711148868));
#62000=CARTESIAN_POINT('Ctrl Pts',(80.6005192195217,10.9650379715123,133.2878550751));
#62001=CARTESIAN_POINT('Ctrl Pts',(80.6687201287411,10.9441956481736,133.283999347755));
#62002=CARTESIAN_POINT('Ctrl Pts',(80.7358564197638,10.9197919393744,133.280143620409));
#62003=CARTESIAN_POINT('Ctrl Pts',(80.8015369135473,10.8919662097197,133.276287893064));
#62004=CARTESIAN_POINT('Ctrl Pts',(80.8672135547284,10.864142112231,133.272432391883));
#62005=CARTESIAN_POINT('Ctrl Pts',(80.9314341240358,10.8328965896448,133.268576890702));
#62006=CARTESIAN_POINT('Ctrl Pts',(80.9938281893631,10.7984168294718,133.264721389521));
#62007=CARTESIAN_POINT('Ctrl Pts',(81.0562666112036,10.7639125573211,133.260863147428));
#62008=CARTESIAN_POINT('Ctrl Pts',(81.1168755162782,10.7261697014419,133.257004905336));
#62009=CARTESIAN_POINT('Ctrl Pts',(81.1753108603474,10.6854204057295,133.253146663244));
#62010=CARTESIAN_POINT('Ctrl Pts',(81.2013268068549,10.6672784487623,133.251428938783));
#62011=CARTESIAN_POINT('Ctrl Pts',(81.2269123268175,10.6485411485174,133.249711214322));
#62012=CARTESIAN_POINT('Ctrl Pts',(81.252039109102,10.6292316077768,133.247993489861));
#62013=CARTESIAN_POINT('',(77.9452500001325,8.99997666224458,133.554074719471));
#62014=CARTESIAN_POINT('Ctrl Pts',(77.9452500001325,8.99997666241271,133.554074719462));
#62015=CARTESIAN_POINT('Ctrl Pts',(77.9452491949294,9.07087049904514,133.550206920375));
#62016=CARTESIAN_POINT('Ctrl Pts',(77.948921710863,9.14190368830042,133.546339121287));
#62017=CARTESIAN_POINT('Ctrl Pts',(77.9562848605137,9.21266403347663,133.5424713222));
#62018=CARTESIAN_POINT('Ctrl Pts',(77.9636370380662,9.28331893607806,133.538609286661));
#62019=CARTESIAN_POINT('Ctrl Pts',(77.97466888319,9.35370132203602,133.534747251122));
#62020=CARTESIAN_POINT('Ctrl Pts',(77.9893456969756,9.42339914528644,133.530885215583));
#62021=CARTESIAN_POINT('Ctrl Pts',(78.0040053078095,9.49301527449238,133.527027706804));
#62022=CARTESIAN_POINT('Ctrl Pts',(78.0223013014783,9.56194796136903,133.523170198025));
#62023=CARTESIAN_POINT('Ctrl Pts',(78.0441474066621,9.62979218448103,133.519312689246));
#62024=CARTESIAN_POINT('Ctrl Pts',(78.0659797748482,9.69759374662769,133.515457606098));
#62025=CARTESIAN_POINT('Ctrl Pts',(78.0913576770541,9.7643077412314,133.51160252295));
#62026=CARTESIAN_POINT('Ctrl Pts',(78.1201445418238,9.82954265644696,133.507747439802));
#62027=CARTESIAN_POINT('Ctrl Pts',(78.1489229525421,9.89475841364288,133.503893488805));
#62028=CARTESIAN_POINT('Ctrl Pts',(78.1811081421473,9.95849550926161,133.500039537807));
#62029=CARTESIAN_POINT('Ctrl Pts',(78.2165154281123,10.0203824500346,133.49618558681));
#62030=CARTESIAN_POINT('Ctrl Pts',(78.2519241814885,10.0822719556352,133.492331476091));
#62031=CARTESIAN_POINT('Ctrl Pts',(78.2905550529744,10.1423107333029,133.488477365371));
#62032=CARTESIAN_POINT('Ctrl Pts',(78.3321782980711,10.2001534623018,133.484623254651));
#62033=CARTESIAN_POINT('Ctrl Pts',(78.3738451508804,10.258056791792,133.480765106069));
#62034=CARTESIAN_POINT('Ctrl Pts',(78.4185103508028,10.3137590845539,133.476906957487));
#62035=CARTESIAN_POINT('Ctrl Pts',(78.4659023851082,10.3669462573501,133.473048808905));
#62036=CARTESIAN_POINT('Ctrl Pts',(78.513321406382,10.4201637171042,133.469188463334));
#62037=CARTESIAN_POINT('Ctrl Pts',(78.5634700109467,10.4708628601754,133.465328117764));
#62038=CARTESIAN_POINT('Ctrl Pts',(78.6160400988868,10.5187667874334,133.461467772193));
#62039=CARTESIAN_POINT('Ctrl Pts',(78.6687019134685,10.566754299607,133.457600690919));
#62040=CARTESIAN_POINT('Ctrl Pts',(78.7237932705989,10.6119365506021,133.453733609645));
#62041=CARTESIAN_POINT('Ctrl Pts',(78.7809738927825,10.6540776621496,133.449866528371));
#62042=CARTESIAN_POINT('Ctrl Pts',(78.8140980817258,10.6784896060542,133.44762636508));
#62043=CARTESIAN_POINT('Ctrl Pts',(78.8479228431126,10.7018818260453,133.445386201789));
#62044=CARTESIAN_POINT('Ctrl Pts',(78.882378183025,10.7242154844222,133.443146038498));
#62045=CARTESIAN_POINT('Ctrl Pts',(78.9418874898537,10.7627889111347,133.439276955651));
#62046=CARTESIAN_POINT('Ctrl Pts',(79.0035126729263,10.7983534291896,133.435407872804));
#62047=CARTESIAN_POINT('Ctrl Pts',(79.0669169949676,10.8306702784007,133.431538789957));
#62048=CARTESIAN_POINT('Ctrl Pts',(79.1302268477313,10.8629389771182,133.427675471851));
#62049=CARTESIAN_POINT('Ctrl Pts',(79.1953101483621,10.8919693932024,133.423812153744));
#62050=CARTESIAN_POINT('Ctrl Pts',(79.261802009964,10.917566502108,133.419948835638));
#62051=CARTESIAN_POINT('Ctrl Pts',(79.3282158766378,10.9431335856148,133.416090049202));
#62052=CARTESIAN_POINT('Ctrl Pts',(79.3960345712215,10.9652751877834,133.412231262766));
#62053=CARTESIAN_POINT('Ctrl Pts',(79.4648710613889,10.9838433863491,133.408372476331));
#62054=CARTESIAN_POINT('Ctrl Pts',(79.5336641896151,11.0023998883112,133.404516120647));
#62055=CARTESIAN_POINT('Ctrl Pts',(79.6034733735092,11.0173873263681,133.400659764964));
#62056=CARTESIAN_POINT('Ctrl Pts',(79.67389556436,11.0287073370883,133.396803409281));
#62057=CARTESIAN_POINT('Ctrl Pts',(79.7442969517905,11.040024003764,133.392948192804));
#62058=CARTESIAN_POINT('Ctrl Pts',(79.815310507302,11.0476753168868,133.389092976327));
#62059=CARTESIAN_POINT('Ctrl Pts',(79.8865238136955,11.0516141736793,133.385237759849));
#62060=CARTESIAN_POINT('Ctrl Pts',(79.9577399043162,11.0555531844694,133.381382392645));
#62061=CARTESIAN_POINT('Ctrl Pts',(80.0291552761605,11.0557794261325,133.37752702544));
#62062=CARTESIAN_POINT('Ctrl Pts',(80.1003549610611,11.0522978449266,133.373671658236));
#62063=CARTESIAN_POINT('Ctrl Pts',(80.1716291726167,11.0488126194546,133.369812255513));
#62064=CARTESIAN_POINT('Ctrl Pts',(80.2426867603528,11.0416118473837,133.36595285279));
#62065=CARTESIAN_POINT('Ctrl Pts',(80.313116238991,11.0307525165268,133.362093450067));
#62066=CARTESIAN_POINT('Ctrl Pts',(80.3835855953533,11.0198870370316,133.35823186212));
#62067=CARTESIAN_POINT('Ctrl Pts',(80.4534256588204,11.0053589740045,133.354370274173));
#62068=CARTESIAN_POINT('Ctrl Pts',(80.5222362332715,10.9872762463126,133.350508686226));
#62069=CARTESIAN_POINT('Ctrl Pts',(80.591167194289,10.9691618822405,133.346640342293));
#62070=CARTESIAN_POINT('Ctrl Pts',(80.6590646073791,10.9474805848859,133.34277199836));
#62071=CARTESIAN_POINT('Ctrl Pts',(80.7255451693941,10.9223895988246,133.338903654426));
#62072=CARTESIAN_POINT('Ctrl Pts',(80.7650194139748,10.907491293357,133.33660674312));
#62073=CARTESIAN_POINT('Ctrl Pts',(80.8039945234928,10.8913917709617,133.334309831813));
#62074=CARTESIAN_POINT('Ctrl Pts',(80.842394382625,10.8741316033358,133.332012920507));
#62075=CARTESIAN_POINT('Ctrl Pts',(80.9070806959089,10.8450560641121,133.328143668699));
#62076=CARTESIAN_POINT('Ctrl Pts',(80.9703866144579,10.8125706362717,133.324274416892));
#62077=CARTESIAN_POINT('Ctrl Pts',(81.0319288584356,10.7768287462859,133.320405165084));
#62078=CARTESIAN_POINT('Ctrl Pts',(81.0933729772624,10.7411438444454,133.31654208255));
#62079=CARTESIAN_POINT('Ctrl Pts',(81.1530585893509,10.702213033733,133.312679000016));
#62080=CARTESIAN_POINT('Ctrl Pts',(81.2106240071159,10.6602370541265,133.308815917482));
#62081=CARTESIAN_POINT('Ctrl Pts',(81.2245547333255,10.6500789435458,133.307881058547));
#62082=CARTESIAN_POINT('Ctrl Pts',(81.2383614027949,10.6397427119916,133.306946199613));
#62083=CARTESIAN_POINT('Ctrl Pts',(81.252039109102,10.6292316077768,133.306011340678));
#62084=CARTESIAN_POINT('Ctrl Pts',(81.252039109102,10.6292316077768,134.006113615495));
#62085=CARTESIAN_POINT('Ctrl Pts',(81.2874945667089,10.6019846409595,134.003679619815));
#62086=CARTESIAN_POINT('Ctrl Pts',(81.3220223711118,10.5736088323219,134.001245624136));
#62087=CARTESIAN_POINT('Ctrl Pts',(81.3555499459168,10.5441767731141,133.998811628456));
#62088=CARTESIAN_POINT('Ctrl Pts',(81.4088454244804,10.4973915317205,133.994942545609));
#62089=CARTESIAN_POINT('Ctrl Pts',(81.4598203372149,10.4477522689847,133.991073462762));
#62090=CARTESIAN_POINT('Ctrl Pts',(81.5081533895657,10.3955181532469,133.987204379915));
#62091=CARTESIAN_POINT('Ctrl Pts',(81.556414428079,10.3433618637364,133.983341061809));
#62092=CARTESIAN_POINT('Ctrl Pts',(81.6020410922966,10.2886187491794,133.979477743702));
#62093=CARTESIAN_POINT('Ctrl Pts',(81.6447465261169,10.2315869548377,133.975614425596));
#62094=CARTESIAN_POINT('Ctrl Pts',(81.6874018664798,10.1746220587688,133.97175563916));
#62095=CARTESIAN_POINT('Ctrl Pts',(81.7271424930792,10.1153742024436,133.967896852724));
#62096=CARTESIAN_POINT('Ctrl Pts',(81.7637208600582,10.0541756448978,133.964038066288));
#62097=CARTESIAN_POINT('Ctrl Pts',(81.8002761853481,9.9930156379557,133.960181710605));
#62098=CARTESIAN_POINT('Ctrl Pts',(81.8336729544594,9.92990778370281,133.956325354922));
#62099=CARTESIAN_POINT('Ctrl Pts',(81.8637069616786,9.86521322429253,133.952468999239));
#62100=CARTESIAN_POINT('Ctrl Pts',(81.8937320965514,9.8005377763029,133.948613782761));
#62101=CARTESIAN_POINT('Ctrl Pts',(81.9203962372521,9.73427699408904,133.944758566284));
#62102=CARTESIAN_POINT('Ctrl Pts',(81.9435419628081,9.6668149678164,133.940903349807));
#62103=CARTESIAN_POINT('Ctrl Pts',(81.9666885932928,9.59935030398031,133.937047982602));
#62104=CARTESIAN_POINT('Ctrl Pts',(81.9863163799621,9.5306847630487,133.933192615398));
#62105=CARTESIAN_POINT('Ctrl Pts',(82.0023172982287,9.46121903659115,133.929337248193));
#62106=CARTESIAN_POINT('Ctrl Pts',(82.0183349650936,9.39168059846039,133.92547784547));
#62107=CARTESIAN_POINT('Ctrl Pts',(82.0307180759414,9.32134077717102,133.921618442747));
#62108=CARTESIAN_POINT('Ctrl Pts',(82.0394096353204,9.25061105694344,133.917759040025));
#62109=CARTESIAN_POINT('Ctrl Pts',(82.0481061159286,9.17984128899266,133.913897452078));
#62110=CARTESIAN_POINT('Ctrl Pts',(82.053106850083,9.10868166744837,133.910035864131));
#62111=CARTESIAN_POINT('Ctrl Pts',(82.0544069244437,9.03754665494593,133.906174276184));
#62112=CARTESIAN_POINT('Ctrl Pts',(82.0557092733312,8.96628718918938,133.90230593225));
#62113=CARTESIAN_POINT('Ctrl Pts',(82.0532980524678,8.89505290409261,133.898437588317));
#62114=CARTESIAN_POINT('Ctrl Pts',(82.0472204087787,8.82425541152011,133.894569244383));
#62115=CARTESIAN_POINT('Ctrl Pts',(82.0436116788555,8.78221789780502,133.892272333077));
#62116=CARTESIAN_POINT('Ctrl Pts',(82.0387112898198,8.74033424979566,133.889975421771));
#62117=CARTESIAN_POINT('Ctrl Pts',(82.0325375986326,8.6986887445766,133.887678510464));
#62118=CARTESIAN_POINT('Ctrl Pts',(82.0221381885171,8.6285380559354,133.883809427617));
#62119=CARTESIAN_POINT('Ctrl Pts',(82.0080823914301,8.55878898639692,133.87994034477));
#62120=CARTESIAN_POINT('Ctrl Pts',(81.9904136794235,8.48985203395129,133.876071261923));
#62121=CARTESIAN_POINT('Ctrl Pts',(81.9727712929166,8.42101779412675,133.872207943817));
#62122=CARTESIAN_POINT('Ctrl Pts',(81.9515267963478,8.35299373629002,133.868344625711));
#62123=CARTESIAN_POINT('Ctrl Pts',(81.9267750863094,8.2861825658633,133.864481307604));
#62124=CARTESIAN_POINT('Ctrl Pts',(81.9020524100172,8.21944976491376,133.860622521168));
#62125=CARTESIAN_POINT('Ctrl Pts',(81.8738308599145,8.15392747869419,133.856763734733));
#62126=CARTESIAN_POINT('Ctrl Pts',(81.842255313806,8.09000388942938,133.852904948297));
#62127=CARTESIAN_POINT('Ctrl Pts',(81.8106996579762,8.0261205673385,133.849048592614));
#62128=CARTESIAN_POINT('Ctrl Pts',(81.7757944124787,7.96383437872305,133.84519223693));
#62129=CARTESIAN_POINT('Ctrl Pts',(81.7377322276222,7.90351275995428,133.841335881247));
#62130=CARTESIAN_POINT('Ctrl Pts',(81.6996812867163,7.8432089607957,133.83748066477));
#62131=CARTESIAN_POINT('Ctrl Pts',(81.6584755169941,7.7848689899309,133.833625448293));
#62132=CARTESIAN_POINT('Ctrl Pts',(81.614352223271,7.72883342487303,133.829770231815));
#62133=CARTESIAN_POINT('Ctrl Pts',(81.5702272044591,7.6727956689922,133.825914864611));
#62134=CARTESIAN_POINT('Ctrl Pts',(81.5231847374417,7.61906287809244,133.822059497406));
#62135=CARTESIAN_POINT('Ctrl Pts',(81.4735028660501,7.56794313442445,133.818204130202));
#62136=CARTESIAN_POINT('Ctrl Pts',(81.4237689912868,7.51676988232451,133.814344727479));
#62137=CARTESIAN_POINT('Ctrl Pts',(81.3713905363677,7.46821548650309,133.810485324756));
#62138=CARTESIAN_POINT('Ctrl Pts',(81.316682289586,7.42255101166775,133.806625922033));
#62139=CARTESIAN_POINT('Ctrl Pts',(81.2619430665653,7.37686068124805,133.802764334086));
#62140=CARTESIAN_POINT('Ctrl Pts',(81.2048718145002,7.33406382075419,133.798902746139));
#62141=CARTESIAN_POINT('Ctrl Pts',(81.1458140722613,7.29438935442232,133.795041158192));
#62142=CARTESIAN_POINT('Ctrl Pts',(81.0866530063856,7.25464547618953,133.791172814259));
#62143=CARTESIAN_POINT('Ctrl Pts',(81.0254989284646,7.21803514823513,133.787304470326));
#62144=CARTESIAN_POINT('Ctrl Pts',(80.9627232188051,7.18474201104264,133.783436126392));
#62145=CARTESIAN_POINT('Ctrl Pts',(80.9254488089371,7.16497350427086,133.781139215086));
#62146=CARTESIAN_POINT('Ctrl Pts',(80.8876030962549,7.14637361677536,133.778842303779));
#62147=CARTESIAN_POINT('Ctrl Pts',(80.8492668411795,7.12897263649808,133.776545392473));
#62148=CARTESIAN_POINT('Ctrl Pts',(80.7846904918394,7.09966117195791,133.772676309626));
#62149=CARTESIAN_POINT('Ctrl Pts',(80.7184684036558,7.07363938935495,133.768807226779));
#62150=CARTESIAN_POINT('Ctrl Pts',(80.6509690279539,7.05109341241178,133.764938143932));
#62151=CARTESIAN_POINT('Ctrl Pts',(80.5835702229554,7.02858102784983,133.761074825826));
#62152=CARTESIAN_POINT('Ctrl Pts',(80.5148983650352,7.00953432186643,133.757211507719));
#62153=CARTESIAN_POINT('Ctrl Pts',(80.4453432503829,6.99409198819128,133.753348189613));
#62154=CARTESIAN_POINT('Ctrl Pts',(80.3758697238534,6.97866776836761,133.749489403177));
#62155=CARTESIAN_POINT('Ctrl Pts',(80.3055154704918,6.96683962753385,133.745630616741));
#62156=CARTESIAN_POINT('Ctrl Pts',(80.2346851938957,6.95869639145322,133.741771830305));
#62157=CARTESIAN_POINT('Ctrl Pts',(80.1638995351801,6.9505582850142,133.737915474622));
#62158=CARTESIAN_POINT('Ctrl Pts',(80.0926389296103,6.94610053341757,133.734059118939));
#62159=CARTESIAN_POINT('Ctrl Pts',(80.0213165623717,6.94536057502328,133.730202763256));
#62160=CARTESIAN_POINT('Ctrl Pts',(79.9500152644746,6.94462083522012,133.726347546778));
#62161=CARTESIAN_POINT('Ctrl Pts',(79.8786527266226,6.94759671327875,133.722492330301));
#62162=CARTESIAN_POINT('Ctrl Pts',(79.8076437887117,6.95427356411498,133.718637113824));
#62163=CARTESIAN_POINT('Ctrl Pts',(79.7366320745637,6.96095067599612,133.714781746619));
#62164=CARTESIAN_POINT('Ctrl Pts',(79.6659744712473,6.97132900026171,133.710926379415));
#62165=CARTESIAN_POINT('Ctrl Pts',(79.5960806143545,6.98534204084173,133.70707101221));
#62166=CARTESIAN_POINT('Ctrl Pts',(79.5261135976526,6.99936974925407,133.703211609487));
#62167=CARTESIAN_POINT('Ctrl Pts',(79.4569124005045,7.0170396730388,133.699352206764));
#62168=CARTESIAN_POINT('Ctrl Pts',(79.3888754883123,7.03823436830124,133.695492804042));
#62169=CARTESIAN_POINT('Ctrl Pts',(79.3208000530859,7.05944106416663,133.691631216095));
#62170=CARTESIAN_POINT('Ctrl Pts',(79.2538906709939,7.08417633591524,133.687769628148));
#62171=CARTESIAN_POINT('Ctrl Pts',(79.1885270823425,7.11227404891269,133.683908040201));
#62172=CARTESIAN_POINT('Ctrl Pts',(79.12304913775,7.14042091986613,133.680039696267));
#62173=CARTESIAN_POINT('Ctrl Pts',(79.0591228218857,7.17194176216646,133.676171352334));
#62174=CARTESIAN_POINT('Ctrl Pts',(78.9971038465641,7.20662416991768,133.6723030084));
#62175=CARTESIAN_POINT('Ctrl Pts',(78.9602787637691,7.22721758556743,133.670006097094));
#62176=CARTESIAN_POINT('Ctrl Pts',(78.92412561328,7.24892480770593,133.667709185788));
#62177=CARTESIAN_POINT('Ctrl Pts',(78.8887136438618,7.27169441441594,133.665412274481));
#62178=CARTESIAN_POINT('Ctrl Pts',(78.8290631719135,7.31004918001196,133.661543191634));
#62179=CARTESIAN_POINT('Ctrl Pts',(78.7712838542149,7.35157084399013,133.657674108787));
#62180=CARTESIAN_POINT('Ctrl Pts',(78.7157319002096,7.39605080804882,133.65380502594));
#62181=CARTESIAN_POINT('Ctrl Pts',(78.6602627158453,7.44046449917939,133.649941707834));
#62182=CARTESIAN_POINT('Ctrl Pts',(78.6070146838403,7.48782744003637,133.646078389728));
#62183=CARTESIAN_POINT('Ctrl Pts',(78.5563157431666,7.53788737469662,133.642215071621));
#62184=CARTESIAN_POINT('Ctrl Pts',(78.5056762723309,7.58788858907282,133.638356285185));
#62185=CARTESIAN_POINT('Ctrl Pts',(78.4575802975035,7.64058017366701,133.63449749875));
#62186=CARTESIAN_POINT('Ctrl Pts',(78.4123219474131,7.69567030094621,133.630638712314));
#62187=CARTESIAN_POINT('Ctrl Pts',(78.3670921067645,7.75072572548481,133.626782356631));
#62188=CARTESIAN_POINT('Ctrl Pts',(78.3246966521299,7.80817632062366,133.622926000947));
#62189=CARTESIAN_POINT('Ctrl Pts',(78.285391140227,7.86769526165083,133.619069645264));
#62190=CARTESIAN_POINT('Ctrl Pts',(78.246097239566,7.9271966201868,133.615214428787));
#62191=CARTESIAN_POINT('Ctrl Pts',(78.2098917370284,7.98876470644017,133.61135921231));
#62192=CARTESIAN_POINT('Ctrl Pts',(78.1769873297903,8.05204305648689,133.607503995832));
#62193=CARTESIAN_POINT('Ctrl Pts',(78.1440816360882,8.11532388052786,133.603648628628));
#62194=CARTESIAN_POINT('Ctrl Pts',(78.1144775160843,8.18031466910409,133.599793261423));
#62195=CARTESIAN_POINT('Ctrl Pts',(78.0883412825139,8.24663520764542,133.595937894219));
#62196=CARTESIAN_POINT('Ctrl Pts',(78.062177691434,8.31302516570584,133.592078491496));
#62197=CARTESIAN_POINT('Ctrl Pts',(78.0394894114194,8.38074719936749,133.588219088773));
#62198=CARTESIAN_POINT('Ctrl Pts',(78.0203938937618,8.44940284540844,133.58435968605));
#62199=CARTESIAN_POINT('Ctrl Pts',(78.0012875640721,8.51809736481545,133.580498098103));
#62200=CARTESIAN_POINT('Ctrl Pts',(77.9857781519714,8.58772607453131,133.576636510156));
#62201=CARTESIAN_POINT('Ctrl Pts',(77.9739320459271,8.65787983400754,133.572774922209));
#62202=CARTESIAN_POINT('Ctrl Pts',(77.9620652146956,8.72815633000059,133.568906578276));
#62203=CARTESIAN_POINT('Ctrl Pts',(77.9538745412823,8.79895922703413,133.565038234342));
#62204=CARTESIAN_POINT('Ctrl Pts',(77.9493745075559,8.86987447506888,133.561169890409));
#62205=CARTESIAN_POINT('Ctrl Pts',(77.9467025170289,8.9119819085886,133.558872979102));
#62206=CARTESIAN_POINT('Ctrl Pts',(77.9453307150346,8.95412893627204,133.556576067796));
#62207=CARTESIAN_POINT('Ctrl Pts',(77.9452534594865,8.99622948970539,133.554279156489));
#62208=CARTESIAN_POINT('Ctrl Pts',(77.9452511674388,8.99747854533371,133.55421101083));
#62209=CARTESIAN_POINT('Ctrl Pts',(77.9452500143197,8.99872760305263,133.55414286517));
#62210=CARTESIAN_POINT('Ctrl Pts',(77.9452500001325,8.99997666154031,133.55407471951));
#62211=CARTESIAN_POINT('Origin',(80.,9.,141.545925280538));
#62212=CARTESIAN_POINT('',(81.252039109102,10.6292316077768,134.706120114193));
#62213=CARTESIAN_POINT('',(81.252039109102,10.6292316077768,134.647862573787));
#62214=CARTESIAN_POINT('',(81.252039109102,10.6292316077768,141.545925280538));
#62215=CARTESIAN_POINT('',(77.9452508583196,8.99812189887428,134.19592528059));
#62216=CARTESIAN_POINT('Ctrl Pts',(81.252039109102,10.6292316077768,134.647862573787));
#62217=CARTESIAN_POINT('Ctrl Pts',(81.3084423618865,10.585886586707,134.644002866747));
#62218=CARTESIAN_POINT('Ctrl Pts',(81.3626623260567,10.5395551758588,134.640143159707));
#62219=CARTESIAN_POINT('Ctrl Pts',(81.4143696942849,10.4904884871707,134.636283452668));
#62220=CARTESIAN_POINT('Ctrl Pts',(81.4660396062807,10.4414573418367,134.632426541556));
#62221=CARTESIAN_POINT('Ctrl Pts',(81.5152001817136,10.3896951826727,134.628569630445));
#62222=CARTESIAN_POINT('Ctrl Pts',(81.5615557470333,10.3354928720915,134.624712719334));
#62223=CARTESIAN_POINT('Ctrl Pts',(81.6078932397547,10.2813116933115,134.620857311912));
#62224=CARTESIAN_POINT('Ctrl Pts',(81.6514275774129,10.2246926201218,134.617001904491));
#62225=CARTESIAN_POINT('Ctrl Pts',(81.6919016788026,10.1659615224204,134.613146497069));
#62226=CARTESIAN_POINT('Ctrl Pts',(81.7323735395747,10.1072336760311,134.609291303081));
#62227=CARTESIAN_POINT('Ctrl Pts',(81.7697852261202,10.0463944381793,134.605436109092));
#62228=CARTESIAN_POINT('Ctrl Pts',(81.8039225228185,9.983799316003,134.601580915103));
#62229=CARTESIAN_POINT('Ctrl Pts',(81.8380934840931,9.92114246549826,134.597721919306));
#62230=CARTESIAN_POINT('Ctrl Pts',(81.8689833723166,9.85672669935811,134.593862923508));
#62231=CARTESIAN_POINT('Ctrl Pts',(81.8964240068341,9.7909320759731,134.590003927711));
#62232=CARTESIAN_POINT('Ctrl Pts',(81.9238778541335,9.72510577219794,134.586143073791));
#62233=CARTESIAN_POINT('Ctrl Pts',(81.9478789755098,9.6578997467298,134.58228221987));
#62234=CARTESIAN_POINT('Ctrl Pts',(81.9683084272647,9.5897113680935,134.57842136595));
#62235=CARTESIAN_POINT('Ctrl Pts',(81.9887754589296,9.52139755715708,134.574553410002));
#62236=CARTESIAN_POINT('Ctrl Pts',(82.0056575789907,9.45209825584912,134.570685454053));
#62237=CARTESIAN_POINT('Ctrl Pts',(82.0188866562537,9.38222275141696,134.566817498105));
#62238=CARTESIAN_POINT('Ctrl Pts',(82.0304714634763,9.32103222147011,134.563430298596));
#62239=CARTESIAN_POINT('Ctrl Pts',(82.0392556565754,9.25940017058367,134.560043099087));
#62240=CARTESIAN_POINT('Ctrl Pts',(82.045226284189,9.19760316030519,134.556655899578));
#62241=CARTESIAN_POINT('Ctrl Pts',(82.052046329133,9.12701453633118,134.552786816731));
#62242=CARTESIAN_POINT('Ctrl Pts',(82.0552210145704,9.05593416276994,134.548917733884));
#62243=CARTESIAN_POINT('Ctrl Pts',(82.054693562872,8.98477090967419,134.545048651037));
#62244=CARTESIAN_POINT('Ctrl Pts',(82.0541668970505,8.91371368627649,134.541185332931));
#62245=CARTESIAN_POINT('Ctrl Pts',(82.0499490467711,8.84257431027376,134.537322014824));
#62246=CARTESIAN_POINT('Ctrl Pts',(82.0420350207687,8.77176648700508,134.533458696718));
#62247=CARTESIAN_POINT('Ctrl Pts',(82.0341302779158,8.70104172128582,134.529599910282));
#62248=CARTESIAN_POINT('Ctrl Pts',(82.0225380250317,8.63064821622525,134.525741123846));
#62249=CARTESIAN_POINT('Ctrl Pts',(82.0073052791557,8.5609976323826,134.52188233741));
#62250=CARTESIAN_POINT('Ctrl Pts',(81.9920821287927,8.49139092330051,134.518025981727));
#62251=CARTESIAN_POINT('Ctrl Pts',(81.9732231387407,8.42252668040407,134.514169626044));
#62252=CARTESIAN_POINT('Ctrl Pts',(81.9508266910127,8.35480794786941,134.510313270361));
#62253=CARTESIAN_POINT('Ctrl Pts',(81.9284368594196,8.28710922012641,134.506458053883));
#62254=CARTESIAN_POINT('Ctrl Pts',(81.9025117972192,8.22055579189908,134.502602837406));
#62255=CARTESIAN_POINT('Ctrl Pts',(81.8731996991641,8.15553540657313,134.498747620929));
#62256=CARTESIAN_POINT('Ctrl Pts',(81.8438864550936,8.09051247914459,134.494892253724));
#62257=CARTESIAN_POINT('Ctrl Pts',(81.8111861139161,8.02702315557092,134.49103688652));
#62258=CARTESIAN_POINT('Ctrl Pts',(81.7752942420166,7.96543346431333,134.487181519315));
#62259=CARTESIAN_POINT('Ctrl Pts',(81.7393648011145,7.90377930544371,134.483322116592));
#62260=CARTESIAN_POINT('Ctrl Pts',(81.7002374058725,7.8440291687504,134.479462713869));
#62261=CARTESIAN_POINT('Ctrl Pts',(81.6581522078642,7.78652201583427,134.475603311147));
#62262=CARTESIAN_POINT('Ctrl Pts',(81.6160431808863,7.72898230191644,134.4717417232));
#62263=CARTESIAN_POINT('Ctrl Pts',(81.5709733243342,7.67368847666641,134.467880135253));
#62264=CARTESIAN_POINT('Ctrl Pts',(81.5232227929822,7.62094601793851,134.464018547306));
#62265=CARTESIAN_POINT('Ctrl Pts',(81.475388720364,7.56811128438857,134.460150203372));
#62266=CARTESIAN_POINT('Ctrl Pts',(81.424864953814,7.51783717203536,134.456281859439));
#62267=CARTESIAN_POINT('Ctrl Pts',(81.3719676447899,7.47039144087459,134.452413515505));
#62268=CARTESIAN_POINT('Ctrl Pts',(81.3405587449435,7.44221953108068,134.450116604199));
#62269=CARTESIAN_POINT('Ctrl Pts',(81.308313650705,7.41504403327825,134.447819692893));
#62270=CARTESIAN_POINT('Ctrl Pts',(81.2753034381162,7.38891381260064,134.445522781586));
#62271=CARTESIAN_POINT('Ctrl Pts',(81.2196986583658,7.34489818677875,134.441653698739));
#62272=CARTESIAN_POINT('Ctrl Pts',(81.1617035722648,7.30367843275997,134.437784615892));
#62273=CARTESIAN_POINT('Ctrl Pts',(81.1016308900003,7.26552401437867,134.433915533045));
#62274=CARTESIAN_POINT('Ctrl Pts',(81.0416477130365,7.22742644417791,134.430052214939));
#62275=CARTESIAN_POINT('Ctrl Pts',(80.9795934911436,7.19238540217982,134.426188896833));
#62276=CARTESIAN_POINT('Ctrl Pts',(80.9158130846975,7.16062946734575,134.422325578726));
#62277=CARTESIAN_POINT('Ctrl Pts',(80.8521074926436,7.12891078221101,134.41846679229));
#62278=CARTESIAN_POINT('Ctrl Pts',(80.786680170755,7.10046976549005,134.414608005855));
#62279=CARTESIAN_POINT('Ctrl Pts',(80.7199024698011,7.07549019319872,134.410749219419));
#62280=CARTESIAN_POINT('Ctrl Pts',(80.6531668339022,7.05052635620628,134.406892863736));
#62281=CARTESIAN_POINT('Ctrl Pts',(80.5850829605103,7.02901980744925,134.403036508052));
#62282=CARTESIAN_POINT('Ctrl Pts',(80.5160428208372,7.01110649617373,134.399180152369));
#62283=CARTESIAN_POINT('Ctrl Pts',(80.4470230763127,6.99319847666972,134.395324935892));
#62284=CARTESIAN_POINT('Ctrl Pts',(80.3770480962865,6.97888170925424,134.391469719415));
#62285=CARTESIAN_POINT('Ctrl Pts',(80.3065240147198,6.96824199499546,134.387614502937));
#62286=CARTESIAN_POINT('Ctrl Pts',(80.2359971758725,6.95760186475567,134.383759135733));
#62287=CARTESIAN_POINT('Ctrl Pts',(80.1649216735383,6.95063914338275,134.379903768528));
#62288=CARTESIAN_POINT('Ctrl Pts',(80.0937110916935,6.94738805572178,134.376048401324));
#62289=CARTESIAN_POINT('Ctrl Pts',(80.0224259717877,6.94413356505856,134.372188998601));
#62290=CARTESIAN_POINT('Ctrl Pts',(79.9510059763941,6.9445984857749,134.368329595878));
#62291=CARTESIAN_POINT('Ctrl Pts',(79.8798661318531,6.94876490469179,134.364470193155));
#62292=CARTESIAN_POINT('Ctrl Pts',(79.8086860073733,6.9529336826678,134.360608605208));
#62293=CARTESIAN_POINT('Ctrl Pts',(79.7377868325597,6.96080807732131,134.356747017261));
#62294=CARTESIAN_POINT('Ctrl Pts',(79.6675771998984,6.97231840653602,134.352885429315));
#62295=CARTESIAN_POINT('Ctrl Pts',(79.5972447329682,6.98384887348426,134.349017085381));
#62296=CARTESIAN_POINT('Ctrl Pts',(79.5276046915489,6.99902787181811,134.345148741448));
#62297=CARTESIAN_POINT('Ctrl Pts',(79.4590535039986,7.01773501999257,134.341280397514));
#62298=CARTESIAN_POINT('Ctrl Pts',(79.4183497815629,7.02884278623367,134.338983486208));
#62299=CARTESIAN_POINT('Ctrl Pts',(79.378029642418,7.04119350129801,134.336686574901));
#62300=CARTESIAN_POINT('Ctrl Pts',(79.3381726900253,7.05475395533839,134.334389663595));
#62301=CARTESIAN_POINT('Ctrl Pts',(79.2710347685908,7.07759616085897,134.330520580748));
#62302=CARTESIAN_POINT('Ctrl Pts',(79.2049492964154,7.10396296765435,134.326651497901));
#62303=CARTESIAN_POINT('Ctrl Pts',(79.140312266831,7.13373780943334,134.322782415054));
#62304=CARTESIAN_POINT('Ctrl Pts',(79.075771543197,7.16346828818303,134.318919096948));
#62305=CARTESIAN_POINT('Ctrl Pts',(79.0126754159973,7.19659652102821,134.315055778841));
#62306=CARTESIAN_POINT('Ctrl Pts',(78.9514029674593,7.23295675609033,134.311192460735));
#62307=CARTESIAN_POINT('Ctrl Pts',(78.8902023914798,7.26927434061071,134.307333674299));
#62308=CARTESIAN_POINT('Ctrl Pts',(78.8308216607735,7.30881615015988,134.303474887863));
#62309=CARTESIAN_POINT('Ctrl Pts',(78.7736165849994,7.3513698771673,134.299616101428));
#62310=CARTESIAN_POINT('Ctrl Pts',(78.7164475442283,7.39389679844704,134.295759745744));
#62311=CARTESIAN_POINT('Ctrl Pts',(78.6614518281799,7.43943158374137,134.291903390061));
#62312=CARTESIAN_POINT('Ctrl Pts',(78.6089562497839,7.48771866126542,134.288047034378));
#62313=CARTESIAN_POINT('Ctrl Pts',(78.5564761791075,7.53599147430328,134.284191817901));
#62314=CARTESIAN_POINT('Ctrl Pts',(78.5064951371637,7.58701463674079,134.280336601423));
#62315=CARTESIAN_POINT('Ctrl Pts',(78.4593054873361,7.64049347881392,134.276481384946));
#62316=CARTESIAN_POINT('Ctrl Pts',(78.4121139925344,7.69397441174974,134.272626017742));
#62317=CARTESIAN_POINT('Ctrl Pts',(78.3677144262844,7.74991084922807,134.268770650537));
#62318=CARTESIAN_POINT('Ctrl Pts',(78.3263598618199,7.80797388855254,134.264915283332));
#62319=CARTESIAN_POINT('Ctrl Pts',(78.2849620104032,7.86609770404621,134.261055880609));
#62320=CARTESIAN_POINT('Ctrl Pts',(78.2466158057059,7.92635216843353,134.257196477887));
#62321=CARTESIAN_POINT('Ctrl Pts',(78.211531300393,7.98837888860206,134.253337075164));
#62322=CARTESIAN_POINT('Ctrl Pts',(78.1764269299576,8.05044072878677,134.249475487217));
#62323=CARTESIAN_POINT('Ctrl Pts',(78.1445881522363,8.11427638742378,134.24561389927));
#62324=CARTESIAN_POINT('Ctrl Pts',(78.1161780375015,8.17950479824165,134.241752311323));
#62325=CARTESIAN_POINT('Ctrl Pts',(78.0877182182528,8.24484732850228,134.23788396739));
#62326=CARTESIAN_POINT('Ctrl Pts',(78.0626992088764,8.31158702080849,134.234015623456));
#62327=CARTESIAN_POINT('Ctrl Pts',(78.0412348877945,8.37932553000272,134.230147279523));
#62328=CARTESIAN_POINT('Ctrl Pts',(78.0284899916254,8.41954670741753,134.227850368216));
#62329=CARTESIAN_POINT('Ctrl Pts',(78.0169973859048,8.46011977480232,134.22555345691));
#62330=CARTESIAN_POINT('Ctrl Pts',(78.0067723452923,8.50095984228864,134.223256545603));
#62331=CARTESIAN_POINT('Ctrl Pts',(77.9843222460634,8.59062829470186,134.218213447125));
#62332=CARTESIAN_POINT('Ctrl Pts',(77.9679136797141,8.68186550115405,134.213170348647));
#62333=CARTESIAN_POINT('Ctrl Pts',(77.9577201042086,8.77396816651993,134.208127250169));
#62334=CARTESIAN_POINT('Ctrl Pts',(77.9494988556529,8.84825013992636,134.204059926976));
#62335=CARTESIAN_POINT('Ctrl Pts',(77.9453194352602,8.92309483675305,134.199992603783));
#62336=CARTESIAN_POINT('Ctrl Pts',(77.9452508583196,8.99812189887429,134.195925280589));
#62337=CARTESIAN_POINT('Ctrl Pts',(77.9452508583188,8.99812189982399,134.195925280538));
#62338=CARTESIAN_POINT('Ctrl Pts',(77.9451865584667,9.06846962007642,134.192111631088));
#62339=CARTESIAN_POINT('Ctrl Pts',(77.9487392155753,9.13891228886075,134.188297981638));
#62340=CARTESIAN_POINT('Ctrl Pts',(77.9559113871452,9.20904378798979,134.184484332188));
#62341=CARTESIAN_POINT('Ctrl Pts',(77.9630788626377,9.27912936756171,134.180673179777));
#62342=CARTESIAN_POINT('Ctrl Pts',(77.9738611037572,9.34890368688671,134.176862027366));
#62343=CARTESIAN_POINT('Ctrl Pts',(77.9882086454291,9.41796304642114,134.173050874956));
#62344=CARTESIAN_POINT('Ctrl Pts',(78.0025518660922,9.48700160754263,134.169240870339));
#62345=CARTESIAN_POINT('Ctrl Pts',(78.0204581554944,9.55532514838178,134.165430865722));
#62346=CARTESIAN_POINT('Ctrl Pts',(78.0418267999906,9.62253938129632,134.161620861105));
#62347=CARTESIAN_POINT('Ctrl Pts',(78.0631965645669,9.6897571373792,134.157810656779));
#62348=CARTESIAN_POINT('Ctrl Pts',(78.0880288903438,9.75586499614043,134.154000452454));
#62349=CARTESIAN_POINT('Ctrl Pts',(78.1161735511141,9.82048490112727,134.150190248128));
#62350=CARTESIAN_POINT('Ctrl Pts',(78.1443474516828,9.88517194044597,134.146376085339));
#62351=CARTESIAN_POINT('Ctrl Pts',(78.1758403520865,9.94836748481235,134.14256192255));
#62352=CARTESIAN_POINT('Ctrl Pts',(78.2104547888993,10.0097155539689,134.138747759761));
#62353=CARTESIAN_POINT('Ctrl Pts',(78.2450904309215,10.0711012056709,134.134931260371));
#62354=CARTESIAN_POINT('Ctrl Pts',(78.2828511440641,10.1306367118239,134.131114760981));
#62355=CARTESIAN_POINT('Ctrl Pts',(78.3234961567954,10.1879951288705,134.127298261591));
#62356=CARTESIAN_POINT('Ctrl Pts',(78.3642086074964,10.2454487146705,134.123475429888));
#62357=CARTESIAN_POINT('Ctrl Pts',(78.4078145926627,10.3007176182968,134.119652598184));
#62358=CARTESIAN_POINT('Ctrl Pts',(78.4540338348359,10.3535088395233,134.115829766481));
#62359=CARTESIAN_POINT('Ctrl Pts',(78.4689707705128,10.3705696790934,134.114594320191));
#62360=CARTESIAN_POINT('Ctrl Pts',(78.4841803654166,10.3873720424415,134.113358873901));
#62361=CARTESIAN_POINT('Ctrl Pts',(78.4996524028238,10.4039069236055,134.112123427611));
#62362=CARTESIAN_POINT('Ctrl Pts',(78.548106629474,10.4556896887627,134.108254344765));
#62363=CARTESIAN_POINT('Ctrl Pts',(78.5993397400989,10.5050624191808,134.104385261918));
#62364=CARTESIAN_POINT('Ctrl Pts',(78.6530824932537,10.5517122131762,134.100516179071));
#62365=CARTESIAN_POINT('Ctrl Pts',(78.7067451723865,10.5982925013052,134.096652860964));
#62366=CARTESIAN_POINT('Ctrl Pts',(78.7629097078902,10.6421575902791,134.092789542858));
#62367=CARTESIAN_POINT('Ctrl Pts',(78.821268994773,10.6830302373447,134.088926224751));
#62368=CARTESIAN_POINT('Ctrl Pts',(78.8795598262348,10.723854940811,134.085067438316));
#62369=CARTESIAN_POINT('Ctrl Pts',(78.9400398993909,10.7616938973594,134.08120865188));
#62370=CARTESIAN_POINT('Ctrl Pts',(79.0023692611189,10.7963102380545,134.077349865444));
#62371=CARTESIAN_POINT('Ctrl Pts',(79.0646593599195,10.8309047729934,134.073493509761));
#62372=CARTESIAN_POINT('Ctrl Pts',(79.1287960124374,10.8622804842886,134.069637154078));
#62373=CARTESIAN_POINT('Ctrl Pts',(79.1944117734203,10.8902447385712,134.065780798394));
#62374=CARTESIAN_POINT('Ctrl Pts',(79.2600081508502,10.9182007319331,134.061925581917));
#62375=CARTESIAN_POINT('Ctrl Pts',(79.3270823226435,10.9427470786496,134.05807036544));
#62376=CARTESIAN_POINT('Ctrl Pts',(79.3952453929252,10.9637386352878,134.054215148963));
#62377=CARTESIAN_POINT('Ctrl Pts',(79.463411128179,10.984731012633,134.050359781758));
#62378=CARTESIAN_POINT('Ctrl Pts',(79.5326653815291,11.0021681830996,134.046504414553));
#62379=CARTESIAN_POINT('Ctrl Pts',(79.602604232826,11.0159549019589,134.042649047349));
#62380=CARTESIAN_POINT('Ctrl Pts',(79.6726162910289,11.0297560517535,134.038789644626));
#62381=CARTESIAN_POINT('Ctrl Pts',(79.7433139000601,11.0398990281692,134.034930241903));
#62382=CARTESIAN_POINT('Ctrl Pts',(79.8142839731728,11.0463399326308,134.03107083918));
#62383=CARTESIAN_POINT('Ctrl Pts',(79.8852942300985,11.0527844839832,134.027209251234));
#62384=CARTESIAN_POINT('Ctrl Pts',(79.9565767725574,11.0555227719526,134.023347663287));
#62385=CARTESIAN_POINT('Ctrl Pts',(80.0277171909408,11.0545630483941,134.01948607534));
#62386=CARTESIAN_POINT('Ctrl Pts',(80.098982072036,11.0536016457648,134.015617731406));
#62387=CARTESIAN_POINT('Ctrl Pts',(80.170103847725,11.0489293463164,134.011749387473));
#62388=CARTESIAN_POINT('Ctrl Pts',(80.2406726110885,11.0406063453719,134.007881043539));
#62389=CARTESIAN_POINT('Ctrl Pts',(80.2825743119814,11.0356643869261,134.005584132233));
#62390=CARTESIAN_POINT('Ctrl Pts',(80.3242812036119,11.0294363074637,134.003287220927));
#62391=CARTESIAN_POINT('Ctrl Pts',(80.3657096343969,11.0219431312006,134.00099030962));
#62392=CARTESIAN_POINT('Ctrl Pts',(80.4354967859363,11.0093207021712,133.997121109306));
#62393=CARTESIAN_POINT('Ctrl Pts',(80.504766368103,10.9930562639826,133.993251908992));
#62394=CARTESIAN_POINT('Ctrl Pts',(80.5731094334081,10.973206309497,133.989382708677));
#62395=CARTESIAN_POINT('Ctrl Pts',(80.6413358826976,10.9533902256402,133.985520110506));
#62396=CARTESIAN_POINT('Ctrl Pts',(80.7086384934946,10.9300009151042,133.981657512336));
#62397=CARTESIAN_POINT('Ctrl Pts',(80.7746179998123,10.9031459525919,133.977794914165));
#62398=CARTESIAN_POINT('Ctrl Pts',(80.8405321010282,10.876317611248,133.973936144965));
#62399=CARTESIAN_POINT('Ctrl Pts',(80.9051252521823,10.846030615393,133.970077375766));
#62400=CARTESIAN_POINT('Ctrl Pts',(80.9680140702191,10.8124420880011,133.966218606566));
#62401=CARTESIAN_POINT('Ctrl Pts',(81.0308625996586,10.778875078499,133.962362309418));
#62402=CARTESIAN_POINT('Ctrl Pts',(81.0920085350437,10.7420109626267,133.95850601227));
#62403=CARTESIAN_POINT('Ctrl Pts',(81.151090755897,10.702053945734,133.954649715122));
#62404=CARTESIAN_POINT('Ctrl Pts',(81.1854604262026,10.678809905866,133.952406406396));
#62405=CARTESIAN_POINT('Ctrl Pts',(81.2191321621777,10.6545200838374,133.95016309767));
#62406=CARTESIAN_POINT('Ctrl Pts',(81.252039109102,10.6292316077769,133.947919788944));
#62407=CARTESIAN_POINT('',(77.9452507619582,9.00176953857242,134.254074719427));
#62408=CARTESIAN_POINT('Ctrl Pts',(77.9452507619582,9.00176953857242,134.254074719427));
#62409=CARTESIAN_POINT('Ctrl Pts',(77.9453248874363,9.08784241202325,134.249416661534));
#62410=CARTESIAN_POINT('Ctrl Pts',(77.950811182931,9.17367901479838,134.24475860364));
#62411=CARTESIAN_POINT('Ctrl Pts',(77.961598209329,9.25868069562512,134.240100545746));
#62412=CARTESIAN_POINT('Ctrl Pts',(77.972541792015,9.34491603873662,134.235374883655));
#62413=CARTESIAN_POINT('Ctrl Pts',(77.9889410126126,9.43029206338749,134.230649221565));
#62414=CARTESIAN_POINT('Ctrl Pts',(78.0106307458962,9.51420573054619,134.225923559474));
#62415=CARTESIAN_POINT('Ctrl Pts',(78.0180442984582,9.54288742865743,134.224308327796));
#62416=CARTESIAN_POINT('Ctrl Pts',(78.0260755171321,9.57139846976164,134.222693096117));
#62417=CARTESIAN_POINT('Ctrl Pts',(78.0347165430365,9.59971534604805,134.221077864439));
#62418=CARTESIAN_POINT('Ctrl Pts',(78.0554150258307,9.66754483563481,134.217208781592));
#62419=CARTESIAN_POINT('Ctrl Pts',(78.0796697562116,9.73443434293891,134.213339698745));
#62420=CARTESIAN_POINT('Ctrl Pts',(78.1073768028462,9.79998437240689,134.209470615898));
#62421=CARTESIAN_POINT('Ctrl Pts',(78.135042567363,9.86543673560005,134.205607297791));
#62422=CARTESIAN_POINT('Ctrl Pts',(78.1661502502832,9.92955313866793,134.201743979685));
#62423=CARTESIAN_POINT('Ctrl Pts',(78.2005462224256,9.99194942657027,134.197880661579));
#62424=CARTESIAN_POINT('Ctrl Pts',(78.2349018481058,10.054272523651,134.194021875143));
#62425=CARTESIAN_POINT('Ctrl Pts',(78.2725378680004,10.114879090029,134.190163088707));
#62426=CARTESIAN_POINT('Ctrl Pts',(78.313253381618,10.1734067529535,134.186304302271));
#62427=CARTESIAN_POINT('Ctrl Pts',(78.3539432474475,10.2318975477419,134.182447946588));
#62428=CARTESIAN_POINT('Ctrl Pts',(78.3977084815971,10.2883116393796,134.178591590905));
#62429=CARTESIAN_POINT('Ctrl Pts',(78.4443040202919,10.3423142632111,134.174735235221));
#62430=CARTESIAN_POINT('Ctrl Pts',(78.4908857941979,10.3963009341267,134.170880018744));
#62431=CARTESIAN_POINT('Ctrl Pts',(78.5402958955814,10.4478771838951,134.167024802267));
#62432=CARTESIAN_POINT('Ctrl Pts',(78.5922490883442,10.4967414383361,134.16316958579));
#62433=CARTESIAN_POINT('Ctrl Pts',(78.6442043123215,10.5456076032234,134.159314218585));
#62434=CARTESIAN_POINT('Ctrl Pts',(78.6987024697097,10.5917612310576,134.15545885138));
#62435=CARTESIAN_POINT('Ctrl Pts',(78.7554228609497,10.6349389308024,134.151603484176));
#62436=CARTESIAN_POINT('Ctrl Pts',(78.8122026229723,10.6781618258248,134.147744081453));
#62437=CARTESIAN_POINT('Ctrl Pts',(78.8712088748859,10.7184022797039,134.14388467873));
#62438=CARTESIAN_POINT('Ctrl Pts',(78.9320900753219,10.7554389636994,134.140025276007));
#62439=CARTESIAN_POINT('Ctrl Pts',(78.9930057471718,10.7924966181563,134.136163688061));
#62440=CARTESIAN_POINT('Ctrl Pts',(79.0557980530733,10.8263466609921,134.132302100114));
#62441=CARTESIAN_POINT('Ctrl Pts',(79.1200912978449,10.8568140020938,134.128440512167));
#62442=CARTESIAN_POINT('Ctrl Pts',(79.1844970259526,10.8873346469009,134.124572168233));
#62443=CARTESIAN_POINT('Ctrl Pts',(79.2504084863378,10.9144605892661,134.1207038243));
#62444=CARTESIAN_POINT('Ctrl Pts',(79.3174311513886,10.9380653573616,134.116835480366));
#62445=CARTESIAN_POINT('Ctrl Pts',(79.3572272811514,10.9520811893707,134.11453856906));
#62446=CARTESIAN_POINT('Ctrl Pts',(79.3974148942616,10.9648565381244,134.112241657753));
#62447=CARTESIAN_POINT('Ctrl Pts',(79.437909628772,10.976373440692,134.109944746447));
#62448=CARTESIAN_POINT('Ctrl Pts',(79.5061249302263,10.9957742094579,134.10607549038));
#62449=CARTESIAN_POINT('Ctrl Pts',(79.5754794623167,11.0116771155591,134.102206234313));
#62450=CARTESIAN_POINT('Ctrl Pts',(79.6455811722356,11.0239527803351,134.098336978246));
#62451=CARTESIAN_POINT('Ctrl Pts',(79.715560976673,11.0362070979737,134.094474450739));
#62452=CARTESIAN_POINT('Ctrl Pts',(79.786284902651,11.0448466246093,134.090611923232));
#62453=CARTESIAN_POINT('Ctrl Pts',(79.8573471332515,11.0497921168032,134.086749395724));
#62454=CARTESIAN_POINT('Ctrl Pts',(79.9283395278631,11.0547327488437,134.082890664093));
#62455=CARTESIAN_POINT('Ctrl Pts',(79.9996690856373,11.055986514164,134.079031932462));
#62456=CARTESIAN_POINT('Ctrl Pts',(80.0709224192409,11.0535256445803,134.07517320083));
#62457=CARTESIAN_POINT('Ctrl Pts',(80.1421295659905,11.0510663701476,134.071316970453));
#62458=CARTESIAN_POINT('Ctrl Pts',(80.2132601023318,11.0448972558307,134.067460740076));
#62459=CARTESIAN_POINT('Ctrl Pts',(80.2838999035955,11.0350426057551,134.063604509698));
#62460=CARTESIAN_POINT('Ctrl Pts',(80.3545175459519,11.0251910469718,134.059749488977));
#62461=CARTESIAN_POINT('Ctrl Pts',(80.4246442782314,11.0116563158045,134.055894468255));
#62462=CARTESIAN_POINT('Ctrl Pts',(80.4938720915145,10.9945144571356,134.052039447534));
#62463=CARTESIAN_POINT('Ctrl Pts',(80.5631419758927,10.9773621810243,134.048182084041));
#62464=CARTESIAN_POINT('Ctrl Pts',(80.631511375826,10.956598508231,134.044324720548));
#62465=CARTESIAN_POINT('Ctrl Pts',(80.6985844526089,10.9323502076676,134.040467357055));
#62466=CARTESIAN_POINT('Ctrl Pts',(80.7656748958071,10.908095628787,134.036608994822));
#62467=CARTESIAN_POINT('Ctrl Pts',(80.8314678959154,10.8803548068018,134.032750632588));
#62468=CARTESIAN_POINT('Ctrl Pts',(80.8955871455509,10.8493029030486,134.028892270355));
#62469=CARTESIAN_POINT('Ctrl Pts',(80.9598054148628,10.8182030456859,134.025027949634));
#62470=CARTESIAN_POINT('Ctrl Pts',(81.0223443385665,10.7837821180665,134.021163628913));
#62471=CARTESIAN_POINT('Ctrl Pts',(81.0828523129216,10.7462612722329,134.017299308192));
#62472=CARTESIAN_POINT('Ctrl Pts',(81.1412345966972,10.7100585618909,134.01357074396));
#62473=CARTESIAN_POINT('Ctrl Pts',(81.1977259678891,10.6709704106653,134.009842179727));
#62474=CARTESIAN_POINT('Ctrl Pts',(81.252039109102,10.6292316077768,134.006113615495));
#62475=CARTESIAN_POINT('Ctrl Pts',(81.252039109102,10.6292316077768,134.706120114193));
#62476=CARTESIAN_POINT('Ctrl Pts',(81.3086174334394,10.585752046946,134.702260546401));
#62477=CARTESIAN_POINT('Ctrl Pts',(81.3628983035071,10.539344867176,134.69840097861));
#62478=CARTESIAN_POINT('Ctrl Pts',(81.4145767274719,10.4902919997755,134.694541410819));
#62479=CARTESIAN_POINT('Ctrl Pts',(81.4662859518312,10.4412098968149,134.690679542721));
#62480=CARTESIAN_POINT('Ctrl Pts',(81.5153893085673,10.3894793202318,134.686817674624));
#62481=CARTESIAN_POINT('Ctrl Pts',(81.5616202009819,10.3354175041481,134.682955806526));
#62482=CARTESIAN_POINT('Ctrl Pts',(81.6079305738289,10.2812627446604,134.679087299081));
#62483=CARTESIAN_POINT('Ctrl Pts',(81.6513583294713,10.2247691308874,134.675218791636));
#62484=CARTESIAN_POINT('Ctrl Pts',(81.6916789789069,10.1662846114155,134.671350284191));
#62485=CARTESIAN_POINT('Ctrl Pts',(81.7116210733504,10.1373588915395,134.669436968263));
#62486=CARTESIAN_POINT('Ctrl Pts',(81.7308038117887,10.1079465715868,134.667523652334));
#62487=CARTESIAN_POINT('Ctrl Pts',(81.7492042338688,10.0780918841711,134.665610336405));
#62488=CARTESIAN_POINT('Ctrl Pts',(81.786413330588,10.0177201195048,134.661741253558));
#62489=CARTESIAN_POINT('Ctrl Pts',(81.8205661439276,9.95530150469948,134.657872170711));
#62490=CARTESIAN_POINT('Ctrl Pts',(81.851431639158,9.89117812362332,134.654003087864));
#62491=CARTESIAN_POINT('Ctrl Pts',(81.8822511463398,9.82715028318705,134.650139769758));
#62492=CARTESIAN_POINT('Ctrl Pts',(81.9097928487124,9.76142315249177,134.646276451652));
#62493=CARTESIAN_POINT('Ctrl Pts',(81.9338700765013,9.69436596238065,134.642413133545));
#62494=CARTESIAN_POINT('Ctrl Pts',(81.9579190617113,9.6273874303276,134.638554347109));
#62495=CARTESIAN_POINT('Ctrl Pts',(81.9785114811097,9.55908239284894,134.634695560674));
#62496=CARTESIAN_POINT('Ctrl Pts',(81.9955082589979,9.48984114850744,134.630836774238));
#62497=CARTESIAN_POINT('Ctrl Pts',(82.0124943301624,9.42064352107262,134.626980418555));
#62498=CARTESIAN_POINT('Ctrl Pts',(82.0258891379882,9.35051132747519,134.623124062871));
#62499=CARTESIAN_POINT('Ctrl Pts',(82.035603517282,9.27984975063267,134.619267707188));
#62500=CARTESIAN_POINT('Ctrl Pts',(82.0453150268509,9.20920904792752,134.615412490711));
#62501=CARTESIAN_POINT('Ctrl Pts',(82.0513482002261,9.13803975343951,134.611557274234));
#62502=CARTESIAN_POINT('Ctrl Pts',(82.0536653328037,9.06675524953479,134.607702057756));
#62503=CARTESIAN_POINT('Ctrl Pts',(82.0559825559742,8.9954679586192,134.603846690552));
#62504=CARTESIAN_POINT('Ctrl Pts',(82.0545834363202,8.92406593494232,134.599991323347));
#62505=CARTESIAN_POINT('Ctrl Pts',(82.0494823628482,8.85296392662273,134.596135956143));
#62506=CARTESIAN_POINT('Ctrl Pts',(82.0443759499432,8.78178749388894,134.59227655342));
#62507=CARTESIAN_POINT('Ctrl Pts',(82.0355598828126,8.71091218892561,134.588417150697));
#62508=CARTESIAN_POINT('Ctrl Pts',(82.0231004992737,8.64074809347968,134.584557747974));
#62509=CARTESIAN_POINT('Ctrl Pts',(82.010634061134,8.57054427057179,134.580696160027));
#62510=CARTESIAN_POINT('Ctrl Pts',(81.9945203098238,8.50105293226893,134.57683457208));
#62511=CARTESIAN_POINT('Ctrl Pts',(81.9748762440994,8.43267171497294,134.572972984134));
#62512=CARTESIAN_POINT('Ctrl Pts',(81.9551978103779,8.36417086228623,134.5691046402));
#62513=CARTESIAN_POINT('Ctrl Pts',(81.9319768891767,8.29678446768117,134.565236296267));
#62514=CARTESIAN_POINT('Ctrl Pts',(81.9053794077271,8.23089215638534,134.561367952333));
#62515=CARTESIAN_POINT('Ctrl Pts',(81.8895865886511,8.19176719815339,134.559071041027));
#62516=CARTESIAN_POINT('Ctrl Pts',(81.8726042233082,8.15316858353259,134.55677412972));
#62517=CARTESIAN_POINT('Ctrl Pts',(81.8544746051533,8.11517148478284,134.554477218414));
#62518=CARTESIAN_POINT('Ctrl Pts',(81.8239357704899,8.05116643478686,134.550608135567));
#62519=CARTESIAN_POINT('Ctrl Pts',(81.7900196413613,7.9886188983192,134.54673905272));
#62520=CARTESIAN_POINT('Ctrl Pts',(81.7528883050503,7.9279085148562,134.542869969873));
#62521=CARTESIAN_POINT('Ctrl Pts',(81.7158122925786,7.8672885868368,134.539006651767));
#62522=CARTESIAN_POINT('Ctrl Pts',(81.6755308333296,7.8085007894651,134.53514333366));
#62523=CARTESIAN_POINT('Ctrl Pts',(81.6322528843361,7.75190221373627,134.531280015554));
#62524=CARTESIAN_POINT('Ctrl Pts',(81.5890257003601,7.69537002811496,134.527421229118));
#62525=CARTESIAN_POINT('Ctrl Pts',(81.5428093020265,7.64102234732982,134.523562442682));
#62526=CARTESIAN_POINT('Ctrl Pts',(81.4938561601464,7.58918770373492,134.519703656246));
#62527=CARTESIAN_POINT('Ctrl Pts',(81.4449338551561,7.53738571216467,134.515847300563));
#62528=CARTESIAN_POINT('Ctrl Pts',(81.3932785596597,7.48809396942154,134.51199094488));
#62529=CARTESIAN_POINT('Ctrl Pts',(81.3391823197827,7.44160714937429,134.508134589197));
#62530=CARTESIAN_POINT('Ctrl Pts',(81.2851020604767,7.39513406199919,134.504279372719));
#62531=CARTESIAN_POINT('Ctrl Pts',(81.2285826565668,7.35146456875093,134.500424156242));
#62532=CARTESIAN_POINT('Ctrl Pts',(81.1699509540174,7.31085455697452,134.496568939765));
#62533=CARTESIAN_POINT('Ctrl Pts',(81.1113169591437,7.270242957468,134.49271357256));
#62534=CARTESIAN_POINT('Ctrl Pts',(81.0505709022709,7.2326913517047,134.488858205356));
#62535=CARTESIAN_POINT('Ctrl Pts',(80.9880690313265,7.1984126022217,134.485002838151));
#62536=CARTESIAN_POINT('Ctrl Pts',(80.9255017379667,7.1640979722354,134.481143435428));
#62537=CARTESIAN_POINT('Ctrl Pts',(80.8611753885608,7.13306327124748,134.477284032705));
#62538=CARTESIAN_POINT('Ctrl Pts',(80.7954704866755,7.10547518693255,134.473424629983));
#62539=CARTESIAN_POINT('Ctrl Pts',(80.7297283821587,7.07787148202758,134.469563042036));
#62540=CARTESIAN_POINT('Ctrl Pts',(80.6626066286407,7.05371844319009,134.465701454089));
#62541=CARTESIAN_POINT('Ctrl Pts',(80.5945027514386,7.03313344605386,134.461839866142));
#62542=CARTESIAN_POINT('Ctrl Pts',(80.5262797240621,7.01251243472729,134.457971522208));
#62543=CARTESIAN_POINT('Ctrl Pts',(80.4570716142902,6.995472044441,134.454103178275));
#62544=CARTESIAN_POINT('Ctrl Pts',(80.3872873534986,6.98207877549195,134.450234834341));
#62545=CARTESIAN_POINT('Ctrl Pts',(80.3458514676571,6.97412623781481,134.447937923035));
#62546=CARTESIAN_POINT('Ctrl Pts',(80.3042125940085,6.96745855572034,134.445641011728));
#62547=CARTESIAN_POINT('Ctrl Pts',(80.2624568263924,6.96208096903237,134.443344100422));
#62548=CARTESIAN_POINT('Ctrl Pts',(80.192120403827,6.95302257467726,134.439475017575));
#62549=CARTESIAN_POINT('Ctrl Pts',(80.1211767085347,6.94759208376961,134.435605934728));
#62550=CARTESIAN_POINT('Ctrl Pts',(80.0500326011492,6.94585923040259,134.431736851881));
#62551=CARTESIAN_POINT('Ctrl Pts',(79.9789944949355,6.94412895890066,134.427873533775));
#62552=CARTESIAN_POINT('Ctrl Pts',(79.9077570510322,6.94608540087243,134.424010215668));
#62553=CARTESIAN_POINT('Ctrl Pts',(79.8367336075784,6.95174668373132,134.420146897562));
#62554=CARTESIAN_POINT('Ctrl Pts',(79.7657934745967,6.95740132590758,134.416288111126));
#62555=CARTESIAN_POINT('Ctrl Pts',(79.6950673253459,6.96675213837446,134.41242932469));
#62556=CARTESIAN_POINT('Ctrl Pts',(79.624968105923,6.97976520153597,134.408570538255));
#62557=CARTESIAN_POINT('Ctrl Pts',(79.5549130438682,6.99277006742189,134.404714182571));
#62558=CARTESIAN_POINT('Ctrl Pts',(79.4854846046205,7.00943251859566,134.400857826888));
#62559=CARTESIAN_POINT('Ctrl Pts',(79.4170887535154,7.02966702275434,134.397001471205));
#62560=CARTESIAN_POINT('Ctrl Pts',(79.3487131072294,7.04989554943792,134.393146254728));
#62561=CARTESIAN_POINT('Ctrl Pts',(79.2813699090746,7.07369389646482,134.38929103825));
#62562=CARTESIAN_POINT('Ctrl Pts',(79.2154514132926,7.10092625798908,134.385435821773));
#62563=CARTESIAN_POINT('Ctrl Pts',(79.1495303402946,7.12815968421718,134.381580454569));
#62564=CARTESIAN_POINT('Ctrl Pts',(79.0850345283947,7.15882720397901,134.377725087364));
#62565=CARTESIAN_POINT('Ctrl Pts',(79.022336032316,7.19274497405804,134.373869720159));
#62566=CARTESIAN_POINT('Ctrl Pts',(78.9595719080091,7.22669824679341,134.370010317436));
#62567=CARTESIAN_POINT('Ctrl Pts',(78.8986092831646,7.26390832963901,134.366150914714));
#62568=CARTESIAN_POINT('Ctrl Pts',(78.8397945752582,7.30414595707656,134.362291511991));
#62569=CARTESIAN_POINT('Ctrl Pts',(78.7809465660022,7.34440636737485,134.358429924044));
#62570=CARTESIAN_POINT('Ctrl Pts',(78.7242492809826,7.38769743980121,134.354568336097));
#62571=CARTESIAN_POINT('Ctrl Pts',(78.6700169412605,7.43374886242149,134.35070674815));
#62572=CARTESIAN_POINT('Ctrl Pts',(78.6156897201163,7.47988085365626,134.346838404217));
#62573=CARTESIAN_POINT('Ctrl Pts',(78.5638364078417,7.52878250358203,134.342970060283));
#62574=CARTESIAN_POINT('Ctrl Pts',(78.5147346698664,7.58014632387587,134.33910171635));
#62575=CARTESIAN_POINT('Ctrl Pts',(78.4855794708822,7.6106446822438,134.336804805043));
#62576=CARTESIAN_POINT('Ctrl Pts',(78.4573936249812,7.64201045776524,134.334507893737));
#62577=CARTESIAN_POINT('Ctrl Pts',(78.430228229917,7.67417416213494,134.332210982431));
#62578=CARTESIAN_POINT('Ctrl Pts',(78.3847678948149,7.72799899241335,134.328367181984));
#62579=CARTESIAN_POINT('Ctrl Pts',(78.3419831696139,7.78427842280377,134.324523381537));
#62580=CARTESIAN_POINT('Ctrl Pts',(78.3021523840385,7.84271393533238,134.32067958109));
#62581=CARTESIAN_POINT('Ctrl Pts',(78.262377579922,7.90106731779013,134.316841183036));
#62582=CARTESIAN_POINT('Ctrl Pts',(78.2255487573432,7.96157037052464,134.313002784982));
#62583=CARTESIAN_POINT('Ctrl Pts',(78.1919047913615,8.02389074433322,134.309164386928));
#62584=CARTESIAN_POINT('Ctrl Pts',(78.1582964950691,8.08614504542086,134.305330058384));
#62585=CARTESIAN_POINT('Ctrl Pts',(78.1278665893404,8.15021241435526,134.301495729841));
#62586=CARTESIAN_POINT('Ctrl Pts',(78.10081028452,8.21573219681344,134.297661401297));
#62587=CARTESIAN_POINT('Ctrl Pts',(78.0737690938024,8.2812153788293,134.293829214673));
#62588=CARTESIAN_POINT('Ctrl Pts',(78.0500979587481,8.34814891320326,134.289997028049));
#62589=CARTESIAN_POINT('Ctrl Pts',(78.0299450759375,8.41614971210322,134.286164841425));
#62590=CARTESIAN_POINT('Ctrl Pts',(78.0097994694118,8.48412595902305,134.282334038429));
#62591=CARTESIAN_POINT('Ctrl Pts',(77.9931697296337,8.55316823242713,134.278503235433));
#62592=CARTESIAN_POINT('Ctrl Pts',(77.9801543906814,8.62287763654694,134.274672432436));
#62593=CARTESIAN_POINT('Ctrl Pts',(77.9671331495253,8.69261865252947,134.270839892245));
#62594=CARTESIAN_POINT('Ctrl Pts',(77.9577296763162,8.76302691922407,134.267007352053));
#62595=CARTESIAN_POINT('Ctrl Pts',(77.9519912481153,8.83369391260768,134.263174811862));
#62596=CARTESIAN_POINT('Ctrl Pts',(77.9474494190888,8.88962515205753,134.260141447729));
#62597=CARTESIAN_POINT('Ctrl Pts',(77.9452024908778,8.9457182021302,134.257108083595));
#62598=CARTESIAN_POINT('Ctrl Pts',(77.9452507619577,9.00176953792933,134.254074719462));
#62599=CARTESIAN_POINT('Origin',(80.,9.,141.545925280538));
#62600=CARTESIAN_POINT('',(81.252039109102,10.6292316077768,135.406026966675));
#62601=CARTESIAN_POINT('',(81.252039109102,10.6292316077768,135.347982838459));
#62602=CARTESIAN_POINT('',(81.252039109102,10.6292316077768,141.545925280538));
#62603=CARTESIAN_POINT('',(77.9452501039006,9.00065343667963,134.895925280576));
#62604=CARTESIAN_POINT('Ctrl Pts',(81.252039109102,10.6292316077768,135.347982838459));
#62605=CARTESIAN_POINT('Ctrl Pts',(81.3084942653525,10.585846699702,135.344113662479));
#62606=CARTESIAN_POINT('Ctrl Pts',(81.3626078688897,10.5395885223021,135.340244486498));
#62607=CARTESIAN_POINT('Ctrl Pts',(81.4140911481656,10.4907527585686,135.336375310518));
#62608=CARTESIAN_POINT('Ctrl Pts',(81.4220196871467,10.483231942842,135.335779448852));
#62609=CARTESIAN_POINT('Ctrl Pts',(81.4298859203367,10.4756500603419,135.335183587185));
#62610=CARTESIAN_POINT('Ctrl Pts',(81.4376888783052,10.4680082600917,135.334587725519));
#62611=CARTESIAN_POINT('Ctrl Pts',(81.4883554885788,10.4183880882766,135.330718642672));
#62612=CARTESIAN_POINT('Ctrl Pts',(81.5365494452545,10.3660446008768,135.326849559825));
#62613=CARTESIAN_POINT('Ctrl Pts',(81.5819640552088,10.3112540907572,135.322980476978));
#62614=CARTESIAN_POINT('Ctrl Pts',(81.6273109996591,10.2565452157652,135.319117158872));
#62615=CARTESIAN_POINT('Ctrl Pts',(81.6698865098526,10.1993969261075,135.315253840765));
#62616=CARTESIAN_POINT('Ctrl Pts',(81.7094204040751,10.1401225568471,135.311390522659));
#62617=CARTESIAN_POINT('Ctrl Pts',(81.748907925055,10.0809177163991,135.307531736223));
#62618=CARTESIAN_POINT('Ctrl Pts',(81.7853606487122,10.0195921522385,135.303672949787));
#62619=CARTESIAN_POINT('Ctrl Pts',(81.8185495042662,9.95649112020606,135.299814163351));
#62620=CARTESIAN_POINT('Ctrl Pts',(81.8517174532748,9.89342983719681,135.295957807668));
#62621=CARTESIAN_POINT('Ctrl Pts',(81.8816253876486,9.82859573415704,135.292101451985));
#62622=CARTESIAN_POINT('Ctrl Pts',(81.9080890863941,9.76236054520402,135.288245096302));
#62623=CARTESIAN_POINT('Ctrl Pts',(81.934544967498,9.69614492278905,135.284389879824));
#62624=CARTESIAN_POINT('Ctrl Pts',(81.9575584527788,9.6285294870208,135.280534663347));
#62625=CARTESIAN_POINT('Ctrl Pts',(81.9769932870615,9.55990633628632,135.27667944687));
#62626=CARTESIAN_POINT('Ctrl Pts',(81.9964288811882,9.49128050259189,135.272824079665));
#62627=CARTESIAN_POINT('Ctrl Pts',(82.0122854162816,9.42164734371053,135.268968712461));
#62628=CARTESIAN_POINT('Ctrl Pts',(82.0244768648761,9.35141284279525,135.265113345256));
#62629=CARTESIAN_POINT('Ctrl Pts',(82.0366810745928,9.28110482550954,135.261253942533));
#62630=CARTESIAN_POINT('Ctrl Pts',(82.0452124563531,9.21019468929086,135.25739453981));
#62631=CARTESIAN_POINT('Ctrl Pts',(82.0500365241631,9.13909641295679,135.253535137088));
#62632=CARTESIAN_POINT('Ctrl Pts',(82.0548633233981,9.06795788022017,135.249673549141));
#62633=CARTESIAN_POINT('Ctrl Pts',(82.0559786224031,8.99663148126061,135.245811961194));
#62634=CARTESIAN_POINT('Ctrl Pts',(82.0534001022136,8.92553133055263,135.241950373247));
#62635=CARTESIAN_POINT('Ctrl Pts',(82.0508170708106,8.85430678758249,135.238082029313));
#62636=CARTESIAN_POINT('Ctrl Pts',(82.0445273605926,8.78330976718955,135.23421368538));
#62637=CARTESIAN_POINT('Ctrl Pts',(82.0346004801355,8.71294870017266,135.230345341446));
#62638=CARTESIAN_POINT('Ctrl Pts',(82.0287061841907,8.67117032339324,135.22804843014));
#62639=CARTESIAN_POINT('Ctrl Pts',(82.0215305338992,8.62961597553206,135.225751518834));
#62640=CARTESIAN_POINT('Ctrl Pts',(82.0130964518113,8.58836880802734,135.223454607527));
#62641=CARTESIAN_POINT('Ctrl Pts',(81.9988894764508,8.51888910812375,135.21958552468));
#62642=CARTESIAN_POINT('Ctrl Pts',(81.9810534349363,8.45000969351871,135.215716441833));
#62643=CARTESIAN_POINT('Ctrl Pts',(81.9596541057284,8.3821380830625,135.211847358986));
#62644=CARTESIAN_POINT('Ctrl Pts',(81.9382866604538,8.31436759792095,135.20798404088));
#62645=CARTESIAN_POINT('Ctrl Pts',(81.9133666108286,8.2476023958639,135.204120722774));
#62646=CARTESIAN_POINT('Ctrl Pts',(81.8850106587592,8.18223941225805,135.200257404667));
#62647=CARTESIAN_POINT('Ctrl Pts',(81.8566879682107,8.11695309940681,135.196398618231));
#62648=CARTESIAN_POINT('Ctrl Pts',(81.824937573179,8.05306618136426,135.192539831796));
#62649=CARTESIAN_POINT('Ctrl Pts',(81.7899252910328,7.99095836804368,135.18868104536));
#62650=CARTESIAN_POINT('Ctrl Pts',(81.754935064057,7.92888967809133,135.184824689677));
#62651=CARTESIAN_POINT('Ctrl Pts',(81.7166872645513,7.86859829157177,135.180968333993));
#62652=CARTESIAN_POINT('Ctrl Pts',(81.6753942808023,7.8104405999047,135.17711197831));
#62653=CARTESIAN_POINT('Ctrl Pts',(81.6341134954141,7.75230008860211,135.173256761833));
#62654=CARTESIAN_POINT('Ctrl Pts',(81.5897895927765,7.69629241668233,135.169401545356));
#62655=CARTESIAN_POINT('Ctrl Pts',(81.5426780855886,7.64274472307355,135.165546328878));
#62656=CARTESIAN_POINT('Ctrl Pts',(81.4955647364817,7.58919493591011,135.161690961674));
#62657=CARTESIAN_POINT('Ctrl Pts',(81.4456638889808,7.53810568127019,135.157835594469));
#62658=CARTESIAN_POINT('Ctrl Pts',(81.3932699633574,7.48976943094574,135.153980227265));
#62659=CARTESIAN_POINT('Ctrl Pts',(81.3408211955811,7.44138258574787,135.150120824542));
#62660=CARTESIAN_POINT('Ctrl Pts',(81.2858744981693,7.39575482734537,135.146261421819));
#62661=CARTESIAN_POINT('Ctrl Pts',(81.228758963896,7.35313966252593,135.142402019096));
#62662=CARTESIAN_POINT('Ctrl Pts',(81.1716110903585,7.31050036866542,135.138540431149));
#62663=CARTESIAN_POINT('Ctrl Pts',(81.1122923395098,7.27087733397399,135.134678843202));
#62664=CARTESIAN_POINT('Ctrl Pts',(81.0511602124635,7.2344803115701,135.130817255255));
#62665=CARTESIAN_POINT('Ctrl Pts',(80.9899211325698,7.19801961127091,135.126948911322));
#62666=CARTESIAN_POINT('Ctrl Pts',(80.9268627722766,7.16479641822085,135.123080567389));
#62667=CARTESIAN_POINT('Ctrl Pts',(80.8623659678916,7.1349738607938,135.119212223455));
#62668=CARTESIAN_POINT('Ctrl Pts',(80.8240696215045,7.11726608441226,135.116915312149));
#62669=CARTESIAN_POINT('Ctrl Pts',(80.7852665078412,7.10075632507813,135.114618400842));
#62670=CARTESIAN_POINT('Ctrl Pts',(80.7460389179154,7.08547042450225,135.112321489536));
#62671=CARTESIAN_POINT('Ctrl Pts',(80.6799611399519,7.05972175255636,135.108452406689));
#62672=CARTESIAN_POINT('Ctrl Pts',(80.6124193474611,7.03734756206001,135.104583323842));
#62673=CARTESIAN_POINT('Ctrl Pts',(80.5437915874515,7.0185136205573,135.100714240995));
#62674=CARTESIAN_POINT('Ctrl Pts',(80.4752660793817,6.99970774068812,135.096850922889));
#62675=CARTESIAN_POINT('Ctrl Pts',(80.4056582801984,6.98443176700711,135.092987604782));
#62676=CARTESIAN_POINT('Ctrl Pts',(80.3353649652504,6.97280294431385,135.089124286676));
#62677=CARTESIAN_POINT('Ctrl Pts',(80.2651541043337,6.96118776222513,135.08526550024));
#62678=CARTESIAN_POINT('Ctrl Pts',(80.1942598018295,6.95321131225774,135.081406713804));
#62679=CARTESIAN_POINT('Ctrl Pts',(80.1230910006734,6.94894023293976,135.077547927368));
#62680=CARTESIAN_POINT('Ctrl Pts',(80.0519670306434,6.94467184408856,135.073691571685));
#62681=CARTESIAN_POINT('Ctrl Pts',(79.9805693887846,6.9441042240778,135.069835216002));
#62682=CARTESIAN_POINT('Ctrl Pts',(79.9093126865442,6.94725223817485,135.065978860319));
#62683=CARTESIAN_POINT('Ctrl Pts',(79.8380770342471,6.95039932231701,135.062123643841));
#62684=CARTESIAN_POINT('Ctrl Pts',(79.7669827239569,6.95725984002718,135.058268427364));
#62685=CARTESIAN_POINT('Ctrl Pts',(79.6964431809676,6.96779656035156,135.054413210887));
#62686=CARTESIAN_POINT('Ctrl Pts',(79.6259008800932,6.97833369263019,135.050557843682));
#62687=CARTESIAN_POINT('Ctrl Pts',(79.5559138697091,6.99254723893165,135.046702476478));
#62688=CARTESIAN_POINT('Ctrl Pts',(79.4868875528032,7.01034847799125,135.042847109273));
#62689=CARTESIAN_POINT('Ctrl Pts',(79.4177889841661,7.02816835009397,135.03898770655));
#62690=CARTESIAN_POINT('Ctrl Pts',(79.3496535877346,7.04958328988869,135.035128303828));
#62691=CARTESIAN_POINT('Ctrl Pts',(79.2828728363905,7.07445431274316,135.031268901105));
#62692=CARTESIAN_POINT('Ctrl Pts',(79.2160542732604,7.09933941776615,135.027407313158));
#62693=CARTESIAN_POINT('Ctrl Pts',(79.150592328098,7.12768430823989,135.023545725211));
#62694=CARTESIAN_POINT('Ctrl Pts',(79.0868571230049,7.15930240161697,135.019684137264));
#62695=CARTESIAN_POINT('Ctrl Pts',(79.0230104108859,7.1909758119817,135.015815793331));
#62696=CARTESIAN_POINT('Ctrl Pts',(78.9608968938108,7.22593362020604,135.011947449397));
#62697=CARTESIAN_POINT('Ctrl Pts',(78.9008601794406,7.26394435073046,135.008079105464));
#62698=CARTESIAN_POINT('Ctrl Pts',(78.8652121061538,7.28651402866228,135.005782194157));
#62699=CARTESIAN_POINT('Ctrl Pts',(78.8302956660187,7.31015923941541,135.003485282851));
#62700=CARTESIAN_POINT('Ctrl Pts',(78.7961772025377,7.33482486362246,135.001188371544));
#62701=CARTESIAN_POINT('Ctrl Pts',(78.7391631807262,7.37604261767866,134.99735009344));
#62702=CARTESIAN_POINT('Ctrl Pts',(78.6841480871174,7.42027912081088,134.993511815336));
#62703=CARTESIAN_POINT('Ctrl Pts',(78.6314732100562,7.46731216886606,134.989673537232));
#62704=CARTESIAN_POINT('Ctrl Pts',(78.5778665128151,7.51517723297413,134.985767359871));
#62705=CARTESIAN_POINT('Ctrl Pts',(78.5266841028894,7.56593851962773,134.981861182511));
#62706=CARTESIAN_POINT('Ctrl Pts',(78.4782549032977,7.6193155961037,134.97795500515));
#62707=CARTESIAN_POINT('Ctrl Pts',(78.4307943615623,7.67162504963916,134.974126957294));
#62708=CARTESIAN_POINT('Ctrl Pts',(78.3859782647129,7.72644623971398,134.970298909439));
#62709=CARTESIAN_POINT('Ctrl Pts',(78.3440811368766,7.78347614850676,134.966470861583));
#62710=CARTESIAN_POINT('Ctrl Pts',(78.3022091390411,7.84047185061926,134.9626451098));
#62711=CARTESIAN_POINT('Ctrl Pts',(78.2632529300739,7.89967324655135,134.958819358016));
#62712=CARTESIAN_POINT('Ctrl Pts',(78.2274466135476,7.96074447094278,134.954993606233));
#62713=CARTESIAN_POINT('Ctrl Pts',(78.1916493141244,8.0218003157704,134.951168817889));
#62714=CARTESIAN_POINT('Ctrl Pts',(78.1590005823019,8.08472462791576,134.947344029545));
#62715=CARTESIAN_POINT('Ctrl Pts',(78.1296900536076,8.14915438126208,134.9435192412));
#62716=CARTESIAN_POINT('Ctrl Pts',(78.0992961245191,8.2159656412982,134.939553077815));
#62717=CARTESIAN_POINT('Ctrl Pts',(78.0724922819993,8.28439531441747,134.93558691443));
#62718=CARTESIAN_POINT('Ctrl Pts',(78.0494357340078,8.35401501044195,134.931620751044));
#62719=CARTESIAN_POINT('Ctrl Pts',(78.0271754962613,8.42123023216181,134.927791568118));
#62720=CARTESIAN_POINT('Ctrl Pts',(78.0084080033321,8.48955410547027,134.923962385192));
#62721=CARTESIAN_POINT('Ctrl Pts',(77.9932234204897,8.55858712928934,134.920133202266));
#62722=CARTESIAN_POINT('Ctrl Pts',(77.9780288922086,8.62766536763404,134.916301511342));
#62723=CARTESIAN_POINT('Ctrl Pts',(77.9664220204801,8.69745319300213,134.912469820418));
#62724=CARTESIAN_POINT('Ctrl Pts',(77.9584413426124,8.76754395911139,134.908638129495));
#62725=CARTESIAN_POINT('Ctrl Pts',(77.9504482845426,8.83774345506282,134.904800494576));
#62726=CARTESIAN_POINT('Ctrl Pts',(77.9460926623442,8.90824633703059,134.900962859657));
#62727=CARTESIAN_POINT('Ctrl Pts',(77.9453609729324,8.97864511880522,134.897125224738));
#62728=CARTESIAN_POINT('Ctrl Pts',(77.9452847118622,8.98598250315872,134.896725243351));
#62729=CARTESIAN_POINT('Ctrl Pts',(77.9452477713803,8.9933187615579,134.896325261963));
#62730=CARTESIAN_POINT('Ctrl Pts',(77.9452501039006,9.00065343667963,134.895925280576));
#62731=CARTESIAN_POINT('Ctrl Pts',(77.9452501039008,9.00065343737377,134.895925280538));
#62732=CARTESIAN_POINT('Ctrl Pts',(77.9452615144079,9.03653405769225,134.893968604876));
#62733=CARTESIAN_POINT('Ctrl Pts',(77.9462127014812,9.07239853358728,134.892011929214));
#62734=CARTESIAN_POINT('Ctrl Pts',(77.9481014934011,9.10821312821006,134.890055253553));
#62735=CARTESIAN_POINT('Ctrl Pts',(77.9518363445886,9.17903203623747,134.886186170706));
#62736=CARTESIAN_POINT('Ctrl Pts',(77.9592491642671,9.24979606832758,134.882317087859));
#62737=CARTESIAN_POINT('Ctrl Pts',(77.9703354015929,9.32009245613253,134.878448005012));
#62738=CARTESIAN_POINT('Ctrl Pts',(77.981405120978,9.39028410582552,134.874584686905));
#62739=CARTESIAN_POINT('Ctrl Pts',(77.9961373187821,9.46000901835258,134.870721368799));
#62740=CARTESIAN_POINT('Ctrl Pts',(78.0144755138151,9.52885733166927,134.866858050692));
#62741=CARTESIAN_POINT('Ctrl Pts',(78.0327921981525,9.5976248859409,134.862999264257));
#62742=CARTESIAN_POINT('Ctrl Pts',(78.0547063534122,9.66551741631721,134.859140477821));
#62743=CARTESIAN_POINT('Ctrl Pts',(78.0801103699651,9.73213480383369,134.855281691385));
#62744=CARTESIAN_POINT('Ctrl Pts',(78.1054983838505,9.79871022728089,134.851425335702));
#62745=CARTESIAN_POINT('Ctrl Pts',(78.134371724842,9.86401164867024,134.847568980018));
#62746=CARTESIAN_POINT('Ctrl Pts',(78.1665732666698,9.92765509539378,134.843712624335));
#62747=CARTESIAN_POINT('Ctrl Pts',(78.1987652958396,9.99127974120586,134.839857407858));
#62748=CARTESIAN_POINT('Ctrl Pts',(78.2342833547566,10.0532469514842,134.836002191381));
#62749=CARTESIAN_POINT('Ctrl Pts',(78.2729233278854,10.1131952798756,134.832146974903));
#62750=CARTESIAN_POINT('Ctrl Pts',(78.3115648117215,10.1731459520675,134.828291607699));
#62751=CARTESIAN_POINT('Ctrl Pts',(78.353328187066,10.2310771785417,134.824436240494));
#62752=CARTESIAN_POINT('Ctrl Pts',(78.3979657153936,10.2866560198615,134.82058087329));
#62753=CARTESIAN_POINT('Ctrl Pts',(78.4426499670414,10.3422930370725,134.816721470567));
#62754=CARTESIAN_POINT('Ctrl Pts',(78.4902140724078,10.3955723742868,134.812862067844));
#62755=CARTESIAN_POINT('Ctrl Pts',(78.5403702200735,10.4461944779496,134.809002665121));
#62756=CARTESIAN_POINT('Ctrl Pts',(78.5905547665441,10.4968452442451,134.805141077174));
#62757=CARTESIAN_POINT('Ctrl Pts',(78.6433339173326,10.5448354549391,134.801279489227));
#62758=CARTESIAN_POINT('Ctrl Pts',(78.6983852719673,10.5899046079147,134.797417901281));
#62759=CARTESIAN_POINT('Ctrl Pts',(78.7535329409203,10.6350526109889,134.793549557347));
#62760=CARTESIAN_POINT('Ctrl Pts',(78.8109603589959,10.6772690652749,134.789681213414));
#62761=CARTESIAN_POINT('Ctrl Pts',(78.8703151273712,10.7163361124948,134.78581286948));
#62762=CARTESIAN_POINT('Ctrl Pts',(78.9055582807508,10.7395330008821,134.783515958174));
#62763=CARTESIAN_POINT('Ctrl Pts',(78.9414804390348,10.7616203802528,134.781219046867));
#62764=CARTESIAN_POINT('Ctrl Pts',(78.978004059442,10.7825604786326,134.778922135561));
#62765=CARTESIAN_POINT('Ctrl Pts',(79.0395270763863,10.8178334886212,134.775053052714));
#62766=CARTESIAN_POINT('Ctrl Pts',(79.1029988479684,10.8499867519932,134.771183969867));
#62767=CARTESIAN_POINT('Ctrl Pts',(79.1680701255576,10.8788002146344,134.76731488702));
#62768=CARTESIAN_POINT('Ctrl Pts',(79.2330444501884,10.9075707466532,134.763451568914));
#62769=CARTESIAN_POINT('Ctrl Pts',(79.2996131097051,10.9330111603523,134.759588250807));
#62770=CARTESIAN_POINT('Ctrl Pts',(79.3674011311609,10.9549466063408,134.755724932701));
#62771=CARTESIAN_POINT('Ctrl Pts',(79.4351096372937,10.9768563220596,134.751866146265));
#62772=CARTESIAN_POINT('Ctrl Pts',(79.504034204339,10.99526908772,134.74800735983));
#62773=CARTESIAN_POINT('Ctrl Pts',(79.5737803137746,11.0100582930786,134.744148573394));
#62774=CARTESIAN_POINT('Ctrl Pts',(79.6434824882756,11.0248381823222,134.740292217711));
#62775=CARTESIAN_POINT('Ctrl Pts',(79.7140047043384,11.0359989393333,134.736435862027));
#62776=CARTESIAN_POINT('Ctrl Pts',(79.7849391516778,11.0434643119024,134.732579506344));
#62777=CARTESIAN_POINT('Ctrl Pts',(79.8558526442711,11.0509274791258,134.728724289867));
#62778=CARTESIAN_POINT('Ctrl Pts',(79.9271776435275,11.0546973783256,134.72486907339));
#62779=CARTESIAN_POINT('Ctrl Pts',(79.9984997781607,11.0547494523261,134.721013856912));
#62780=CARTESIAN_POINT('Ctrl Pts',(80.0698247012759,11.0548015283625,134.717158489708));
#62781=CARTESIAN_POINT('Ctrl Pts',(80.1411462737611,11.0511354924629,134.713303122503));
#62782=CARTESIAN_POINT('Ctrl Pts',(80.2120504136818,11.0437788981584,134.709447755299));
#62783=CARTESIAN_POINT('Ctrl Pts',(80.2830287709023,11.0364146035056,134.705588352576));
#62784=CARTESIAN_POINT('Ctrl Pts',(80.3535883391529,11.0253520892534,134.701728949853));
#62785=CARTESIAN_POINT('Ctrl Pts',(80.423321350334,11.0106706833421,134.69786954713));
#62786=CARTESIAN_POINT('Ctrl Pts',(80.4930938448937,10.9959809647035,134.694007959183));
#62787=CARTESIAN_POINT('Ctrl Pts',(80.5620383810083,10.9776684001547,134.690146371236));
#62788=CARTESIAN_POINT('Ctrl Pts',(80.6297612385615,10.9558625577748,134.686284783289));
#62789=CARTESIAN_POINT('Ctrl Pts',(80.6976025796814,10.9340185652921,134.682416439356));
#62790=CARTESIAN_POINT('Ctrl Pts',(80.7642175207544,10.9086692657921,134.678548095423));
#62791=CARTESIAN_POINT('Ctrl Pts',(80.8292318976487,10.87999255914,134.674679751489));
#62792=CARTESIAN_POINT('Ctrl Pts',(80.8678355636976,10.8629651559738,134.672382840183));
#62793=CARTESIAN_POINT('Ctrl Pts',(80.9058753734192,10.8447655224717,134.670085928876));
#62794=CARTESIAN_POINT('Ctrl Pts',(80.9432775356499,10.8254383181138,134.66778901757));
#62795=CARTESIAN_POINT('Ctrl Pts',(81.0062654073906,10.7928899466669,134.663920857385));
#62796=CARTESIAN_POINT('Ctrl Pts',(81.0676899896179,10.757013862428,134.6600526972));
#62797=CARTESIAN_POINT('Ctrl Pts',(81.1271772473677,10.7179839974565,134.656184537015));
#62798=CARTESIAN_POINT('Ctrl Pts',(81.1698375602728,10.6899943688316,134.653410549272));
#62799=CARTESIAN_POINT('Ctrl Pts',(81.2115018532227,10.6603838573982,134.650636561529));
#62800=CARTESIAN_POINT('Ctrl Pts',(81.252039109102,10.6292316077768,134.647862573787));
#62801=CARTESIAN_POINT('',(77.9452502540764,8.99897817482853,134.954074719507));
#62802=CARTESIAN_POINT('Ctrl Pts',(77.9452502540759,8.99897817566031,134.954074719462));
#62803=CARTESIAN_POINT('Ctrl Pts',(77.9452142125462,9.07145278908982,134.950163294815));
#62804=CARTESIAN_POINT('Ctrl Pts',(77.9490169737962,9.14392164400065,134.946251870168));
#62805=CARTESIAN_POINT('Ctrl Pts',(77.9566303437358,9.21595835329659,134.942340445521));
#62806=CARTESIAN_POINT('Ctrl Pts',(77.9642467236715,9.28802354278169,134.938427474467));
#62807=CARTESIAN_POINT('Ctrl Pts',(77.9756766562268,9.35965578405013,134.934514503412));
#62808=CARTESIAN_POINT('Ctrl Pts',(77.9908402897156,9.43043561779875,134.930601532358));
#62809=CARTESIAN_POINT('Ctrl Pts',(78.0060265783599,9.50132119982606,134.926682715147));
#62810=CARTESIAN_POINT('Ctrl Pts',(78.0249576060861,9.57135137549333,134.922763897937));
#62811=CARTESIAN_POINT('Ctrl Pts',(78.0475028581238,9.64011910881129,134.918845080726));
#62812=CARTESIAN_POINT('Ctrl Pts',(78.0700662114441,9.7089420548265,134.914923117149));
#62813=CARTESIAN_POINT('Ctrl Pts',(78.0962493989038,9.77650010586642,134.911001153572));
#62814=CARTESIAN_POINT('Ctrl Pts',(78.125873680429,9.84240613767435,134.907079189996));
#62815=CARTESIAN_POINT('Ctrl Pts',(78.1555587274251,9.90844735625634,134.903149181668));
#62816=CARTESIAN_POINT('Ctrl Pts',(78.1886987529191,9.97282937301543,134.89921917334));
#62817=CARTESIAN_POINT('Ctrl Pts',(78.2250691444902,10.0351898476412,134.895289165013));
#62818=CARTESIAN_POINT('Ctrl Pts',(78.2479358387257,10.0743969566121,134.892818300805));
#62819=CARTESIAN_POINT('Ctrl Pts',(78.2720785667059,10.1128055448757,134.890347436597));
#62820=CARTESIAN_POINT('Ctrl Pts',(78.2974332054892,10.150332070634,134.887876572388));
#62821=CARTESIAN_POINT('Ctrl Pts',(78.3371355888425,10.209094197924,134.884007489541));
#62822=CARTESIAN_POINT('Ctrl Pts',(78.3799614657708,10.2659135819277,134.880138406695));
#62823=CARTESIAN_POINT('Ctrl Pts',(78.4256941852282,10.3204388528348,134.876269323848));
#62824=CARTESIAN_POINT('Ctrl Pts',(78.4713587652144,10.3748828838076,134.872406005741));
#62825=CARTESIAN_POINT('Ctrl Pts',(78.5199212810801,10.4270392173812,134.868542687635));
#62826=CARTESIAN_POINT('Ctrl Pts',(78.5711220788574,10.476585740474,134.864679369528));
#62827=CARTESIAN_POINT('Ctrl Pts',(78.6222628181186,10.5260741455143,134.860820583093));
#62828=CARTESIAN_POINT('Ctrl Pts',(78.6760353447626,10.5729584846901,134.856961796657));
#62829=CARTESIAN_POINT('Ctrl Pts',(78.7321412129297,10.6169513469949,134.853103010221));
#62830=CARTESIAN_POINT('Ctrl Pts',(78.7882117385139,10.6609164970222,134.849246654538));
#62831=CARTESIAN_POINT('Ctrl Pts',(78.846612308118,10.701993484806,134.845390298854));
#62832=CARTESIAN_POINT('Ctrl Pts',(78.9070103656069,10.7399342578412,134.841533943171));
#62833=CARTESIAN_POINT('Ctrl Pts',(78.9673905809049,10.7778638227921,134.837678726694));
#62834=CARTESIAN_POINT('Ctrl Pts',(79.0297667014886,10.8126587540296,134.833823510217));
#62835=CARTESIAN_POINT('Ctrl Pts',(79.0937775151041,10.8441145220319,134.82996829374));
#62836=CARTESIAN_POINT('Ctrl Pts',(79.1577908313509,10.8755715198607,134.826112926535));
#62837=CARTESIAN_POINT('Ctrl Pts',(79.2234385305612,10.9036888829903,134.82225755933));
#62838=CARTESIAN_POINT('Ctrl Pts',(79.2903367116241,10.9283089948531,134.818402192126));
#62839=CARTESIAN_POINT('Ctrl Pts',(79.3573049168402,10.9529548772595,134.814542789403));
#62840=CARTESIAN_POINT('Ctrl Pts',(79.4255257599696,10.9740960327627,134.81068338668));
#62841=CARTESIAN_POINT('Ctrl Pts',(79.4945982079864,10.9916241088944,134.806823983957));
#62842=CARTESIAN_POINT('Ctrl Pts',(79.5637097653658,11.0091621095605,134.80296239601));
#62843=CARTESIAN_POINT('Ctrl Pts',(79.6336734108459,11.0230828635466,134.799100808063));
#62844=CARTESIAN_POINT('Ctrl Pts',(79.7040785989502,11.0333293109825,134.795239220117));
#62845=CARTESIAN_POINT('Ctrl Pts',(79.7746069634547,11.0435936849456,134.791370876183));
#62846=CARTESIAN_POINT('Ctrl Pts',(79.8455779290275,11.0501708731723,134.78750253225));
#62847=CARTESIAN_POINT('Ctrl Pts',(79.9165772232863,11.0530558206794,134.783634188316));
#62848=CARTESIAN_POINT('Ctrl Pts',(79.9587345610352,11.0547688194875,134.78133727701));
#62849=CARTESIAN_POINT('Ctrl Pts',(80.0009018924252,11.0551810654193,134.779040365703));
#62850=CARTESIAN_POINT('Ctrl Pts',(80.0429932997398,11.0543001578828,134.776743454397));
#62851=CARTESIAN_POINT('Ctrl Pts',(80.1138837197785,11.0528165319065,134.772874992454));
#62852=CARTESIAN_POINT('Ctrl Pts',(80.1848360783879,11.0476562316637,134.769006530512));
#62853=CARTESIAN_POINT('Ctrl Pts',(80.2554378698445,11.0388106967419,134.765138068569));
#62854=CARTESIAN_POINT('Ctrl Pts',(80.3259407904934,11.0299775491147,134.761275024024));
#62855=CARTESIAN_POINT('Ctrl Pts',(80.3960936402557,11.0174694659644,134.757411979479));
#62856=CARTESIAN_POINT('Ctrl Pts',(80.4654850568478,11.0013298639533,134.753548934934));
#62857=CARTESIAN_POINT('Ctrl Pts',(80.5364815860529,10.9848169322131,134.749596533205));
#62858=CARTESIAN_POINT('Ctrl Pts',(80.6066804956812,10.9645023747784,134.745644131477));
#62859=CARTESIAN_POINT('Ctrl Pts',(80.675648519535,10.9404887633146,134.741691729748));
#62860=CARTESIAN_POINT('Ctrl Pts',(80.7429382613713,10.9170595039903,134.737835506573));
#62861=CARTESIAN_POINT('Ctrl Pts',(80.8090558645679,10.89010936257,134.733979283398));
#62862=CARTESIAN_POINT('Ctrl Pts',(80.8736130179299,10.8597843577693,134.730123060223));
#62863=CARTESIAN_POINT('Ctrl Pts',(80.9405853635626,10.8283248432607,134.726122569218));
#62864=CARTESIAN_POINT('Ctrl Pts',(81.0058776655747,10.793233114247,134.722122078213));
#62865=CARTESIAN_POINT('Ctrl Pts',(81.069080187921,10.754726506979,134.718121587208));
#62866=CARTESIAN_POINT('Ctrl Pts',(81.1322827102672,10.716219899711,134.714121096203));
#62867=CARTESIAN_POINT('Ctrl Pts',(81.1933949577799,10.6742987244623,134.710120605198));
#62868=CARTESIAN_POINT('Ctrl Pts',(81.252039109102,10.6292316077768,134.706120114193));
#62869=CARTESIAN_POINT('Ctrl Pts',(81.252039109102,10.6292316077768,135.406026966675));
#62870=CARTESIAN_POINT('Ctrl Pts',(81.3085478678901,10.5858055069868,135.402170997582));
#62871=CARTESIAN_POINT('Ctrl Pts',(81.3628300798522,10.5394088010384,135.398315028489));
#62872=CARTESIAN_POINT('Ctrl Pts',(81.4145642475669,10.4903038455313,135.394459059396));
#62873=CARTESIAN_POINT('Ctrl Pts',(81.466287232803,10.4412095041917,135.390603923781));
#62874=CARTESIAN_POINT('Ctrl Pts',(81.5154629153913,10.3894084102282,135.386748788166));
#62875=CARTESIAN_POINT('Ctrl Pts',(81.5618051096492,10.335201243998,135.382893652551));
#62876=CARTESIAN_POINT('Ctrl Pts',(81.6081527886018,10.2809876622372,135.379038060673));
#62877=CARTESIAN_POINT('Ctrl Pts',(81.6516659997839,10.2243678137742,135.375182468795));
#62878=CARTESIAN_POINT('Ctrl Pts',(81.6920985961299,10.1656757282689,135.371326876917));
#62879=CARTESIAN_POINT('Ctrl Pts',(81.7325754830453,10.1069193504322,135.367467061556));
#62880=CARTESIAN_POINT('Ctrl Pts',(81.7699647460227,10.0460866071276,135.363607246195));
#62881=CARTESIAN_POINT('Ctrl Pts',(81.8040639124926,9.98354001552652,135.359747430835));
#62882=CARTESIAN_POINT('Ctrl Pts',(81.8381848096327,9.9209535643191,135.355885155696));
#62883=CARTESIAN_POINT('Ctrl Pts',(81.8690112283502,9.85665152939536,135.352022880558));
#62884=CARTESIAN_POINT('Ctrl Pts',(81.8963881550408,9.79101803261434,135.348160605419));
#62885=CARTESIAN_POINT('Ctrl Pts',(81.923811028795,9.72527438225437,135.344291848172));
#62886=CARTESIAN_POINT('Ctrl Pts',(81.9477726962357,9.6581952681585,135.340423090926));
#62887=CARTESIAN_POINT('Ctrl Pts',(81.9681677224467,9.59018080180495,135.336554333679));
#62888=CARTESIAN_POINT('Ctrl Pts',(81.9754519982523,9.5658887942063,135.335172570571));
#62889=CARTESIAN_POINT('Ctrl Pts',(81.9822817780071,9.54147756623832,135.333790807462));
#62890=CARTESIAN_POINT('Ctrl Pts',(81.9886538483546,9.51696560226421,135.332409044354));
#62891=CARTESIAN_POINT('Ctrl Pts',(82.0064963192772,9.44832951059983,135.328539961507));
#62892=CARTESIAN_POINT('Ctrl Pts',(82.0208162221759,9.37863418425578,135.32467087866));
#62893=CARTESIAN_POINT('Ctrl Pts',(82.031493149485,9.30827446552624,135.320801795813));
#62894=CARTESIAN_POINT('Ctrl Pts',(82.0421541687049,9.23801957926842,135.316938477707));
#62895=CARTESIAN_POINT('Ctrl Pts',(82.0491829141827,9.16710274194419,135.313075159601));
#62896=CARTESIAN_POINT('Ctrl Pts',(82.0525093587264,9.09593171967852,135.309211841494));
#62897=CARTESIAN_POINT('Ctrl Pts',(82.0558319013519,9.02484418099479,135.305353055058));
#62898=CARTESIAN_POINT('Ctrl Pts',(82.0554607467397,8.95350353251239,135.301494268623));
#62899=CARTESIAN_POINT('Ctrl Pts',(82.0513775498521,8.88232370475398,135.297635482187));
#62900=CARTESIAN_POINT('Ctrl Pts',(82.0472969250791,8.81118871506761,135.293779126504));
#62901=CARTESIAN_POINT('Ctrl Pts',(82.0395089249652,8.74021482895654,135.28992277082));
#62902=CARTESIAN_POINT('Ctrl Pts',(82.0280472853771,8.66981555037436,135.286066415137));
#62903=CARTESIAN_POINT('Ctrl Pts',(82.0165890316721,8.599437068444,135.28221119866));
#62904=CARTESIAN_POINT('Ctrl Pts',(82.0014593709949,8.52963333626083,135.278355982183));
#62905=CARTESIAN_POINT('Ctrl Pts',(81.9827436390369,8.4608105858246,135.274500765705));
#62906=CARTESIAN_POINT('Ctrl Pts',(81.9640271753497,8.39198514462455,135.270645398501));
#62907=CARTESIAN_POINT('Ctrl Pts',(81.9417244916244,8.32414122949848,135.266790031296));
#62908=CARTESIAN_POINT('Ctrl Pts',(81.9159711219687,8.25767108214607,135.262934664091));
#62909=CARTESIAN_POINT('Ctrl Pts',(81.8901907955576,8.19113135867504,135.259075261369));
#62910=CARTESIAN_POINT('Ctrl Pts',(81.8609527488607,8.12596872736965,135.255215858646));
#62911=CARTESIAN_POINT('Ctrl Pts',(81.8284408048184,8.062555715909,135.251356455923));
#62912=CARTESIAN_POINT('Ctrl Pts',(81.7959104522581,7.99910679950317,135.247494867976));
#62913=CARTESIAN_POINT('Ctrl Pts',(81.7601027561561,7.93740989536472,135.243633280029));
#62914=CARTESIAN_POINT('Ctrl Pts',(81.7212463131001,7.87781075921244,135.239771692082));
#62915=CARTESIAN_POINT('Ctrl Pts',(81.6823218893042,7.81810735223518,135.235903348149));
#62916=CARTESIAN_POINT('Ctrl Pts',(81.6403383555219,7.76050943343201,135.232035004216));
#62917=CARTESIAN_POINT('Ctrl Pts',(81.5955657916367,7.70533117475602,135.228166660282));
#62918=CARTESIAN_POINT('Ctrl Pts',(81.5689811316442,7.6725679126466,135.225869748976));
#62919=CARTESIAN_POINT('Ctrl Pts',(81.5414139051121,7.6406570711572,135.223572837669));
#62920=CARTESIAN_POINT('Ctrl Pts',(81.5129266135235,7.60965809075886,135.221275926363));
#62921=CARTESIAN_POINT('Ctrl Pts',(81.4649405676832,7.55744117537499,135.217406843516));
#62922=CARTESIAN_POINT('Ctrl Pts',(81.4141540521789,7.50760917786172,135.213537760669));
#62923=CARTESIAN_POINT('Ctrl Pts',(81.3608334803881,7.46047741128786,135.209668677822));
#62924=CARTESIAN_POINT('Ctrl Pts',(81.3075923535901,7.41341586869575,135.205805359716));
#62925=CARTESIAN_POINT('Ctrl Pts',(81.2518250260103,7.36904689019028,135.201942041609));
#62926=CARTESIAN_POINT('Ctrl Pts',(81.1938360940872,7.32765047225327,135.198078723503));
#62927=CARTESIAN_POINT('Ctrl Pts',(81.1359151831588,7.28630261229848,135.194219937067));
#62928=CARTESIAN_POINT('Ctrl Pts',(81.0757782376257,7.24792066779854,135.190361150631));
#62929=CARTESIAN_POINT('Ctrl Pts',(81.0137630642245,7.21274455879579,135.186502364195));
#62930=CARTESIAN_POINT('Ctrl Pts',(80.9517869558352,7.17759060816235,135.182646008512));
#62931=CARTESIAN_POINT('Ctrl Pts',(80.887935388464,7.14563872559304,135.178789652829));
#62932=CARTESIAN_POINT('Ctrl Pts',(80.8225740581302,7.11708484487717,135.174933297146));
#62933=CARTESIAN_POINT('Ctrl Pts',(80.7572320361878,7.08853939926357,135.171078080668));
#62934=CARTESIAN_POINT('Ctrl Pts',(80.6903815816303,7.06339015704093,135.167222864191));
#62935=CARTESIAN_POINT('Ctrl Pts',(80.6224102677975,7.04178575711436,135.163367647714));
#62936=CARTESIAN_POINT('Ctrl Pts',(80.5544362964897,7.02018051252036,135.159512280509));
#62937=CARTESIAN_POINT('Ctrl Pts',(80.4853418425306,7.00212053043067,135.155656913305));
#62938=CARTESIAN_POINT('Ctrl Pts',(80.4155299521795,6.98770468833681,135.1518015461));
#62939=CARTESIAN_POINT('Ctrl Pts',(80.3456449878162,6.97327375678731,135.147942143377));
#62940=CARTESIAN_POINT('Ctrl Pts',(80.2750415646964,6.96249467811315,135.144082740654));
#62941=CARTESIAN_POINT('Ctrl Pts',(80.2041323575912,6.95541506826343,135.140223337932));
#62942=CARTESIAN_POINT('Ctrl Pts',(80.133183001136,6.948331449883,135.136361749985));
#62943=CARTESIAN_POINT('Ctrl Pts',(80.0619280014996,6.94495149319357,135.132500162038));
#62944=CARTESIAN_POINT('Ctrl Pts',(79.9907818257887,6.94527067773777,135.128638574091));
#62945=CARTESIAN_POINT('Ctrl Pts',(79.9195111772933,6.94559042070676,135.124770230157));
#62946=CARTESIAN_POINT('Ctrl Pts',(79.8483502180037,6.94962219851369,135.120901886224));
#62947=CARTESIAN_POINT('Ctrl Pts',(79.7777093801836,6.95730950879933,135.117033542291));
#62948=CARTESIAN_POINT('Ctrl Pts',(79.7357648835524,6.9618740124254,135.114736630984));
#62949=CARTESIAN_POINT('Ctrl Pts',(79.694003608926,6.96772633887129,135.112439719678));
#62950=CARTESIAN_POINT('Ctrl Pts',(79.6525093937844,6.97484621791531,135.110142808371));
#62951=CARTESIAN_POINT('Ctrl Pts',(79.5826135490466,6.98683945500908,135.106273725524));
#62952=CARTESIAN_POINT('Ctrl Pts',(79.5132024330664,7.00247899181911,135.102404642677));
#62953=CARTESIAN_POINT('Ctrl Pts',(79.4446854481558,7.02171202525768,135.098535559831));
#62954=CARTESIAN_POINT('Ctrl Pts',(79.3762705501358,7.04091640243557,135.094672241724));
#62955=CARTESIAN_POINT('Ctrl Pts',(79.3087476026799,7.06370351822278,135.090808923618));
#62956=CARTESIAN_POINT('Ctrl Pts',(79.242517047208,7.08996933565726,135.086945605511));
#62957=CARTESIAN_POINT('Ctrl Pts',(79.1763641801522,7.116204343298,135.083086819076));
#62958=CARTESIAN_POINT('Ctrl Pts',(79.1115011432173,7.14590976908554,135.07922803264));
#62959=CARTESIAN_POINT('Ctrl Pts',(79.0483127208929,7.17893193831597,135.075369246204));
#62960=CARTESIAN_POINT('Ctrl Pts',(78.985164102641,7.21193330600122,135.071512890521));
#62961=CARTESIAN_POINT('Ctrl Pts',(78.9236884356438,7.24824704751499,135.067656534837));
#62962=CARTESIAN_POINT('Ctrl Pts',(78.8642486766827,7.28767220016641,135.063800179154));
#62963=CARTESIAN_POINT('Ctrl Pts',(78.8048264768215,7.32708570623301,135.059944962677));
#62964=CARTESIAN_POINT('Ctrl Pts',(78.747439395603,7.36960853031767,135.0560897462));
#62965=CARTESIAN_POINT('Ctrl Pts',(78.69242252164,7.41499567805454,135.052234529723));
#62966=CARTESIAN_POINT('Ctrl Pts',(78.6374034966817,7.46038460029324,135.048379162518));
#62967=CARTESIAN_POINT('Ctrl Pts',(78.5847552362834,7.50863775768248,135.044523795313));
#62968=CARTESIAN_POINT('Ctrl Pts',(78.5347794150553,7.5594701669336,135.040668428109));
#62969=CARTESIAN_POINT('Ctrl Pts',(78.4847512827704,7.61035578385566,135.036809025386));
#62970=CARTESIAN_POINT('Ctrl Pts',(78.4374015149906,7.66382569487572,135.032949622663));
#62971=CARTESIAN_POINT('Ctrl Pts',(78.3929939421244,7.71955902422212,135.029090219941));
#62972=CARTESIAN_POINT('Ctrl Pts',(78.3485612253415,7.77532391021734,135.025228631994));
#62973=CARTESIAN_POINT('Ctrl Pts',(78.3070743024075,7.83335437037287,135.021367044047));
#62974=CARTESIAN_POINT('Ctrl Pts',(78.2687541743386,7.89329974535568,135.0175054561));
#62975=CARTESIAN_POINT('Ctrl Pts',(78.2303670038319,7.95334999692082,135.013637112166));
#62976=CARTESIAN_POINT('Ctrl Pts',(78.1951579298448,8.01532142959978,135.009768768233));
#62977=CARTESIAN_POINT('Ctrl Pts',(78.1633020932589,8.07883857990415,135.005900424299));
#62978=CARTESIAN_POINT('Ctrl Pts',(78.1443870142257,8.11655323588991,135.003603512993));
#62979=CARTESIAN_POINT('Ctrl Pts',(78.1266532537511,8.15481245076237,135.001306601687));
#62980=CARTESIAN_POINT('Ctrl Pts',(78.1101292539508,8.19353479571181,134.99900969038));
#62981=CARTESIAN_POINT('Ctrl Pts',(78.0793053040282,8.26576764708191,134.994725020812));
#62982=CARTESIAN_POINT('Ctrl Pts',(78.0525904917818,8.33985380574526,134.990440351244));
#62983=CARTESIAN_POINT('Ctrl Pts',(78.0301869119697,8.41533431713122,134.986155681676));
#62984=CARTESIAN_POINT('Ctrl Pts',(78.007854285939,8.49057577619793,134.981884581971));
#62985=CARTESIAN_POINT('Ctrl Pts',(77.9898057879733,8.56720250551917,134.977613482266));
#62986=CARTESIAN_POINT('Ctrl Pts',(77.9761951891261,8.64473720996497,134.973342382561));
#62987=CARTESIAN_POINT('Ctrl Pts',(77.9626561574421,8.72186422192664,134.969093741125));
#62988=CARTESIAN_POINT('Ctrl Pts',(77.9535086041256,8.79988940239672,134.964845099689));
#62989=CARTESIAN_POINT('Ctrl Pts',(77.9488557708438,8.87832455589048,134.960596458253));
#62990=CARTESIAN_POINT('Ctrl Pts',(77.9464750440831,8.9184576656747,134.958422545337));
#62991=CARTESIAN_POINT('Ctrl Pts',(77.9452702854505,8.95869783904917,134.956248632422));
#62992=CARTESIAN_POINT('Ctrl Pts',(77.9452502540763,8.99897817482853,134.954074719507));
#62993=CARTESIAN_POINT('Origin',(80.,9.,141.545925280538));
#62994=CARTESIAN_POINT('',(81.252039109102,10.6292316077768,136.106053391442));
#62995=CARTESIAN_POINT('',(81.252039109102,10.6292316077768,136.047954616544));
#62996=CARTESIAN_POINT('',(81.252039109102,10.6292316077768,141.545925280538));
#62997=CARTESIAN_POINT('',(77.9452505223076,9.00146506745653,135.595925280489));
#62998=CARTESIAN_POINT('Ctrl Pts',(81.252039109102,10.6292316077768,136.047954616544));
#62999=CARTESIAN_POINT('Ctrl Pts',(81.3089518203792,10.5854950757921,136.044073934621));
#63000=CARTESIAN_POINT('Ctrl Pts',(81.3635519286423,10.5387868553141,136.040193252698));
#63001=CARTESIAN_POINT('Ctrl Pts',(81.4155258477759,10.4893905252748,136.036312570775));
#63002=CARTESIAN_POINT('Ctrl Pts',(81.4672299052006,10.4402506734511,136.032452038332));
#63003=CARTESIAN_POINT('Ctrl Pts',(81.5163346813592,10.3884509528018,136.02859150589));
#63004=CARTESIAN_POINT('Ctrl Pts',(81.5625698786793,10.3343061630466,136.024730973447));
#63005=CARTESIAN_POINT('Ctrl Pts',(81.6091670526988,10.2797374721637,136.020840216784));
#63006=CARTESIAN_POINT('Ctrl Pts',(81.6528492120465,10.2227872289702,136.016949460121));
#63007=CARTESIAN_POINT('Ctrl Pts',(81.6933836043985,10.1638082019192,136.013058703458));
#63008=CARTESIAN_POINT('Ctrl Pts',(81.7339179967505,10.1048291748683,136.009167946794));
#63009=CARTESIAN_POINT('Ctrl Pts',(81.771304416678,10.043821822193,136.005277190131));
#63010=CARTESIAN_POINT('Ctrl Pts',(81.8053578201978,9.98116293425242,136.001386433468));
#63011=CARTESIAN_POINT('Ctrl Pts',(81.8392215261156,9.91885309338356,135.997517350621));
#63012=CARTESIAN_POINT('Ctrl Pts',(81.8699219428302,9.85466600319565,135.993648267774));
#63013=CARTESIAN_POINT('Ctrl Pts',(81.8972470215781,9.78895582995059,135.989779184927));
#63014=CARTESIAN_POINT('Ctrl Pts',(81.9245313873213,9.7233435615867,135.985915866821));
#63015=CARTESIAN_POINT('Ctrl Pts',(81.9484502126878,9.65621315959098,135.982052548715));
#63016=CARTESIAN_POINT('Ctrl Pts',(81.9688372273746,9.58794347908959,135.978189230608));
#63017=CARTESIAN_POINT('Ctrl Pts',(81.989200328101,9.51975387889703,135.974330444172));
#63018=CARTESIAN_POINT('Ctrl Pts',(82.0060397088494,9.4504281179012,135.970471657737));
#63019=CARTESIAN_POINT('Ctrl Pts',(82.019237770797,9.38036349389328,135.966612871301));
#63020=CARTESIAN_POINT('Ctrl Pts',(82.0324275189334,9.31034300546086,135.962756515618));
#63021=CARTESIAN_POINT('Ctrl Pts',(82.0419804093478,9.23958505368009,135.958900159934));
#63022=CARTESIAN_POINT('Ctrl Pts',(82.047829490708,9.16849907859232,135.955043804251));
#63023=CARTESIAN_POINT('Ctrl Pts',(82.0536768441911,9.09743410301335,135.951188587774));
#63024=CARTESIAN_POINT('Ctrl Pts',(82.0558225209815,9.02604178038674,135.947333371297));
#63025=CARTESIAN_POINT('Ctrl Pts',(82.0542514007093,8.9547369335569,135.943478154819));
#63026=CARTESIAN_POINT('Ctrl Pts',(82.052680219011,8.88342929892084,135.939622787615));
#63027=CARTESIAN_POINT('Ctrl Pts',(82.0473919646486,8.81220963248827,135.93576742041));
#63028=CARTESIAN_POINT('Ctrl Pts',(82.0384236078769,8.74149128186784,135.931912053206));
#63029=CARTESIAN_POINT('Ctrl Pts',(82.0294458636812,8.67069890841833,135.928052650483));
#63030=CARTESIAN_POINT('Ctrl Pts',(82.0167803887356,8.60040938119204,135.92419324776));
#63031=CARTESIAN_POINT('Ctrl Pts',(82.0005157706016,8.53102855729332,135.920333845037));
#63032=CARTESIAN_POINT('Ctrl Pts',(81.984241943313,8.46160844942698,135.91647225709));
#63033=CARTESIAN_POINT('Ctrl Pts',(81.964365051502,8.39309853589352,135.912610669143));
#63034=CARTESIAN_POINT('Ctrl Pts',(81.9410235901458,8.32588948606509,135.908749081196));
#63035=CARTESIAN_POINT('Ctrl Pts',(81.9176412920663,8.25856285159507,135.904880737263));
#63036=CARTESIAN_POINT('Ctrl Pts',(81.8907825058248,8.19254207485823,135.90101239333));
#63037=CARTESIAN_POINT('Ctrl Pts',(81.8606336006024,8.12819717435119,135.897144049396));
#63038=CARTESIAN_POINT('Ctrl Pts',(81.8427320482914,8.08999102411536,135.89484713809));
#63039=CARTESIAN_POINT('Ctrl Pts',(81.8236714017528,8.05237526230223,135.892550226783));
#63040=CARTESIAN_POINT('Ctrl Pts',(81.8034979882716,8.01542264458276,135.890253315477));
#63041=CARTESIAN_POINT('Ctrl Pts',(81.7695164375492,7.95317699366571,135.88638423263));
#63042=CARTESIAN_POINT('Ctrl Pts',(81.7322420417679,7.89257074355593,135.882515149783));
#63043=CARTESIAN_POINT('Ctrl Pts',(81.691857336643,7.83397413624427,135.878646066936));
#63044=CARTESIAN_POINT('Ctrl Pts',(81.6515328027146,7.77546483495515,135.87478274883));
#63045=CARTESIAN_POINT('Ctrl Pts',(81.6081074316386,7.71895962965557,135.870919430723));
#63046=CARTESIAN_POINT('Ctrl Pts',(81.5618093303979,7.66480369309158,135.867056112617));
#63047=CARTESIAN_POINT('Ctrl Pts',(81.5155655368122,7.61071128142028,135.863197326181));
#63048=CARTESIAN_POINT('Ctrl Pts',(81.466456020584,7.55896303219886,135.859338539745));
#63049=CARTESIAN_POINT('Ctrl Pts',(81.4147507814424,7.50987323059139,135.855479753309));
#63050=CARTESIAN_POINT('Ctrl Pts',(81.3630781128102,7.46081435195943,135.851623397626));
#63051=CARTESIAN_POINT('Ctrl Pts',(81.3088133167696,7.41441093219164,135.847767041943));
#63052=CARTESIAN_POINT('Ctrl Pts',(81.252264064358,7.37094129153745,135.84391068626));
#63053=CARTESIAN_POINT('Ctrl Pts',(81.1957315171616,7.32748449225032,135.840055469782));
#63054=CARTESIAN_POINT('Ctrl Pts',(81.1369162382928,7.28696004739923,135.836200253305));
#63055=CARTESIAN_POINT('Ctrl Pts',(81.0761585331535,7.24960565185417,135.832345036828));
#63056=CARTESIAN_POINT('Ctrl Pts',(81.0153984525697,7.212249795864,135.828489669623));
#63057=CARTESIAN_POINT('Ctrl Pts',(80.9526962099217,7.17806448779367,135.824634302419));
#63058=CARTESIAN_POINT('Ctrl Pts',(80.8884191241467,7.14724285931739,135.820778935214));
#63059=CARTESIAN_POINT('Ctrl Pts',(80.8240747577905,7.11638896900076,135.816919532491));
#63060=CARTESIAN_POINT('Ctrl Pts',(80.7581526965945,7.08890599716434,135.813060129768));
#63061=CARTESIAN_POINT('Ctrl Pts',(80.6910419626868,7.06493964737377,135.809200727046));
#63062=CARTESIAN_POINT('Ctrl Pts',(80.6238932301544,7.04095972764768,135.805339139099));
#63063=CARTESIAN_POINT('Ctrl Pts',(80.5555549506989,7.02050053310161,135.801477551152));
#63064=CARTESIAN_POINT('Ctrl Pts',(80.4864304555323,7.00365760090344,135.797615963205));
#63065=CARTESIAN_POINT('Ctrl Pts',(80.4171850245838,6.98678520139167,135.793747619271));
#63066=CARTESIAN_POINT('Ctrl Pts',(80.3471511091492,6.97354178611454,135.789879275338));
#63067=CARTESIAN_POINT('Ctrl Pts',(80.2767406569831,6.96397147090897,135.786010931404));
#63068=CARTESIAN_POINT('Ctrl Pts',(80.2349329567233,6.95828889314961,135.783714020098));
#63069=CARTESIAN_POINT('Ctrl Pts',(80.1929925914078,6.95390032385284,135.781417108791));
#63070=CARTESIAN_POINT('Ctrl Pts',(80.15100581249,6.95080630317819,135.779120197485));
#63071=CARTESIAN_POINT('Ctrl Pts',(80.0802802578494,6.94559451189713,135.775251114638));
#63072=CARTESIAN_POINT('Ctrl Pts',(80.0091460436972,6.94403832740463,135.771382031791));
#63073=CARTESIAN_POINT('Ctrl Pts',(79.9380132263564,6.94618520737792,135.767512948944));
#63074=CARTESIAN_POINT('Ctrl Pts',(79.8669863933657,6.94832888860713,135.763649630838));
#63075=CARTESIAN_POINT('Ctrl Pts',(79.7959614346618,6.9541646679172,135.759786312731));
#63076=CARTESIAN_POINT('Ctrl Pts',(79.7253520620245,6.963688119991,135.755922994625));
#63077=CARTESIAN_POINT('Ctrl Pts',(79.6548255141543,6.97320040105916,135.752064208189));
#63078=CARTESIAN_POINT('Ctrl Pts',(79.5847140631333,6.98639169809088,135.748205421753));
#63079=CARTESIAN_POINT('Ctrl Pts',(79.5154281928634,7.00320563747082,135.744346635317));
#63080=CARTESIAN_POINT('Ctrl Pts',(79.4461859676111,7.02000898530186,135.740490279634));
#63081=CARTESIAN_POINT('Ctrl Pts',(79.3777687622934,7.04043033373929,135.736633923951));
#63082=CARTESIAN_POINT('Ctrl Pts',(79.3105772776738,7.06436215359373,135.732777568268));
#63083=CARTESIAN_POINT('Ctrl Pts',(79.2434056420915,7.08828690374894,135.72892235179));
#63084=CARTESIAN_POINT('Ctrl Pts',(79.1774594657311,7.11571990362766,135.725067135313));
#63085=CARTESIAN_POINT('Ctrl Pts',(79.1131230188681,7.14650417242486,135.721211918836));
#63086=CARTESIAN_POINT('Ctrl Pts',(79.0487840566424,7.17728964479496,135.717356551631));
#63087=CARTESIAN_POINT('Ctrl Pts',(78.9860553861163,7.2114264345535,135.713501184427));
#63088=CARTESIAN_POINT('Ctrl Pts',(78.9252984901607,7.2487106957304,135.709645817222));
#63089=CARTESIAN_POINT('Ctrl Pts',(78.8644779983027,7.28603398336174,135.705786414499));
#63090=CARTESIAN_POINT('Ctrl Pts',(78.8056338159299,7.32651106445915,135.701927011776));
#63091=CARTESIAN_POINT('Ctrl Pts',(78.7490993513736,7.36989413541142,135.698067609054));
#63092=CARTESIAN_POINT('Ctrl Pts',(78.6925328765594,7.41330177019929,135.694206021107));
#63093=CARTESIAN_POINT('Ctrl Pts',(78.6382790925854,7.4596183547552,135.69034443316));
#63094=CARTESIAN_POINT('Ctrl Pts',(78.5866370222985,7.50855685466637,135.686482845213));
#63095=CARTESIAN_POINT('Ctrl Pts',(78.5349046023586,7.55758097423724,135.682614501279));
#63096=CARTESIAN_POINT('Ctrl Pts',(78.4857933536446,7.60923581533726,135.678746157346));
#63097=CARTESIAN_POINT('Ctrl Pts',(78.4395637716856,7.6631992145933,135.674877813413));
#63098=CARTESIAN_POINT('Ctrl Pts',(78.4121139762903,7.69524112813968,135.672580902106));
#63099=CARTESIAN_POINT('Ctrl Pts',(78.3856793652917,7.72809634271189,135.6702839908));
#63100=CARTESIAN_POINT('Ctrl Pts',(78.3603071735869,7.76169268858276,135.667987079493));
#63101=CARTESIAN_POINT('Ctrl Pts',(78.3174433117299,7.81845046280503,135.664106670182));
#63102=CARTESIAN_POINT('Ctrl Pts',(78.2774445565978,7.87754940196065,135.660226260871));
#63103=CARTESIAN_POINT('Ctrl Pts',(78.240575222393,7.93866969588037,135.65634585156));
#63104=CARTESIAN_POINT('Ctrl Pts',(78.203760818831,7.99969892829601,135.652471223568));
#63105=CARTESIAN_POINT('Ctrl Pts',(78.1700668305628,8.06274313086389,135.648596595576));
#63106=CARTESIAN_POINT('Ctrl Pts',(78.1397161676285,8.12745107557382,135.644721967583));
#63107=CARTESIAN_POINT('Ctrl Pts',(78.1078633935518,8.19536153763767,135.640655576996));
#63108=CARTESIAN_POINT('Ctrl Pts',(78.07969379902,8.26510427275798,135.636589186409));
#63109=CARTESIAN_POINT('Ctrl Pts',(78.055412144488,8.3362412827726,135.632522795822));
#63110=CARTESIAN_POINT('Ctrl Pts',(78.0323224526798,8.40388624639017,135.62865602038));
#63111=CARTESIAN_POINT('Ctrl Pts',(78.0127481522003,8.4727913054781,135.624789244939));
#63112=CARTESIAN_POINT('Ctrl Pts',(77.9968162204211,8.54255895709712,135.620922469497));
#63113=CARTESIAN_POINT('Ctrl Pts',(77.9808915414104,8.61229484805866,135.617057454346));
#63114=CARTESIAN_POINT('Ctrl Pts',(77.9686060422558,8.68289208198892,135.613192439195));
#63115=CARTESIAN_POINT('Ctrl Pts',(77.9600362376921,8.75394022886587,135.609327424043));
#63116=CARTESIAN_POINT('Ctrl Pts',(77.9514663540313,8.82498903149886,135.605462373219));
#63117=CARTESIAN_POINT('Ctrl Pts',(77.9466122932739,8.89648827757465,135.601597322395));
#63118=CARTESIAN_POINT('Ctrl Pts',(77.945498864882,8.96802112730593,135.59773227157));
#63119=CARTESIAN_POINT('Ctrl Pts',(77.9453253479641,8.97916882185064,135.597129941226));
#63120=CARTESIAN_POINT('Ctrl Pts',(77.9452425738058,8.99031732822184,135.596527610882));
#63121=CARTESIAN_POINT('Ctrl Pts',(77.9452505223069,9.00146506654286,135.595925280538));
#63122=CARTESIAN_POINT('Ctrl Pts',(77.9452505223076,9.00146506745653,135.595925280489));
#63123=CARTESIAN_POINT('Ctrl Pts',(77.9453088390013,9.08325392669816,135.591506096049));
#63124=CARTESIAN_POINT('Ctrl Pts',(77.9502545524832,9.1648475422697,135.587086911609));
#63125=CARTESIAN_POINT('Ctrl Pts',(77.9599940449638,9.24570971880849,135.582667727169));
#63126=CARTESIAN_POINT('Ctrl Pts',(77.9698223745248,9.32730946557315,135.57820823391));
#63127=CARTESIAN_POINT('Ctrl Pts',(77.9845322237858,9.40816418156723,135.573748740651));
#63128=CARTESIAN_POINT('Ctrl Pts',(78.0039776882024,9.48774224064146,135.569289247391));
#63129=CARTESIAN_POINT('Ctrl Pts',(78.0220522312963,9.56170998074051,135.565144152095));
#63130=CARTESIAN_POINT('Ctrl Pts',(78.0442176079849,9.63457482938802,135.560999056799));
#63131=CARTESIAN_POINT('Ctrl Pts',(78.0703199470976,9.70592666469722,135.556853961502));
#63132=CARTESIAN_POINT('Ctrl Pts',(78.0946841909335,9.77252734389711,135.552984878655));
#63133=CARTESIAN_POINT('Ctrl Pts',(78.1225481710408,9.83799563198995,135.549115795808));
#63134=CARTESIAN_POINT('Ctrl Pts',(78.153786339128,9.9019382910762,135.545246712961));
#63135=CARTESIAN_POINT('Ctrl Pts',(78.1849779639026,9.96578567878933,135.541383394855));
#63136=CARTESIAN_POINT('Ctrl Pts',(78.2195335859642,10.0281115166334,135.537520076748));
#63137=CARTESIAN_POINT('Ctrl Pts',(78.2572788690437,10.0885405928207,135.533656758642));
#63138=CARTESIAN_POINT('Ctrl Pts',(78.2949798769207,10.148898785725,135.529797972206));
#63139=CARTESIAN_POINT('Ctrl Pts',(78.3358628578837,10.2073642263649,135.52593918577));
#63140=CARTESIAN_POINT('Ctrl Pts',(78.3797074616772,10.2635860290283,135.522080399335));
#63141=CARTESIAN_POINT('Ctrl Pts',(78.4235244465854,10.3197724160787,135.518224043651));
#63142=CARTESIAN_POINT('Ctrl Pts',(78.4702990549621,10.3737175870088,135.514367687968));
#63143=CARTESIAN_POINT('Ctrl Pts',(78.5197683434639,10.4251006299516,135.510511332285));
#63144=CARTESIAN_POINT('Ctrl Pts',(78.5692230182425,10.476468493829,135.506656115807));
#63145=CARTESIAN_POINT('Ctrl Pts',(78.6213704560565,10.5252753825675,135.50280089933));
#63146=CARTESIAN_POINT('Ctrl Pts',(78.6759094097278,10.571235714733,135.498945682853));
#63147=CARTESIAN_POINT('Ctrl Pts',(78.7304504957091,10.6171978438101,135.495090315648));
#63148=CARTESIAN_POINT('Ctrl Pts',(78.7873829102914,10.6603128840023,135.491234948444));
#63149=CARTESIAN_POINT('Ctrl Pts',(78.8463720764135,10.7003353129373,135.487379581239));
#63150=CARTESIAN_POINT('Ctrl Pts',(78.9054229881071,10.7403996344418,135.483520178516));
#63151=CARTESIAN_POINT('Ctrl Pts',(78.9665345461115,10.7773646093717,135.479660775793));
#63152=CARTESIAN_POINT('Ctrl Pts',(79.0293436696688,10.8110283959364,135.475801373071));
#63153=CARTESIAN_POINT('Ctrl Pts',(79.0921883562452,10.8447112432015,135.471939785124));
#63154=CARTESIAN_POINT('Ctrl Pts',(79.1567320820348,10.8750889742164,135.468078197177));
#63155=CARTESIAN_POINT('Ctrl Pts',(79.2225901682393,10.90200723342,135.46421660923));
#63156=CARTESIAN_POINT('Ctrl Pts',(79.2885634755262,10.9289725870829,135.460348265296));
#63157=CARTESIAN_POINT('Ctrl Pts',(79.3558552755063,10.9524662248332,135.456479921363));
#63158=CARTESIAN_POINT('Ctrl Pts',(79.4240647345005,10.9723833634601,135.45261157743));
#63159=CARTESIAN_POINT('Ctrl Pts',(79.464565548354,10.9842095872114,135.450314666123));
#63160=CARTESIAN_POINT('Ctrl Pts',(79.505389660854,10.9947758363981,135.448017754817));
#63161=CARTESIAN_POINT('Ctrl Pts',(79.5464518564914,11.004068772278,135.44572084351));
#63162=CARTESIAN_POINT('Ctrl Pts',(79.6192550065553,11.0205451198015,135.441648426633));
#63163=CARTESIAN_POINT('Ctrl Pts',(79.6931072766589,11.0330831288442,135.437576009756));
#63164=CARTESIAN_POINT('Ctrl Pts',(79.7675435324096,11.0415586088025,135.433503592879));
#63165=CARTESIAN_POINT('Ctrl Pts',(79.8381398310474,11.0495968625834,135.429641260536));
#63166=CARTESIAN_POINT('Ctrl Pts',(79.909260795605,11.053981240602,135.425778928194));
#63167=CARTESIAN_POINT('Ctrl Pts',(79.9804964623781,11.0546574348344,135.421916595851));
#63168=CARTESIAN_POINT('Ctrl Pts',(80.0516622917356,11.0553329661452,135.418058050029));
#63169=CARTESIAN_POINT('Ctrl Pts',(80.1229421170099,11.0523075215454,135.414199504207));
#63170=CARTESIAN_POINT('Ctrl Pts',(80.1939215984958,11.0455786409075,135.410340958385));
#63171=CARTESIAN_POINT('Ctrl Pts',(80.2648552395298,11.038854105961,135.406484904516));
#63172=CARTESIAN_POINT('Ctrl Pts',(80.3354884393489,11.0284309281795,135.402628850646));
#63173=CARTESIAN_POINT('Ctrl Pts',(80.4054093391821,11.0143586647377,135.398772796776));
#63174=CARTESIAN_POINT('Ctrl Pts',(80.4753084720615,11.0002907821078,135.394917943328));
#63175=CARTESIAN_POINT('Ctrl Pts',(80.544495269775,10.9825761669819,135.39106308988));
#63176=CARTESIAN_POINT('Ctrl Pts',(80.6125671728234,10.9613156353018,135.387208236432));
#63177=CARTESIAN_POINT('Ctrl Pts',(80.6806707823523,10.940045200907,135.383351587473));
#63178=CARTESIAN_POINT('Ctrl Pts',(80.7476579947613,10.9152256926984,135.379494938514));
#63179=CARTESIAN_POINT('Ctrl Pts',(80.8131416936283,10.8870077235092,135.375638289555));
#63180=CARTESIAN_POINT('Ctrl Pts',(80.8786429814658,10.8587821749523,135.371780604697));
#63181=CARTESIAN_POINT('Ctrl Pts',(80.9426395124891,10.8271565562098,135.367922919839));
#63182=CARTESIAN_POINT('Ctrl Pts',(81.0047666250961,10.7923285389663,135.364065234981));
#63183=CARTESIAN_POINT('Ctrl Pts',(81.066965856771,10.7574600922865,135.360203072004));
#63184=CARTESIAN_POINT('Ctrl Pts',(81.12729092478,10.7193820818662,135.356340909027));
#63185=CARTESIAN_POINT('Ctrl Pts',(81.1854050201064,10.678336229963,135.352478746049));
#63186=CARTESIAN_POINT('Ctrl Pts',(81.2079550440027,10.6624091999359,135.350980110186));
#63187=CARTESIAN_POINT('Ctrl Pts',(81.2301725095293,10.646035748893,135.349481474322));
#63188=CARTESIAN_POINT('Ctrl Pts',(81.252039109102,10.6292316077768,135.347982838459));
#63189=CARTESIAN_POINT('',(77.945250359968,8.99878374008951,135.654074719411));
#63190=CARTESIAN_POINT('Ctrl Pts',(77.945250359968,8.99878374008951,135.654074719411));
#63191=CARTESIAN_POINT('Ctrl Pts',(77.9452088811236,9.068858104785,135.650257838806));
#63192=CARTESIAN_POINT('Ctrl Pts',(77.9487563144495,9.13907557315805,135.646440958201));
#63193=CARTESIAN_POINT('Ctrl Pts',(77.9559102037764,9.20903221635555,135.642624077596));
#63194=CARTESIAN_POINT('Ctrl Pts',(77.9630536357837,9.27888659923843,135.638812776381));
#63195=CARTESIAN_POINT('Ctrl Pts',(77.9737930081513,9.34848042062324,135.635001475166));
#63196=CARTESIAN_POINT('Ctrl Pts',(77.9880938466836,9.41741010139615,135.631190173951));
#63197=CARTESIAN_POINT('Ctrl Pts',(78.0023832068387,9.48628445668118,135.627381931827));
#63198=CARTESIAN_POINT('Ctrl Pts',(78.0202282665398,9.55449524075859,135.623573689702));
#63199=CARTESIAN_POINT('Ctrl Pts',(78.0415429670004,9.62164588987172,135.619765447577));
#63200=CARTESIAN_POINT('Ctrl Pts',(78.062848127941,9.68876648531526,135.615958909853));
#63201=CARTESIAN_POINT('Ctrl Pts',(78.0876196992428,9.75482741121009,135.61215237213));
#63202=CARTESIAN_POINT('Ctrl Pts',(78.1157214210871,9.81944603211567,135.608345834406));
#63203=CARTESIAN_POINT('Ctrl Pts',(78.1438205431129,9.8840586748575,135.604539648843));
#63204=CARTESIAN_POINT('Ctrl Pts',(78.1752490033443,9.94722882012437,135.60073346328));
#63205=CARTESIAN_POINT('Ctrl Pts',(78.2098226719939,10.0085944163998,135.596927277716));
#63206=CARTESIAN_POINT('Ctrl Pts',(78.2444287085065,10.0700174631367,135.593117528803));
#63207=CARTESIAN_POINT('Ctrl Pts',(78.2821855870685,10.1296321514811,135.589307779889));
#63208=CARTESIAN_POINT('Ctrl Pts',(78.3228640638332,10.1871026131374,135.585498030976));
#63209=CARTESIAN_POINT('Ctrl Pts',(78.3635622899696,10.2446009766625,135.581686432432));
#63210=CARTESIAN_POINT('Ctrl Pts',(78.4071846270008,10.2999526497124,135.577874833887));
#63211=CARTESIAN_POINT('Ctrl Pts',(78.4534612670306,10.3528545782624,135.574063235343));
#63212=CARTESIAN_POINT('Ctrl Pts',(78.4998192121046,10.4058494520572,135.570244940069));
#63213=CARTESIAN_POINT('Ctrl Pts',(78.5488404216444,10.4563856306972,135.566426644794));
#63214=CARTESIAN_POINT('Ctrl Pts',(78.6002185439981,10.5041972736092,135.56260834952));
#63215=CARTESIAN_POINT('Ctrl Pts',(78.6358004088325,10.5373091768409,135.559963993126));
#63216=CARTESIAN_POINT('Ctrl Pts',(78.6725119658445,10.5691151417946,135.557319636732));
#63217=CARTESIAN_POINT('Ctrl Pts',(78.710243122645,10.5995389210067,135.554675280338));
#63218=CARTESIAN_POINT('Ctrl Pts',(78.7654493618272,10.6440533905974,135.550806197491));
#63219=CARTESIAN_POINT('Ctrl Pts',(78.8230709826141,10.6857936224021,135.546937114644));
#63220=CARTESIAN_POINT('Ctrl Pts',(78.8827977135628,10.7244873480775,135.543068031797));
#63221=CARTESIAN_POINT('Ctrl Pts',(78.9424354546612,10.7631234220315,135.539204713691));
#63222=CARTESIAN_POINT('Ctrl Pts',(79.0041716756562,10.7987217379512,135.535341395584));
#63223=CARTESIAN_POINT('Ctrl Pts',(79.0676635881195,10.8310506212505,135.531478077478));
#63224=CARTESIAN_POINT('Ctrl Pts',(79.1310810245939,10.8633415827821,135.527619291042));
#63225=CARTESIAN_POINT('Ctrl Pts',(79.1962496310252,10.8923705100348,135.523760504606));
#63226=CARTESIAN_POINT('Ctrl Pts',(79.2627997262898,10.9179502910507,135.51990171817));
#63227=CARTESIAN_POINT('Ctrl Pts',(79.3293078998742,10.9435139586803,135.516045362487));
#63228=CARTESIAN_POINT('Ctrl Pts',(79.3971953833868,10.9656326168175,135.512189006804));
#63229=CARTESIAN_POINT('Ctrl Pts',(79.4660714454977,10.9841667926833,135.50833265112));
#63230=CARTESIAN_POINT('Ctrl Pts',(79.5349271609302,11.002695493368,135.504477434643));
#63231=CARTESIAN_POINT('Ctrl Pts',(79.6047704063481,11.0176416878133,135.500622218166));
#63232=CARTESIAN_POINT('Ctrl Pts',(79.6751958367456,11.0289159218737,135.496767001689));
#63233=CARTESIAN_POINT('Ctrl Pts',(79.7456240205668,11.0401905967229,135.492911634484));
#63234=CARTESIAN_POINT('Ctrl Pts',(79.8166339545343,11.0477929515476,135.48905626728));
#63235=CARTESIAN_POINT('Ctrl Pts',(79.8878123795722,11.0516850392599,135.485200900075));
#63236=CARTESIAN_POINT('Ctrl Pts',(79.9590653090118,11.0555812009267,135.481341497352));
#63237=CARTESIAN_POINT('Ctrl Pts',(80.0304865955321,11.0557593162919,135.477482094629));
#63238=CARTESIAN_POINT('Ctrl Pts',(80.1016610683358,11.0522335611925,135.473622691907));
#63239=CARTESIAN_POINT('Ctrl Pts',(80.1728758406852,11.0487058097829,135.46976110396));
#63240=CARTESIAN_POINT('Ctrl Pts',(80.2438430376168,11.0414700624067,135.465899516013));
#63241=CARTESIAN_POINT('Ctrl Pts',(80.3141534558345,11.0305923196662,135.462037928066));
#63242=CARTESIAN_POINT('Ctrl Pts',(80.384586884649,11.0196955459248,135.458169584132));
#63243=CARTESIAN_POINT('Ctrl Pts',(80.4543607649211,11.0051441545454,135.454301240199));
#63244=CARTESIAN_POINT('Ctrl Pts',(80.5230776005263,10.9870549530216,135.450432896265));
#63245=CARTESIAN_POINT('Ctrl Pts',(80.5638796800102,10.9763141057187,135.448135984959));
#63246=CARTESIAN_POINT('Ctrl Pts',(80.604309382419,10.9643269064461,135.445839073652));
#63247=CARTESIAN_POINT('Ctrl Pts',(80.6442868085188,10.9511258470095,135.443542162346));
#63248=CARTESIAN_POINT('Ctrl Pts',(80.7116141902564,10.9288934810286,135.439673853667));
#63249=CARTESIAN_POINT('Ctrl Pts',(80.777921307324,10.9031285968536,135.435805544988));
#63250=CARTESIAN_POINT('Ctrl Pts',(80.8428113700402,10.873944117905,135.431937236309));
#63251=CARTESIAN_POINT('Ctrl Pts',(80.9076166286747,10.8447977798186,135.428073983078));
#63252=CARTESIAN_POINT('Ctrl Pts',(80.9710080660991,10.8122409062393,135.424210729848));
#63253=CARTESIAN_POINT('Ctrl Pts',(81.0326051384999,10.7764358109551,135.420347476617));
#63254=CARTESIAN_POINT('Ctrl Pts',(81.0941310956297,10.7406720534967,135.416488683604));
#63255=CARTESIAN_POINT('Ctrl Pts',(81.153866384326,10.7016677655053,135.41262989059));
#63256=CARTESIAN_POINT('Ctrl Pts',(81.2114532906714,10.6596320336211,135.408771097576));
#63257=CARTESIAN_POINT('Ctrl Pts',(81.225104019335,10.6496676440308,135.407856387276));
#63258=CARTESIAN_POINT('Ctrl Pts',(81.238634140733,10.6395331171351,135.406941676975));
#63259=CARTESIAN_POINT('Ctrl Pts',(81.252039109102,10.6292316077768,135.406026966675));
#63260=CARTESIAN_POINT('Ctrl Pts',(81.252039109102,10.6292316077768,136.106053391442));
#63261=CARTESIAN_POINT('Ctrl Pts',(81.3083146843325,10.5859847049182,136.102186604502));
#63262=CARTESIAN_POINT('Ctrl Pts',(81.3624484325911,10.5397406392775,136.098319817562));
#63263=CARTESIAN_POINT('Ctrl Pts',(81.4141045122279,10.4907400816362,136.094453030622));
#63264=CARTESIAN_POINT('Ctrl Pts',(81.4671200795666,10.440449924475,136.090484477359));
#63265=CARTESIAN_POINT('Ctrl Pts',(81.5175252596536,10.3872563791613,136.086515924095));
#63266=CARTESIAN_POINT('Ctrl Pts',(81.5649910392335,10.3314655870952,136.082547370832));
#63267=CARTESIAN_POINT('Ctrl Pts',(81.6111305643379,10.277233660981,136.078689704013));
#63268=CARTESIAN_POINT('Ctrl Pts',(81.6544924626276,10.2205481259674,136.074832037194));
#63269=CARTESIAN_POINT('Ctrl Pts',(81.6948115861983,10.1617277003618,136.070974370375));
#63270=CARTESIAN_POINT('Ctrl Pts',(81.7351106654874,10.1029365167901,136.06711862136));
#63271=CARTESIAN_POINT('Ctrl Pts',(81.7723696975057,10.0420129487833,136.063262872345));
#63272=CARTESIAN_POINT('Ctrl Pts',(81.8063653518934,9.97930678440356,136.05940712333));
#63273=CARTESIAN_POINT('Ctrl Pts',(81.8403554776345,9.91661081780456,136.055552001367));
#63274=CARTESIAN_POINT('Ctrl Pts',(81.8710830487273,9.85213325781443,136.051696879405));
#63275=CARTESIAN_POINT('Ctrl Pts',(81.8983702878578,9.78624920520071,136.047841757443));
#63276=CARTESIAN_POINT('Ctrl Pts',(81.9270569662787,9.71698625700147,136.043788923681));
#63277=CARTESIAN_POINT('Ctrl Pts',(81.9519407103413,9.64616921090295,136.039736089919));
#63278=CARTESIAN_POINT('Ctrl Pts',(81.9728728497112,9.57425628544433,136.035683256158));
#63279=CARTESIAN_POINT('Ctrl Pts',(81.9928102662182,9.50576075702419,136.031823018401));
#63280=CARTESIAN_POINT('Ctrl Pts',(82.0091630510908,9.43627164366354,136.027962780643));
#63281=CARTESIAN_POINT('Ctrl Pts',(82.0218549345478,9.36619692263136,136.024102542886));
#63282=CARTESIAN_POINT('Ctrl Pts',(82.0345557099355,9.29607310726548,136.020239600647));
#63283=CARTESIAN_POINT('Ctrl Pts',(82.0435904205792,9.22536334930288,136.016376658408));
#63284=CARTESIAN_POINT('Ctrl Pts',(82.0489346541452,9.1544808905425,136.012513716169));
#63285=CARTESIAN_POINT('Ctrl Pts',(82.054287535372,9.08348373480052,136.00864452319));
#63286=CARTESIAN_POINT('Ctrl Pts',(82.0559380205628,9.01231380499041,136.004775330211));
#63287=CARTESIAN_POINT('Ctrl Pts',(82.0539137429832,8.94138345894926,136.000906137232));
#63288=CARTESIAN_POINT('Ctrl Pts',(82.0536175569697,8.9310051508368,136.000340008922));
#63289=CARTESIAN_POINT('Ctrl Pts',(82.0532427894648,8.92063195935964,135.999773880613));
#63290=CARTESIAN_POINT('Ctrl Pts',(82.0527896193309,8.91026516135016,135.999207752304));
#63291=CARTESIAN_POINT('Ctrl Pts',(82.0496925249742,8.83941549759563,135.995338669457));
#63292=CARTESIAN_POINT('Ctrl Pts',(82.0429171171316,8.76858759361845,135.99146958661));
#63293=CARTESIAN_POINT('Ctrl Pts',(82.0324642301757,8.69819424200943,135.987600503763));
#63294=CARTESIAN_POINT('Ctrl Pts',(82.0220269175001,8.6279057729836,135.983737185657));
#63295=CARTESIAN_POINT('Ctrl Pts',(82.0079230726633,8.55805104773285,135.97987386755));
#63296=CARTESIAN_POINT('Ctrl Pts',(81.990205484446,8.48904042020795,135.976010549444));
#63297=CARTESIAN_POINT('Ctrl Pts',(81.9725086789528,8.42011074212258,135.972151763008));
#63298=CARTESIAN_POINT('Ctrl Pts',(81.9512066702232,8.35202366327697,135.968292976572));
#63299=CARTESIAN_POINT('Ctrl Pts',(81.9264034611248,8.28518025526267,135.964434190136));
#63300=CARTESIAN_POINT('Ctrl Pts',(81.9016158762294,8.218378953694,135.960577834453));
#63301=CARTESIAN_POINT('Ctrl Pts',(81.8733316352396,8.15282022302366,135.95672147877));
#63302=CARTESIAN_POINT('Ctrl Pts',(81.8417044010275,8.08888943495536,135.952865123087));
#63303=CARTESIAN_POINT('Ctrl Pts',(81.8100865098171,8.024977532682,135.949009906609));
#63304=CARTESIAN_POINT('Ctrl Pts',(81.7751278012398,7.96269305344755,135.945154690132));
#63305=CARTESIAN_POINT('Ctrl Pts',(81.7370291283397,7.90239926667326,135.941299473655));
#63306=CARTESIAN_POINT('Ctrl Pts',(81.6989289658955,7.84210312259222,135.93744410645));
#63307=CARTESIAN_POINT('Ctrl Pts',(81.6576888567548,7.78379823498375,135.933588739246));
#63308=CARTESIAN_POINT('Ctrl Pts',(81.6135535318407,7.72781976026015,135.929733372041));
#63309=CARTESIAN_POINT('Ctrl Pts',(81.5693720092765,7.67178269133812,135.925873969318));
#63310=CARTESIAN_POINT('Ctrl Pts',(81.5222895227633,7.61807727860314,135.922014566595));
#63311=CARTESIAN_POINT('Ctrl Pts',(81.4725911750781,7.56700565472777,135.918155163873));
#63312=CARTESIAN_POINT('Ctrl Pts',(81.4228646877979,7.51590511369777,135.914293575926));
#63313=CARTESIAN_POINT('Ctrl Pts',(81.3705197475215,7.46744166037609,135.910431987979));
#63314=CARTESIAN_POINT('Ctrl Pts',(81.3158763962686,7.42187868899659,135.906570400032));
#63315=CARTESIAN_POINT('Ctrl Pts',(81.2611374445141,7.37623600356553,135.902702056098));
#63316=CARTESIAN_POINT('Ctrl Pts',(81.2040924423584,7.33350422278879,135.898833712165));
#63317=CARTESIAN_POINT('Ctrl Pts',(81.1450918128928,7.29390436887442,135.894965368231));
#63318=CARTESIAN_POINT('Ctrl Pts',(81.1100589370067,7.2703911152048,135.892668456925));
#63319=CARTESIAN_POINT('Ctrl Pts',(81.0743370944693,7.24798121228253,135.890371545619));
#63320=CARTESIAN_POINT('Ctrl Pts',(81.038003484846,7.22671312869363,135.888074634312));
#63321=CARTESIAN_POINT('Ctrl Pts',(80.9768005357521,7.19088763679479,135.884205551465));
#63322=CARTESIAN_POINT('Ctrl Pts',(80.9136208229207,7.15816421980074,135.880336468618));
#63323=CARTESIAN_POINT('Ctrl Pts',(80.8488115996088,7.12876606730488,135.876467385771));
#63324=CARTESIAN_POINT('Ctrl Pts',(80.7840989388074,7.09941171659008,135.872604067665));
#63325=CARTESIAN_POINT('Ctrl Pts',(80.7177620256111,7.07337299491202,135.868740749559));
#63326=CARTESIAN_POINT('Ctrl Pts',(80.6501742435433,7.05082812057713,135.864877431452));
#63327=CARTESIAN_POINT('Ctrl Pts',(80.5826657419179,7.02830969137116,135.861018645016));
#63328=CARTESIAN_POINT('Ctrl Pts',(80.5139097444993,7.0092771219014,135.857159858581));
#63329=CARTESIAN_POINT('Ctrl Pts',(80.4442996139068,6.9938605692569,135.853301072145));
#63330=CARTESIAN_POINT('Ctrl Pts',(80.3747333325923,6.97845372791013,135.849444716462));
#63331=CARTESIAN_POINT('Ctrl Pts',(80.3043144587388,6.96665848901139,135.845588360778));
#63332=CARTESIAN_POINT('Ctrl Pts',(80.2334500995796,6.95855477332693,135.841732005095));
#63333=CARTESIAN_POINT('Ctrl Pts',(80.1626066744617,6.95045345156123,135.837876788618));
#63334=CARTESIAN_POINT('Ctrl Pts',(80.091318507677,6.94604154320104,135.834021572141));
#63335=CARTESIAN_POINT('Ctrl Pts',(80.0199997326209,6.94534733514516,135.830166355663));
#63336=CARTESIAN_POINT('Ctrl Pts',(79.948678169214,6.94465309994782,135.826310988459));
#63337=CARTESIAN_POINT('Ctrl Pts',(79.8773264809413,6.94767685615559,135.822455621254));
#63338=CARTESIAN_POINT('Ctrl Pts',(79.8063589810274,6.95439477946715,135.81860025405));
#63339=CARTESIAN_POINT('Ctrl Pts',(79.735317197493,6.96111973461253,135.814740851327));
#63340=CARTESIAN_POINT('Ctrl Pts',(79.6646608896917,6.97154652995798,135.810881448604));
#63341=CARTESIAN_POINT('Ctrl Pts',(79.5947985234109,6.98559951204583,135.807022045881));
#63342=CARTESIAN_POINT('Ctrl Pts',(79.5248966005095,6.99966045104253,135.803160457934));
#63343=CARTESIAN_POINT('Ctrl Pts',(79.4557899848462,7.01735154348953,135.799298869987));
#63344=CARTESIAN_POINT('Ctrl Pts',(79.3878735471225,7.03854677134845,135.79543728204));
#63345=CARTESIAN_POINT('Ctrl Pts',(79.3198382871566,7.05977908101822,135.791568938107));
#63346=CARTESIAN_POINT('Ctrl Pts',(79.2529978181219,7.08452759730746,135.787700594174));
#63347=CARTESIAN_POINT('Ctrl Pts',(79.1877278906748,7.11261779628174,135.78383225024));
#63348=CARTESIAN_POINT('Ctrl Pts',(79.1489724860618,7.12929694806709,135.781535338934));
#63349=CARTESIAN_POINT('Ctrl Pts',(79.110770360955,7.14715335925725,135.779238427627));
#63350=CARTESIAN_POINT('Ctrl Pts',(79.073195705611,7.1661430365478,135.776941516321));
#63351=CARTESIAN_POINT('Ctrl Pts',(79.0099022497152,7.1981306167681,135.773072433474));
#63352=CARTESIAN_POINT('Ctrl Pts',(78.9481427918075,7.23346144597127,135.769203350627));
#63353=CARTESIAN_POINT('Ctrl Pts',(78.8882931841807,7.27196483885281,135.76533426778));
#63354=CARTESIAN_POINT('Ctrl Pts',(78.8285327494845,7.31041086359923,135.761470949674));
#63355=CARTESIAN_POINT('Ctrl Pts',(78.7706769218814,7.35201980844774,135.757607631567));
#63356=CARTESIAN_POINT('Ctrl Pts',(78.7150779443408,7.39657464365177,135.753744313461));
#63357=CARTESIAN_POINT('Ctrl Pts',(78.6595441843794,7.44107721605125,135.749885527025));
#63358=CARTESIAN_POINT('Ctrl Pts',(78.606262393319,7.48851851265072,135.746026740589));
#63359=CARTESIAN_POINT('Ctrl Pts',(78.5555552725787,7.53863865114589,135.742167954153));
#63360=CARTESIAN_POINT('Ctrl Pts',(78.5048800936062,7.58872721762896,135.73831159847));
#63361=CARTESIAN_POINT('Ctrl Pts',(78.4567767118996,7.64149093739805,135.734455242787));
#63362=CARTESIAN_POINT('Ctrl Pts',(78.4115330784898,7.69663113365102,135.730598887103));
#63363=CARTESIAN_POINT('Ctrl Pts',(78.3663028105023,7.75175504093786,135.726743670626));
#63364=CARTESIAN_POINT('Ctrl Pts',(78.3239309216265,7.80925365563422,135.722888454149));
#63365=CARTESIAN_POINT('Ctrl Pts',(78.2846657944253,7.86879439283327,135.719033237672));
#63366=CARTESIAN_POINT('Ctrl Pts',(78.2453991320751,7.92833745789711,135.715177870467));
#63367=CARTESIAN_POINT('Ctrl Pts',(78.2092397381526,7.98992239722593,135.711322503263));
#63368=CARTESIAN_POINT('Ctrl Pts',(78.1763923124136,8.0531882107431,135.707467136058));
#63369=CARTESIAN_POINT('Ctrl Pts',(78.143510504377,8.1165202463152,135.703607733335));
#63370=CARTESIAN_POINT('Ctrl Pts',(78.1139478091924,8.18153623624629,135.699748330612));
#63371=CARTESIAN_POINT('Ctrl Pts',(78.0878622116923,8.24785198197061,135.695888927889));
#63372=CARTESIAN_POINT('Ctrl Pts',(78.0617618443218,8.31420527619113,135.692027339943));
#63373=CARTESIAN_POINT('Ctrl Pts',(78.0391426479366,8.38185933028476,135.688165751996));
#63374=CARTESIAN_POINT('Ctrl Pts',(78.0201129207117,8.45041405060964,135.684304164049));
#63375=CARTESIAN_POINT('Ctrl Pts',(78.001049900297,8.51908870987492,135.680435820115));
#63376=CARTESIAN_POINT('Ctrl Pts',(77.9855889924591,8.58866670703014,135.676567476182));
#63377=CARTESIAN_POINT('Ctrl Pts',(77.9737873736293,8.65873770317237,135.672699132248));
#63378=CARTESIAN_POINT('Ctrl Pts',(77.9667799119893,8.70034384421349,135.670402220942));
#63379=CARTESIAN_POINT('Ctrl Pts',(77.9610615928321,8.74212367917311,135.668105309635));
#63380=CARTESIAN_POINT('Ctrl Pts',(77.9566356952624,8.78399101726015,135.665808398329));
#63381=CARTESIAN_POINT('Ctrl Pts',(77.9490991887904,8.85528355385796,135.66189717204));
#63382=CARTESIAN_POINT('Ctrl Pts',(77.94529286412,8.92697727577637,135.657985945751));
#63383=CARTESIAN_POINT('Ctrl Pts',(77.9452503599685,8.99878373915154,135.654074719462));
#63384=CARTESIAN_POINT('Origin',(80.,9.,141.545925280538));
#63385=CARTESIAN_POINT('',(81.252039109102,10.6292316077768,136.806140361941));
#63386=CARTESIAN_POINT('',(81.252039109102,10.6292316077768,136.747866922016));
#63387=CARTESIAN_POINT('',(81.252039109102,10.6292316077768,141.545925280538));
#63388=CARTESIAN_POINT('',(77.9452505319477,8.99852147413462,136.295925280587));
#63389=CARTESIAN_POINT('Ctrl Pts',(81.252039109102,10.6292316077768,136.747866922016));
#63390=CARTESIAN_POINT('Ctrl Pts',(81.3085184540973,10.5858281110284,136.74401000082));
#63391=CARTESIAN_POINT('Ctrl Pts',(81.3627855868937,10.5394478623079,136.740153079624));
#63392=CARTESIAN_POINT('Ctrl Pts',(81.4145162186297,10.4903494320908,136.736296158428));
#63393=CARTESIAN_POINT('Ctrl Pts',(81.4662266011205,10.4412702207799,136.732440746972));
#63394=CARTESIAN_POINT('Ctrl Pts',(81.5154021011393,10.3894752738317,136.728585335515));
#63395=CARTESIAN_POINT('Ctrl Pts',(81.5617531753342,10.3352619899605,136.724729924058));
#63396=CARTESIAN_POINT('Ctrl Pts',(81.6081016109247,10.281051792262,136.720874732076));
#63397=CARTESIAN_POINT('Ctrl Pts',(81.6516256254678,10.2244239012393,136.717019540094));
#63398=CARTESIAN_POINT('Ctrl Pts',(81.6920752293629,10.1657096468146,136.713164348112));
#63399=CARTESIAN_POINT('Ctrl Pts',(81.732564681132,10.106937551571,136.709305358288));
#63400=CARTESIAN_POINT('Ctrl Pts',(81.7699733961127,10.0460753883556,136.705446368464));
#63401=CARTESIAN_POINT('Ctrl Pts',(81.8040946189889,9.98348368986742,136.701587378641));
#63402=CARTESIAN_POINT('Ctrl Pts',(81.8382322234244,9.92086194117785,136.69772653612));
#63403=CARTESIAN_POINT('Ctrl Pts',(81.86907898119,9.85650944175953,136.6938656936));
#63404=CARTESIAN_POINT('Ctrl Pts',(81.8964753088183,9.79080905757488,136.690004851079));
#63405=CARTESIAN_POINT('Ctrl Pts',(81.923922074071,9.72498771662032,136.686136900609));
#63406=CARTESIAN_POINT('Ctrl Pts',(81.9479055535397,9.65781399157883,136.682268950139));
#63407=CARTESIAN_POINT('Ctrl Pts',(81.9683154621906,9.58968788676836,136.678400999669));
#63408=CARTESIAN_POINT('Ctrl Pts',(81.986284042303,9.52971067702336,136.674995713585));
#63409=CARTESIAN_POINT('Ctrl Pts',(82.0014835402419,9.46899572838118,136.671590427501));
#63410=CARTESIAN_POINT('Ctrl Pts',(82.0138717544802,9.40782118508842,136.668185141418));
#63411=CARTESIAN_POINT('Ctrl Pts',(82.0279472318518,9.33831472650817,136.664316058571));
#63412=CARTESIAN_POINT('Ctrl Pts',(82.0384476506383,9.26794257762408,136.660446975724));
#63413=CARTESIAN_POINT('Ctrl Pts',(82.045274300028,9.19710555584454,136.656577892877));
#63414=CARTESIAN_POINT('Ctrl Pts',(82.0520907780507,9.12637407769456,136.652714574771));
#63415=CARTESIAN_POINT('Ctrl Pts',(82.0552443056657,9.05517958111897,136.648851256664));
#63416=CARTESIAN_POINT('Ctrl Pts',(82.0546871818792,8.98393304255929,136.644987938558));
#63417=CARTESIAN_POINT('Ctrl Pts',(82.0541307115987,8.91277007616198,136.641129152122));
#63418=CARTESIAN_POINT('Ctrl Pts',(82.0498722394196,8.84155567244782,136.637270365686));
#63419=CARTESIAN_POINT('Ctrl Pts',(82.0419160056416,8.77070414655999,136.63341157925));
#63420=CARTESIAN_POINT('Ctrl Pts',(82.0339647837074,8.69989725193819,136.629555223567));
#63421=CARTESIAN_POINT('Ctrl Pts',(82.022320475588,8.62945326323857,136.625698867884));
#63422=CARTESIAN_POINT('Ctrl Pts',(82.0070393018439,8.55978323140311,136.6218425122));
#63423=CARTESIAN_POINT('Ctrl Pts',(81.9917626423116,8.49013378079267,136.617987295723));
#63424=CARTESIAN_POINT('Ctrl Pts',(81.9728513540896,8.42125830738812,136.614132079246));
#63425=CARTESIAN_POINT('Ctrl Pts',(81.9504127845803,8.35355778893574,136.610276862769));
#63426=CARTESIAN_POINT('Ctrl Pts',(81.9279733377901,8.28585462359568,136.606421495564));
#63427=CARTESIAN_POINT('Ctrl Pts',(81.9020064908408,8.21932696483277,136.602566128359));
#63428=CARTESIAN_POINT('Ctrl Pts',(81.8726689525194,8.15435908520832,136.598710761155));
#63429=CARTESIAN_POINT('Ctrl Pts',(81.8433007057954,8.08932320192966,136.594851358432));
#63430=CARTESIAN_POINT('Ctrl Pts',(81.8105549249677,8.02585080059414,136.590991955709));
#63431=CARTESIAN_POINT('Ctrl Pts',(81.7746354615354,7.96430383743053,136.587132552986));
#63432=CARTESIAN_POINT('Ctrl Pts',(81.7386956602207,7.90272202589287,136.583270965039));
#63433=CARTESIAN_POINT('Ctrl Pts',(81.6995788656066,7.84306822920265,136.579409377092));
#63434=CARTESIAN_POINT('Ctrl Pts',(81.6575321773042,7.7856752313729,136.575547789146));
#63435=CARTESIAN_POINT('Ctrl Pts',(81.6154119268134,7.7281818224363,136.571679445212));
#63436=CARTESIAN_POINT('Ctrl Pts',(81.5703518557311,7.67295748583205,136.567811101279));
#63437=CARTESIAN_POINT('Ctrl Pts',(81.5226387640879,7.62030120801794,136.563942757345));
#63438=CARTESIAN_POINT('Ctrl Pts',(81.4943081033344,7.58903542556877,136.561645846039));
#63439=CARTESIAN_POINT('Ctrl Pts',(81.4650427907926,7.55867434414894,136.559348934732));
#63440=CARTESIAN_POINT('Ctrl Pts',(81.4349084744055,7.52927390973731,136.557052023426));
#63441=CARTESIAN_POINT('Ctrl Pts',(81.3841480613612,7.47974970035277,136.553182940579));
#63442=CARTESIAN_POINT('Ctrl Pts',(81.3307213118376,7.43275948255617,136.549313857732));
#63443=CARTESIAN_POINT('Ctrl Pts',(81.2749114269959,7.38860358203972,136.545444774885));
#63444=CARTESIAN_POINT('Ctrl Pts',(81.2191846960995,7.34451347161309,136.541581456779));
#63445=CARTESIAN_POINT('Ctrl Pts',(81.1610822558932,7.30324959490401,136.537718138672));
#63446=CARTESIAN_POINT('Ctrl Pts',(81.1009235091995,7.2650749326291,136.533854820566));
#63447=CARTESIAN_POINT('Ctrl Pts',(81.0408353286922,7.22694504921818,136.52999603413));
#63448=CARTESIAN_POINT('Ctrl Pts',(80.9786960410184,7.1918974414676,136.526137247694));
#63449=CARTESIAN_POINT('Ctrl Pts',(80.9148560258897,7.16015326334141,136.522278461259));
#63450=CARTESIAN_POINT('Ctrl Pts',(80.8510562252894,7.12842908171974,136.518422105575));
#63451=CARTESIAN_POINT('Ctrl Pts',(80.7855582566907,7.10000441699144,136.514565749892));
#63452=CARTESIAN_POINT('Ctrl Pts',(80.7187379505123,7.07505498234537,136.510709394209));
#63453=CARTESIAN_POINT('Ctrl Pts',(80.6519373837216,7.05011291801217,136.506854177731));
#63454=CARTESIAN_POINT('Ctrl Pts',(80.5838157097105,7.0286442154711,136.502998961254));
#63455=CARTESIAN_POINT('Ctrl Pts',(80.5147680262655,7.01077617105698,136.499143744777));
#63456=CARTESIAN_POINT('Ctrl Pts',(80.4457176432624,6.99290742805571,136.495288377572));
#63457=CARTESIAN_POINT('Ctrl Pts',(80.3757416497901,6.97863974224021,136.491433010368));
#63458=CARTESIAN_POINT('Ctrl Pts',(80.3052478817002,6.96804987924961,136.487577643163));
#63459=CARTESIAN_POINT('Ctrl Pts',(80.2346803258581,6.9574489315602,136.48371824044));
#63460=CARTESIAN_POINT('Ctrl Pts',(80.1635943948842,6.95053356382926,136.479858837718));
#63461=CARTESIAN_POINT('Ctrl Pts',(80.0924047452203,6.94732883160483,136.475999434995));
#63462=CARTESIAN_POINT('Ctrl Pts',(80.0211747874175,6.94412228483584,136.472137847048));
#63463=CARTESIAN_POINT('Ctrl Pts',(79.9498414800195,6.94463055253553,136.468276259101));
#63464=CARTESIAN_POINT('Ctrl Pts',(79.8788184278493,6.94882653364688,136.464414671154));
#63465=CARTESIAN_POINT('Ctrl Pts',(79.8076711183036,6.95302985577759,136.46054632722));
#63466=CARTESIAN_POINT('Ctrl Pts',(79.7368356306462,6.96093371860795,136.456677983287));
#63467=CARTESIAN_POINT('Ctrl Pts',(79.6667187079827,6.97245933631621,136.452809639354));
#63468=CARTESIAN_POINT('Ctrl Pts',(79.6250852970938,6.97930291643309,136.450512728047));
#63469=CARTESIAN_POINT('Ctrl Pts',(79.5837050187288,6.98742242046764,136.448215816741));
#63470=CARTESIAN_POINT('Ctrl Pts',(79.5426604811077,6.99679303940922,136.445918905434));
#63471=CARTESIAN_POINT('Ctrl Pts',(79.4735221055763,7.01257758490282,136.442049822587));
#63472=CARTESIAN_POINT('Ctrl Pts',(79.4050664517631,7.03197659503789,136.43818073974));
#63473=CARTESIAN_POINT('Ctrl Pts',(79.3376994359528,7.05491503389628,136.434311656893));
#63474=CARTESIAN_POINT('Ctrl Pts',(79.2704327936362,7.0778192956248,136.430448338787));
#63475=CARTESIAN_POINT('Ctrl Pts',(79.2042520257748,7.10425236287628,136.426585020681));
#63476=CARTESIAN_POINT('Ctrl Pts',(79.1395513089728,7.13408853033979,136.422721702574));
#63477=CARTESIAN_POINT('Ctrl Pts',(79.0749264860866,7.16388969999036,136.418862916138));
#63478=CARTESIAN_POINT('Ctrl Pts',(79.0117787047756,7.19708583827694,136.415004129703));
#63479=CARTESIAN_POINT('Ctrl Pts',(78.9504838028604,7.23350252917202,136.411145343267));
#63480=CARTESIAN_POINT('Ctrl Pts',(78.8892275122389,7.26989628022215,136.407288987584));
#63481=CARTESIAN_POINT('Ctrl Pts',(78.8298222019973,7.3095063114083,136.4034326319));
#63482=CARTESIAN_POINT('Ctrl Pts',(78.7726193376205,7.35211217853979,136.399576276217));
#63483=CARTESIAN_POINT('Ctrl Pts',(78.7154333715427,7.39470545947148,136.39572105974));
#63484=CARTESIAN_POINT('Ctrl Pts',(78.6604489490401,7.44029252935922,136.391865843263));
#63485=CARTESIAN_POINT('Ctrl Pts',(78.6079873092383,7.48861049651041,136.388010626785));
#63486=CARTESIAN_POINT('Ctrl Pts',(78.5555236183434,7.53693035274952,136.384155259581));
#63487=CARTESIAN_POINT('Ctrl Pts',(78.5055832618023,7.58798098751036,136.380299892376));
#63488=CARTESIAN_POINT('Ctrl Pts',(78.4584519351075,7.64146140057548,136.376444525172));
#63489=CARTESIAN_POINT('Ctrl Pts',(78.4112712747657,7.6949977930498,136.372585122449));
#63490=CARTESIAN_POINT('Ctrl Pts',(78.3669058355876,7.75096867565695,136.368725719726));
#63491=CARTESIAN_POINT('Ctrl Pts',(78.3256015690616,7.80903927144048,136.364866317003));
#63492=CARTESIAN_POINT('Ctrl Pts',(78.2842739157354,7.86714274725158,136.361004729056));
#63493=CARTESIAN_POINT('Ctrl Pts',(78.2460111461352,7.92734789273723,136.357143141109));
#63494=CARTESIAN_POINT('Ctrl Pts',(78.2110148228832,7.98929252572442,136.353281553162));
#63495=CARTESIAN_POINT('Ctrl Pts',(78.1759572723093,8.05134553306729,136.349413209229));
#63496=CARTESIAN_POINT('Ctrl Pts',(78.1441777944383,8.11514366897695,136.345544865295));
#63497=CARTESIAN_POINT('Ctrl Pts',(78.115830808151,8.18030248323716,136.341676521362));
#63498=CARTESIAN_POINT('Ctrl Pts',(78.0989991834487,8.21899191203774,136.339379610056));
#63499=CARTESIAN_POINT('Ctrl Pts',(78.0833767987337,8.25816071185491,136.337082698749));
#63500=CARTESIAN_POINT('Ctrl Pts',(78.0689876162082,8.29772602487152,136.334785787443));
#63501=CARTESIAN_POINT('Ctrl Pts',(78.0409616303174,8.37478786646014,136.330312065342));
#63502=CARTESIAN_POINT('Ctrl Pts',(78.0175257042648,8.45360303856632,136.325838343242));
#63503=CARTESIAN_POINT('Ctrl Pts',(77.9988702448825,8.53365542172823,136.321364621142));
#63504=CARTESIAN_POINT('Ctrl Pts',(77.9803784740623,8.61300540141546,136.316930152813));
#63505=CARTESIAN_POINT('Ctrl Pts',(77.9665837380257,8.69357080831013,136.312495684485));
#63506=CARTESIAN_POINT('Ctrl Pts',(77.9576251286371,8.77482796060499,136.308061216156));
#63507=CARTESIAN_POINT('Ctrl Pts',(77.9494527016198,8.84895421368233,136.3040159043));
#63508=CARTESIAN_POINT('Ctrl Pts',(77.9453044026692,8.92365579951472,136.299970592443));
#63509=CARTESIAN_POINT('Ctrl Pts',(77.9452505319477,8.99852147413461,136.295925280587));
#63510=CARTESIAN_POINT('Ctrl Pts',(77.945250531947,8.9985214750451,136.295925280538));
#63511=CARTESIAN_POINT('Ctrl Pts',(77.9451990745752,9.07003329291146,136.292061191873));
#63512=CARTESIAN_POINT('Ctrl Pts',(77.9488851993071,9.14157794387393,136.288197103208));
#63513=CARTESIAN_POINT('Ctrl Pts',(77.9562925982608,9.21273838059117,136.284333014543));
#63514=CARTESIAN_POINT('Ctrl Pts',(77.963699599031,9.2838949920902,136.280469133592));
#63515=CARTESIAN_POINT('Ctrl Pts',(77.9748274258944,9.35466695085,136.276605252641));
#63516=CARTESIAN_POINT('Ctrl Pts',(77.9896079183788,9.42464248569205,136.272741371689));
#63517=CARTESIAN_POINT('Ctrl Pts',(78.004392467588,9.4946372263551,136.268876430239));
#63518=CARTESIAN_POINT('Ctrl Pts',(78.0228315710416,9.56383463791113,136.265011488788));
#63519=CARTESIAN_POINT('Ctrl Pts',(78.0448063606778,9.63183494304609,136.261146547337));
#63520=CARTESIAN_POINT('Ctrl Pts',(78.066809060374,9.69992161499648,136.257276697046));
#63521=CARTESIAN_POINT('Ctrl Pts',(78.0923562553077,9.76680768829056,136.253406846754));
#63522=CARTESIAN_POINT('Ctrl Pts',(78.1212800534335,9.83211112531514,136.249536996462));
#63523=CARTESIAN_POINT('Ctrl Pts',(78.1502258976062,9.89746433735987,136.245664196527));
#63524=CARTESIAN_POINT('Ctrl Pts',(78.1825532470504,9.96123208405092,136.241791396591));
#63525=CARTESIAN_POINT('Ctrl Pts',(78.2180484155873,10.0230572385303,136.237918596656));
#63526=CARTESIAN_POINT('Ctrl Pts',(78.2536056682719,10.0849905306007,136.234039022855));
#63527=CARTESIAN_POINT('Ctrl Pts',(78.2923415309165,10.1449740495301,136.230159449055));
#63528=CARTESIAN_POINT('Ctrl Pts',(78.3339997518961,10.2026806458148,136.226279875254));
#63529=CARTESIAN_POINT('Ctrl Pts',(78.3434032521698,10.2157067420139,136.225404139987));
#63530=CARTESIAN_POINT('Ctrl Pts',(78.3529555021341,10.228616961064,136.224528404719));
#63531=CARTESIAN_POINT('Ctrl Pts',(78.3626532888618,10.2414077936056,136.223652669452));
#63532=CARTESIAN_POINT('Ctrl Pts',(78.4054990456461,10.2979189250149,136.219783586605));
#63533=CARTESIAN_POINT('Ctrl Pts',(78.4513577800801,10.3523199783994,136.215914503758));
#63534=CARTESIAN_POINT('Ctrl Pts',(78.4999940143905,10.4042719129982,136.212045420911));
#63535=CARTESIAN_POINT('Ctrl Pts',(78.5485577831374,10.4561464418055,136.208182102804));
#63536=CARTESIAN_POINT('Ctrl Pts',(78.5998905079848,10.5055787433783,136.204318784698));
#63537=CARTESIAN_POINT('Ctrl Pts',(78.6537153665542,10.5522613337476,136.200455466592));
#63538=CARTESIAN_POINT('Ctrl Pts',(78.7074770885853,10.5988891654564,136.196596680156));
#63539=CARTESIAN_POINT('Ctrl Pts',(78.7637247725268,10.6427733759751,136.19273789372));
#63540=CARTESIAN_POINT('Ctrl Pts',(78.8221447529238,10.6836432458912,136.188879107284));
#63541=CARTESIAN_POINT('Ctrl Pts',(78.8805279330169,10.7244873707861,136.185022751601));
#63542=CARTESIAN_POINT('Ctrl Pts',(78.9410802976008,10.7623206444849,136.181166395918));
#63543=CARTESIAN_POINT('Ctrl Pts',(79.0034562665658,10.796913506503,136.177310040234));
#63544=CARTESIAN_POINT('Ctrl Pts',(79.065813809045,10.8314961494433,136.173454823757));
#63545=CARTESIAN_POINT('Ctrl Pts',(79.1299934618203,10.8628400456359,136.16959960728));
#63546=CARTESIAN_POINT('Ctrl Pts',(79.1956234031313,10.8907606545805,136.165744390803));
#63547=CARTESIAN_POINT('Ctrl Pts',(79.2612559103766,10.9186823551374,136.161889023598));
#63548=CARTESIAN_POINT('Ctrl Pts',(79.3283383708567,10.9431803145808,136.158033656394));
#63549=CARTESIAN_POINT('Ctrl Pts',(79.3964788642986,10.9641180721285,136.154178289189));
#63550=CARTESIAN_POINT('Ctrl Pts',(79.4646906822562,10.9850777457989,136.150318886466));
#63551=CARTESIAN_POINT('Ctrl Pts',(79.5339622786307,11.0024696355473,136.146459483743));
#63552=CARTESIAN_POINT('Ctrl Pts',(79.6038873114516,11.0162074051225,136.142600081021));
#63553=CARTESIAN_POINT('Ctrl Pts',(79.6738519363753,11.0299529531309,136.138738493074));
#63554=CARTESIAN_POINT('Ctrl Pts',(79.7444702531338,11.0400401935167,136.134876905127));
#63555=CARTESIAN_POINT('Ctrl Pts',(79.8153292167478,11.0464345248048,136.13101531718));
#63556=CARTESIAN_POINT('Ctrl Pts',(79.8863121506584,11.0528400432047,136.127146973246));
#63557=CARTESIAN_POINT('Ctrl Pts',(79.9575360864153,11.0555397347778,136.123278629313));
#63558=CARTESIAN_POINT('Ctrl Pts',(80.0285870917953,11.0545511287585,136.119410285379));
#63559=CARTESIAN_POINT('Ctrl Pts',(80.0707751341203,11.0539641229538,136.117113374073));
#63560=CARTESIAN_POINT('Ctrl Pts',(80.1129022677807,11.0520777526687,136.114816462766));
#63561=CARTESIAN_POINT('Ctrl Pts',(80.1548831168876,11.0489042882973,136.11251955146));
#63562=CARTESIAN_POINT('Ctrl Pts',(80.2255915701654,11.0435592140074,136.108650857776));
#63563=CARTESIAN_POINT('Ctrl Pts',(80.2961614847426,11.0345391130104,136.104782164092));
#63564=CARTESIAN_POINT('Ctrl Pts',(80.3661804272609,11.021857922108,136.100913470407));
#63565=CARTESIAN_POINT('Ctrl Pts',(80.4361002562164,11.0091946817483,136.097050252956));
#63566=CARTESIAN_POINT('Ctrl Pts',(80.5054701866998,10.992880720234,136.093187035504));
#63567=CARTESIAN_POINT('Ctrl Pts',(80.5738817794949,10.9729818209157,136.089323818053));
#63568=CARTESIAN_POINT('Ctrl Pts',(80.6422141511607,10.9531059646696,136.085465074235));
#63569=CARTESIAN_POINT('Ctrl Pts',(80.7095899251634,10.9296535509445,136.081606330418));
#63570=CARTESIAN_POINT('Ctrl Pts',(80.7756115466406,10.9027412570336,136.077747586601));
#63571=CARTESIAN_POINT('Ctrl Pts',(80.8415882785372,10.8758472613947,136.07389146643));
#63572=CARTESIAN_POINT('Ctrl Pts',(80.9062122370559,10.8454982386467,136.070035346259));
#63573=CARTESIAN_POINT('Ctrl Pts',(80.9691031912758,10.81185997449,136.066179226088));
#63574=CARTESIAN_POINT('Ctrl Pts',(81.0319836313127,10.7782273340175,136.062323750588));
#63575=CARTESIAN_POINT('Ctrl Pts',(81.0931312103808,10.7413067658456,136.058468275088));
#63576=CARTESIAN_POINT('Ctrl Pts',(81.1521891448271,10.7013105939371,136.054612799588));
#63577=CARTESIAN_POINT('Ctrl Pts',(81.1861856897139,10.6782869026018,136.05239340524));
#63578=CARTESIAN_POINT('Ctrl Pts',(81.2194902550006,10.6542448950816,136.050174010892));
#63579=CARTESIAN_POINT('Ctrl Pts',(81.252039109102,10.6292316077768,136.047954616544));
#63580=CARTESIAN_POINT('',(77.9452507823625,9.00179307496101,136.35407471951));
#63581=CARTESIAN_POINT('Ctrl Pts',(77.9452507823632,9.00179307584224,136.354074719462));
#63582=CARTESIAN_POINT('Ctrl Pts',(77.9453413919223,9.10562578405504,136.348435142862));
#63583=CARTESIAN_POINT('Ctrl Pts',(77.9533058453993,9.20912640739788,136.342795566262));
#63584=CARTESIAN_POINT('Ctrl Pts',(77.968974501846,9.31134063073801,136.337155989661));
#63585=CARTESIAN_POINT('Ctrl Pts',(77.9731872821066,9.3388226336721,136.3356396952));
#63586=CARTESIAN_POINT('Ctrl Pts',(77.9779567533559,9.36621181729645,136.334123400739));
#63587=CARTESIAN_POINT('Ctrl Pts',(77.9832790921584,9.39348995206298,136.332607106279));
#63588=CARTESIAN_POINT('Ctrl Pts',(77.9968599435676,9.46309474588194,136.328738023432));
#63589=CARTESIAN_POINT('Ctrl Pts',(78.014075118604,9.53213195238462,136.324868940585));
#63590=CARTESIAN_POINT('Ctrl Pts',(78.0348625104968,9.6001934770131,136.320999857738));
#63591=CARTESIAN_POINT('Ctrl Pts',(78.0556189302125,9.66815359336439,136.317136539631));
#63592=CARTESIAN_POINT('Ctrl Pts',(78.0799368611766,9.73514045261806,136.313273221525));
#63593=CARTESIAN_POINT('Ctrl Pts',(78.1077031799501,9.80075608479058,136.309409903418));
#63594=CARTESIAN_POINT('Ctrl Pts',(78.1354369288423,9.86629474985172,136.305551116983));
#63595=CARTESIAN_POINT('Ctrl Pts',(78.1666108424928,9.93046493755091,136.301692330547));
#63596=CARTESIAN_POINT('Ctrl Pts',(78.2010625289044,9.99288546045757,136.297833544111));
#63597=CARTESIAN_POINT('Ctrl Pts',(78.2354925132797,10.0552666630119,136.293977188428));
#63598=CARTESIAN_POINT('Ctrl Pts',(78.2731959397889,10.1158999631443,136.290120832745));
#63599=CARTESIAN_POINT('Ctrl Pts',(78.3139636374603,10.1744270716796,136.286264477061));
#63600=CARTESIAN_POINT('Ctrl Pts',(78.3547192919456,10.232936890721,136.282409260584));
#63601=CARTESIAN_POINT('Ctrl Pts',(78.398537142981,10.2893413549905,136.278554044107));
#63602=CARTESIAN_POINT('Ctrl Pts',(78.4451646335606,10.343311038356,136.27469882763));
#63603=CARTESIAN_POINT('Ctrl Pts',(78.4917939471356,10.3972828317747,136.270843460425));
#63604=CARTESIAN_POINT('Ctrl Pts',(78.5412327990926,10.4488192891436,136.26698809322));
#63605=CARTESIAN_POINT('Ctrl Pts',(78.5931894143111,10.4976252997641,136.263132726016));
#63606=CARTESIAN_POINT('Ctrl Pts',(78.6452004139378,10.546482396969,136.259273323293));
#63607=CARTESIAN_POINT('Ctrl Pts',(78.6997340829046,10.592603008872,136.25541392057));
#63608=CARTESIAN_POINT('Ctrl Pts',(78.7564636241796,10.6357306760318,136.251554517847));
#63609=CARTESIAN_POINT('Ctrl Pts',(78.8132252861664,10.6788827624155,136.2476929299));
#63610=CARTESIAN_POINT('Ctrl Pts',(78.8721848938307,10.7190382569895,136.243831341954));
#63611=CARTESIAN_POINT('Ctrl Pts',(78.9329868490235,10.7559841964389,136.239969754007));
#63612=CARTESIAN_POINT('Ctrl Pts',(78.9938951794163,10.7929947741337,136.236101410073));
#63613=CARTESIAN_POINT('Ctrl Pts',(79.056651864793,10.8267843553657,136.23223306614));
#63614=CARTESIAN_POINT('Ctrl Pts',(79.1208775529789,10.8571863895806,136.228364722206));
#63615=CARTESIAN_POINT('Ctrl Pts',(79.1590129183693,10.8752382426031,136.2260678109));
#63616=CARTESIAN_POINT('Ctrl Pts',(79.1976658166299,10.8920966897238,136.223770899593));
#63617=CARTESIAN_POINT('Ctrl Pts',(79.2367541927435,10.9077351493867,136.221473988287));
#63618=CARTESIAN_POINT('Ctrl Pts',(79.3025974689341,10.9340776972527,136.21760490544));
#63619=CARTESIAN_POINT('Ctrl Pts',(79.3699350818583,10.9570590814341,136.213735822593));
#63620=CARTESIAN_POINT('Ctrl Pts',(79.4383904922891,10.9765101374263,136.209866739746));
#63621=CARTESIAN_POINT('Ctrl Pts',(79.5067439075725,10.9959322123151,136.20600342164));
#63622=CARTESIAN_POINT('Ctrl Pts',(79.5762113509863,11.0118342683011,136.202140103533));
#63623=CARTESIAN_POINT('Ctrl Pts',(79.6463971188564,11.0240954930405,136.198276785427));
#63624=CARTESIAN_POINT('Ctrl Pts',(79.7165005588477,11.036342335368,136.194417998991));
#63625=CARTESIAN_POINT('Ctrl Pts',(79.7873201734043,11.0449567462995,136.190559212555));
#63626=CARTESIAN_POINT('Ctrl Pts',(79.8584476361334,11.0498684081628,136.186700426119));
#63627=CARTESIAN_POINT('Ctrl Pts',(79.9295302937766,11.0547769760392,136.182844070436));
#63628=CARTESIAN_POINT('Ctrl Pts',(80.0009199313711,11.0559873890258,136.178987714753));
#63629=CARTESIAN_POINT('Ctrl Pts',(80.0722020881111,11.0534810495771,136.17513135907));
#63630=CARTESIAN_POINT('Ctrl Pts',(80.1434631873882,11.0509754505262,136.171276142592));
#63631=CARTESIAN_POINT('Ctrl Pts',(80.2146163836265,11.0447552958678,136.167420926115));
#63632=CARTESIAN_POINT('Ctrl Pts',(80.285247933086,11.0348540928455,136.163565709638));
#63633=CARTESIAN_POINT('Ctrl Pts',(80.3558822440277,11.0249525027158,136.159710342433));
#63634=CARTESIAN_POINT('Ctrl Pts',(80.4259943869258,11.0113696481118,136.155854975229));
#63635=CARTESIAN_POINT('Ctrl Pts',(80.4951781764376,10.9941905967284,136.151999608024));
#63636=CARTESIAN_POINT('Ctrl Pts',(80.5644343825115,10.9769935635627,136.148140205301));
#63637=CARTESIAN_POINT('Ctrl Pts',(80.6327598229711,10.9561929366659,136.144280802578));
#63638=CARTESIAN_POINT('Ctrl Pts',(80.6997617894777,10.9319241704806,136.140421399856));
#63639=CARTESIAN_POINT('Ctrl Pts',(80.7668016930241,10.9076416631292,136.136559811909));
#63640=CARTESIAN_POINT('Ctrl Pts',(80.832516183151,10.8798872964858,136.132698223962));
#63641=CARTESIAN_POINT('Ctrl Pts',(80.8965334728954,10.8488443132071,136.128836636015));
#63642=CARTESIAN_POINT('Ctrl Pts',(80.9606627631828,10.8177470191164,136.124968292081));
#63643=CARTESIAN_POINT('Ctrl Pts',(81.0230884991667,10.7833498557715,136.121099948148));
#63644=CARTESIAN_POINT('Ctrl Pts',(81.0834650030633,10.7458811957396,136.117231604214));
#63645=CARTESIAN_POINT('Ctrl Pts',(81.1193148335926,10.7236333836668,136.114934692908));
#63646=CARTESIAN_POINT('Ctrl Pts',(81.1544427439925,10.7003034952357,136.112637781602));
#63647=CARTESIAN_POINT('Ctrl Pts',(81.188781897192,10.6759460502679,136.110340870295));
#63648=CARTESIAN_POINT('Ctrl Pts',(81.210148038287,10.6607906210448,136.108911710678));
#63649=CARTESIAN_POINT('Ctrl Pts',(81.2312397268701,10.6452156089926,136.10748255106));
#63650=CARTESIAN_POINT('Ctrl Pts',(81.252039109102,10.6292316077768,136.106053391442));
#63651=CARTESIAN_POINT('Ctrl Pts',(81.252039109102,10.6292316077768,136.806140361941));
#63652=CARTESIAN_POINT('Ctrl Pts',(81.3085695498613,10.5857888447297,136.802278511158));
#63653=CARTESIAN_POINT('Ctrl Pts',(81.3627835829033,10.5394409897777,136.798416660376));
#63654=CARTESIAN_POINT('Ctrl Pts',(81.4143830440724,10.4904758190391,136.794554809593));
#63655=CARTESIAN_POINT('Ctrl Pts',(81.466071309253,10.4414263779713,136.790686312465));
#63656=CARTESIAN_POINT('Ctrl Pts',(81.5151356865827,10.3897509821785,136.786817815337));
#63657=CARTESIAN_POINT('Ctrl Pts',(81.5613166914088,10.3357723427396,136.782949318209));
#63658=CARTESIAN_POINT('Ctrl Pts',(81.5844350256915,10.3087504917564,136.781012738221));
#63659=CARTESIAN_POINT('Ctrl Pts',(81.6068314366704,10.2811519287676,136.779076158233));
#63660=CARTESIAN_POINT('Ctrl Pts',(81.6284774886263,10.2530198049262,136.777139578245));
#63661=CARTESIAN_POINT('Ctrl Pts',(81.671724020576,10.1968147844913,136.773270495398));
#63662=CARTESIAN_POINT('Ctrl Pts',(81.7121420629603,10.1382581453866,136.769401412551));
#63663=CARTESIAN_POINT('Ctrl Pts',(81.7494664792501,10.0776662750964,136.765532329704));
#63664=CARTESIAN_POINT('Ctrl Pts',(81.7867352840212,10.0171646836711,136.761669011597));
#63665=CARTESIAN_POINT('Ctrl Pts',(81.8209193594216,9.95463429051528,136.757805693491));
#63666=CARTESIAN_POINT('Ctrl Pts',(81.8517948922017,9.89042306782545,136.753942375384));
#63667=CARTESIAN_POINT('Ctrl Pts',(81.8826342079938,9.82628716487507,136.750083588949));
#63668=CARTESIAN_POINT('Ctrl Pts',(81.9101724804935,9.76047478435637,136.746224802513));
#63669=CARTESIAN_POINT('Ctrl Pts',(81.9342310595732,9.69335977001998,136.742366016077));
#63670=CARTESIAN_POINT('Ctrl Pts',(81.9582744835123,9.62628703322128,136.738509660393));
#63671=CARTESIAN_POINT('Ctrl Pts',(81.9788423992928,9.55791374679973,136.73465330471));
#63672=CARTESIAN_POINT('Ctrl Pts',(81.9958042626972,9.48863371506656,136.730796949027));
#63673=CARTESIAN_POINT('Ctrl Pts',(82.0127611153972,9.41937414934849,136.72694173255));
#63674=CARTESIAN_POINT('Ctrl Pts',(82.0261139151062,9.34920884168869,136.723086516072));
#63675=CARTESIAN_POINT('Ctrl Pts',(82.0357824558692,9.27854506794288,136.719231299595));
#63676=CARTESIAN_POINT('Ctrl Pts',(82.0454513746432,9.20787853145486,136.71537593239));
#63677=CARTESIAN_POINT('Ctrl Pts',(82.0514356848208,9.13671397178629,136.711520565186));
#63678=CARTESIAN_POINT('Ctrl Pts',(82.0537068542763,9.06546540459287,136.707665197981));
#63679=CARTESIAN_POINT('Ctrl Pts',(82.0559804010269,8.99414225957815,136.703805795258));
#63680=CARTESIAN_POINT('Ctrl Pts',(82.0545330329303,8.92273541803588,136.699946392535));
#63681=CARTESIAN_POINT('Ctrl Pts',(82.0493883707933,8.85165962061112,136.696086989812));
#63682=CARTESIAN_POINT('Ctrl Pts',(82.0442407957081,8.78054357951155,136.692225401865));
#63683=CARTESIAN_POINT('Ctrl Pts',(82.0353918194841,8.7097594379235,136.688363813918));
#63684=CARTESIAN_POINT('Ctrl Pts',(82.022916738459,8.63971479108562,136.684502225971));
#63685=CARTESIAN_POINT('Ctrl Pts',(82.0104198318325,8.56954759862744,136.680633882038));
#63686=CARTESIAN_POINT('Ctrl Pts',(81.9942842644375,8.5001229572938,136.676765538104));
#63687=CARTESIAN_POINT('Ctrl Pts',(81.9746358599067,8.43183560189818,136.672897194171));
#63688=CARTESIAN_POINT('Ctrl Pts',(81.9629692027315,8.39128853541449,136.670600282865));
#63689=CARTESIAN_POINT('Ctrl Pts',(81.9500649911237,8.35114211458861,136.668303371559));
#63690=CARTESIAN_POINT('Ctrl Pts',(81.9359575268556,8.31147547849692,136.666006460253));
#63691=CARTESIAN_POINT('Ctrl Pts',(81.9121938979013,8.24465813953113,136.662137377406));
#63692=CARTESIAN_POINT('Ctrl Pts',(81.8849204792403,8.17894163652207,136.658268294559));
#63693=CARTESIAN_POINT('Ctrl Pts',(81.8542592736281,8.11472032178283,136.654399211712));
#63694=CARTESIAN_POINT('Ctrl Pts',(81.8236437516831,8.05059469359969,136.650535893606));
#63695=CARTESIAN_POINT('Ctrl Pts',(81.7896506697925,7.9879602664643,136.6466725755));
#63696=CARTESIAN_POINT('Ctrl Pts',(81.7524509790067,7.92719380656225,136.642809257393));
#63697=CARTESIAN_POINT('Ctrl Pts',(81.7152949234439,7.86649862569425,136.638950470957));
#63698=CARTESIAN_POINT('Ctrl Pts',(81.6749399827042,7.80766747204671,136.635091684522));
#63699=CARTESIAN_POINT('Ctrl Pts',(81.6316033389748,7.75105320099439,136.631232898086));
#63700=CARTESIAN_POINT('Ctrl Pts',(81.5882939941532,7.69447459278149,136.627376542403));
#63701=CARTESIAN_POINT('Ctrl Pts',(81.5420069673465,7.6401104814134,136.623520186719));
#63702=CARTESIAN_POINT('Ctrl Pts',(81.4930023019681,7.58828413311394,136.619663831036));
#63703=CARTESIAN_POINT('Ctrl Pts',(81.4440121130586,7.53647309483671,136.615808614559));
#63704=CARTESIAN_POINT('Ctrl Pts',(81.3923062129687,7.48719868408667,136.611953398082));
#63705=CARTESIAN_POINT('Ctrl Pts',(81.3381832654851,7.44074918294852,136.608098181605));
#63706=CARTESIAN_POINT('Ctrl Pts',(81.2840582019561,7.39429786577382,136.6042428144));
#63707=CARTESIAN_POINT('Ctrl Pts',(81.2275162734895,7.35067199218708,136.600387447195));
#63708=CARTESIAN_POINT('Ctrl Pts',(81.1688898330687,7.31012008691486,136.596532079991));
#63709=CARTESIAN_POINT('Ctrl Pts',(81.1102020267514,7.26952573485577,136.592672677268));
#63710=CARTESIAN_POINT('Ctrl Pts',(81.0494257532267,7.23201205108959,136.588813274545));
#63711=CARTESIAN_POINT('Ctrl Pts',(80.9869222612898,7.19778413815918,136.584953871822));
#63712=CARTESIAN_POINT('Ctrl Pts',(80.9243833793848,7.1635368451156,136.581092283876));
#63713=CARTESIAN_POINT('Ctrl Pts',(80.860115770103,7.13257923736585,136.577230695929));
#63714=CARTESIAN_POINT('Ctrl Pts',(80.7945027069386,7.10506912760196,136.573369107982));
#63715=CARTESIAN_POINT('Ctrl Pts',(80.7287748513684,7.07751088791499,136.569500764048));
#63716=CARTESIAN_POINT('Ctrl Pts',(80.6616972995672,7.05341235261474,136.565632420115));
#63717=CARTESIAN_POINT('Ctrl Pts',(80.5936699255708,7.0328819094999,136.561764076181));
#63718=CARTESIAN_POINT('Ctrl Pts',(80.5532772285471,7.0206915231924,136.559467164875));
#63719=CARTESIAN_POINT('Ctrl Pts',(80.5125499020234,7.00975814962006,136.557170253568));
#63720=CARTESIAN_POINT('Ctrl Pts',(80.4715730379618,7.00009589420705,136.554873342262));
#63721=CARTESIAN_POINT('Ctrl Pts',(80.4025486566506,6.98382009523546,136.551004259415));
#63722=CARTESIAN_POINT('Ctrl Pts',(80.3325454831749,6.97109005845098,136.547135176568));
#63723=CARTESIAN_POINT('Ctrl Pts',(80.2619609978507,6.96201717423697,136.543266093721));
#63724=CARTESIAN_POINT('Ctrl Pts',(80.1914816798895,6.95295780816795,136.539402775615));
#63725=CARTESIAN_POINT('Ctrl Pts',(80.1204232472092,6.947544840033,136.535539457508));
#63726=CARTESIAN_POINT('Ctrl Pts',(80.0491949540305,6.94583899876423,136.531676139402));
#63727=CARTESIAN_POINT('Ctrl Pts',(79.9780502116122,6.94413515844662,136.527817352966));
#63728=CARTESIAN_POINT('Ctrl Pts',(79.906736487753,6.94612981905869,136.52395856653));
#63729=CARTESIAN_POINT('Ctrl Pts',(79.8356680232693,6.95183190047209,136.520099780094));
#63730=CARTESIAN_POINT('Ctrl Pts',(79.7646443267069,6.95753038999231,136.516243424411));
#63731=CARTESIAN_POINT('Ctrl Pts',(79.6938660660859,6.96693162815089,136.512387068728));
#63732=CARTESIAN_POINT('Ctrl Pts',(79.6237458704835,6.97999247711257,136.508530713045));
#63733=CARTESIAN_POINT('Ctrl Pts',(79.5536463890891,6.99304946776869,136.504675496567));
#63734=CARTESIAN_POINT('Ctrl Pts',(79.4842050640865,7.00976383406735,136.50082028009));
#63735=CARTESIAN_POINT('Ctrl Pts',(79.4158260801511,7.03004101721169,136.496965063613));
#63736=CARTESIAN_POINT('Ctrl Pts',(79.3474444228019,7.05031899313324,136.493109696408));
#63737=CARTESIAN_POINT('Ctrl Pts',(79.2801256540914,7.07415992223124,136.489254329204));
#63738=CARTESIAN_POINT('Ctrl Pts',(79.2142588295807,7.10141937869151,136.485398961999));
#63739=CARTESIAN_POINT('Ctrl Pts',(79.1483230604658,7.12870736836938,136.481539559276));
#63740=CARTESIAN_POINT('Ctrl Pts',(79.0838427191725,7.15942084228506,136.477680156553));
#63741=CARTESIAN_POINT('Ctrl Pts',(79.0211860533687,7.19336754695926,136.473820753831));
#63742=CARTESIAN_POINT('Ctrl Pts',(78.9584939108685,7.22733347252431,136.469959165884));
#63743=CARTESIAN_POINT('Ctrl Pts',(78.8976279140908,7.26453601970387,136.466097577937));
#63744=CARTESIAN_POINT('Ctrl Pts',(78.8389285266988,7.30473878225623,136.46223598999));
#63745=CARTESIAN_POINT('Ctrl Pts',(78.7801264426245,7.34501188098269,136.458367646056));
#63746=CARTESIAN_POINT('Ctrl Pts',(78.7234989219706,7.38829537973079,136.454499302123));
#63747=CARTESIAN_POINT('Ctrl Pts',(78.6693539087197,7.43431211850494,136.45063095819));
#63748=CARTESIAN_POINT('Ctrl Pts',(78.637204158008,7.46163553374357,136.448334046883));
#63749=CARTESIAN_POINT('Ctrl Pts',(78.6059289688188,7.48992186126369,136.446037135576));
#63750=CARTESIAN_POINT('Ctrl Pts',(78.5755863437912,7.51910726299782,136.44374022427));
#63751=CARTESIAN_POINT('Ctrl Pts',(78.5252398783668,7.5675335879439,136.439929038996));
#63752=CARTESIAN_POINT('Ctrl Pts',(78.4772533655963,7.61863876644744,136.436117853722));
#63753=CARTESIAN_POINT('Ctrl Pts',(78.4319314969755,7.67216012549613,136.432306668448));
#63754=CARTESIAN_POINT('Ctrl Pts',(78.3866698572083,7.72561035927573,136.428500547911));
#63755=CARTESIAN_POINT('Ctrl Pts',(78.3440661660634,7.78147003319481,136.424694427373));
#63756=CARTESIAN_POINT('Ctrl Pts',(78.3043895848261,7.83943854860947,136.420888306836));
#63757=CARTESIAN_POINT('Ctrl Pts',(78.264751534915,7.8973507687559,136.417085882556));
#63758=CARTESIAN_POINT('Ctrl Pts',(78.2280352419786,7.95736735964087,136.413283458277));
#63759=CARTESIAN_POINT('Ctrl Pts',(78.1944694698458,8.0191549219264,136.409481033997));
#63760=CARTESIAN_POINT('Ctrl Pts',(78.1609242933764,8.08090457190576,136.405680942852));
#63761=CARTESIAN_POINT('Ctrl Pts',(78.1305260421692,8.14442259847235,136.401880851706));
#63762=CARTESIAN_POINT('Ctrl Pts',(78.1034589744871,8.20934855906894,136.398080760561));
#63763=CARTESIAN_POINT('Ctrl Pts',(78.0763869021232,8.27428652442972,136.394279966781));
#63764=CARTESIAN_POINT('Ctrl Pts',(78.0526474523865,8.34063248743644,136.390479173001));
#63765=CARTESIAN_POINT('Ctrl Pts',(78.0323772815507,8.40800472945968,136.386678379222));
#63766=CARTESIAN_POINT('Ctrl Pts',(78.0121062978094,8.47537967334783,136.382877433017));
#63767=CARTESIAN_POINT('Ctrl Pts',(77.9953050033774,8.5437804942492,136.379076486812));
#63768=CARTESIAN_POINT('Ctrl Pts',(77.9820598198688,8.61281142590203,136.375275540607));
#63769=CARTESIAN_POINT('Ctrl Pts',(77.9687990309018,8.68192368971067,136.371470116132));
#63770=CARTESIAN_POINT('Ctrl Pts',(77.9591028023244,8.75166705108641,136.367664691657));
#63771=CARTESIAN_POINT('Ctrl Pts',(77.9530059961544,8.82163769815253,136.363859267182));
#63772=CARTESIAN_POINT('Ctrl Pts',(77.9477806053111,8.88160745416809,136.360597751291));
#63773=CARTESIAN_POINT('Ctrl Pts',(77.9451983804903,8.9417438812321,136.357336235401));
#63774=CARTESIAN_POINT('Ctrl Pts',(77.9452507823624,9.00179307496101,136.35407471951));
#63775=CARTESIAN_POINT('Origin',(80.,9.,141.545925280538));
#63776=CARTESIAN_POINT('',(81.252039109102,10.6292316077768,137.506056941317));
#63777=CARTESIAN_POINT('',(81.252039109102,10.6292316077768,137.447938223076));
#63778=CARTESIAN_POINT('',(81.252039109102,10.6292316077768,141.545925280538));
#63779=CARTESIAN_POINT('',(77.9452500969073,8.99936893701588,136.9959252805));
#63780=CARTESIAN_POINT('Ctrl Pts',(81.252039109102,10.6292316077768,137.447938223076));
#63781=CARTESIAN_POINT('Ctrl Pts',(81.2608674552356,10.6224471613082,137.447331137836));
#63782=CARTESIAN_POINT('Ctrl Pts',(81.2696380418088,10.6155929637395,137.446724052597));
#63783=CARTESIAN_POINT('Ctrl Pts',(81.2783497233123,10.608670117646,137.446116967358));
#63784=CARTESIAN_POINT('Ctrl Pts',(81.3338711151904,10.5645493528188,137.442247884512));
#63785=CARTESIAN_POINT('Ctrl Pts',(81.387214404888,10.5174644128168,137.438378801666));
#63786=CARTESIAN_POINT('Ctrl Pts',(81.4380459985658,10.4676584304629,137.43450971882));
#63787=CARTESIAN_POINT('Ctrl Pts',(81.488801855704,10.417926656539,137.430646400714));
#63788=CARTESIAN_POINT('Ctrl Pts',(81.5370531010316,10.3654822249852,137.426783082609));
#63789=CARTESIAN_POINT('Ctrl Pts',(81.5824986302668,10.3106088843373,137.422919764503));
#63790=CARTESIAN_POINT('Ctrl Pts',(81.6278908519133,10.2557999100972,137.419060978068));
#63791=CARTESIAN_POINT('Ctrl Pts',(81.6704835863644,10.1985680583769,137.415202191633));
#63792=CARTESIAN_POINT('Ctrl Pts',(81.710013322863,10.1392330745423,137.411343405199));
#63793=CARTESIAN_POINT('Ctrl Pts',(81.7495181585261,10.0799354673968,137.407487049516));
#63794=CARTESIAN_POINT('Ctrl Pts',(81.785963555563,10.018537759882,137.403630693834));
#63795=CARTESIAN_POINT('Ctrl Pts',(81.8191278778125,9.95539066703914,137.399774338151));
#63796=CARTESIAN_POINT('Ctrl Pts',(81.8522824029889,9.89226222848004,137.395919121675));
#63797=CARTESIAN_POINT('Ctrl Pts',(81.8821575518827,9.82738586039962,137.392063905199));
#63798=CARTESIAN_POINT('Ctrl Pts',(81.9085772938752,9.76113748810835,137.388208688723));
#63799=CARTESIAN_POINT('Ctrl Pts',(81.9349980688006,9.69488652570406,137.384353321519));
#63800=CARTESIAN_POINT('Ctrl Pts',(81.9579629907077,9.62726390463224,137.380497954315));
#63801=CARTESIAN_POINT('Ctrl Pts',(81.9773445536542,9.55866454929059,137.376642587112));
#63802=CARTESIAN_POINT('Ctrl Pts',(81.996746403812,9.48999338913019,137.37278318439));
#63803=CARTESIAN_POINT('Ctrl Pts',(82.0125572752226,9.42034392225216,137.368923781668));
#63804=CARTESIAN_POINT('Ctrl Pts',(82.0247001017077,9.35012435026009,137.365064378946));
#63805=CARTESIAN_POINT('Ctrl Pts',(82.0368498035564,9.27986501939488,137.361202791));
#63806=CARTESIAN_POINT('Ctrl Pts',(82.0453272683025,9.2090354233933,137.357341203054));
#63807=CARTESIAN_POINT('Ctrl Pts',(82.0501073036935,9.13804928772871,137.353479615108));
#63808=CARTESIAN_POINT('Ctrl Pts',(82.0548957019278,9.06693895927535,137.349611271176));
#63809=CARTESIAN_POINT('Ctrl Pts',(82.0559737483448,8.99567203024745,137.345742927243));
#63810=CARTESIAN_POINT('Ctrl Pts',(82.0533683880917,8.92466192671876,137.341874583311));
#63811=CARTESIAN_POINT('Ctrl Pts',(82.0518214001433,8.88249817057678,137.339577671996));
#63812=CARTESIAN_POINT('Ctrl Pts',(82.048976770436,8.84042487883738,137.337280760681));
#63813=CARTESIAN_POINT('Ctrl Pts',(82.0448487092084,8.7985271260225,137.334983849367));
#63814=CARTESIAN_POINT('Ctrl Pts',(82.0378951055635,8.72795153360239,137.331114766519));
#63815=CARTESIAN_POINT('Ctrl Pts',(82.0272698405453,8.65759812659177,137.327245683672));
#63816=CARTESIAN_POINT('Ctrl Pts',(82.0129962433474,8.58787903866796,137.323376600825));
#63817=CARTESIAN_POINT('Ctrl Pts',(81.9987439130975,8.51826382870794,137.319513282718));
#63818=CARTESIAN_POINT('Ctrl Pts',(81.9808541372858,8.44928153386452,137.315649964611));
#63819=CARTESIAN_POINT('Ctrl Pts',(81.9594019894066,8.38133902142668,137.311786646504));
#63820=CARTESIAN_POINT('Ctrl Pts',(81.9379750048886,8.3134762055296,137.307927860067));
#63821=CARTESIAN_POINT('Ctrl Pts',(81.9129940940925,8.24665121036451,137.304069073631));
#63822=CARTESIAN_POINT('Ctrl Pts',(81.884584962628,8.18125884362858,137.300210287195));
#63823=CARTESIAN_POINT('Ctrl Pts',(81.8561937268332,8.11590766928859,137.296353931511));
#63824=CARTESIAN_POINT('Ctrl Pts',(81.8243787479479,8.05198777742893,137.292497575827));
#63825=CARTESIAN_POINT('Ctrl Pts',(81.7893144621874,7.98987559285651,137.288641220143));
#63826=CARTESIAN_POINT('Ctrl Pts',(81.754260534768,7.9277817568453,137.284786003665));
#63827=CARTESIAN_POINT('Ctrl Pts',(81.7159594447802,7.86749499075219,137.280930787188));
#63828=CARTESIAN_POINT('Ctrl Pts',(81.6746315439692,7.80936707821282,137.27707557071));
#63829=CARTESIAN_POINT('Ctrl Pts',(81.6333020273608,7.75123689304586,137.273220203505));
#63830=CARTESIAN_POINT('Ctrl Pts',(81.5889457482664,7.6952661236463,137.269364836299));
#63831=CARTESIAN_POINT('Ctrl Pts',(81.5418253390223,7.64177609119524,137.265509469094));
#63832=CARTESIAN_POINT('Ctrl Pts',(81.4946556075587,7.58823006926622,137.261650066371));
#63833=CARTESIAN_POINT('Ctrl Pts',(81.4447162920577,7.5371703330557,137.257790663648));
#63834=CARTESIAN_POINT('Ctrl Pts',(81.3923085370104,7.48888302892592,137.253931260924));
#63835=CARTESIAN_POINT('Ctrl Pts',(81.3398711082804,7.44056838414523,137.250069672977));
#63836=CARTESIAN_POINT('Ctrl Pts',(81.2849628318099,7.39502960663895,137.246208085029));
#63837=CARTESIAN_POINT('Ctrl Pts',(81.2279176282723,7.35251225780639,137.242346497082));
#63838=CARTESIAN_POINT('Ctrl Pts',(81.1707726221064,7.30992052334813,137.238478153148));
#63839=CARTESIAN_POINT('Ctrl Pts',(81.1114836288105,7.27036104111439,137.234609809214));
#63840=CARTESIAN_POINT('Ctrl Pts',(81.0504125958221,7.23403540776204,137.23074146528));
#63841=CARTESIAN_POINT('Ctrl Pts',(81.0141503739873,7.2124662920871,137.228444553978));
#63842=CARTESIAN_POINT('Ctrl Pts',(80.9772603389442,7.19203643427558,137.226147642677));
#63843=CARTESIAN_POINT('Ctrl Pts',(80.9398216719651,7.17278003858192,137.223850731375));
#63844=CARTESIAN_POINT('Ctrl Pts',(80.8767572845332,7.14034317860384,137.219981648528));
#63845=CARTESIAN_POINT('Ctrl Pts',(80.8118881255422,7.11111151178797,137.216112565681));
#63846=CARTESIAN_POINT('Ctrl Pts',(80.745573095422,7.08528897170284,137.212243482835));
#63847=CARTESIAN_POINT('Ctrl Pts',(80.6793568713896,7.05950490591462,137.208380164728));
#63848=CARTESIAN_POINT('Ctrl Pts',(80.6116995013936,7.03712005916351,137.204516846622));
#63849=CARTESIAN_POINT('Ctrl Pts',(80.5429835264874,7.01829203653433,137.200653528516));
#63850=CARTESIAN_POINT('Ctrl Pts',(80.4743481553933,6.99948609916842,137.19679474208));
#63851=CARTESIAN_POINT('Ctrl Pts',(80.4046571121522,6.98422882636421,137.192935955644));
#63852=CARTESIAN_POINT('Ctrl Pts',(80.3343102680185,6.97262874460611,137.189077169208));
#63853=CARTESIAN_POINT('Ctrl Pts',(80.2640077372383,6.96103597004892,137.185220813525));
#63854=CARTESIAN_POINT('Ctrl Pts',(80.1930507033395,6.95309589476036,137.181364457842));
#63855=CARTESIAN_POINT('Ctrl Pts',(80.1218500240238,6.94886613451355,137.177508102159));
#63856=CARTESIAN_POINT('Ctrl Pts',(80.0506703781018,6.94463762378026,137.173652885682));
#63857=CARTESIAN_POINT('Ctrl Pts',(79.9792477143178,6.94411728088903,137.169797669205));
#63858=CARTESIAN_POINT('Ctrl Pts',(79.9079970921904,6.94731078157102,137.165942452728));
#63859=CARTESIAN_POINT('Ctrl Pts',(79.8367436843767,6.95050440710934,137.162087085523));
#63860=CARTESIAN_POINT('Ctrl Pts',(79.7656628167711,6.9574121405448,137.158231718318));
#63861=CARTESIAN_POINT('Ctrl Pts',(79.6951668885367,6.96798761404966,137.154376351114));
#63862=CARTESIAN_POINT('Ctrl Pts',(79.6245971702888,6.97857415719149,137.150516948391));
#63863=CARTESIAN_POINT('Ctrl Pts',(79.5546140950361,6.9928360319378,137.146657545668));
#63864=CARTESIAN_POINT('Ctrl Pts',(79.485621398648,7.01067543699598,137.142798142946));
#63865=CARTESIAN_POINT('Ctrl Pts',(79.4165896380533,7.02852494286543,137.138936554999));
#63866=CARTESIAN_POINT('Ctrl Pts',(79.3485498361858,7.04995586543194,137.135074967052));
#63867=CARTESIAN_POINT('Ctrl Pts',(79.2818894093015,7.07482085456273,137.131213379105));
#63868=CARTESIAN_POINT('Ctrl Pts',(79.2151123576109,7.09972934588327,137.127345035172));
#63869=CARTESIAN_POINT('Ctrl Pts',(79.1497199448873,7.12808370564152,137.123476691238));
#63870=CARTESIAN_POINT('Ctrl Pts',(79.0860778523175,7.15968919188213,137.119608347305));
#63871=CARTESIAN_POINT('Ctrl Pts',(79.0482890091985,7.17845562009058,137.117311435998));
#63872=CARTESIAN_POINT('Ctrl Pts',(79.0111167807685,7.19836740599221,137.115014524691));
#63873=CARTESIAN_POINT('Ctrl Pts',(78.9746328495175,7.21937657849519,137.112717613384));
#63874=CARTESIAN_POINT('Ctrl Pts',(78.9131766878652,7.25476594190127,137.108848530537));
#63875=CARTESIAN_POINT('Ctrl Pts',(78.8534344424327,7.29340998728555,137.10497944769));
#63876=CARTESIAN_POINT('Ctrl Pts',(78.7957721050869,7.3351178000792,137.101110364844));
#63877=CARTESIAN_POINT('Ctrl Pts',(78.7381956817479,7.37676347031184,137.097247046737));
#63878=CARTESIAN_POINT('Ctrl Pts',(78.6826934055512,7.42146356444802,137.093383728631));
#63879=CARTESIAN_POINT('Ctrl Pts',(78.6296051684808,7.46898217899156,137.089520410524));
#63880=CARTESIAN_POINT('Ctrl Pts',(78.576579203892,7.51644505421851,137.085661624089));
#63881=CARTESIAN_POINT('Ctrl Pts',(78.5259620139861,7.56671956035663,137.081802837653));
#63882=CARTESIAN_POINT('Ctrl Pts',(78.4780616577513,7.61952861496759,137.077944051217));
#63883=CARTESIAN_POINT('Ctrl Pts',(78.4301914752286,7.67230440374645,137.074087695534));
#63884=CARTESIAN_POINT('Ctrl Pts',(78.3850350565734,7.72761121444358,137.070231339851));
#63885=CARTESIAN_POINT('Ctrl Pts',(78.3428636478342,7.78513512157504,137.066374984168));
#63886=CARTESIAN_POINT('Ctrl Pts',(78.3007046969514,7.8426420355683,137.062519767691));
#63887=CARTESIAN_POINT('Ctrl Pts',(78.2615292924246,7.90236435416734,137.058664551214));
#63888=CARTESIAN_POINT('Ctrl Pts',(78.2255673227379,7.96395645054636,137.054809334737));
#63889=CARTESIAN_POINT('Ctrl Pts',(78.1896039470457,8.02555095499218,137.050953967532));
#63890=CARTESIAN_POINT('Ctrl Pts',(78.1568544986653,8.08901496173253,137.047098600327));
#63891=CARTESIAN_POINT('Ctrl Pts',(78.1275036996412,8.15397685159183,137.043243233123));
#63892=CARTESIAN_POINT('Ctrl Pts',(78.098122178334,8.21900673883551,137.0393838304));
#63893=CARTESIAN_POINT('Ctrl Pts',(78.0721466082949,8.28553719542662,137.035524427677));
#63894=CARTESIAN_POINT('Ctrl Pts',(78.049713801813,8.35317598401014,137.031665024955));
#63895=CARTESIAN_POINT('Ctrl Pts',(78.0272682936998,8.42085307020704,137.027803437008));
#63896=CARTESIAN_POINT('Ctrl Pts',(78.008369671111,8.48963926900039,137.023941849061));
#63897=CARTESIAN_POINT('Ctrl Pts',(77.993104267279,8.55912917936653,137.020080261114));
#63898=CARTESIAN_POINT('Ctrl Pts',(77.9778121560757,8.62874066482163,137.016211917181));
#63899=CARTESIAN_POINT('Ctrl Pts',(77.9661660338546,8.6990578405065,137.012343573247));
#63900=CARTESIAN_POINT('Ctrl Pts',(77.9582006297367,8.76966786135613,137.008475229314));
#63901=CARTESIAN_POINT('Ctrl Pts',(77.953471001994,8.81159405977307,137.006178318007));
#63902=CARTESIAN_POINT('Ctrl Pts',(77.9500380668079,8.85362343926592,137.003881406699));
#63903=CARTESIAN_POINT('Ctrl Pts',(77.9479004012491,8.89566975842765,137.001584495392));
#63904=CARTESIAN_POINT('Ctrl Pts',(77.9461447814819,8.93020151610125,136.999698090441));
#63905=CARTESIAN_POINT('Ctrl Pts',(77.9452607206379,8.96477795933226,136.997811685489));
#63906=CARTESIAN_POINT('Ctrl Pts',(77.9452500969075,8.99936893632434,136.995925280538));
#63907=CARTESIAN_POINT('Ctrl Pts',(77.9452500969073,8.99936893701588,136.9959252805));
#63908=CARTESIAN_POINT('Ctrl Pts',(77.9452284795406,9.06975538523751,136.992086783991));
#63909=CARTESIAN_POINT('Ctrl Pts',(77.9488278088239,9.14028801803307,136.988248287481));
#63910=CARTESIAN_POINT('Ctrl Pts',(77.956066989778,9.2105597592725,136.984409790972));
#63911=CARTESIAN_POINT('Ctrl Pts',(77.9634503271985,9.28223084747754,136.980494857073));
#63912=CARTESIAN_POINT('Ctrl Pts',(77.9746201460017,9.3536300259173,136.976579923174));
#63913=CARTESIAN_POINT('Ctrl Pts',(77.9895405666956,9.42432349632931,136.972664989275));
#63914=CARTESIAN_POINT('Ctrl Pts',(78.0041321582483,9.49345896287313,136.968836336077));
#63915=CARTESIAN_POINT('Ctrl Pts',(78.0223106191684,9.56191899783839,136.965007682879));
#63916=CARTESIAN_POINT('Ctrl Pts',(78.0439901438108,9.62930358730175,136.961179029681));
#63917=CARTESIAN_POINT('Ctrl Pts',(78.0656575011448,9.69665035817348,136.957352525257));
#63918=CARTESIAN_POINT('Ctrl Pts',(78.0908218742363,9.76292241108565,136.953526020833));
#63919=CARTESIAN_POINT('Ctrl Pts',(78.1193471946889,9.82773340416793,136.949699516409));
#63920=CARTESIAN_POINT('Ctrl Pts',(78.1478664215463,9.89253055228909,136.945873829405));
#63921=CARTESIAN_POINT('Ctrl Pts',(78.1797449711962,9.95586680813673,136.942048142401));
#63922=CARTESIAN_POINT('Ctrl Pts',(78.2147987712682,10.0173761032354,136.938222455397));
#63923=CARTESIAN_POINT('Ctrl Pts',(78.2512749609402,10.0813812812762,136.934241532231));
#63924=CARTESIAN_POINT('Ctrl Pts',(78.2911893552542,10.1434075386599,136.930260609065));
#63925=CARTESIAN_POINT('Ctrl Pts',(78.3342831480841,10.2030731198657,136.926279685898));
#63926=CARTESIAN_POINT('Ctrl Pts',(78.3757481853333,10.2604836048734,136.922449224095));
#63927=CARTESIAN_POINT('Ctrl Pts',(78.4201562185496,10.3157083061125,136.918618762292));
#63928=CARTESIAN_POINT('Ctrl Pts',(78.467235362494,10.3684407654374,136.914788300489));
#63929=CARTESIAN_POINT('Ctrl Pts',(78.5143468858398,10.421209492318,136.910955204227));
#63930=CARTESIAN_POINT('Ctrl Pts',(78.5641328247557,10.4714822194488,136.907122107966));
#63931=CARTESIAN_POINT('Ctrl Pts',(78.6162853882316,10.5189902684608,136.903289011704));
#63932=CARTESIAN_POINT('Ctrl Pts',(78.6685215402371,10.566574461917,136.899449771873));
#63933=CARTESIAN_POINT('Ctrl Pts',(78.7231314966093,10.6113848335142,136.895610532042));
#63934=CARTESIAN_POINT('Ctrl Pts',(78.7797764230505,10.6531944788066,136.891771292212));
#63935=CARTESIAN_POINT('Ctrl Pts',(78.7862678537046,10.6579858066472,136.891331320608));
#63936=CARTESIAN_POINT('Ctrl Pts',(78.7927859814813,10.6627377753602,136.890891349004));
#63937=CARTESIAN_POINT('Ctrl Pts',(78.799330275612,10.6674500818429,136.8904513774));
#63938=CARTESIAN_POINT('Ctrl Pts',(78.8568803901065,10.7088898112004,136.886582294554));
#63939=CARTESIAN_POINT('Ctrl Pts',(78.9166911084278,10.747427793855,136.882713211707));
#63940=CARTESIAN_POINT('Ctrl Pts',(78.9784377823449,10.782809075016,136.87884412886));
#63941=CARTESIAN_POINT('Ctrl Pts',(79.0400924567972,10.8181376398326,136.874980810753));
#63942=CARTESIAN_POINT('Ctrl Pts',(79.1036769431804,10.8503185995815,136.871117492647));
#63943=CARTESIAN_POINT('Ctrl Pts',(79.1688363368494,10.8791393049899,136.867254174541));
#63944=CARTESIAN_POINT('Ctrl Pts',(79.2339192985749,10.9079262037222,136.863395388105));
#63945=CARTESIAN_POINT('Ctrl Pts',(79.3005730559833,10.9333604818709,136.859536601669));
#63946=CARTESIAN_POINT('Ctrl Pts',(79.3684182802395,10.9552754521459,136.855677815233));
#63947=CARTESIAN_POINT('Ctrl Pts',(79.4362207669791,10.9771766175966,136.85182145955));
#63948=CARTESIAN_POINT('Ctrl Pts',(79.5052127703407,10.9955627245148,136.847965103867));
#63949=CARTESIAN_POINT('Ctrl Pts',(79.574996538769,11.010315801172,136.844108748183));
#63950=CARTESIAN_POINT('Ctrl Pts',(79.6447596923733,11.0250645196225,136.840253531706));
#63951=CARTESIAN_POINT('Ctrl Pts',(79.7153136716781,11.0361822380541,136.836398315229));
#63952=CARTESIAN_POINT('Ctrl Pts',(79.7862488590477,11.043601725445,136.832543098752));
#63953=CARTESIAN_POINT('Ctrl Pts',(79.8571868197708,11.0510215029156,136.828687731547));
#63954=CARTESIAN_POINT('Ctrl Pts',(79.9285055347723,11.0547427139375,136.824832364343));
#63955=CARTESIAN_POINT('Ctrl Pts',(79.9997902910998,11.0547499892985,136.820976997138));
#63956=CARTESIAN_POINT('Ctrl Pts',(80.071149663129,11.0547572722748,136.817117594415));
#63957=CARTESIAN_POINT('Ctrl Pts',(80.1424745187492,11.0510428592633,136.813258191693));
#63958=CARTESIAN_POINT('Ctrl Pts',(80.2133510766842,11.0436435307014,136.80939878897));
#63959=CARTESIAN_POINT('Ctrl Pts',(80.284267765483,11.0362400125815,136.805537201023));
#63960=CARTESIAN_POINT('Ctrl Pts',(80.3547351711987,11.0251475010506,136.801675613076));
#63961=CARTESIAN_POINT('Ctrl Pts',(80.4243482954951,11.010454199083,136.797814025129));
#63962=CARTESIAN_POINT('Ctrl Pts',(80.4940832104478,10.9957351906568,136.793945681196));
#63963=CARTESIAN_POINT('Ctrl Pts',(80.5629603903896,10.977402939226,136.790077337262));
#63964=CARTESIAN_POINT('Ctrl Pts',(80.6305892955942,10.9555957411444,136.786208993329));
#63965=CARTESIAN_POINT('Ctrl Pts',(80.6707453933164,10.9426472544793,136.783912082022));
#63966=CARTESIAN_POINT('Ctrl Pts',(80.7104617445909,10.9284745615488,136.781615170716));
#63967=CARTESIAN_POINT('Ctrl Pts',(80.7496603396344,10.9131144601615,136.779318259409));
#63968=CARTESIAN_POINT('Ctrl Pts',(80.8156837929553,10.8872429477816,136.775449497882));
#63969=CARTESIAN_POINT('Ctrl Pts',(80.8804957013763,10.8578989545749,136.771580736354));
#63970=CARTESIAN_POINT('Ctrl Pts',(80.9437058827513,10.825216910222,136.767711974827));
#63971=CARTESIAN_POINT('Ctrl Pts',(81.0068160594629,10.7925865720466,136.763849334057));
#63972=CARTESIAN_POINT('Ctrl Pts',(81.0683291135876,10.7566288912025,136.759986693287));
#63973=CARTESIAN_POINT('Ctrl Pts',(81.1278740897059,10.7175265937592,136.756124052518));
#63974=CARTESIAN_POINT('Ctrl Pts',(81.1703036664166,10.6896637237559,136.753371675684));
#63975=CARTESIAN_POINT('Ctrl Pts',(81.2117343082329,10.6602052193443,136.75061929885));
#63976=CARTESIAN_POINT('Ctrl Pts',(81.252039109102,10.6292316077768,136.747866922016));
#63977=CARTESIAN_POINT('',(77.9452500020166,9.0000910330137,137.054074719424));
#63978=CARTESIAN_POINT('Ctrl Pts',(77.9452500020166,9.00009103301371,137.054074719424));
#63979=CARTESIAN_POINT('Ctrl Pts',(77.9452533307477,9.07522542642048,137.050023196181));
#63980=CARTESIAN_POINT('Ctrl Pts',(77.9493820167298,9.15027470161127,137.045971672937));
#63981=CARTESIAN_POINT('Ctrl Pts',(77.9575824977975,9.22478502885367,137.041920149694));
#63982=CARTESIAN_POINT('Ctrl Pts',(77.9658071971074,9.29951540527881,137.037856661204));
#63983=CARTESIAN_POINT('Ctrl Pts',(77.9781276780619,9.37370324566178,137.033793172715));
#63984=CARTESIAN_POINT('Ctrl Pts',(77.9944388833352,9.44690286396755,137.029729684225));
#63985=CARTESIAN_POINT('Ctrl Pts',(78.0107756928435,9.52021738611964,137.025659817145));
#63986=CARTESIAN_POINT('Ctrl Pts',(78.0311156065381,9.59254020057874,137.021589950064));
#63987=CARTESIAN_POINT('Ctrl Pts',(78.0553039258147,9.66344158864827,137.017520082983));
#63988=CARTESIAN_POINT('Ctrl Pts',(78.0795588774128,9.73453829099468,137.013439004512));
#63989=CARTESIAN_POINT('Ctrl Pts',(78.1076832711743,9.80420536132707,137.00935792604));
#63990=CARTESIAN_POINT('Ctrl Pts',(78.1394743984716,9.87203328408803,137.005276847569));
#63991=CARTESIAN_POINT('Ctrl Pts',(78.1547192877517,9.90455899992451,137.003319836455));
#63992=CARTESIAN_POINT('Ctrl Pts',(78.1708066784997,9.93666218503223,137.001362825341));
#63993=CARTESIAN_POINT('Ctrl Pts',(78.1877106415429,9.96829997610412,136.999405814228));
#63994=CARTESIAN_POINT('Ctrl Pts',(78.22113039731,10.0308490510122,136.995536731381));
#63995=CARTESIAN_POINT('Ctrl Pts',(78.2578576247283,10.0917884381047,136.991667648534));
#63996=CARTESIAN_POINT('Ctrl Pts',(78.2977131288889,10.1507462669689,136.987798565687));
#63997=CARTESIAN_POINT('Ctrl Pts',(78.337509250336,10.2096162516085,136.983935247581));
#63998=CARTESIAN_POINT('Ctrl Pts',(78.3804241267736,10.2665101393224,136.980071929474));
#63999=CARTESIAN_POINT('Ctrl Pts',(78.4262327681656,10.321080717634,136.976208611368));
#64000=CARTESIAN_POINT('Ctrl Pts',(78.4719876760388,10.3755872846782,136.972349824932));
#64001=CARTESIAN_POINT('Ctrl Pts',(78.5206292956546,10.4277755853078,136.968491038496));
#64002=CARTESIAN_POINT('Ctrl Pts',(78.571890467838,10.4773289162025,136.964632252061));
#64003=CARTESIAN_POINT('Ctrl Pts',(78.6231193492416,10.5268510321322,136.960775896378));
#64004=CARTESIAN_POINT('Ctrl Pts',(78.6769641609447,10.5737411345841,136.956919540694));
#64005=CARTESIAN_POINT('Ctrl Pts',(78.7331197501872,10.6177181445278,136.953063185011));
#64006=CARTESIAN_POINT('Ctrl Pts',(78.7892587505064,10.6616821632223,136.949207968534));
#64007=CARTESIAN_POINT('Ctrl Pts',(78.8477067909092,10.7027344985004,136.945352752057));
#64008=CARTESIAN_POINT('Ctrl Pts',(78.9081257198302,10.7406344012468,136.94149753558));
#64009=CARTESIAN_POINT('Ctrl Pts',(78.9685470109507,10.778535785766,136.937642168375));
#64010=CARTESIAN_POINT('Ctrl Pts',(79.0309389308829,10.8132842367812,136.933786801171));
#64011=CARTESIAN_POINT('Ctrl Pts',(79.094935914404,10.8446833233551,136.929931433966));
#64012=CARTESIAN_POINT('Ctrl Pts',(79.1589998853157,10.8761152762105,136.926072031243));
#64013=CARTESIAN_POINT('Ctrl Pts',(79.2246718365875,10.9041906517067,136.922212628521));
#64014=CARTESIAN_POINT('Ctrl Pts',(79.291564073675,10.928760249692,136.918353225798));
#64015=CARTESIAN_POINT('Ctrl Pts',(79.3584941856725,10.9533437591767,136.914491637851));
#64016=CARTESIAN_POINT('Ctrl Pts',(79.4266454946035,10.9744173960534,136.910630049904));
#64017=CARTESIAN_POINT('Ctrl Pts',(79.4956155457552,10.9918819957056,136.906768461957));
#64018=CARTESIAN_POINT('Ctrl Pts',(79.5647062624835,11.0093771503009,136.902900118024));
#64019=CARTESIAN_POINT('Ctrl Pts',(79.6346181046547,11.023250566727,136.899031774091));
#64020=CARTESIAN_POINT('Ctrl Pts',(79.7049395383999,11.0334544220366,136.895163430157));
#64021=CARTESIAN_POINT('Ctrl Pts',(79.7466943820955,11.0395131776799,136.89286651885));
#64022=CARTESIAN_POINT('Ctrl Pts',(79.7885935358452,11.0442791717332,136.890569607543));
#64023=CARTESIAN_POINT('Ctrl Pts',(79.8305507565544,11.0477510875093,136.888272696236));
#64024=CARTESIAN_POINT('Ctrl Pts',(79.9012083638594,11.053597930016,136.884404607397));
#64025=CARTESIAN_POINT('Ctrl Pts',(79.9723072994884,11.05579487151,136.880536518558));
#64026=CARTESIAN_POINT('Ctrl Pts',(80.0434382677727,11.0542907971835,136.876668429718));
#64027=CARTESIAN_POINT('Ctrl Pts',(80.1144716684088,11.0527887859386,136.87280564659));
#64028=CARTESIAN_POINT('Ctrl Pts',(80.1855365333495,11.0475958395282,136.868942863461));
#64029=CARTESIAN_POINT('Ctrl Pts',(80.2562193003067,11.0387126410189,136.865080080333));
#64030=CARTESIAN_POINT('Ctrl Pts',(80.3268287676256,11.0298386545887,136.861221302998));
#64031=CARTESIAN_POINT('Ctrl Pts',(80.3970564438634,11.0172820708638,136.857362525663));
#64032=CARTESIAN_POINT('Ctrl Pts',(80.4664913551483,11.0010955444636,136.853503748329));
#64033=CARTESIAN_POINT('Ctrl Pts',(80.5375128266071,10.9845391623572,136.849556799463));
#64034=CARTESIAN_POINT('Ctrl Pts',(80.6077043345164,10.964184925508,136.845609850597));
#64035=CARTESIAN_POINT('Ctrl Pts',(80.6766354064323,10.940144862958,136.841662901732));
#64036=CARTESIAN_POINT('Ctrl Pts',(80.7439678383179,10.916662334264,136.837807489967));
#64037=CARTESIAN_POINT('Ctrl Pts',(80.8100972020252,10.8896633060689,136.833952078201));
#64038=CARTESIAN_POINT('Ctrl Pts',(80.8746382140914,10.8593024382685,136.830096666436));
#64039=CARTESIAN_POINT('Ctrl Pts',(80.9414777732899,10.8278603062706,136.82610394902));
#64040=CARTESIAN_POINT('Ctrl Pts',(81.0066131911813,10.792812551216,136.822111231604));
#64041=CARTESIAN_POINT('Ctrl Pts',(81.0696421214655,10.7543840213838,136.818118514188));
#64042=CARTESIAN_POINT('Ctrl Pts',(81.1326710517497,10.7159554915516,136.814125796773));
#64043=CARTESIAN_POINT('Ctrl Pts',(81.1935930198934,10.6741465168137,136.810133079357));
#64044=CARTESIAN_POINT('Ctrl Pts',(81.252039109102,10.6292316077768,136.806140361941));
#64045=CARTESIAN_POINT('Ctrl Pts',(81.252039109102,10.6292316077768,137.506056941317));
#64046=CARTESIAN_POINT('Ctrl Pts',(81.3085836328015,10.5857780222097,137.502201804569));
#64047=CARTESIAN_POINT('Ctrl Pts',(81.3628760664577,10.5393675421866,137.498346667822));
#64048=CARTESIAN_POINT('Ctrl Pts',(81.4146004937637,10.4902694405856,137.494491531074));
#64049=CARTESIAN_POINT('Ctrl Pts',(81.4663309400818,10.44116562559,137.490635945716));
#64050=CARTESIAN_POINT('Ctrl Pts',(81.5154924362568,10.3893739044095,137.486780360358));
#64051=CARTESIAN_POINT('Ctrl Pts',(81.5618054162374,10.335200885377,137.482924775));
#64052=CARTESIAN_POINT('Ctrl Pts',(81.6081690728818,10.280968589056,137.479064970777));
#64053=CARTESIAN_POINT('Ctrl Pts',(81.6516776780836,10.2243501657366,137.475205166554));
#64054=CARTESIAN_POINT('Ctrl Pts',(81.6920921377846,10.1656851031679,137.471345362332));
#64055=CARTESIAN_POINT('Ctrl Pts',(81.7325322808141,10.1069827590399,137.467483105209));
#64056=CARTESIAN_POINT('Ctrl Pts',(81.7698741114574,10.0462316012982,137.463620848086));
#64057=CARTESIAN_POINT('Ctrl Pts',(81.8039234886228,9.9837975450746,137.459758590964));
#64058=CARTESIAN_POINT('Ctrl Pts',(81.8380300704416,9.92125859652008,137.455889845057));
#64059=CARTESIAN_POINT('Ctrl Pts',(81.868832952186,9.85703154543904,137.452021099149));
#64060=CARTESIAN_POINT('Ctrl Pts',(81.8961856371569,9.79150337456002,137.448152353242));
#64061=CARTESIAN_POINT('Ctrl Pts',(81.9061170250162,9.7677109870339,137.446747664226));
#64062=CARTESIAN_POINT('Ctrl Pts',(81.9155940428794,9.74374721974154,137.44534297521));
#64063=CARTESIAN_POINT('Ctrl Pts',(81.9246113195382,9.71963103824482,137.443938286194));
#64064=CARTESIAN_POINT('Ctrl Pts',(81.9494485540355,9.65320530044445,137.440069203343));
#64065=CARTESIAN_POINT('Ctrl Pts',(81.9708914866249,9.58536210780795,137.436200120492));
#64066=CARTESIAN_POINT('Ctrl Pts',(81.9887795660641,9.51648175195817,137.432331037641));
#64067=CARTESIAN_POINT('Ctrl Pts',(82.0066409931574,9.44770402440215,137.42846771953));
#64068=CARTESIAN_POINT('Ctrl Pts',(82.0209579595017,9.37789266740923,137.424604401419));
#64069=CARTESIAN_POINT('Ctrl Pts',(82.0316186896446,9.30744603166563,137.420741083309));
#64070=CARTESIAN_POINT('Ctrl Pts',(82.0422669147553,9.23708202979736,137.416882296868));
#64071=CARTESIAN_POINT('Ctrl Pts',(82.0492673502678,9.16608470734499,137.413023510428));
#64072=CARTESIAN_POINT('Ctrl Pts',(82.0525589895963,9.09486388526352,137.409164723988));
#64073=CARTESIAN_POINT('Ctrl Pts',(82.0558485554335,9.02368792707688,137.405308368301));
#64074=CARTESIAN_POINT('Ctrl Pts',(82.0554339378344,8.95228923270109,137.401452012613));
#64075=CARTESIAN_POINT('Ctrl Pts',(82.051305976554,8.88108257884583,137.397595656925));
#64076=CARTESIAN_POINT('Ctrl Pts',(82.0471792347146,8.80989696014851,137.393740440444));
#64077=CARTESIAN_POINT('Ctrl Pts',(82.0393413550609,8.73890375405027,137.389885223962));
#64078=CARTESIAN_POINT('Ctrl Pts',(82.0278352523221,8.66851583455668,137.38603000748));
#64079=CARTESIAN_POINT('Ctrl Pts',(82.016328699729,8.59812516310539,137.382174640271));
#64080=CARTESIAN_POINT('Ctrl Pts',(82.0011537198593,8.52834030430681,137.378319273062));
#64081=CARTESIAN_POINT('Ctrl Pts',(81.9824046025217,8.45956540229117,137.374463905853));
#64082=CARTESIAN_POINT('Ctrl Pts',(81.9636358599709,8.39071851170714,137.370604503126));
#64083=CARTESIAN_POINT('Ctrl Pts',(81.9412856398149,8.32288415785246,137.366745100399));
#64084=CARTESIAN_POINT('Ctrl Pts',(81.9154982988436,8.25645186461982,137.362885697672));
#64085=CARTESIAN_POINT('Ctrl Pts',(81.8896963568773,8.18998195690079,137.35902410972));
#64086=CARTESIAN_POINT('Ctrl Pts',(81.860453619195,8.12491613342951,137.355162521769));
#64087=CARTESIAN_POINT('Ctrl Pts',(81.8279617422855,8.0616219145565,137.351300933817));
#64088=CARTESIAN_POINT('Ctrl Pts',(81.795413019673,7.9982169601795,137.34743258988));
#64089=CARTESIAN_POINT('Ctrl Pts',(81.7596040527343,7.93659021876824,137.343564245942));
#64090=CARTESIAN_POINT('Ctrl Pts',(81.7207710219754,7.87708208116986,137.339695902004));
#64091=CARTESIAN_POINT('Ctrl Pts',(81.6977130862504,7.84174786220621,137.337398990737));
#64092=CARTESIAN_POINT('Ctrl Pts',(81.6735897842482,7.80716000273841,137.33510207947));
#64093=CARTESIAN_POINT('Ctrl Pts',(81.648457142774,7.77338408173651,137.332805168203));
#64094=CARTESIAN_POINT('Ctrl Pts',(81.6061219104926,7.71648948661011,137.328936085356));
#64095=CARTESIAN_POINT('Ctrl Pts',(81.5607548249675,7.66167775717641,137.32506700251));
#64096=CARTESIAN_POINT('Ctrl Pts',(81.5125883019347,7.60929004053679,137.321197919663));
#64097=CARTESIAN_POINT('Ctrl Pts',(81.464493544619,7.55698037898212,137.317334601557));
#64098=CARTESIAN_POINT('Ctrl Pts',(81.4136079552719,7.50708791587218,137.313471283451));
#64099=CARTESIAN_POINT('Ctrl Pts',(81.3602055766749,7.45992261503438,137.309607965345));
#64100=CARTESIAN_POINT('Ctrl Pts',(81.3068658390473,7.4128126390762,137.305749178909));
#64101=CARTESIAN_POINT('Ctrl Pts',(81.2510155385615,7.36842379119041,137.301890392473));
#64102=CARTESIAN_POINT('Ctrl Pts',(81.1929658905854,7.32702960384834,137.298031606038));
#64103=CARTESIAN_POINT('Ctrl Pts',(81.1349528096308,7.28566149180894,137.294175250355));
#64104=CARTESIAN_POINT('Ctrl Pts',(81.0747435244405,7.24728457906612,137.290318894672));
#64105=CARTESIAN_POINT('Ctrl Pts',(81.0126815343106,7.21213152816929,137.286462538989));
#64106=CARTESIAN_POINT('Ctrl Pts',(80.950637877914,7.17698886183566,137.282607322512));
#64107=CARTESIAN_POINT('Ctrl Pts',(80.8867430255922,7.14506840593426,137.278752106035));
#64108=CARTESIAN_POINT('Ctrl Pts',(80.8213671225576,7.11655804111691,137.274896889558));
#64109=CARTESIAN_POINT('Ctrl Pts',(80.7559886635206,7.08804656162947,137.271041522354));
#64110=CARTESIAN_POINT('Ctrl Pts',(80.689129484972,7.06294563009214,137.267186155149));
#64111=CARTESIAN_POINT('Ctrl Pts',(80.6211802626994,7.04139523034056,137.263330787945));
#64112=CARTESIAN_POINT('Ctrl Pts',(80.5531599161197,7.01982227319688,137.259471385222));
#64113=CARTESIAN_POINT('Ctrl Pts',(80.4840477121684,7.00180741384327,137.2556119825));
#64114=CARTESIAN_POINT('Ctrl Pts',(80.4142491990333,6.98744064345911,137.251752579777));
#64115=CARTESIAN_POINT('Ctrl Pts',(80.3444111654316,6.97306573849666,137.247890991831));
#64116=CARTESIAN_POINT('Ctrl Pts',(80.2738865295672,6.96234310748402,137.244029403884));
#64117=CARTESIAN_POINT('Ctrl Pts',(80.2030880081502,6.95531106927103,137.240167815937));
#64118=CARTESIAN_POINT('Ctrl Pts',(80.1321656221821,6.94826672825512,137.236299472004));
#64119=CARTESIAN_POINT('Ctrl Pts',(80.0609688793824,6.94492589404826,137.232431128071));
#64120=CARTESIAN_POINT('Ctrl Pts',(79.9899118530188,6.94527476489179,137.228562784137));
#64121=CARTESIAN_POINT('Ctrl Pts',(79.9477202355614,6.94548191435928,137.226265872829));
#64122=CARTESIAN_POINT('Ctrl Pts',(79.9055778257029,6.9469889240259,137.22396896152));
#64123=CARTESIAN_POINT('Ctrl Pts',(79.8635701063463,6.94978429266147,137.221672050211));
#64124=CARTESIAN_POINT('Ctrl Pts',(79.7928092782107,6.95449301293067,137.217802967365));
#64125=CARTESIAN_POINT('Ctrl Pts',(79.722153916906,6.96287859875673,137.213933884519));
#64126=CARTESIAN_POINT('Ctrl Pts',(79.6520166891177,6.97493082146625,137.210064801673));
#64127=CARTESIAN_POINT('Ctrl Pts',(79.5819839623012,6.98696508696495,137.206201483567));
#64128=CARTESIAN_POINT('Ctrl Pts',(79.5124683114819,7.00265506363271,137.202338165462));
#64129=CARTESIAN_POINT('Ctrl Pts',(79.4438787829355,7.02193863734446,137.198474847356));
#64130=CARTESIAN_POINT('Ctrl Pts',(79.3753697098801,7.04119959143154,137.194616060921));
#64131=CARTESIAN_POINT('Ctrl Pts',(79.3077850666392,7.06404563873356,137.190757274486));
#64132=CARTESIAN_POINT('Ctrl Pts',(79.2415234539804,7.09036367555543,137.186898488051));
#64133=CARTESIAN_POINT('Ctrl Pts',(79.1753035812791,7.11666513394383,137.183042132369));
#64134=CARTESIAN_POINT('Ctrl Pts',(79.1104055360912,7.14643406378743,137.179185776687));
#64135=CARTESIAN_POINT('Ctrl Pts',(79.0472110931786,7.1795080715537,137.175329421004));
#64136=CARTESIAN_POINT('Ctrl Pts',(78.9840353185376,7.21257230892673,137.171474204528));
#64137=CARTESIAN_POINT('Ctrl Pts',(78.9225625772242,7.24893946075519,137.167618988052));
#64138=CARTESIAN_POINT('Ctrl Pts',(78.8631514734676,7.28840045857067,137.163763771576));
#64139=CARTESIAN_POINT('Ctrl Pts',(78.8037380469146,7.32786299919311,137.159908404372));
#64140=CARTESIAN_POINT('Ctrl Pts',(78.7463868213836,7.37041935534479,137.156053037168));
#64141=CARTESIAN_POINT('Ctrl Pts',(78.6914272967841,7.41581723185161,137.152197669964));
#64142=CARTESIAN_POINT('Ctrl Pts',(78.6364102445493,7.46126262755558,137.148338267243));
#64143=CARTESIAN_POINT('Ctrl Pts',(78.5837902660095,7.50955517097194,137.144478864521));
#64144=CARTESIAN_POINT('Ctrl Pts',(78.5338629270875,7.5604029570982,137.140619461799));
#64145=CARTESIAN_POINT('Ctrl Pts',(78.483907318914,7.61127953364038,137.136757873853));
#64146=CARTESIAN_POINT('Ctrl Pts',(78.4366477073383,7.66471386896874,137.132896285907));
#64147=CARTESIAN_POINT('Ctrl Pts',(78.3923401347151,7.72038000951368,137.129034697961));
#64148=CARTESIAN_POINT('Ctrl Pts',(78.3479550444055,7.77614353996672,137.125166354028));
#64149=CARTESIAN_POINT('Ctrl Pts',(78.3065325869224,7.83414627587793,137.121298010096));
#64150=CARTESIAN_POINT('Ctrl Pts',(78.2682857521432,7.89403285479645,137.117429666163));
#64151=CARTESIAN_POINT('Ctrl Pts',(78.245575882213,7.9295917821078,137.115132754849));
#64152=CARTESIAN_POINT('Ctrl Pts',(78.2239847570714,7.96581438708238,137.112835843534));
#64153=CARTESIAN_POINT('Ctrl Pts',(78.2035490783992,8.00262261466407,137.11053893222));
#64154=CARTESIAN_POINT('Ctrl Pts',(78.1674867936404,8.0675770899133,137.106485635472));
#64155=CARTESIAN_POINT('Ctrl Pts',(78.1348950465756,8.1345905325921,137.102432338725));
#64156=CARTESIAN_POINT('Ctrl Pts',(78.1060020779534,8.20327581072033,137.098379041977));
#64157=CARTESIAN_POINT('Ctrl Pts',(78.0771900219366,8.27176874084605,137.094337096186));
#64158=CARTESIAN_POINT('Ctrl Pts',(78.0520562805303,8.34192379971445,137.090295150394));
#64159=CARTESIAN_POINT('Ctrl Pts',(78.0307828211536,8.41333036124561,137.086253204602));
#64160=CARTESIAN_POINT('Ctrl Pts',(78.0095451555341,8.48461677733726,137.082218059604));
#64161=CARTESIAN_POINT('Ctrl Pts',(77.9921549775742,8.55715011048446,137.078182914607));
#64162=CARTESIAN_POINT('Ctrl Pts',(77.9787459929169,8.63050060710388,137.074147769609));
#64163=CARTESIAN_POINT('Ctrl Pts',(77.9653646220904,8.70370004916919,137.070120934399));
#64164=CARTESIAN_POINT('Ctrl Pts',(77.9559481961506,8.7777128936758,137.066094099189));
#64165=CARTESIAN_POINT('Ctrl Pts',(77.950580037019,8.85209672811253,137.062067263979));
#64166=CARTESIAN_POINT('Ctrl Pts',(77.9470284265033,8.90130957782711,137.059403082473));
#64167=CARTESIAN_POINT('Ctrl Pts',(77.945247813142,8.95068451301232,137.056738900968));
#64168=CARTESIAN_POINT('Ctrl Pts',(77.9452500020165,9.00009103231601,137.054074719462));
#64169=CARTESIAN_POINT('Origin',(80.,9.,141.545925280538));
#64170=CARTESIAN_POINT('',(81.252039109102,10.6292316077768,138.206016809239));
#64171=CARTESIAN_POINT('',(81.252039109102,10.6292316077768,138.147982307292));
#64172=CARTESIAN_POINT('',(81.252039109102,10.6292316077768,141.545925280538));
#64173=CARTESIAN_POINT('',(77.9452508576385,9.00187735576022,137.695925280507));
#64174=CARTESIAN_POINT('Ctrl Pts',(81.252039109102,10.6292316077768,138.147982307292));
#64175=CARTESIAN_POINT('Ctrl Pts',(81.3085983146724,10.5857667394206,138.144121802391));
#64176=CARTESIAN_POINT('Ctrl Pts',(81.3628508290673,10.5393845312925,138.14026129749));
#64177=CARTESIAN_POINT('Ctrl Pts',(81.414494838156,10.4903697243738,138.136400792589));
#64178=CARTESIAN_POINT('Ctrl Pts',(81.4668569704548,10.4406733539764,138.132486606375));
#64179=CARTESIAN_POINT('Ctrl Pts',(81.516537134486,10.3882709770766,138.128572420162));
#64180=CARTESIAN_POINT('Ctrl Pts',(81.563262117768,10.3334950744759,138.124658233948));
#64181=CARTESIAN_POINT('Ctrl Pts',(81.60998710105,10.2787191718752,138.120744047735));
#64182=CARTESIAN_POINT('Ctrl Pts',(81.6537566438285,10.2215701911493,138.116829861521));
#64183=CARTESIAN_POINT('Ctrl Pts',(81.6943435741606,10.1624101751107,138.112915675308));
#64184=CARTESIAN_POINT('Ctrl Pts',(81.7344628184565,10.1039318640733,138.109046592536));
#64185=CARTESIAN_POINT('Ctrl Pts',(81.7716296199641,10.0432595740049,138.105177509764));
#64186=CARTESIAN_POINT('Ctrl Pts',(81.8055964784114,9.98072367140205,138.101308426992));
#64187=CARTESIAN_POINT('Ctrl Pts',(81.8395127279206,9.91828094419922,138.097445108962));
#64188=CARTESIAN_POINT('Ctrl Pts',(81.8702382682615,9.85398053951649,138.093581790931));
#64189=CARTESIAN_POINT('Ctrl Pts',(81.8975685823103,9.78818210962237,138.089718472901));
#64190=CARTESIAN_POINT('Ctrl Pts',(81.9248668378987,9.7224608612915,138.085859686543));
#64191=CARTESIAN_POINT('Ctrl Pts',(81.9487775925512,9.65524552455614,138.082000900185));
#64192=CARTESIAN_POINT('Ctrl Pts',(81.9691428350777,9.5869191235275,138.078142113828));
#64193=CARTESIAN_POINT('Ctrl Pts',(81.9894952489891,9.51863576313988,138.074285758223));
#64194=CARTESIAN_POINT('Ctrl Pts',(82.0063064434009,9.44924319147191,138.070429402619));
#64195=CARTESIAN_POINT('Ctrl Pts',(82.0194675293387,9.37914174189442,138.066573047015));
#64196=CARTESIAN_POINT('Ctrl Pts',(82.0326247273568,9.30906100100354,138.062717830617));
#64197=CARTESIAN_POINT('Ctrl Pts',(82.0421338679971,9.23827227512134,138.05886261422));
#64198=CARTESIAN_POINT('Ctrl Pts',(82.0479370599032,9.16718660584799,138.055007397822));
#64199=CARTESIAN_POINT('Ctrl Pts',(82.0537404786956,9.09609815735139,138.051152030698));
#64200=CARTESIAN_POINT('Ctrl Pts',(82.0558376237616,9.02471322676606,138.047296663574));
#64201=CARTESIAN_POINT('Ctrl Pts',(82.0542225680827,8.95344676939605,138.04344129645));
#64202=CARTESIAN_POINT('Ctrl Pts',(82.0526058218812,8.88210571548853,138.039581893809));
#64203=CARTESIAN_POINT('Ctrl Pts',(82.0472691293125,8.81088386899975,138.035722491167));
#64204=CARTESIAN_POINT('Ctrl Pts',(82.0382586782974,8.74019406695541,138.031863088525));
#64205=CARTESIAN_POINT('Ctrl Pts',(82.0292431254952,8.66946423979759,138.02800150066));
#64206=CARTESIAN_POINT('Ctrl Pts',(82.0165497598692,8.59926753503242,138.024139912795));
#64207=CARTESIAN_POINT('Ctrl Pts',(82.0002759786724,8.53000683872418,138.02027832493));
#64208=CARTESIAN_POINT('Ctrl Pts',(81.9839737259109,8.46062496834006,138.016409981078));
#64209=CARTESIAN_POINT('Ctrl Pts',(81.9640786868343,8.39218284251079,138.012541637226));
#64210=CARTESIAN_POINT('Ctrl Pts',(81.9407380100454,8.32506775238905,138.008673293374));
#64211=CARTESIAN_POINT('Ctrl Pts',(81.9268789832615,8.28521673007253,138.006376381355));
#64212=CARTESIAN_POINT('Ctrl Pts',(81.91180607447,8.24583320161199,138.004079469335));
#64213=CARTESIAN_POINT('Ctrl Pts',(81.8955578473675,8.20699431919846,138.001782557316));
#64214=CARTESIAN_POINT('Ctrl Pts',(81.8681881715652,8.14157132790987,137.997913474436));
#64215=CARTESIAN_POINT('Ctrl Pts',(81.8373739143585,8.07743881058132,137.994044391556));
#64216=CARTESIAN_POINT('Ctrl Pts',(81.8032583883217,8.01498388467632,137.990175308676));
#64217=CARTESIAN_POINT('Ctrl Pts',(81.7691936927131,7.95262201348841,137.986311990536));
#64218=CARTESIAN_POINT('Ctrl Pts',(81.7318377227886,7.89193319508389,137.982448672396));
#64219=CARTESIAN_POINT('Ctrl Pts',(81.6913817082807,7.83328431938484,137.978585354256));
#64220=CARTESIAN_POINT('Ctrl Pts',(81.650973148657,7.77470423878668,137.974726567787));
#64221=CARTESIAN_POINT('Ctrl Pts',(81.6074720419694,7.71815974581528,137.970867781317));
#64222=CARTESIAN_POINT('Ctrl Pts',(81.5611144773103,7.66399133564481,137.967008994847));
#64223=CARTESIAN_POINT('Ctrl Pts',(81.5147861145142,7.60985704759662,137.96315263913));
#64224=CARTESIAN_POINT('Ctrl Pts',(81.4656051787584,7.55809624101094,137.959296283412));
#64225=CARTESIAN_POINT('Ctrl Pts',(81.4138489441385,7.50901753006334,137.955439927695));
#64226=CARTESIAN_POINT('Ctrl Pts',(81.3621079988254,7.4599533174554,137.951584711183));
#64227=CARTESIAN_POINT('Ctrl Pts',(81.3077936172911,7.41356996159437,137.947729494671));
#64228=CARTESIAN_POINT('Ctrl Pts',(81.2512197300716,7.37013903980138,137.94387427816));
#64229=CARTESIAN_POINT('Ctrl Pts',(81.1946436309801,7.32670641998749,137.940018910921));
#64230=CARTESIAN_POINT('Ctrl Pts',(81.1358082374883,7.28622675748109,137.936163543681));
#64231=CARTESIAN_POINT('Ctrl Pts',(81.0750589525976,7.24893009535893,137.932308176442));
#64232=CARTESIAN_POINT('Ctrl Pts',(81.0142460797713,7.21159439380193,137.928448773685));
#64233=CARTESIAN_POINT('Ctrl Pts',(80.9515157313008,7.17744859820139,137.924589370927));
#64234=CARTESIAN_POINT('Ctrl Pts',(80.8872397966678,7.1466778192368,137.92072996817));
#64235=CARTESIAN_POINT('Ctrl Pts',(80.8229274684949,7.11588961761509,137.916868380188));
#64236=CARTESIAN_POINT('Ctrl Pts',(80.7570682607646,7.08848042350474,137.913006792207));
#64237=CARTESIAN_POINT('Ctrl Pts',(80.6900534777598,7.06458692772534,137.909145204225));
#64238=CARTESIAN_POINT('Ctrl Pts',(80.6229214499959,7.04065162942075,137.905276860257));
#64239=CARTESIAN_POINT('Ctrl Pts',(80.5546302761291,7.0202444489042,137.901408516289));
#64240=CARTESIAN_POINT('Ctrl Pts',(80.4855851427937,7.00345182086732,137.897540172321));
#64241=CARTESIAN_POINT('Ctrl Pts',(80.4445881354207,6.99348084301294,137.895243261322));
#64242=CARTESIAN_POINT('Ctrl Pts',(80.4033254996481,6.98478324591936,137.892946350324));
#64243=CARTESIAN_POINT('Ctrl Pts',(80.3618829696559,6.9773684767677,137.890649439325));
#64244=CARTESIAN_POINT('Ctrl Pts',(80.2920741777508,6.96487850386233,137.886780356478));
#64245=CARTESIAN_POINT('Ctrl Pts',(80.2214812825329,6.95598236534361,137.88291127363));
#64246=CARTESIAN_POINT('Ctrl Pts',(80.1505072441009,6.95076962447529,137.879042190783));
#64247=CARTESIAN_POINT('Ctrl Pts',(80.0796389534446,6.94556465033074,137.875178872676));
#64248=CARTESIAN_POINT('Ctrl Pts',(80.0083911273403,6.94403221544512,137.871315554569));
#64249=CARTESIAN_POINT('Ctrl Pts',(79.9371757213845,6.94621065527244,137.867452236462));
#64250=CARTESIAN_POINT('Ctrl Pts',(79.8660438510696,6.94838653979077,137.863593450026));
#64251=CARTESIAN_POINT('Ctrl Pts',(79.7949448085646,6.95426463799844,137.85973466359));
#64252=CARTESIAN_POINT('Ctrl Pts',(79.7242927051995,6.96383128152558,137.855875877153));
#64253=CARTESIAN_POINT('Ctrl Pts',(79.6536851074769,6.97339189876904,137.852019521469));
#64254=CARTESIAN_POINT('Ctrl Pts',(79.5835243705778,6.98663638649006,137.848163165785));
#64255=CARTESIAN_POINT('Ctrl Pts',(79.5142201594867,7.00349918380912,137.844306810101));
#64256=CARTESIAN_POINT('Ctrl Pts',(79.4449364215518,7.02035699968939,137.840451593623));
#64257=CARTESIAN_POINT('Ctrl Pts',(79.3765091788523,7.04083088834935,137.836596377145));
#64258=CARTESIAN_POINT('Ctrl Pts',(79.3093368622184,7.06480440456019,137.832741160667));
#64259=CARTESIAN_POINT('Ctrl Pts',(79.2421619193466,7.08877885806425,137.828885793462));
#64260=CARTESIAN_POINT('Ctrl Pts',(79.176242456728,7.11625304540635,137.825030426256));
#64261=CARTESIAN_POINT('Ctrl Pts',(79.1119590809463,7.14706155294187,137.821175059051));
#64262=CARTESIAN_POINT('Ctrl Pts',(79.0476084179968,7.17790230858494,137.817315656327));
#64263=CARTESIAN_POINT('Ctrl Pts',(78.9848976994599,7.21208414111098,137.813456253603));
#64264=CARTESIAN_POINT('Ctrl Pts',(78.9241841484722,7.24939501425894,137.809596850879));
#64265=CARTESIAN_POINT('Ctrl Pts',(78.8634362209937,7.28672701311709,137.805735262931));
#64266=CARTESIAN_POINT('Ctrl Pts',(78.8046881124189,7.32719130379329,137.801873674983));
#64267=CARTESIAN_POINT('Ctrl Pts',(78.7482668969645,7.37053327703049,137.798012087035));
#64268=CARTESIAN_POINT('Ctrl Pts',(78.6917469705695,7.41395107860471,137.7941437431));
#64269=CARTESIAN_POINT('Ctrl Pts',(78.637562434545,7.46025629878071,137.790275399166));
#64270=CARTESIAN_POINT('Ctrl Pts',(78.5860056707863,7.50915540734408,137.786407055231));
#64271=CARTESIAN_POINT('Ctrl Pts',(78.5553927482467,7.53819029071482,137.784110143932));
#64272=CARTESIAN_POINT('Ctrl Pts',(78.5257055636269,7.56813899419849,137.781813232633));
#64273=CARTESIAN_POINT('Ctrl Pts',(78.4969985543698,7.59893461361234,137.779516321333));
#64274=CARTESIAN_POINT('Ctrl Pts',(78.4492223163315,7.6501868646037,137.775693638866));
#64275=CARTESIAN_POINT('Ctrl Pts',(78.4039661357278,7.70399804441434,137.771870956398));
#64276=CARTESIAN_POINT('Ctrl Pts',(78.3615208436958,7.76008725433738,137.76804827393));
#64277=CARTESIAN_POINT('Ctrl Pts',(78.3191332469992,7.81610022292423,137.764230787586));
#64278=CARTESIAN_POINT('Ctrl Pts',(78.2795492636144,7.87438469113794,137.760413301241));
#64279=CARTESIAN_POINT('Ctrl Pts',(78.2430220975302,7.93462391019277,137.756595814896));
#64280=CARTESIAN_POINT('Ctrl Pts',(78.2065316626786,7.99480255348986,137.752782167364));
#64281=CARTESIAN_POINT('Ctrl Pts',(78.1730922068975,8.05693162628516,137.748968519833));
#64282=CARTESIAN_POINT('Ctrl Pts',(78.1429147652304,8.12066389059655,137.745154872302));
#64283=CARTESIAN_POINT('Ctrl Pts',(78.1127570014877,8.18435459675692,137.741343711551));
#64284=CARTESIAN_POINT('Ctrl Pts',(78.0858572438908,8.24964597086899,137.7375325508));
#64285=CARTESIAN_POINT('Ctrl Pts',(78.062380601309,8.31616622756962,137.733721390049));
#64286=CARTESIAN_POINT('Ctrl Pts',(78.0389040931843,8.38268610329087,137.729910251125));
#64287=CARTESIAN_POINT('Ctrl Pts',(78.0188508409774,8.45043438279459,137.726099112202));
#64288=CARTESIAN_POINT('Ctrl Pts',(78.0023372240668,8.51902079447142,137.722287973278));
#64289=CARTESIAN_POINT('Ctrl Pts',(77.9858234661275,8.58760779188607,137.718476801807));
#64290=CARTESIAN_POINT('Ctrl Pts',(77.9728495099846,8.65703244869873,137.714665630336));
#64291=CARTESIAN_POINT('Ctrl Pts',(77.9634808603815,8.72689314093621,137.710854458865));
#64292=CARTESIAN_POINT('Ctrl Pts',(77.9541049328187,8.79680810388833,137.707040326716));
#64293=CARTESIAN_POINT('Ctrl Pts',(77.9483399514157,8.86715928237804,137.703226194567));
#64294=CARTESIAN_POINT('Ctrl Pts',(77.946199539787,8.9375401558698,137.699412062418));
#64295=CARTESIAN_POINT('Ctrl Pts',(77.9455473032982,8.95898695292022,137.698249801791));
#64296=CARTESIAN_POINT('Ctrl Pts',(77.9452312678571,8.98043650827389,137.697087541165));
#64297=CARTESIAN_POINT('Ctrl Pts',(77.945250857638,9.00187735519529,137.695925280538));
#64298=CARTESIAN_POINT('Ctrl Pts',(77.9452508576385,9.00187735576021,137.695925280507));
#64299=CARTESIAN_POINT('Ctrl Pts',(77.9453355911812,9.09461746279061,137.690898045562));
#64300=CARTESIAN_POINT('Ctrl Pts',(77.9517027473501,9.18707803688478,137.685870810616));
#64301=CARTESIAN_POINT('Ctrl Pts',(77.9642171232008,9.27854199150456,137.68084357567));
#64302=CARTESIAN_POINT('Ctrl Pts',(77.9745563908267,9.35410870903171,137.676690118228));
#64303=CARTESIAN_POINT('Ctrl Pts',(77.9890907794787,9.42899580347728,137.672536660785));
#64304=CARTESIAN_POINT('Ctrl Pts',(78.0077202195898,9.50281093769801,137.668383203342));
#64305=CARTESIAN_POINT('Ctrl Pts',(78.0250741586275,9.57157217430436,137.664514120491));
#64306=CARTESIAN_POINT('Ctrl Pts',(78.0460260884595,9.63956860642717,137.66064503764));
#64307=CARTESIAN_POINT('Ctrl Pts',(78.0704917545785,9.70639613061694,137.656775954788));
#64308=CARTESIAN_POINT('Ctrl Pts',(78.0949209680756,9.77312408512974,137.652912636678));
#64309=CARTESIAN_POINT('Ctrl Pts',(78.122853360305,9.83868613630884,137.649049318567));
#64310=CARTESIAN_POINT('Ctrl Pts',(78.1541542876673,9.90269107050148,137.645186000456));
#64311=CARTESIAN_POINT('Ctrl Pts',(78.1854184990544,9.96662092693204,137.641327214016));
#64312=CARTESIAN_POINT('Ctrl Pts',(78.2200431845958,10.0289968601426,137.637468427576));
#64313=CARTESIAN_POINT('Ctrl Pts',(78.2578454199541,10.0894470990943,137.633609641136));
#64314=CARTESIAN_POINT('Ctrl Pts',(78.2956238426764,10.1498592588286,137.629753285448));
#64315=CARTESIAN_POINT('Ctrl Pts',(78.3365755870685,10.2083477200628,137.625896929761));
#64316=CARTESIAN_POINT('Ctrl Pts',(78.3804722672278,10.2645661253101,137.622040574073));
#64317=CARTESIAN_POINT('Ctrl Pts',(78.4243559798687,10.3207679230781,137.618185357591));
#64318=CARTESIAN_POINT('Ctrl Pts',(78.4711826023525,10.3747006135015,137.61433014111));
#64319=CARTESIAN_POINT('Ctrl Pts',(78.5206820001741,10.4260490236633,137.610474924628));
#64320=CARTESIAN_POINT('Ctrl Pts',(78.5701833332744,10.4773994413948,137.606619557419));
#64321=CARTESIAN_POINT('Ctrl Pts',(78.6223573104468,10.5261650300569,137.60276419021));
#64322=CARTESIAN_POINT('Ctrl Pts',(78.6768965074492,10.5720670184505,137.598908823001));
#64323=CARTESIAN_POINT('Ctrl Pts',(78.7314927921189,10.6180170537092,137.595049420274));
#64324=CARTESIAN_POINT('Ctrl Pts',(78.7884588663221,10.6610971917516,137.591190017547));
#64325=CARTESIAN_POINT('Ctrl Pts',(78.847454442338,10.7010691637948,137.587330614819));
#64326=CARTESIAN_POINT('Ctrl Pts',(78.9064834221127,10.7410637682828,137.583469026868));
#64327=CARTESIAN_POINT('Ctrl Pts',(78.9675437752333,10.7779464521318,137.579607438917));
#64328=CARTESIAN_POINT('Ctrl Pts',(79.0302688260821,10.8115239476286,137.575745850965));
#64329=CARTESIAN_POINT('Ctrl Pts',(79.0931036166551,10.8451601881569,137.571877507027));
#64330=CARTESIAN_POINT('Ctrl Pts',(79.1576084799627,10.8754794886075,137.568009163089));
#64331=CARTESIAN_POINT('Ctrl Pts',(79.2233955510299,10.9023362195837,137.564140819151));
#64332=CARTESIAN_POINT('Ctrl Pts',(79.2624580199291,10.9182829732766,137.561843907884));
#64333=CARTESIAN_POINT('Ctrl Pts',(79.3019722152479,10.9330098904872,137.559546996617));
#64334=CARTESIAN_POINT('Ctrl Pts',(79.3418547552921,10.9464949009356,137.55725008535));
#64335=CARTESIAN_POINT('Ctrl Pts',(79.4090365153638,10.9692102730134,137.553380960127));
#64336=CARTESIAN_POINT('Ctrl Pts',(79.4775272460009,10.9884879637316,137.549511834903));
#64337=CARTESIAN_POINT('Ctrl Pts',(79.5469417357711,11.0041795757152,137.54564270968));
#64338=CARTESIAN_POINT('Ctrl Pts',(79.6162525807636,11.0198477581002,137.541779361559));
#64339=CARTESIAN_POINT('Ctrl Pts',(79.6864839770015,11.0319403841584,137.537916013439));
#64340=CARTESIAN_POINT('Ctrl Pts',(79.757234215337,11.0403583842788,137.534052665318));
#64341=CARTESIAN_POINT('Ctrl Pts',(79.827900600162,11.0487664073465,137.530193896055));
#64342=CARTESIAN_POINT('Ctrl Pts',(79.899084125485,11.0535083988416,137.526335126793));
#64343=CARTESIAN_POINT('Ctrl Pts',(79.9703732449644,11.0545363997472,137.52247635753));
#64344=CARTESIAN_POINT('Ctrl Pts',(80.0416171339066,11.0555637484209,137.518620036526));
#64345=CARTESIAN_POINT('Ctrl Pts',(80.1129659995103,11.0528817748708,137.514763715522));
#64346=CARTESIAN_POINT('Ctrl Pts',(80.1840049945603,11.0464944965665,137.510907394518));
#64347=CARTESIAN_POINT('Ctrl Pts',(80.2550226814983,11.0401091341232,137.507052230216));
#64348=CARTESIAN_POINT('Ctrl Pts',(80.3257301988894,11.0300207171257,137.503197065913));
#64349=CARTESIAN_POINT('Ctrl Pts',(80.3957162605863,11.0162852485716,137.499341901611));
#64350=CARTESIAN_POINT('Ctrl Pts',(80.4657047407185,11.0025493053753,137.49548660409));
#64351=CARTESIAN_POINT('Ctrl Pts',(80.5349712394909,10.985166156402,137.491631306569));
#64352=CARTESIAN_POINT('Ctrl Pts',(80.6031148326331,10.9642428722431,137.487776009047));
#64353=CARTESIAN_POINT('Ctrl Pts',(80.6713261626792,10.9432987896728,137.483916879237));
#64354=CARTESIAN_POINT('Ctrl Pts',(80.7384118941879,10.9188076915413,137.480057749428));
#64355=CARTESIAN_POINT('Ctrl Pts',(80.8039873646162,10.8909261963486,137.476198619618));
#64356=CARTESIAN_POINT('Ctrl Pts',(80.869599845037,10.8630289651815,137.472337311762));
#64357=CARTESIAN_POINT('Ctrl Pts',(80.9336999310049,10.8317377409704,137.468476003907));
#64358=CARTESIAN_POINT('Ctrl Pts',(80.9959264492264,10.7972557052994,137.464614696051));
#64359=CARTESIAN_POINT('Ctrl Pts',(81.0582543739492,10.7627174765022,137.460747095674));
#64360=CARTESIAN_POINT('Ctrl Pts',(81.1187022253178,10.7249783151754,137.456879495297));
#64361=CARTESIAN_POINT('Ctrl Pts',(81.1769374678752,10.6842849400299,137.45301189492));
#64362=CARTESIAN_POINT('Ctrl Pts',(81.2024025695469,10.6664905445756,137.451320670972));
#64363=CARTESIAN_POINT('Ctrl Pts',(81.2274450168065,10.6481317845595,137.449629447024));
#64364=CARTESIAN_POINT('Ctrl Pts',(81.252039109102,10.6292316077768,137.447938223076));
#64365=CARTESIAN_POINT('',(77.9452508246239,8.99815913298199,137.754074719432));
#64366=CARTESIAN_POINT('Ctrl Pts',(77.9452508246239,8.998159132982,137.754074719432));
#64367=CARTESIAN_POINT('Ctrl Pts',(77.9451879957237,9.06828784391594,137.750267950527));
#64368=CARTESIAN_POINT('Ctrl Pts',(77.948719643209,9.1385287266768,137.746461181623));
#64369=CARTESIAN_POINT('Ctrl Pts',(77.955853571024,9.20847767123739,137.742654412718));
#64370=CARTESIAN_POINT('Ctrl Pts',(77.9629816800018,9.27836956146164,137.73885074883));
#64371=CARTESIAN_POINT('Ctrl Pts',(77.9737061958358,9.34796948932302,137.735047084943));
#64372=CARTESIAN_POINT('Ctrl Pts',(77.9879828890358,9.41687493050971,137.731243421055));
#64373=CARTESIAN_POINT('Ctrl Pts',(78.0022530301468,9.48574874850582,137.727441502806));
#64374=CARTESIAN_POINT('Ctrl Pts',(78.0200720145925,9.55392822213815,137.723639584557));
#64375=CARTESIAN_POINT('Ctrl Pts',(78.0413442350491,9.62101944971517,137.719837666308));
#64376=CARTESIAN_POINT('Ctrl Pts',(78.0626142800831,9.68810381614818,137.716036136865));
#64377=CARTESIAN_POINT('Ctrl Pts',(78.0873367072412,9.75409968062593,137.712234607423));
#64378=CARTESIAN_POINT('Ctrl Pts',(78.1153661610104,9.81862864318035,137.70843307798));
#64379=CARTESIAN_POINT('Ctrl Pts',(78.143421601976,9.88321743304506,137.704628023992));
#64380=CARTESIAN_POINT('Ctrl Pts',(78.1747899917167,9.94633614509237,137.700822970003));
#64381=CARTESIAN_POINT('Ctrl Pts',(78.2092783941031,10.0076277550137,137.697017916015));
#64382=CARTESIAN_POINT('Ctrl Pts',(78.243783338819,10.0689487633976,137.693211036936));
#64383=CARTESIAN_POINT('Ctrl Pts',(78.2814110055482,10.1284405026701,137.689404157857));
#64384=CARTESIAN_POINT('Ctrl Pts',(78.3219247244603,10.1857744018667,137.685597278778));
#64385=CARTESIAN_POINT('Ctrl Pts',(78.3625095297344,10.2432089005249,137.681783720056));
#64386=CARTESIAN_POINT('Ctrl Pts',(78.4059901860523,10.2984776074081,137.677970161334));
#64387=CARTESIAN_POINT('Ctrl Pts',(78.4520898455625,10.351285209084,137.674156602612));
#64388=CARTESIAN_POINT('Ctrl Pts',(78.4841323747905,10.3879902333325,137.671505909134));
#64389=CARTESIAN_POINT('Ctrl Pts',(78.5174393844088,10.423506973414,137.668855215655));
#64390=CARTESIAN_POINT('Ctrl Pts',(78.5519082624529,10.4577475371778,137.666204522177));
#64391=CARTESIAN_POINT('Ctrl Pts',(78.6022207357355,10.5077267516837,137.66233543933));
#64392=CARTESIAN_POINT('Ctrl Pts',(78.6552222517718,10.5551960831898,137.658466356483));
#64393=CARTESIAN_POINT('Ctrl Pts',(78.7106323248073,10.5998526684255,137.654597273635));
#64394=CARTESIAN_POINT('Ctrl Pts',(78.7659598395989,10.6444427175775,137.650733955528));
#64395=CARTESIAN_POINT('Ctrl Pts',(78.8236884129037,10.6862280368351,137.646870637421));
#64396=CARTESIAN_POINT('Ctrl Pts',(78.8835010225446,10.7249427804542,137.643007319315));
#64397=CARTESIAN_POINT('Ctrl Pts',(78.9432434720197,10.7636121116955,137.639148532878));
#64398=CARTESIAN_POINT('Ctrl Pts',(79.0050646962487,10.7992177589796,137.635289746442));
#64399=CARTESIAN_POINT('Ctrl Pts',(79.0686163208411,10.831535422725,137.631430960005));
#64400=CARTESIAN_POINT('Ctrl Pts',(79.1321279125715,10.8638327287127,137.627574604321));
#64401=CARTESIAN_POINT('Ctrl Pts',(79.1973673100851,10.8928459406904,137.623718248637));
#64402=CARTESIAN_POINT('Ctrl Pts',(79.2639602801978,10.9183959688692,137.619861892953));
#64403=CARTESIAN_POINT('Ctrl Pts',(79.3305335780819,10.9439384493143,137.616006676475));
#64404=CARTESIAN_POINT('Ctrl Pts',(79.3984592014349,10.9660196030974,137.612151459997));
#64405=CARTESIAN_POINT('Ctrl Pts',(79.4673432145737,10.9845085818508,137.608296243519));
#64406=CARTESIAN_POINT('Ctrl Pts',(79.5362299208732,11.0029982834684,137.604440876314));
#64407=CARTESIAN_POINT('Ctrl Pts',(79.6060746216028,11.0178954074216,137.600585509108));
#64408=CARTESIAN_POINT('Ctrl Pts',(79.6764701885863,11.0291195193055,137.596730141903));
#64409=CARTESIAN_POINT('Ctrl Pts',(79.7469394405348,11.0403553797743,137.592870739179));
#64410=CARTESIAN_POINT('Ctrl Pts',(79.8179602290672,11.047910476761,137.589011336455));
#64411=CARTESIAN_POINT('Ctrl Pts',(79.889118140131,11.0517560224481,137.585151933731));
#64412=CARTESIAN_POINT('Ctrl Pts',(79.9603163413645,11.0556037455135,137.581290345783));
#64413=CARTESIAN_POINT('Ctrl Pts',(80.0316513336741,11.0557377351632,137.577428757835));
#64414=CARTESIAN_POINT('Ctrl Pts',(80.102709285001,11.0521813675391,137.573567169887));
#64415=CARTESIAN_POINT('Ctrl Pts',(80.1738915547628,11.0486187779222,137.569698825952));
#64416=CARTESIAN_POINT('Ctrl Pts',(80.2447953324329,11.0413529901579,137.565830482018));
#64417=CARTESIAN_POINT('Ctrl Pts',(80.3150131820574,11.0304591248361,137.561962138083));
#64418=CARTESIAN_POINT('Ctrl Pts',(80.3567065203266,11.0239906611285,137.559665226784));
#64419=CARTESIAN_POINT('Ctrl Pts',(80.3981582238866,11.0162440461926,137.557368315484));
#64420=CARTESIAN_POINT('Ctrl Pts',(80.4392854645031,11.007243344285,137.555071404185));
#64421=CARTESIAN_POINT('Ctrl Pts',(80.5085688299935,10.9920806708212,137.55120200418));
#64422=CARTESIAN_POINT('Ctrl Pts',(80.5772019369505,10.9732969381624,137.547332604175));
#64423=CARTESIAN_POINT('Ctrl Pts',(80.6447781102469,10.9509635442638,137.543463204171));
#64424=CARTESIAN_POINT('Ctrl Pts',(80.7122373862153,10.928668784013,137.539600497686));
#64425=CARTESIAN_POINT('Ctrl Pts',(80.7786429038363,10.902836714354,137.535737791202));
#64426=CARTESIAN_POINT('Ctrl Pts',(80.84359955841,10.8735894287571,137.531875084718));
#64427=CARTESIAN_POINT('Ctrl Pts',(80.9084915578505,10.8443712546833,137.52801622301));
#64428=CARTESIAN_POINT('Ctrl Pts',(80.9719371146386,10.8117448069602,137.524157361303));
#64429=CARTESIAN_POINT('Ctrl Pts',(81.0335588124541,10.7758811175578,137.520298499595));
#64430=CARTESIAN_POINT('Ctrl Pts',(81.0951364101892,10.740043094303,137.516442399513));
#64431=CARTESIAN_POINT('Ctrl Pts',(81.1548923224202,10.7009726742508,137.512586299432));
#64432=CARTESIAN_POINT('Ctrl Pts',(81.2124731810451,10.6588870810717,137.508730199351));
#64433=CARTESIAN_POINT('Ctrl Pts',(81.2257792406795,10.6491617413326,137.507839113339));
#64434=CARTESIAN_POINT('Ctrl Pts',(81.2389692655704,10.6392755789184,137.506948027328));
#64435=CARTESIAN_POINT('Ctrl Pts',(81.252039109102,10.6292316077768,137.506056941317));
#64436=CARTESIAN_POINT('Ctrl Pts',(81.252039109102,10.6292316077768,138.206016809239));
#64437=CARTESIAN_POINT('Ctrl Pts',(81.3100004164792,10.5846892460251,138.202046816943));
#64438=CARTESIAN_POINT('Ctrl Pts',(81.365664648856,10.5369863629426,138.198076824648));
#64439=CARTESIAN_POINT('Ctrl Pts',(81.4186724477197,10.4863936385026,138.194106832352));
#64440=CARTESIAN_POINT('Ctrl Pts',(81.4701805437359,10.4372322893419,138.190249159543));
#64441=CARTESIAN_POINT('Ctrl Pts',(81.519180147956,10.3853428098416,138.186391486734));
#64442=CARTESIAN_POINT('Ctrl Pts',(81.5653745129687,10.3310147244295,138.182533813925));
#64443=CARTESIAN_POINT('Ctrl Pts',(81.611545872447,10.2767136952748,138.178678062298));
#64444=CARTESIAN_POINT('Ctrl Pts',(81.6549144507438,10.2199768396543,138.174822310672));
#64445=CARTESIAN_POINT('Ctrl Pts',(81.6952218725276,10.1611289185116,138.170966559046));
#64446=CARTESIAN_POINT('Ctrl Pts',(81.7355227039307,10.1022906191751,138.167111437846));
#64447=CARTESIAN_POINT('Ctrl Pts',(81.7727630987943,10.0413423408248,138.163256316647));
#64448=CARTESIAN_POINT('Ctrl Pts',(81.8067273659854,9.97863874207973,138.159401195447));
#64449=CARTESIAN_POINT('Ctrl Pts',(81.8424556835949,9.91267841740622,138.155345845338));
#64450=CARTESIAN_POINT('Ctrl Pts',(81.8745580059818,9.84477598534579,138.15129049523));
#64451=CARTESIAN_POINT('Ctrl Pts',(81.9028386321676,9.77537262166675,138.147235145121));
#64452=CARTESIAN_POINT('Ctrl Pts',(81.929758577429,9.70930849922059,138.143374912246));
#64453=CARTESIAN_POINT('Ctrl Pts',(81.9532159962972,9.64188504771407,138.13951467937));
#64454=CARTESIAN_POINT('Ctrl Pts',(81.9730927839647,9.57350015550693,138.135654446495));
#64455=CARTESIAN_POINT('Ctrl Pts',(81.9929834856272,9.50506739303689,138.131791511409));
#64456=CARTESIAN_POINT('Ctrl Pts',(82.0092884593221,9.4356723233551,138.127928576323));
#64457=CARTESIAN_POINT('Ctrl Pts',(82.0219406338674,9.36572344143639,138.124065641237));
#64458=CARTESIAN_POINT('Ctrl Pts',(82.0346132881541,9.29566133510642,138.12019645332));
#64459=CARTESIAN_POINT('Ctrl Pts',(82.0436212918391,9.22504410920679,138.116327265403));
#64460=CARTESIAN_POINT('Ctrl Pts',(82.0489494312964,9.15428477076475,138.112458077486));
#64461=CARTESIAN_POINT('Ctrl Pts',(82.0497394482429,9.1437931015921,138.111884383039));
#64462=CARTESIAN_POINT('Ctrl Pts',(82.0504486576402,9.13329830491125,138.111310688591));
#64463=CARTESIAN_POINT('Ctrl Pts',(82.0510771071998,9.12280172157117,138.110736994143));
#64464=CARTESIAN_POINT('Ctrl Pts',(82.0553154671478,9.05201115813191,138.106867911044));
#64465=CARTESIAN_POINT('Ctrl Pts',(82.0558929439494,8.98086226244677,138.102998827945));
#64466=CARTESIAN_POINT('Ctrl Pts',(82.0527677254126,8.90976570494383,138.099129744846));
#64467=CARTESIAN_POINT('Ctrl Pts',(82.0496471632929,8.83877507770455,138.095266426484));
#64468=CARTESIAN_POINT('Ctrl Pts',(82.0428348777455,8.76783711521766,138.091403108123));
#64469=CARTESIAN_POINT('Ctrl Pts',(82.0323409849502,8.69736542928556,138.087539789761));
#64470=CARTESIAN_POINT('Ctrl Pts',(82.0218594014778,8.62697640655115,138.083681003067));
#64471=CARTESIAN_POINT('Ctrl Pts',(82.007704860003,8.55705305211314,138.079822216373));
#64472=CARTESIAN_POINT('Ctrl Pts',(81.9899393756834,8.48800503556719,138.075963429679));
#64473=CARTESIAN_POINT('Ctrl Pts',(81.9721850823073,8.41900051417354,138.072107073736));
#64474=CARTESIAN_POINT('Ctrl Pts',(81.950824479671,8.35087070605488,138.068250717793));
#64475=CARTESIAN_POINT('Ctrl Pts',(81.9259705990824,8.28401479486638,138.064394361849));
#64476=CARTESIAN_POINT('Ctrl Pts',(81.9011240605695,8.2171786335578,138.060539145111));
#64477=CARTESIAN_POINT('Ctrl Pts',(81.8727864619881,8.15161607716593,138.056683928372));
#64478=CARTESIAN_POINT('Ctrl Pts',(81.8411200555549,8.08770920012657,138.052828711633));
#64479=CARTESIAN_POINT('Ctrl Pts',(81.8094524110515,8.02379982450278,138.048973344166));
#64480=CARTESIAN_POINT('Ctrl Pts',(81.7744559179631,7.96154669104812,138.045117976699));
#64481=CARTESIAN_POINT('Ctrl Pts',(81.7363393757596,7.90130844424522,138.041262609232));
#64482=CARTESIAN_POINT('Ctrl Pts',(81.6981829359356,7.84100714443256,138.037403206247));
#64483=CARTESIAN_POINT('Ctrl Pts',(81.6569001879319,7.78272535272691,138.033543803262));
#64484=CARTESIAN_POINT('Ctrl Pts',(81.6127434984906,7.72679303702179,138.029684400277));
#64485=CARTESIAN_POINT('Ctrl Pts',(81.5685618071839,7.67082905199876,138.025822812068));
#64486=CARTESIAN_POINT('Ctrl Pts',(81.5215032557044,7.61721755643728,138.021961223858));
#64487=CARTESIAN_POINT('Ctrl Pts',(81.4718589648583,7.56625359631968,138.018099635649));
#64488=CARTESIAN_POINT('Ctrl Pts',(81.4221278195836,7.51520047296578,138.014231291455));
#64489=CARTESIAN_POINT('Ctrl Pts',(81.3698022597075,7.46680446283967,138.010362947262));
#64490=CARTESIAN_POINT('Ctrl Pts',(81.3152080016696,7.42132160499855,138.006494603069));
#64491=CARTESIAN_POINT('Ctrl Pts',(81.2827915374538,7.39431522215488,138.004197694096));
#64492=CARTESIAN_POINT('Ctrl Pts',(81.2495758162514,7.36833511378297,138.001900785124));
#64493=CARTESIAN_POINT('Ctrl Pts',(81.2156336505183,7.34342751736379,137.999603876152));
#64494=CARTESIAN_POINT('Ctrl Pts',(81.1584589632513,7.30147132496761,137.995734793277));
#64495=CARTESIAN_POINT('Ctrl Pts',(81.0989976384081,7.26239640879816,137.991865710402));
#64496=CARTESIAN_POINT('Ctrl Pts',(81.0375720156332,7.22646063622065,137.987996627528));
#64497=CARTESIAN_POINT('Ctrl Pts',(80.9762379139519,7.19057840613981,137.984133309392));
#64498=CARTESIAN_POINT('Ctrl Pts',(80.9129457396515,7.15782627890905,137.980269991257));
#64499=CARTESIAN_POINT('Ctrl Pts',(80.8480484684533,7.12842009049735,137.976406673121));
#64500=CARTESIAN_POINT('Ctrl Pts',(80.7832273216991,7.09904839551966,137.972547886654));
#64501=CARTESIAN_POINT('Ctrl Pts',(80.716805258211,7.07301504293452,137.968689100188));
#64502=CARTESIAN_POINT('Ctrl Pts',(80.6491600907199,7.05049012848959,137.964830313721));
#64503=CARTESIAN_POINT('Ctrl Pts',(80.5815575347049,7.02797940308269,137.960973958006));
#64504=CARTESIAN_POINT('Ctrl Pts',(80.512733863091,7.00897288420731,137.957117602291));
#64505=CARTESIAN_POINT('Ctrl Pts',(80.4430857491829,6.99359211988912,137.953261246575));
#64506=CARTESIAN_POINT('Ctrl Pts',(80.3734582100062,6.97821589919857,137.949406030065));
#64507=CARTESIAN_POINT('Ctrl Pts',(80.303007186142,6.96646341136475,137.945550813555));
#64508=CARTESIAN_POINT('Ctrl Pts',(80.232141673328,6.95840557259664,137.941695597045));
#64509=CARTESIAN_POINT('Ctrl Pts',(80.1612733898665,6.95034741878909,137.937840229806));
#64510=CARTESIAN_POINT('Ctrl Pts',(80.0899910682033,6.94598425352913,137.933984862568));
#64511=CARTESIAN_POINT('Ctrl Pts',(80.0187092661136,6.94533517919309,137.930129495329));
#64512=CARTESIAN_POINT('Ctrl Pts',(79.9473528513918,6.944685425453,137.926270092571));
#64513=CARTESIAN_POINT('Ctrl Pts',(79.8759974440872,6.94775752767298,137.922410689813));
#64514=CARTESIAN_POINT('Ctrl Pts',(79.8050571398562,6.95451843230525,137.918551287055));
#64515=CARTESIAN_POINT('Ctrl Pts',(79.7340766686538,6.96128316501617,137.914689699072));
#64516=CARTESIAN_POINT('Ctrl Pts',(79.6635122491687,6.97174078670801,137.910828111089));
#64517=CARTESIAN_POINT('Ctrl Pts',(79.5937696574457,6.98580674430475,137.906966523106));
#64518=CARTESIAN_POINT('Ctrl Pts',(79.5239050485447,6.99989731080131,137.903098179136));
#64519=CARTESIAN_POINT('Ctrl Pts',(79.4548656087432,7.01760869636137,137.899229835166));
#64520=CARTESIAN_POINT('Ctrl Pts',(79.3870431070686,7.03880612638427,137.895361491195));
#64521=CARTESIAN_POINT('Ctrl Pts',(79.3467720628865,7.05139254858813,137.893064580184));
#64522=CARTESIAN_POINT('Ctrl Pts',(79.3069297253038,7.06520708629177,137.890767669172));
#64523=CARTESIAN_POINT('Ctrl Pts',(79.2675944322128,7.08021364553911,137.88847075816));
#64524=CARTESIAN_POINT('Ctrl Pts',(79.201335224064,7.10549177758364,137.884601675388));
#64525=CARTESIAN_POINT('Ctrl Pts',(79.1362564439872,7.13425373682997,137.880732592616));
#64526=CARTESIAN_POINT('Ctrl Pts',(79.0727495655537,7.1663685772983,137.876863509844));
#64527=CARTESIAN_POINT('Ctrl Pts',(79.0093373092264,7.19843556824356,137.873000191814));
#64528=CARTESIAN_POINT('Ctrl Pts',(78.9474927356015,7.2338453067949,137.869136873784));
#64529=CARTESIAN_POINT('Ctrl Pts',(78.8875886226931,7.27241831158752,137.865273555754));
#64530=CARTESIAN_POINT('Ctrl Pts',(78.8277547773136,7.31094607024263,137.861414769397));
#64531=CARTESIAN_POINT('Ctrl Pts',(78.769857277877,7.35262946308729,137.857555983039));
#64532=CARTESIAN_POINT('Ctrl Pts',(78.7142439456327,7.39724333376594,137.853697196681));
#64533=CARTESIAN_POINT('Ctrl Pts',(78.6586656457248,7.44182910096534,137.849840841077));
#64534=CARTESIAN_POINT('Ctrl Pts',(78.6053690363638,7.48934138033019,137.845984485473));
#64535=CARTESIAN_POINT('Ctrl Pts',(78.5546713818588,7.53951283878216,137.842128129869));
#64536=CARTESIAN_POINT('Ctrl Pts',(78.5039887039606,7.58966947607113,137.838272913472));
#64537=CARTESIAN_POINT('Ctrl Pts',(78.4559038018054,7.64248339139704,137.834417697074));
#64538=CARTESIAN_POINT('Ctrl Pts',(78.410698085686,7.69764943749475,137.830562480677));
#64539=CARTESIAN_POINT('Ctrl Pts',(78.3654906021672,7.75281764040895,137.826707113553));
#64540=CARTESIAN_POINT('Ctrl Pts',(78.3231628343684,7.81033777953276,137.82285174643));
#64541=CARTESIAN_POINT('Ctrl Pts',(78.2839556788086,7.86987193194451,137.818996379306));
#64542=CARTESIAN_POINT('Ctrl Pts',(78.2447074840536,7.92946840037153,137.815136976664));
#64543=CARTESIAN_POINT('Ctrl Pts',(78.2085866897949,7.99108268383364,137.811277574023));
#64544=CARTESIAN_POINT('Ctrl Pts',(78.1757901239915,8.05434895930209,137.807418171382));
#64545=CARTESIAN_POINT('Ctrl Pts',(78.1429749885184,8.11765105662577,137.803556583517));
#64546=CARTESIAN_POINT('Ctrl Pts',(78.1134880292856,8.18260656544209,137.799694995651));
#64547=CARTESIAN_POINT('Ctrl Pts',(78.0874782954018,8.24882871997077,137.795833407786));
#64548=CARTESIAN_POINT('Ctrl Pts',(78.0614230565543,8.31516673253733,137.791965063935));
#64549=CARTESIAN_POINT('Ctrl Pts',(78.0388573428445,8.38277535426736,137.788096720083));
#64550=CARTESIAN_POINT('Ctrl Pts',(78.0198804134868,8.45125234797139,137.784228376231));
#64551=CARTESIAN_POINT('Ctrl Pts',(78.0086124552002,8.49191202974123,137.781931464211));
#64552=CARTESIAN_POINT('Ctrl Pts',(77.9986088005083,8.53287764689449,137.77963455219));
#64553=CARTESIAN_POINT('Ctrl Pts',(77.9898816146324,8.57406380840876,137.777337640169));
#64554=CARTESIAN_POINT('Ctrl Pts',(77.96929780918,8.67120485112274,137.771920179048));
#64555=CARTESIAN_POINT('Ctrl Pts',(77.9557497500285,8.76988496615924,137.766502717927));
#64556=CARTESIAN_POINT('Ctrl Pts',(77.9494139417945,8.86925452056241,137.761085256806));
#64557=CARTESIAN_POINT('Ctrl Pts',(77.9466809629302,8.91211801672847,137.758748411025));
#64558=CARTESIAN_POINT('Ctrl Pts',(77.9452893931581,8.95510950520192,137.756411565243));
#64559=CARTESIAN_POINT('Ctrl Pts',(77.9452508246244,8.99815913242806,137.754074719462));
#64560=CARTESIAN_POINT('Origin',(80.,9.,141.545925280538));
#64561=CARTESIAN_POINT('',(81.252039109102,10.6292316077768,138.906139397334));
#64562=CARTESIAN_POINT('',(81.252039109102,10.6292316077768,138.847890491445));
#64563=CARTESIAN_POINT('',(81.252039109102,10.6292316077768,141.545925280538));
#64564=CARTESIAN_POINT('',(77.9452500654425,8.99948140989303,138.39592528059));
#64565=CARTESIAN_POINT('Ctrl Pts',(81.252039109102,10.6292316077768,138.847890491445));
#64566=CARTESIAN_POINT('Ctrl Pts',(81.3085681361867,10.5857899311167,138.844035069102));
#64567=CARTESIAN_POINT('Ctrl Pts',(81.3628582544148,10.539383794229,138.840179646758));
#64568=CARTESIAN_POINT('Ctrl Pts',(81.4145905601348,10.4902788697682,138.836324224414));
#64569=CARTESIAN_POINT('Ctrl Pts',(81.4663198247622,10.4411768319489,138.832469028712));
#64570=CARTESIAN_POINT('Ctrl Pts',(81.5154912241929,10.3893766571317,138.82861383301));
#64571=CARTESIAN_POINT('Ctrl Pts',(81.5618216637909,10.3351818801247,138.824758637308));
#64572=CARTESIAN_POINT('Ctrl Pts',(81.6081976885301,10.2809337801495,138.820899648428));
#64573=CARTESIAN_POINT('Ctrl Pts',(81.6517268533141,10.224286741716,138.817040659547));
#64574=CARTESIAN_POINT('Ctrl Pts',(81.69216602467,10.1655778427255,138.813181670666));
#64575=CARTESIAN_POINT('Ctrl Pts',(81.7326245432036,10.1068408558323,138.809320835542));
#64576=CARTESIAN_POINT('Ctrl Pts',(81.7699898684382,10.0460404577005,138.805460000418));
#64577=CARTESIAN_POINT('Ctrl Pts',(81.804063459511,9.9835408464101,138.801599165294));
#64578=CARTESIAN_POINT('Ctrl Pts',(81.8381998446866,9.92092605480304,138.797731215051));
#64579=CARTESIAN_POINT('Ctrl Pts',(81.8690321646211,9.85660623253018,138.793863264807));
#64580=CARTESIAN_POINT('Ctrl Pts',(81.8964091252976,9.79096775660459,138.789995314564));
#64581=CARTESIAN_POINT('Ctrl Pts',(81.9206649226727,9.73281252195765,138.786568337462));
#64582=CARTESIAN_POINT('Ctrl Pts',(81.9422089599303,9.6736226676844,138.783141360359));
#64583=CARTESIAN_POINT('Ctrl Pts',(81.9609690692891,9.61367570572054,138.779714383257));
#64584=CARTESIAN_POINT('Ctrl Pts',(81.9821493409619,9.54599523989408,138.775845306342));
#64585=CARTESIAN_POINT('Ctrl Pts',(81.9998631210447,9.47708440544685,138.771976229427));
#64586=CARTESIAN_POINT('Ctrl Pts',(82.0139708209142,9.40733167690024,138.768107152513));
#64587=CARTESIAN_POINT('Ctrl Pts',(82.0280575006178,9.33768287840135,138.764243840438));
#64588=CARTESIAN_POINT('Ctrl Pts',(82.0385486698086,9.26719514802455,138.760380528364));
#64589=CARTESIAN_POINT('Ctrl Pts',(82.0453544272793,9.19627233454816,138.756517216289));
#64590=CARTESIAN_POINT('Ctrl Pts',(82.0521522013768,9.12543271582156,138.752658436005));
#64591=CARTESIAN_POINT('Ctrl Pts',(82.0552731047301,9.05415950897263,138.74879965572));
#64592=CARTESIAN_POINT('Ctrl Pts',(82.0546785546215,8.98286524939013,138.744940875435));
#64593=CARTESIAN_POINT('Ctrl Pts',(82.0540843790473,8.91161590133201,138.741084525973));
#64594=CARTESIAN_POINT('Ctrl Pts',(82.0497793976358,8.84034601147169,138.737228176511));
#64595=CARTESIAN_POINT('Ctrl Pts',(82.0417770670292,8.76947023824714,138.733371827049));
#64596=CARTESIAN_POINT('Ctrl Pts',(82.0337771005213,8.69861540358891,138.729516616854));
#64597=CARTESIAN_POINT('Ctrl Pts',(82.0220820077972,8.62815493687063,138.725661406659));
#64598=CARTESIAN_POINT('Ctrl Pts',(82.0067571394029,8.5584987588291,138.721806196464));
#64599=CARTESIAN_POINT('Ctrl Pts',(81.9914316720566,8.48883985836872,138.717950835594));
#64600=CARTESIAN_POINT('Ctrl Pts',(81.9724762539173,8.41998578295924,138.714095474723));
#64601=CARTESIAN_POINT('Ctrl Pts',(81.9500070585298,8.35233493672745,138.710240113852));
#64602=CARTESIAN_POINT('Ctrl Pts',(81.9275143441895,8.28461327901221,138.706380717499));
#64603=CARTESIAN_POINT('Ctrl Pts',(81.9015006640426,8.21809782657285,138.702521321145));
#64604=CARTESIAN_POINT('Ctrl Pts',(81.8721313874739,8.15316965658103,138.698661924792));
#64605=CARTESIAN_POINT('Ctrl Pts',(81.8427454819877,8.0882047241864,138.694800343244));
#64606=CARTESIAN_POINT('Ctrl Pts',(81.8100004209771,8.02482929510083,138.690938761696));
#64607=CARTESIAN_POINT('Ctrl Pts',(81.7741076041258,7.96339989799194,138.687077180148));
#64608=CARTESIAN_POINT('Ctrl Pts',(81.7381519911912,7.90186302741413,138.683208842591));
#64609=CARTESIAN_POINT('Ctrl Pts',(81.6990378939293,7.84227939256143,138.679340505034));
#64610=CARTESIAN_POINT('Ctrl Pts',(81.6570196914156,7.78497600650816,138.675472167477));
#64611=CARTESIAN_POINT('Ctrl Pts',(81.632069841485,7.75095001784094,138.673175200073));
#64612=CARTESIAN_POINT('Ctrl Pts',(81.6060968319195,7.7177273775482,138.670878232669));
#64613=CARTESIAN_POINT('Ctrl Pts',(81.5791601846843,7.68537051850804,138.668581265266));
#64614=CARTESIAN_POINT('Ctrl Pts',(81.5337872424878,7.63086759978652,138.664712180583));
#64615=CARTESIAN_POINT('Ctrl Pts',(81.4855004608702,7.57860968239259,138.6608430959));
#64616=CARTESIAN_POINT('Ctrl Pts',(81.4345505022327,7.52892474052351,138.656974011217));
#64617=CARTESIAN_POINT('Ctrl Pts',(81.3836764562117,7.47931382646594,138.653110691256));
#64618=CARTESIAN_POINT('Ctrl Pts',(81.3301474544714,7.43226861475334,138.649247371294));
#64619=CARTESIAN_POINT('Ctrl Pts',(81.2742540251656,7.38808367405459,138.645384051333));
#64620=CARTESIAN_POINT('Ctrl Pts',(81.2184261585317,7.34395056203783,138.641525263024));
#64621=CARTESIAN_POINT('Ctrl Pts',(81.1602397526017,7.3026713565031,138.637666474715));
#64622=CARTESIAN_POINT('Ctrl Pts',(81.1000204674381,7.26450222307339,138.633807686406));
#64623=CARTESIAN_POINT('Ctrl Pts',(81.0398391158282,7.22635713328464,138.629951328839));
#64624=CARTESIAN_POINT('Ctrl Pts',(80.9776278349285,7.19131848821236,138.626094971273));
#64625=CARTESIAN_POINT('Ctrl Pts',(80.913742293429,7.15959988488941,138.622238613706));
#64626=CARTESIAN_POINT('Ctrl Pts',(80.8498756242241,7.12789065149294,138.618383395337));
#64627=CARTESIAN_POINT('Ctrl Pts',(80.7843361111867,7.09949972866039,138.614528176969));
#64628=CARTESIAN_POINT('Ctrl Pts',(80.7175035888128,7.07459454593566,138.610672958601));
#64629=CARTESIAN_POINT('Ctrl Pts',(80.6506684534069,7.04968838946285,138.6068175895));
#64630=CARTESIAN_POINT('Ctrl Pts',(80.5825406642678,7.02826841124369,138.6029622204));
#64631=CARTESIAN_POINT('Ctrl Pts',(80.5135179456951,7.0104530963184,138.599106851299));
#64632=CARTESIAN_POINT('Ctrl Pts',(80.4444229793004,6.9926191336532,138.595247446687));
#64633=CARTESIAN_POINT('Ctrl Pts',(80.3744316848496,6.97839748787347,138.591388042074));
#64634=CARTESIAN_POINT('Ctrl Pts',(80.3039539124666,6.96785591514867,138.587528637461));
#64635=CARTESIAN_POINT('Ctrl Pts',(80.2334362350443,6.95730837370693,138.583667047625));
#64636=CARTESIAN_POINT('Ctrl Pts',(80.1624320151168,6.95044510005407,138.579805457789));
#64637=CARTESIAN_POINT('Ctrl Pts',(80.0913554446739,6.94728186415464,138.575943867953));
#64638=CARTESIAN_POINT('Ctrl Pts',(80.0201545236788,6.9441130940809,138.572075522151));
#64639=CARTESIAN_POINT('Ctrl Pts',(79.9488814853711,6.9446572822268,138.56820717635));
#64640=CARTESIAN_POINT('Ctrl Pts',(79.8779490358511,6.94887808147582,138.564338830549));
#64641=CARTESIAN_POINT('Ctrl Pts',(79.8358317184722,6.95138425097605,138.562041936124));
#64642=CARTESIAN_POINT('Ctrl Pts',(79.7938343729143,6.955185648202,138.559745041699));
#64643=CARTESIAN_POINT('Ctrl Pts',(79.7520417263487,6.96026613083279,138.557448147274));
#64644=CARTESIAN_POINT('Ctrl Pts',(79.6816426567328,6.96882412559498,138.553579063983));
#64645=CARTESIAN_POINT('Ctrl Pts',(79.6115492768566,6.98104777513134,138.549709980692));
#64646=CARTESIAN_POINT('Ctrl Pts',(79.5421730827995,6.99690437662436,138.545840897401));
#64647=CARTESIAN_POINT('Ctrl Pts',(79.4729002555485,7.01273735263207,138.541977578836));
#64648=CARTESIAN_POINT('Ctrl Pts',(79.4043429627509,7.03219242877522,138.538114260271));
#64649=CARTESIAN_POINT('Ctrl Pts',(79.3369062578221,7.05518529119493,138.534250941707));
#64650=CARTESIAN_POINT('Ctrl Pts',(79.2695486557868,7.07815118311026,138.530392154794));
#64651=CARTESIAN_POINT('Ctrl Pts',(79.2033094882509,7.10464646237816,138.526533367881));
#64652=CARTESIAN_POINT('Ctrl Pts',(79.1385805998373,7.13453647059951,138.522674580969));
#64653=CARTESIAN_POINT('Ctrl Pts',(79.0738924856827,7.16440765039717,138.518818224797));
#64654=CARTESIAN_POINT('Ctrl Pts',(79.0107132031554,7.19766911338125,138.514961868626));
#64655=CARTESIAN_POINT('Ctrl Pts',(78.9494151097006,7.23413790154083,138.511105512455));
#64656=CARTESIAN_POINT('Ctrl Pts',(78.8881351241464,7.27059591655638,138.507250295479));
#64657=CARTESIAN_POINT('Ctrl Pts',(78.8287356416693,7.31025912751879,138.503395078503));
#64658=CARTESIAN_POINT('Ctrl Pts',(78.7715633399465,7.35289923358147,138.499539861527));
#64659=CARTESIAN_POINT('Ctrl Pts',(78.7143888028114,7.39554100685382,138.495684493814));
#64660=CARTESIAN_POINT('Ctrl Pts',(78.6594420074097,7.44115961412183,138.4918291261));
#64661=CARTESIAN_POINT('Ctrl Pts',(78.6070382146028,7.48948517818491,138.487973758387));
#64662=CARTESIAN_POINT('Ctrl Pts',(78.554579569164,7.5378613260748,138.484114355144));
#64663=CARTESIAN_POINT('Ctrl Pts',(78.504669597791,7.58894975696965,138.480254951901));
#64664=CARTESIAN_POINT('Ctrl Pts',(78.4575875191527,7.64244289202017,138.476395548658));
#64665=CARTESIAN_POINT('Ctrl Pts',(78.4104787821856,7.69596631540177,138.472533960184));
#64666=CARTESIAN_POINT('Ctrl Pts',(78.3662014270749,7.75189677233906,138.468672371709));
#64667=CARTESIAN_POINT('Ctrl Pts',(78.3249933520973,7.8098948399483,138.464810783235));
#64668=CARTESIAN_POINT('Ctrl Pts',(78.2837131820615,7.86799437733164,138.460942438768));
#64669=CARTESIAN_POINT('Ctrl Pts',(78.2455132735932,7.92816833730001,138.457074094301));
#64670=CARTESIAN_POINT('Ctrl Pts',(78.2105869337642,7.99005027804126,138.453205749834));
#64671=CARTESIAN_POINT('Ctrl Pts',(78.1898487213581,8.02679391729671,138.450908842983));
#64672=CARTESIAN_POINT('Ctrl Pts',(78.170263755318,8.06413927692115,138.448611936133));
#64673=CARTESIAN_POINT('Ctrl Pts',(78.1518644287987,8.10200641819649,138.446315029283));
#64674=CARTESIAN_POINT('Ctrl Pts',(78.1182272557155,8.17123414693458,138.442115883558));
#64675=CARTESIAN_POINT('Ctrl Pts',(78.0884378127231,8.24244848245112,138.437916737834));
#64676=CARTESIAN_POINT('Ctrl Pts',(78.0627161720013,8.3152161419288,138.433717592109));
#64677=CARTESIAN_POINT('Ctrl Pts',(78.0373092445351,8.38709346368423,138.429569824399));
#64678=CARTESIAN_POINT('Ctrl Pts',(78.0158713067275,8.46048596644007,138.425422056689));
#64679=CARTESIAN_POINT('Ctrl Pts',(77.9985686429253,8.53495152358244,138.421274288979));
#64680=CARTESIAN_POINT('Ctrl Pts',(77.980944489384,8.61080067765593,138.417049454247));
#64681=CARTESIAN_POINT('Ctrl Pts',(77.9676110562608,8.68776283901531,138.412824619516));
#64682=CARTESIAN_POINT('Ctrl Pts',(77.958692352975,8.76534993565489,138.408599784784));
#64683=CARTESIAN_POINT('Ctrl Pts',(77.9497736496892,8.84293703229448,138.404374950053));
#64684=CARTESIAN_POINT('Ctrl Pts',(77.9452698355283,8.92114867256129,138.400150115321));
#64685=CARTESIAN_POINT('Ctrl Pts',(77.9452500654424,8.99948140989304,138.39592528059));
#64686=CARTESIAN_POINT('Ctrl Pts',(77.9452500654422,8.99948141084969,138.395925280538));
#64687=CARTESIAN_POINT('Ctrl Pts',(77.9452314949112,9.07306142557031,138.391956781385));
#64688=CARTESIAN_POINT('Ctrl Pts',(77.949169578864,9.14659881544574,138.387988282232));
#64689=CARTESIAN_POINT('Ctrl Pts',(77.9570245321472,9.21965609541188,138.38401978308));
#64690=CARTESIAN_POINT('Ctrl Pts',(77.9650800376541,9.29457866972499,138.379949960431));
#64691=CARTESIAN_POINT('Ctrl Pts',(77.9772551019451,9.36899578842017,138.375880137782));
#64692=CARTESIAN_POINT('Ctrl Pts',(77.9934509662062,9.44244608426484,138.371810315133));
#64693=CARTESIAN_POINT('Ctrl Pts',(78.0092901747818,9.51427890140046,138.367830115696));
#64694=CARTESIAN_POINT('Ctrl Pts',(78.0289746941144,9.58518663635699,138.36384991626));
#64695=CARTESIAN_POINT('Ctrl Pts',(78.052361793148,9.65475413531354,138.359869716823));
#64696=CARTESIAN_POINT('Ctrl Pts',(78.0765388125048,9.72667133917291,138.355755082568));
#64697=CARTESIAN_POINT('Ctrl Pts',(78.1046727995203,9.79715566665106,138.351640448313));
#64698=CARTESIAN_POINT('Ctrl Pts',(78.1365533044659,9.86577362826731,138.347525814057));
#64699=CARTESIAN_POINT('Ctrl Pts',(78.1684338094115,9.93439158988357,138.343411179802));
#64700=CARTESIAN_POINT('Ctrl Pts',(78.2040605214235,10.0011427673637,138.339296545546));
#64701=CARTESIAN_POINT('Ctrl Pts',(78.2431735357086,10.0656257958895,138.335181911291));
#64702=CARTESIAN_POINT('Ctrl Pts',(78.2799523824072,10.1262606373654,138.331312828193));
#64703=CARTESIAN_POINT('Ctrl Pts',(78.3199460623988,10.1851079346325,138.327443745094));
#64704=CARTESIAN_POINT('Ctrl Pts',(78.3629553810925,10.2418061355163,138.323574661996));
#64705=CARTESIAN_POINT('Ctrl Pts',(78.4059006180832,10.2984198589572,138.319711343635));
#64706=CARTESIAN_POINT('Ctrl Pts',(78.4518522838045,10.3528904581085,138.315848025274));
#64707=CARTESIAN_POINT('Ctrl Pts',(78.5005668003867,10.4048834978024,138.311984706913));
#64708=CARTESIAN_POINT('Ctrl Pts',(78.5492241749031,10.456815549727,138.308125920219));
#64709=CARTESIAN_POINT('Ctrl Pts',(78.6006376323835,10.506275462065,138.304267133526));
#64710=CARTESIAN_POINT('Ctrl Pts',(78.6545231511545,10.5529615615722,138.300408346833));
#64711=CARTESIAN_POINT('Ctrl Pts',(78.7083747260272,10.5996182522837,138.29655199089));
#64712=CARTESIAN_POINT('Ctrl Pts',(78.7646949064156,10.6435042794298,138.292695634947));
#64713=CARTESIAN_POINT('Ctrl Pts',(78.823163674952,10.6843556116651,138.288839279005));
#64714=CARTESIAN_POINT('Ctrl Pts',(78.8816151712512,10.7251948760234,138.284984062267));
#64715=CARTESIAN_POINT('Ctrl Pts',(78.9422135976179,10.7630009471533,138.281128845529));
#64716=CARTESIAN_POINT('Ctrl Pts',(79.0046081847904,10.7975518620373,138.277273628791));
#64717=CARTESIAN_POINT('Ctrl Pts',(79.0670052114209,10.8321041277678,138.273418261324));
#64718=CARTESIAN_POINT('Ctrl Pts',(79.1311981122362,10.8634007511762,138.269562893858));
#64719=CARTESIAN_POINT('Ctrl Pts',(79.1968111602771,10.8912655155331,138.265707526391));
#64720=CARTESIAN_POINT('Ctrl Pts',(79.2624928872782,10.9191594466959,138.261848123407));
#64721=CARTESIAN_POINT('Ctrl Pts',(79.3295972808572,10.9436141576524,138.257988720422));
#64722=CARTESIAN_POINT('Ctrl Pts',(79.3977290915692,10.9645017982578,138.254129317438));
#64723=CARTESIAN_POINT('Ctrl Pts',(79.4658994790494,10.9854012656098,138.250267729229));
#64724=CARTESIAN_POINT('Ctrl Pts',(79.5350979702551,11.0027295239452,138.246406141021));
#64725=CARTESIAN_POINT('Ctrl Pts',(79.6049173043078,11.0164094886864,138.242544552812));
#64726=CARTESIAN_POINT('Ctrl Pts',(79.6748587897351,11.0301133870059,138.238676208619));
#64727=CARTESIAN_POINT('Ctrl Pts',(79.7454228055223,11.0401561797858,138.234807864426));
#64728=CARTESIAN_POINT('Ctrl Pts',(79.8161958231075,11.0465125426092,138.230939520234));
#64729=CARTESIAN_POINT('Ctrl Pts',(79.8582187588651,11.0502867638547,138.228642611255));
#64730=CARTESIAN_POINT('Ctrl Pts',(79.9003153380743,11.0527622827936,138.226345702277));
#64731=CARTESIAN_POINT('Ctrl Pts',(79.9423993743182,11.0539424846916,138.224048793299));
#64732=CARTESIAN_POINT('Ctrl Pts',(80.0132740183776,11.0559300884698,138.220180518752));
#64733=CARTESIAN_POINT('Ctrl Pts',(80.0843904485706,11.0542488114017,138.216312244204));
#64734=CARTESIAN_POINT('Ctrl Pts',(80.1553371324466,11.048869917243,138.212443969656));
#64735=CARTESIAN_POINT('Ctrl Pts',(80.2261854267701,11.0434984825871,138.20858105967));
#64736=CARTESIAN_POINT('Ctrl Pts',(80.2968639617745,11.0344396404561,138.204718149683));
#64737=CARTESIAN_POINT('Ctrl Pts',(80.3669597863491,11.0217166165669,138.200855239696));
#64738=CARTESIAN_POINT('Ctrl Pts',(80.4369818596963,11.0090069791901,138.196996394065));
#64739=CARTESIAN_POINT('Ctrl Pts',(80.5064219639407,10.9926408981213,138.193137548434));
#64740=CARTESIAN_POINT('Ctrl Pts',(80.5748725845545,10.9726933552956,138.189278702803));
#64741=CARTESIAN_POINT('Ctrl Pts',(80.643281445159,10.9527579819663,138.185422211356));
#64742=CARTESIAN_POINT('Ctrl Pts',(80.7107015541047,10.9292456161871,138.18156571991));
#64743=CARTESIAN_POINT('Ctrl Pts',(80.7767374728931,10.902281908841,138.177709228464));
#64744=CARTESIAN_POINT('Ctrl Pts',(80.8427490507325,10.875328140362,138.173854158527));
#64745=CARTESIAN_POINT('Ctrl Pts',(80.907377003523,10.8449257435894,138.16999908859));
#64746=CARTESIAN_POINT('Ctrl Pts',(80.970244639271,10.8112489896384,138.166144018653));
#64747=CARTESIAN_POINT('Ctrl Pts',(81.0331314679079,10.7775619544959,138.1622877718));
#64748=CARTESIAN_POINT('Ctrl Pts',(81.0942564769342,10.7405987939562,138.158431524947));
#64749=CARTESIAN_POINT('Ctrl Pts',(81.1532675878569,10.7005797344726,138.154575278094));
#64750=CARTESIAN_POINT('Ctrl Pts',(81.1868977422625,10.6777730608045,138.15237762116));
#64751=CARTESIAN_POINT('Ctrl Pts',(81.2198418360838,10.6539747104964,138.150179964226));
#64752=CARTESIAN_POINT('Ctrl Pts',(81.252039109102,10.6292316077768,138.147982307292));
#64753=CARTESIAN_POINT('',(77.9452502723122,9.00105785954894,138.454074719513));
#64754=CARTESIAN_POINT('Ctrl Pts',(77.9452502723127,9.00105786047649,138.454074719462));
#64755=CARTESIAN_POINT('Ctrl Pts',(77.9452815714097,9.06185208850311,138.450761929014));
#64756=CARTESIAN_POINT('Ctrl Pts',(77.9480107215796,9.12257484666211,138.447449138566));
#64757=CARTESIAN_POINT('Ctrl Pts',(77.9534202484127,9.18305431678253,138.444136348118));
#64758=CARTESIAN_POINT('Ctrl Pts',(77.9597381600835,9.25368969061685,138.440267263431));
#64759=CARTESIAN_POINT('Ctrl Pts',(77.9697295884017,9.32413594375426,138.436398178743));
#64760=CARTESIAN_POINT('Ctrl Pts',(77.983374915349,9.39398074883996,138.432529094056));
#64761=CARTESIAN_POINT('Ctrl Pts',(77.9969999115152,9.46372148903559,138.428665774091));
#64762=CARTESIAN_POINT('Ctrl Pts',(78.0142679075233,9.53286208707632,138.424802454126));
#64763=CARTESIAN_POINT('Ctrl Pts',(78.0351074957408,9.60099501595759,138.42093913416));
#64764=CARTESIAN_POINT('Ctrl Pts',(78.055922639241,9.6690480253051,138.417080345847));
#64765=CARTESIAN_POINT('Ctrl Pts',(78.0803009118727,9.73609525104177,138.413221557534));
#64766=CARTESIAN_POINT('Ctrl Pts',(78.108120167371,9.80174076944595,138.40936276922));
#64767=CARTESIAN_POINT('Ctrl Pts',(78.1359218988618,9.86734493618424,138.405506411649));
#64768=CARTESIAN_POINT('Ctrl Pts',(78.1671601237219,9.93154870116641,138.401650054078));
#64769=CARTESIAN_POINT('Ctrl Pts',(78.2016638015601,9.99397408410912,138.397793696507));
#64770=CARTESIAN_POINT('Ctrl Pts',(78.2361572867389,10.0563810261,138.393938478134));
#64771=CARTESIAN_POINT('Ctrl Pts',(78.2739140749496,10.1170102040835,138.390083259762));
#64772=CARTESIAN_POINT('Ctrl Pts',(78.3147169902911,10.1755078645787,138.386228041389));
#64773=CARTESIAN_POINT('Ctrl Pts',(78.3555215009537,10.234007812228,138.382372672284));
#64774=CARTESIAN_POINT('Ctrl Pts',(78.3993720954813,10.2903756797582,138.37851730318));
#64775=CARTESIAN_POINT('Ctrl Pts',(78.4460090448423,10.3442877942569,138.374661934075));
#64776=CARTESIAN_POINT('Ctrl Pts',(78.4926948102755,10.3982563399268,138.370802529458));
#64777=CARTESIAN_POINT('Ctrl Pts',(78.5421724341588,10.4497636331277,138.366943124841));
#64778=CARTESIAN_POINT('Ctrl Pts',(78.5941433601851,10.4985208276124,138.363083720224));
#64779=CARTESIAN_POINT('Ctrl Pts',(78.6461437125364,10.5473056287835,138.359222130383));
#64780=CARTESIAN_POINT('Ctrl Pts',(78.7006398060556,10.5933369178648,138.355360540543));
#64781=CARTESIAN_POINT('Ctrl Pts',(78.757299944185,10.6363661368341,138.351498950702));
#64782=CARTESIAN_POINT('Ctrl Pts',(78.8140592108931,10.679470636688,138.347630604897));
#64783=CARTESIAN_POINT('Ctrl Pts',(78.8729896794131,10.7195623069091,138.343762259091));
#64784=CARTESIAN_POINT('Ctrl Pts',(78.9337312317319,10.756436300102,138.339893913285));
#64785=CARTESIAN_POINT('Ctrl Pts',(78.9697975343688,10.7783308442346,138.337597018899));
#64786=CARTESIAN_POINT('Ctrl Pts',(79.0065018721909,10.7990918456519,138.335300124513));
#64787=CARTESIAN_POINT('Ctrl Pts',(79.0437653768912,10.8186843893507,138.333003230127));
#64788=CARTESIAN_POINT('Ctrl Pts',(79.1065351778374,10.8516877280838,138.329134146835));
#64789=CARTESIAN_POINT('Ctrl Pts',(79.1711385346629,10.8815022513654,138.325265063544));
#64790=CARTESIAN_POINT('Ctrl Pts',(79.2372183974119,10.907920802668,138.321395980252));
#64791=CARTESIAN_POINT('Ctrl Pts',(79.303199804712,10.934299991747,138.317532661687));
#64792=CARTESIAN_POINT('Ctrl Pts',(79.370652903771,10.9572930735746,138.313669343123));
#64793=CARTESIAN_POINT('Ctrl Pts',(79.4391965878754,10.9767390053948,138.309806024558));
#64794=CARTESIAN_POINT('Ctrl Pts',(79.507659870606,10.9961621272414,138.305947237644));
#64795=CARTESIAN_POINT('Ctrl Pts',(79.577210732286,11.0120462318728,138.302088450731));
#64796=CARTESIAN_POINT('Ctrl Pts',(79.6474502948483,11.0242791971212,138.298229663818));
#64797=CARTESIAN_POINT('Ctrl Pts',(79.7176456118477,11.0365044565352,138.294373307647));
#64798=CARTESIAN_POINT('Ctrl Pts',(79.7885282915718,11.0450830564567,138.290516951475));
#64799=CARTESIAN_POINT('Ctrl Pts',(79.8596880116023,11.0499536844553,138.286660595303));
#64800=CARTESIAN_POINT('Ctrl Pts',(79.9308267105368,11.0548228736352,138.282805378327));
#64801=CARTESIAN_POINT('Ctrl Pts',(80.0022418029183,11.0559862323347,138.27895016135));
#64802=CARTESIAN_POINT('Ctrl Pts',(80.0735182970643,11.0534343482315,138.275094944374));
#64803=CARTESIAN_POINT('Ctrl Pts',(80.1447975780902,11.0508823643506,138.27123957666));
#64804=CARTESIAN_POINT('Ctrl Pts',(80.2159377647285,11.0446148688463,138.267384208947));
#64805=CARTESIAN_POINT('Ctrl Pts',(80.2865260569924,11.034674514797,138.263528841233));
#64806=CARTESIAN_POINT('Ctrl Pts',(80.3571882361534,11.0247237558789,138.25966943799));
#64807=CARTESIAN_POINT('Ctrl Pts',(80.4272968857301,11.0110925318276,138.255810034746));
#64808=CARTESIAN_POINT('Ctrl Pts',(80.4964474056167,10.9938750050985,138.251950631503));
#64809=CARTESIAN_POINT('Ctrl Pts',(80.5656370791975,10.976647729639,138.248089043028));
#64810=CARTESIAN_POINT('Ctrl Pts',(80.633867078276,10.9558302510362,138.244227454553));
#64811=CARTESIAN_POINT('Ctrl Pts',(80.7007486756041,10.9315664255052,138.240365866078));
#64812=CARTESIAN_POINT('Ctrl Pts',(80.7677472847718,10.9072601495099,138.23649752161));
#64813=CARTESIAN_POINT('Ctrl Pts',(80.8333923346689,10.8794956777869,138.232629177143));
#64814=CARTESIAN_POINT('Ctrl Pts',(80.8973164055592,10.848464452137,138.228760832675));
#64815=CARTESIAN_POINT('Ctrl Pts',(80.9352726003437,10.8300390416655,138.226463925829));
#64816=CARTESIAN_POINT('Ctrl Pts',(80.97262251972,10.8104627729485,138.224167018982));
#64817=CARTESIAN_POINT('Ctrl Pts',(81.009294052642,10.7897829694691,138.221870112135));
#64818=CARTESIAN_POINT('Ctrl Pts',(81.0710608673569,10.7549514397217,138.218001372316));
#64819=CARTESIAN_POINT('Ctrl Pts',(81.1311434378446,10.7168505093526,138.214132632498));
#64820=CARTESIAN_POINT('Ctrl Pts',(81.1891741649048,10.6756677379549,138.210263892679));
#64821=CARTESIAN_POINT('Ctrl Pts',(81.2104094466327,10.6605976570294,138.208848198199));
#64822=CARTESIAN_POINT('Ctrl Pts',(81.2313701765688,10.6451153604314,138.207432503719));
#64823=CARTESIAN_POINT('Ctrl Pts',(81.252039109102,10.6292316077768,138.206016809239));
#64824=CARTESIAN_POINT('Ctrl Pts',(81.252039109102,10.6292316077768,138.906139397334));
#64825=CARTESIAN_POINT('Ctrl Pts',(81.3085407521982,10.5858109752852,138.902270840373));
#64826=CARTESIAN_POINT('Ctrl Pts',(81.3627052394123,10.5395059841607,138.898402283413));
#64827=CARTESIAN_POINT('Ctrl Pts',(81.4142409434871,10.4906106521371,138.894533726453));
#64828=CARTESIAN_POINT('Ctrl Pts',(81.4402844253443,10.4659014778799,138.892578757663));
#64829=CARTESIAN_POINT('Ctrl Pts',(81.4656571881398,10.4405313514877,138.890623788874));
#64830=CARTESIAN_POINT('Ctrl Pts',(81.4903255365783,10.4145413947717,138.888668820084));
#64831=CARTESIAN_POINT('Ctrl Pts',(81.5391460723885,10.3631052957673,138.884799788315));
#64832=CARTESIAN_POINT('Ctrl Pts',(81.5853962816342,10.3090380201616,138.880930756546));
#64833=CARTESIAN_POINT('Ctrl Pts',(81.6287797626174,10.2526268588004,138.877061724777));
#64834=CARTESIAN_POINT('Ctrl Pts',(81.6720985943052,10.1962997603531,138.873198458571));
#64835=CARTESIAN_POINT('Ctrl Pts',(81.712558883679,10.1376360912374,138.869335192365));
#64836=CARTESIAN_POINT('Ctrl Pts',(81.7499020673934,10.0769588279188,138.865471926159));
#64837=CARTESIAN_POINT('Ctrl Pts',(81.7872014376145,10.0163527551793,138.861613192592));
#64838=CARTESIAN_POINT('Ctrl Pts',(81.8213907132125,9.95373819263796,138.857754459025));
#64839=CARTESIAN_POINT('Ctrl Pts',(81.8522535789957,9.88946851636106,138.853895725458));
#64840=CARTESIAN_POINT('Ctrl Pts',(81.883096998617,9.82523933530386,138.850039423213));
#64841=CARTESIAN_POINT('Ctrl Pts',(81.9106179568823,9.75935754641112,138.846183120968));
#64842=CARTESIAN_POINT('Ctrl Pts',(81.9346459246051,9.69220134997619,138.842326818723));
#64843=CARTESIAN_POINT('Ctrl Pts',(81.9586667910779,9.62506500095187,138.838471656174));
#64844=CARTESIAN_POINT('Ctrl Pts',(81.9791965528858,9.55665544927177,138.834616493624));
#64845=CARTESIAN_POINT('Ctrl Pts',(81.9961133578074,9.48736949564268,138.830761331075));
#64846=CARTESIAN_POINT('Ctrl Pts',(82.0130308223352,9.41808084047218,138.826906018208));
#64847=CARTESIAN_POINT('Ctrl Pts',(82.0263349372039,9.34791618796618,138.823050705341));
#64848=CARTESIAN_POINT('Ctrl Pts',(82.0359545511563,9.27728438132338,138.819195392474));
#64849=CARTESIAN_POINT('Ctrl Pts',(82.0455842337334,9.20657864602208,138.815336044342));
#64850=CARTESIAN_POINT('Ctrl Pts',(82.0515216513016,9.1354052628522,138.811476696209));
#64851=CARTESIAN_POINT('Ctrl Pts',(82.0537474515665,9.06417918419796,138.807617348076));
#64852=CARTESIAN_POINT('Ctrl Pts',(82.0559745119851,8.99291278035721,138.803755814944));
#64853=CARTESIAN_POINT('Ctrl Pts',(82.0544857820866,8.92159410756425,138.799894281813));
#64854=CARTESIAN_POINT('Ctrl Pts',(82.0493140468048,8.85063634957434,138.796032748681));
#64855=CARTESIAN_POINT('Ctrl Pts',(82.0441332629383,8.77955444229137,138.792164459323));
#64856=CARTESIAN_POINT('Ctrl Pts',(82.0352566688447,8.70883519271668,138.788296169966));
#64857=CARTESIAN_POINT('Ctrl Pts',(82.022768635003,8.63888421282376,138.784427880609));
#64858=CARTESIAN_POINT('Ctrl Pts',(82.0153519407318,8.59734004034512,138.78213048777));
#64859=CARTESIAN_POINT('Ctrl Pts',(82.0066623866894,8.55606663228185,138.779833094931));
#64860=CARTESIAN_POINT('Ctrl Pts',(81.9967259333571,8.51514630087099,138.777535702093));
#64861=CARTESIAN_POINT('Ctrl Pts',(81.9799917090061,8.44623136880734,138.773666606562));
#64862=CARTESIAN_POINT('Ctrl Pts',(81.9596527305356,8.37804882930313,138.769797511031));
#64863=CARTESIAN_POINT('Ctrl Pts',(81.9357896132602,8.31100352998452,138.765928415499));
#64864=CARTESIAN_POINT('Ctrl Pts',(81.9119620501116,8.24405812277302,138.76206508461));
#64865=CARTESIAN_POINT('Ctrl Pts',(81.8846209321863,8.17824704634329,138.75820175372));
#64866=CARTESIAN_POINT('Ctrl Pts',(81.8538973778349,8.11396271243415,138.75433842283));
#64867=CARTESIAN_POINT('Ctrl Pts',(81.8232098614146,8.04975378237869,138.750479623527));
#64868=CARTESIAN_POINT('Ctrl Pts',(81.7891479978466,7.98706847381701,138.746620824224));
#64869=CARTESIAN_POINT('Ctrl Pts',(81.7518913592263,7.92628019112604,138.742762024921));
#64870=CARTESIAN_POINT('Ctrl Pts',(81.7146581890478,7.86553019976588,138.738905656326));
#64871=CARTESIAN_POINT('Ctrl Pts',(81.6742344896948,7.80667527669055,138.735049287731));
#64872=CARTESIAN_POINT('Ctrl Pts',(81.6308455216996,7.75006382288835,138.731192919135));
#64873=CARTESIAN_POINT('Ctrl Pts',(81.5874693709153,7.69346909225297,138.727337689721));
#64874=CARTESIAN_POINT('Ctrl Pts',(81.541129985835,7.63911690054514,138.723482460307));
#64875=CARTESIAN_POINT('Ctrl Pts',(81.4920946545808,7.58732484120678,138.719627230893));
#64876=CARTESIAN_POINT('Ctrl Pts',(81.4430574061278,7.53553075688624,138.715771850746));
#64877=CARTESIAN_POINT('Ctrl Pts',(81.3913243378103,7.48629735490751,138.711916470599));
#64878=CARTESIAN_POINT('Ctrl Pts',(81.3372003536463,7.43990616413363,138.708061090452));
#64879=CARTESIAN_POINT('Ctrl Pts',(81.2830197177678,7.39346641558012,138.704201674869));
#64880=CARTESIAN_POINT('Ctrl Pts',(81.226443539926,7.34987513368378,138.700342259285));
#64881=CARTESIAN_POINT('Ctrl Pts',(81.1678099508912,7.30937364237406,138.696482843702));
#64882=CARTESIAN_POINT('Ctrl Pts',(81.1091431635748,7.26884921915905,138.692621242921));
#64883=CARTESIAN_POINT('Ctrl Pts',(81.0484170598279,7.23141832413785,138.68875964214));
#64884=CARTESIAN_POINT('Ctrl Pts',(80.9859965624117,7.19727751957983,138.684898041359));
#64885=CARTESIAN_POINT('Ctrl Pts',(80.9234668614125,7.16307698627339,138.681029684775));
#64886=CARTESIAN_POINT('Ctrl Pts',(80.8592372863073,7.1321782460189,138.67716132819));
#64887=CARTESIAN_POINT('Ctrl Pts',(80.7936943772722,7.10473041548533,138.673292971605));
#64888=CARTESIAN_POINT('Ctrl Pts',(80.7547789678034,7.08843355622214,138.670996175771));
#64889=CARTESIAN_POINT('Ctrl Pts',(80.7154009159473,7.07335229548095,138.668699379936));
#64890=CARTESIAN_POINT('Ctrl Pts',(80.6756433883754,7.0595094501017,138.666402584101));
#64891=CARTESIAN_POINT('Ctrl Pts',(80.6086694833816,7.03619035890327,138.66253349577));
#64892=CARTESIAN_POINT('Ctrl Pts',(80.5403557403813,7.01629696299707,138.658664407438));
#64893=CARTESIAN_POINT('Ctrl Pts',(80.4710860080223,6.99998111620275,138.654795319106));
#64894=CARTESIAN_POINT('Ctrl Pts',(80.401919481385,6.98368957856462,138.650931995371));
#64895=CARTESIAN_POINT('Ctrl Pts',(80.3318002616527,6.97096512014625,138.647068671636));
#64896=CARTESIAN_POINT('Ctrl Pts',(80.2611291415901,6.9619104205378,138.643205347901));
#64897=CARTESIAN_POINT('Ctrl Pts',(80.1905409151791,6.9528663416343,138.639346555649));
#64898=CARTESIAN_POINT('Ctrl Pts',(80.119402553801,6.94748353289814,138.635487763397));
#64899=CARTESIAN_POINT('Ctrl Pts',(80.04812516192,6.94581365711624,138.631628971146));
#64900=CARTESIAN_POINT('Ctrl Pts',(79.9768926674239,6.94414483318336,138.627772609534));
#64901=CARTESIAN_POINT('Ctrl Pts',(79.9055218006725,6.94618431348433,138.623916247922));
#64902=CARTESIAN_POINT('Ctrl Pts',(79.8344274404792,6.95193181509166,138.62005988631));
#64903=CARTESIAN_POINT('Ctrl Pts',(79.7633540803268,6.95767761898671,138.616204663801));
#64904=CARTESIAN_POINT('Ctrl Pts',(79.6925575485226,6.96712923061955,138.612349441292));
#64905=CARTESIAN_POINT('Ctrl Pts',(79.622449636365,6.98023434888622,138.608494218782));
#64906=CARTESIAN_POINT('Ctrl Pts',(79.5523389814721,6.99333997984638,138.60463884545));
#64907=CARTESIAN_POINT('Ctrl Pts',(79.4829174768171,7.01009930978598,138.600783472118));
#64908=CARTESIAN_POINT('Ctrl Pts',(79.4145870167333,7.03040887453188,138.596928098786));
#64909=CARTESIAN_POINT('Ctrl Pts',(79.3461850315659,7.05073969836654,138.593068689833));
#64910=CARTESIAN_POINT('Ctrl Pts',(79.278876837367,7.07462803672365,138.589209280879));
#64911=CARTESIAN_POINT('Ctrl Pts',(79.2130485724695,7.10192070418339,138.585349871925));
#64912=CARTESIAN_POINT('Ctrl Pts',(79.1471830339926,7.12922882542137,138.581488277679));
#64913=CARTESIAN_POINT('Ctrl Pts',(79.0827995316105,7.15994490377779,138.577626683433));
#64914=CARTESIAN_POINT('Ctrl Pts',(79.0202611292601,7.193868967195,138.573765089187));
#64915=CARTESIAN_POINT('Ctrl Pts',(78.9576133132683,7.2278523822293,138.569896738915));
#64916=CARTESIAN_POINT('Ctrl Pts',(78.8968174567556,7.26505473422092,138.566028388643));
#64917=CARTESIAN_POINT('Ctrl Pts',(78.8382084878197,7.30523215609752,138.562160038371));
#64918=CARTESIAN_POINT('Ctrl Pts',(78.8034090421307,7.32908775424069,138.559863180951));
#64919=CARTESIAN_POINT('Ctrl Pts',(78.7693799733918,7.35399140607145,138.55756632353));
#64920=CARTESIAN_POINT('Ctrl Pts',(78.7361855638254,7.37988561100871,138.55526946611));
#64921=CARTESIAN_POINT('Ctrl Pts',(78.6809217158299,7.42299568358746,138.551445533676));
#64922=CARTESIAN_POINT('Ctrl Pts',(78.6277456591824,7.4690309331306,138.547621601243));
#64923=CARTESIAN_POINT('Ctrl Pts',(78.5769890146386,7.51775936567617,138.54379766881));
#64924=CARTESIAN_POINT('Ctrl Pts',(78.526318708678,7.5664049096883,138.539980241001));
#64925=CARTESIAN_POINT('Ctrl Pts',(78.4780599994551,7.61773419861886,138.536162813192));
#64926=CARTESIAN_POINT('Ctrl Pts',(78.432512620332,7.67147417146613,138.532345385383));
#64927=CARTESIAN_POINT('Ctrl Pts',(78.3870085968665,7.72516299028648,138.528531591308));
#64928=CARTESIAN_POINT('Ctrl Pts',(78.3442111085944,7.78125756695914,138.524717797234));
#64929=CARTESIAN_POINT('Ctrl Pts',(78.3043830638176,7.8394480760296,138.52090400316));
#64930=CARTESIAN_POINT('Ctrl Pts',(78.2645788522619,7.8976037637254,138.517092491271));
#64931=CARTESIAN_POINT('Ctrl Pts',(78.2277408414614,7.9578524865062,138.513280979383));
#64932=CARTESIAN_POINT('Ctrl Pts',(78.1940904589338,8.01985292328849,138.509469467494));
#64933=CARTESIAN_POINT('Ctrl Pts',(78.1604483202982,8.08183817079624,138.505658889375));
#64934=CARTESIAN_POINT('Ctrl Pts',(78.1299924969411,8.14557384247176,138.501848311256));
#64935=CARTESIAN_POINT('Ctrl Pts',(78.1028990533745,8.2106929869736,138.498037733137));
#64936=CARTESIAN_POINT('Ctrl Pts',(78.0757855808063,8.27586027121978,138.494224338023));
#64937=CARTESIAN_POINT('Ctrl Pts',(78.0520396483184,8.34241261158696,138.49041094291));
#64938=CARTESIAN_POINT('Ctrl Pts',(78.0317891512923,8.40996303714985,138.486597547796));
#64939=CARTESIAN_POINT('Ctrl Pts',(78.0115315635821,8.47753711540316,138.482782817427));
#64940=CARTESIAN_POINT('Ctrl Pts',(77.9947719694412,8.54610949060837,138.478968087059));
#64941=CARTESIAN_POINT('Ctrl Pts',(77.9815875948563,8.61528071888466,138.47515335669));
#64942=CARTESIAN_POINT('Ctrl Pts',(77.9683814171201,8.68456633641301,138.471332317858));
#64943=CARTESIAN_POINT('Ctrl Pts',(77.9587623377827,8.75445229062171,138.467511279026));
#64944=CARTESIAN_POINT('Ctrl Pts',(77.9527558264947,8.82453246297826,138.463690240194));
#64945=CARTESIAN_POINT('Ctrl Pts',(77.947717429342,8.88331729229607,138.460485066634));
#64946=CARTESIAN_POINT('Ctrl Pts',(77.9452199900013,8.94223854834861,138.457279893073));
#64947=CARTESIAN_POINT('Ctrl Pts',(77.9452502723122,9.00105785954894,138.454074719513));
#64948=CARTESIAN_POINT('Origin',(80.,9.,141.545925280538));
#64949=CARTESIAN_POINT('',(81.252039109102,10.6292316077768,139.606097362941));
#64950=CARTESIAN_POINT('',(81.252039109102,10.6292316077768,139.54788294617));
#64951=CARTESIAN_POINT('',(81.252039109102,10.6292316077768,141.545925280538));
#64952=CARTESIAN_POINT('',(77.9455904459809,8.99784754164576,139.854074871274));
#64953=CARTESIAN_POINT('Ctrl Pts',(77.9452511248424,8.99784999107146,139.854074719462));
#64954=CARTESIAN_POINT('Ctrl Pts',(77.9451772245318,9.06847601408026,139.850255479513));
#64955=CARTESIAN_POINT('Ctrl Pts',(77.948748952018,9.13916590444103,139.846436239564));
#64956=CARTESIAN_POINT('Ctrl Pts',(77.9559592417713,9.20951119588218,139.842616999616));
#64957=CARTESIAN_POINT('Ctrl Pts',(77.9631671377139,9.27983313273904,139.838799027652));
#64958=CARTESIAN_POINT('Ctrl Pts',(77.9740111489395,9.34981020491898,139.834981055688));
#64959=CARTESIAN_POINT('Ctrl Pts',(77.9884322523696,9.41903789708474,139.831163083724));
#64960=CARTESIAN_POINT('Ctrl Pts',(78.0028536112544,9.48826681554625,139.827345044128));
#64961=CARTESIAN_POINT('Ctrl Pts',(78.0208520847495,9.55674584287351,139.823527004533));
#64962=CARTESIAN_POINT('Ctrl Pts',(78.0423176863816,9.6240813420106,139.819708964937));
#64963=CARTESIAN_POINT('Ctrl Pts',(78.0638064102382,9.6914893733109,139.815886812643));
#64964=CARTESIAN_POINT('Ctrl Pts',(78.0887695660473,9.75775094445758,139.812064660348));
#64965=CARTESIAN_POINT('Ctrl Pts',(78.1170477875132,9.82248922667171,139.808242508053));
#64966=CARTESIAN_POINT('Ctrl Pts',(78.1453421859075,9.88726454327152,139.804418169246));
#64967=CARTESIAN_POINT('Ctrl Pts',(78.1769552003258,9.9505143942472,139.800593830438));
#64968=CARTESIAN_POINT('Ctrl Pts',(78.2116812500701,10.0118861651139,139.796769491631));
#64969=CARTESIAN_POINT('Ctrl Pts',(78.2464714535704,10.0733713156956,139.792938087646));
#64970=CARTESIAN_POINT('Ctrl Pts',(78.2843859059249,10.1329710424756,139.789106683661));
#64971=CARTESIAN_POINT('Ctrl Pts',(78.3251758574949,10.1903619845165,139.785275279677));
#64972=CARTESIAN_POINT('Ctrl Pts',(78.3519387238618,10.2280169964347,139.782761441124));
#64973=CARTESIAN_POINT('Ctrl Pts',(78.3799385966649,10.2647218133961,139.78024760257));
#64974=CARTESIAN_POINT('Ctrl Pts',(78.4090964374419,10.3003935624033,139.777733764017));
#64975=CARTESIAN_POINT('Ctrl Pts',(78.4539904417997,10.3553169590851,139.773863234652));
#64976=CARTESIAN_POINT('Ctrl Pts',(78.5018202761645,10.4080207897608,139.769992705286));
#64977=CARTESIAN_POINT('Ctrl Pts',(78.5523382569853,10.4581745575587,139.766122175921));
#64978=CARTESIAN_POINT('Ctrl Pts',(78.6027802752742,10.5082529104821,139.762257466566));
#64979=CARTESIAN_POINT('Ctrl Pts',(78.6559020748355,10.5557884727724,139.758392757212));
#64980=CARTESIAN_POINT('Ctrl Pts',(78.711415789056,10.6004837686793,139.754528047858));
#64981=CARTESIAN_POINT('Ctrl Pts',(78.7668631203186,10.6451256182264,139.750667959899));
#64982=CARTESIAN_POINT('Ctrl Pts',(78.8246963083252,10.6869336452058,139.74680787194));
#64983=CARTESIAN_POINT('Ctrl Pts',(78.8845919934093,10.7256484408284,139.742947783981));
#64984=CARTESIAN_POINT('Ctrl Pts',(78.9444490883844,10.7643382929482,139.739090183033));
#64985=CARTESIAN_POINT('Ctrl Pts',(79.0063656373174,10.7999386049239,139.735232582086));
#64986=CARTESIAN_POINT('Ctrl Pts',(79.069987857513,10.832232238917,139.731374981138));
#64987=CARTESIAN_POINT('Ctrl Pts',(79.1335903276766,10.8645158481058,139.727518577692));
#64988=CARTESIAN_POINT('Ctrl Pts',(79.198896985352,10.8934945976222,139.723662174246));
#64989=CARTESIAN_POINT('Ctrl Pts',(79.2655294269345,10.9189972745684,139.7198057708));
#64990=CARTESIAN_POINT('Ctrl Pts',(79.3321634293518,10.9445005489032,139.71594927702));
#64991=CARTESIAN_POINT('Ctrl Pts',(79.4001228232358,10.9665274175566,139.712092783239));
#64992=CARTESIAN_POINT('Ctrl Pts',(79.4690108268965,10.9849554303679,139.708236289459));
#64993=CARTESIAN_POINT('Ctrl Pts',(79.5379691156553,11.0034022449242,139.704375860973));
#64994=CARTESIAN_POINT('Ctrl Pts',(79.6078574357236,11.0182427478266,139.700515432486));
#64995=CARTESIAN_POINT('Ctrl Pts',(79.6782663795838,11.0294050950941,139.696655004));
#64996=CARTESIAN_POINT('Ctrl Pts',(79.7487141688414,11.0405736007527,139.692792445672));
#64997=CARTESIAN_POINT('Ctrl Pts',(79.8196826707769,11.0480598596463,139.688929887345));
#64998=CARTESIAN_POINT('Ctrl Pts',(79.8907576027215,11.0518439660795,139.685067329017));
#64999=CARTESIAN_POINT('Ctrl Pts',(79.9619550325507,11.0556345944329,139.681198113557));
#65000=CARTESIAN_POINT('Ctrl Pts',(80.0332587730399,11.0557103301937,139.677328898097));
#65001=CARTESIAN_POINT('Ctrl Pts',(80.104255499616,11.0521033973218,139.673459682637));
#65002=CARTESIAN_POINT('Ctrl Pts',(80.1462079446659,11.0499720363366,139.6711733371));
#65003=CARTESIAN_POINT('Ctrl Pts',(80.188053284814,11.0465557851209,139.668886991563));
#65004=CARTESIAN_POINT('Ctrl Pts',(80.2297077887632,11.0418697055105,139.666600646025));
#65005=CARTESIAN_POINT('Ctrl Pts',(80.3003043705021,11.0339276783372,139.662725718603));
#65006=CARTESIAN_POINT('Ctrl Pts',(80.3706219865153,11.0223050986904,139.658850791181));
#65007=CARTESIAN_POINT('Ctrl Pts',(80.4402478017776,11.0070324948864,139.654975863759));
#65008=CARTESIAN_POINT('Ctrl Pts',(80.5097766126523,10.9917811692473,139.65110633498));
#65009=CARTESIAN_POINT('Ctrl Pts',(80.5786150665536,10.972890014512,139.647236806202));
#65010=CARTESIAN_POINT('Ctrl Pts',(80.6463564374629,10.9504412111751,139.643367277423));
#65011=CARTESIAN_POINT('Ctrl Pts',(80.7140191932826,10.9280184600817,139.639502239303));
#65012=CARTESIAN_POINT('Ctrl Pts',(80.7805869383724,10.902046414884,139.635637201183));
#65013=CARTESIAN_POINT('Ctrl Pts',(80.8456659041088,10.8726576678955,139.631772163063));
#65014=CARTESIAN_POINT('Ctrl Pts',(80.9107018355553,10.8432883545879,139.627909680748));
#65015=CARTESIAN_POINT('Ctrl Pts',(80.9742505024658,10.8105070244793,139.624047198433));
#65016=CARTESIAN_POINT('Ctrl Pts',(81.0359374021744,10.7744946495485,139.620184716118));
#65017=CARTESIAN_POINT('Ctrl Pts',(81.097608619952,10.7384914296178,139.616323215717));
#65018=CARTESIAN_POINT('Ctrl Pts',(81.1574185920664,10.6992590385842,139.612461715315));
#65019=CARTESIAN_POINT('Ctrl Pts',(81.2150181804927,10.6570239538318,139.608600214913));
#65020=CARTESIAN_POINT('Ctrl Pts',(81.2274626734363,10.6478989890788,139.607765930923));
#65021=CARTESIAN_POINT('Ctrl Pts',(81.2398040956947,10.6386340249735,139.606931646932));
#65022=CARTESIAN_POINT('Ctrl Pts',(81.252039109102,10.6292316077768,139.606097362941));
#65023=CARTESIAN_POINT('',(79.4698297828112,7.01482567432834,140.));
#65024=CARTESIAN_POINT('Ctrl Pts',(79.4698297828112,7.01482567432834,140.));
#65025=CARTESIAN_POINT('Ctrl Pts',(78.8097404375817,7.19111231424644,139.962955627336));
#65026=CARTESIAN_POINT('Ctrl Pts',(78.0751152861664,7.88746878509532,139.914314179013));
#65027=CARTESIAN_POINT('Ctrl Pts',(77.9457329218076,8.78359621258651,139.86567273069));
#65028=CARTESIAN_POINT('Ctrl Pts',(77.9473422520121,8.99783489604774,139.85407565503));
#65029=CARTESIAN_POINT('',(80.5303700321158,7.01487904863873,139.999999991429));
#65030=CARTESIAN_POINT('Origin',(80.,9.,140.));
#65031=CARTESIAN_POINT('',(77.94525054989,9.00150325402769,139.795925280583));
#65032=CARTESIAN_POINT('Ctrl Pts',(80.5303700321158,7.01487904863873,139.999999991429));
#65033=CARTESIAN_POINT('Ctrl Pts',(80.4620742005438,6.99663227009389,139.996143017033));
#65034=CARTESIAN_POINT('Ctrl Pts',(80.3926969237085,6.98187705917305,139.992286042637));
#65035=CARTESIAN_POINT('Ctrl Pts',(80.3226296813442,6.97073716556584,139.988429068241));
#65036=CARTESIAN_POINT('Ctrl Pts',(80.2526676763219,6.95961400349758,139.984577886819));
#65037=CARTESIAN_POINT('Ctrl Pts',(80.1820182414636,6.95209545848432,139.980726705397));
#65038=CARTESIAN_POINT('Ctrl Pts',(80.1110863019471,6.94825503631184,139.976875523975));
#65039=CARTESIAN_POINT('Ctrl Pts',(80.0402381740564,6.94441915189807,139.973028893025));
#65040=CARTESIAN_POINT('Ctrl Pts',(79.9691086905236,6.94425278531202,139.969182262075));
#65041=CARTESIAN_POINT('Ctrl Pts',(79.8981094276751,6.94777782056345,139.965335631125));
#65042=CARTESIAN_POINT('Ctrl Pts',(79.8271548669589,6.95130063640322,139.961491422068));
#65043=CARTESIAN_POINT('Ctrl Pts',(79.7563308517412,6.95851021955747,139.95764721301));
#65044=CARTESIAN_POINT('Ctrl Pts',(79.6860489785746,6.96937637198669,139.953803003953));
#65045=CARTESIAN_POINT('Ctrl Pts',(79.6157874515818,6.98023937873102,139.949959907771));
#65046=CARTESIAN_POINT('Ctrl Pts',(79.5460682382953,6.99475677865711,139.946116811588));
#65047=CARTESIAN_POINT('Ctrl Pts',(79.4772960600091,7.01284672115663,139.942273715406));
#65048=CARTESIAN_POINT('Ctrl Pts',(79.4085204004781,7.03093757936825,139.938430424687));
#65049=CARTESIAN_POINT('Ctrl Pts',(79.3406923435553,7.05260121217767,139.934587133967));
#65050=CARTESIAN_POINT('Ctrl Pts',(79.2742029617191,7.07770547997382,139.930743843247));
#65051=CARTESIAN_POINT('Ctrl Pts',(79.2076449190222,7.10283567191889,139.926896583719));
#65052=CARTESIAN_POINT('Ctrl Pts',(79.1424287685514,7.13141341594115,139.92304932419));
#65053=CARTESIAN_POINT('Ctrl Pts',(79.078926116778,7.16325819339072,139.919202064662));
#65054=CARTESIAN_POINT('Ctrl Pts',(79.0153861545328,7.19512168098292,139.915352544707));
#65055=CARTESIAN_POINT('Ctrl Pts',(78.953562119514,7.23025577981269,139.911503024752));
#65056=CARTESIAN_POINT('Ctrl Pts',(78.8937990765748,7.26843507788096,139.907653504797));
#65057=CARTESIAN_POINT('Ctrl Pts',(78.8339359110614,7.30667833871634,139.903797535642));
#65058=CARTESIAN_POINT('Ctrl Pts',(78.7761410253502,7.34797669509396,139.899941566487));
#65059=CARTESIAN_POINT('Ctrl Pts',(78.7207279840538,7.39206322521163,139.896085597331));
#65060=CARTESIAN_POINT('Ctrl Pts',(78.6965850159507,7.41127133336641,139.894405585945));
#65061=CARTESIAN_POINT('Ctrl Pts',(78.6728937264846,7.43100822304824,139.892725574559));
#65062=CARTESIAN_POINT('Ctrl Pts',(78.6496778175411,7.4512496760099,139.891045563173));
#65063=CARTESIAN_POINT('Ctrl Pts',(78.5949087487768,7.4990016521157,139.887082218065));
#65064=CARTESIAN_POINT('Ctrl Pts',(78.5425524775813,7.54977030605766,139.883118872957));
#65065=CARTESIAN_POINT('Ctrl Pts',(78.4929635885723,7.60327568320336,139.879155527849));
#65066=CARTESIAN_POINT('Ctrl Pts',(78.4452783589226,7.65472705159813,139.875344330917));
#65067=CARTESIAN_POINT('Ctrl Pts',(78.4001523191138,7.70870846833804,139.871533133985));
#65068=CARTESIAN_POINT('Ctrl Pts',(78.3578674318731,7.76492988409682,139.867721937053));
#65069=CARTESIAN_POINT('Ctrl Pts',(78.3156213126652,7.82109975440216,139.863914234339));
#65070=CARTESIAN_POINT('Ctrl Pts',(78.2762114818338,7.87950515554645,139.860106531624));
#65071=CARTESIAN_POINT('Ctrl Pts',(78.2398808669802,7.93982161874629,139.85629882891));
#65072=CARTESIAN_POINT('Ctrl Pts',(78.2035706386586,8.00010423601464,139.852493262847));
#65073=CARTESIAN_POINT('Ctrl Pts',(78.1703364568118,8.06229536107818,139.848687696784));
#65074=CARTESIAN_POINT('Ctrl Pts',(78.1403778852329,8.12604167561079,139.844882130721));
#65075=CARTESIAN_POINT('Ctrl Pts',(78.1104254709766,8.18977488849674,139.841077346809));
#65076=CARTESIAN_POINT('Ctrl Pts',(78.0837475415326,8.25506220336587,139.837272562896));
#65077=CARTESIAN_POINT('Ctrl Pts',(78.0604967835646,8.32152757171954,139.833467778983));
#65078=CARTESIAN_POINT('Ctrl Pts',(78.0372308381719,8.38803635533663,139.82966050978));
#65079=CARTESIAN_POINT('Ctrl Pts',(78.0173966988217,8.45572425618672,139.825853240578));
#65080=CARTESIAN_POINT('Ctrl Pts',(78.0010976898141,8.52419844805488,139.822045971375));
#65081=CARTESIAN_POINT('Ctrl Pts',(77.9847922409877,8.59269969441341,139.818237197902));
#65082=CARTESIAN_POINT('Ctrl Pts',(77.9720247942908,8.66198735860674,139.814428424428));
#65083=CARTESIAN_POINT('Ctrl Pts',(77.9628473589046,8.73165939670294,139.810619650955));
#65084=CARTESIAN_POINT('Ctrl Pts',(77.9536577739424,8.80142367033923,139.806805835225));
#65085=CARTESIAN_POINT('Ctrl Pts',(77.9480677197906,8.87157283521784,139.802992019495));
#65086=CARTESIAN_POINT('Ctrl Pts',(77.9460771919704,8.94170196267724,139.799178203766));
#65087=CARTESIAN_POINT('Ctrl Pts',(77.9455112640781,8.96164040759028,139.798093896038));
#65088=CARTESIAN_POINT('Ctrl Pts',(77.9452359720325,8.98157725069431,139.79700958831));
#65089=CARTESIAN_POINT('Ctrl Pts',(77.94525054989,9.00150325402769,139.795925280583));
#65090=CARTESIAN_POINT('Ctrl Pts',(77.9452505498906,9.0015032548487,139.795925280538));
#65091=CARTESIAN_POINT('Ctrl Pts',(77.945322310872,9.0995909724926,139.790587668752));
#65092=CARTESIAN_POINT('Ctrl Pts',(77.9524183464193,9.19742452109931,139.785250056967));
#65093=CARTESIAN_POINT('Ctrl Pts',(77.9664267220482,9.29424018369419,139.779912445181));
#65094=CARTESIAN_POINT('Ctrl Pts',(77.9765717595288,9.36435527424839,139.776046881246));
#65095=CARTESIAN_POINT('Ctrl Pts',(77.990367502887,9.43408480533988,139.772181317311));
#65096=CARTESIAN_POINT('Ctrl Pts',(78.0077726792506,9.50301875209562,139.768315753376));
#65097=CARTESIAN_POINT('Ctrl Pts',(78.0251516710698,9.57184899384097,139.764456004839));
#65098=CARTESIAN_POINT('Ctrl Pts',(78.0461291999042,9.63988555882835,139.760596256302));
#65099=CARTESIAN_POINT('Ctrl Pts',(78.0706125287104,9.70672593565721,139.756736507765));
#65100=CARTESIAN_POINT('Ctrl Pts',(78.0950667440095,9.7734868315547,139.752881348915));
#65101=CARTESIAN_POINT('Ctrl Pts',(78.1230183124154,9.83905390971274,139.749026190065));
#65102=CARTESIAN_POINT('Ctrl Pts',(78.1543244441948,9.90303892784481,139.745171031215));
#65103=CARTESIAN_POINT('Ctrl Pts',(78.1856105615418,9.9669830394916,139.74131833702));
#65104=CARTESIAN_POINT('Ctrl Pts',(78.2202467742583,10.0293466614236,139.737465642825));
#65105=CARTESIAN_POINT('Ctrl Pts',(78.2580424198006,10.0897620617758,139.733612948631));
#65106=CARTESIAN_POINT('Ctrl Pts',(78.2958266099266,10.1501591509297,139.729761422142));
#65107=CARTESIAN_POINT('Ctrl Pts',(78.336768073914,10.2086087782143,139.725909895653));
#65108=CARTESIAN_POINT('Ctrl Pts',(78.3806313708818,10.2647698626737,139.722058369165));
#65109=CARTESIAN_POINT('Ctrl Pts',(78.4244961209918,10.3209328076874,139.71820671508));
#65110=CARTESIAN_POINT('Ctrl Pts',(78.4712825948598,10.3748066770552,139.714355060994));
#65111=CARTESIAN_POINT('Ctrl Pts',(78.5207144708289,10.4260827064673,139.710503406909));
#65112=CARTESIAN_POINT('Ctrl Pts',(78.5701980116868,10.4774123282285,139.706647727177));
#65113=CARTESIAN_POINT('Ctrl Pts',(78.6223321354694,10.5261383386816,139.702792047444));
#65114=CARTESIAN_POINT('Ctrl Pts',(78.676803622504,10.5719888387267,139.698936367712));
#65115=CARTESIAN_POINT('Ctrl Pts',(78.7313058224108,10.6178651908392,139.695078514017));
#65116=CARTESIAN_POINT('Ctrl Pts',(78.7881476204764,10.6608625113955,139.691220660322));
#65117=CARTESIAN_POINT('Ctrl Pts',(78.8469848839622,10.7007509237653,139.687362806626));
#65118=CARTESIAN_POINT('Ctrl Pts',(78.9059255314841,10.7407094247969,139.683498174226));
#65119=CARTESIAN_POINT('Ctrl Pts',(78.9668682279573,10.7775478593986,139.679633541825));
#65120=CARTESIAN_POINT('Ctrl Pts',(79.0294428290257,10.811081538852,139.675768909424));
#65121=CARTESIAN_POINT('Ctrl Pts',(79.0671670137654,10.8312978997572,139.673439048679));
#65122=CARTESIAN_POINT('Ctrl Pts',(79.105483874496,10.8503140641317,139.671109187935));
#65123=CARTESIAN_POINT('Ctrl Pts',(79.1443091091393,10.8680981403015,139.66877932719));
#65124=CARTESIAN_POINT('Ctrl Pts',(79.2087912872131,10.8976344966686,139.664909820751));
#65125=CARTESIAN_POINT('Ctrl Pts',(79.2749307245336,10.9238860812921,139.661040314313));
#65126=CARTESIAN_POINT('Ctrl Pts',(79.342359528159,10.9466655008749,139.657170807875));
#65127=CARTESIAN_POINT('Ctrl Pts',(79.4096878426605,10.9694109722963,139.653307068161));
#65128=CARTESIAN_POINT('Ctrl Pts',(79.4783012528629,10.9886943959418,139.649443328446));
#65129=CARTESIAN_POINT('Ctrl Pts',(79.5478103620977,11.0043757367005,139.645579588732));
#65130=CARTESIAN_POINT('Ctrl Pts',(79.6172378543529,11.0200386645681,139.641720385787));
#65131=CARTESIAN_POINT('Ctrl Pts',(79.6875584850885,11.032107804553,139.637861182842));
#65132=CARTESIAN_POINT('Ctrl Pts',(79.7583677824048,11.0404929389537,139.634001979896));
#65133=CARTESIAN_POINT('Ctrl Pts',(79.829132417637,11.0488727845352,139.630145211095));
#65134=CARTESIAN_POINT('Ctrl Pts',(79.9003846267903,11.0535731776611,139.626288442294));
#65135=CARTESIAN_POINT('Ctrl Pts',(79.9717112810358,11.054555258658,139.622431673493));
#65136=CARTESIAN_POINT('Ctrl Pts',(80.0430167923961,11.0555370485432,139.618576047929));
#65137=CARTESIAN_POINT('Ctrl Pts',(80.1143962196894,11.0528027077946,139.614720422364));
#65138=CARTESIAN_POINT('Ctrl Pts',(80.1854345999683,11.0463654540757,139.610864796799));
#65139=CARTESIAN_POINT('Ctrl Pts',(80.2564756712516,11.0399279565073,139.60700902518));
#65140=CARTESIAN_POINT('Ctrl Pts',(80.3271751863906,11.0297873135014,139.60315325356));
#65141=CARTESIAN_POINT('Ctrl Pts',(80.3971232064518,11.0160086114393,139.59929748194));
#65142=CARTESIAN_POINT('Ctrl Pts',(80.4671442536227,11.002215524141,139.595437684819));
#65143=CARTESIAN_POINT('Ctrl Pts',(80.5364117620413,10.9847768897435,139.591577887698));
#65144=CARTESIAN_POINT('Ctrl Pts',(80.6045267855586,10.963808780926,139.587718090577));
#65145=CARTESIAN_POINT('Ctrl Pts',(80.672680283083,10.9428288285075,139.583856113293));
#65146=CARTESIAN_POINT('Ctrl Pts',(80.7396795434922,10.9183155999389,139.579994136009));
#65147=CARTESIAN_POINT('Ctrl Pts',(80.8051441729494,10.8904339245966,139.576132158724));
#65148=CARTESIAN_POINT('Ctrl Pts',(80.8707231147958,10.8625035631019,139.57226343777));
#65149=CARTESIAN_POINT('Ctrl Pts',(80.9347616390688,10.8311932248292,139.568394716816));
#65150=CARTESIAN_POINT('Ctrl Pts',(80.9969032165026,10.796714095071,139.564525995862));
#65151=CARTESIAN_POINT('Ctrl Pts',(81.0337388874113,10.7762758968559,139.562232733641));
#65152=CARTESIAN_POINT('Ctrl Pts',(81.0699085400531,10.7547251089265,139.559939471419));
#65153=CARTESIAN_POINT('Ctrl Pts',(81.1053430762912,10.7321126540139,139.557646209198));
#65154=CARTESIAN_POINT('Ctrl Pts',(81.1556290392832,10.7000228006784,139.554391788189));
#65155=CARTESIAN_POINT('Ctrl Pts',(81.2045988673975,10.6656886944647,139.551137367179));
#65156=CARTESIAN_POINT('Ctrl Pts',(81.252039109102,10.6292316077768,139.54788294617));
#65157=CARTESIAN_POINT('Origin',(80.,9.,134.));
#65158=CARTESIAN_POINT('',(78.4365593800808,9.57550797386886,129.733376810833));
#65159=CARTESIAN_POINT('',(78.4365593657201,9.57550793485619,129.539973235759));
#65160=CARTESIAN_POINT('',(78.4365593737638,9.57550795670799,134.));
#65161=CARTESIAN_POINT('',(79.2300979593294,7.52256748114468,129.));
#65162=CARTESIAN_POINT('Ctrl Pts',(78.4365593657201,9.57550793485619,129.539973235759));
#65163=CARTESIAN_POINT('Ctrl Pts',(78.4421052637371,9.59057407345864,129.538809962392));
#65164=CARTESIAN_POINT('Ctrl Pts',(78.4478695319474,9.60556165591258,129.537643358189));
#65165=CARTESIAN_POINT('Ctrl Pts',(78.5031580487101,9.74333604487815,129.526842861615));
#65166=CARTESIAN_POINT('Ctrl Pts',(78.5669464972497,9.85991522303598,129.517194278958));
#65167=CARTESIAN_POINT('Ctrl Pts',(78.6598171209095,9.99006006994452,129.506139719031));
#65168=CARTESIAN_POINT('Ctrl Pts',(78.6763077958987,10.0120020731591,129.50426270079));
#65169=CARTESIAN_POINT('Ctrl Pts',(78.7011007282667,10.0433472219657,129.501560088528));
#65170=CARTESIAN_POINT('Ctrl Pts',(78.7089781487769,10.0530789800813,129.500717898703));
#65171=CARTESIAN_POINT('Ctrl Pts',(78.7231800079559,10.0702250439487,129.499228154612));
#65172=CARTESIAN_POINT('Ctrl Pts',(78.7294611210524,10.0776743018317,129.498578886966));
#65173=CARTESIAN_POINT('Ctrl Pts',(78.7427544320876,10.0931620902856,129.497224457056));
#65174=CARTESIAN_POINT('Ctrl Pts',(78.7497792260504,10.1011892657614,129.496519855671));
#65175=CARTESIAN_POINT('Ctrl Pts',(78.7685141268927,10.1221870976884,129.494669306634));
#65176=CARTESIAN_POINT('Ctrl Pts',(78.7803522397377,10.1350421651102,129.493528779948));
#65177=CARTESIAN_POINT('Ctrl Pts',(78.8415590012961,10.1994433750242,129.487770910074));
#65178=CARTESIAN_POINT('Ctrl Pts',(78.8940041737191,10.2479683608845,129.483290074258));
#65179=CARTESIAN_POINT('Ctrl Pts',(79.0025519003157,10.3361671038191,129.474652016076));
#65180=CARTESIAN_POINT('Ctrl Pts',(79.058309757714,10.3760323161562,129.470496763705));
#65181=CARTESIAN_POINT('Ctrl Pts',(79.1346986627444,10.4238249094655,129.464983961084));
#65182=CARTESIAN_POINT('Ctrl Pts',(79.1532553342286,10.4349380544061,129.463657588021));
#65183=CARTESIAN_POINT('Ctrl Pts',(79.2285831123431,10.478079965539,129.458304650354));
#65184=CARTESIAN_POINT('Ctrl Pts',(79.2869891060929,10.5071223578696,129.454225168522));
#65185=CARTESIAN_POINT('Ctrl Pts',(79.3574418761431,10.5371419664763,129.449214067501));
#65186=CARTESIAN_POINT('Ctrl Pts',(79.3679913198908,10.541509447957,129.448461390351));
#65187=CARTESIAN_POINT('Ctrl Pts',(79.384501113993,10.5481465646681,129.447278582831));
#65188=CARTESIAN_POINT('Ctrl Pts',(79.3904312540788,10.5504910850961,129.446852759523));
#65189=CARTESIAN_POINT('Ctrl Pts',(79.400982359402,10.5545926496143,129.446093148331));
#65190=CARTESIAN_POINT('Ctrl Pts',(79.4055979035018,10.5563632561535,129.445760176098));
#65191=CARTESIAN_POINT('Ctrl Pts',(79.4167433048174,10.5605820260795,129.444954544452));
#65192=CARTESIAN_POINT('Ctrl Pts',(79.423280699858,10.5630097495067,129.444480704337));
#65193=CARTESIAN_POINT('Ctrl Pts',(79.4435054582284,10.5703762482551,129.443011220069));
#65194=CARTESIAN_POINT('Ctrl Pts',(79.457242008678,10.575176645065,129.442008141136));
#65195=CARTESIAN_POINT('Ctrl Pts',(79.5275832894102,10.5987289149312,129.436852303154));
#65196=CARTESIAN_POINT('Ctrl Pts',(79.5850978491061,10.6146103213682,129.432574634257));
#65197=CARTESIAN_POINT('Ctrl Pts',(79.7468893872503,10.6500696849958,129.420573238285));
#65198=CARTESIAN_POINT('Ctrl Pts',(79.8523860621301,10.6628315071718,129.412800258245));
#65199=CARTESIAN_POINT('Ctrl Pts',(80.0157918246257,10.6669146285504,129.401185248619));
#65200=CARTESIAN_POINT('Ctrl Pts',(80.0732409160692,10.6653800937205,129.397177609033));
#65201=CARTESIAN_POINT('Ctrl Pts',(80.1476560853385,10.6595329932857,129.39208658213));
#65202=CARTESIAN_POINT('Ctrl Pts',(80.1647886741462,10.6579194210251,129.390921244584));
#65203=CARTESIAN_POINT('Ctrl Pts',(80.1925155230282,10.6548740001333,129.389045625889));
#65204=CARTESIAN_POINT('Ctrl Pts',(80.2031260221025,10.6536051557802,129.388330321576));
#65205=CARTESIAN_POINT('Ctrl Pts',(80.223526547605,10.6509662577916,129.386959496613));
#65206=CARTESIAN_POINT('Ctrl Pts',(80.2333179953775,10.6496109911206,129.386303544279));
#65207=CARTESIAN_POINT('Ctrl Pts',(80.2560603864477,10.6462565973157,129.384784306296));
#65208=CARTESIAN_POINT('Ctrl Pts',(80.2690010749719,10.6441916383344,129.383923119468));
#65209=CARTESIAN_POINT('Ctrl Pts',(80.3110258832341,10.6369762500305,129.381135923457));
#65210=CARTESIAN_POINT('Ctrl Pts',(80.3399986476222,10.6312049020792,129.37922935071));
#65211=CARTESIAN_POINT('Ctrl Pts',(80.4091450361678,10.615508461367,129.374702342521));
#65212=CARTESIAN_POINT('Ctrl Pts',(80.4491327278415,10.6048512079816,129.372103669431));
#65213=CARTESIAN_POINT('Ctrl Pts',(80.560341944949,10.5707294800036,129.364874693538));
#65214=CARTESIAN_POINT('Ctrl Pts',(80.6304358066673,10.5439317786606,129.360319236208));
#65215=CARTESIAN_POINT('Ctrl Pts',(80.7739282488995,10.4776657870666,129.350644234482));
#65216=CARTESIAN_POINT('Ctrl Pts',(80.8466481112711,10.4372351042523,129.345529949491));
#65217=CARTESIAN_POINT('Ctrl Pts',(80.9294111313012,10.3827534953977,129.33910314609));
#65218=CARTESIAN_POINT('Ctrl Pts',(80.9426545581567,10.3737593014519,129.338054850521));
#65219=CARTESIAN_POINT('Ctrl Pts',(80.9616541606417,10.360451748159,129.336518608309));
#65220=CARTESIAN_POINT('Ctrl Pts',(80.9675157024037,10.3562894398521,129.336040121293));
#65221=CARTESIAN_POINT('Ctrl Pts',(80.9778644109002,10.3488395514504,129.335186890215));
#65222=CARTESIAN_POINT('Ctrl Pts',(80.9823623132901,10.3455672502953,129.334813162941));
#65223=CARTESIAN_POINT('Ctrl Pts',(80.9921298270897,10.3383861369073,129.333995234183));
#65224=CARTESIAN_POINT('Ctrl Pts',(80.9973927282431,10.3344687284806,129.333550479961));
#65225=CARTESIAN_POINT('Ctrl Pts',(81.0123578563145,10.3231915472474,129.332274548498));
#65226=CARTESIAN_POINT('Ctrl Pts',(81.0220024797696,10.3157565163065,129.331438593885));
#65227=CARTESIAN_POINT('Ctrl Pts',(81.0438460953933,10.2985322323532,129.329515457863));
#65228=CARTESIAN_POINT('Ctrl Pts',(81.0559903525255,10.2886756638844,129.328424541292));
#65229=CARTESIAN_POINT('Ctrl Pts',(81.0962111605375,10.2550811973876,129.324742745478));
#65230=CARTESIAN_POINT('Ctrl Pts',(81.1236392228932,10.2305861584681,129.322117436049));
#65231=CARTESIAN_POINT('Ctrl Pts',(81.2005146447394,10.1572172330857,129.314467595596));
#65232=CARTESIAN_POINT('Ctrl Pts',(81.2477436994239,10.1061296456846,129.309398850474));
#65233=CARTESIAN_POINT('Ctrl Pts',(81.3523830233236,9.97768317039373,129.297428658333));
#65234=CARTESIAN_POINT('Ctrl Pts',(81.40656099785,9.89799550323873,129.290600319234));
#65235=CARTESIAN_POINT('Ctrl Pts',(81.4627742385456,9.79762313193904,129.282738186384));
#65236=CARTESIAN_POINT('Ctrl Pts',(81.4717032196639,9.78102549042416,129.281459998393));
#65237=CARTESIAN_POINT('Ctrl Pts',(81.4854258159986,9.754445899681,129.279446813918));
#65238=CARTESIAN_POINT('Ctrl Pts',(81.4904046423317,9.74456194007761,129.278705439598));
#65239=CARTESIAN_POINT('Ctrl Pts',(81.4996269501798,9.72579059027314,129.277310818001));
#65240=CARTESIAN_POINT('Ctrl Pts',(81.5038908127876,9.71691380297453,129.276656891018));
#65241=CARTESIAN_POINT('Ctrl Pts',(81.513393158668,9.69667331344693,129.275178164977));
#65242=CARTESIAN_POINT('Ctrl Pts',(81.5185828699014,9.68528726804384,129.274355058024));
#65243=CARTESIAN_POINT('Ctrl Pts',(81.5341701538642,9.65004248487715,129.271833019883));
#65244=CARTESIAN_POINT('Ctrl Pts',(81.5441376573839,9.62599705010563,129.270148554315));
#65245=CARTESIAN_POINT('Ctrl Pts',(81.566102383168,9.56928852987476,129.266251535939));
#65246=CARTESIAN_POINT('Ctrl Pts',(81.5776481006429,9.53646324109283,129.264053157243));
#65247=CARTESIAN_POINT('Ctrl Pts',(81.6148606590356,9.41903911259476,129.256350713396));
#65248=CARTESIAN_POINT('Ctrl Pts',(81.6348156733792,9.33278723538462,129.250992605335));
#65249=CARTESIAN_POINT('Ctrl Pts',(81.6601640139988,9.16254566183368,129.240471142832));
#65250=CARTESIAN_POINT('Ctrl Pts',(81.6662327894088,9.07893320225307,129.235324504706));
#65251=CARTESIAN_POINT('Ctrl Pts',(81.6659483502786,8.9795731222314,129.228879113168));
#65252=CARTESIAN_POINT('Ctrl Pts',(81.6656827969888,8.96391760074245,129.227853728557));
#65253=CARTESIAN_POINT('Ctrl Pts',(81.664973537675,8.9410869417171,129.226341018184));
#65254=CARTESIAN_POINT('Ctrl Pts',(81.6647039685041,8.93390671677452,129.225862761744));
#65255=CARTESIAN_POINT('Ctrl Pts',(81.6641482375454,8.92128307028129,129.225017162389));
#65256=CARTESIAN_POINT('Ctrl Pts',(81.6638817884667,8.91583882519387,129.224650916077));
#65257=CARTESIAN_POINT('Ctrl Pts',(81.6632662496597,8.9044107152855,129.223878657379));
#65258=CARTESIAN_POINT('Ctrl Pts',(81.6629115816535,8.89842738921801,129.223472308653));
#65259=CARTESIAN_POINT('Ctrl Pts',(81.6618278269037,8.88167512252505,129.222329119015));
#65260=CARTESIAN_POINT('Ctrl Pts',(81.6610263744618,8.87091138731775,129.221588264218));
#65261=CARTESIAN_POINT('Ctrl Pts',(81.6550401224703,8.79984691148014,129.21665855689));
#65262=CARTESIAN_POINT('Ctrl Pts',(81.6466777194428,8.73986584875166,129.212316118882));
#65263=CARTESIAN_POINT('Ctrl Pts',(81.6120314710883,8.5625710469104,129.199179394477));
#65264=CARTESIAN_POINT('Ctrl Pts',(81.5762996584439,8.44748338016553,129.190280313369));
#65265=CARTESIAN_POINT('Ctrl Pts',(81.5058252377969,8.28495162080501,129.177662769845));
#65266=CARTESIAN_POINT('Ctrl Pts',(81.4804837657359,8.23385834426226,129.173681908576));
#65267=CARTESIAN_POINT('Ctrl Pts',(81.4443816512748,8.16958008505786,129.168654392649));
#65268=CARTESIAN_POINT('Ctrl Pts',(81.4359741238892,8.15512489551793,129.167522293067));
#65269=CARTESIAN_POINT('Ctrl Pts',(81.4220593176879,8.13200890448575,129.165708807347));
#65270=CARTESIAN_POINT('Ctrl Pts',(81.4166873503246,8.123268453397,129.165022374217));
#65271=CARTESIAN_POINT('Ctrl Pts',(81.4062416354628,8.10661949144168,129.163713187218));
#65272=CARTESIAN_POINT('Ctrl Pts',(81.4011810706918,8.09870322095879,129.163089963262));
#65273=CARTESIAN_POINT('Ctrl Pts',(81.3893400792669,8.08052107595637,129.161656568709));
#65274=CARTESIAN_POINT('Ctrl Pts',(81.3825123108633,8.07028656464253,129.160848259831));
#65275=CARTESIAN_POINT('Ctrl Pts',(81.3603507215971,8.03785143932297,129.158280849402));
#65276=CARTESIAN_POINT('Ctrl Pts',(81.3445902443944,8.01594657222786,129.156538356072));
#65277=CARTESIAN_POINT('Ctrl Pts',(81.2908143401557,7.9449112745238,129.150844862917));
#65278=CARTESIAN_POINT('Ctrl Pts',(81.2505826803052,7.89752191058231,129.146978849729));
#65279=CARTESIAN_POINT('Ctrl Pts',(81.1435476543303,7.78486409520348,129.137424732861));
#65280=CARTESIAN_POINT('Ctrl Pts',(81.0737378659551,7.72275990899696,129.131817797626));
#65281=CARTESIAN_POINT('Ctrl Pts',(80.9565423541843,7.63493179343378,129.122726203493));
#65282=CARTESIAN_POINT('Ctrl Pts',(80.9124853750812,7.60509725697729,129.119367998485));
#65283=CARTESIAN_POINT('Ctrl Pts',(80.85780221054,7.57176700268609,129.115169872359));
#65284=CARTESIAN_POINT('Ctrl Pts',(80.8484668084741,7.566201483465,129.114452150317));
#65285=CARTESIAN_POINT('Ctrl Pts',(80.8337512761374,7.55762250909674,129.113318058977));
#65286=CARTESIAN_POINT('Ctrl Pts',(80.828407505868,7.55454677752086,129.112905668379));
#65287=CARTESIAN_POINT('Ctrl Pts',(80.8182589828174,7.5487803191333,129.11212117998));
#65288=CARTESIAN_POINT('Ctrl Pts',(80.8134577215516,7.54608361380095,129.111749496323));
#65289=CARTESIAN_POINT('Ctrl Pts',(80.8038649102653,7.54075804750255,129.111005926905));
#65290=CARTESIAN_POINT('Ctrl Pts',(80.7990736107777,7.53812885919815,129.110634067701));
#65291=CARTESIAN_POINT('Ctrl Pts',(80.7836765336083,7.52977814261942,129.109437770323));
#65292=CARTESIAN_POINT('Ctrl Pts',(80.7730218780729,7.52414825469413,129.108607961825));
#65293=CARTESIAN_POINT('Ctrl Pts',(80.7479994785996,7.51127178073218,129.106656052089));
#65294=CARTESIAN_POINT('Ctrl Pts',(80.7335861425987,7.50411689668719,129.105529360302));
#65295=CARTESIAN_POINT('Ctrl Pts',(80.6846726700445,7.48071281040507,129.101702845179));
#65296=CARTESIAN_POINT('Ctrl Pts',(80.6497205286664,7.46544043065128,129.098963851328));
#65297=CARTESIAN_POINT('Ctrl Pts',(80.5077824575865,7.40913901578415,129.087893673856));
#65298=CARTESIAN_POINT('Ctrl Pts',(80.3972036766103,7.37799080291186,129.0794112534));
#65299=CARTESIAN_POINT('Ctrl Pts',(80.2097943597768,7.34553314225501,129.065735328632));
#65300=CARTESIAN_POINT('Ctrl Pts',(80.1344841321471,7.33771508262403,129.060413112386));
#65301=CARTESIAN_POINT('Ctrl Pts',(80.0392876188853,7.33434777179128,129.053897753106));
#65302=CARTESIAN_POINT('Ctrl Pts',(80.0196706028896,7.33400060528584,129.052566066229));
#65303=CARTESIAN_POINT('Ctrl Pts',(79.9881368591672,7.33399963369054,129.050441638302));
#65304=CARTESIAN_POINT('Ctrl Pts',(79.9762224867312,7.33412707680401,129.049642681699));
#65305=CARTESIAN_POINT('Ctrl Pts',(79.9534381704869,7.33461528391728,129.048121448116));
#65306=CARTESIAN_POINT('Ctrl Pts',(79.9425684321,7.33495469124979,129.047398604261));
#65307=CARTESIAN_POINT('Ctrl Pts',(79.9174640604423,7.33598470685588,129.045735338325));
#65308=CARTESIAN_POINT('Ctrl Pts',(79.9032332937088,7.33675158191233,129.044797097068));
#65309=CARTESIAN_POINT('Ctrl Pts',(79.8572146220244,7.33982409655593,129.041776170394));
#65310=CARTESIAN_POINT('Ctrl Pts',(79.8254816201813,7.34285932669461,129.039713439047));
#65311=CARTESIAN_POINT('Ctrl Pts',(79.7061241588802,7.35774266817347,129.032002917664));
#65312=CARTESIAN_POINT('Ctrl Pts',(79.6194021641204,7.37564818230039,129.026506098934));
#65313=CARTESIAN_POINT('Ctrl Pts',(79.4530584097834,7.42405378440747,129.015705166427));
#65314=CARTESIAN_POINT('Ctrl Pts',(79.3735465083349,7.45393889046513,129.01041518196));
#65315=CARTESIAN_POINT('Ctrl Pts',(79.2839670996566,7.49565660341621,129.003983010553));
#65316=CARTESIAN_POINT('Ctrl Pts',(79.2713458564728,7.50172923543078,129.003065239095));
#65317=CARTESIAN_POINT('Ctrl Pts',(79.2534737802052,7.51060750191127,129.001747280436));
#65318=CARTESIAN_POINT('Ctrl Pts',(79.2481587877413,7.51328341649854,129.001352990102));
#65319=CARTESIAN_POINT('Ctrl Pts',(79.238595383939,7.51816265612658,129.000639116768));
#65320=CARTESIAN_POINT('Ctrl Pts',(79.2343418898436,7.52035593461265,129.000320021224));
#65321=CARTESIAN_POINT('Ctrl Pts',(79.2300979593294,7.52256748114467,129.));
#65322=CARTESIAN_POINT('',(78.6641544560541,9.99806607121007,128.999128940953));
#65323=CARTESIAN_POINT('Origin',(80.,9.,129.));
#65324=CARTESIAN_POINT('',(78.4365593751704,9.57550796052904,129.032769692033));
#65325=CARTESIAN_POINT('Ctrl Pts',(78.6653336530456,9.99710668551929,128.998257881905));
#65326=CARTESIAN_POINT('Ctrl Pts',(78.6618063509199,9.99238525348894,128.998659033531));
#65327=CARTESIAN_POINT('Ctrl Pts',(78.6583041843105,9.98764521447221,128.999061823807));
#65328=CARTESIAN_POINT('Ctrl Pts',(78.6476926070415,9.97312227605533,129.000295854233));
#65329=CARTESIAN_POINT('Ctrl Pts',(78.6406646880971,9.96328071655673,129.001132000887));
#65330=CARTESIAN_POINT('Ctrl Pts',(78.5881391515514,9.8880069505415,129.007521328091));
#65331=CARTESIAN_POINT('Ctrl Pts',(78.5472863866272,9.81946814375683,129.013299876743));
#65332=CARTESIAN_POINT('Ctrl Pts',(78.4832806040723,9.69214545423395,129.023673465825));
#65333=CARTESIAN_POINT('Ctrl Pts',(78.4582610564981,9.63446334002325,129.028253032547));
#65334=CARTESIAN_POINT('Ctrl Pts',(78.4365593751704,9.57550796052904,129.032769692033));
#65335=CARTESIAN_POINT('',(78.4365593737638,9.57550795670799,128.));
#65336=CARTESIAN_POINT('',(78.4365593737638,9.57550795670799,134.));
#65337=CARTESIAN_POINT('Origin',(80.,9.,128.));
#65338=CARTESIAN_POINT('Ctrl Pts',(78.4365593751704,9.57550796052904,129.032769692033));
#65339=CARTESIAN_POINT('Ctrl Pts',(78.4347777866976,9.57066804868406,129.033140484892));
#65340=CARTESIAN_POINT('Ctrl Pts',(78.4330185594245,9.56581955693993,129.033510872514));
#65341=CARTESIAN_POINT('Ctrl Pts',(78.4063955140418,9.49136886452314,129.039181825837));
#65342=CARTESIAN_POINT('Ctrl Pts',(78.3861651481576,9.4201885652767,129.044377203584));
#65343=CARTESIAN_POINT('Ctrl Pts',(78.3670101448335,9.33048005745388,129.050637648145));
#65344=CARTESIAN_POINT('Ctrl Pts',(78.3635718150495,9.31301081984255,129.051843862163));
#65345=CARTESIAN_POINT('Ctrl Pts',(78.3584909485671,9.28481853175811,129.053770529289));
#65346=CARTESIAN_POINT('Ctrl Pts',(78.3566720343398,9.27412910966829,129.054496466218));
#65347=CARTESIAN_POINT('Ctrl Pts',(78.3533933195721,9.25365392060171,129.05587850655));
#65348=CARTESIAN_POINT('Ctrl Pts',(78.3519160849664,9.24387145710935,129.056535127821));
#65349=CARTESIAN_POINT('Ctrl Pts',(78.3487413011671,9.22149958673453,129.058028695935));
#65350=CARTESIAN_POINT('Ctrl Pts',(78.3471004114896,9.20890266237401,129.058863850537));
#65351=CARTESIAN_POINT('Ctrl Pts',(78.343098820237,9.17517558433679,129.061085240416));
#65352=CARTESIAN_POINT('Ctrl Pts',(78.3409981990532,9.15401653667092,129.062463494616));
#65353=CARTESIAN_POINT('Ctrl Pts',(78.3320442728569,9.04206426885929,129.069685148554));
#65354=CARTESIAN_POINT('Ctrl Pts',(78.3322369658389,8.95085951131381,129.075312514644));
#65355=CARTESIAN_POINT('Ctrl Pts',(78.3462738045227,8.78426953166294,129.085567496954));
#65356=CARTESIAN_POINT('Ctrl Pts',(78.3578552328199,8.70895117483196,129.090198764656));
#65357=CARTESIAN_POINT('Ctrl Pts',(78.3812850995571,8.60469866154225,129.096890537881));
#65358=CARTESIAN_POINT('Ctrl Pts',(78.3888545189105,8.57489872039203,129.098837056392));
#65359=CARTESIAN_POINT('Ctrl Pts',(78.4027543438487,8.52590078818045,129.10211916224));
#65360=CARTESIAN_POINT('Ctrl Pts',(78.4086176559482,8.5065773645729,129.103434963398));
#65361=CARTESIAN_POINT('Ctrl Pts',(78.4172944788986,8.47974682900903,129.105298251857));
#65362=CARTESIAN_POINT('Ctrl Pts',(78.4198134187382,8.47214538884944,129.105830259008));
#65363=CARTESIAN_POINT('Ctrl Pts',(78.4224620540941,8.46434144852794,129.106380968942));
#65364=CARTESIAN_POINT('Ctrl Pts',(78.4225371561925,8.46412032045925,129.106396577302));
#65365=CARTESIAN_POINT('Ctrl Pts',(78.4226868859589,8.46367976544649,129.106427681441));
#65366=CARTESIAN_POINT('Ctrl Pts',(78.422761512932,8.46346033825167,129.106443177181));
#65367=CARTESIAN_POINT('Ctrl Pts',(78.4237785991695,8.46047182498789,129.106654273693));
#65368=CARTESIAN_POINT('Ctrl Pts',(78.4247282947769,8.45770523655226,129.106850285473));
#65369=CARTESIAN_POINT('Ctrl Pts',(78.4274900444015,8.44972836679543,129.107417190554));
#65370=CARTESIAN_POINT('Ctrl Pts',(78.4293206265183,8.44452476828116,129.107789181213));
#65371=CARTESIAN_POINT('Ctrl Pts',(78.4337241304446,8.43220321823269,129.108675118552));
#65372=CARTESIAN_POINT('Ctrl Pts',(78.4363197452551,8.42509362469957,129.109190346749));
#65373=CARTESIAN_POINT('Ctrl Pts',(78.4438026778957,8.40502288117145,129.110655833664));
#65374=CARTESIAN_POINT('Ctrl Pts',(78.4488032042892,8.39210498601955,129.111612064394));
#65375=CARTESIAN_POINT('Ctrl Pts',(78.4913106689426,8.28623591671504,129.119548155318));
#65376=CARTESIAN_POINT('Ctrl Pts',(78.5369720372605,8.19678864365701,129.126874362315));
#65377=CARTESIAN_POINT('Ctrl Pts',(78.6324060131299,8.04529759346339,129.139888978404));
#65378=CARTESIAN_POINT('Ctrl Pts',(78.6791076919509,7.98166026180064,129.145579759877));
#65379=CARTESIAN_POINT('Ctrl Pts',(78.7596137649616,7.88686457320794,129.154328737659));
#65380=CARTESIAN_POINT('Ctrl Pts',(78.7904948318971,7.85338479962445,129.157481101567));
#65381=CARTESIAN_POINT('Ctrl Pts',(78.833576827254,7.81035770208752,129.161620762236));
#65382=CARTESIAN_POINT('Ctrl Pts',(78.8445920853445,7.79965655210509,129.162658228661));
#65383=CARTESIAN_POINT('Ctrl Pts',(78.8632358937586,7.78203886336869,129.164380146634));
#65384=CARTESIAN_POINT('Ctrl Pts',(78.8707832394547,7.77503817224922,129.165068176284));
#65385=CARTESIAN_POINT('Ctrl Pts',(78.8857664572206,7.76139635422207,129.166416689183));
#65386=CARTESIAN_POINT('Ctrl Pts',(78.893198002534,7.75475113937178,129.167077327917));
#65387=CARTESIAN_POINT('Ctrl Pts',(78.9113672907195,7.7387955009853,129.168673085497));
#65388=CARTESIAN_POINT('Ctrl Pts',(78.9221655068856,7.72955488507779,129.169605309563));
#65389=CARTESIAN_POINT('Ctrl Pts',(78.9593349770426,7.69856202035065,129.172761403095));
#65390=CARTESIAN_POINT('Ctrl Pts',(78.9862578662103,7.67748283673119,129.174958513971));
#65391=CARTESIAN_POINT('Ctrl Pts',(79.114206734068,7.58351057113798,129.185037705792));
#65392=CARTESIAN_POINT('Ctrl Pts',(79.2225521275357,7.52126796767256,129.192526099914));
#65393=CARTESIAN_POINT('Ctrl Pts',(79.3842718805351,7.45109402431918,129.203355546841));
#65394=CARTESIAN_POINT('Ctrl Pts',(79.4326462624453,7.43272854468055,129.206560163478));
#65395=CARTESIAN_POINT('Ctrl Pts',(79.5002359686298,7.41060750318749,129.2110873664));
#65396=CARTESIAN_POINT('Ctrl Pts',(79.5187826226719,7.40489424692561,129.212334709194));
#65397=CARTESIAN_POINT('Ctrl Pts',(79.5512026615698,7.39552417899927,129.214530668929));
#65398=CARTESIAN_POINT('Ctrl Pts',(79.5650316368868,7.39172011126247,129.215472238595));
#65399=CARTESIAN_POINT('Ctrl Pts',(79.5856149125803,7.38634295462076,129.216883244935));
#65400=CARTESIAN_POINT('Ctrl Pts',(79.5923331215503,7.38463261989123,129.21734528632));
#65401=CARTESIAN_POINT('Ctrl Pts',(79.6038545031768,7.38177593364863,129.21814053735));
#65402=CARTESIAN_POINT('Ctrl Pts',(79.6086524149382,7.38060892602714,129.218472566003));
#65403=CARTESIAN_POINT('Ctrl Pts',(79.6196847313583,7.37797740252185,129.219238089481));
#65404=CARTESIAN_POINT('Ctrl Pts',(79.6259222878408,7.37652752653623,129.219672384669));
#65405=CARTESIAN_POINT('Ctrl Pts',(79.64342688159,7.37256494089247,129.220894991332));
#65406=CARTESIAN_POINT('Ctrl Pts',(79.6547116459802,7.37013338141764,129.221687613858));
#65407=CARTESIAN_POINT('Ctrl Pts',(79.7352020638562,7.35366329236513,129.22736830653));
#65408=CARTESIAN_POINT('Ctrl Pts',(79.8052063281276,7.34392159934582,129.23244867565));
#65409=CARTESIAN_POINT('Ctrl Pts',(79.8905084908212,7.33753470245526,129.238659942851));
#65410=CARTESIAN_POINT('Ctrl Pts',(79.9054227819681,7.33661958643051,129.239746823039));
#65411=CARTESIAN_POINT('Ctrl Pts',(79.9873562521137,7.33269779944641,129.24571766886));
#65412=CARTESIAN_POINT('Ctrl Pts',(80.0545010602895,7.33354059475028,129.250607147323));
#65413=CARTESIAN_POINT('Ctrl Pts',(80.1947665608827,7.34379009724053,129.260694913019));
#65414=CARTESIAN_POINT('Ctrl Pts',(80.2676912775604,7.35400201812732,129.265865668435));
#65415=CARTESIAN_POINT('Ctrl Pts',(80.3569433059803,7.37259185111791,129.272087507702));
#65416=CARTESIAN_POINT('Ctrl Pts',(80.3741174191915,7.37645387965648,129.273280049958));
#65417=CARTESIAN_POINT('Ctrl Pts',(80.4016206721994,7.38309828568305,129.275182953486));
#65418=CARTESIAN_POINT('Ctrl Pts',(80.4119894431973,7.38570912594357,129.275898771115));
#65419=CARTESIAN_POINT('Ctrl Pts',(80.4317477931971,7.39088702159278,129.277260036902));
#65420=CARTESIAN_POINT('Ctrl Pts',(80.4411413750809,7.39343688941268,129.277906010332));
#65421=CARTESIAN_POINT('Ctrl Pts',(80.4625078028249,7.39943829297402,129.279372854245));
#65422=CARTESIAN_POINT('Ctrl Pts',(80.4744654486544,7.40294214324621,129.280191985236));
#65423=CARTESIAN_POINT('Ctrl Pts',(80.5062186926012,7.41263465059423,129.282363217799));
#65424=CARTESIAN_POINT('Ctrl Pts',(80.5259403251162,7.41905947203715,129.283707606306));
#65425=CARTESIAN_POINT('Ctrl Pts',(80.6639914423166,7.46690251416941,129.29310124537));
#65426=CARTESIAN_POINT('Ctrl Pts',(80.7774346730707,7.52119243848336,129.300691901771));
#65427=CARTESIAN_POINT('Ctrl Pts',(80.9619136228956,7.63662704888598,129.313983320184));
#65428=CARTESIAN_POINT('Ctrl Pts',(81.0358953665722,7.69195585105125,129.319643762182));
#65429=CARTESIAN_POINT('Ctrl Pts',(81.1137259044816,7.76092397072454,129.326443676871));
#65430=CARTESIAN_POINT('Ctrl Pts',(81.1224599058962,7.76883041915964,129.327219942902));
#65431=CARTESIAN_POINT('Ctrl Pts',(81.1357897107494,7.78115695146703,129.328426571261));
#65432=CARTESIAN_POINT('Ctrl Pts',(81.140445426345,7.78551209552131,129.328852213041));
#65433=CARTESIAN_POINT('Ctrl Pts',(81.1490511772298,7.79365537907541,129.329647092406));
#65434=CARTESIAN_POINT('Ctrl Pts',(81.1530076900014,7.79743639851791,129.3300157968));
#65435=CARTESIAN_POINT('Ctrl Pts',(81.1620621088825,7.8061749621513,129.330867013768));
#65436=CARTESIAN_POINT('Ctrl Pts',(81.1671469916541,7.8111457359596,129.331350525344));
#65437=CARTESIAN_POINT('Ctrl Pts',(81.1830092431168,7.82685187163933,129.332875679245));
#65438=CARTESIAN_POINT('Ctrl Pts',(81.1936711422671,7.83770203307569,129.333925527378));
#65439=CARTESIAN_POINT('Ctrl Pts',(81.2719275150088,7.91955267277769,129.341807448212));
#65440=CARTESIAN_POINT('Ctrl Pts',(81.3332803237026,7.9962439060047,129.348972027664));
#65441=CARTESIAN_POINT('Ctrl Pts',(81.4322585482761,8.14517740855901,129.361983553953));
#65442=CARTESIAN_POINT('Ctrl Pts',(81.4720345507428,8.21565124300376,129.367826121522));
#65443=CARTESIAN_POINT('Ctrl Pts',(81.5197623801728,8.31674500962452,129.37569629884));
#65444=CARTESIAN_POINT('Ctrl Pts',(81.5322010794933,8.34511441011223,129.377853571202));
#65445=CARTESIAN_POINT('Ctrl Pts',(81.5527756795281,8.39584059315205,129.381621210999));
#65446=CARTESIAN_POINT('Ctrl Pts',(81.5612370336259,8.41805504932632,129.383241673076));
#65447=CARTESIAN_POINT('Ctrl Pts',(81.5732563561312,8.45176207278793,129.385657655368));
#65448=CARTESIAN_POINT('Ctrl Pts',(81.5771697052544,8.46312373783989,129.386464813307));
#65449=CARTESIAN_POINT('Ctrl Pts',(81.5840276272669,8.48375676707399,129.387917969608));
#65450=CARTESIAN_POINT('Ctrl Pts',(81.5870145455663,8.49301337441842,129.388565333821));
#65451=CARTESIAN_POINT('Ctrl Pts',(81.5932726866105,8.51300505818161,129.389953904057));
#65452=CARTESIAN_POINT('Ctrl Pts',(81.5965168684075,8.52374814805455,129.390694201176));
#65453=CARTESIAN_POINT('Ctrl Pts',(81.6052025699393,8.5535973462121,129.392735407041));
#65454=CARTESIAN_POINT('Ctrl Pts',(81.6104114046925,8.57276963825767,129.394028784438));
#65455=CARTESIAN_POINT('Ctrl Pts',(81.6415725961252,8.69614655347753,129.402248398149));
#65456=CARTESIAN_POINT('Ctrl Pts',(81.6577427127657,8.80256493602061,129.408846579788));
#65457=CARTESIAN_POINT('Ctrl Pts',(81.6694752598998,9.01897428520423,129.422090543117));
#65458=CARTESIAN_POINT('Ctrl Pts',(81.6646333286551,9.12843991030868,129.428709345097));
#65459=CARTESIAN_POINT('Ctrl Pts',(81.6470203446566,9.25119017299837,129.43677153411));
#65460=CARTESIAN_POINT('Ctrl Pts',(81.6447376193638,9.26572663750609,129.437736843581));
#65461=CARTESIAN_POINT('Ctrl Pts',(81.6410854518559,9.28712981107423,129.439176306087));
#65462=CARTESIAN_POINT('Ctrl Pts',(81.6398647082845,9.29402163666587,129.439642604748));
#65463=CARTESIAN_POINT('Ctrl Pts',(81.6376115023218,9.30629162092016,129.440478100688));
#65464=CARTESIAN_POINT('Ctrl Pts',(81.6365958990972,9.31167266643159,129.440846353045));
#65465=CARTESIAN_POINT('Ctrl Pts',(81.6342946628625,9.32354401430019,129.441662910215));
#65466=CARTESIAN_POINT('Ctrl Pts',(81.6329969083748,9.33003161621972,129.442111859903));
#65467=CARTESIAN_POINT('Ctrl Pts',(81.6290745956412,9.34904995358731,129.443435565807));
#65468=CARTESIAN_POINT('Ctrl Pts',(81.6263442653778,9.36155803657349,129.444315873255));
#65469=CARTESIAN_POINT('Ctrl Pts',(81.6197105334249,9.39035139977126,129.446362921784));
#65470=CARTESIAN_POINT('Ctrl Pts',(81.6157052318908,9.40661158858356,129.44753423841));
#65471=CARTESIAN_POINT('Ctrl Pts',(81.6010479660502,9.4624750961828,129.451605284335));
#65472=CARTESIAN_POINT('Ctrl Pts',(81.5891797667841,9.50174200902299,129.454548382122));
#65473=CARTESIAN_POINT('Ctrl Pts',(81.5358512393681,9.65721792035685,129.4664382622));
#65474=CARTESIAN_POINT('Ctrl Pts',(81.4829829089807,9.7691182369275,129.475500162609));
#65475=CARTESIAN_POINT('Ctrl Pts',(81.3937418889939,9.91390334882249,129.487486178465));
#65476=CARTESIAN_POINT('Ctrl Pts',(81.3675826585501,9.95260389991338,129.490723965499));
#65477=CARTESIAN_POINT('Ctrl Pts',(81.3303744326982,10.0029521260012,129.494984464727));
#65478=CARTESIAN_POINT('Ctrl Pts',(81.3207361097378,10.0156107803398,129.496060046533));
#65479=CARTESIAN_POINT('Ctrl Pts',(81.3045169540851,10.0362910259982,129.497825106386));
#65480=CARTESIAN_POINT('Ctrl Pts',(81.298040070851,10.0443924343476,129.498518619685));
#65481=CARTESIAN_POINT('Ctrl Pts',(81.2852057545574,10.0601420007298,129.499871155293));
#65482=CARTESIAN_POINT('Ctrl Pts',(81.2788546736406,10.0677947481888,129.50053039288));
#65483=CARTESIAN_POINT('Ctrl Pts',(81.2635681200239,10.0858822748211,129.50209373222));
#65484=CARTESIAN_POINT('Ctrl Pts',(81.2545712675656,10.0962644124401,129.502995282206));
#65485=CARTESIAN_POINT('Ctrl Pts',(81.2230539405644,10.1317383715663,129.506091858278));
#65486=CARTESIAN_POINT('Ctrl Pts',(81.199900057064,10.1562580960445,129.508260468486));
#65487=CARTESIAN_POINT('Ctrl Pts',(81.140760899942,10.215194636087,129.513565495721));
#65488=CARTESIAN_POINT('Ctrl Pts',(81.1039466648126,10.2487336585203,129.516667718456));
#65489=CARTESIAN_POINT('Ctrl Pts',(81.014768441482,10.3229469653433,129.523823324164));
#65490=CARTESIAN_POINT('Ctrl Pts',(80.9613716284186,10.3622438804543,129.52784437241));
#65491=CARTESIAN_POINT('Ctrl Pts',(80.8995940312351,10.4022627585908,129.532351109272));
#65492=CARTESIAN_POINT('Ctrl Pts',(80.8933849373708,10.4062267306376,129.532802546915));
#65493=CARTESIAN_POINT('Ctrl Pts',(80.8215338585801,10.4514295085387,129.538011258822));
#65494=CARTESIAN_POINT('Ctrl Pts',(80.7531250159643,10.488074270534,129.542821431468));
#65495=CARTESIAN_POINT('Ctrl Pts',(80.6718315826542,10.5245763877766,129.548650184149));
#65496=CARTESIAN_POINT('Ctrl Pts',(80.6611894169383,10.5292218197511,129.54941540588));
#65497=CARTESIAN_POINT('Ctrl Pts',(80.6445757042174,10.5362680661741,129.550614697985));
#65498=CARTESIAN_POINT('Ctrl Pts',(80.6386370933414,10.538746265356,129.551044310206));
#65499=CARTESIAN_POINT('Ctrl Pts',(80.6276137554963,10.5432715309818,129.55184373476));
#65500=CARTESIAN_POINT('Ctrl Pts',(80.6225331045855,10.5453279829771,129.552212982888));
#65501=CARTESIAN_POINT('Ctrl Pts',(80.6107467876728,10.5500310742925,129.553071371104));
#65502=CARTESIAN_POINT('Ctrl Pts',(80.6040340294598,10.5526592853368,129.553561567881));
#65503=CARTESIAN_POINT('Ctrl Pts',(80.5824444773069,10.5609509361831,129.555141853933));
#65504=CARTESIAN_POINT('Ctrl Pts',(80.5675040059945,10.5664445573315,129.556241079376));
#65505=CARTESIAN_POINT('Ctrl Pts',(80.4837476663599,10.5958863590341,129.562425804127));
#65506=CARTESIAN_POINT('Ctrl Pts',(80.4135028499004,10.6155118040121,129.567693364414));
#65507=CARTESIAN_POINT('Ctrl Pts',(80.2093102768779,10.6583681050053,129.58286567028));
#65508=CARTESIAN_POINT('Ctrl Pts',(80.0734733888392,10.6699134390871,129.592743073796));
#65509=CARTESIAN_POINT('Ctrl Pts',(79.9140871152084,10.663951483139,129.603723895439));
#65510=CARTESIAN_POINT('Ctrl Pts',(79.8904691072906,10.6625638770361,129.605337181268));
#65511=CARTESIAN_POINT('Ctrl Pts',(79.8547924971121,10.6597041940744,129.607754341897));
#65512=CARTESIAN_POINT('Ctrl Pts',(79.8427081067325,10.6586025758322,129.608569643622));
#65513=CARTESIAN_POINT('Ctrl Pts',(79.8209710349715,10.6563813049417,129.61003030904));
#65514=CARTESIAN_POINT('Ctrl Pts',(79.8113141765709,10.6553090540994,129.610677127022));
#65515=CARTESIAN_POINT('Ctrl Pts',(79.790652146366,10.6528316759417,129.612056830998));
#65516=CARTESIAN_POINT('Ctrl Pts',(79.7796504691827,10.651400971026,129.612788880886));
#65517=CARTESIAN_POINT('Ctrl Pts',(79.7495225479429,10.6471765637074,129.614787047563));
#65518=CARTESIAN_POINT('Ctrl Pts',(79.7304289630211,10.6441596919199,129.616046119965));
#65519=CARTESIAN_POINT('Ctrl Pts',(79.6880292075684,10.6367018388551,129.618828776504));
#65520=CARTESIAN_POINT('Ctrl Pts',(79.6647564931687,10.6320939187829,129.620347121593));
#65521=CARTESIAN_POINT('Ctrl Pts',(79.5906070408004,10.6157594872455,129.62516562559));
#65522=CARTESIAN_POINT('Ctrl Pts',(79.5401785324455,10.602137993007,129.628412610739));
#65523=CARTESIAN_POINT('Ctrl Pts',(79.3969926614764,10.5561419652216,129.63767205075));
#65524=CARTESIAN_POINT('Ctrl Pts',(79.3063576440549,10.517911196502,129.64357512185));
#65525=CARTESIAN_POINT('Ctrl Pts',(79.1753103881707,10.4484330408034,129.652810886703));
#65526=CARTESIAN_POINT('Ctrl Pts',(79.1320884604503,10.4229545831172,129.65598605807));
#65527=CARTESIAN_POINT('Ctrl Pts',(79.0809209660061,10.3895932622691,129.659987470087));
#65528=CARTESIAN_POINT('Ctrl Pts',(79.0718153432976,10.383527713008,129.660709318309));
#65529=CARTESIAN_POINT('Ctrl Pts',(79.0575775671282,10.3738396591732,129.661854612215));
#65530=CARTESIAN_POINT('Ctrl Pts',(79.0524048435202,10.3702769308661,129.66227420681));
#65531=CARTESIAN_POINT('Ctrl Pts',(79.0428586108828,10.3636220333786,129.663055321648));
#65532=CARTESIAN_POINT('Ctrl Pts',(79.0384797087742,10.3605379138305,129.663416306065));
#65533=CARTESIAN_POINT('Ctrl Pts',(79.0340685596031,10.357399151251,129.663782637891));
#65534=CARTESIAN_POINT('Ctrl Pts',(79.0340213028523,10.357365521892,129.663786562725));
#65535=CARTESIAN_POINT('Ctrl Pts',(79.0339277424457,10.3572989340651,129.663794333853));
#65536=CARTESIAN_POINT('Ctrl Pts',(79.0338814387615,10.357265975725,129.663798180137));
#65537=CARTESIAN_POINT('Ctrl Pts',(79.0337897235461,10.357200686996,129.66380579919));
#65538=CARTESIAN_POINT('Ctrl Pts',(79.033744311954,10.3571683566994,129.663809571953));
#65539=CARTESIAN_POINT('Ctrl Pts',(79.0336543239906,10.3571042839268,129.663817048659));
#65540=CARTESIAN_POINT('Ctrl Pts',(79.033609747549,10.3570725415254,129.663820752599));
#65541=CARTESIAN_POINT('Ctrl Pts',(79.0335213766921,10.3570096070329,129.663828096048));
#65542=CARTESIAN_POINT('Ctrl Pts',(79.0334775821751,10.3569784149841,129.663831735556));
#65543=CARTESIAN_POINT('Ctrl Pts',(79.0333907250902,10.3569165458693,129.663838954277));
#65544=CARTESIAN_POINT('Ctrl Pts',(79.0333476625048,10.3568858688963,129.663842533481));
#65545=CARTESIAN_POINT('Ctrl Pts',(79.0332622225816,10.3568249969763,129.663849635449));
#65546=CARTESIAN_POINT('Ctrl Pts',(79.033219845126,10.3567948020424,129.663853158213));
#65547=CARTESIAN_POINT('Ctrl Pts',(79.0331357309802,10.3567348627936,129.663860150975));
#65548=CARTESIAN_POINT('Ctrl Pts',(79.0330939943671,10.356705118623,129.663863620958));
#65549=CARTESIAN_POINT('Ctrl Pts',(79.0330111206988,10.3566460517983,129.66387051156));
#65550=CARTESIAN_POINT('Ctrl Pts',(79.0329699834751,10.3566167291066,129.663873932185));
#65551=CARTESIAN_POINT('Ctrl Pts',(79.032888268857,10.3565584771652,129.663880727356));
#65552=CARTESIAN_POINT('Ctrl Pts',(79.0328476915594,10.3565295480606,129.663884101886));
#65553=CARTESIAN_POINT('Ctrl Pts',(79.0327670597441,10.356472057104,129.663890807928));
#65554=CARTESIAN_POINT('Ctrl Pts',(79.0327270051818,10.3564434952904,129.663894139437));
#65555=CARTESIAN_POINT('Ctrl Pts',(79.032647383606,10.3563867140007,129.663900762349));
#65556=CARTESIAN_POINT('Ctrl Pts',(79.0326078165229,10.3563584945395,129.663904053753));
#65557=CARTESIAN_POINT('Ctrl Pts',(79.0325291360862,10.3563023740251,129.663910599251));
#65558=CARTESIAN_POINT('Ctrl Pts',(79.0324900228057,10.3562744730835,129.663913853335));
#65559=CARTESIAN_POINT('Ctrl Pts',(79.0324122183353,10.3562189672145,129.66392032681));
#65560=CARTESIAN_POINT('Ctrl Pts',(79.0323735270077,10.3561913622434,129.663923546209));
#65561=CARTESIAN_POINT('Ctrl Pts',(79.0264207909083,10.3519438992621,129.664418889186));
#65562=CARTESIAN_POINT('Ctrl Pts',(79.0205345479884,10.3476854998635,129.664913583756));
#65563=CARTESIAN_POINT('Ctrl Pts',(79.0077412375502,10.3383021037272,129.665999147917));
#65564=CARTESIAN_POINT('Ctrl Pts',(79.0008456604322,10.3331618696556,129.66659096064));
#65565=CARTESIAN_POINT('Ctrl Pts',(78.9817985734491,10.3187326483449,129.668243689541));
#65566=CARTESIAN_POINT('Ctrl Pts',(78.969735017926,10.3093295890135,129.669311074949));
#65567=CARTESIAN_POINT('Ctrl Pts',(78.8442370938526,10.2087007591404,129.680620020114));
#65568=CARTESIAN_POINT('Ctrl Pts',(78.7430949105268,10.1031494354936,129.691449345628));
#65569=CARTESIAN_POINT('Ctrl Pts',(78.6184171537561,9.93328804114736,129.706494452053));
#65570=CARTESIAN_POINT('Ctrl Pts',(78.5829878783349,9.87856490149784,129.711056760906));
#65571=CARTESIAN_POINT('Ctrl Pts',(78.5421550483921,9.80656974110068,129.716705271632));
#65572=CARTESIAN_POINT('Ctrl Pts',(78.5337033961841,9.7911011068514,129.717899442309));
#65573=CARTESIAN_POINT('Ctrl Pts',(78.5205013086131,9.76599926386559,129.719806951901));
#65574=CARTESIAN_POINT('Ctrl Pts',(78.5155959539046,9.75644952728044,129.720525713145));
#65575=CARTESIAN_POINT('Ctrl Pts',(78.5063930892301,9.73809911028932,129.721893930794));
#65576=CARTESIAN_POINT('Ctrl Pts',(78.5020802189354,9.72930668239751,129.722543902177));
#65577=CARTESIAN_POINT('Ctrl Pts',(78.4923182109651,9.70895342019374,129.724035940363));
#65578=CARTESIAN_POINT('Ctrl Pts',(78.4869240276894,9.69736679454486,129.724876082676));
#65579=CARTESIAN_POINT('Ctrl Pts',(78.470170671262,9.66027108577868,129.727537672019));
#65580=CARTESIAN_POINT('Ctrl Pts',(78.4593188578045,9.63453718989222,129.729341916015));
#65581=CARTESIAN_POINT('Ctrl Pts',(78.4448148482087,9.59757339521375,129.731880578999));
#65582=CARTESIAN_POINT('Ctrl Pts',(78.4406282675188,9.58656162418711,129.732630321618));
#65583=CARTESIAN_POINT('Ctrl Pts',(78.4365593800808,9.57550797386886,129.733376810833));
#65584=CARTESIAN_POINT('Origin',(80.,9.,134.));
#65585=CARTESIAN_POINT('',(78.4345148001033,9.5762760062711,130.432124665951));
#65586=CARTESIAN_POINT('',(78.4365593450135,9.57550787860402,130.240113160697));
#65587=CARTESIAN_POINT('',(78.4365593737638,9.57550795670799,134.));
#65588=CARTESIAN_POINT('Ctrl Pts',(78.4365593450135,9.57550787860402,130.240113160697));
#65589=CARTESIAN_POINT('Ctrl Pts',(78.4584396377415,9.63494848830862,130.236203505864));
#65590=CARTESIAN_POINT('Ctrl Pts',(78.48370025951,9.69311543856741,130.232233234758));
#65591=CARTESIAN_POINT('Ctrl Pts',(78.5175577135617,9.76030341362332,130.227313276936));
#65592=CARTESIAN_POINT('Ctrl Pts',(78.5230027528047,9.77082781830187,130.226532472749));
#65593=CARTESIAN_POINT('Ctrl Pts',(78.5315681194996,9.78695932128886,130.225318578752));
#65594=CARTESIAN_POINT('Ctrl Pts',(78.5346094847926,9.79260822322694,130.224890228581));
#65595=CARTESIAN_POINT('Ctrl Pts',(78.5403123336663,9.80305542989845,130.224091675299));
#65596=CARTESIAN_POINT('Ctrl Pts',(78.5429649853485,9.80785832270995,130.223722020747));
#65597=CARTESIAN_POINT('Ctrl Pts',(78.5491155823773,9.81886576320299,130.222869041378));
#65598=CARTESIAN_POINT('Ctrl Pts',(78.552629631519,9.82506105424188,130.222384723356));
#65599=CARTESIAN_POINT('Ctrl Pts',(78.5640897687712,9.84496681951748,130.220815338122));
#65600=CARTESIAN_POINT('Ctrl Pts',(78.5721915086987,9.85858603803132,130.219721181053));
#65601=CARTESIAN_POINT('Ctrl Pts',(78.6239893833583,9.94289851439503,130.212828785794));
#65602=CARTESIAN_POINT('Ctrl Pts',(78.6727263845778,10.0103489176001,130.206792932316));
#65603=CARTESIAN_POINT('Ctrl Pts',(78.7849432153425,10.1434483555392,130.194121185347));
#65604=CARTESIAN_POINT('Ctrl Pts',(78.8492083490042,10.2081054845086,130.187507124277));
#65605=CARTESIAN_POINT('Ctrl Pts',(78.9435463543594,10.2886238119911,130.178753033757));
#65606=CARTESIAN_POINT('Ctrl Pts',(78.9692868373261,10.30930373172,130.176448576161));
#65607=CARTESIAN_POINT('Ctrl Pts',(79.0155264189662,10.3442432398726,130.17245368182));
#65608=CARTESIAN_POINT('Ctrl Pts',(79.0357625266469,10.3588319731765,130.170751319968));
#65609=CARTESIAN_POINT('Ctrl Pts',(79.0644071402272,10.3785203334929,130.168403343902));
#65610=CARTESIAN_POINT('Ctrl Pts',(79.0725437973101,10.3840076980862,130.167743130963));
#65611=CARTESIAN_POINT('Ctrl Pts',(79.0890092917068,10.3949016147028,130.16642041019));
#65612=CARTESIAN_POINT('Ctrl Pts',(79.0973389253431,10.4003062439859,130.165757993237));
#65613=CARTESIAN_POINT('Ctrl Pts',(79.1144836587366,10.4112139395308,130.164407999066));
#65614=CARTESIAN_POINT('Ctrl Pts',(79.1233029362681,10.4167096528558,130.163720714678));
#65615=CARTESIAN_POINT('Ctrl Pts',(79.1458399657848,10.4304625020145,130.161982073889));
#65616=CARTESIAN_POINT('Ctrl Pts',(79.1596265880928,10.438605189575,130.160934908638));
#65617=CARTESIAN_POINT('Ctrl Pts',(79.2149162649246,10.4701944069642,130.156797282838));
#65618=CARTESIAN_POINT('Ctrl Pts',(79.2573019386848,10.4920550588343,130.153762979926));
#65619=CARTESIAN_POINT('Ctrl Pts',(79.4019403855505,10.5589596945325,130.143770081131));
#65620=CARTESIAN_POINT('Ctrl Pts',(79.507766621818,10.5955366874004,130.137058399044));
#65621=CARTESIAN_POINT('Ctrl Pts',(79.679428206345,10.636146959915,130.126203662879));
#65622=CARTESIAN_POINT('Ctrl Pts',(79.7432060297944,10.6473609673009,130.12217143354));
#65623=CARTESIAN_POINT('Ctrl Pts',(79.8224532895596,10.6565810608224,130.11698855349));
#65624=CARTESIAN_POINT('Ctrl Pts',(79.8374624756375,10.6581209725366,130.115999317393));
#65625=CARTESIAN_POINT('Ctrl Pts',(79.8595218555694,10.6600818445882,130.114531517717));
#65626=CARTESIAN_POINT('Ctrl Pts',(79.8665576017127,10.6606622057536,130.114061298943));
#65627=CARTESIAN_POINT('Ctrl Pts',(79.8785327299134,10.6615734133995,130.113257122165));
#65628=CARTESIAN_POINT('Ctrl Pts',(79.8834702415549,10.6619269900686,130.112924429056));
#65629=CARTESIAN_POINT('Ctrl Pts',(79.8947206927008,10.6626822546039,130.112163737765));
#65630=CARTESIAN_POINT('Ctrl Pts',(79.9010342473554,10.6630699891434,130.111734995978));
#65631=CARTESIAN_POINT('Ctrl Pts',(79.9184541870998,10.6640402555346,130.110547205473));
#65632=CARTESIAN_POINT('Ctrl Pts',(79.929564194952,10.6645475278126,130.109784245536));
#65633=CARTESIAN_POINT('Ctrl Pts',(79.9939823596229,10.6668427468095,130.105332213628));
#65634=CARTESIAN_POINT('Ctrl Pts',(80.0473418230552,10.6661808194633,130.101533324885));
#65635=CARTESIAN_POINT('Ctrl Pts',(80.2017424916781,10.656843068918,130.090375726615));
#65636=CARTESIAN_POINT('Ctrl Pts',(80.3021513344009,10.641503993704,130.082927733981));
#65637=CARTESIAN_POINT('Ctrl Pts',(80.4708338847551,10.5997235399595,130.070473194759));
#65638=CARTESIAN_POINT('Ctrl Pts',(80.5399226803025,10.5777471410824,130.065385513374));
#65639=CARTESIAN_POINT('Ctrl Pts',(80.6237556504052,10.5449254058465,130.059241761507));
#65640=CARTESIAN_POINT('Ctrl Pts',(80.6400385455896,10.5382510596255,130.058049607999));
#65641=CARTESIAN_POINT('Ctrl Pts',(80.6660756878975,10.5270934184494,130.056144477513));
#65642=CARTESIAN_POINT('Ctrl Pts',(80.6758973084406,10.5227718044534,130.055426102522));
#65643=CARTESIAN_POINT('Ctrl Pts',(80.6946042937851,10.5143238858072,130.054058091017));
#65644=CARTESIAN_POINT('Ctrl Pts',(80.7034963204906,10.5102135246776,130.053407944338));
#65645=CARTESIAN_POINT('Ctrl Pts',(80.7237243376113,10.5006456461992,130.051928930369));
#65646=CARTESIAN_POINT('Ctrl Pts',(80.7350358883612,10.4951376289706,130.051101843743));
#65647=CARTESIAN_POINT('Ctrl Pts',(80.7650953607622,10.4800769497162,130.048903034176));
#65648=CARTESIAN_POINT('Ctrl Pts',(80.7837269008944,10.4702961934403,130.047539240461));
#65649=CARTESIAN_POINT('Ctrl Pts',(80.9074946751918,10.4023020488292,130.038461107788));
#65650=CARTESIAN_POINT('Ctrl Pts',(81.0062529326323,10.3332128475217,130.031159541367));
#65651=CARTESIAN_POINT('Ctrl Pts',(81.1469125988658,10.2102034550111,130.019742157113));
#65652=CARTESIAN_POINT('Ctrl Pts',(81.1944157119895,10.1633446339648,130.01565827716));
#65653=CARTESIAN_POINT('Ctrl Pts',(81.2540444014471,10.09701248229,130.010013830069));
#65654=CARTESIAN_POINT('Ctrl Pts',(81.2687662662898,10.0799517614735,130.0085729031));
#65655=CARTESIAN_POINT('Ctrl Pts',(81.2933707213458,10.0502407467067,130.006071280877));
#65656=CARTESIAN_POINT('Ctrl Pts',(81.3034250661465,10.0377362378484,130.005020667906));
#65657=CARTESIAN_POINT('Ctrl Pts',(81.3177488380146,10.0193852821972,130.003478815302));
#65658=CARTESIAN_POINT('Ctrl Pts',(81.3221635803626,10.0136527095466,130.00299715874));
#65659=CARTESIAN_POINT('Ctrl Pts',(81.3298306653722,10.0035616445375,130.002148929247));
#65660=CARTESIAN_POINT('Ctrl Pts',(81.3330992226438,9.99921570960611,130.00178349062));
#65661=CARTESIAN_POINT('Ctrl Pts',(81.3401709167182,9.98971659088475,130.000984354978));
#65662=CARTESIAN_POINT('Ctrl Pts',(81.3439655749581,9.9845575382707,130.000550128481));
#65663=CARTESIAN_POINT('Ctrl Pts',(81.3544715323461,9.97010018478609,129.999332996871));
#65664=CARTESIAN_POINT('Ctrl Pts',(81.361116562477,9.96075448769974,129.998545876653));
#65665=CARTESIAN_POINT('Ctrl Pts',(81.4049740195483,9.89770426300165,129.993237415687));
#65666=CARTESIAN_POINT('Ctrl Pts',(81.4390920973017,9.84192456583974,129.988551816221));
#65667=CARTESIAN_POINT('Ctrl Pts',(81.4805337001838,9.76425886454824,129.982171680867));
#65668=CARTESIAN_POINT('Ctrl Pts',(81.490812938907,9.74400833928629,129.980520381267));
#65669=CARTESIAN_POINT('Ctrl Pts',(81.5318115955084,9.65897580128198,129.973650239493));
#65670=CARTESIAN_POINT('Ctrl Pts',(81.5587491220857,9.59245101053975,129.968430948267));
#65671=CARTESIAN_POINT('Ctrl Pts',(81.6024927256106,9.46054167359784,129.958500401865));
#65672=CARTESIAN_POINT('Ctrl Pts',(81.6197828134281,9.39545835218695,129.953786265238));
#65673=CARTESIAN_POINT('Ctrl Pts',(81.6365059221305,9.312573996056,129.948019147026));
#65674=CARTESIAN_POINT('Ctrl Pts',(81.6396576674137,9.2955958538804,129.946849781926));
#65675=CARTESIAN_POINT('Ctrl Pts',(81.6443275251638,9.26806087832203,129.94497198196));
#65676=CARTESIAN_POINT('Ctrl Pts',(81.6460091627837,9.25753347289706,129.944258427745));
#65677=CARTESIAN_POINT('Ctrl Pts',(81.6490453337277,9.23728020331689,129.942893796032));
#65678=CARTESIAN_POINT('Ctrl Pts',(81.6504151514682,9.22755711901948,129.942242262867));
#65679=CARTESIAN_POINT('Ctrl Pts',(81.6533636090416,9.20519961009279,129.940752058773));
#65680=CARTESIAN_POINT('Ctrl Pts',(81.6548835460823,9.19255795890532,129.939915263133));
#65681=CARTESIAN_POINT('Ctrl Pts',(81.6593278738961,9.15164099102099,129.937224523326));
#65682=CARTESIAN_POINT('Ctrl Pts',(81.6616737109153,9.12330699418316,129.93538860175));
#65683=CARTESIAN_POINT('Ctrl Pts',(81.6707448141518,8.96436217257609,129.925215961396));
#65684=CARTESIAN_POINT('Ctrl Pts',(81.6627981750819,8.8333778861654,129.917353388849));
#65685=CARTESIAN_POINT('Ctrl Pts',(81.626977310635,8.63451135661191,129.904955328123));
#65686=CARTESIAN_POINT('Ctrl Pts',(81.6098530056037,8.5652493924233,129.900536182257));
#65687=CARTESIAN_POINT('Ctrl Pts',(81.5835917996731,8.48227262855247,129.894889332106));
#65688=CARTESIAN_POINT('Ctrl Pts',(81.578621142618,8.46730884841996,129.893856503465));
#65689=CARTESIAN_POINT('Ctrl Pts',(81.571077433808,8.44563250026466,129.892336075947));
#65690=CARTESIAN_POINT('Ctrl Pts',(81.5686719621035,8.43886196141422,129.891857693171));
#65691=CARTESIAN_POINT('Ctrl Pts',(81.5643716149956,8.42700179417144,129.891013213612));
#65692=CARTESIAN_POINT('Ctrl Pts',(81.5624955366561,8.4219055523686,129.890648219713));
#65693=CARTESIAN_POINT('Ctrl Pts',(81.5583436261761,8.41079503495413,129.889847736274));
#65694=CARTESIAN_POINT('Ctrl Pts',(81.5560579182983,8.40478482925533,129.889411696266));
#65695=CARTESIAN_POINT('Ctrl Pts',(81.5495509905438,8.38796869772132,129.888183498437));
#65696=CARTESIAN_POINT('Ctrl Pts',(81.5452517046582,8.37719365954709,129.887386997125));
#65697=CARTESIAN_POINT('Ctrl Pts',(81.5119759071059,8.29626257375875,129.881336992445));
#65698=CARTESIAN_POINT('Ctrl Pts',(81.4783505602131,8.2281227339408,129.875862336352));
#65699=CARTESIAN_POINT('Ctrl Pts',(81.4356024673256,8.15460937656808,129.869681905552));
#65700=CARTESIAN_POINT('Ctrl Pts',(81.4309370072611,8.14673624797593,129.869016237437));
#65701=CARTESIAN_POINT('Ctrl Pts',(81.3985134747587,8.09303426970591,129.864451292215));
#65702=CARTESIAN_POINT('Ctrl Pts',(81.3686226565074,8.04852792971969,129.860546414805));
#65703=CARTESIAN_POINT('Ctrl Pts',(81.2850909161257,7.93625436121085,129.850449641161));
#65704=CARTESIAN_POINT('Ctrl Pts',(81.2282280395239,7.871074149271,129.844341359641));
#65705=CARTESIAN_POINT('Ctrl Pts',(81.1535016636901,7.7977835681413,129.837190913773));
#65706=CARTESIAN_POINT('Ctrl Pts',(81.1402351497289,7.78519372458252,129.835950907164));
#65707=CARTESIAN_POINT('Ctrl Pts',(81.1187539842749,7.76547022713178,129.833988567409));
#65708=CARTESIAN_POINT('Ctrl Pts',(81.1106724473106,7.75819447500012,129.833260229961));
#65709=CARTESIAN_POINT('Ctrl Pts',(81.0952079750569,7.74454366080545,129.831884909927));
#65710=CARTESIAN_POINT('Ctrl Pts',(81.0878391939669,7.73815332816009,129.831237306303));
#65711=CARTESIAN_POINT('Ctrl Pts',(81.0709027222248,7.7237243623422,129.829766073322));
#65712=CARTESIAN_POINT('Ctrl Pts',(81.0612997831911,7.71572786056812,129.828944189754));
#65713=CARTESIAN_POINT('Ctrl Pts',(81.0358733514287,7.6950348911552,129.826799188378));
#65714=CARTESIAN_POINT('Ctrl Pts',(81.0199060525578,7.68251784199807,129.825483205459));
#65715=CARTESIAN_POINT('Ctrl Pts',(80.8821310171022,7.57851982758275,129.814374571546));
#65716=CARTESIAN_POINT('Ctrl Pts',(80.7485436306297,7.50385666001635,129.805297286916));
#65717=CARTESIAN_POINT('Ctrl Pts',(80.5501760935155,7.42629697231077,129.792162776031));
#65718=CARTESIAN_POINT('Ctrl Pts',(80.4925279210409,7.40731371028175,129.788370911648));
#65719=CARTESIAN_POINT('Ctrl Pts',(80.419846098496,7.38770363504316,129.783476291972));
#65720=CARTESIAN_POINT('Ctrl Pts',(80.4056629557903,7.38407678236913,129.782515844207));
#65721=CARTESIAN_POINT('Ctrl Pts',(80.3846562163795,7.37899900544596,129.781082992177));
#65722=CARTESIAN_POINT('Ctrl Pts',(80.3778679007759,7.37740316950115,129.780618384398));
#65723=CARTESIAN_POINT('Ctrl Pts',(80.3662540756319,7.37474975617759,129.779820493409));
#65724=CARTESIAN_POINT('Ctrl Pts',(80.3614335655779,7.37367094977928,129.779488421072));
#65725=CARTESIAN_POINT('Ctrl Pts',(80.3503726349639,7.37124717456981,129.778724349434));
#65726=CARTESIAN_POINT('Ctrl Pts',(80.3441293699365,7.36991665151617,129.778291564562));
#65727=CARTESIAN_POINT('Ctrl Pts',(80.3267385481417,7.36631479511656,129.777082122721));
#65728=CARTESIAN_POINT('Ctrl Pts',(80.315575388386,7.36412176982262,129.776301330267));
#65729=CARTESIAN_POINT('Ctrl Pts',(80.2469314789489,7.35136527212779,129.771476416119));
#65730=CARTESIAN_POINT('Ctrl Pts',(80.1889557303079,7.34371926179262,129.767300871583));
#65731=CARTESIAN_POINT('Ctrl Pts',(79.9813694698386,7.32738284537932,129.75224532073));
#65732=CARTESIAN_POINT('Ctrl Pts',(79.8310939293539,7.33582386691991,129.741233678064));
#65733=CARTESIAN_POINT('Ctrl Pts',(79.655555976692,7.36973884939697,129.728852717221));
#65734=CARTESIAN_POINT('Ctrl Pts',(79.6272949355791,7.37596668127421,129.726871477612));
#65735=CARTESIAN_POINT('Ctrl Pts',(79.5866285560327,7.38604583854641,129.724036443155));
#65736=CARTESIAN_POINT('Ctrl Pts',(79.5740847748836,7.38931063719569,129.723164152799));
#65737=CARTESIAN_POINT('Ctrl Pts',(79.5521039765462,7.3953063751952,129.721639113229));
#65738=CARTESIAN_POINT('Ctrl Pts',(79.5426507708356,7.39797497928408,129.720984389695));
#65739=CARTESIAN_POINT('Ctrl Pts',(79.5229872476007,7.40371415546975,129.71962465741));
#65740=CARTESIAN_POINT('Ctrl Pts',(79.5127816669158,7.4067994576257,129.718920160765));
#65741=CARTESIAN_POINT('Ctrl Pts',(79.4861319848341,7.41513608738089,129.717083258668));
#65742=CARTESIAN_POINT('Ctrl Pts',(79.4697383768697,7.42054547204248,129.715956044717));
#65743=CARTESIAN_POINT('Ctrl Pts',(79.3965459086622,7.44596479959832,129.710931736298));
#65744=CARTESIAN_POINT('Ctrl Pts',(79.3407696868641,7.4687917096451,129.707127905632));
#65745=CARTESIAN_POINT('Ctrl Pts',(79.1920033861133,7.53931574632667,129.69689562568));
#65746=CARTESIAN_POINT('Ctrl Pts',(79.1020757738566,7.59280825793535,129.690622686182));
#65747=CARTESIAN_POINT('Ctrl Pts',(78.9832024540604,7.67958040109962,129.681531268652));
#65748=CARTESIAN_POINT('Ctrl Pts',(78.9496440237056,7.70611554138256,129.678860849499));
#65749=CARTESIAN_POINT('Ctrl Pts',(78.9040700977414,7.74509374912829,129.67502762809));
#65750=CARTESIAN_POINT('Ctrl Pts',(78.8911687822314,7.75647865717337,129.673917828306));
#65751=CARTESIAN_POINT('Ctrl Pts',(78.8687793946973,7.77686188174313,129.671943025247));
#65752=CARTESIAN_POINT('Ctrl Pts',(78.8592164332387,7.7857760741961,129.671083302788));
#65753=CARTESIAN_POINT('Ctrl Pts',(78.8449329266381,7.79940823933097,129.669772569093));
#65754=CARTESIAN_POINT('Ctrl Pts',(78.8401339421055,7.80404379526237,129.669327543101));
#65755=CARTESIAN_POINT('Ctrl Pts',(78.8314481082018,7.81253528418582,129.668513278921));
#65756=CARTESIAN_POINT('Ctrl Pts',(78.8275522570026,7.81638170748038,129.668144763176));
#65757=CARTESIAN_POINT('Ctrl Pts',(78.8187625615994,7.82514586161174,129.667305831887));
#65758=CARTESIAN_POINT('Ctrl Pts',(78.8138804556329,7.83007497910539,129.666834549982));
#65759=CARTESIAN_POINT('Ctrl Pts',(78.7989693094706,7.84531897930945,129.665379127904));
#65760=CARTESIAN_POINT('Ctrl Pts',(78.7890432867686,7.85573308044749,129.664387742278));
#65761=CARTESIAN_POINT('Ctrl Pts',(78.7025442093338,7.94887147343087,129.655556885467));
#65762=CARTESIAN_POINT('Ctrl Pts',(78.6344217207973,8.03903429878547,129.647274372975));
#65763=CARTESIAN_POINT('Ctrl Pts',(78.5208163116355,8.22614703515834,129.631386156901));
#65764=CARTESIAN_POINT('Ctrl Pts',(78.4745007280648,8.32199392122424,129.623806061303));
#65765=CARTESIAN_POINT('Ctrl Pts',(78.4310549688759,8.43935281318309,129.615249420679));
#65766=CARTESIAN_POINT('Ctrl Pts',(78.4247905745595,8.45720252776885,129.613966017212));
#65767=CARTESIAN_POINT('Ctrl Pts',(78.4153589338174,8.48561669847658,129.611950593604));
#65768=CARTESIAN_POINT('Ctrl Pts',(78.411990402685,8.49611209734192,129.611212027168));
#65769=CARTESIAN_POINT('Ctrl Pts',(78.4061270348181,8.5150237049355,129.609891468943));
#65770=CARTESIAN_POINT('Ctrl Pts',(78.4035941096849,8.52342757705197,129.609308253963));
#65771=CARTESIAN_POINT('Ctrl Pts',(78.3978011802359,8.54321221569553,129.607943484687));
#65772=CARTESIAN_POINT('Ctrl Pts',(78.394595801618,8.55460858803986,129.607163726408));
#65773=CARTESIAN_POINT('Ctrl Pts',(78.385558706467,8.58810477414046,129.604889751872));
#65774=CARTESIAN_POINT('Ctrl Pts',(78.3800598098539,8.61029212278691,129.603406228698));
#65775=CARTESIAN_POINT('Ctrl Pts',(78.3567709503096,8.71329311408802,129.596613030725));
#65776=CARTESIAN_POINT('Ctrl Pts',(78.344559571524,8.7952517264195,129.591479869621));
#65777=CARTESIAN_POINT('Ctrl Pts',(78.3342832370164,8.93496023441837,129.582891629397));
#65778=CARTESIAN_POINT('Ctrl Pts',(78.3330316953672,8.99231227401811,129.579409299768));
#65779=CARTESIAN_POINT('Ctrl Pts',(78.3370332831663,9.12662227422245,129.571163214109));
#65780=CARTESIAN_POINT('Ctrl Pts',(78.3446663326461,9.20336869120854,129.566381276082));
#65781=CARTESIAN_POINT('Ctrl Pts',(78.3595251703247,9.29074579232956,129.560584057839));
#65782=CARTESIAN_POINT('Ctrl Pts',(78.3615910027081,9.3021700210342,129.559819002062));
#65783=CARTESIAN_POINT('Ctrl Pts',(78.3649871346774,9.3198911330595,129.558619896541));
#65784=CARTESIAN_POINT('Ctrl Pts',(78.3662348614166,9.32620373274114,129.558190303674));
#65785=CARTESIAN_POINT('Ctrl Pts',(78.368609225478,9.337860879347,129.557392197737));
#65786=CARTESIAN_POINT('Ctrl Pts',(78.3697256115303,9.34320729673908,129.557024261282));
#65787=CARTESIAN_POINT('Ctrl Pts',(78.3723670577676,9.35555355090209,129.556170231338));
#65788=CARTESIAN_POINT('Ctrl Pts',(78.3739109820356,9.36254906299039,129.55568310139));
#65789=CARTESIAN_POINT('Ctrl Pts',(78.3790046809061,9.38494134313742,129.554113935181));
#65790=CARTESIAN_POINT('Ctrl Pts',(78.3827282745611,9.4002971179156,129.553022836315));
#65791=CARTESIAN_POINT('Ctrl Pts',(78.4006110602173,9.46971737512293,129.548028830699));
#65792=CARTESIAN_POINT('Ctrl Pts',(78.4172634432597,9.52308810287248,129.544020629459));
#65793=CARTESIAN_POINT('Ctrl Pts',(78.4365593657201,9.57550793485619,129.539973235759));
#65794=CARTESIAN_POINT('',(78.3314564671933,8.99960363844182,129.771406544454));
#65795=CARTESIAN_POINT('Ctrl Pts',(78.4365593800808,9.57550797386886,129.733376810833));
#65796=CARTESIAN_POINT('Ctrl Pts',(78.414507417672,9.51560101281142,129.737422524153));
#65797=CARTESIAN_POINT('Ctrl Pts',(78.3959123009134,9.45446380635038,129.741369971414));
#65798=CARTESIAN_POINT('Ctrl Pts',(78.3537670691965,9.28056134816839,129.752338051858));
#65799=CARTESIAN_POINT('Ctrl Pts',(78.3383266317708,9.16623277136057,129.759240425368));
#65800=CARTESIAN_POINT('Ctrl Pts',(78.334257702077,9.0340011424429,129.767706247489));
#65801=CARTESIAN_POINT('Ctrl Pts',(78.3339949934347,9.01675531302839,129.768820136022));
#65802=CARTESIAN_POINT('Ctrl Pts',(78.3340000722429,8.9995093746836,129.769946555234));
#65803=CARTESIAN_POINT('Ctrl Pts',(78.3313278592448,8.99960840453889,129.77148036339));
#65804=CARTESIAN_POINT('Ctrl Pts',(78.3312607575407,8.97840260638213,129.772904623852));
#65805=CARTESIAN_POINT('Ctrl Pts',(78.3316300830525,8.9571992057451,129.774328884314));
#65806=CARTESIAN_POINT('Ctrl Pts',(78.3535890732394,8.38496486156091,129.81279751744));
#65807=CARTESIAN_POINT('Ctrl Pts',(78.9961810022836,7.30590926040735,129.886886262768));
#65808=CARTESIAN_POINT('Ctrl Pts',(80.8788147478848,7.23781766213866,129.99801938076));
#65809=CARTESIAN_POINT('Ctrl Pts',(81.9571171728831,8.78254798385477,130.10915249875));
#65810=CARTESIAN_POINT('Ctrl Pts',(81.2441916059336,10.5262973432389,130.220285616743));
#65811=CARTESIAN_POINT('Ctrl Pts',(79.4504429460659,10.8622730768263,130.327943005808));
#65812=CARTESIAN_POINT('Ctrl Pts',(78.6106061858031,10.0444575566693,130.398556022212));
#65813=CARTESIAN_POINT('Ctrl Pts',(78.4345148001033,9.5762760062711,130.432124665951));
#65814=CARTESIAN_POINT('Origin',(80.,9.,134.));
#65815=CARTESIAN_POINT('',(78.4365594215428,9.57550808650568,131.131996250734));
#65816=CARTESIAN_POINT('',(78.4365593737218,9.57550795659375,130.937771496081));
#65817=CARTESIAN_POINT('',(78.4365593737638,9.57550795670799,134.));
#65818=CARTESIAN_POINT('',(78.3340004596976,8.99985719244809,130.276978875517));
#65819=CARTESIAN_POINT('Ctrl Pts',(78.4365593737218,9.57550795659375,130.937771496081));
#65820=CARTESIAN_POINT('Ctrl Pts',(78.4379751834906,9.57935418406338,130.937505244088));
#65821=CARTESIAN_POINT('Ctrl Pts',(78.4394052087154,9.58319524748535,130.937239436776));
#65822=CARTESIAN_POINT('Ctrl Pts',(78.4707358569938,9.66640923904976,130.931482506129));
#65823=CARTESIAN_POINT('Ctrl Pts',(78.5066422199259,9.7433944779014,130.926197199358));
#65824=CARTESIAN_POINT('Ctrl Pts',(78.5811685246371,9.87576981268402,130.916866755145));
#65825=CARTESIAN_POINT('Ctrl Pts',(78.6175760510482,9.93217992512712,130.912799799818));
#65826=CARTESIAN_POINT('Ctrl Pts',(78.7005830826991,10.0451896256856,130.904182177699));
#65827=CARTESIAN_POINT('Ctrl Pts',(78.747711173067,10.1012155235608,130.899629886433));
#65828=CARTESIAN_POINT('Ctrl Pts',(78.8063923458778,10.1623214944161,130.894088379128));
#65829=CARTESIAN_POINT('Ctrl Pts',(78.8145118041003,10.1706016432865,130.893324142678));
#65830=CARTESIAN_POINT('Ctrl Pts',(78.8272677976328,10.1833412662076,130.89212605099));
#65831=CARTESIAN_POINT('Ctrl Pts',(78.8318450244955,10.1878599751282,130.891696640511));
#65832=CARTESIAN_POINT('Ctrl Pts',(78.8403363103109,10.19614616166,130.890900684722));
#65833=CARTESIAN_POINT('Ctrl Pts',(78.8442427714225,10.1999211385471,130.890534728785));
#65834=CARTESIAN_POINT('Ctrl Pts',(78.8533621412183,10.2086477207897,130.889681001054));
#65835=CARTESIAN_POINT('Ctrl Pts',(78.8585886869604,10.2135847320351,130.889192159077));
#65836=CARTESIAN_POINT('Ctrl Pts',(78.8753979035261,10.2292581314186,130.887621891715));
#65837=CARTESIAN_POINT('Ctrl Pts',(78.8871009585734,10.2398633422209,130.886531495123));
#65838=CARTESIAN_POINT('Ctrl Pts',(78.952643611711,10.2975819471989,130.880448895773));
#65839=CARTESIAN_POINT('Ctrl Pts',(79.0093195498349,10.3413517606602,130.875280771577));
#65840=CARTESIAN_POINT('Ctrl Pts',(79.1777139782204,10.4548923896384,130.86051579327));
#65841=CARTESIAN_POINT('Ctrl Pts',(79.2951524804599,10.5152781903522,130.850933440117));
#65842=CARTESIAN_POINT('Ctrl Pts',(79.4444118699137,10.5708733631537,130.839919217809));
#65843=CARTESIAN_POINT('Ctrl Pts',(79.4705736242051,10.5798826426471,130.838026795321));
#65844=CARTESIAN_POINT('Ctrl Pts',(79.5089589691052,10.592040644828,130.835303612249));
#65845=CARTESIAN_POINT('Ctrl Pts',(79.5210119441027,10.5957083587699,130.834456067366));
#65846=CARTESIAN_POINT('Ctrl Pts',(79.5425108481101,10.6019849166262,130.832957301368));
#65847=CARTESIAN_POINT('Ctrl Pts',(79.5519402478758,10.6046477690668,130.832304350989));
#65848=CARTESIAN_POINT('Ctrl Pts',(79.5717352190971,10.6100497538394,130.830942588391));
#65849=CARTESIAN_POINT('Ctrl Pts',(79.5821048723999,10.612772334768,130.830234337694));
#65850=CARTESIAN_POINT('Ctrl Pts',(79.6095212898809,10.6196884043995,130.828374762362));
#65851=CARTESIAN_POINT('Ctrl Pts',(79.626609589312,10.6237129640936,130.827228880746));
#65852=CARTESIAN_POINT('Ctrl Pts',(79.7138364572567,10.6428063178926,130.821441573491));
#65853=CARTESIAN_POINT('Ctrl Pts',(79.7848364561503,10.6536047522235,130.816937519547));
#65854=CARTESIAN_POINT('Ctrl Pts',(79.9242077807574,10.6656695290136,130.808296220132));
#65855=CARTESIAN_POINT('Ctrl Pts',(79.9923934714281,10.6673757167706,130.8041594857));
#65856=CARTESIAN_POINT('Ctrl Pts',(80.081361403172,10.6641431416272,130.798710716352));
#65857=CARTESIAN_POINT('Ctrl Pts',(80.1022136202209,10.6629926111476,130.79742969099));
#65858=CARTESIAN_POINT('Ctrl Pts',(80.1886094363188,10.6565945862949,130.792087569456));
#65859=CARTESIAN_POINT('Ctrl Pts',(80.2538278840491,10.6478617817643,130.787973383496));
#65860=CARTESIAN_POINT('Ctrl Pts',(80.3296164783878,10.6331076791544,130.78292160702));
#65861=CARTESIAN_POINT('Ctrl Pts',(80.3408583486454,10.6307983574793,130.782165132843));
#65862=CARTESIAN_POINT('Ctrl Pts',(80.3583356251815,10.6270195470387,130.780976656589));
#65863=CARTESIAN_POINT('Ctrl Pts',(80.3645881837285,10.625629871642,130.780548986807));
#65864=CARTESIAN_POINT('Ctrl Pts',(80.3761326778587,10.6229940744072,130.779754483507));
#65865=CARTESIAN_POINT('Ctrl Pts',(80.38142671777,10.6217580623257,130.779388219889));
#65866=CARTESIAN_POINT('Ctrl Pts',(80.3937469828435,10.6188179591084,130.778531419909));
#65867=CARTESIAN_POINT('Ctrl Pts',(80.4007682341566,10.6170940259757,130.778039786706));
#65868=CARTESIAN_POINT('Ctrl Pts',(80.4233065847499,10.6114043699215,130.776451341093));
#65869=CARTESIAN_POINT('Ctrl Pts',(80.4387772555274,10.6072607072406,130.775345274263));
#65870=CARTESIAN_POINT('Ctrl Pts',(80.4758124162859,10.5967666835419,130.772663361832));
#65871=CARTESIAN_POINT('Ctrl Pts',(80.4973124638019,10.5902017193229,130.771078375536));
#65872=CARTESIAN_POINT('Ctrl Pts',(80.5817602739066,10.5625358540965,130.764757841005));
#65873=CARTESIAN_POINT('Ctrl Pts',(80.6435535133111,10.5381161465364,130.759924364264));
#65874=CARTESIAN_POINT('Ctrl Pts',(80.8130248808979,10.4591395914823,130.746314219354));
#65875=CARTESIAN_POINT('Ctrl Pts',(80.9164940894801,10.396476432135,130.737608136743));
#65876=CARTESIAN_POINT('Ctrl Pts',(81.0289943146054,10.3104077263546,130.727863912798));
#65877=CARTESIAN_POINT('Ctrl Pts',(81.0454439082223,10.29732217024,130.726430182854));
#65878=CARTESIAN_POINT('Ctrl Pts',(81.071332379409,10.2759157629804,130.724158394585));
#65879=CARTESIAN_POINT('Ctrl Pts',(81.08093180173,10.2677935780116,130.723312512529));
#65880=CARTESIAN_POINT('Ctrl Pts',(81.0978436067285,10.2531525633496,130.721815639502));
#65881=CARTESIAN_POINT('Ctrl Pts',(81.1051920852422,10.2466765392935,130.721162934409));
#65882=CARTESIAN_POINT('Ctrl Pts',(81.1204723230433,10.232969165474,130.719800643321));
#65883=CARTESIAN_POINT('Ctrl Pts',(81.1283921959165,10.2257251939178,130.71909162793));
#65884=CARTESIAN_POINT('Ctrl Pts',(81.1491205565637,10.2063946542118,130.717227670653));
#65885=CARTESIAN_POINT('Ctrl Pts',(81.161808582558,10.1941804600788,130.716078219406));
#65886=CARTESIAN_POINT('Ctrl Pts',(81.225841915318,10.1305516696461,130.710227969528));
#65887=CARTESIAN_POINT('Ctrl Pts',(81.273980786006,10.0760159614782,130.705668397266));
#65888=CARTESIAN_POINT('Ctrl Pts',(81.3809295934146,9.9375755129988,130.694867246262));
#65889=CARTESIAN_POINT('Ctrl Pts',(81.4358624136164,9.85106525470375,130.688726261868));
#65890=CARTESIAN_POINT('Ctrl Pts',(81.5063776286733,9.71352513366368,130.679116690121));
#65891=CARTESIAN_POINT('Ctrl Pts',(81.5280322765162,9.66588878563137,130.675810654387));
#65892=CARTESIAN_POINT('Ctrl Pts',(81.5514981865764,9.60706769079477,130.671662921655));
#65893=CARTESIAN_POINT('Ctrl Pts',(81.5554855446139,9.59677676613751,130.670934886726));
#65894=CARTESIAN_POINT('Ctrl Pts',(81.5615901230528,9.58054462139988,130.669781670562));
#65895=CARTESIAN_POINT('Ctrl Pts',(81.5637764315996,9.57462947935327,130.669360420274));
#65896=CARTESIAN_POINT('Ctrl Pts',(81.5678090406744,9.56352563651781,130.668567514503));
#65897=CARTESIAN_POINT('Ctrl Pts',(81.5696632596676,9.55834002074372,130.668196326457));
#65898=CARTESIAN_POINT('Ctrl Pts',(81.573956625873,9.54614252324408,130.667321211606));
#65899=CARTESIAN_POINT('Ctrl Pts',(81.5763746487272,9.53912343430509,130.666816086222));
#65900=CARTESIAN_POINT('Ctrl Pts',(81.5842137849916,9.51586414568231,130.665137711104));
#65901=CARTESIAN_POINT('Ctrl Pts',(81.5894312608824,9.4995571473227,130.663953740887));
#65902=CARTESIAN_POINT('Ctrl Pts',(81.6015260909296,9.45964611434461,130.661043135637));
#65903=CARTESIAN_POINT('Ctrl Pts',(81.6081339217301,9.43596505755872,130.659305325025));
#65904=CARTESIAN_POINT('Ctrl Pts',(81.633546312065,9.33643507725013,130.65197913931));
#65905=CARTESIAN_POINT('Ctrl Pts',(81.647526082088,9.25945914963048,130.646264701835));
#65906=CARTESIAN_POINT('Ctrl Pts',(81.667423910441,9.07819559960313,130.633008930474));
#65907=CARTESIAN_POINT('Ctrl Pts',(81.669052001544,8.97374774645698,130.625533904966));
#65908=CARTESIAN_POINT('Ctrl Pts',(81.6590634216884,8.84631013655199,130.616734301889));
#65909=CARTESIAN_POINT('Ctrl Pts',(81.6567219299989,8.82284312982841,130.615126257091));
#65910=CARTESIAN_POINT('Ctrl Pts',(81.652423251002,8.78739612316469,130.612714875513));
#65911=CARTESIAN_POINT('Ctrl Pts',(81.6508321860757,8.77537561175177,130.611900211062));
#65912=CARTESIAN_POINT('Ctrl Pts',(81.6477290037477,8.75374877024306,130.610439705239));
#65913=CARTESIAN_POINT('Ctrl Pts',(81.64626375615,8.74413638396045,130.609792420744));
#65914=CARTESIAN_POINT('Ctrl Pts',(81.6429428411197,8.72356115916944,130.608410659103));
#65915=CARTESIAN_POINT('Ctrl Pts',(81.6410614052011,8.71260291173512,130.60767702883));
#65916=CARTESIAN_POINT('Ctrl Pts',(81.6355939092437,8.68256425262057,130.605671737902));
#65917=CARTESIAN_POINT('Ctrl Pts',(81.6317837493595,8.66352602462411,130.604407193925));
#65918=CARTESIAN_POINT('Ctrl Pts',(81.6028575915234,8.53106720762236,130.595644496151));
#65919=CARTESIAN_POINT('Ctrl Pts',(81.5662715114293,8.42047566357502,130.588540312815));
#65920=CARTESIAN_POINT('Ctrl Pts',(81.476932078692,8.22255435650235,130.575280547878));
#65921=CARTESIAN_POINT('Ctrl Pts',(81.4271189293108,8.13450814711946,130.569139348136));
#65922=CARTESIAN_POINT('Ctrl Pts',(81.3609018802561,8.03888691193086,130.561587454789));
#65923=CARTESIAN_POINT('Ctrl Pts',(81.3519763410698,8.02637161722389,130.560579999477));
#65924=CARTESIAN_POINT('Ctrl Pts',(81.3387142794975,8.00830972481361,130.5590951707));
#65925=CARTESIAN_POINT('Ctrl Pts',(81.3345134474343,8.00266385898142,130.558626550384));
#65926=CARTESIAN_POINT('Ctrl Pts',(81.3269786699658,7.99267004996689,130.557788688147));
#65927=CARTESIAN_POINT('Ctrl Pts',(81.3236588661302,7.98831169647088,130.55742041788));
#65928=CARTESIAN_POINT('Ctrl Pts',(81.3163678386827,7.97883710556991,130.556613457213));
#65929=CARTESIAN_POINT('Ctrl Pts',(81.3123883197203,7.97372769774461,130.556174214063));
#65930=CARTESIAN_POINT('Ctrl Pts',(81.3008643653609,7.95910843049711,130.554905995547));
#65931=CARTESIAN_POINT('Ctrl Pts',(81.2932458339906,7.9496578900392,130.554072120965));
#65932=CARTESIAN_POINT('Ctrl Pts',(81.2755804531359,7.92822813368963,130.552150459386));
#65933=CARTESIAN_POINT('Ctrl Pts',(81.2654669809685,7.91630552886297,130.551058802804));
#65934=CARTESIAN_POINT('Ctrl Pts',(81.2309127485646,7.87671343903414,130.547361946567));
#65935=CARTESIAN_POINT('Ctrl Pts',(81.2057215142613,7.84971560884039,130.544720794932));
#65936=CARTESIAN_POINT('Ctrl Pts',(81.1291445831258,7.77292812281802,130.53689579221));
#65937=CARTESIAN_POINT('Ctrl Pts',(81.0754238043893,7.72558386155537,130.531661241336));
#65938=CARTESIAN_POINT('Ctrl Pts',(80.9404379982862,7.62125128455429,130.519296313703));
#65939=CARTESIAN_POINT('Ctrl Pts',(80.8567899206597,7.56776786926971,130.512245523886));
#65940=CARTESIAN_POINT('Ctrl Pts',(80.7521330391565,7.51332322641634,130.504179360152));
#65941=CARTESIAN_POINT('Ctrl Pts',(80.7352487806133,7.50490093334936,130.502899285896));
#65942=CARTESIAN_POINT('Ctrl Pts',(80.7082977092897,7.49202407490775,130.500888553128));
#65943=CARTESIAN_POINT('Ctrl Pts',(80.6983240025823,7.48737954756951,130.500151375384));
#65944=CARTESIAN_POINT('Ctrl Pts',(80.680323587927,7.47921315545119,130.498833058953));
#65945=CARTESIAN_POINT('Ctrl Pts',(80.6723137912849,7.4756552286603,130.498250701579));
#65946=CARTESIAN_POINT('Ctrl Pts',(80.6534318567758,7.46744571459277,130.496887656463));
#65947=CARTESIAN_POINT('Ctrl Pts',(80.6425374378173,7.46284630494088,130.496108764508));
#65948=CARTESIAN_POINT('Ctrl Pts',(80.6104565959959,7.44970307275177,130.493836452397));
#65949=CARTESIAN_POINT('Ctrl Pts',(80.5891418046517,7.44147831774979,130.492353729362));
#65950=CARTESIAN_POINT('Ctrl Pts',(80.4898363110133,7.40548781878745,130.485559013421));
#65951=CARTESIAN_POINT('Ctrl Pts',(80.4100103511362,7.38311950339621,130.480423833744));
#65952=CARTESIAN_POINT('Ctrl Pts',(80.2727397187093,7.35548050643793,130.471839427105));
#65953=CARTESIAN_POINT('Ctrl Pts',(80.2160909649248,7.34708259823131,130.468362901742));
#65954=CARTESIAN_POINT('Ctrl Pts',(80.0825177367668,7.3342661686926,130.460127696746));
#65955=CARTESIAN_POINT('Ctrl Pts',(80.0055050252363,7.33223354426396,130.45535075556));
#65956=CARTESIAN_POINT('Ctrl Pts',(79.9170408600521,7.33602627915006,130.449559160304));
#65957=CARTESIAN_POINT('Ctrl Pts',(79.9054486979025,7.33664471765062,130.448794160939));
#65958=CARTESIAN_POINT('Ctrl Pts',(79.8874428068185,7.33779415159064,130.447595126332));
#65959=CARTESIAN_POINT('Ctrl Pts',(79.8810238300042,7.33824127150751,130.447165547032));
#65960=CARTESIAN_POINT('Ctrl Pts',(79.8691909442959,7.33913441248831,130.446369451352));
#65961=CARTESIAN_POINT('Ctrl Pts',(79.8637764292165,7.33956974114881,130.446003526252));
#65962=CARTESIAN_POINT('Ctrl Pts',(79.8512043989583,7.34064244217347,130.445150100061));
#65963=CARTESIAN_POINT('Ctrl Pts',(79.8440488146847,7.3412996477322,130.444661531375));
#65964=CARTESIAN_POINT('Ctrl Pts',(79.8212019341303,7.34354716388725,130.443093031704));
#65965=CARTESIAN_POINT('Ctrl Pts',(79.8055294121196,7.34531395969264,130.442004156747));
#65966=CARTESIAN_POINT('Ctrl Pts',(79.719130041258,7.35629830664496,130.435938445662));
#65967=CARTESIAN_POINT('Ctrl Pts',(79.6490324121429,7.36982732819119,130.430786673978));
#65968=CARTESIAN_POINT('Ctrl Pts',(79.4533815193548,7.4207941395087,130.416088888591));
#65969=CARTESIAN_POINT('Ctrl Pts',(79.3310418462584,7.46859885380323,130.406555418746));
#65970=CARTESIAN_POINT('Ctrl Pts',(79.1905787409609,7.54356794918062,130.395537323088));
#65971=CARTESIAN_POINT('Ctrl Pts',(79.1659515198911,7.55752975915162,130.393600151537));
#65972=CARTESIAN_POINT('Ctrl Pts',(79.130797679826,7.57866089291665,130.390825443182));
#65973=CARTESIAN_POINT('Ctrl Pts',(79.1199797385251,7.58533329520533,130.389970214342));
#65974=CARTESIAN_POINT('Ctrl Pts',(79.1009457236331,7.59737613094564,130.388462666514));
#65975=CARTESIAN_POINT('Ctrl Pts',(79.0926988775666,7.60269652894867,130.387808548181));
#65976=CARTESIAN_POINT('Ctrl Pts',(79.0769006243771,7.61308750712869,130.386553418377));
#65977=CARTESIAN_POINT('Ctrl Pts',(79.0693428079217,7.61814765023938,130.385952048806));
#65978=CARTESIAN_POINT('Ctrl Pts',(79.0487863392184,7.63215586080771,130.384313557993));
#65979=CARTESIAN_POINT('Ctrl Pts',(79.0358725624422,7.64122727076419,130.383281119173));
#65980=CARTESIAN_POINT('Ctrl Pts',(78.9827183725594,7.67970535188176,130.379015587948));
#65981=CARTESIAN_POINT('Ctrl Pts',(78.9436766476088,7.71072827803331,130.375844971515));
#65982=CARTESIAN_POINT('Ctrl Pts',(78.836253223589,7.80424876936312,130.366923470229));
#65983=CARTESIAN_POINT('Ctrl Pts',(78.7716131032048,7.8707550438073,130.361314970597));
#65984=CARTESIAN_POINT('Ctrl Pts',(78.6980357500565,7.96029419829377,130.354223638092));
#65985=CARTESIAN_POINT('Ctrl Pts',(78.6836203236812,7.97860704175427,130.352794267241));
#65986=CARTESIAN_POINT('Ctrl Pts',(78.6308044802056,8.04867847097712,130.347379744998));
#65987=CARTESIAN_POINT('Ctrl Pts',(78.5950381104905,8.10234242618471,130.343343423165));
#65988=CARTESIAN_POINT('Ctrl Pts',(78.5566899316897,8.16780833247951,130.338378968576));
#65989=CARTESIAN_POINT('Ctrl Pts',(78.5510086192705,8.17774037824937,130.337624719736));
#65990=CARTESIAN_POINT('Ctrl Pts',(78.5423110812292,8.19331546141852,130.336438998139));
#65991=CARTESIAN_POINT('Ctrl Pts',(78.5392241732181,8.19891891224169,130.336011825583));
#65992=CARTESIAN_POINT('Ctrl Pts',(78.5338113326874,8.20887978890448,130.335251183753));
#65993=CARTESIAN_POINT('Ctrl Pts',(78.5314723965651,8.21322997498409,130.334918542861));
#65994=CARTESIAN_POINT('Ctrl Pts',(78.5258857265647,8.22373232375973,130.334114423012));
#65995=CARTESIAN_POINT('Ctrl Pts',(78.522657180175,8.22989443277911,130.333641775742));
#65996=CARTESIAN_POINT('Ctrl Pts',(78.512800337365,8.24899762312796,130.332174345595));
#65997=CARTESIAN_POINT('Ctrl Pts',(78.50630299643,8.26200499166559,130.331172111793));
#65998=CARTESIAN_POINT('Ctrl Pts',(78.4739807616227,8.32888838532927,130.326009272974));
#65999=CARTESIAN_POINT('Ctrl Pts',(78.4508994752541,8.38403598699598,130.321722937486));
#66000=CARTESIAN_POINT('Ctrl Pts',(78.3894022111586,8.55644829478213,130.30845887476));
#66001=CARTESIAN_POINT('Ctrl Pts',(78.3609911265938,8.67685813804039,130.299415487429));
#66002=CARTESIAN_POINT('Ctrl Pts',(78.3409517216926,8.84199936052571,130.287727994914));
#66003=CARTESIAN_POINT('Ctrl Pts',(78.3374257995158,8.88487833286846,130.284752268311));
#66004=CARTESIAN_POINT('Ctrl Pts',(78.3349203898872,8.9426753329174,130.28081837542));
#66005=CARTESIAN_POINT('Ctrl Pts',(78.3344758100571,8.95750973122619,130.279815428835));
#66006=CARTESIAN_POINT('Ctrl Pts',(78.3341359416264,8.97798396044864,130.278440093409));
#66007=CARTESIAN_POINT('Ctrl Pts',(78.3340709916946,8.98361990179935,130.278062435538));
#66008=CARTESIAN_POINT('Ctrl Pts',(78.3340118553245,8.99278969776598,130.277449460922));
#66009=CARTESIAN_POINT('Ctrl Pts',(78.3340003093644,8.99632335331074,130.277213604314));
#66010=CARTESIAN_POINT('Ctrl Pts',(78.3340000061339,8.99985703818127,130.276978098673));
#66011=CARTESIAN_POINT('Ctrl Pts',(78.3340000061251,8.99985714018325,130.276978091875));
#66012=CARTESIAN_POINT('Ctrl Pts',(78.3339997153914,9.00324761329807,130.276752130718));
#66013=CARTESIAN_POINT('Ctrl Pts',(78.3340097745725,9.00663810598721,130.27652649315));
#66014=CARTESIAN_POINT('Ctrl Pts',(78.3340655951653,9.01591115401808,130.275910246183));
#66015=CARTESIAN_POINT('Ctrl Pts',(78.3341321637657,9.02179357117993,130.27552028939));
#66016=CARTESIAN_POINT('Ctrl Pts',(78.3344228076602,9.03928718690984,130.274363386318));
#66017=CARTESIAN_POINT('Ctrl Pts',(78.3347371366475,9.05089669954057,130.273599264679));
#66018=CARTESIAN_POINT('Ctrl Pts',(78.3360564312599,9.08603780792438,130.271296633948));
#66019=CARTESIAN_POINT('Ctrl Pts',(78.3374390364098,9.1095528901347,130.269769849068));
#66020=CARTESIAN_POINT('Ctrl Pts',(78.3485166095364,9.24783798778132,130.260858993039));
#66021=CARTESIAN_POINT('Ctrl Pts',(78.3695931772456,9.36138392066019,130.253845393381));
#66022=CARTESIAN_POINT('Ctrl Pts',(78.4125350010222,9.50679159710878,130.244585066166));
#66023=CARTESIAN_POINT('Ctrl Pts',(78.4239893636677,9.54135991886436,130.242359213294));
#66024=CARTESIAN_POINT('Ctrl Pts',(78.4365593450135,9.57550787860402,130.240113160697));
#66025=CARTESIAN_POINT('',(78.33440142911,9.00151625010545,130.471480117369));
#66026=CARTESIAN_POINT('Ctrl Pts',(78.4345148001033,9.5762760062711,130.432124665951));
#66027=CARTESIAN_POINT('Ctrl Pts',(78.4162821325133,9.5278000484821,130.435600394876));
#66028=CARTESIAN_POINT('Ctrl Pts',(78.356496074576,9.34162384460564,130.448718878682));
#66029=CARTESIAN_POINT('Ctrl Pts',(78.3331165140057,9.14577591746124,130.461837362488));
#66030=CARTESIAN_POINT('Ctrl Pts',(78.33440142911,9.00151625010545,130.471480117369));
#66031=CARTESIAN_POINT('Ctrl Pts',(78.3340007022066,9.00152962470499,130.471710596613));
#66032=CARTESIAN_POINT('Ctrl Pts',(78.3339349670933,8.92993385869101,130.476901080138));
#66033=CARTESIAN_POINT('Ctrl Pts',(78.3384844518672,8.85840001862447,130.482032138836));
#66034=CARTESIAN_POINT('Ctrl Pts',(78.3517694833915,8.75515916674562,130.489305905419));
#66035=CARTESIAN_POINT('Ctrl Pts',(78.3568560013911,8.72307235552932,130.491548616382));
#66036=CARTESIAN_POINT('Ctrl Pts',(78.3651832410862,8.67893172959673,130.494610001404));
#66037=CARTESIAN_POINT('Ctrl Pts',(78.367625596883,8.66673660252718,130.495453285581));
#66038=CARTESIAN_POINT('Ctrl Pts',(78.3721831580371,8.6452332982515,130.496936029329));
#66039=CARTESIAN_POINT('Ctrl Pts',(78.3742421993977,8.63591393324561,130.497577239465));
#66040=CARTESIAN_POINT('Ctrl Pts',(78.3785753698302,8.61707179535778,130.498870991796));
#66041=CARTESIAN_POINT('Ctrl Pts',(78.3808535852037,8.6075503398954,130.49952337475));
#66042=CARTESIAN_POINT('Ctrl Pts',(78.3858060350955,8.58762987610369,130.50088559758));
#66043=CARTESIAN_POINT('Ctrl Pts',(78.3884971431201,8.57723549488165,130.501594861914));
#66044=CARTESIAN_POINT('Ctrl Pts',(78.3958740677599,8.54983661170472,130.503460844982));
#66045=CARTESIAN_POINT('Ctrl Pts',(78.4007298354169,8.53287896428565,130.504612048516));
#66046=CARTESIAN_POINT('Ctrl Pts',(78.4248565060553,8.45341301743886,130.509993928854));
#66047=CARTESIAN_POINT('Ctrl Pts',(78.4475295088691,8.39199408089226,130.51411291791));
#66048=CARTESIAN_POINT('Ctrl Pts',(78.5128897814093,8.24264556511574,130.524212896189));
#66049=CARTESIAN_POINT('Ctrl Pts',(78.559802257106,8.15684370752952,130.530086677449));
#66050=CARTESIAN_POINT('Ctrl Pts',(78.6492501745467,8.02271929388212,130.540039760952));
#66051=CARTESIAN_POINT('Ctrl Pts',(78.6875434077936,7.97186653027002,130.544027023178));
#66052=CARTESIAN_POINT('Ctrl Pts',(78.7358147800287,7.91486644300933,130.548915602511));
#66053=CARTESIAN_POINT('Ctrl Pts',(78.7430694160422,7.90647149200695,130.549647003246));
#66054=CARTESIAN_POINT('Ctrl Pts',(78.7546703987577,7.89331497871181,130.550812618005));
#66055=CARTESIAN_POINT('Ctrl Pts',(78.7589616143101,7.88850493756123,130.551242940473));
#66056=CARTESIAN_POINT('Ctrl Pts',(78.7669530552219,7.87965127123934,130.552043047157));
#66057=CARTESIAN_POINT('Ctrl Pts',(78.7706454515475,7.87560085685648,130.552412259912));
#66058=CARTESIAN_POINT('Ctrl Pts',(78.7791495899779,7.86636411201824,130.553261493479));
#66059=CARTESIAN_POINT('Ctrl Pts',(78.7839744310211,7.86119015582598,130.553742476706));
#66060=CARTESIAN_POINT('Ctrl Pts',(78.7991481678409,7.84512485570245,130.555252109593));
#66061=CARTESIAN_POINT('Ctrl Pts',(78.8096112027599,7.83434302046208,130.556288740022));
#66062=CARTESIAN_POINT('Ctrl Pts',(78.8925199174556,7.75118856805887,130.564459220716));
#66063=CARTESIAN_POINT('Ctrl Pts',(78.9713472063525,7.68549929084553,130.571956412736));
#66064=CARTESIAN_POINT('Ctrl Pts',(79.1504630765912,7.56226757199929,130.587768204633));
#66065=CARTESIAN_POINT('Ctrl Pts',(79.2517428498069,7.50704720212146,130.596016806403));
#66066=CARTESIAN_POINT('Ctrl Pts',(79.3757981899376,7.45523355036414,130.605215866465));
#66067=CARTESIAN_POINT('Ctrl Pts',(79.3938033944958,7.44807957225725,130.606530994378));
#66068=CARTESIAN_POINT('Ctrl Pts',(79.4223223577848,7.43732027734014,130.608583623627));
#66069=CARTESIAN_POINT('Ctrl Pts',(79.4327539147653,7.43350350684733,130.609328115552));
#66070=CARTESIAN_POINT('Ctrl Pts',(79.4523853109874,7.42654245257867,130.610717676921));
#66071=CARTESIAN_POINT('Ctrl Pts',(79.4615759577565,7.42337383671914,130.611363528665));
#66072=CARTESIAN_POINT('Ctrl Pts',(79.4822977338793,7.41643201866503,130.612809471937));
#66073=CARTESIAN_POINT('Ctrl Pts',(79.4938434842861,7.41270393988582,130.613608052565));
#66074=CARTESIAN_POINT('Ctrl Pts',(79.5279895054301,7.40208878553154,130.615949876095));
#66075=CARTESIAN_POINT('Ctrl Pts',(79.5506973044518,7.39555575540211,130.617481626438));
#66076=CARTESIAN_POINT('Ctrl Pts',(79.6728438715802,7.36321101846698,130.625598729195));
#66077=CARTESIAN_POINT('Ctrl Pts',(79.7743737672135,7.34615435164159,130.631898403886));
#66078=CARTESIAN_POINT('Ctrl Pts',(79.9558735343654,7.33269985091961,130.643013764065));
#66079=CARTESIAN_POINT('Ctrl Pts',(80.0352208257703,7.33248847788776,130.647830824273));
#66080=CARTESIAN_POINT('Ctrl Pts',(80.1389827755485,7.33962259595009,130.654388862713));
#66081=CARTESIAN_POINT('Ctrl Pts',(80.163647825943,7.34187196059625,130.655967458107));
#66082=CARTESIAN_POINT('Ctrl Pts',(80.205355856979,7.3466152021734,130.658683995238));
#66083=CARTESIAN_POINT('Ctrl Pts',(80.2224275011186,7.34882518558433,130.659809395225));
#66084=CARTESIAN_POINT('Ctrl Pts',(80.2468224335836,7.35236836033992,130.661440867223));
#66085=CARTESIAN_POINT('Ctrl Pts',(80.2541764399192,7.353486815758,130.661935731058));
#66086=CARTESIAN_POINT('Ctrl Pts',(80.2669620914676,7.35551905513369,130.662801795851));
#66087=CARTESIAN_POINT('Ctrl Pts',(80.2723970889858,7.3564105861812,130.663171753714));
#66088=CARTESIAN_POINT('Ctrl Pts',(80.2840344827063,7.35837883827611,130.663967901826));
#66089=CARTESIAN_POINT('Ctrl Pts',(80.2902351244666,7.35946374766563,130.664394513261));
#66090=CARTESIAN_POINT('Ctrl Pts',(80.307244545841,7.36253928844591,130.665571122954));
#66091=CARTESIAN_POINT('Ctrl Pts',(80.3180397798927,7.36460173806758,130.666324919242));
#66092=CARTESIAN_POINT('Ctrl Pts',(80.3793244857265,7.37694001572888,130.670641404663));
#66093=CARTESIAN_POINT('Ctrl Pts',(80.4293316251349,7.38944604413835,130.674306765041));
#66094=CARTESIAN_POINT('Ctrl Pts',(80.5706408205097,7.43183416271274,130.684938125982));
#66095=CARTESIAN_POINT('Ctrl Pts',(80.6600520111634,7.46732017385028,130.691990508206));
#66096=CARTESIAN_POINT('Ctrl Pts',(80.7929207132847,7.5338497158724,130.702676501373));
#66097=CARTESIAN_POINT('Ctrl Pts',(80.8387928166537,7.55960164785768,130.706410243536));
#66098=CARTESIAN_POINT('Ctrl Pts',(80.9035796892431,7.60011868429707,130.711735689284));
#66099=CARTESIAN_POINT('Ctrl Pts',(80.9235128048892,7.61318777367779,130.713382003522));
#66100=CARTESIAN_POINT('Ctrl Pts',(80.9591520528946,7.63766387001872,130.716340436158));
#66101=CARTESIAN_POINT('Ctrl Pts',(80.9749520443428,7.64892599830254,130.717657544614));
#66102=CARTESIAN_POINT('Ctrl Pts',(80.9994880135385,7.66706968690371,130.719712546723));
#66103=CARTESIAN_POINT('Ctrl Pts',(81.0083575622236,7.67376678301002,130.720457457919));
#66104=CARTESIAN_POINT('Ctrl Pts',(81.0248581170491,7.6864870278332,130.721847399327));
#66105=CARTESIAN_POINT('Ctrl Pts',(81.0325046596709,7.69248915005022,130.722493215984));
#66106=CARTESIAN_POINT('Ctrl Pts',(81.0495689159257,7.70612671873863,130.723938561877));
#66107=CARTESIAN_POINT('Ctrl Pts',(81.0589567626536,7.71379878516604,130.724736585766));
#66108=CARTESIAN_POINT('Ctrl Pts',(81.0863570763557,7.73669462624715,130.727075129104));
#66109=CARTESIAN_POINT('Ctrl Pts',(81.1041314703856,7.75219955510301,130.728604205435));
#66110=CARTESIAN_POINT('Ctrl Pts',(81.1982313123699,7.83787026496663,130.736779573197));
#66111=CARTESIAN_POINT('Ctrl Pts',(81.2682127008343,7.91466884671018,130.743134056571));
#66112=CARTESIAN_POINT('Ctrl Pts',(81.3778889258898,8.06023834334087,130.754264965202));
#66113=CARTESIAN_POINT('Ctrl Pts',(81.4206687124359,8.12625601637327,130.759042643378));
#66114=CARTESIAN_POINT('Ctrl Pts',(81.47053989672,8.21662510655833,130.765551998821));
#66115=CARTESIAN_POINT('Ctrl Pts',(81.4819706529042,8.23847083629505,130.767123714949));
#66116=CARTESIAN_POINT('Ctrl Pts',(81.5005265475841,8.27593479675374,130.769829562372));
#66117=CARTESIAN_POINT('Ctrl Pts',(81.5079029221145,8.29142462652006,130.770951281153));
#66118=CARTESIAN_POINT('Ctrl Pts',(81.5181284550755,8.31378051531,130.772578348521));
#66119=CARTESIAN_POINT('Ctrl Pts',(81.5211731876138,8.32055661358258,130.773072571699));
#66120=CARTESIAN_POINT('Ctrl Pts',(81.5263957183504,8.33239050811154,130.773937914446));
#66121=CARTESIAN_POINT('Ctrl Pts',(81.5285939207964,8.33743909944149,130.774307797431));
#66122=CARTESIAN_POINT('Ctrl Pts',(81.5332536521584,8.3482876906121,130.775104254059));
#66123=CARTESIAN_POINT('Ctrl Pts',(81.5357072808463,8.35409068722947,130.775531253031));
#66124=CARTESIAN_POINT('Ctrl Pts',(81.5423600229295,8.37007707285946,130.776709949134));
#66125=CARTESIAN_POINT('Ctrl Pts',(81.5464910584003,8.38028819234525,130.777465465534));
#66126=CARTESIAN_POINT('Ctrl Pts',(81.5695499588197,8.43895200483574,130.781817991473));
#66127=CARTESIAN_POINT('Ctrl Pts',(81.5862997607267,8.48822477531962,130.785519633376));
#66128=CARTESIAN_POINT('Ctrl Pts',(81.6290810310146,8.63651378204172,130.796644393227));
#66129=CARTESIAN_POINT('Ctrl Pts',(81.6483290203995,8.73724451009196,130.804166432138));
#66130=CARTESIAN_POINT('Ctrl Pts',(81.6652515442867,8.91164979887429,130.816727648109));
#66131=CARTESIAN_POINT('Ctrl Pts',(81.6675231792014,8.98458737357917,130.821849624644));
#66132=CARTESIAN_POINT('Ctrl Pts',(81.6644015842552,9.07505902154765,130.828027487396));
#66133=CARTESIAN_POINT('Ctrl Pts',(81.6635146000215,9.0926590919079,130.829221347458));
#66134=CARTESIAN_POINT('Ctrl Pts',(81.6616382991473,9.12095189503007,130.831128384632));
#66135=CARTESIAN_POINT('Ctrl Pts',(81.6608245839014,9.13165450595382,130.831846982175));
#66136=CARTESIAN_POINT('Ctrl Pts',(81.6590709170206,9.15210375652171,130.833214899008));
#66137=CARTESIAN_POINT('Ctrl Pts',(81.6581483628256,9.16185139570663,130.833864733082));
#66138=CARTESIAN_POINT('Ctrl Pts',(81.6558459261604,9.18408723825744,130.835342323088));
#66139=CARTESIAN_POINT('Ctrl Pts',(81.6544105920383,9.19656919850586,130.8361683077));
#66140=CARTESIAN_POINT('Ctrl Pts',(81.650200954025,9.2298548502577,130.838362574281));
#66141=CARTESIAN_POINT('Ctrl Pts',(81.6471744681804,9.25062476983929,130.839722976738));
#66142=CARTESIAN_POINT('Ctrl Pts',(81.6240309562504,9.39083008971631,130.848858832549));
#66143=CARTESIAN_POINT('Ctrl Pts',(81.5913343822639,9.50782225275512,130.856213892762));
#66144=CARTESIAN_POINT('Ctrl Pts',(81.5216463352326,9.68155087194645,130.867652201914));
#66145=CARTESIAN_POINT('Ctrl Pts',(81.4934320765618,9.74133564189957,130.871699999128));
#66146=CARTESIAN_POINT('Ctrl Pts',(81.4509934796962,9.81894826582743,130.877298986023));
#66147=CARTESIAN_POINT('Ctrl Pts',(81.4398453905923,9.83839339888407,130.878732475706));
#66148=CARTESIAN_POINT('Ctrl Pts',(81.420083078219,9.87130672371198,130.881222352099));
#66149=CARTESIAN_POINT('Ctrl Pts',(81.4116608121343,9.88488703310924,130.882268778605));
#66150=CARTESIAN_POINT('Ctrl Pts',(81.3991505077208,9.9044257944107,130.883805490688));
#66151=CARTESIAN_POINT('Ctrl Pts',(81.3952166949713,9.91048258089235,130.884286278145));
#66152=CARTESIAN_POINT('Ctrl Pts',(81.3882540577914,9.92105168399021,130.885133398084));
#66153=CARTESIAN_POINT('Ctrl Pts',(81.3852423477297,9.92557504849522,130.885498603588));
#66154=CARTESIAN_POINT('Ctrl Pts',(81.3786316481288,9.93539928796301,130.886297688812));
#66155=CARTESIAN_POINT('Ctrl Pts',(81.3750242529463,9.94069407859132,130.886732101832));
#66156=CARTESIAN_POINT('Ctrl Pts',(81.3648628274479,9.95542527908854,130.887950933577));
#66157=CARTESIAN_POINT('Ctrl Pts',(81.3582417370053,9.96481468026115,130.888739590056));
#66158=CARTESIAN_POINT('Ctrl Pts',(81.3127340311825,10.0279525415454,130.894119235841));
#66159=CARTESIAN_POINT('Ctrl Pts',(81.2707679350355,10.0793998113737,130.898879573392));
#66160=CARTESIAN_POINT('Ctrl Pts',(81.2110402372178,10.1442971578128,130.90527418687));
#66161=CARTESIAN_POINT('Ctrl Pts',(81.1959124148381,10.1600982367291,130.906864971188));
#66162=CARTESIAN_POINT('Ctrl Pts',(81.1296875273683,10.2265981037423,130.913695526737));
#66163=CARTESIAN_POINT('Ctrl Pts',(81.075642173953,10.2742573957305,130.918935484296));
#66164=CARTESIAN_POINT('Ctrl Pts',(80.9657371687861,10.3591852475982,130.92885848432));
#66165=CARTESIAN_POINT('Ctrl Pts',(80.9103715097435,10.3968745834076,130.933546328581));
#66166=CARTESIAN_POINT('Ctrl Pts',(80.8380747238104,10.4399596765993,130.939286400286));
#66167=CARTESIAN_POINT('Ctrl Pts',(80.8231312263737,10.4485538084109,130.940453720669));
#66168=CARTESIAN_POINT('Ctrl Pts',(80.798742503525,10.4620806581149,130.942328835508));
#66169=CARTESIAN_POINT('Ctrl Pts',(80.7893789600739,10.4671572186624,130.943041727857));
#66170=CARTESIAN_POINT('Ctrl Pts',(80.7712939490611,10.4767389699349,130.944405468081));
#66171=CARTESIAN_POINT('Ctrl Pts',(80.7625801178148,10.4812575441587,130.945056767822));
#66172=CARTESIAN_POINT('Ctrl Pts',(80.742469640984,10.4914613708557,130.946546948994));
#66173=CARTESIAN_POINT('Ctrl Pts',(80.7310466278264,10.4970935279538,130.947383950616));
#66174=CARTESIAN_POINT('Ctrl Pts',(80.6938862915828,10.5148888088814,130.950077510568));
#66175=CARTESIAN_POINT('Ctrl Pts',(80.6679006936046,10.5265238636066,130.951915982009));
#66176=CARTESIAN_POINT('Ctrl Pts',(80.5209915438054,10.5878323688928,130.96208716754));
#66177=CARTESIAN_POINT('Ctrl Pts',(80.3948510712179,10.6238038232796,130.969946361092));
#66178=CARTESIAN_POINT('Ctrl Pts',(80.1954414673756,10.6560306964566,130.982340185736));
#66179=CARTESIAN_POINT('Ctrl Pts',(80.1244376110809,10.6628734135012,130.986758475592));
#66180=CARTESIAN_POINT('Ctrl Pts',(80.0374668105584,10.6656532495786,130.992404188399));
#66181=CARTESIAN_POINT('Ctrl Pts',(80.0217050097537,10.6659331793492,130.993436795096));
#66182=CARTESIAN_POINT('Ctrl Pts',(79.998759082803,10.6660150238512,130.994956867852));
#66183=CARTESIAN_POINT('Ctrl Pts',(79.9915759186875,10.66599418657,130.995435121023));
#66184=CARTESIAN_POINT('Ctrl Pts',(79.9789629057277,10.6658760254634,130.99627945692));
#66185=CARTESIAN_POINT('Ctrl Pts',(79.9735330617507,10.6657986047097,130.996644438308));
#66186=CARTESIAN_POINT('Ctrl Pts',(79.9616716766522,10.6655714706829,130.997445097487));
#66187=CARTESIAN_POINT('Ctrl Pts',(79.9552406934064,10.6654110559558,130.997881327482));
#66188=CARTESIAN_POINT('Ctrl Pts',(79.9372100686732,10.6648567901944,130.999110064727));
#66189=CARTESIAN_POINT('Ctrl Pts',(79.9256136436994,10.6643789708214,130.999906915947));
#66190=CARTESIAN_POINT('Ctrl Pts',(79.837221257765,10.6598112626147,131.006026370728));
#66191=CARTESIAN_POINT('Ctrl Pts',(79.7607942880031,10.6505297004094,131.01157572479));
#66192=CARTESIAN_POINT('Ctrl Pts',(79.629167615956,10.6252094503092,131.021318545275));
#66193=CARTESIAN_POINT('Ctrl Pts',(79.5736354253558,10.6115321672092,131.025489188911));
#66194=CARTESIAN_POINT('Ctrl Pts',(79.4395578060655,10.571092320798,131.035609598302));
#66195=CARTESIAN_POINT('Ctrl Pts',(79.3620877741717,10.5412651095284,131.041496315316));
#66196=CARTESIAN_POINT('Ctrl Pts',(79.2664931051318,10.4960100242077,131.048767716817));
#66197=CARTESIAN_POINT('Ctrl Pts',(79.2460384139042,10.485806304336,131.050324696564));
#66198=CARTESIAN_POINT('Ctrl Pts',(79.2153282749773,10.4696891249464,131.052665109169));
#66199=CARTESIAN_POINT('Ctrl Pts',(79.204915880094,10.4640823388088,131.053459145629));
#66200=CARTESIAN_POINT('Ctrl Pts',(79.1868936901026,10.4541289160625,131.054834683528));
#66201=CARTESIAN_POINT('Ctrl Pts',(79.1792569673692,10.4498322851782,131.055417931629));
#66202=CARTESIAN_POINT('Ctrl Pts',(79.1621138857072,10.4400082539625,131.056728266123));
#66203=CARTESIAN_POINT('Ctrl Pts',(79.1526275755255,10.4344465469314,131.057454087016));
#66204=CARTESIAN_POINT('Ctrl Pts',(79.1270319126599,10.4190975967963,131.059415011104));
#66205=CARTESIAN_POINT('Ctrl Pts',(79.1110321582611,10.4091300486523,131.060643524565));
#66206=CARTESIAN_POINT('Ctrl Pts',(79.0091998969472,10.3432655470614,131.068488248232));
#66207=CARTESIAN_POINT('Ctrl Pts',(78.9285037580023,10.279822976562,131.074805775984));
#66208=CARTESIAN_POINT('Ctrl Pts',(78.7941289886919,10.1525038020543,131.086122604903));
#66209=CARTESIAN_POINT('Ctrl Pts',(78.7384389752836,10.0912616765704,131.091130794565));
#66210=CARTESIAN_POINT('Ctrl Pts',(78.6702839415317,10.0040891244896,131.098074834778));
#66211=CARTESIAN_POINT('Ctrl Pts',(78.6536000200431,9.98160413731893,131.099851611055));
#66212=CARTESIAN_POINT('Ctrl Pts',(78.6266525871325,9.94330676374587,131.102873844687));
#66213=CARTESIAN_POINT('Ctrl Pts',(78.6160762759367,9.9277207661565,131.104102747688));
#66214=CARTESIAN_POINT('Ctrl Pts',(78.6015483033417,9.90550993825809,131.10585761507));
#66215=CARTESIAN_POINT('Ctrl Pts',(78.5973744996113,9.89903119859064,131.106369922964));
#66216=CARTESIAN_POINT('Ctrl Pts',(78.5902748140422,9.88784100875058,131.107255946476));
#66217=CARTESIAN_POINT('Ctrl Pts',(78.5873272494154,9.88314350795715,131.107628241312));
#66218=CARTESIAN_POINT('Ctrl Pts',(78.5811559362732,9.87319840227937,131.108417322133));
#66219=CARTESIAN_POINT('Ctrl Pts',(78.577937861096,9.86794769250251,131.108834425622));
#66220=CARTESIAN_POINT('Ctrl Pts',(78.5692311644274,9.85356317347049,131.109978181863));
#66221=CARTESIAN_POINT('Ctrl Pts',(78.5638010595987,9.84439454093521,131.110708392939));
#66222=CARTESIAN_POINT('Ctrl Pts',(78.5367501787327,9.79770378399011,131.114430501027));
#66223=CARTESIAN_POINT('Ctrl Pts',(78.5165121254638,9.75940396939928,131.117494858768));
#66224=CARTESIAN_POINT('Ctrl Pts',(78.4751022088955,9.6730498221801,131.124362681666));
#66225=CARTESIAN_POINT('Ctrl Pts',(78.4546709720977,9.62471040657779,131.128179664619));
#66226=CARTESIAN_POINT('Ctrl Pts',(78.4365594215428,9.57550808650568,131.131996250734));
#66227=CARTESIAN_POINT('Origin',(80.,9.,134.));
#66228=CARTESIAN_POINT('',(78.4365593737656,9.57550795671282,131.83373138687));
#66229=CARTESIAN_POINT('',(78.4365593658221,9.57550793513344,131.638964603241));
#66230=CARTESIAN_POINT('',(78.4365593737638,9.57550795670799,134.));
#66231=CARTESIAN_POINT('Ctrl Pts',(78.4365593658221,9.57550793513344,131.638964603241));
#66232=CARTESIAN_POINT('Ctrl Pts',(78.4410865932633,9.58780672531445,131.638013474793));
#66233=CARTESIAN_POINT('Ctrl Pts',(78.4457595240313,9.60005367347163,131.637063674998));
#66234=CARTESIAN_POINT('Ctrl Pts',(78.4814911855288,9.690480448225,131.630033607877));
#66235=CARTESIAN_POINT('Ctrl Pts',(78.518289588667,9.7662703727031,131.624055371267));
#66236=CARTESIAN_POINT('Ctrl Pts',(78.5722517890723,9.85884847048592,131.616686802588));
#66237=CARTESIAN_POINT('Ctrl Pts',(78.5842524715201,9.87848999795307,131.615118761154));
#66238=CARTESIAN_POINT('Ctrl Pts',(78.6030481180432,9.90786677153953,131.612765155056));
#66239=CARTESIAN_POINT('Ctrl Pts',(78.609546036157,9.91778778724255,131.611968807391));
#66240=CARTESIAN_POINT('Ctrl Pts',(78.6210313403621,9.93492155110456,131.610590584195));
#66241=CARTESIAN_POINT('Ctrl Pts',(78.6259706903703,9.9421657668927,131.610006942427));
#66242=CARTESIAN_POINT('Ctrl Pts',(78.6372227168631,9.9583916663193,131.608697393663));
#66243=CARTESIAN_POINT('Ctrl Pts',(78.6435674842272,9.96735068582696,131.607972738205));
#66244=CARTESIAN_POINT('Ctrl Pts',(78.6609899248764,9.99144325481061,131.606019109763));
#66245=CARTESIAN_POINT('Ctrl Pts',(78.6722355385141,10.00645381903,131.60479663852));
#66246=CARTESIAN_POINT('Ctrl Pts',(78.7392294105224,10.092798952227,131.597726433202));
#66247=CARTESIAN_POINT('Ctrl Pts',(78.8004673337255,10.1596881025449,131.592105785667));
#66248=CARTESIAN_POINT('Ctrl Pts',(78.9150004674912,10.2659570793858,131.582529114542));
#66249=CARTESIAN_POINT('Ctrl Pts',(78.9657554679509,10.3077497090344,131.578545029437));
#66250=CARTESIAN_POINT('Ctrl Pts',(79.0695694592559,10.3833995646239,131.570632669384));
#66251=CARTESIAN_POINT('Ctrl Pts',(79.122337536334,10.4174633074637,131.566715485063));
#66252=CARTESIAN_POINT('Ctrl Pts',(79.1898292327841,10.4558161491801,131.561670528063));
#66253=CARTESIAN_POINT('Ctrl Pts',(79.202861240022,10.4629925126462,131.560694814238));
#66254=CARTESIAN_POINT('Ctrl Pts',(79.2221815807616,10.4732969131412,131.559243350765));
#66255=CARTESIAN_POINT('Ctrl Pts',(79.2283968022564,10.4765614746314,131.558775682831));
#66256=CARTESIAN_POINT('Ctrl Pts',(79.2390254716282,10.4820587807989,131.557974341266));
#66257=CARTESIAN_POINT('Ctrl Pts',(79.2434285260009,10.4843113104594,131.557641907458));
#66258=CARTESIAN_POINT('Ctrl Pts',(79.2535096884958,10.4894121546568,131.556879631707));
#66259=CARTESIAN_POINT('Ctrl Pts',(79.2591939716037,10.492247558727,131.556449027186));
#66260=CARTESIAN_POINT('Ctrl Pts',(79.2749812824152,10.5000100690363,131.555251175446));
#66261=CARTESIAN_POINT('Ctrl Pts',(79.2851179514816,10.5048674318992,131.554479912925));
#66262=CARTESIAN_POINT('Ctrl Pts',(79.3465597866294,10.533548722851,131.54979550102));
#66263=CARTESIAN_POINT('Ctrl Pts',(79.3989970903866,10.5548472392851,131.545758910591));
#66264=CARTESIAN_POINT('Ctrl Pts',(79.5421910286139,10.6046818880271,131.534806034923));
#66265=CARTESIAN_POINT('Ctrl Pts',(79.6344878401091,10.628187736783,131.52782898108));
#66266=CARTESIAN_POINT('Ctrl Pts',(79.8022403726075,10.6559184430193,131.51562674881));
#66267=CARTESIAN_POINT('Ctrl Pts',(79.8769440943925,10.6631400600698,131.510353790725));
#66268=CARTESIAN_POINT('Ctrl Pts',(79.9696264712868,10.6658176024287,131.504024885058));
#66269=CARTESIAN_POINT('Ctrl Pts',(79.9873703067059,10.6660466286799,131.502822526215));
#66270=CARTESIAN_POINT('Ctrl Pts',(80.0158762798348,10.6659591079554,131.500905141759));
#66271=CARTESIAN_POINT('Ctrl Pts',(80.0266371715041,10.6658218020348,131.500184591987));
#66272=CARTESIAN_POINT('Ctrl Pts',(80.0471805556072,10.6653605546711,131.498814961023));
#66273=CARTESIAN_POINT('Ctrl Pts',(80.0569629593501,10.6650546567961,131.498165345811));
#66274=CARTESIAN_POINT('Ctrl Pts',(80.079249614272,10.6641611050317,131.496690961775));
#66275=CARTESIAN_POINT('Ctrl Pts',(80.091751173574,10.6635186867707,131.495867934007));
#66276=CARTESIAN_POINT('Ctrl Pts',(80.1250211097009,10.6614328401725,131.493687518938));
#66277=CARTESIAN_POINT('Ctrl Pts',(80.145772081453,10.6597409201807,131.492337847951));
#66278=CARTESIAN_POINT('Ctrl Pts',(80.289619965818,10.6452935990251,131.483041029028));
#66279=CARTESIAN_POINT('Ctrl Pts',(80.4109935310661,10.6192464106593,131.475536083806));
#66280=CARTESIAN_POINT('Ctrl Pts',(80.6158378379316,10.5507435306029,131.462332877392));
#66281=CARTESIAN_POINT('Ctrl Pts',(80.7007114433986,10.5142854378087,131.456671525805));
#66282=CARTESIAN_POINT('Ctrl Pts',(80.7928337453661,10.4653047061575,131.449853061736));
#66283=CARTESIAN_POINT('Ctrl Pts',(80.8034844174734,10.4594916921608,131.449053913532));
#66284=CARTESIAN_POINT('Ctrl Pts',(80.8197199042674,10.4503989825166,131.447817521257));
#66285=CARTESIAN_POINT('Ctrl Pts',(80.8253509327864,10.4472020467607,131.44738529673));
#66286=CARTESIAN_POINT('Ctrl Pts',(80.8357119944896,10.441239564817,131.446583434735));
#66287=CARTESIAN_POINT('Ctrl Pts',(80.8404471949042,10.4384834133275,131.446214388775));
#66288=CARTESIAN_POINT('Ctrl Pts',(80.8512345304339,10.4321331360761,131.445367786591));
#66289=CARTESIAN_POINT('Ctrl Pts',(80.8572775417827,10.4285239784817,131.444889292235));
#66290=CARTESIAN_POINT('Ctrl Pts',(80.8764515893997,10.4169068999556,131.443357978796));
#66291=CARTESIAN_POINT('Ctrl Pts',(80.8894942466889,10.4087556547604,131.442296654562));
#66292=CARTESIAN_POINT('Ctrl Pts',(81.0111068004752,10.3303896126583,131.432227243793));
#66293=CARTESIAN_POINT('Ctrl Pts',(81.1112635131095,10.2479441466168,131.422659533723));
#66294=CARTESIAN_POINT('Ctrl Pts',(81.2522453839789,10.1013310585399,131.407965590616));
#66295=CARTESIAN_POINT('Ctrl Pts',(81.2999980282605,10.0445363745583,131.402693473354));
#66296=CARTESIAN_POINT('Ctrl Pts',(81.3602967435253,9.96225066708802,131.395637288046));
#66297=CARTESIAN_POINT('Ctrl Pts',(81.3762126076897,9.9393468994684,131.393729399413));
#66298=CARTESIAN_POINT('Ctrl Pts',(81.3985706186698,9.90538356367474,131.390979111804));
#66299=CARTESIAN_POINT('Ctrl Pts',(81.4054715963334,9.89463332178909,131.390119716124));
#66300=CARTESIAN_POINT('Ctrl Pts',(81.4174433447792,9.87550343199851,131.388609610631));
#66301=CARTESIAN_POINT('Ctrl Pts',(81.4225650738873,9.86715656757827,131.387957043791));
#66302=CARTESIAN_POINT('Ctrl Pts',(81.4331488513412,9.84956206784787,131.386594447773));
#66303=CARTESIAN_POINT('Ctrl Pts',(81.4385956886187,9.84030577233851,131.385884994388));
#66304=CARTESIAN_POINT('Ctrl Pts',(81.4527525912494,9.81570653568241,131.384018526801));
#66305=CARTESIAN_POINT('Ctrl Pts',(81.4613092581451,9.80027653627426,131.382867030597));
#66306=CARTESIAN_POINT('Ctrl Pts',(81.5004425464562,9.72698726940665,131.377482922703));
#66307=CARTESIAN_POINT('Ctrl Pts',(81.5278398522601,9.6674917078628,131.373362107518));
#66308=CARTESIAN_POINT('Ctrl Pts',(81.6045948230536,9.47113254555161,131.360300791297));
#66309=CARTESIAN_POINT('Ctrl Pts',(81.6395640625237,9.32940782173374,131.351719711866));
#66310=CARTESIAN_POINT('Ctrl Pts',(81.657390348583,9.16983799396937,131.341412464653));
#66311=CARTESIAN_POINT('Ctrl Pts',(81.6588728865297,9.1546881458148,131.340427062463));
#66312=CARTESIAN_POINT('Ctrl Pts',(81.6611433363872,9.12767221402564,131.338654338946));
#66313=CARTESIAN_POINT('Ctrl Pts',(81.662012189372,9.11581381932494,131.33787091085));
#66314=CARTESIAN_POINT('Ctrl Pts',(81.663154841474,9.09753585942371,131.336653799124));
#66315=CARTESIAN_POINT('Ctrl Pts',(81.6635185732042,9.09112202662904,131.336224894794));
#66316=CARTESIAN_POINT('Ctrl Pts',(81.6641241218618,9.07922753699883,131.335425861555));
#66317=CARTESIAN_POINT('Ctrl Pts',(81.6643759744755,9.07374759619245,131.335056287257));
#66318=CARTESIAN_POINT('Ctrl Pts',(81.6648921256197,9.06116184899341,131.334204209956));
#66319=CARTESIAN_POINT('Ctrl Pts',(81.6651379998377,9.0540555138625,131.33372072167));
#66320=CARTESIAN_POINT('Ctrl Pts',(81.6657830013253,9.03117602980832,131.332156901905));
#66321=CARTESIAN_POINT('Ctrl Pts',(81.666003532449,9.01539925543115,131.331067568332));
#66322=CARTESIAN_POINT('Ctrl Pts',(81.6659806632938,8.91448203356335,131.324039125622));
#66323=CARTESIAN_POINT('Ctrl Pts',(81.659434788834,8.82947631811198,131.317850294563));
#66324=CARTESIAN_POINT('Ctrl Pts',(81.6350846663098,8.67204071762693,131.306254004232));
#66325=CARTESIAN_POINT('Ctrl Pts',(81.6188610592164,8.59956339385728,131.300860253684));
#66326=CARTESIAN_POINT('Ctrl Pts',(81.5862085306613,8.48893004154032,131.292645014825));
#66327=CARTESIAN_POINT('Ctrl Pts',(81.5730982939475,8.44989798560129,131.289749120723));
#66328=CARTESIAN_POINT('Ctrl Pts',(81.5481651176254,8.38387864501267,131.284859533391));
#66329=CARTESIAN_POINT('Ctrl Pts',(81.5370484041738,8.3566469486293,131.282845120287));
#66330=CARTESIAN_POINT('Ctrl Pts',(81.519970276162,8.31778569464955,131.279972299204));
#66331=CARTESIAN_POINT('Ctrl Pts',(81.5145845141784,8.30591083783706,131.27909468369));
#66332=CARTESIAN_POINT('Ctrl Pts',(81.5048949101959,8.28519658050985,131.277563830432));
#66333=CARTESIAN_POINT('Ctrl Pts',(81.5006512643181,8.27632990301453,131.276908565233));
#66334=CARTESIAN_POINT('Ctrl Pts',(81.4916601534637,8.25796309944716,131.275551006098));
#66335=CARTESIAN_POINT('Ctrl Pts',(81.48689981391,8.2484697428402,131.274849195456));
#66336=CARTESIAN_POINT('Ctrl Pts',(81.4742460726599,8.22382583373515,131.273026586034));
#66337=CARTESIAN_POINT('Ctrl Pts',(81.4662097188689,8.20874977745495,131.271910834853));
#66338=CARTESIAN_POINT('Ctrl Pts',(81.4304902716076,8.14415429852324,131.267123130825));
#66339=CARTESIAN_POINT('Ctrl Pts',(81.4005183103492,8.09594039852424,131.26353298698));
#66340=CARTESIAN_POINT('Ctrl Pts',(81.3075365922007,7.96212500363168,131.253384620198));
#66341=CARTESIAN_POINT('Ctrl Pts',(81.2387315878149,7.88090205860205,131.247004433365));
#66342=CARTESIAN_POINT('Ctrl Pts',(81.1198548023238,7.76506933558316,131.236763365018));
#66343=CARTESIAN_POINT('Ctrl Pts',(81.0748367092265,7.72569507313518,131.233023959831));
#66344=CARTESIAN_POINT('Ctrl Pts',(81.0163610927935,7.67985697310843,131.228192162456));
#66345=CARTESIAN_POINT('Ctrl Pts',(81.0047994363253,7.67103591472545,131.227237948238));
#66346=CARTESIAN_POINT('Ctrl Pts',(80.9875384424815,7.65822050042419,131.225812519137));
#66347=CARTESIAN_POINT('Ctrl Pts',(80.9819268073224,7.65410842130923,131.225348977124));
#66348=CARTESIAN_POINT('Ctrl Pts',(80.9722874839488,7.64713731523539,131.22455220226));
#66349=CARTESIAN_POINT('Ctrl Pts',(80.9682725777707,7.64426086234522,131.224220168922));
#66350=CARTESIAN_POINT('Ctrl Pts',(80.9590281959238,7.63769979773673,131.22345521242));
#66351=CARTESIAN_POINT('Ctrl Pts',(80.9537903636151,7.63402750375541,131.223021494924));
#66352=CARTESIAN_POINT('Ctrl Pts',(80.9391268672623,7.62387224441488,131.221806758452));
#66353=CARTESIAN_POINT('Ctrl Pts',(80.9296555938553,7.61745621000202,131.221021546651));
#66354=CARTESIAN_POINT('Ctrl Pts',(80.8664544895885,7.57558554433474,131.215781824065));
#66355=CARTESIAN_POINT('Ctrl Pts',(80.8107798027646,7.54317667659819,131.211167713057));
#66356=CARTESIAN_POINT('Ctrl Pts',(80.7325220715034,7.50349936437941,131.204810285286));
#66357=CARTESIAN_POINT('Ctrl Pts',(80.7114469254506,7.49336600819205,131.203110009697));
#66358=CARTESIAN_POINT('Ctrl Pts',(80.6267034638844,7.45479431941971,131.196333694296));
#66359=CARTESIAN_POINT('Ctrl Pts',(80.5614868708045,7.42991995744521,131.191256414685));
#66360=CARTESIAN_POINT('Ctrl Pts',(80.4508932414423,7.39551398482469,131.182969789702));
#66361=CARTESIAN_POINT('Ctrl Pts',(80.4063337447617,7.38365424340168,131.179713294615));
#66362=CARTESIAN_POINT('Ctrl Pts',(80.3301768179263,7.36673391331792,131.174293407551));
#66363=CARTESIAN_POINT('Ctrl Pts',(80.2988230980426,7.36070751875075,131.172102740033));
#66364=CARTESIAN_POINT('Ctrl Pts',(80.2540341395632,7.35342669137153,131.169028972613));
#66365=CARTESIAN_POINT('Ctrl Pts',(80.2407286640204,7.35142888127001,131.168122732515));
#66366=CARTESIAN_POINT('Ctrl Pts',(80.2175981583668,7.34824186287692,131.166558838441));
#66367=CARTESIAN_POINT('Ctrl Pts',(80.2077842011987,7.34697863441529,131.165898885599));
#66368=CARTESIAN_POINT('Ctrl Pts',(80.1875731393064,7.34455995685847,131.164546894072));
#66369=CARTESIAN_POINT('Ctrl Pts',(80.1771752210296,7.34341484718729,131.163855208107));
#66370=CARTESIAN_POINT('Ctrl Pts',(80.15051287771,7.34073246753245,131.162091065625));
#66371=CARTESIAN_POINT('Ctrl Pts',(80.1342351287995,7.33933632790771,131.161023053958));
#66372=CARTESIAN_POINT('Ctrl Pts',(80.0674390118767,7.33459582304453,131.156674269505));
#66373=CARTESIAN_POINT('Ctrl Pts',(80.0167987504378,7.33331537134916,131.153457538602));
#66374=CARTESIAN_POINT('Ctrl Pts',(79.8570709782273,7.33655903920439,131.143462544086));
#66375=CARTESIAN_POINT('Ctrl Pts',(79.7484513633614,7.34948855735244,131.136903845277));
#66376=CARTESIAN_POINT('Ctrl Pts',(79.5795838957457,7.38665735135284,131.126258808066));
#66377=CARTESIAN_POINT('Ctrl Pts',(79.5181378420725,7.40393255876608,131.122281318358));
#66378=CARTESIAN_POINT('Ctrl Pts',(79.4436679096794,7.42956208097032,131.117164059071));
#66379=CARTESIAN_POINT('Ctrl Pts',(79.4295624329273,7.43463052413377,131.116181209754));
#66380=CARTESIAN_POINT('Ctrl Pts',(79.40893402193,7.44235864504746,131.114721115307));
#66381=CARTESIAN_POINT('Ctrl Pts',(79.4023560535668,7.44487065171404,131.114252089801));
#66382=CARTESIAN_POINT('Ctrl Pts',(79.3911828978629,7.44921883480678,131.113449235571));
#66383=CARTESIAN_POINT('Ctrl Pts',(79.3865796490973,7.4510339066486,131.11311665993));
#66384=CARTESIAN_POINT('Ctrl Pts',(79.3760985413356,7.45522068182605,131.112355217867));
#66385=CARTESIAN_POINT('Ctrl Pts',(79.3702262192284,7.45760538328177,131.111925598969));
#66386=CARTESIAN_POINT('Ctrl Pts',(79.3540357507133,7.46428807193745,131.110733076775));
#66387=CARTESIAN_POINT('Ctrl Pts',(79.3437472558831,7.46865638856319,131.109966213512));
#66388=CARTESIAN_POINT('Ctrl Pts',(79.2833493555423,7.49502072132314,131.105414030899));
#66389=CARTESIAN_POINT('Ctrl Pts',(79.2343090593134,7.5193694249011,131.101513148835));
#66390=CARTESIAN_POINT('Ctrl Pts',(79.1002519005994,7.59437188738399,131.090425460632));
#66391=CARTESIAN_POINT('Ctrl Pts',(79.0184081695503,7.65025329293981,131.08316172444));
#66392=CARTESIAN_POINT('Ctrl Pts',(78.8854079538635,7.75959332249958,131.070816527248));
#66393=CARTESIAN_POINT('Ctrl Pts',(78.8319356076494,7.80980992791756,131.065666786494));
#66394=CARTESIAN_POINT('Ctrl Pts',(78.769898191039,7.87629321882591,131.059460923687));
#66395=CARTESIAN_POINT('Ctrl Pts',(78.7580646006197,7.88938580243971,131.058265299305));
#66396=CARTESIAN_POINT('Ctrl Pts',(78.7393665219918,7.91074585583485,131.056356013149));
#66397=CARTESIAN_POINT('Ctrl Pts',(78.7323703660262,7.91889571415527,131.055636910379));
#66398=CARTESIAN_POINT('Ctrl Pts',(78.7191471873315,7.93460431641017,131.054268382645));
#66399=CARTESIAN_POINT('Ctrl Pts',(78.7129070663044,7.94215139204652,131.053618439313));
#66400=CARTESIAN_POINT('Ctrl Pts',(78.6988169351788,7.95950187675413,131.05214107284));
#66401=CARTESIAN_POINT('Ctrl Pts',(78.6910104434207,7.96933998438703,131.051315416562));
#66402=CARTESIAN_POINT('Ctrl Pts',(78.6665041686598,8.00095156461892,131.048699444944));
#66403=CARTESIAN_POINT('Ctrl Pts',(78.650230180274,8.02305042062074,131.046925747146));
#66404=CARTESIAN_POINT('Ctrl Pts',(78.5589795075367,8.1535978424108,131.036737001547));
#66405=CARTESIAN_POINT('Ctrl Pts',(78.4965435930344,8.27023424013042,131.02880988654));
#66406=CARTESIAN_POINT('Ctrl Pts',(78.4224132107557,8.4597170679087,131.01632754284));
#66407=CARTESIAN_POINT('Ctrl Pts',(78.4006499718142,8.52802239663518,131.011888479251));
#66408=CARTESIAN_POINT('Ctrl Pts',(78.3795331560638,8.61283997819181,131.006217747639));
#66409=CARTESIAN_POINT('Ctrl Pts',(78.3759342300766,8.62822586798793,131.005182776081));
#66410=CARTESIAN_POINT('Ctrl Pts',(78.3710167301025,8.65068464263671,131.003659777954));
#66411=CARTESIAN_POINT('Ctrl Pts',(78.3695241538756,8.6577190876727,131.003181011982));
#66412=CARTESIAN_POINT('Ctrl Pts',(78.3669840173551,8.67008438263633,131.002336024379));
#66413=CARTESIAN_POINT('Ctrl Pts',(78.3659169208175,8.67541102419258,131.001970908544));
#66414=CARTESIAN_POINT('Ctrl Pts',(78.3636434814016,8.68705479300864,131.001170254383));
#66415=CARTESIAN_POINT('Ctrl Pts',(78.3624476751794,8.69337361737917,131.000734166319));
#66416=CARTESIAN_POINT('Ctrl Pts',(78.359198905829,8.7111018199006,130.999506517904));
#66417=CARTESIAN_POINT('Ctrl Pts',(78.3572284489884,8.72252567410388,130.998710626697));
#66418=CARTESIAN_POINT('Ctrl Pts',(78.3438152440272,8.80544698478327,130.992903234864));
#66419=CARTESIAN_POINT('Ctrl Pts',(78.3369264836571,8.8775952243093,130.987690507324));
#66420=CARTESIAN_POINT('Ctrl Pts',(78.3342650540324,8.96615169152368,130.981256628272));
#66421=CARTESIAN_POINT('Ctrl Pts',(78.3340146151872,8.98235602539027,130.980077712919));
#66422=CARTESIAN_POINT('Ctrl Pts',(78.3338894071065,9.12734903413172,130.969524624792));
#66423=CARTESIAN_POINT('Ctrl Pts',(78.3487122805385,9.25574058191219,130.960198832495));
#66424=CARTESIAN_POINT('Ctrl Pts',(78.3828536558729,9.40101071746689,130.949942245357));
#66425=CARTESIAN_POINT('Ctrl Pts',(78.3878837037746,9.42077666899251,130.948551968283));
#66426=CARTESIAN_POINT('Ctrl Pts',(78.3965884142704,9.45253100131099,130.946326188072));
#66427=CARTESIAN_POINT('Ctrl Pts',(78.4000375337431,9.46457845608474,130.945483543669));
#66428=CARTESIAN_POINT('Ctrl Pts',(78.4064150746454,9.48594073036294,130.943992266882));
#66429=CARTESIAN_POINT('Ctrl Pts',(78.4092900356052,9.49527075815947,130.943341932972));
#66430=CARTESIAN_POINT('Ctrl Pts',(78.4155376911458,9.51493033611623,130.94197343865));
#66431=CARTESIAN_POINT('Ctrl Pts',(78.4189297746091,9.52525328275073,130.941255947176));
#66432=CARTESIAN_POINT('Ctrl Pts',(78.4269651646265,9.54892357731872,130.939612821827));
#66433=CARTESIAN_POINT('Ctrl Pts',(78.4316777713226,9.56224646224829,130.938689512326));
#66434=CARTESIAN_POINT('Ctrl Pts',(78.4365593737218,9.57550795659375,130.937771496081));
#66435=CARTESIAN_POINT('Ctrl Pts',(78.4365594215428,9.57550808650568,131.131996250734));
#66436=CARTESIAN_POINT('Ctrl Pts',(78.4235762003059,9.5402375222916,131.134732161266));
#66437=CARTESIAN_POINT('Ctrl Pts',(78.4117850163223,9.50452355026856,131.13746812972));
#66438=CARTESIAN_POINT('Ctrl Pts',(78.3772966037958,9.38681082419089,131.146340195646));
#66439=CARTESIAN_POINT('Ctrl Pts',(78.359665808306,9.30347410969482,131.152387267124));
#66440=CARTESIAN_POINT('Ctrl Pts',(78.345433631865,9.19621682020707,131.159828461515));
#66441=CARTESIAN_POINT('Ctrl Pts',(78.3428690187422,9.17322791705642,131.161404432355));
#66442=CARTESIAN_POINT('Ctrl Pts',(78.3397128500697,9.13836077904294,131.163767262995));
#66443=CARTESIAN_POINT('Ctrl Pts',(78.3387684405541,9.12651815671475,131.164565037516));
#66444=CARTESIAN_POINT('Ctrl Pts',(78.3373473110502,9.10591934266505,131.165944699593));
#66445=CARTESIAN_POINT('Ctrl Pts',(78.3368129071141,9.09716774322538,131.166528367109));
#66446=CARTESIAN_POINT('Ctrl Pts',(78.3357660832314,9.07746965506702,131.167836665302));
#66447=CARTESIAN_POINT('Ctrl Pts',(78.3352925226641,9.06652143821342,131.168560056616));
#66448=CARTESIAN_POINT('Ctrl Pts',(78.3343042583983,9.03690909074114,131.170507019118));
#66449=CARTESIAN_POINT('Ctrl Pts',(78.3339952102391,9.01823930776351,131.171724165173));
#66450=CARTESIAN_POINT('Ctrl Pts',(78.3340253996539,8.90191346801314,131.179250673094));
#66451=CARTESIAN_POINT('Ctrl Pts',(78.3426363780776,8.80444502640658,131.185291027661));
#66452=CARTESIAN_POINT('Ctrl Pts',(78.3768930542379,8.61182820431648,131.197262526315));
#66453=CARTESIAN_POINT('Ctrl Pts',(78.4025198774541,8.51708428296653,131.203173278665));
#66454=CARTESIAN_POINT('Ctrl Pts',(78.447470718423,8.39481108078381,131.211423044028));
#66455=CARTESIAN_POINT('Ctrl Pts',(78.4595035481729,8.36480620504668,131.213500902847));
#66456=CARTESIAN_POINT('Ctrl Pts',(78.476276242608,8.32626693308885,131.216263602511));
#66457=CARTESIAN_POINT('Ctrl Pts',(78.4802297979179,8.31739553475856,131.21690615221));
#66458=CARTESIAN_POINT('Ctrl Pts',(78.4867307764065,8.3031444328207,131.217949838884));
#66459=CARTESIAN_POINT('Ctrl Pts',(78.4892299286579,8.297742772678,131.218348118143));
#66460=CARTESIAN_POINT('Ctrl Pts',(78.4941536302193,8.28724862517868,131.219127347401));
#66461=CARTESIAN_POINT('Ctrl Pts',(78.496575177531,8.28215488355518,131.219508118904));
#66462=CARTESIAN_POINT('Ctrl Pts',(78.5025998881814,8.26964606367031,131.220449298143));
#66463=CARTESIAN_POINT('Ctrl Pts',(78.5062322894477,8.26224530702715,131.221011452269));
#66464=CARTESIAN_POINT('Ctrl Pts',(78.5199557776886,8.23480156012626,131.223115061736));
#66465=CARTESIAN_POINT('Ctrl Pts',(78.5303960739844,8.21493711603471,131.224675669072));
#66466=CARTESIAN_POINT('Ctrl Pts',(78.61158165603,8.06776495263437,131.236492723373));
#66467=CARTESIAN_POINT('Ctrl Pts',(78.6983468654732,7.95001404882297,131.247327947995));
#66468=CARTESIAN_POINT('Ctrl Pts',(78.8443871142556,7.7981928418889,131.262368632087));
#66469=CARTESIAN_POINT('Ctrl Pts',(78.892159349527,7.7540174237506,131.266921998763));
#66470=CARTESIAN_POINT('Ctrl Pts',(78.956008819376,7.70155910718446,131.272561377032));
#66471=CARTESIAN_POINT('Ctrl Pts',(78.9697973217676,7.6905921870938,131.2737549367));
#66472=CARTESIAN_POINT('Ctrl Pts',(78.9922618757992,7.67329918552118,131.275661612631));
#66473=CARTESIAN_POINT('Ctrl Pts',(79.000829325183,7.66683491269287,131.276380145632));
#66474=CARTESIAN_POINT('Ctrl Pts',(79.0173313379767,7.6546323305015,131.277748013801));
#66475=CARTESIAN_POINT('Ctrl Pts',(79.0252551635601,7.64888032496345,131.278397863051));
#66476=CARTESIAN_POINT('Ctrl Pts',(79.0436370363312,7.63578257029402,131.27988973555));
#66477=CARTESIAN_POINT('Ctrl Pts',(79.0541299041157,7.62848656928552,131.280729833309));
#66478=CARTESIAN_POINT('Ctrl Pts',(79.0878176248686,7.60563301429186,131.28339170792));
#66479=CARTESIAN_POINT('Ctrl Pts',(79.111320906235,7.59053712703901,131.285196268376));
#66480=CARTESIAN_POINT('Ctrl Pts',(79.1999431372831,7.53671470207934,131.291825193935));
#66481=CARTESIAN_POINT('Ctrl Pts',(79.2673026571117,7.50185075437514,131.296516656739));
#66482=CARTESIAN_POINT('Ctrl Pts',(79.4164798422585,7.43711701002357,131.306483645639));
#66483=CARTESIAN_POINT('Ctrl Pts',(79.4987298045304,7.40882879141641,131.311728152343));
#66484=CARTESIAN_POINT('Ctrl Pts',(79.6291641476374,7.37509086591643,131.320132710838));
#66485=CARTESIAN_POINT('Ctrl Pts',(79.6760138195103,7.36510521604603,131.323169988916));
#66486=CARTESIAN_POINT('Ctrl Pts',(79.7338855472494,7.35535535540694,131.327015757329));
#66487=CARTESIAN_POINT('Ctrl Pts',(79.7445646255032,7.3536629557517,131.327729307688));
#66488=CARTESIAN_POINT('Ctrl Pts',(79.7614457653593,7.35115586044723,131.328864478885));
#66489=CARTESIAN_POINT('Ctrl Pts',(79.7676374575457,7.35027191178136,131.329282366114));
#66490=CARTESIAN_POINT('Ctrl Pts',(79.7793003961619,7.34867382718593,131.330072638895));
#66491=CARTESIAN_POINT('Ctrl Pts',(79.7847703925035,7.3479519811486,131.330444595255));
#66492=CARTESIAN_POINT('Ctrl Pts',(79.7976965519505,7.34631147027733,131.331326575419));
#66493=CARTESIAN_POINT('Ctrl Pts',(79.8051554558104,7.34541605332656,131.331837857318));
#66494=CARTESIAN_POINT('Ctrl Pts',(79.8301578871399,7.34258599749483,131.333558965552));
#66495=CARTESIAN_POINT('Ctrl Pts',(79.8477253783501,7.34087978233342,131.334780249793));
#66496=CARTESIAN_POINT('Ctrl Pts',(79.8908503356319,7.33738198775142,131.337802362622));
#66497=CARTESIAN_POINT('Ctrl Pts',(79.9164279372204,7.33590028203161,131.339615436418));
#66498=CARTESIAN_POINT('Ctrl Pts',(80.0265993838604,7.33206431430459,131.347487411208));
#66499=CARTESIAN_POINT('Ctrl Pts',(80.1112693931006,7.33556754715333,131.353688194992));
#66500=CARTESIAN_POINT('Ctrl Pts',(80.290401117718,7.35671286504456,131.366779069647));
#66501=CARTESIAN_POINT('Ctrl Pts',(80.3843658708892,7.37611773348157,131.373623880965));
#66502=CARTESIAN_POINT('Ctrl Pts',(80.4988595815248,7.41026528695757,131.381849781459));
#66503=CARTESIAN_POINT('Ctrl Pts',(80.5214178253391,7.41752065055162,131.383465679649));
#66504=CARTESIAN_POINT('Ctrl Pts',(80.5552953409186,7.42921974523854,131.385886249113));
#66505=CARTESIAN_POINT('Ctrl Pts',(80.5667325638681,7.43330994162865,131.386702380894));
#66506=CARTESIAN_POINT('Ctrl Pts',(80.5872424428761,7.44089870885088,131.388164313768));
#66507=CARTESIAN_POINT('Ctrl Pts',(80.596331038977,7.44435228229296,131.388811572854));
#66508=CARTESIAN_POINT('Ctrl Pts',(80.6157282354767,7.45191799262971,131.390191995608));
#66509=CARTESIAN_POINT('Ctrl Pts',(80.6260270718441,7.45605399160166,131.390924324673));
#66510=CARTESIAN_POINT('Ctrl Pts',(80.6541460536771,7.46767416035524,131.392922718365));
#66511=CARTESIAN_POINT('Ctrl Pts',(80.6718788542828,7.47536614428118,131.394181747104));
#66512=CARTESIAN_POINT('Ctrl Pts',(80.7934853518374,7.53064943951328,131.402816423442));
#66513=CARTESIAN_POINT('Ctrl Pts',(80.892360480221,7.58850884789987,131.40981223985));
#66514=CARTESIAN_POINT('Ctrl Pts',(81.0679966421746,7.71717470052997,131.423107252336));
#66515=CARTESIAN_POINT('Ctrl Pts',(81.1455616145988,7.7859405755097,131.429390685733));
#66516=CARTESIAN_POINT('Ctrl Pts',(81.2265571595683,7.87246221681966,131.437089803609));
#66517=CARTESIAN_POINT('Ctrl Pts',(81.2367238273314,7.88362279942544,131.438079620097));
#66518=CARTESIAN_POINT('Ctrl Pts',(81.2514203350729,7.90020320235381,131.439548061852));
#66519=CARTESIAN_POINT('Ctrl Pts',(81.2560699417644,7.9055164925745,131.440018331003));
#66520=CARTESIAN_POINT('Ctrl Pts',(81.2642617062196,7.91499849668367,131.440857372002));
#66521=CARTESIAN_POINT('Ctrl Pts',(81.2678173055301,7.9191553292739,131.441225150972));
#66522=CARTESIAN_POINT('Ctrl Pts',(81.2755814521041,7.92832337874343,131.442036264536));
#66523=CARTESIAN_POINT('Ctrl Pts',(81.2797809131637,7.93334183913899,131.442480200937));
#66524=CARTESIAN_POINT('Ctrl Pts',(81.2918958564495,7.9479940302786,131.443775856325));
#66525=CARTESIAN_POINT('Ctrl Pts',(81.2997326858398,7.95769179871589,131.444632797467));
#66526=CARTESIAN_POINT('Ctrl Pts',(81.3174909108477,7.98017860567078,131.446616705633));
#66527=CARTESIAN_POINT('Ctrl Pts',(81.3273361401949,7.99302596634875,131.447747888699));
#66528=CARTESIAN_POINT('Ctrl Pts',(81.3602184211425,8.03725532337097,131.451629052493));
#66529=CARTESIAN_POINT('Ctrl Pts',(81.3823410662821,8.06929905044129,131.454418594285));
#66530=CARTESIAN_POINT('Ctrl Pts',(81.4413234942914,8.16148070103518,131.462325693619));
#66531=CARTESIAN_POINT('Ctrl Pts',(81.4755180261119,8.22322805971814,131.467484899157));
#66532=CARTESIAN_POINT('Ctrl Pts',(81.5470987445032,8.3743813658722,131.479599038857));
#66533=CARTESIAN_POINT('Ctrl Pts',(81.5808131634194,8.46525825756831,131.486477450796));
#66534=CARTESIAN_POINT('Ctrl Pts',(81.6114269662395,8.57666605409916,131.494378719636));
#66535=CARTESIAN_POINT('Ctrl Pts',(81.6160955118886,8.59485330585436,131.495652894904));
#66536=CARTESIAN_POINT('Ctrl Pts',(81.6230301398396,8.62389887354653,131.497663692752));
#66537=CARTESIAN_POINT('Ctrl Pts',(81.6254968554871,8.63470713771841,131.498406684726));
#66538=CARTESIAN_POINT('Ctrl Pts',(81.6299046894759,8.65495005903992,131.499788719347));
#66539=CARTESIAN_POINT('Ctrl Pts',(81.6318722144995,8.66437842629522,131.500428580265));
#66540=CARTESIAN_POINT('Ctrl Pts',(81.6361303237541,8.68570650969085,131.501867636462));
#66541=CARTESIAN_POINT('Ctrl Pts',(81.6383730783219,8.69761530537912,131.50266528239));
#66542=CARTESIAN_POINT('Ctrl Pts',(81.6447301724061,8.73352042679518,131.505053403141));
#66543=CARTESIAN_POINT('Ctrl Pts',(81.6484487741186,8.7575841582587,131.506631405808));
#66544=CARTESIAN_POINT('Ctrl Pts',(81.655828207381,8.81342187993793,131.51024766948));
#66545=CARTESIAN_POINT('Ctrl Pts',(81.6591043222183,8.84523733393254,131.512274375918));
#66546=CARTESIAN_POINT('Ctrl Pts',(81.6677853875625,8.96262269049376,131.519659214281));
#66547=CARTESIAN_POINT('Ctrl Pts',(81.6674999585984,9.04847849197426,131.524872500957));
#66548=CARTESIAN_POINT('Ctrl Pts',(81.6533278410382,9.22419335818003,131.535642664903));
#66549=CARTESIAN_POINT('Ctrl Pts',(81.6387024059977,9.31369703704057,131.541186384887));
#66550=CARTESIAN_POINT('Ctrl Pts',(81.6130939379413,9.41681048747162,131.548080407421));
#66551=CARTESIAN_POINT('Ctrl Pts',(81.6090900740642,9.43200940358648,131.549110011833));
#66552=CARTESIAN_POINT('Ctrl Pts',(81.6029667213484,9.45398687269942,131.550621421989));
#66553=CARTESIAN_POINT('Ctrl Pts',(81.6010178352607,9.4608126267098,131.551094025884));
#66554=CARTESIAN_POINT('Ctrl Pts',(81.5974863252881,9.47288847268219,131.551936147182));
#66555=CARTESIAN_POINT('Ctrl Pts',(81.5959213167361,9.47814351044607,131.552304652405));
#66556=CARTESIAN_POINT('Ctrl Pts',(81.5924649087459,9.48954351131489,131.553108601247));
#66557=CARTESIAN_POINT('Ctrl Pts',(81.5905639020135,9.49568518757177,131.553544564653));
#66558=CARTESIAN_POINT('Ctrl Pts',(81.5850372752455,9.51318115885471,131.554794324178));
#66559=CARTESIAN_POINT('Ctrl Pts',(81.5813253758679,9.52450748422618,131.555612809863));
#66560=CARTESIAN_POINT('Ctrl Pts',(81.5468873364763,9.62590072140347,131.563018922027));
#66561=CARTESIAN_POINT('Ctrl Pts',(81.5086211631642,9.7132114143114,131.569948916389));
#66562=CARTESIAN_POINT('Ctrl Pts',(81.4053325592501,9.9028818180346,131.585670156419));
#66563=CARTESIAN_POINT('Ctrl Pts',(81.3361640812508,10.00241250003,131.594394165559));
#66564=CARTESIAN_POINT('Ctrl Pts',(81.2430374545382,10.1094390286121,131.604153492306));
#66565=CARTESIAN_POINT('Ctrl Pts',(81.2289526489535,10.1250211233254,131.605586164094));
#66566=CARTESIAN_POINT('Ctrl Pts',(81.2059740737672,10.1494957515072,131.607856493799));
#66567=CARTESIAN_POINT('Ctrl Pts',(81.1972681514024,10.1585607183027,131.608701962165));
#66568=CARTESIAN_POINT('Ctrl Pts',(81.1815984830226,10.1745113438437,131.610198217245));
#66569=CARTESIAN_POINT('Ctrl Pts',(81.1746751269483,10.1814356626849,131.610850715529));
#66570=CARTESIAN_POINT('Ctrl Pts',(81.1600370231907,10.1958199100198,131.612212683915));
#66571=CARTESIAN_POINT('Ctrl Pts',(81.1523104119806,10.2032671673007,131.6129215828));
#66572=CARTESIAN_POINT('Ctrl Pts',(81.131714897616,10.2227377198584,131.614785471104));
#66573=CARTESIAN_POINT('Ctrl Pts',(81.1187261602245,10.2346327219037,131.615934968153));
#66574=CARTESIAN_POINT('Ctrl Pts',(81.0511480862688,10.2945780019843,131.621789276029));
#66575=CARTESIAN_POINT('Ctrl Pts',(80.9936403080464,10.3392256561434,131.626352594241));
#66576=CARTESIAN_POINT('Ctrl Pts',(80.8485778984843,10.4373433972192,131.637165141609));
#66577=CARTESIAN_POINT('Ctrl Pts',(80.7586595416916,10.4867665338019,131.643313510126));
#66578=CARTESIAN_POINT('Ctrl Pts',(80.6169705487816,10.5484255305124,131.652921882488));
#66579=CARTESIAN_POINT('Ctrl Pts',(80.5682186142069,10.566971835703,131.656217855357));
#66580=CARTESIAN_POINT('Ctrl Pts',(80.5082087672168,10.5866320739973,131.660353885233));
#66581=CARTESIAN_POINT('Ctrl Pts',(80.4977008951034,10.5899595253757,131.661080997133));
#66582=CARTESIAN_POINT('Ctrl Pts',(80.4811345117288,10.5950251714944,131.662232998727));
#66583=CARTESIAN_POINT('Ctrl Pts',(80.4750976102733,10.5968337338346,131.662653969603));
#66584=CARTESIAN_POINT('Ctrl Pts',(80.4637671335971,10.6001582313595,131.663446527335));
#66585=CARTESIAN_POINT('Ctrl Pts',(80.4584761280154,10.6016822269449,131.663817648866));
#66586=CARTESIAN_POINT('Ctrl Pts',(80.4460317459932,10.6051999337018,131.664692836212));
#66587=CARTESIAN_POINT('Ctrl Pts',(80.4388724950879,10.6071720733584,131.665198102675));
#66588=CARTESIAN_POINT('Ctrl Pts',(80.4151459553601,10.6135376083416,131.666877918186));
#66589=CARTESIAN_POINT('Ctrl Pts',(80.3985246743736,10.6177230308913,131.668063214499));
#66590=CARTESIAN_POINT('Ctrl Pts',(80.3578759335465,10.6272944002076,131.670977878784));
#66591=CARTESIAN_POINT('Ctrl Pts',(80.3337883352276,10.632405423534,131.672718462475));
#66592=CARTESIAN_POINT('Ctrl Pts',(80.2325830586402,10.6515461023721,131.680064701137));
#66593=CARTESIAN_POINT('Ctrl Pts',(80.1546396322059,10.6606580387945,131.685797011849));
#66594=CARTESIAN_POINT('Ctrl Pts',(79.9725432637179,10.6690117288328,131.69904745732));
#66595=CARTESIAN_POINT('Ctrl Pts',(79.8685057633726,10.6640522683722,131.706499814795));
#66596=CARTESIAN_POINT('Ctrl Pts',(79.7422480369526,10.6461093451544,131.715278623998));
#66597=CARTESIAN_POINT('Ctrl Pts',(79.7189739821184,10.642296114171,131.716886726127));
#66598=CARTESIAN_POINT('Ctrl Pts',(79.6838685515317,10.6357762293792,131.719298042399));
#66599=CARTESIAN_POINT('Ctrl Pts',(79.6719736992034,10.6334324977711,131.720112586589));
#66600=CARTESIAN_POINT('Ctrl Pts',(79.6505892027233,10.628975930472,131.721572800149));
#66601=CARTESIAN_POINT('Ctrl Pts',(79.6410905644552,10.6269094969481,131.722219912869));
#66602=CARTESIAN_POINT('Ctrl Pts',(79.6207717061567,10.6223025048802,131.723601221309));
#66603=CARTESIAN_POINT('Ctrl Pts',(79.609957679577,10.6197365571404,131.724334571447));
#66604=CARTESIAN_POINT('Ctrl Pts',(79.5803374208064,10.612394422509,131.726338856894));
#66605=CARTESIAN_POINT('Ctrl Pts',(79.5615873069736,10.6073975288431,131.727602684996));
#66606=CARTESIAN_POINT('Ctrl Pts',(79.5200082929675,10.5955350318481,131.730397250035));
#66607=CARTESIAN_POINT('Ctrl Pts',(79.4972306424051,10.5885046851489,131.731922683992));
#66608=CARTESIAN_POINT('Ctrl Pts',(79.4247113591903,10.5644052901091,131.736771743078));
#66609=CARTESIAN_POINT('Ctrl Pts',(79.3756226218998,10.545469005002,131.740041452459));
#66610=CARTESIAN_POINT('Ctrl Pts',(79.2414178545118,10.4862582188833,131.749071251283));
#66611=CARTESIAN_POINT('Ctrl Pts',(79.1587034679735,10.4410514571943,131.754736443701));
#66612=CARTESIAN_POINT('Ctrl Pts',(79.0358843578375,10.3597309657736,131.763888191661));
#66613=CARTESIAN_POINT('Ctrl Pts',(78.9929556689949,10.3282498900722,131.767248903843));
#66614=CARTESIAN_POINT('Ctrl Pts',(78.9429732560593,10.2877787074443,131.771460298706));
#66615=CARTESIAN_POINT('Ctrl Pts',(78.9344056817388,10.2806983521752,131.77219338812));
#66616=CARTESIAN_POINT('Ctrl Pts',(78.9210764556528,10.2694565629013,131.773352805125));
#66617=CARTESIAN_POINT('Ctrl Pts',(78.9162663805771,10.2653526854059,131.77377513105));
#66618=CARTESIAN_POINT('Ctrl Pts',(78.9077330343718,10.2579878266643,131.77453164724));
#66619=CARTESIAN_POINT('Ctrl Pts',(78.904000769313,10.2547374945224,131.774865061432));
#66620=CARTESIAN_POINT('Ctrl Pts',(78.9002486109599,10.2514403239504,131.775202801851));
#66621=CARTESIAN_POINT('Ctrl Pts',(78.9002141507659,10.2514100398866,131.77520590391));
#66622=CARTESIAN_POINT('Ctrl Pts',(78.9001468073939,10.2513508527311,131.77521196649));
#66623=CARTESIAN_POINT('Ctrl Pts',(78.9001139241717,10.2513219498258,131.775214926997));
#66624=CARTESIAN_POINT('Ctrl Pts',(78.9000496414552,10.2512654436549,131.775220714815));
#66625=CARTESIAN_POINT('Ctrl Pts',(78.9000182418703,10.2512378405123,131.775223542118));
#66626=CARTESIAN_POINT('Ctrl Pts',(78.8999568403929,10.2511838588304,131.775229071223));
#66627=CARTESIAN_POINT('Ctrl Pts',(78.899926838313,10.2511574803085,131.775231773027));
#66628=CARTESIAN_POINT('Ctrl Pts',(78.8998681519487,10.2511058781583,131.775237058285));
#66629=CARTESIAN_POINT('Ctrl Pts',(78.8998394675703,10.2510806546114,131.775239641733));
#66630=CARTESIAN_POINT('Ctrl Pts',(78.8997608113842,10.2510114836653,131.775246726285));
#66631=CARTESIAN_POINT('Ctrl Pts',(78.8997108412508,10.2509675341781,131.775251227545));
#66632=CARTESIAN_POINT('Ctrl Pts',(78.8996112950469,10.2508799712089,131.775260195478));
#66633=CARTESIAN_POINT('Ctrl Pts',(78.8995617190306,10.250836357857,131.775264662139));
#66634=CARTESIAN_POINT('Ctrl Pts',(78.8994629441931,10.2507494525646,131.775273562371));
#66635=CARTESIAN_POINT('Ctrl Pts',(78.899413745256,10.2507061606002,131.775277995947));
#66636=CARTESIAN_POINT('Ctrl Pts',(78.8993157076356,10.2506198834079,131.775286831516));
#66637=CARTESIAN_POINT('Ctrl Pts',(78.8992668690136,10.250576898308,131.775291233497));
#66638=CARTESIAN_POINT('Ctrl Pts',(78.8991695359932,10.2504912209563,131.775300007303));
#66639=CARTESIAN_POINT('Ctrl Pts',(78.8991210415293,10.2504485287171,131.775304379128));
#66640=CARTESIAN_POINT('Ctrl Pts',(78.8990243810791,10.2503634234336,131.775313094022));
#66641=CARTESIAN_POINT('Ctrl Pts',(78.8989762150178,10.2503210103899,131.775317437092));
#66642=CARTESIAN_POINT('Ctrl Pts',(78.8988801961044,10.2502364502506,131.775326095836));
#66643=CARTESIAN_POINT('Ctrl Pts',(78.8988323431614,10.2501943031381,131.775330411514));
#66644=CARTESIAN_POINT('Ctrl Pts',(78.8987369353573,10.2501102617251,131.77533901682));
#66645=CARTESIAN_POINT('Ctrl Pts',(78.898689380537,10.2500683675202,131.775343306441));
#66646=CARTESIAN_POINT('Ctrl Pts',(78.8985945544824,10.2499848193294,131.775351860926));
#66647=CARTESIAN_POINT('Ctrl Pts',(78.8985472832385,10.2499431653913,131.775356125787));
#66648=CARTESIAN_POINT('Ctrl Pts',(78.8984530101794,10.2498600854266,131.775364632016));
#66649=CARTESIAN_POINT('Ctrl Pts',(78.8984060083371,10.2498186594292,131.775368873381));
#66650=CARTESIAN_POINT('Ctrl Pts',(78.898312260135,10.2497360232124,131.775377333865));
#66651=CARTESIAN_POINT('Ctrl Pts',(78.8982655138022,10.2496948130667,131.775381552976));
#66652=CARTESIAN_POINT('Ctrl Pts',(78.8981722631248,10.2496125968062,131.775389970154));
#66653=CARTESIAN_POINT('Ctrl Pts',(78.8981257587633,10.2495715907235,131.775394168219));
#66654=CARTESIAN_POINT('Ctrl Pts',(78.8980329788979,10.2494897711508,131.775402544478));
#66655=CARTESIAN_POINT('Ctrl Pts',(78.8979867033324,10.2494489576509,131.775406722675));
#66656=CARTESIAN_POINT('Ctrl Pts',(78.8926578890969,10.2447485955114,131.775887903631));
#66657=CARTESIAN_POINT('Ctrl Pts',(78.8874050709824,10.2400556987704,131.776367328106));
#66658=CARTESIAN_POINT('Ctrl Pts',(78.8700641490564,10.22436435013,131.777966616281));
#66659=CARTESIAN_POINT('Ctrl Pts',(78.8581085679564,10.2132217426786,131.779096272608));
#66660=CARTESIAN_POINT('Ctrl Pts',(78.8292729705187,10.1855431385927,131.781883749071));
#66661=CARTESIAN_POINT('Ctrl Pts',(78.8125774324182,10.168820705091,131.783552145622));
#66662=CARTESIAN_POINT('Ctrl Pts',(78.7460516622809,10.0992910289822,131.790406928328));
#66663=CARTESIAN_POINT('Ctrl Pts',(78.6993444134696,10.0436097549103,131.795706010284));
#66664=CARTESIAN_POINT('Ctrl Pts',(78.5903691088932,9.89497245956752,131.809116088394));
#66665=CARTESIAN_POINT('Ctrl Pts',(78.5335362523315,9.79845297575904,131.817152867725));
#66666=CARTESIAN_POINT('Ctrl Pts',(78.4769926821523,9.67568706995518,131.826455327091));
#66667=CARTESIAN_POINT('Ctrl Pts',(78.4676459179303,9.65421355116837,131.828051949695));
#66668=CARTESIAN_POINT('Ctrl Pts',(78.4541646053471,9.62136549156057,131.830449632312));
#66669=CARTESIAN_POINT('Ctrl Pts',(78.4496964371472,9.61013196755477,131.83126183149));
#66670=CARTESIAN_POINT('Ctrl Pts',(78.4423621792914,9.59109182805984,131.832625701042));
#66671=CARTESIAN_POINT('Ctrl Pts',(78.4394316094756,9.583310750653,131.833179510178));
#66672=CARTESIAN_POINT('Ctrl Pts',(78.4365593737656,9.57550795671282,131.83373138687));
#66673=CARTESIAN_POINT('Origin',(80.,9.,134.));
#66674=CARTESIAN_POINT('',(78.4365593745624,9.57550795887745,132.531716954706));
#66675=CARTESIAN_POINT('',(78.4365593734337,9.57550795581125,132.340765796073));
#66676=CARTESIAN_POINT('',(78.4365593737638,9.57550795670799,134.));
#66677=CARTESIAN_POINT('',(78.3340003204331,9.00103328753322,131.67971837006));
#66678=CARTESIAN_POINT('Ctrl Pts',(78.4365593734337,9.57550795581125,132.340765796073));
#66679=CARTESIAN_POINT('Ctrl Pts',(78.4390138527709,9.58217586139625,132.340304604494));
#66680=CARTESIAN_POINT('Ctrl Pts',(78.4415110860817,9.58882832869225,132.339841377572));
#66681=CARTESIAN_POINT('Ctrl Pts',(78.4479889033644,9.60575485622253,132.338654312622));
#66682=CARTESIAN_POINT('Ctrl Pts',(78.4520287230219,9.61600511328503,132.337927491696));
#66683=CARTESIAN_POINT('Ctrl Pts',(78.4585385959357,9.63205415596764,132.336775781979));
#66684=CARTESIAN_POINT('Ctrl Pts',(78.4609404859263,9.63788049441641,132.336354807383));
#66685=CARTESIAN_POINT('Ctrl Pts',(78.4655035584109,9.64877346727423,132.33556211255));
#66686=CARTESIAN_POINT('Ctrl Pts',(78.4676568817167,9.65384318105349,132.335190856561));
#66687=CARTESIAN_POINT('Ctrl Pts',(78.4727743996705,9.66572756575533,132.33431516263));
#66688=CARTESIAN_POINT('Ctrl Pts',(78.4757590914988,9.6725331766438,132.333809521163));
#66689=CARTESIAN_POINT('Ctrl Pts',(78.485788061143,9.69499124181602,132.332127626535));
#66690=CARTESIAN_POINT('Ctrl Pts',(78.4930284404067,9.71055420855854,132.330940593191));
#66691=CARTESIAN_POINT('Ctrl Pts',(78.5112573689462,9.74820444751152,132.328020888363));
#66692=CARTESIAN_POINT('Ctrl Pts',(78.5224983779539,9.7701644913867,132.326276955941));
#66693=CARTESIAN_POINT('Ctrl Pts',(78.5716048551329,9.86106272255202,132.318907798201));
#66694=CARTESIAN_POINT('Ctrl Pts',(78.6138391705723,9.92752304124814,132.313155275592));
#66695=CARTESIAN_POINT('Ctrl Pts',(78.7221886185351,10.074000497477,132.299912297943));
#66696=CARTESIAN_POINT('Ctrl Pts',(78.791406265167,10.1513412954622,132.292486963747));
#66697=CARTESIAN_POINT('Ctrl Pts',(78.8846665958901,10.2377979294419,132.283732607803));
#66698=CARTESIAN_POINT('Ctrl Pts',(78.9023029743275,10.2534646604678,132.282124112159));
#66699=CARTESIAN_POINT('Ctrl Pts',(78.929501555907,10.2766111866273,132.279712197102));
#66700=CARTESIAN_POINT('Ctrl Pts',(78.9388219389407,10.2843691746692,132.278897442431));
#66701=CARTESIAN_POINT('Ctrl Pts',(78.9557669456565,10.2981632668954,132.277436841167));
#66702=CARTESIAN_POINT('Ctrl Pts',(78.9633612055754,10.3042356213783,132.276789550596));
#66703=CARTESIAN_POINT('Ctrl Pts',(78.9797514805819,10.3171076450253,132.275407846758));
#66704=CARTESIAN_POINT('Ctrl Pts',(78.988563311556,10.323886485052,132.274674279711));
#66705=CARTESIAN_POINT('Ctrl Pts',(79.0129439059284,10.3422566746645,132.272669345638));
#66706=CARTESIAN_POINT('Ctrl Pts',(79.0286487147295,10.3536651894777,132.271405091017));
#66707=CARTESIAN_POINT('Ctrl Pts',(79.0640824399794,10.378471191151,132.268609540911));
#66708=CARTESIAN_POINT('Ctrl Pts',(79.0839070112697,10.3917249099864,132.267083552912));
#66709=CARTESIAN_POINT('Ctrl Pts',(79.1483620682851,10.4328420827666,132.262232387711));
#66710=CARTESIAN_POINT('Ctrl Pts',(79.1940314019558,10.4590198230951,132.258961176229));
#66711=CARTESIAN_POINT('Ctrl Pts',(79.326296364182,10.5267253240894,132.249814538132));
#66712=CARTESIAN_POINT('Ctrl Pts',(79.4153417702033,10.5629907794155,132.24403963887));
#66713=CARTESIAN_POINT('Ctrl Pts',(79.5562149503113,10.6066313642942,132.234865176505));
#66714=CARTESIAN_POINT('Ctrl Pts',(79.606095684983,10.6195825953491,132.231607110909));
#66715=CARTESIAN_POINT('Ctrl Pts',(79.6672460723956,10.6324679611317,132.22751368908));
#66716=CARTESIAN_POINT('Ctrl Pts',(79.678023533096,10.6346277739441,132.22678854052));
#66717=CARTESIAN_POINT('Ctrl Pts',(79.6950066511224,10.6378567396888,132.225638905835));
#66718=CARTESIAN_POINT('Ctrl Pts',(79.7011985728069,10.6389976651727,132.225218310871));
#66719=CARTESIAN_POINT('Ctrl Pts',(79.7128206281102,10.6410711026307,132.224425902874));
#66720=CARTESIAN_POINT('Ctrl Pts',(79.7182491008089,10.6420118095776,132.224054549673));
#66721=CARTESIAN_POINT('Ctrl Pts',(79.7310207883624,10.6441598353183,132.22317804452));
#66722=CARTESIAN_POINT('Ctrl Pts',(79.7383675299625,10.6453448956663,132.222671682156));
#66723=CARTESIAN_POINT('Ctrl Pts',(79.7627451334605,10.6491097096597,132.220984874354));
#66724=CARTESIAN_POINT('Ctrl Pts',(79.7798074146923,10.6514744544618,132.219793565263));
#66725=CARTESIAN_POINT('Ctrl Pts',(79.8215033733309,10.6565956930603,132.216861147464));
#66726=CARTESIAN_POINT('Ctrl Pts',(79.8461673992109,10.6590677308374,132.215108658155));
#66727=CARTESIAN_POINT('Ctrl Pts',(79.9500013399327,10.6671397031637,132.207679049791));
#66728=CARTESIAN_POINT('Ctrl Pts',(80.0294620111311,10.6676287937855,132.201872894601));
#66729=CARTESIAN_POINT('Ctrl Pts',(80.2110512464068,10.6557607959364,132.188647894191));
#66730=CARTESIAN_POINT('Ctrl Pts',(80.31262824295,10.6396208285482,132.181292363647));
#66731=CARTESIAN_POINT('Ctrl Pts',(80.4349492535965,10.6083941848069,132.172601673988));
#66732=CARTESIAN_POINT('Ctrl Pts',(80.4576850996068,10.6020727684417,132.170992601716));
#66733=CARTESIAN_POINT('Ctrl Pts',(80.4918928920256,10.5917739992773,132.168580002099));
#66734=CARTESIAN_POINT('Ctrl Pts',(80.5034674828791,10.5881509969698,132.167765129868));
#66735=CARTESIAN_POINT('Ctrl Pts',(80.5242487849829,10.5813961405454,132.166304401418));
#66736=CARTESIAN_POINT('Ctrl Pts',(80.5334694928912,10.5783094908542,132.165657100138));
#66737=CARTESIAN_POINT('Ctrl Pts',(80.5531725091705,10.5715214725207,132.164275462519));
#66738=CARTESIAN_POINT('Ctrl Pts',(80.563645905216,10.5677955437813,132.163541971584));
#66739=CARTESIAN_POINT('Ctrl Pts',(80.5922965609809,10.5572788059536,132.161537476843));
#66740=CARTESIAN_POINT('Ctrl Pts',(80.6103940656554,10.5502746954223,132.16027358011));
#66741=CARTESIAN_POINT('Ctrl Pts',(80.6504398833067,10.5339661147666,132.157478940686));
#66742=CARTESIAN_POINT('Ctrl Pts',(80.6723193690304,10.5245034713234,132.155953500046));
#66743=CARTESIAN_POINT('Ctrl Pts',(80.7417880472896,10.4926724087618,132.151104742971));
#66744=CARTESIAN_POINT('Ctrl Pts',(80.7885256086428,10.4685191231564,132.147835328958));
#66745=CARTESIAN_POINT('Ctrl Pts',(80.9171323419402,10.3941436674144,132.138689894579));
#66746=CARTESIAN_POINT('Ctrl Pts',(80.9959075317428,10.3390052677834,132.132914549906));
#66747=CARTESIAN_POINT('Ctrl Pts',(81.1090204913883,10.2443018063335,132.123737490756));
#66748=CARTESIAN_POINT('Ctrl Pts',(81.1469850496162,10.2093955559901,132.120477113869));
#66749=CARTESIAN_POINT('Ctrl Pts',(81.191005572531,10.1649817966471,132.116381097494));
#66750=CARTESIAN_POINT('Ctrl Pts',(81.1986668823445,10.1570974676378,132.11565583174));
#66751=CARTESIAN_POINT('Ctrl Pts',(81.21059251829,10.1445791376865,132.114506051638));
#66752=CARTESIAN_POINT('Ctrl Pts',(81.2149097154227,10.1399956262496,132.114085430065));
#66753=CARTESIAN_POINT('Ctrl Pts',(81.2229554854038,10.1313559277382,132.113293002017));
#66754=CARTESIAN_POINT('Ctrl Pts',(81.2266900463082,10.1273055846822,132.112921655684));
#66755=CARTESIAN_POINT('Ctrl Pts',(81.2354212509468,10.1177413395842,132.112045207636));
#66756=CARTESIAN_POINT('Ctrl Pts',(81.2404011139916,10.1122124080508,132.111538895995));
#66757=CARTESIAN_POINT('Ctrl Pts',(81.2567827326659,10.09377772971,132.109852434224));
#66758=CARTESIAN_POINT('Ctrl Pts',(81.2680209863795,10.0807290499715,132.108661426332));
#66759=CARTESIAN_POINT('Ctrl Pts',(81.2949308813777,10.0484864983784,132.105729904596));
#66760=CARTESIAN_POINT('Ctrl Pts',(81.3103801893936,10.0291129931921,132.103978018607));
#66761=CARTESIAN_POINT('Ctrl Pts',(81.3734456722168,9.94630524212548,132.096552687401));
#66762=CARTESIAN_POINT('Ctrl Pts',(81.41693141149,9.87985859548995,132.090750329207));
#66763=CARTESIAN_POINT('Ctrl Pts',(81.5054772720264,9.72085934380122,132.077524055374));
#66764=CARTESIAN_POINT('Ctrl Pts',(81.5470432090717,9.62670867912194,132.070163587505));
#66765=CARTESIAN_POINT('Ctrl Pts',(81.5871737825231,9.50694384516692,132.061468394675));
#66766=CARTESIAN_POINT('Ctrl Pts',(81.5941942172462,9.48441467218927,132.059859364991));
#66767=CARTESIAN_POINT('Ctrl Pts',(81.6040952861907,9.45009042620961,132.057446815933));
#66768=CARTESIAN_POINT('Ctrl Pts',(81.6073292721404,9.43840130400958,132.056631952383));
#66769=CARTESIAN_POINT('Ctrl Pts',(81.6129256186727,9.41727867226319,132.055171233327));
#66770=CARTESIAN_POINT('Ctrl Pts',(81.6153335460166,9.4078579209575,132.054523932838));
#66771=CARTESIAN_POINT('Ctrl Pts',(81.6203172453292,9.38762299975282,132.053142290333));
#66772=CARTESIAN_POINT('Ctrl Pts',(81.6228675478002,9.37680299603075,132.05240879378));
#66773=CARTESIAN_POINT('Ctrl Pts',(81.6295717328665,9.34702806679832,132.050404266611));
#66774=CARTESIAN_POINT('Ctrl Pts',(81.6335031438414,9.32802445305044,132.049140343462));
#66775=CARTESIAN_POINT('Ctrl Pts',(81.6415219697934,9.28553412545088,132.046345636821));
#66776=CARTESIAN_POINT('Ctrl Pts',(81.6454391542386,9.26201944358941,132.044820155781));
#66777=CARTESIAN_POINT('Ctrl Pts',(81.6563754912358,9.18638909082043,132.039971220987));
#66778=CARTESIAN_POINT('Ctrl Pts',(81.6614330282506,9.13402080964627,132.036701674323));
#66779=CARTESIAN_POINT('Ctrl Pts',(81.6687006183625,8.98563262243248,132.027556155132));
#66780=CARTESIAN_POINT('Ctrl Pts',(81.6651025899473,8.88954566138587,132.021780847144));
#66781=CARTESIAN_POINT('Ctrl Pts',(81.6468889545434,8.74315389156069,132.012603980365));
#66782=CARTESIAN_POINT('Ctrl Pts',(81.6381546073884,8.69232888696934,132.009343770407));
#66783=CARTESIAN_POINT('Ctrl Pts',(81.6247175973539,8.63125945939537,132.00524794143));
#66784=CARTESIAN_POINT('Ctrl Pts',(81.6222490815676,8.62054676320443,132.004522684149));
#66785=CARTESIAN_POINT('Ctrl Pts',(81.6182002831897,8.60373810317127,132.003372914561));
#66786=CARTESIAN_POINT('Ctrl Pts',(81.6166910924922,8.59762510567916,132.002952294911));
#66787=CARTESIAN_POINT('Ctrl Pts',(81.6137964673571,8.58617960837191,132.002159868313));
#66788=CARTESIAN_POINT('Ctrl Pts',(81.6124191900852,8.58084524756849,132.001788521483));
#66789=CARTESIAN_POINT('Ctrl Pts',(81.6091195679808,8.56832235842835,132.000912069307));
#66790=CARTESIAN_POINT('Ctrl Pts',(81.6071754942407,8.56113977656776,132.000405753999));
#66791=CARTESIAN_POINT('Ctrl Pts',(81.6005728762602,8.53737808358832,131.998719267217));
#66792=CARTESIAN_POINT('Ctrl Pts',(81.5957055606148,8.52085881433693,131.997528237554));
#66793=CARTESIAN_POINT('Ctrl Pts',(81.5832126218306,8.48076233898569,131.994596651056));
#66794=CARTESIAN_POINT('Ctrl Pts',(81.5753154773496,8.45727449844457,131.992844721464));
#66795=CARTESIAN_POINT('Ctrl Pts',(81.5399497935568,8.35937386944984,131.985419081214));
#66796=CARTESIAN_POINT('Ctrl Pts',(81.5077097119981,8.28679752008612,131.979616448682));
#66797=CARTESIAN_POINT('Ctrl Pts',(81.4221538810516,8.12617085872966,131.966390266842));
#66798=CARTESIAN_POINT('Ctrl Pts',(81.3656016229424,8.04018872417165,131.959030155715));
#66799=CARTESIAN_POINT('Ctrl Pts',(81.2867522254879,7.94151930090832,131.950335288274));
#66800=CARTESIAN_POINT('Ctrl Pts',(81.2716324412234,7.92340178644546,131.948726255539));
#66801=CARTESIAN_POINT('Ctrl Pts',(81.2481656183724,7.89646673440405,131.946313702858));
#66802=CARTESIAN_POINT('Ctrl Pts',(81.240099244862,7.88740979891581,131.945498838686));
#66803=CARTESIAN_POINT('Ctrl Pts',(81.2253887654404,7.87125161561904,131.944038118956));
#66804=CARTESIAN_POINT('Ctrl Pts',(81.2187800927997,7.86411900536034,131.94339081841));
#66805=CARTESIAN_POINT('Ctrl Pts',(81.2044831308971,7.84895701527119,131.942009176253));
#66806=CARTESIAN_POINT('Ctrl Pts',(81.1967761263927,7.84094586896147,131.941275680102));
#66807=CARTESIAN_POINT('Ctrl Pts',(81.1753974676037,7.81916415039868,131.939271155252));
#66808=CARTESIAN_POINT('Ctrl Pts',(81.1615642451314,7.80555407572372,131.938007233993));
#66809=CARTESIAN_POINT('Ctrl Pts',(81.1302160269946,7.77577132682943,131.935212532161));
#66810=CARTESIAN_POINT('Ctrl Pts',(81.1125852054254,7.75972649888601,131.933687054013));
#66811=CARTESIAN_POINT('Ctrl Pts',(81.0549774627006,7.70951823043555,131.928838131937));
#66812=CARTESIAN_POINT('Ctrl Pts',(81.0137243817552,7.67686578690892,131.925568594767));
#66813=CARTESIAN_POINT('Ctrl Pts',(80.8930004882725,7.5902772216071,131.916423081668));
#66814=CARTESIAN_POINT('Ctrl Pts',(80.8103231358185,7.54118430901875,131.910647771076));
#66815=CARTESIAN_POINT('Ctrl Pts',(80.6774556564384,7.47708601493515,131.901470890533));
#66816=CARTESIAN_POINT('Ctrl Pts',(80.6300183734611,7.45685745929915,131.898210668606));
#66817=CARTESIAN_POINT('Ctrl Pts',(80.5714237646628,7.43502340630212,131.894114826193));
#66818=CARTESIAN_POINT('Ctrl Pts',(80.5610847910996,7.43128692905135,131.893389568305));
#66819=CARTESIAN_POINT('Ctrl Pts',(80.5447672804534,7.42557176804789,131.892239797962));
#66820=CARTESIAN_POINT('Ctrl Pts',(80.5388129917335,7.42352411877329,131.891819178175));
#66821=CARTESIAN_POINT('Ctrl Pts',(80.5276272616244,7.41974817596469,131.891026751472));
#66822=CARTESIAN_POINT('Ctrl Pts',(80.522398681053,7.41801201993512,131.890655404678));
#66823=CARTESIAN_POINT('Ctrl Pts',(80.5100881416732,7.41399197418184,131.889778952799));
#66824=CARTESIAN_POINT('Ctrl Pts',(80.5029993933729,7.41172956483827,131.889272637754));
#66825=CARTESIAN_POINT('Ctrl Pts',(80.4794553039468,7.4043887752591,131.887586152767));
#66826=CARTESIAN_POINT('Ctrl Pts',(80.462937004629,7.39951824722721,131.886395124666));
#66827=CARTESIAN_POINT('Ctrl Pts',(80.4224747686478,7.38826645432181,131.883463542814));
#66828=CARTESIAN_POINT('Ctrl Pts',(80.3984586434108,7.38216177243315,131.881711616348));
#66829=CARTESIAN_POINT('Ctrl Pts',(80.2970277363352,7.35877433359403,131.874285998263));
#66830=CARTESIAN_POINT('Ctrl Pts',(80.2185678234387,7.34649632054733,131.868483385404));
#66831=CARTESIAN_POINT('Ctrl Pts',(80.0372161823935,7.3312537473824,131.855257196962));
#66832=CARTESIAN_POINT('Ctrl Pts',(79.9343065701634,7.33213012454231,131.847897060247));
#66833=CARTESIAN_POINT('Ctrl Pts',(79.8086444248078,7.34485779346857,131.839202169469));
#66834=CARTESIAN_POINT('Ctrl Pts',(79.7852226313434,7.34773384082206,131.837593136954));
#66835=CARTESIAN_POINT('Ctrl Pts',(79.7498656640781,7.35284005235047,131.835180584534));
#66836=CARTESIAN_POINT('Ctrl Pts',(79.7378815914028,7.35470457591523,131.834365720408));
#66837=CARTESIAN_POINT('Ctrl Pts',(79.7163278933248,7.3582994555634,131.832905000728));
#66838=CARTESIAN_POINT('Ctrl Pts',(79.7067511376011,7.35998303262163,131.832257700187));
#66839=CARTESIAN_POINT('Ctrl Pts',(79.6862586570776,7.36377081829597,131.830876058008));
#66840=CARTESIAN_POINT('Ctrl Pts',(79.6753481000852,7.36590063971851,131.830142561829));
#66841=CARTESIAN_POINT('Ctrl Pts',(79.6454531915931,7.37204758322549,131.828138036817));
#66842=CARTESIAN_POINT('Ctrl Pts',(79.626516048026,7.37628749487896,131.826874115426));
#66843=CARTESIAN_POINT('Ctrl Pts',(79.5844919138071,7.38647059451865,131.824079413257));
#66844=CARTESIAN_POINT('Ctrl Pts',(79.5614495093685,7.39258043304805,131.822553934905));
#66845=CARTESIAN_POINT('Ctrl Pts',(79.4880225626582,7.41374663145598,131.817705011935));
#66846=CARTESIAN_POINT('Ctrl Pts',(79.4382152952725,7.43069467128549,131.814435474097));
#66847=CARTESIAN_POINT('Ctrl Pts',(79.3010761743782,7.48472736583335,131.805361753301));
#66848=CARTESIAN_POINT('Ctrl Pts',(79.2159943864409,7.52694888187069,131.799654645729));
#66849=CARTESIAN_POINT('Ctrl Pts',(79.0900528403074,7.60346348141398,131.790494747482));
#66850=CARTESIAN_POINT('Ctrl Pts',(79.0464580256391,7.63285896594573,131.78717364008));
#66851=CARTESIAN_POINT('Ctrl Pts',(78.9954457554362,7.67088392042171,131.783006955854));
#66852=CARTESIAN_POINT('Ctrl Pts',(78.9866281861097,7.67759448963587,131.782276059823));
#66853=CARTESIAN_POINT('Ctrl Pts',(78.9728906244354,7.68826747139531,131.781119294417));
#66854=CARTESIAN_POINT('Ctrl Pts',(78.9679249266102,7.69217090735795,131.78069739561));
#66855=CARTESIAN_POINT('Ctrl Pts',(78.9588177569431,7.6994140391134,131.779916408637));
#66856=CARTESIAN_POINT('Ctrl Pts',(78.9546699320347,7.70274545643338,131.779557897802));
#66857=CARTESIAN_POINT('Ctrl Pts',(78.9504874664583,7.70613777928122,131.77919356162));
#66858=CARTESIAN_POINT('Ctrl Pts',(78.9504367514988,7.70617891821937,131.779189143399));
#66859=CARTESIAN_POINT('Ctrl Pts',(78.9503356591736,7.70626093210177,131.779180335527));
#66860=CARTESIAN_POINT('Ctrl Pts',(78.9502852816959,7.7063018070723,131.779175945872));
#66861=CARTESIAN_POINT('Ctrl Pts',(78.9501848475955,7.70638330640876,131.779167193691));
#66862=CARTESIAN_POINT('Ctrl Pts',(78.9501347909267,7.70642393075108,131.779162831165));
#66863=CARTESIAN_POINT('Ctrl Pts',(78.9500349822592,7.70650494178493,131.779154131848));
#66864=CARTESIAN_POINT('Ctrl Pts',(78.9499852302099,7.70654532845987,131.779149795057));
#66865=CARTESIAN_POINT('Ctrl Pts',(78.9498860149407,7.70662587684671,131.779141145843));
#66866=CARTESIAN_POINT('Ctrl Pts',(78.949836551719,7.70666603850583,131.779136833424));
#66867=CARTESIAN_POINT('Ctrl Pts',(78.9497378986349,7.70674614926079,131.779128231619));
#66868=CARTESIAN_POINT('Ctrl Pts',(78.9496887088085,7.70678609827639,131.77912394224));
#66869=CARTESIAN_POINT('Ctrl Pts',(78.9495905875734,7.70686579572739,131.779115385226));
#66870=CARTESIAN_POINT('Ctrl Pts',(78.9495416561191,7.70690554415188,131.77911111759));
#66871=CARTESIAN_POINT('Ctrl Pts',(78.9494440371514,7.70698485203819,131.779102602812));
#66872=CARTESIAN_POINT('Ctrl Pts',(78.9493953494971,7.70702441156951,131.779098355661));
#66873=CARTESIAN_POINT('Ctrl Pts',(78.9492982035649,7.70710335336997,131.779089880592));
#66874=CARTESIAN_POINT('Ctrl Pts',(78.9492497453263,7.70714273556504,131.779085652682));
#66875=CARTESIAN_POINT('Ctrl Pts',(78.9491530441415,7.70722133401415,131.779077214877));
#66876=CARTESIAN_POINT('Ctrl Pts',(78.9491048012547,7.70726055018061,131.779073004991));
#66877=CARTESIAN_POINT('Ctrl Pts',(78.9435936542307,7.71174101956509,131.778592034527));
#66878=CARTESIAN_POINT('Ctrl Pts',(78.9381590781216,7.71621675497583,131.778112854273));
#66879=CARTESIAN_POINT('Ctrl Pts',(78.9263376052806,7.72607893967102,131.777060077229));
#66880=CARTESIAN_POINT('Ctrl Pts',(78.919962564018,7.73147923322922,131.776485574723));
#66881=CARTESIAN_POINT('Ctrl Pts',(78.9025202450491,7.74648140544285,131.774895603843));
#66882=CARTESIAN_POINT('Ctrl Pts',(78.8915388603403,7.7561814648169,131.773874226398));
#66883=CARTESIAN_POINT('Ctrl Pts',(78.8558974833036,7.78851099972673,131.770495534403));
#66884=CARTESIAN_POINT('Ctrl Pts',(78.8317923897985,7.81173787721554,131.768108160864));
#66885=CARTESIAN_POINT('Ctrl Pts',(78.7191948906083,7.92697242573903,131.756513342766));
#66886=CARTESIAN_POINT('Ctrl Pts',(78.6407610399778,8.02823593192158,131.747098873635));
#66887=CARTESIAN_POINT('Ctrl Pts',(78.5472856779196,8.18270375317607,131.734313248665));
#66888=CARTESIAN_POINT('Ctrl Pts',(78.522076365869,8.22922451973882,131.730633166426));
#66889=CARTESIAN_POINT('Ctrl Pts',(78.4919275287124,8.29179943941586,131.725900959521));
#66890=CARTESIAN_POINT('Ctrl Pts',(78.4849576008098,8.30683539055494,131.724779638178));
#66891=CARTESIAN_POINT('Ctrl Pts',(78.4739354608275,8.33157387107286,131.722959726897));
#66892=CARTESIAN_POINT('Ctrl Pts',(78.4697488337423,8.34121487230785,131.722256581635));
#66893=CARTESIAN_POINT('Ctrl Pts',(78.461807386397,8.35998676841101,131.720899031883));
#66894=CARTESIAN_POINT('Ctrl Pts',(78.4580419495825,8.36911266374234,131.720244290199));
#66895=CARTESIAN_POINT('Ctrl Pts',(78.4493891406325,8.3906239025751,131.718712880616));
#66896=CARTESIAN_POINT('Ctrl Pts',(78.4445686360912,8.40303555003665,131.717838485136));
#66897=CARTESIAN_POINT('Ctrl Pts',(78.42900136871,8.44458679033562,131.71494047257));
#66898=CARTESIAN_POINT('Ctrl Pts',(78.4189202622286,8.47396996969817,131.712938811937));
#66899=CARTESIAN_POINT('Ctrl Pts',(78.3964472039559,8.54597050419559,131.708133198753));
#66900=CARTESIAN_POINT('Ctrl Pts',(78.3849248036476,8.58883471803644,131.70535523583));
#66901=CARTESIAN_POINT('Ctrl Pts',(78.3477145017679,8.75318296227013,131.694918523051));
#66902=CARTESIAN_POINT('Ctrl Pts',(78.333923345181,8.87692383949796,131.687524599961));
#66903=CARTESIAN_POINT('Ctrl Pts',(78.3340003204331,9.00103328753322,131.67971837006));
#66904=CARTESIAN_POINT('Ctrl Pts',(78.3340003219602,9.00103574665424,131.679718215386));
#66905=CARTESIAN_POINT('Ctrl Pts',(78.3340235477417,9.03839444284753,131.677368428309));
#66906=CARTESIAN_POINT('Ctrl Pts',(78.3353033761624,9.07573933155099,131.674981797394));
#66907=CARTESIAN_POINT('Ctrl Pts',(78.3383818254571,9.12101870446789,131.67200839924));
#66908=CARTESIAN_POINT('Ctrl Pts',(78.338984433172,9.12902622004195,131.671479522037));
#66909=CARTESIAN_POINT('Ctrl Pts',(78.3401157666353,9.1427343912963,131.670568437123));
#66910=CARTESIAN_POINT('Ctrl Pts',(78.3406160393469,9.14843733822041,131.670187712284));
#66911=CARTESIAN_POINT('Ctrl Pts',(78.3416182455442,9.15922325460433,131.669464259105));
#66912=CARTESIAN_POINT('Ctrl Pts',(78.3421141834323,9.16430674360668,131.669121861723));
#66913=CARTESIAN_POINT('Ctrl Pts',(78.3431534772886,9.17447566293804,131.668433932483));
#66914=CARTESIAN_POINT('Ctrl Pts',(78.3436968892138,9.1795610207734,131.668088404159));
#66915=CARTESIAN_POINT('Ctrl Pts',(78.3450460613825,9.19165931192057,131.667262926474));
#66916=CARTESIAN_POINT('Ctrl Pts',(78.3458729885,9.19866971623309,131.666781836851));
#66917=CARTESIAN_POINT('Ctrl Pts',(78.3489767353649,9.22361829732525,131.665060389841));
#66918=CARTESIAN_POINT('Ctrl Pts',(78.3515009223379,9.24152368075207,131.663807692287));
#66919=CARTESIAN_POINT('Ctrl Pts',(78.3619153610792,9.30759910931665,131.65912951612));
#66920=CARTESIAN_POINT('Ctrl Pts',(78.3716295252477,9.35545367340081,131.65563257661));
#66921=CARTESIAN_POINT('Ctrl Pts',(78.3980044333927,9.4613027324769,131.647742105841));
#66922=CARTESIAN_POINT('Ctrl Pts',(78.4157414300658,9.51895336013236,131.643338258236));
#66923=CARTESIAN_POINT('Ctrl Pts',(78.4365593658221,9.57550793513344,131.638964603241));
#66924=CARTESIAN_POINT('',(78.3340002424278,8.99871136581395,131.870599642122));
#66925=CARTESIAN_POINT('Ctrl Pts',(78.4365593737656,9.57550795671282,131.83373138687));
#66926=CARTESIAN_POINT('Ctrl Pts',(78.4360745518862,9.57419087635994,131.833824541444));
#66927=CARTESIAN_POINT('Ctrl Pts',(78.4355913920686,9.57287317725898,131.833917640984));
#66928=CARTESIAN_POINT('Ctrl Pts',(78.4312888554247,9.56109303599931,131.834749065508));
#66929=CARTESIAN_POINT('Ctrl Pts',(78.4275727469838,9.55059294788695,131.835483950254));
#66930=CARTESIAN_POINT('Ctrl Pts',(78.417635866271,9.52159429691574,131.837497098183));
#66931=CARTESIAN_POINT('Ctrl Pts',(78.4116342732758,9.50302209926302,131.83876814628));
#66932=CARTESIAN_POINT('Ctrl Pts',(78.3737904607603,9.37847418408069,131.847179937131));
#66933=CARTESIAN_POINT('Ctrl Pts',(78.3522467171661,9.26965446890637,131.853967829947));
#66934=CARTESIAN_POINT('Ctrl Pts',(78.3365122009242,9.106050039411,131.864005637014));
#66935=CARTESIAN_POINT('Ctrl Pts',(78.3339590443037,9.05239520490956,131.867276149316));
#66936=CARTESIAN_POINT('Ctrl Pts',(78.3340004966975,8.99871353358091,131.870599064419));
#66937=CARTESIAN_POINT('Ctrl Pts',(78.3340004983938,8.99871133866798,131.870599200285));
#66938=CARTESIAN_POINT('Ctrl Pts',(78.3340316402379,8.95845072455788,131.87309134809));
#66939=CARTESIAN_POINT('Ctrl Pts',(78.3355221838307,8.91820640698278,131.875611367354));
#66940=CARTESIAN_POINT('Ctrl Pts',(78.3399331311568,8.85810475873496,131.879468884735));
#66941=CARTESIAN_POINT('Ctrl Pts',(78.3417567416082,8.83818070644958,131.880763270043));
#66942=CARTESIAN_POINT('Ctrl Pts',(78.3447889344087,8.81054521362256,131.882586340663));
#66943=CARTESIAN_POINT('Ctrl Pts',(78.3456936612383,8.8028013193423,131.883100227923));
#66944=CARTESIAN_POINT('Ctrl Pts',(78.3473458863135,8.78947176722082,131.883990456338));
#66945=CARTESIAN_POINT('Ctrl Pts',(78.3480674427875,8.78388294740192,131.884365434232));
#66946=CARTESIAN_POINT('Ctrl Pts',(78.3495612860912,8.77275716531181,131.885115537949));
#66947=CARTESIAN_POINT('Ctrl Pts',(78.3503331210716,8.76722018570077,131.88549064018));
#66948=CARTESIAN_POINT('Ctrl Pts',(78.3519976259096,8.75570360970529,131.886274744676));
#66949=CARTESIAN_POINT('Ctrl Pts',(78.3528949894902,8.74972488590105,131.886683983951));
#66950=CARTESIAN_POINT('Ctrl Pts',(78.3553845610003,8.73373155311702,131.887784315166));
#66951=CARTESIAN_POINT('Ctrl Pts',(78.3570356655544,8.72372656494716,131.888478540562));
#66952=CARTESIAN_POINT('Ctrl Pts',(78.365108168319,8.67744466039859,131.891715353203));
#66953=CARTESIAN_POINT('Ctrl Pts',(78.3726399727852,8.64137466936291,131.894310308466));
#66954=CARTESIAN_POINT('Ctrl Pts',(78.3955410670832,8.54739034158854,131.901214182282));
#66955=CARTESIAN_POINT('Ctrl Pts',(78.4128495312938,8.49000322142901,131.905572920464));
#66956=CARTESIAN_POINT('Ctrl Pts',(78.4688726432898,8.33500992385575,131.917569925703));
#66957=CARTESIAN_POINT('Ctrl Pts',(78.5137809246817,8.23992008586034,131.925169288583));
#66958=CARTESIAN_POINT('Ctrl Pts',(78.5853165251336,8.11939407162546,131.934939051558));
#66959=CARTESIAN_POINT('Ctrl Pts',(78.6042471911213,8.08968656230755,131.937361611782));
#66960=CARTESIAN_POINT('Ctrl Pts',(78.6319775211428,8.04907132466332,131.940696381739));
#66961=CARTESIAN_POINT('Ctrl Pts',(78.6399931891947,8.03764229966226,131.941637427042));
#66962=CARTESIAN_POINT('Ctrl Pts',(78.6539847138118,8.01821669597899,131.943241905762));
#66963=CARTESIAN_POINT('Ctrl Pts',(78.6598904165466,8.01017076295418,131.943907976668));
#66964=CARTESIAN_POINT('Ctrl Pts',(78.6713122039051,7.99489932823909,131.945175327185));
#66965=CARTESIAN_POINT('Ctrl Pts',(78.6768157979363,7.98766497994507,131.945777060179));
#66966=CARTESIAN_POINT('Ctrl Pts',(78.691304412121,7.96894005623519,131.947338404459));
#66967=CARTESIAN_POINT('Ctrl Pts',(78.7003817418318,7.95752162868693,131.948294341491));
#66968=CARTESIAN_POINT('Ctrl Pts',(78.732919426878,7.91767791575345,131.951645497409));
#66969=CARTESIAN_POINT('Ctrl Pts',(78.7571727634297,7.88991214301204,131.954008857723));
#66970=CARTESIAN_POINT('Ctrl Pts',(78.8792664844338,7.75915896415067,131.965332882698));
#66971=CARTESIAN_POINT('Ctrl Pts',(78.9890744921864,7.66817486594924,131.973770183453));
#66972=CARTESIAN_POINT('Ctrl Pts',(79.1405664360587,7.57230344207744,131.984898644657));
#66973=CARTESIAN_POINT('Ctrl Pts',(79.1726994951628,7.55344650036948,131.987237301765));
#66974=CARTESIAN_POINT('Ctrl Pts',(79.2192568135953,7.5281836525115,131.990633834411));
#66975=CARTESIAN_POINT('Ctrl Pts',(79.2331833508589,7.52088016999526,131.991650840466));
#66976=CARTESIAN_POINT('Ctrl Pts',(79.2580880975047,7.50826563903372,131.993475055217));
#66977=CARTESIAN_POINT('Ctrl Pts',(79.2690253408589,7.50287585648964,131.994278035975));
#66978=CARTESIAN_POINT('Ctrl Pts',(79.2858700142636,7.4948035210287,131.995519054706));
#66979=CARTESIAN_POINT('Ctrl Pts',(79.2917358664506,7.4920344863332,131.995952013122));
#66980=CARTESIAN_POINT('Ctrl Pts',(79.3025832041484,7.48699114344993,131.996754392575));
#66981=CARTESIAN_POINT('Ctrl Pts',(79.3075599132548,7.48470705460791,131.997123213011));
#66982=CARTESIAN_POINT('Ctrl Pts',(79.3189412437748,7.4795513046145,131.99796821665));
#66983=CARTESIAN_POINT('Ctrl Pts',(79.3253528106485,7.47669555565565,131.998445325647));
#66984=CARTESIAN_POINT('Ctrl Pts',(79.3457764474946,7.46775297954117,131.999968120125));
#66985=CARTESIAN_POINT('Ctrl Pts',(79.3598538234333,7.46181853483207,132.001022184795));
#66986=CARTESIAN_POINT('Ctrl Pts',(79.494265610946,7.40732066936147,132.011115255864));
#66987=CARTESIAN_POINT('Ctrl Pts',(79.6197987020533,7.37278169333299,132.020719015859));
#66988=CARTESIAN_POINT('Ctrl Pts',(79.8363958854486,7.33964605483098,132.036546682854));
#66989=CARTESIAN_POINT('Ctrl Pts',(79.9256855260011,7.3332596019077,132.042876337841));
#66990=CARTESIAN_POINT('Ctrl Pts',(80.0334757976223,7.33423465614544,132.050241616456));
#66991=CARTESIAN_POINT('Ctrl Pts',(80.0518784187392,7.3347061860848,132.051489870549));
#66992=CARTESIAN_POINT('Ctrl Pts',(80.0811619853997,7.33594243591086,132.053462284287));
#66993=CARTESIAN_POINT('Ctrl Pts',(80.0920493070806,7.33650915863104,132.05419254896));
#66994=CARTESIAN_POINT('Ctrl Pts',(80.1126639561657,7.33778523169112,132.055569742338));
#66995=CARTESIAN_POINT('Ctrl Pts',(80.1223920969227,7.33847320680039,132.056217309416));
#66996=CARTESIAN_POINT('Ctrl Pts',(80.1445324500483,7.34023448362968,132.057686067956));
#66997=CARTESIAN_POINT('Ctrl Pts',(80.1569398846019,7.34136167742539,132.058505540383));
#66998=CARTESIAN_POINT('Ctrl Pts',(80.1893777119806,7.34467585208633,132.060639275625));
#66999=CARTESIAN_POINT('Ctrl Pts',(80.2093834837405,7.34708724814287,132.061946535181));
#67000=CARTESIAN_POINT('Ctrl Pts',(80.3593515745496,7.36793026703697,132.071692469615));
#67001=CARTESIAN_POINT('Ctrl Pts',(80.4867709206836,7.40129956560474,132.079622332589));
#67002=CARTESIAN_POINT('Ctrl Pts',(80.6884719389161,7.48050692875075,132.092884394717));
#67003=CARTESIAN_POINT('Ctrl Pts',(80.7654527719295,7.51779526018346,132.098150772127));
#67004=CARTESIAN_POINT('Ctrl Pts',(80.8499776377055,7.56708375628951,132.104540859735));
#67005=CARTESIAN_POINT('Ctrl Pts',(80.8606597016236,7.57347421984896,132.105360257314));
#67006=CARTESIAN_POINT('Ctrl Pts',(80.8768427248161,7.58340351503491,132.106621384711));
#67007=CARTESIAN_POINT('Ctrl Pts',(80.8823963837906,7.58685620564829,132.107057777122));
#67008=CARTESIAN_POINT('Ctrl Pts',(80.8925583992115,7.59325715477464,132.107863198879));
#67009=CARTESIAN_POINT('Ctrl Pts',(80.8971727370576,7.59619552444934,132.108231590072));
#67010=CARTESIAN_POINT('Ctrl Pts',(80.9077140146641,7.60298131803264,132.109079273762));
#67011=CARTESIAN_POINT('Ctrl Pts',(80.9136309872968,7.60684374721721,132.109559526849));
#67012=CARTESIAN_POINT('Ctrl Pts',(80.9321372734362,7.61909271525781,132.111075141032));
#67013=CARTESIAN_POINT('Ctrl Pts',(80.9446366313429,7.62761287522598,132.112118650243));
#67014=CARTESIAN_POINT('Ctrl Pts',(81.0414571257971,7.69555966590559,132.120347731364));
#67015=CARTESIAN_POINT('Ctrl Pts',(81.1202029629156,7.76252701759398,132.127902356081));
#67016=CARTESIAN_POINT('Ctrl Pts',(81.2720493961906,7.91810320028777,132.143711605378));
#67017=CARTESIAN_POINT('Ctrl Pts',(81.3432449235341,8.00787473158587,132.151902768764));
#67018=CARTESIAN_POINT('Ctrl Pts',(81.4151571255812,8.12064528610795,132.161055483773));
#67019=CARTESIAN_POINT('Ctrl Pts',(81.4253284738023,8.1372293466144,132.1623761801));
#67020=CARTESIAN_POINT('Ctrl Pts',(81.4408565097413,8.16357171793795,132.164435478899));
#67021=CARTESIAN_POINT('Ctrl Pts',(81.4464095889559,8.173211596557,132.165181147888));
#67022=CARTESIAN_POINT('Ctrl Pts',(81.4566326609653,8.19137662933929,132.166571776055));
#67023=CARTESIAN_POINT('Ctrl Pts',(81.4613253804112,8.19988838029911,132.167217529178));
#67024=CARTESIAN_POINT('Ctrl Pts',(81.471696135259,8.21909470273719,132.168661797515));
#67025=CARTESIAN_POINT('Ctrl Pts',(81.4773326514158,8.22981116094054,132.16945881738));
#67026=CARTESIAN_POINT('Ctrl Pts',(81.4935672642219,8.26151139583161,132.171791457617));
#67027=CARTESIAN_POINT('Ctrl Pts',(81.5038389294672,8.28265966646983,132.173315723502));
#67028=CARTESIAN_POINT('Ctrl Pts',(81.5589401013627,8.40249692472199,132.181790095452));
#67029=CARTESIAN_POINT('Ctrl Pts',(81.5945039144788,8.5051616567703,132.188417050114));
#67030=CARTESIAN_POINT('Ctrl Pts',(81.6373836568384,8.68351817009856,132.199618286142));
#67031=CARTESIAN_POINT('Ctrl Pts',(81.6499732336384,8.75756913489963,132.204190154683));
#67032=CARTESIAN_POINT('Ctrl Pts',(81.6611300541824,8.86778302629311,132.211182924309));
#67033=CARTESIAN_POINT('Ctrl Pts',(81.6635846515538,8.90345951991959,132.213475852723));
#67034=CARTESIAN_POINT('Ctrl Pts',(81.6652439400975,8.94888411694041,132.216463659033));
#67035=CARTESIAN_POINT('Ctrl Pts',(81.665513475106,8.9585866373357,132.217105805608));
#67036=CARTESIAN_POINT('Ctrl Pts',(81.6658114644099,8.97424008198021,132.218148996003));
#67037=CARTESIAN_POINT('Ctrl Pts',(81.6658928438257,8.98018994112299,132.218547187023));
#67038=CARTESIAN_POINT('Ctrl Pts',(81.6659887292251,8.99171515339399,132.219321971851));
#67039=CARTESIAN_POINT('Ctrl Pts',(81.666007124468,8.99729033951679,132.219698350734));
#67040=CARTESIAN_POINT('Ctrl Pts',(81.665985689979,9.00975289296879,132.220543094886));
#67041=CARTESIAN_POINT('Ctrl Pts',(81.6659311330671,9.01664012762671,132.221012249005));
#67042=CARTESIAN_POINT('Ctrl Pts',(81.6656404977047,9.03721890758763,132.222420604055));
#67043=CARTESIAN_POINT('Ctrl Pts',(81.665278322262,9.05090770671635,132.223366080099));
#67044=CARTESIAN_POINT('Ctrl Pts',(81.6607645858142,9.16724520156487,132.231466498603));
#67045=CARTESIAN_POINT('Ctrl Pts',(81.647295466524,9.26930309814728,132.238988805981));
#67046=CARTESIAN_POINT('Ctrl Pts',(81.599077192505,9.48131831528588,132.254801181296));
#67047=CARTESIAN_POINT('Ctrl Pts',(81.5621485844486,9.59026791946311,132.263026282082));
#67048=CARTESIAN_POINT('Ctrl Pts',(81.5062203774433,9.71220246970613,132.272205682261));
#67049=CARTESIAN_POINT('Ctrl Pts',(81.4978266860374,9.72968997323268,132.273522418533));
#67050=CARTESIAN_POINT('Ctrl Pts',(81.484146496828,9.75696014383506,132.275576974645));
#67051=CARTESIAN_POINT('Ctrl Pts',(81.4790644303846,9.76684281605324,132.276321806964));
#67052=CARTESIAN_POINT('Ctrl Pts',(81.469352088897,9.78527379261788,132.277711676659));
#67053=CARTESIAN_POINT('Ctrl Pts',(81.4647451642479,9.79383379946791,132.278357499702));
#67054=CARTESIAN_POINT('Ctrl Pts',(81.4542240237014,9.81297940041972,132.279802957133));
#67055=CARTESIAN_POINT('Ctrl Pts',(81.4482685927552,9.82354181000819,132.280601085136));
#67056=CARTESIAN_POINT('Ctrl Pts',(81.4303880215247,9.8544604408534,132.2829402422));
#67057=CARTESIAN_POINT('Ctrl Pts',(81.4181449152866,9.87462999372215,132.284469818896));
#67058=CARTESIAN_POINT('Ctrl Pts',(81.3503007304635,9.9812257093451,132.29258715386));
#67059=CARTESIAN_POINT('Ctrl Pts',(81.2872199585986,10.0626307269221,132.298888921183));
#67060=CARTESIAN_POINT('Ctrl Pts',(81.1628992427004,10.1956191483002,132.310007381257));
#67061=CARTESIAN_POINT('Ctrl Pts',(81.1047053011346,10.249585629033,132.31482549069));
#67062=CARTESIAN_POINT('Ctrl Pts',(81.0235809200499,10.3147058921622,132.321384825536));
#67063=CARTESIAN_POINT('Ctrl Pts',(81.0039232110396,10.3297772517555,132.32296360362));
#67064=CARTESIAN_POINT('Ctrl Pts',(80.9700457038409,10.3545714092684,132.325680424689));
#67065=CARTESIAN_POINT('Ctrl Pts',(80.955997367388,10.3645223879495,132.326805922499));
#67066=CARTESIAN_POINT('Ctrl Pts',(80.9356618043696,10.3784586774781,132.328437511756));
#67067=CARTESIAN_POINT('Ctrl Pts',(80.929497613732,10.3826226956406,132.328932392836));
#67068=CARTESIAN_POINT('Ctrl Pts',(80.9187212437622,10.3897976877807,132.329798477217));
#67069=CARTESIAN_POINT('Ctrl Pts',(80.9141216894636,10.3928272945879,132.330168437248));
#67070=CARTESIAN_POINT('Ctrl Pts',(80.9042330880757,10.3992705766097,132.330964577414));
#67071=CARTESIAN_POINT('Ctrl Pts',(80.8989397800303,10.4026770450561,132.331391178623));
#67072=CARTESIAN_POINT('Ctrl Pts',(80.8843522353673,10.4119482647905,132.332567733544));
#67073=CARTESIAN_POINT('Ctrl Pts',(80.8750192688317,10.4177510506833,132.333321484732));
#67074=CARTESIAN_POINT('Ctrl Pts',(80.8216179422312,10.4502252726654,132.337636985714));
#67075=CARTESIAN_POINT('Ctrl Pts',(80.7763926772353,10.4749314245003,132.341301353216));
#67076=CARTESIAN_POINT('Ctrl Pts',(80.6437992502714,10.5395768613531,132.351931419868));
#67077=CARTESIAN_POINT('Ctrl Pts',(80.5540210821498,10.5741143838078,132.358983560135));
#67078=CARTESIAN_POINT('Ctrl Pts',(80.4112411560208,10.6153023841077,132.369670191623));
#67079=CARTESIAN_POINT('Ctrl Pts',(80.3600519300265,10.6274779806804,132.373404753369));
#67080=CARTESIAN_POINT('Ctrl Pts',(80.284945051806,10.6416243251809,132.378731226177));
#67081=CARTESIAN_POINT('Ctrl Pts',(80.2614289582662,10.6455330766647,132.38037777149));
#67082=CARTESIAN_POINT('Ctrl Pts',(80.2186318806754,10.6517059582119,132.383336576203));
#67083=CARTESIAN_POINT('Ctrl Pts',(80.1993801440945,10.6541402857695,132.38465382758));
#67084=CARTESIAN_POINT('Ctrl Pts',(80.1690407853044,10.6574392089392,132.386709000647));
#67085=CARTESIAN_POINT('Ctrl Pts',(80.1579800544197,10.6585300211921,132.387453941836));
#67086=CARTESIAN_POINT('Ctrl Pts',(80.1372264187758,10.6603672476535,132.388843910055));
#67087=CARTESIAN_POINT('Ctrl Pts',(80.1275363505881,10.6611396609605,132.389489723832));
#67088=CARTESIAN_POINT('Ctrl Pts',(80.1057474801884,10.6626847062135,132.390935025706));
#67089=CARTESIAN_POINT('Ctrl Pts',(80.0936458045795,10.663410183357,132.39173300886));
#67090=CARTESIAN_POINT('Ctrl Pts',(80.057985194326,10.6651575713348,132.394071313556));
#67091=CARTESIAN_POINT('Ctrl Pts',(80.0344106400923,10.665811519179,132.395600195557));
#67092=CARTESIAN_POINT('Ctrl Pts',(79.9068353858666,10.6666407882894,132.403796237536));
#67093=CARTESIAN_POINT('Ctrl Pts',(79.8030026316509,10.6575785293874,132.410169498754));
#67094=CARTESIAN_POINT('Ctrl Pts',(79.6236308687163,10.624819163601,132.421304916774));
#67095=CARTESIAN_POINT('Ctrl Pts',(79.5476725897228,10.6053315036096,132.426068225049));
#67096=CARTESIAN_POINT('Ctrl Pts',(79.4500218943596,10.5727955602315,132.432559806305));
#67097=CARTESIAN_POINT('Ctrl Pts',(79.4268475886982,10.564499273461,132.434128998003));
#67098=CARTESIAN_POINT('Ctrl Pts',(79.3878662049638,10.5495618187369,132.436830921199));
#67099=CARTESIAN_POINT('Ctrl Pts',(79.3719618943802,10.5431842712598,132.437951287413));
#67100=CARTESIAN_POINT('Ctrl Pts',(79.3493112470958,10.5336933462092,132.439576735811));
#67101=CARTESIAN_POINT('Ctrl Pts',(79.3424823723078,10.5307781346188,132.440070722904));
#67102=CARTESIAN_POINT('Ctrl Pts',(79.3306239248811,10.5256218363943,132.440935799553));
#67103=CARTESIAN_POINT('Ctrl Pts',(79.3255856122922,10.5234013096555,132.441305654924));
#67104=CARTESIAN_POINT('Ctrl Pts',(79.3148036778202,10.5185854345541,132.442102225564));
#67105=CARTESIAN_POINT('Ctrl Pts',(79.3090638427345,10.5159825016311,132.442529367695));
#67106=CARTESIAN_POINT('Ctrl Pts',(79.2933248836194,10.508737158965,132.443708834835));
#67107=CARTESIAN_POINT('Ctrl Pts',(79.2833570677149,10.5040280669959,132.444464986975));
#67108=CARTESIAN_POINT('Ctrl Pts',(79.2264912904439,10.47646936916,132.44882856354));
#67109=CARTESIAN_POINT('Ctrl Pts',(79.1806446818053,10.4515279060208,132.452541212418));
#67110=CARTESIAN_POINT('Ctrl Pts',(79.0487711760485,10.3715462288854,132.463659331384));
#67111=CARTESIAN_POINT('Ctrl Pts',(78.9665372428196,10.310698981517,132.471162290542));
#67112=CARTESIAN_POINT('Ctrl Pts',(78.8359641791022,10.1941107694014,132.483711465315));
#67113=CARTESIAN_POINT('Ctrl Pts',(78.7847831231749,10.1419853373315,132.488839161652));
#67114=CARTESIAN_POINT('Ctrl Pts',(78.7256827106888,10.0733042909583,132.495022751646));
#67115=CARTESIAN_POINT('Ctrl Pts',(78.7143987446615,10.0597622886962,132.496216934413));
#67116=CARTESIAN_POINT('Ctrl Pts',(78.6965917611611,10.0376888659565,132.498124359699));
#67117=CARTESIAN_POINT('Ctrl Pts',(78.6899328695039,10.0292693245814,132.498843026617));
#67118=CARTESIAN_POINT('Ctrl Pts',(78.6773568393692,10.0130483328765,132.500210995867));
#67119=CARTESIAN_POINT('Ctrl Pts',(78.671426216,10.005257958216,132.500860813736));
#67120=CARTESIAN_POINT('Ctrl Pts',(78.6580440461882,9.98735404511676,132.502338258425));
#67121=CARTESIAN_POINT('Ctrl Pts',(78.6506374605169,9.9772075234007,132.50316411518));
#67122=CARTESIAN_POINT('Ctrl Pts',(78.6311691993435,9.94989388027907,132.505357799955));
#67123=CARTESIAN_POINT('Ctrl Pts',(78.6193156080722,9.93258072973556,132.506717755246));
#67124=CARTESIAN_POINT('Ctrl Pts',(78.5412033247309,9.81373602995264,132.515861037351));
#67125=CARTESIAN_POINT('Ctrl Pts',(78.4858706795807,9.70545752468266,132.523222986965));
#67126=CARTESIAN_POINT('Ctrl Pts',(78.4406741477407,9.58659514057224,132.530993796469));
#67127=CARTESIAN_POINT('Ctrl Pts',(78.4386019183015,9.58105678893567,132.531355281971));
#67128=CARTESIAN_POINT('Ctrl Pts',(78.4365593745624,9.57550795887745,132.531716954706));
#67129=CARTESIAN_POINT('Origin',(80.,9.,134.));
#67130=CARTESIAN_POINT('',(78.4365593737643,9.57550795670927,133.231048988662));
#67131=CARTESIAN_POINT('',(78.4365593647824,9.57550793230875,133.038342764662));
#67132=CARTESIAN_POINT('',(78.4365593737638,9.57550795670799,134.));
#67133=CARTESIAN_POINT('Ctrl Pts',(78.4365593647824,9.57550793230875,133.038342764662));
#67134=CARTESIAN_POINT('Ctrl Pts',(78.458363872793,9.63474265687277,133.034409061954));
#67135=CARTESIAN_POINT('Ctrl Pts',(78.4835221810049,9.69270400732193,133.03055199272));
#67136=CARTESIAN_POINT('Ctrl Pts',(78.5536676740876,9.83204591991857,133.021025947317));
#67137=CARTESIAN_POINT('Ctrl Pts',(78.6022744362798,9.91133808078974,133.015379540216));
#67138=CARTESIAN_POINT('Ctrl Pts',(78.6705019239503,10.0042380022328,133.007981824922));
#67139=CARTESIAN_POINT('Ctrl Pts',(78.6841418566152,10.0220451687343,133.006524471428));
#67140=CARTESIAN_POINT('Ctrl Pts',(78.703280559747,10.0460127435335,133.004499984223));
#67141=CARTESIAN_POINT('Ctrl Pts',(78.708472471434,10.0524165536073,133.003952747093));
#67142=CARTESIAN_POINT('Ctrl Pts',(78.7172966634518,10.0631368554165,133.003025421484));
#67143=CARTESIAN_POINT('Ctrl Pts',(78.720903820544,10.0674740209847,133.00264710751));
#67144=CARTESIAN_POINT('Ctrl Pts',(78.7283635648206,10.0763513512869,133.001866101055));
#67145=CARTESIAN_POINT('Ctrl Pts',(78.7322185525966,10.0808892882716,133.001463249547));
#67146=CARTESIAN_POINT('Ctrl Pts',(78.7424299066295,10.0927799074118,133.000398336395));
#67147=CARTESIAN_POINT('Ctrl Pts',(78.7488263220688,10.1000976693339,132.999733473148));
#67148=CARTESIAN_POINT('Ctrl Pts',(78.7768041857642,10.1315458613859,132.996836376631));
#67149=CARTESIAN_POINT('Ctrl Pts',(78.7990209686983,10.1550987294904,132.994563863957));
#67150=CARTESIAN_POINT('Ctrl Pts',(78.9053963006527,10.2614835050117,132.98386801059));
#67151=CARTESIAN_POINT('Ctrl Pts',(78.9975233571079,10.3358665182641,132.975148044204));
#67152=CARTESIAN_POINT('Ctrl Pts',(79.1407783152589,10.428299923245,132.962889069126));
#67153=CARTESIAN_POINT('Ctrl Pts',(79.1861342775254,10.454622302091,132.959167508737));
#67154=CARTESIAN_POINT('Ctrl Pts',(79.2537714238063,10.4897196495944,132.953857224597));
#67155=CARTESIAN_POINT('Ctrl Pts',(79.2751162906602,10.5002217931661,132.952214243424));
#67156=CARTESIAN_POINT('Ctrl Pts',(79.3142408113898,10.5184418360883,132.949261112801));
#67157=CARTESIAN_POINT('Ctrl Pts',(79.3319438478213,10.5263133055979,132.947946001921));
#67158=CARTESIAN_POINT('Ctrl Pts',(79.3600090145075,10.5382103086532,132.945893264854));
#67159=CARTESIAN_POINT('Ctrl Pts',(79.3702805318703,10.5424437808128,132.945148649509));
#67160=CARTESIAN_POINT('Ctrl Pts',(79.3896208082384,10.5501896009276,132.943758777155));
#67161=CARTESIAN_POINT('Ctrl Pts',(79.3986794091948,10.5537258800983,132.943112738267));
#67162=CARTESIAN_POINT('Ctrl Pts',(79.4191131867078,10.5614973022901,132.94166626658));
#67163=CARTESIAN_POINT('Ctrl Pts',(79.4305048074356,10.5656878851088,132.94086734672));
#67164=CARTESIAN_POINT('Ctrl Pts',(79.4642169670935,10.5776727961898,132.938524156423));
#67165=CARTESIAN_POINT('Ctrl Pts',(79.4866593494814,10.5851171492447,132.936991395942));
#67166=CARTESIAN_POINT('Ctrl Pts',(79.6072911402031,10.6223009381666,132.928882423234));
#67167=CARTESIAN_POINT('Ctrl Pts',(79.7079143655427,10.6434019228162,132.922590953249));
#67168=CARTESIAN_POINT('Ctrl Pts',(79.8886678491112,10.6641681096812,132.911478889195));
#67169=CARTESIAN_POINT('Ctrl Pts',(79.9680269647158,10.6675809779561,132.90665692751));
#67170=CARTESIAN_POINT('Ctrl Pts',(80.0720917264687,10.664623944309,132.900092760462));
#67171=CARTESIAN_POINT('Ctrl Pts',(80.0968425491642,10.6633675131114,132.898513227839));
#67172=CARTESIAN_POINT('Ctrl Pts',(80.1387315127585,10.6603030405283,132.895795178828));
#67173=CARTESIAN_POINT('Ctrl Pts',(80.1558869045101,10.6587802251282,132.894669220452));
#67174=CARTESIAN_POINT('Ctrl Pts',(80.1804159037325,10.6562190300862,132.893037000909));
#67175=CARTESIAN_POINT('Ctrl Pts',(80.187811598653,10.6553966811942,132.892541959607));
#67176=CARTESIAN_POINT('Ctrl Pts',(80.2006728660645,10.6538793048184,132.891675608485));
#67177=CARTESIAN_POINT('Ctrl Pts',(80.2061408962968,10.6532066670416,132.891305542858));
#67178=CARTESIAN_POINT('Ctrl Pts',(80.2178511219851,10.6517071575515,132.890509180806));
#67179=CARTESIAN_POINT('Ctrl Pts',(80.2240918929547,10.650872031951,132.890082463133));
#67180=CARTESIAN_POINT('Ctrl Pts',(80.2412149955069,10.6484817772762,132.888905586246));
#67181=CARTESIAN_POINT('Ctrl Pts',(80.2520866734937,10.6468543156574,132.888151627584));
#67182=CARTESIAN_POINT('Ctrl Pts',(80.313829722362,10.6369858625775,132.883834271339));
#67183=CARTESIAN_POINT('Ctrl Pts',(80.3643085811822,10.6264962272298,132.880168168151));
#67184=CARTESIAN_POINT('Ctrl Pts',(80.5071904680114,10.589820087356,132.869537877139));
#67185=CARTESIAN_POINT('Ctrl Pts',(80.5979306311228,10.5579634488277,132.862487426011));
#67186=CARTESIAN_POINT('Ctrl Pts',(80.7333469544304,10.4968375459011,132.851802904118));
#67187=CARTESIAN_POINT('Ctrl Pts',(80.780221154801,10.4729481433787,132.848068813194));
#67188=CARTESIAN_POINT('Ctrl Pts',(80.8465905447746,10.4350639495914,132.842742818878));
#67189=CARTESIAN_POINT('Ctrl Pts',(80.8670352406487,10.4228050043596,132.841096298208));
#67190=CARTESIAN_POINT('Ctrl Pts',(80.9036340885582,10.399777816193,132.83813746538));
#67191=CARTESIAN_POINT('Ctrl Pts',(80.9198762138907,10.3891581288892,132.836820162547));
#67192=CARTESIAN_POINT('Ctrl Pts',(80.9451257723535,10.3720119673865,132.834764799998));
#67193=CARTESIAN_POINT('Ctrl Pts',(80.9542592831434,10.3656752158268,132.834019721275));
#67194=CARTESIAN_POINT('Ctrl Pts',(80.9712618462955,10.3536251208314,132.832629430069));
#67195=CARTESIAN_POINT('Ctrl Pts',(80.979145578467,10.3479334126121,132.831983431115));
#67196=CARTESIAN_POINT('Ctrl Pts',(80.9967495577334,10.3349881647595,132.83053762395));
#67197=CARTESIAN_POINT('Ctrl Pts',(81.0064414060493,10.3276967989957,132.829739322518));
#67198=CARTESIAN_POINT('Ctrl Pts',(81.0347515316582,10.3059103975364,132.827399773135));
#67199=CARTESIAN_POINT('Ctrl Pts',(81.0531429809031,10.2911245679799,132.825869980262));
#67200=CARTESIAN_POINT('Ctrl Pts',(81.1498161991498,10.2099633976874,132.817760985217));
#67201=CARTESIAN_POINT('Ctrl Pts',(81.2221553308757,10.1368502033465,132.811466923631));
#67202=CARTESIAN_POINT('Ctrl Pts',(81.3376911383935,9.99621144904232,132.800350683934));
#67203=CARTESIAN_POINT('Ctrl Pts',(81.3836202198775,9.93136897466239,132.795527081024));
#67204=CARTESIAN_POINT('Ctrl Pts',(81.4375969469632,9.84230952789956,132.788960886304));
#67205=CARTESIAN_POINT('Ctrl Pts',(81.4499682725651,9.82083019024092,132.787381068504));
#67206=CARTESIAN_POINT('Ctrl Pts',(81.4701170511469,9.7839697424649,132.784662576486));
#67207=CARTESIAN_POINT('Ctrl Pts',(81.4781436031578,9.76872890725481,132.783536465656));
#67208=CARTESIAN_POINT('Ctrl Pts',(81.4892972088397,9.74672967247109,132.78190406371));
#67209=CARTESIAN_POINT('Ctrl Pts',(81.4926177976683,9.74006991889102,132.781408995896));
#67210=CARTESIAN_POINT('Ctrl Pts',(81.4983189134259,9.72844134171625,132.780542614862));
#67211=CARTESIAN_POINT('Ctrl Pts',(81.5007195881627,9.72348259920487,132.780172546106));
#67212=CARTESIAN_POINT('Ctrl Pts',(81.5058111313507,9.71283131207421,132.779376196705));
#67213=CARTESIAN_POINT('Ctrl Pts',(81.5084942956302,9.70713548880917,132.778949494983));
#67214=CARTESIAN_POINT('Ctrl Pts',(81.5157728976149,9.69145451380474,132.777772703947));
#67215=CARTESIAN_POINT('Ctrl Pts',(81.5203018039857,9.68143908787989,132.777018816058));
#67216=CARTESIAN_POINT('Ctrl Pts',(81.5454904102591,9.62423473801289,132.772703008399));
#67217=CARTESIAN_POINT('Ctrl Pts',(81.5640498655995,9.57615670261246,132.769038467298));
#67218=CARTESIAN_POINT('Ctrl Pts',(81.6107309039638,9.43625119684255,132.758410176252));
#67219=CARTESIAN_POINT('Ctrl Pts',(81.633185923138,9.34274473930579,132.751360068374));
#67220=CARTESIAN_POINT('Ctrl Pts',(81.6552883978274,9.19581245952426,132.740674530224));
#67221=CARTESIAN_POINT('Ctrl Pts',(81.6606453380057,9.14345783522433,132.736939172299));
#67222=CARTESIAN_POINT('Ctrl Pts',(81.664817715732,9.06712900057565,132.731611589903));
#67223=CARTESIAN_POINT('Ctrl Pts',(81.6656078919411,9.04329871517843,132.72996471171));
#67224=CARTESIAN_POINT('Ctrl Pts',(81.6661130279278,9.00005310832927,132.727005302984));
#67225=CARTESIAN_POINT('Ctrl Pts',(81.6660006131039,8.98064445695825,132.725687778819));
#67226=CARTESIAN_POINT('Ctrl Pts',(81.6652904696519,8.95012785388706,132.723632151177));
#67227=CARTESIAN_POINT('Ctrl Pts',(81.6649206134033,8.93901688177521,132.722887025676));
#67228=CARTESIAN_POINT('Ctrl Pts',(81.6640188300732,8.91819612781828,132.721496692136));
#67229=CARTESIAN_POINT('Ctrl Pts',(81.6635130563646,8.90848574701562,132.720850697161));
#67230=CARTESIAN_POINT('Ctrl Pts',(81.6621855176908,8.88667585372414,132.719404956828));
#67231=CARTESIAN_POINT('Ctrl Pts',(81.6613165906193,8.87457968240863,132.718606717627));
#67232=CARTESIAN_POINT('Ctrl Pts',(81.6583686253788,8.83898453849543,132.71626753446));
#67233=CARTESIAN_POINT('Ctrl Pts',(81.6559224325431,8.81551839268672,132.714738040061));
#67234=CARTESIAN_POINT('Ctrl Pts',(81.6401040686105,8.68974245662752,132.70659421783));
#67235=CARTESIAN_POINT('Ctrl Pts',(81.6177478784738,8.588786859531,132.700268507794));
#67236=CARTESIAN_POINT('Ctrl Pts',(81.5620501834658,8.41537375840546,132.689144835628));
#67237=CARTESIAN_POINT('Ctrl Pts',(81.5325977294016,8.34202501550044,132.684345510267));
#67238=CARTESIAN_POINT('Ctrl Pts',(81.4872447500361,8.24882094365922,132.677809317136));
#67239=CARTESIAN_POINT('Ctrl Pts',(81.47593727185,8.22684027417586,132.676233727817));
#67240=CARTESIAN_POINT('Ctrl Pts',(81.4559441687673,8.1900135426461,132.673521805443));
#67241=CARTESIAN_POINT('Ctrl Pts',(81.4475097464026,8.17503517572367,132.672397956209));
#67242=CARTESIAN_POINT('Ctrl Pts',(81.4350972443057,8.1537688321937,132.670768260328));
#67243=CARTESIAN_POINT('Ctrl Pts',(81.4313061285966,8.14737226705228,132.67027358608));
#67244=CARTESIAN_POINT('Ctrl Pts',(81.4246320752865,8.13628141372444,132.66940764892));
#67245=CARTESIAN_POINT('Ctrl Pts',(81.4217684719951,8.13157570436811,132.669037626473));
#67246=CARTESIAN_POINT('Ctrl Pts',(81.4155799852824,8.12151892965444,132.66824108861));
#67247=CARTESIAN_POINT('Ctrl Pts',(81.4122481294619,8.11617258289667,132.667814149577));
#67248=CARTESIAN_POINT('Ctrl Pts',(81.4030116158703,8.10153711316241,132.666636081175));
#67249=CARTESIAN_POINT('Ctrl Pts',(81.3970452206595,8.09228760692123,132.665881140234));
#67250=CARTESIAN_POINT('Ctrl Pts',(81.3624652782639,8.03982803140378,132.6615426165));
#67251=CARTESIAN_POINT('Ctrl Pts',(81.3319420159483,7.99791656764431,132.6578551749));
#67252=CARTESIAN_POINT('Ctrl Pts',(81.2370259884891,7.87959983081459,132.64692275476));
#67253=CARTESIAN_POINT('Ctrl Pts',(81.1676541732336,7.80747534998635,132.639583951734));
#67254=CARTESIAN_POINT('Ctrl Pts',(81.0544636093322,7.70919989812938,132.628824437386));
#67255=CARTESIAN_POINT('Ctrl Pts',(81.0152296014073,7.67811950467839,132.625278632196));
#67256=CARTESIAN_POINT('Ctrl Pts',(80.947216176168,7.62905798695339,132.619440996194));
#67257=CARTESIAN_POINT('Ctrl Pts',(80.9191812762621,7.61010555936394,132.617115978724));
#67258=CARTESIAN_POINT('Ctrl Pts',(80.8789638676492,7.58466694315366,132.613890476227));
#67259=CARTESIAN_POINT('Ctrl Pts',(80.867250037415,7.57745912721672,132.612963624196));
#67260=CARTESIAN_POINT('Ctrl Pts',(80.8469136238374,7.56529019362384,132.611375674988));
#67261=CARTESIAN_POINT('Ctrl Pts',(80.8383335497348,7.56025982151991,132.610712080168));
#67262=CARTESIAN_POINT('Ctrl Pts',(80.8207217280619,7.55014509270155,132.609362661168));
#67263=CARTESIAN_POINT('Ctrl Pts',(80.8116865425432,7.54506757132803,132.608677104587));
#67264=CARTESIAN_POINT('Ctrl Pts',(80.7886903129719,7.53242523036049,132.606948759544));
#67265=CARTESIAN_POINT('Ctrl Pts',(80.7746672163916,7.52497496746674,132.605910059923));
#67266=CARTESIAN_POINT('Ctrl Pts',(80.7192406366863,7.49653616491054,132.601861223339));
#67267=CARTESIAN_POINT('Ctrl Pts',(80.6770719202831,7.47708016938978,132.598904060902));
#67268=CARTESIAN_POINT('Ctrl Pts',(80.5298633247235,7.41648573299649,132.588912002858));
#67269=CARTESIAN_POINT('Ctrl Pts',(80.4214979948379,7.3842610085533,132.582135825225));
#67270=CARTESIAN_POINT('Ctrl Pts',(80.2467533101099,7.35108938536976,132.571192963126));
#67271=CARTESIAN_POINT('Ctrl Pts',(80.1821502317034,7.34270919025295,132.567137837064));
#67272=CARTESIAN_POINT('Ctrl Pts',(80.1021383017193,7.33706504119916,132.561927496987));
#67273=CARTESIAN_POINT('Ctrl Pts',(80.0870328818012,7.3362060981031,132.560935575747));
#67274=CARTESIAN_POINT('Ctrl Pts',(80.0648573137609,7.3352479215985,132.559464514824));
#67275=CARTESIAN_POINT('Ctrl Pts',(80.0577943998456,7.33498776085358,132.558993771697));
#67276=CARTESIAN_POINT('Ctrl Pts',(80.0457810338617,7.33462178050525,132.558188996733));
#67277=CARTESIAN_POINT('Ctrl Pts',(80.040831418933,7.33449307675643,132.557856234753));
#67278=CARTESIAN_POINT('Ctrl Pts',(80.0295620456989,7.33425030825084,132.557095814404));
#67279=CARTESIAN_POINT('Ctrl Pts',(80.0232423093397,7.33415014426926,132.556667416102));
#67280=CARTESIAN_POINT('Ctrl Pts',(80.0058231099533,7.33397320073411,132.555481483936));
#67281=CARTESIAN_POINT('Ctrl Pts',(79.9947234507573,7.33397138501693,132.554720058067));
#67282=CARTESIAN_POINT('Ctrl Pts',(79.9308568333433,7.33459915665192,132.550308949639));
#67283=CARTESIAN_POINT('Ctrl Pts',(79.8781483343874,7.3376246616884,132.54655177365));
#67284=CARTESIAN_POINT('Ctrl Pts',(79.7250433324634,7.35373322060475,132.535450183526));
#67285=CARTESIAN_POINT('Ctrl Pts',(79.6255752407566,7.37346893563222,132.528013862693));
#67286=CARTESIAN_POINT('Ctrl Pts',(79.4584095292679,7.42279417085371,132.515518140212));
#67287=CARTESIAN_POINT('Ctrl Pts',(79.3897350897818,7.44807285472084,132.510381181652));
#67288=CARTESIAN_POINT('Ctrl Pts',(79.3068207310512,7.48495230233739,132.504188110223));
#67289=CARTESIAN_POINT('Ctrl Pts',(79.2908212127828,7.49237520769528,132.50299320216));
#67290=CARTESIAN_POINT('Ctrl Pts',(79.265274118672,7.50472437723302,132.501084777423));
#67291=CARTESIAN_POINT('Ctrl Pts',(79.2556514276604,7.50949118723549,132.500365828569));
#67292=CARTESIAN_POINT('Ctrl Pts',(79.2373424597085,7.51878246756278,132.498997417226));
#67293=CARTESIAN_POINT('Ctrl Pts',(79.2286487099196,7.52329112671427,132.498347438041));
#67294=CARTESIAN_POINT('Ctrl Pts',(79.2088942347118,7.53375803780484,132.496869749779));
#67295=CARTESIAN_POINT('Ctrl Pts',(79.1978600494055,7.539765314201,132.496043810347));
#67296=CARTESIAN_POINT('Ctrl Pts',(79.1685849889021,7.55613534359005,132.493850164165));
#67297=CARTESIAN_POINT('Ctrl Pts',(79.1504697574567,7.56671897498553,132.492490327151));
#67298=CARTESIAN_POINT('Ctrl Pts',(79.0289990837983,7.64079928182422,132.483343087422));
#67299=CARTESIAN_POINT('Ctrl Pts',(78.9326446897258,7.71507748669581,132.475977566467));
#67300=CARTESIAN_POINT('Ctrl Pts',(78.7769423582714,7.86481079633191,132.462777109716));
#67301=CARTESIAN_POINT('Ctrl Pts',(78.7144130612452,7.93614588721792,132.456972520335));
#67302=CARTESIAN_POINT('Ctrl Pts',(78.6512058941246,8.02201572094275,132.450001560231));
#67303=CARTESIAN_POINT('Ctrl Pts',(78.6442262120951,8.03171481164655,132.449214309078));
#67304=CARTESIAN_POINT('Ctrl Pts',(78.6336484468648,8.04675246438208,132.447992506668));
#67305=CARTESIAN_POINT('Ctrl Pts',(78.6299758001279,8.05203844001826,132.447562792655));
#67306=CARTESIAN_POINT('Ctrl Pts',(78.6232309133811,8.06186730250599,132.4467630783));
#67307=CARTESIAN_POINT('Ctrl Pts',(78.6201503620369,8.06640423662196,132.446393641615));
#67308=CARTESIAN_POINT('Ctrl Pts',(78.61313702902,8.07684377994631,132.445542937354));
#67309=CARTESIAN_POINT('Ctrl Pts',(78.6092194980376,8.08275635861927,132.445060696256));
#67310=CARTESIAN_POINT('Ctrl Pts',(78.5967639032098,8.10181835731779,132.443505037225));
#67311=CARTESIAN_POINT('Ctrl Pts',(78.588373953011,8.11506290296182,132.442422743279));
#67312=CARTESIAN_POINT('Ctrl Pts',(78.5325283523124,8.20603724123565,132.434989446076));
#67313=CARTESIAN_POINT('Ctrl Pts',(78.4913328088637,8.28742005575831,132.428352542801));
#67314=CARTESIAN_POINT('Ctrl Pts',(78.4247983181732,8.45083157997319,132.415509623882));
#67315=CARTESIAN_POINT('Ctrl Pts',(78.3987241872377,8.53227695919785,132.409321369037));
#67316=CARTESIAN_POINT('Ctrl Pts',(78.3680020355095,8.6617527578773,132.399941832053));
#67317=CARTESIAN_POINT('Ctrl Pts',(78.3589911652403,8.70859076932037,132.396636476905));
#67318=CARTESIAN_POINT('Ctrl Pts',(78.3497214906526,8.77113624633401,132.392336251937));
#67319=CARTESIAN_POINT('Ctrl Pts',(78.3476572785426,8.78654898576195,132.39128552387));
#67320=CARTESIAN_POINT('Ctrl Pts',(78.3445854612189,8.81221103466813,132.389550395346));
#67321=CARTESIAN_POINT('Ctrl Pts',(78.3434565920573,8.82244455366229,132.388862228165));
#67322=CARTESIAN_POINT('Ctrl Pts',(78.3414309106954,8.84251319908358,132.38751981382));
#67323=CARTESIAN_POINT('Ctrl Pts',(78.3405265445635,8.85234711549764,132.386865356495));
#67324=CARTESIAN_POINT('Ctrl Pts',(78.3385587767958,8.87605391770599,132.385295374785));
#67325=CARTESIAN_POINT('Ctrl Pts',(78.3375816034244,8.8899333674968,132.384382577325));
#67326=CARTESIAN_POINT('Ctrl Pts',(78.3349117757002,8.9361039845083,132.381365790222));
#67327=CARTESIAN_POINT('Ctrl Pts',(78.3339852171911,8.9684332389627,132.379285502678));
#67328=CARTESIAN_POINT('Ctrl Pts',(78.334022550631,9.04912758001036,132.374154844899));
#67329=CARTESIAN_POINT('Ctrl Pts',(78.3361502741554,9.09746277210266,132.371137465754));
#67330=CARTESIAN_POINT('Ctrl Pts',(78.3493322671356,9.24767666778614,132.361827880112));
#67331=CARTESIAN_POINT('Ctrl Pts',(78.3676768809818,9.34866524845633,132.355677482683));
#67332=CARTESIAN_POINT('Ctrl Pts',(78.4072396823514,9.49060039028313,132.346514737682));
#67333=CARTESIAN_POINT('Ctrl Pts',(78.4210455027179,9.53336255103003,132.343680820218));
#67334=CARTESIAN_POINT('Ctrl Pts',(78.4365593734337,9.57550795581125,132.340765796073));
#67335=CARTESIAN_POINT('Ctrl Pts',(78.4365593745624,9.57550795887745,132.531716954706));
#67336=CARTESIAN_POINT('Ctrl Pts',(78.4158153041906,9.51915405124514,132.535390102318));
#67337=CARTESIAN_POINT('Ctrl Pts',(78.3981331275018,9.46171927848792,132.5390813048));
#67338=CARTESIAN_POINT('Ctrl Pts',(78.3781664940499,9.38172466887552,132.544300095684));
#67339=CARTESIAN_POINT('Ctrl Pts',(78.3731815460984,9.35988784635904,132.54573262462));
#67340=CARTESIAN_POINT('Ctrl Pts',(78.365398621124,9.3223188212678,132.548220991885));
#67341=CARTESIAN_POINT('Ctrl Pts',(78.3623839053814,9.30663426281379,132.549266886095));
#67342=CARTESIAN_POINT('Ctrl Pts',(78.3583344197384,9.28379968614592,132.550802957639));
#67343=CARTESIAN_POINT('Ctrl Pts',(78.3571198293399,9.27668190998204,132.551283647918));
#67344=CARTESIAN_POINT('Ctrl Pts',(78.3550723079505,9.26419390574105,132.552130660832));
#67345=CARTESIAN_POINT('Ctrl Pts',(78.3542193240584,9.25882715735029,132.552495857473));
#67346=CARTESIAN_POINT('Ctrl Pts',(78.3524177218625,9.24712284102455,132.553295001798));
#67347=CARTESIAN_POINT('Ctrl Pts',(78.3514794201271,9.24078404445869,132.5537294835));
#67348=CARTESIAN_POINT('Ctrl Pts',(78.3489603434048,9.22306087866001,132.554948689038));
#67349=CARTESIAN_POINT('Ctrl Pts',(78.3474608131118,9.21166558704167,132.555737654615));
#67350=CARTESIAN_POINT('Ctrl Pts',(78.3380833661921,9.13421699267986,132.561130159692));
#67351=CARTESIAN_POINT('Ctrl Pts',(78.3340507254895,9.06776530077335,132.565903956972));
#67352=CARTESIAN_POINT('Ctrl Pts',(78.3338866237805,8.85057454433804,132.581651623519));
#67353=CARTESIAN_POINT('Ctrl Pts',(78.3542177053222,8.70053264545152,132.592678381093));
#67354=CARTESIAN_POINT('Ctrl Pts',(78.399968049702,8.53537156616134,132.604461594223));
#67355=CARTESIAN_POINT('Ctrl Pts',(78.4058459399267,8.51558827180375,132.605868735997));
#67356=CARTESIAN_POINT('Ctrl Pts',(78.4158613425301,8.48403869741446,132.608106732611));
#67357=CARTESIAN_POINT('Ctrl Pts',(78.4197658644806,8.47220132299353,132.608945050402));
#67358=CARTESIAN_POINT('Ctrl Pts',(78.4269697471796,8.45115810670466,132.610433193698));
#67359=CARTESIAN_POINT('Ctrl Pts',(78.4302179670185,8.44193550905234,132.611084665797));
#67360=CARTESIAN_POINT('Ctrl Pts',(78.4372192219823,8.42260192085466,132.612449055518));
#67361=CARTESIAN_POINT('Ctrl Pts',(78.4409896335776,8.41249766932211,132.613161361915));
#67362=CARTESIAN_POINT('Ctrl Pts',(78.4512640226325,8.38575913052174,132.615044776518));
#67363=CARTESIAN_POINT('Ctrl Pts',(78.4579379342537,8.36919131360153,132.616210178117));
#67364=CARTESIAN_POINT('Ctrl Pts',(78.4948474479269,8.28165297370368,132.622364571122));
#67365=CARTESIAN_POINT('Ctrl Pts',(78.5297202375517,8.21273493904726,132.627192781898));
#67366=CARTESIAN_POINT('Ctrl Pts',(78.6234638765606,8.05559383548338,132.638466358107));
#67367=CARTESIAN_POINT('Ctrl Pts',(78.6862116460568,7.97009100919123,132.64481399731));
#67368=CARTESIAN_POINT('Ctrl Pts',(78.7863054113061,7.85785818900112,132.654221210498));
#67369=CARTESIAN_POINT('Ctrl Pts',(78.8172908938107,7.82580202834366,132.657055872879));
#67370=CARTESIAN_POINT('Ctrl Pts',(78.8572844312582,7.78761707820762,132.660681139094));
#67371=CARTESIAN_POINT('Ctrl Pts',(78.8651192803846,7.78027996758507,132.661389843263));
#67372=CARTESIAN_POINT('Ctrl Pts',(78.8775723371469,7.76884189568672,132.662515013205));
#67373=CARTESIAN_POINT('Ctrl Pts',(78.8821435488544,7.76468988197728,132.662927769796));
#67374=CARTESIAN_POINT('Ctrl Pts',(78.8908594572922,7.75686124980466,132.663714512337));
#67375=CARTESIAN_POINT('Ctrl Pts',(78.8949995433564,7.75317977126558,132.664088130795));
#67376=CARTESIAN_POINT('Ctrl Pts',(78.9049152154767,7.74445065761625,132.664982647011));
#67377=CARTESIAN_POINT('Ctrl Pts',(78.9107073957882,7.73942217491663,132.66550490769));
#67378=CARTESIAN_POINT('Ctrl Pts',(78.930670049947,7.72233191020739,132.667303349307));
#67379=CARTESIAN_POINT('Ctrl Pts',(78.9450072054279,7.71046813870667,132.66859238136));
#67380=CARTESIAN_POINT('Ctrl Pts',(78.981044202202,7.68165131457063,132.671819860232));
#67381=CARTESIAN_POINT('Ctrl Pts',(79.00297095642,7.66499172682218,132.673772646311));
#67382=CARTESIAN_POINT('Ctrl Pts',(79.104958054512,7.59141779231284,132.682772151182));
#67383=CARTESIAN_POINT('Ctrl Pts',(79.18954183518,7.54110946450824,132.68999384812));
#67384=CARTESIAN_POINT('Ctrl Pts',(79.3572778212561,7.46045801028231,132.703433474745));
#67385=CARTESIAN_POINT('Ctrl Pts',(79.4393906520102,7.42869387562057,132.709657774871));
#67386=CARTESIAN_POINT('Ctrl Pts',(79.5415669179649,7.39820565346661,132.716946633924));
#67387=CARTESIAN_POINT('Ctrl Pts',(79.5595840734671,7.39315841462845,132.718215799916));
#67388=CARTESIAN_POINT('Ctrl Pts',(79.5882910603853,7.38563572707629,132.72021332017));
#67389=CARTESIAN_POINT('Ctrl Pts',(79.5989264398569,7.38296064798719,132.720948051151));
#67390=CARTESIAN_POINT('Ctrl Pts',(79.6181099836043,7.37833638960376,132.72226404378));
#67391=CARTESIAN_POINT('Ctrl Pts',(79.6266485037331,7.37634932477325,132.722846501165));
#67392=CARTESIAN_POINT('Ctrl Pts',(79.6467822340523,7.37183107322512,132.724212416469));
#67393=CARTESIAN_POINT('Ctrl Pts',(79.6583896953554,7.36935618351344,132.724994051237));
#67394=CARTESIAN_POINT('Ctrl Pts',(79.6926342373903,7.36243643230209,132.727283650897));
#67395=CARTESIAN_POINT('Ctrl Pts',(79.7153389039482,7.35833733830105,132.728780659801));
#67396=CARTESIAN_POINT('Ctrl Pts',(79.8216456865524,7.34141667968682,132.735703231742));
#67397=CARTESIAN_POINT('Ctrl Pts',(79.9060648788887,7.33450082558079,132.740943671897));
#67398=CARTESIAN_POINT('Ctrl Pts',(80.079759781727,7.33352626246292,132.75158616841));
#67399=CARTESIAN_POINT('Ctrl Pts',(80.1687582859573,7.3401761214123,132.756965490504));
#67400=CARTESIAN_POINT('Ctrl Pts',(80.300961109487,7.36079997074128,132.765334522732));
#67401=CARTESIAN_POINT('Ctrl Pts',(80.3448301471471,7.36946458966138,132.768177321253));
#67402=CARTESIAN_POINT('Ctrl Pts',(80.3987399752409,7.38238514037267,132.771811771643));
#67403=CARTESIAN_POINT('Ctrl Pts',(80.4091618593135,7.38498979572191,132.772521023632));
#67404=CARTESIAN_POINT('Ctrl Pts',(80.4255356819421,7.38925062710553,132.773646868134));
#67405=CARTESIAN_POINT('Ctrl Pts',(80.4315050567109,7.39083949159219,132.774059744041));
#67406=CARTESIAN_POINT('Ctrl Pts',(80.4428107206027,7.39391614325671,132.774846564453));
#67407=CARTESIAN_POINT('Ctrl Pts',(80.4481485987269,7.39539739533989,132.775220140005));
#67408=CARTESIAN_POINT('Ctrl Pts',(80.4608560055704,7.3989920303435,132.776114345397));
#67409=CARTESIAN_POINT('Ctrl Pts',(80.4682184572554,7.40112969653713,132.776636335574));
#67410=CARTESIAN_POINT('Ctrl Pts',(80.4933772252836,7.40862314091016,132.778432840137));
#67411=CARTESIAN_POINT('Ctrl Pts',(80.5110978173229,7.41422563282207,132.779720169746));
#67412=CARTESIAN_POINT('Ctrl Pts',(80.5547852935542,7.42884604008863,132.782942437674));
#67413=CARTESIAN_POINT('Ctrl Pts',(80.5806292618344,7.43821224947295,132.784891660076));
#67414=CARTESIAN_POINT('Ctrl Pts',(80.6973664294046,7.48381731998525,132.79386016481));
#67415=CARTESIAN_POINT('Ctrl Pts',(80.7851896293361,7.52738084349259,132.801053515718));
#67416=CARTESIAN_POINT('Ctrl Pts',(80.9440628477874,7.62446181479534,132.814500316631));
#67417=CARTESIAN_POINT('Ctrl Pts',(81.0156701985821,7.67645230122932,132.820757441908));
#67418=CARTESIAN_POINT('Ctrl Pts',(81.0970494899205,7.74605075065364,132.828077414278));
#67419=CARTESIAN_POINT('Ctrl Pts',(81.1110679049416,7.75845480812324,132.82934710576));
#67420=CARTESIAN_POINT('Ctrl Pts',(81.1329650929628,7.77849830523119,132.831345256668));
#67421=CARTESIAN_POINT('Ctrl Pts',(81.1409821960153,7.78598355425947,132.8320800997));
#67422=CARTESIAN_POINT('Ctrl Pts',(81.1552730838317,7.799593007555,132.833396189896));
#67423=CARTESIAN_POINT('Ctrl Pts',(81.1615734909718,7.80568853483234,132.833978633909));
#67424=CARTESIAN_POINT('Ctrl Pts',(81.1762878604293,7.8201510018893,132.835344384885));
#67425=CARTESIAN_POINT('Ctrl Pts',(81.1846612032995,7.82855873620775,132.836125870133));
#67426=CARTESIAN_POINT('Ctrl Pts',(81.2090387759521,7.85356515834883,132.838414560437));
#67427=CARTESIAN_POINT('Ctrl Pts',(81.2247894917678,7.87040786441079,132.839910823041));
#67428=CARTESIAN_POINT('Ctrl Pts',(81.296596289534,7.9504614586341,132.846826731609));
#67429=CARTESIAN_POINT('Ctrl Pts',(81.348144591726,8.01755322883263,132.852061692706));
#67430=CARTESIAN_POINT('Ctrl Pts',(81.4430437050401,8.16269090499177,132.862686835265));
#67431=CARTESIAN_POINT('Ctrl Pts',(81.4856639088488,8.24088027471099,132.868054516755));
#67432=CARTESIAN_POINT('Ctrl Pts',(81.5401297620792,8.36315096492667,132.876424772968));
#67433=CARTESIAN_POINT('Ctrl Pts',(81.5567488133593,8.40492964441232,132.879282540408));
#67434=CARTESIAN_POINT('Ctrl Pts',(81.5752319570369,8.45749063800833,132.882935024104));
#67435=CARTESIAN_POINT('Ctrl Pts',(81.5787079938222,8.46769070877485,132.883646453979));
#67436=CARTESIAN_POINT('Ctrl Pts',(81.5840228006412,8.48379653591062,132.884774980131));
#67437=CARTESIAN_POINT('Ctrl Pts',(81.5859281190037,8.48968024971342,132.885188330221));
#67438=CARTESIAN_POINT('Ctrl Pts',(81.5894772090753,8.50085186032292,132.885975462202));
#67439=CARTESIAN_POINT('Ctrl Pts',(81.5911274321993,8.50613751481145,132.886348869353));
#67440=CARTESIAN_POINT('Ctrl Pts',(81.5949950355936,8.51874603587493,132.887241849074));
#67441=CARTESIAN_POINT('Ctrl Pts',(81.5971883567455,8.52607607266579,132.887762771786));
#67442=CARTESIAN_POINT('Ctrl Pts',(81.6045093512998,8.5511708333037,132.889551648223));
#67443=CARTESIAN_POINT('Ctrl Pts',(81.6093915283186,8.56900496838309,132.890832276323));
#67444=CARTESIAN_POINT('Ctrl Pts',(81.6207432476791,8.61335765598293,132.894034057287));
#67445=CARTESIAN_POINT('Ctrl Pts',(81.6268596610508,8.63996048416184,132.895969278331));
#67446=CARTESIAN_POINT('Ctrl Pts',(81.6516012192961,8.76113097272919,132.904817256898));
#67447=CARTESIAN_POINT('Ctrl Pts',(81.6626520440427,8.85705548287418,132.9119005437));
#67448=CARTESIAN_POINT('Ctrl Pts',(81.6678678671305,9.04344174628777,132.925375603963));
#67449=CARTESIAN_POINT('Ctrl Pts',(81.6630809982746,9.13355432024879,132.931760868367));
#67450=CARTESIAN_POINT('Ctrl Pts',(81.6485207269419,9.24142648951733,132.939202037549));
#67451=CARTESIAN_POINT('Ctrl Pts',(81.6457000626636,9.2599590170741,132.940473640124));
#67452=CARTESIAN_POINT('Ctrl Pts',(81.6407330911091,9.28925999589201,132.942474084478));
#67453=CARTESIAN_POINT('Ctrl Pts',(81.6387921577502,9.30006115235657,132.943209334939));
#67454=CARTESIAN_POINT('Ctrl Pts',(81.6351091696299,9.3194539624201,132.944525780391));
#67455=CARTESIAN_POINT('Ctrl Pts',(81.6334057748133,9.32805245089953,132.945108176281));
#67456=CARTESIAN_POINT('Ctrl Pts',(81.6292387070813,9.34824965727235,132.946473332182));
#67457=CARTESIAN_POINT('Ctrl Pts',(81.626718893194,9.35983641161602,132.947254275684));
#67458=CARTESIAN_POINT('Ctrl Pts',(81.618945099474,9.39383043447905,132.949539672752));
#67459=CARTESIAN_POINT('Ctrl Pts',(81.6133501500741,9.41615744984906,132.951033232815));
#67460=CARTESIAN_POINT('Ctrl Pts',(81.5851541067631,9.51954074054812,132.957925055547));
#67461=CARTESIAN_POINT('Ctrl Pts',(81.5568947983073,9.59892996510389,132.96314021144));
#67462=CARTESIAN_POINT('Ctrl Pts',(81.486972424395,9.75647134086693,132.973702274399));
#67463=CARTESIAN_POINT('Ctrl Pts',(81.4448467058316,9.83411769014553,132.979027543099));
#67464=CARTESIAN_POINT('Ctrl Pts',(81.3717116908379,9.94661376218597,132.987411067292));
#67465=CARTESIAN_POINT('Ctrl Pts',(81.3450645485001,9.98410929651989,132.990332342853));
#67466=CARTESIAN_POINT('Ctrl Pts',(81.3102761597338,10.0290041139942,132.994055219915));
#67467=CARTESIAN_POINT('Ctrl Pts',(81.3035655322302,10.0374921538753,132.994769510685));
#67468=CARTESIAN_POINT('Ctrl Pts',(81.2928842066497,10.0507353597904,132.995901559221));
#67469=CARTESIAN_POINT('Ctrl Pts',(81.2889687111907,10.0555349480552,132.996315531793));
#67470=CARTESIAN_POINT('Ctrl Pts',(81.2815042354324,10.0645813849687,132.997103077801));
#67471=CARTESIAN_POINT('Ctrl Pts',(81.2779607444216,10.0688325231977,132.997476268929));
#67472=CARTESIAN_POINT('Ctrl Pts',(81.2694808793058,10.0789033944355,132.998367662583));
#67473=CARTESIAN_POINT('Ctrl Pts',(81.2645256185513,10.084706961251,132.998887202043));
#67474=CARTESIAN_POINT('Ctrl Pts',(81.2475082721929,10.1043624776593,133.000666231312));
#67475=CARTESIAN_POINT('Ctrl Pts',(81.2352575425769,10.1180483466645,133.001938214848));
#67476=CARTESIAN_POINT('Ctrl Pts',(81.2044133177024,10.1513800982963,133.005113628517));
#67477=CARTESIAN_POINT('Ctrl Pts',(81.1855631956721,10.1707806438628,133.007030851371));
#67478=CARTESIAN_POINT('Ctrl Pts',(81.0987425745169,10.2558890770279,133.015726770152));
#67479=CARTESIAN_POINT('Ctrl Pts',(81.0257261485521,10.3161984274356,133.022671525339));
#67480=CARTESIAN_POINT('Ctrl Pts',(80.8721094917607,10.4224963304983,133.036182186964));
#67481=CARTESIAN_POINT('Ctrl Pts',(80.7919880086041,10.4686152851551,133.042729455884));
#67482=CARTESIAN_POINT('Ctrl Pts',(80.6914477481183,10.5158524799551,133.050323749649));
#67483=CARTESIAN_POINT('Ctrl Pts',(80.6743149201014,10.5235511701283,133.051597922004));
#67484=CARTESIAN_POINT('Ctrl Pts',(80.6469634889915,10.5352898225739,133.053601450012));
#67485=CARTESIAN_POINT('Ctrl Pts',(80.6368292535379,10.5395210642342,133.054337248131));
#67486=CARTESIAN_POINT('Ctrl Pts',(80.6185331535562,10.5469484635262,133.055654172333));
#67487=CARTESIAN_POINT('Ctrl Pts',(80.6103865831932,10.5501809684458,133.056236504754));
#67488=CARTESIAN_POINT('Ctrl Pts',(80.591170014908,10.5576310007113,133.057600866738));
#67489=CARTESIAN_POINT('Ctrl Pts',(80.5800796958838,10.561795082413,133.058381086744));
#67490=CARTESIAN_POINT('Ctrl Pts',(80.5473686047823,10.5736806046241,133.060662089585));
#67491=CARTESIAN_POINT('Ctrl Pts',(80.5256310053261,10.5810740539564,133.062152044061));
#67492=CARTESIAN_POINT('Ctrl Pts',(80.4239698308709,10.6133227661132,133.069011839254));
#67493=CARTESIAN_POINT('Ctrl Pts',(80.342394898151,10.6325834949729,133.074200659079));
#67494=CARTESIAN_POINT('Ctrl Pts',(80.1735305712101,10.6592332406143,133.084678021482));
#67495=CARTESIAN_POINT('Ctrl Pts',(80.0864208569186,10.6660425575278,133.089946105605));
#67496=CARTESIAN_POINT('Ctrl Pts',(79.9518613333301,10.6659766059245,133.098344000836));
#67497=CARTESIAN_POINT('Ctrl Pts',(79.904566299961,10.6639371671559,133.101346949218));
#67498=CARTESIAN_POINT('Ctrl Pts',(79.8465579274791,10.6589546537889,133.105162493006));
#67499=CARTESIAN_POINT('Ctrl Pts',(79.8356984302451,10.6579143498844,133.105882533594));
#67500=CARTESIAN_POINT('Ctrl Pts',(79.8186712560455,10.6561142755856,133.107021660441));
#67501=CARTESIAN_POINT('Ctrl Pts',(79.8124960503494,10.6554264927497,133.107436882593));
#67502=CARTESIAN_POINT('Ctrl Pts',(79.8008336670123,10.6540614677923,133.10822527644));
#67503=CARTESIAN_POINT('Ctrl Pts',(79.7953458341789,10.653391434642,133.108598050728));
#67504=CARTESIAN_POINT('Ctrl Pts',(79.7823299136031,10.6517364729172,133.109486336782));
#67505=CARTESIAN_POINT('Ctrl Pts',(79.7748051027522,10.6507273836479,133.110003159542));
#67506=CARTESIAN_POINT('Ctrl Pts',(79.7493361657147,10.6471345756428,133.111762971197));
#67507=CARTESIAN_POINT('Ctrl Pts',(79.7314281207907,10.6443095046291,133.113018105082));
#67508=CARTESIAN_POINT('Ctrl Pts',(79.6873970552532,10.6366249795273,133.116142316988));
#67509=CARTESIAN_POINT('Ctrl Pts',(79.6613378592204,10.6314318013803,133.118024660605));
#67510=CARTESIAN_POINT('Ctrl Pts',(79.5465476998577,10.6056873085211,133.126434521699));
#67511=CARTESIAN_POINT('Ctrl Pts',(79.4594659785083,10.5785034939415,133.133119685991));
#67512=CARTESIAN_POINT('Ctrl Pts',(79.2854473896917,10.5080824350587,133.146715054857));
#67513=CARTESIAN_POINT('Ctrl Pts',(79.1991638130289,10.4640919567255,133.153585283214));
#67514=CARTESIAN_POINT('Ctrl Pts',(79.1012915543917,10.4029361026397,133.161474505971));
#67515=CARTESIAN_POINT('Ctrl Pts',(79.0855806718509,10.3927468974138,133.162744706175));
#67516=CARTESIAN_POINT('Ctrl Pts',(79.0609429621842,10.3761715759078,133.164743467601));
#67517=CARTESIAN_POINT('Ctrl Pts',(79.0519021111862,10.3699586598858,133.165478419101));
#67518=CARTESIAN_POINT('Ctrl Pts',(79.0351461343413,10.3581985463208,133.166843640303));
#67519=CARTESIAN_POINT('Ctrl Pts',(79.0274158771078,10.352673797925,133.167474726944));
#67520=CARTESIAN_POINT('Ctrl Pts',(79.0192318271128,10.3467182984905,133.168144321731));
#67521=CARTESIAN_POINT('Ctrl Pts',(79.0187306902262,10.3463531951666,133.168185329153));
#67522=CARTESIAN_POINT('Ctrl Pts',(79.0177834489313,10.3456622726275,133.168262851953));
#67523=CARTESIAN_POINT('Ctrl Pts',(79.0173373026378,10.3453365112047,133.168299369537));
#67524=CARTESIAN_POINT('Ctrl Pts',(79.0164831042801,10.3447121519121,133.168369295703));
#67525=CARTESIAN_POINT('Ctrl Pts',(79.0160750260463,10.3444135901194,133.16840270566));
#67526=CARTESIAN_POINT('Ctrl Pts',(79.01528530826,10.3438352576828,133.168467368711));
#67527=CARTESIAN_POINT('Ctrl Pts',(79.0149036519001,10.3435555101599,133.168498622686));
#67528=CARTESIAN_POINT('Ctrl Pts',(79.0141582335067,10.3430086429776,133.168559672112));
#67529=CARTESIAN_POINT('Ctrl Pts',(79.0137944607681,10.3427415380721,133.168589468123));
#67530=CARTESIAN_POINT('Ctrl Pts',(79.0130781715019,10.342215145173,133.168648144478));
#67531=CARTESIAN_POINT('Ctrl Pts',(79.0127256485115,10.3419558660371,133.168677025161));
#67532=CARTESIAN_POINT('Ctrl Pts',(79.0120264045867,10.3414411504904,133.168734317195));
#67533=CARTESIAN_POINT('Ctrl Pts',(79.0116796804819,10.3411857184935,133.16876272871));
#67534=CARTESIAN_POINT('Ctrl Pts',(79.0109872994469,10.3406752263985,133.168819470176));
#67535=CARTESIAN_POINT('Ctrl Pts',(79.0106416420438,10.3404201669912,133.168847800151));
#67536=CARTESIAN_POINT('Ctrl Pts',(79.0099470572966,10.3399072202583,133.168904734023));
#67537=CARTESIAN_POINT('Ctrl Pts',(79.0095981319571,10.3396493302479,133.168933337814));
#67538=CARTESIAN_POINT('Ctrl Pts',(78.998242932863,10.3312498645064,133.169864299206));
#67539=CARTESIAN_POINT('Ctrl Pts',(78.9873370692588,10.3229728759129,133.170761420092));
#67540=CARTESIAN_POINT('Ctrl Pts',(78.9459345373154,10.2907385122996,133.17418046036));
#67541=CARTESIAN_POINT('Ctrl Pts',(78.9161743683087,10.2658523905039,133.176665711008));
#67542=CARTESIAN_POINT('Ctrl Pts',(78.8418332495801,10.1991409403637,133.182981079369));
#67543=CARTESIAN_POINT('Ctrl Pts',(78.798635466005,10.1558604189858,133.186755962853));
#67544=CARTESIAN_POINT('Ctrl Pts',(78.6995289695442,10.0449905032841,133.195869447882));
#67545=CARTESIAN_POINT('Ctrl Pts',(78.6463923762766,9.9751794567776,133.201158779527));
#67546=CARTESIAN_POINT('Ctrl Pts',(78.5736601763062,9.86214986167906,133.209550700495));
#67547=CARTESIAN_POINT('Ctrl Pts',(78.5500002320452,9.82173443354892,133.212522689878));
#67548=CARTESIAN_POINT('Ctrl Pts',(78.5229781739841,9.77076646661656,133.216303496342));
#67549=CARTESIAN_POINT('Ctrl Pts',(78.517975303888,9.76110262464493,133.217021778711));
#67550=CARTESIAN_POINT('Ctrl Pts',(78.5102679143547,9.7458504186802,133.218158741245));
#67551=CARTESIAN_POINT('Ctrl Pts',(78.5074992479223,9.740294560261,133.218573581508));
#67552=CARTESIAN_POINT('Ctrl Pts',(78.5023227456048,9.7297598427144,133.219361713918));
#67553=CARTESIAN_POINT('Ctrl Pts',(78.4999085718602,9.72478430576832,133.219734613259));
#67554=CARTESIAN_POINT('Ctrl Pts',(78.4942339071059,9.71293919491742,133.220623838431));
#67555=CARTESIAN_POINT('Ctrl Pts',(78.4909956222077,9.70605920738418,133.221141483102));
#67556=CARTESIAN_POINT('Ctrl Pts',(78.4801663088353,9.68263667605853,133.222907091899));
#67557=CARTESIAN_POINT('Ctrl Pts',(78.4727996201629,9.66599265205912,133.224167305683));
#67558=CARTESIAN_POINT('Ctrl Pts',(78.4554074491306,9.62489074762251,133.22728720334));
#67559=CARTESIAN_POINT('Ctrl Pts',(78.4456887246787,9.60030900062951,133.229159777037));
#67560=CARTESIAN_POINT('Ctrl Pts',(78.4365593737642,9.57550795670914,133.231048988662));
#67561=CARTESIAN_POINT('Origin',(80.,9.,134.));
#67562=CARTESIAN_POINT('',(78.4365594251401,9.5755080962782,133.933539779158));
#67563=CARTESIAN_POINT('',(78.4365593568557,9.5755079107748,133.73811642446));
#67564=CARTESIAN_POINT('',(78.4365593737638,9.57550795670799,134.));
#67565=CARTESIAN_POINT('',(78.3340006446003,8.99853445987493,133.077925722171));
#67566=CARTESIAN_POINT('Ctrl Pts',(78.4365593568556,9.5755079107748,133.73811642446));
#67567=CARTESIAN_POINT('Ctrl Pts',(78.4533138724376,9.62102368931857,133.734685168399));
#67568=CARTESIAN_POINT('Ctrl Pts',(78.4720530953956,9.66579994160906,133.731307672136));
#67569=CARTESIAN_POINT('Ctrl Pts',(78.5003899641021,9.72598161132062,133.726765519516));
#67570=CARTESIAN_POINT('Ctrl Pts',(78.5083159725748,9.74213096291014,133.725546268158));
#67571=CARTESIAN_POINT('Ctrl Pts',(78.5214232527383,9.76777844344069,133.723608574949));
#67572=CARTESIAN_POINT('Ctrl Pts',(78.5264379851748,9.77735959102491,133.722884398203));
#67573=CARTESIAN_POINT('Ctrl Pts',(78.5361622240781,9.79550643991229,133.721511936369));
#67574=CARTESIAN_POINT('Ctrl Pts',(78.5408544996839,9.80408080813696,133.720863078475));
#67575=CARTESIAN_POINT('Ctrl Pts',(78.5517810140162,9.82363657562874,133.719382073356));
#67576=CARTESIAN_POINT('Ctrl Pts',(78.5580652359074,9.83458947440356,133.718551752309));
#67577=CARTESIAN_POINT('Ctrl Pts',(78.5782078655825,9.86878971091871,133.715955453846));
#67578=CARTESIAN_POINT('Ctrl Pts',(78.5925089713435,9.89177215287589,133.7142054799));
#67579=CARTESIAN_POINT('Ctrl Pts',(78.6585091620241,9.9922910884067,133.706509917165));
#67580=CARTESIAN_POINT('Ctrl Pts',(78.7161010395514,10.0657604531942,133.700783869137));
#67581=CARTESIAN_POINT('Ctrl Pts',(78.8564192981992,10.2167724206075,133.688188810723));
#67582=CARTESIAN_POINT('Ctrl Pts',(78.9415014299337,10.291466357208,133.681367664958));
#67583=CARTESIAN_POINT('Ctrl Pts',(79.0451948644778,10.3653243084814,133.67308643364));
#67584=CARTESIAN_POINT('Ctrl Pts',(79.0570298032732,10.3735248406953,133.672141472186));
#67585=CARTESIAN_POINT('Ctrl Pts',(79.0747155131244,10.3854431192072,133.670727260796));
#67586=CARTESIAN_POINT('Ctrl Pts',(79.0804859589658,10.3892796486917,133.67026551086));
#67587=CARTESIAN_POINT('Ctrl Pts',(79.0908495931465,10.3960771474094,133.669435312735));
#67588=CARTESIAN_POINT('Ctrl Pts',(79.0954336441448,10.3990516680198,133.669067769173));
#67589=CARTESIAN_POINT('Ctrl Pts',(79.1056325019292,10.4055984715684,133.668249257963));
#67590=CARTESIAN_POINT('Ctrl Pts',(79.1112540481959,10.4091596482241,133.667797611525));
#67591=CARTESIAN_POINT('Ctrl Pts',(79.1279243777179,10.4195806572977,133.666457195611));
#67592=CARTESIAN_POINT('Ctrl Pts',(79.1390320226525,10.4263447162064,133.665562660636));
#67593=CARTESIAN_POINT('Ctrl Pts',(79.1649197523285,10.4416966258473,133.663476619749));
#67594=CARTESIAN_POINT('Ctrl Pts',(79.1797549276294,10.4501883162241,133.66228029872));
#67595=CARTESIAN_POINT('Ctrl Pts',(79.2317890482612,10.4789189353703,133.658087669552));
#67596=CARTESIAN_POINT('Ctrl Pts',(79.2696253079559,10.4979658318823,133.655045411505));
#67597=CARTESIAN_POINT('Ctrl Pts',(79.4026924223626,10.5587116994226,133.64445562282));
#67598=CARTESIAN_POINT('Ctrl Pts',(79.5010822267611,10.5929352068715,133.636830784168));
#67599=CARTESIAN_POINT('Ctrl Pts',(79.6614132789467,10.6323773405461,133.625069981759));
#67600=CARTESIAN_POINT('Ctrl Pts',(79.7215692931465,10.6437076041462,133.620793936258));
#67601=CARTESIAN_POINT('Ctrl Pts',(79.7994482501544,10.6539761184316,133.615435179758));
#67602=CARTESIAN_POINT('Ctrl Pts',(79.8167124446517,10.6559781751258,133.614258088955));
#67603=CARTESIAN_POINT('Ctrl Pts',(79.8446351488687,10.6587742124256,133.612371093816));
#67604=CARTESIAN_POINT('Ctrl Pts',(79.8552751094234,10.6597363766622,133.611655974854));
#67605=CARTESIAN_POINT('Ctrl Pts',(79.8757008890263,10.6613855499246,133.610290401294));
#67606=CARTESIAN_POINT('Ctrl Pts',(79.8854849257758,10.6620886015135,133.609639472008));
#67607=CARTESIAN_POINT('Ctrl Pts',(79.9081435129188,10.6635157489398,133.608139079746));
#67608=CARTESIAN_POINT('Ctrl Pts',(79.9210215096234,10.6641768760487,133.607291615217));
#67609=CARTESIAN_POINT('Ctrl Pts',(79.9624541130472,10.665821891718,133.604580927236));
#67610=CARTESIAN_POINT('Ctrl Pts',(79.9910277185034,10.6662208503361,133.602735846403));
#67611=CARTESIAN_POINT('Ctrl Pts',(80.1115597627914,10.664802809602,133.595034966983));
#67612=CARTESIAN_POINT('Ctrl Pts',(80.2032771081441,10.6561083420529,133.58938773939));
#67613=CARTESIAN_POINT('Ctrl Pts',(80.4037797510479,10.6201845954713,133.576943439944));
#67614=CARTESIAN_POINT('Ctrl Pts',(80.5114673801259,10.5894748100621,133.570191623868));
#67615=CARTESIAN_POINT('Ctrl Pts',(80.6287550814395,10.5428655388323,133.56198388557));
#67616=CARTESIAN_POINT('Ctrl Pts',(80.642183530831,10.5373247220364,133.561030685729));
#67617=CARTESIAN_POINT('Ctrl Pts',(80.6619303445797,10.5288729763663,133.55960648604));
#67618=CARTESIAN_POINT('Ctrl Pts',(80.6683061046653,10.5260967548224,133.559143140018));
#67619=CARTESIAN_POINT('Ctrl Pts',(80.6796617030663,10.5210673371442,133.558311287544));
#67620=CARTESIAN_POINT('Ctrl Pts',(80.6846480901018,10.5188294392895,133.557943702163));
#67621=CARTESIAN_POINT('Ctrl Pts',(80.6956620371813,10.5138211038266,133.557126602584));
#67622=CARTESIAN_POINT('Ctrl Pts',(80.7016840283085,10.5110392201949,133.556676424345));
#67623=CARTESIAN_POINT('Ctrl Pts',(80.7193684552058,10.5027413167849,133.555344657496));
#67624=CARTESIAN_POINT('Ctrl Pts',(80.7309833048455,10.4971258537808,133.554457410651));
#67625=CARTESIAN_POINT('Ctrl Pts',(80.7576742745415,10.4838368663137,133.552391268937));
#67626=CARTESIAN_POINT('Ctrl Pts',(80.7727008972842,10.4760675550503,133.551207679084));
#67627=CARTESIAN_POINT('Ctrl Pts',(80.8243225568881,10.448373033997,133.547076835809));
#67628=CARTESIAN_POINT('Ctrl Pts',(80.8602849963634,10.4273056449414,133.544084930005));
#67629=CARTESIAN_POINT('Ctrl Pts',(81.0035553774474,10.3359927194376,133.531789739167));
#67630=CARTESIAN_POINT('Ctrl Pts',(81.1033920987968,10.2548044069588,133.522371856285));
#67631=CARTESIAN_POINT('Ctrl Pts',(81.222315669571,10.1328162409611,133.510411830442));
#67632=CARTESIAN_POINT('Ctrl Pts',(81.2505512563477,10.1015672157563,133.507500443784));
#67633=CARTESIAN_POINT('Ctrl Pts',(81.287427847411,10.0575070721881,133.503594197743));
#67634=CARTESIAN_POINT('Ctrl Pts',(81.2971179331146,10.0455987590924,133.502557106785));
#67635=CARTESIAN_POINT('Ctrl Pts',(81.3123683107769,10.0263189588971,133.500907091755));
#67636=CARTESIAN_POINT('Ctrl Pts',(81.3180341397578,10.0190324827392,133.500289980404));
#67637=CARTESIAN_POINT('Ctrl Pts',(81.3296378919313,10.0038509129828,133.499017364066));
#67638=CARTESIAN_POINT('Ctrl Pts',(81.335566747811,9.99594932022478,133.498362232117));
#67639=CARTESIAN_POINT('Ctrl Pts',(81.3493443699952,9.97724311005353,133.496827857507));
#67640=CARTESIAN_POINT('Ctrl Pts',(81.3571342766735,9.9663958284583,133.49595091345));
#67641=CARTESIAN_POINT('Ctrl Pts',(81.3827439718924,9.92981440211319,133.493034652759));
#67642=CARTESIAN_POINT('Ctrl Pts',(81.3999694987182,9.90367102323536,133.491017685084));
#67643=CARTESIAN_POINT('Ctrl Pts',(81.4400596235266,9.83892533369479,133.486167047121));
#67644=CARTESIAN_POINT('Ctrl Pts',(81.4621218896997,9.79985464409008,133.483360052284));
#67645=CARTESIAN_POINT('Ctrl Pts',(81.5152312361153,9.69624243644612,133.476151763462));
#67646=CARTESIAN_POINT('Ctrl Pts',(81.5437424461656,9.63050677051844,133.471806924921));
#67647=CARTESIAN_POINT('Ctrl Pts',(81.5756433514638,9.54168600879277,133.466032482952));
#67648=CARTESIAN_POINT('Ctrl Pts',(81.5829078849972,9.52007528178697,133.464634395126));
#67649=CARTESIAN_POINT('Ctrl Pts',(81.6092253763279,9.43611840251818,133.459207297491));
#67650=CARTESIAN_POINT('Ctrl Pts',(81.6250541268509,9.37283053315452,133.455126576894));
#67651=CARTESIAN_POINT('Ctrl Pts',(81.639258153691,9.29752325179486,133.450112335241));
#67652=CARTESIAN_POINT('Ctrl Pts',(81.6412662424835,9.28623850756035,133.449356803423));
#67653=CARTESIAN_POINT('Ctrl Pts',(81.6442141586173,9.26862015119077,133.448169494538));
#67654=CARTESIAN_POINT('Ctrl Pts',(81.6452342252854,9.26230006776009,133.447742036189));
#67655=CARTESIAN_POINT('Ctrl Pts',(81.6470532161736,9.25060180701274,133.446947707024));
#67656=CARTESIAN_POINT('Ctrl Pts',(81.6478622696715,9.24522540570564,133.446581403729));
#67657=CARTESIAN_POINT('Ctrl Pts',(81.6496865516487,9.23268567794725,133.445724220559));
#67658=CARTESIAN_POINT('Ctrl Pts',(81.6506814460104,9.22551962736021,133.445232240536));
#67659=CARTESIAN_POINT('Ctrl Pts',(81.6537323062779,9.20244223321678,133.443641527536));
#67660=CARTESIAN_POINT('Ctrl Pts',(81.6556050439919,9.18650814890319,133.442533504518));
#67661=CARTESIAN_POINT('Ctrl Pts',(81.6595538068366,9.14813777846912,133.439845912231));
#67662=CARTESIAN_POINT('Ctrl Pts',(81.6614053059014,9.1256819228667,133.438257154254));
#67663=CARTESIAN_POINT('Ctrl Pts',(81.6669297984497,9.03666611442462,133.431913202917));
#67664=CARTESIAN_POINT('Ctrl Pts',(81.6670619414313,8.96995118471119,133.427059445446));
#67665=CARTESIAN_POINT('Ctrl Pts',(81.6562298535306,8.78342873645697,133.413459104192));
#67666=CARTESIAN_POINT('Ctrl Pts',(81.6362979099804,8.66453087580806,133.40478355916));
#67667=CARTESIAN_POINT('Ctrl Pts',(81.5980391094291,8.5285451938593,133.395065365251));
#67668=CARTESIAN_POINT('Ctrl Pts',(81.591957854287,8.50840169879939,133.393630108704));
#67669=CARTESIAN_POINT('Ctrl Pts',(81.5816331484603,8.47640584367857,133.391356389004));
#67670=CARTESIAN_POINT('Ctrl Pts',(81.5776343069374,8.46447757704711,133.390510081107));
#67671=CARTESIAN_POINT('Ctrl Pts',(81.5702821479644,8.443343980226,133.389012723388));
#67672=CARTESIAN_POINT('Ctrl Pts',(81.5669820676809,8.43412090056489,133.388359955569));
#67673=CARTESIAN_POINT('Ctrl Pts',(81.559897123907,8.41485720853457,133.386997800567));
#67674=CARTESIAN_POINT('Ctrl Pts',(81.5560962079875,8.4048229472242,133.386288981656));
#67675=CARTESIAN_POINT('Ctrl Pts',(81.5458068996314,8.37843211267489,133.384426150809));
#67676=CARTESIAN_POINT('Ctrl Pts',(81.5391557514839,8.36214012463879,133.383277617252));
#67677=CARTESIAN_POINT('Ctrl Pts',(81.5038164425773,8.27934971206428,133.377443688775));
#67678=CARTESIAN_POINT('Ctrl Pts',(81.4710707443097,8.21466345169506,133.372898514549));
#67679=CARTESIAN_POINT('Ctrl Pts',(81.382636583747,8.06504129781753,133.362166260359));
#67680=CARTESIAN_POINT('Ctrl Pts',(81.3232036310128,7.98266892405917,133.356077249446));
#67681=CARTESIAN_POINT('Ctrl Pts',(81.2216520015338,7.8659960643519,133.346467892483));
#67682=CARTESIAN_POINT('Ctrl Pts',(81.1847418375529,7.82748812570972,133.343100781389));
#67683=CARTESIAN_POINT('Ctrl Pts',(81.137982467524,7.78316986629655,133.338882124724));
#67684=CARTESIAN_POINT('Ctrl Pts',(81.1298349306032,7.77560109283501,133.338148645584));
#67685=CARTESIAN_POINT('Ctrl Pts',(81.1169353792254,7.76385625084447,133.33698867596));
#67686=CARTESIAN_POINT('Ctrl Pts',(81.1122341339775,7.7596245577064,133.336566191956));
#67687=CARTESIAN_POINT('Ctrl Pts',(81.1038106281421,7.75212877017414,133.335809430434));
#67688=CARTESIAN_POINT('Ctrl Pts',(81.1000977552134,7.74885435076932,133.335475929858));
#67689=CARTESIAN_POINT('Ctrl Pts',(81.0910541402644,7.74095007441324,133.334663797175));
#67690=CARTESIAN_POINT('Ctrl Pts',(81.0857085436646,7.73633754278862,133.334183930127));
#67691=CARTESIAN_POINT('Ctrl Pts',(81.0688457511456,7.72197319877986,133.332671173776));
#67692=CARTESIAN_POINT('Ctrl Pts',(81.0572256459197,7.71234413052489,133.331630180348));
#67693=CARTESIAN_POINT('Ctrl Pts',(80.9950755335242,7.66225143474915,133.326077067913));
#67694=CARTESIAN_POINT('Ctrl Pts',(80.9423541323211,7.62460421608266,133.321418823345));
#67695=CARTESIAN_POINT('Ctrl Pts',(80.7930096781042,7.53058499202765,133.308610104847));
#67696=CARTESIAN_POINT('Ctrl Pts',(80.692673764837,7.48070636574628,133.300432383108));
#67697=CARTESIAN_POINT('Ctrl Pts',(80.5435792296822,7.42445530223334,133.289194010673));
#67698=CARTESIAN_POINT('Ctrl Pts',(80.4983636167282,7.40957428498924,133.285892949317));
#67699=CARTESIAN_POINT('Ctrl Pts',(80.4371689976208,7.39230123550686,133.281565046485));
#67700=CARTESIAN_POINT('Ctrl Pts',(80.4217068877066,7.38817638008139,133.280483087125));
#67701=CARTESIAN_POINT('Ctrl Pts',(80.396111129377,7.38174170220755,133.278710484611));
#67702=CARTESIAN_POINT('Ctrl Pts',(80.3860113234091,7.37930286239629,133.278015732056));
#67703=CARTESIAN_POINT('Ctrl Pts',(80.3662143577409,7.37471797324053,133.276662841383));
#67704=CARTESIAN_POINT('Ctrl Pts',(80.3565195384294,7.37256384201751,133.276004469798));
#67705=CARTESIAN_POINT('Ctrl Pts',(80.3334367970526,7.36765116167709,133.274446466998));
#67706=CARTESIAN_POINT('Ctrl Pts',(80.320032911397,7.36497040343789,133.273549343527));
#67707=CARTESIAN_POINT('Ctrl Pts',(80.273883789589,7.35632991367169,133.270485152579));
#67708=CARTESIAN_POINT('Ctrl Pts',(80.2409925708943,7.35118633459383,133.268343755974));
#67709=CARTESIAN_POINT('Ctrl Pts',(80.1594722961909,7.34092990068269,133.263121066018));
#67710=CARTESIAN_POINT('Ctrl Pts',(80.1107298446527,7.33696529155995,133.260072534283));
#67711=CARTESIAN_POINT('Ctrl Pts',(79.994797432476,7.3326562114703,133.252912883531));
#67712=CARTESIAN_POINT('Ctrl Pts',(79.9276247423833,7.33421959505197,133.2488379159));
#67713=CARTESIAN_POINT('Ctrl Pts',(79.8475185863583,7.34093967521996,133.243916685164));
#67714=CARTESIAN_POINT('Ctrl Pts',(79.834321991487,7.34220552101315,133.243103843953));
#67715=CARTESIAN_POINT('Ctrl Pts',(79.7494057928624,7.3513749262557,133.23785260614));
#67716=CARTESIAN_POINT('Ctrl Pts',(79.6782573197369,7.36377229963186,133.233358685601));
#67717=CARTESIAN_POINT('Ctrl Pts',(79.596880594906,7.3834650976776,133.227882121798));
#67718=CARTESIAN_POINT('Ctrl Pts',(79.5856441738791,7.38630871102959,133.227118283983));
#67719=CARTESIAN_POINT('Ctrl Pts',(79.5682214248156,7.39091186844713,133.225920686043));
#67720=CARTESIAN_POINT('Ctrl Pts',(79.5620138161878,7.3925904528052,133.225491364874));
#67721=CARTESIAN_POINT('Ctrl Pts',(79.5505800575376,7.39575337596857,133.224695484106));
#67722=CARTESIAN_POINT('Ctrl Pts',(79.5453512593809,7.39722739137678,133.224329512885));
#67723=CARTESIAN_POINT('Ctrl Pts',(79.5332174538534,7.40071210346732,133.223475629999));
#67724=CARTESIAN_POINT('Ctrl Pts',(79.5263181941017,7.40274195467925,133.222986646803));
#67725=CARTESIAN_POINT('Ctrl Pts',(79.5042997382551,7.40937526951419,133.221415464369));
#67726=CARTESIAN_POINT('Ctrl Pts',(79.4892333363723,7.41414907614173,133.220324279785));
#67727=CARTESIAN_POINT('Ctrl Pts',(79.4062442277734,7.44174951580364,133.214232923631));
#67728=CARTESIAN_POINT('Ctrl Pts',(79.3397868037485,7.46872373334628,133.209056317954));
#67729=CARTESIAN_POINT('Ctrl Pts',(79.1566026461127,7.55722206374598,133.194265949274));
#67730=CARTESIAN_POINT('Ctrl Pts',(79.0451257459542,7.62844818435537,133.18466760681));
#67731=CARTESIAN_POINT('Ctrl Pts',(78.9220022433216,7.72947695119266,133.173657076169));
#67732=CARTESIAN_POINT('Ctrl Pts',(78.9012348759895,7.74739338269677,133.171781552192));
#67733=CARTESIAN_POINT('Ctrl Pts',(78.8716170469183,7.77424898564333,133.169077864142));
#67734=CARTESIAN_POINT('Ctrl Pts',(78.8624113398681,7.78278773694922,133.168233252829));
#67735=CARTESIAN_POINT('Ctrl Pts',(78.8461994172958,7.79816968845228,133.166737825009));
#67736=CARTESIAN_POINT('Ctrl Pts',(78.8391554475851,7.80497204444058,133.166085305943));
#67737=CARTESIAN_POINT('Ctrl Pts',(78.8291895817662,7.81476734387068,133.165157971275));
#67738=CARTESIAN_POINT('Ctrl Pts',(78.8262184568082,7.81770969131757,133.164880970341));
#67739=CARTESIAN_POINT('Ctrl Pts',(78.8231266848953,7.82079465960108,133.164592150359));
#67740=CARTESIAN_POINT('Ctrl Pts',(78.8229949739282,7.82092612477736,133.164579845402));
#67741=CARTESIAN_POINT('Ctrl Pts',(78.8225491598063,7.82137125608858,133.16453819201));
#67742=CARTESIAN_POINT('Ctrl Pts',(78.8222351597612,7.82168502591829,133.164508848104));
#67743=CARTESIAN_POINT('Ctrl Pts',(78.8216202401235,7.82229998608254,133.164451370525));
#67744=CARTESIAN_POINT('Ctrl Pts',(78.8213193105538,7.8226011663013,133.164423236417));
#67745=CARTESIAN_POINT('Ctrl Pts',(78.8207286263011,7.82319279595478,133.164368001706));
#67746=CARTESIAN_POINT('Ctrl Pts',(78.8204388634105,7.82348323710768,133.164340900744));
#67747=CARTESIAN_POINT('Ctrl Pts',(78.8198688482503,7.82405500878748,133.16428757784));
#67748=CARTESIAN_POINT('Ctrl Pts',(78.8195885891986,7.82433633256011,133.1642613556));
#67749=CARTESIAN_POINT('Ctrl Pts',(78.8190361133961,7.82489130395431,133.164209653719));
#67750=CARTESIAN_POINT('Ctrl Pts',(78.8187638911407,7.82516494599789,133.164184173839));
#67751=CARTESIAN_POINT('Ctrl Pts',(78.8103067761803,7.83367208039258,133.163392444313));
#67752=CARTESIAN_POINT('Ctrl Pts',(78.8022079079764,7.84199097652383,133.162629964288));
#67753=CARTESIAN_POINT('Ctrl Pts',(78.7745942068553,7.87095455071802,133.16001441712));
#67754=CARTESIAN_POINT('Ctrl Pts',(78.7555201524743,7.89201396843054,133.158180071095));
#67755=CARTESIAN_POINT('Ctrl Pts',(78.7111292342008,7.94361886288451,133.153831508313));
#67756=CARTESIAN_POINT('Ctrl Pts',(78.6863461381593,7.97460114388211,133.151337370668));
#67757=CARTESIAN_POINT('Ctrl Pts',(78.6103912907225,8.0768346359254,133.143414767314));
#67758=CARTESIAN_POINT('Ctrl Pts',(78.5637312761252,8.15124842426908,133.138110163814));
#67759=CARTESIAN_POINT('Ctrl Pts',(78.4858206463559,8.30048486186269,133.1277908407));
#67760=CARTESIAN_POINT('Ctrl Pts',(78.4537418747022,8.3745858561639,133.122797735055));
#67761=CARTESIAN_POINT('Ctrl Pts',(78.4233197365001,8.46169631532066,133.116762967672));
#67762=CARTESIAN_POINT('Ctrl Pts',(78.4195970652688,8.47272582514927,133.115995892229));
#67763=CARTESIAN_POINT('Ctrl Pts',(78.4139944305792,8.48991781992767,133.11479428497));
#67764=CARTESIAN_POINT('Ctrl Pts',(78.4120340360187,8.4960539806568,133.114364239368));
#67765=CARTESIAN_POINT('Ctrl Pts',(78.4084708698339,8.50743417084807,133.113564244413));
#67766=CARTESIAN_POINT('Ctrl Pts',(78.4068583423584,8.51267493013052,133.113194862411));
#67767=CARTESIAN_POINT('Ctrl Pts',(78.4031865025385,8.52482152306541,133.112336540812));
#67768=CARTESIAN_POINT('Ctrl Pts',(78.4011461048203,8.53173282449425,133.111846547559));
#67769=CARTESIAN_POINT('Ctrl Pts',(78.3947518778829,8.55392064054761,133.110268800813));
#67770=CARTESIAN_POINT('Ctrl Pts',(78.3905718240015,8.56924574432102,133.109171960131));
#67771=CARTESIAN_POINT('Ctrl Pts',(78.3517969808658,8.71985486158714,133.0983387757));
#67772=CARTESIAN_POINT('Ctrl Pts',(78.3341234680228,8.85891102740731,133.087968181546));
#67773=CARTESIAN_POINT('Ctrl Pts',(78.3340006446003,8.99853445987493,133.077925722171));
#67774=CARTESIAN_POINT('Ctrl Pts',(78.334000643305,8.99853593313598,133.077925616206));
#67775=CARTESIAN_POINT('Ctrl Pts',(78.3339316737719,9.07701813953855,133.072280759997));
#67776=CARTESIAN_POINT('Ctrl Pts',(78.3394083941732,9.15541856497152,133.066746213697));
#67777=CARTESIAN_POINT('Ctrl Pts',(78.3522801515502,9.24648871189249,133.060461213954));
#67778=CARTESIAN_POINT('Ctrl Pts',(78.354326636417,9.25980104488598,133.059545931238));
#67779=CARTESIAN_POINT('Ctrl Pts',(78.3581585251793,9.28286170761914,133.057966092966));
#67780=CARTESIAN_POINT('Ctrl Pts',(78.3598698652317,9.29262146617993,133.057299246906));
#67781=CARTESIAN_POINT('Ctrl Pts',(78.3634800552974,9.31218285113474,133.055966075389));
#67782=CARTESIAN_POINT('Ctrl Pts',(78.3653801422347,9.32198383503753,133.055299819179));
#67783=CARTESIAN_POINT('Ctrl Pts',(78.3694200787876,9.34186442003407,133.053951612522));
#67784=CARTESIAN_POINT('Ctrl Pts',(78.3715655716086,9.3519424408267,133.053269873584));
#67785=CARTESIAN_POINT('Ctrl Pts',(78.3771917656863,9.37721672002002,133.051564068158));
#67786=CARTESIAN_POINT('Ctrl Pts',(78.3807925684521,9.39238544805761,133.050543871151));
#67787=CARTESIAN_POINT('Ctrl Pts',(78.3953380363042,9.45004571296821,133.046677012386));
#67788=CARTESIAN_POINT('Ctrl Pts',(78.4077473246361,9.49215149384497,133.043877153545));
#67789=CARTESIAN_POINT('Ctrl Pts',(78.4265388761537,9.54771743668607,133.04018773218));
#67790=CARTESIAN_POINT('Ctrl Pts',(78.4314573090839,9.56164754784783,133.039263215163));
#67791=CARTESIAN_POINT('Ctrl Pts',(78.4365593647824,9.57550793230875,133.038342764662));
#67792=CARTESIAN_POINT('',(78.3340000765189,9.00050493656018,133.272970309233));
#67793=CARTESIAN_POINT('Ctrl Pts',(78.4365593737642,9.57550795670914,133.231048988662));
#67794=CARTESIAN_POINT('Ctrl Pts',(78.436461916935,9.57524320282636,133.231069156205));
#67795=CARTESIAN_POINT('Ctrl Pts',(78.4363645272696,9.57497842395342,133.23108932565));
#67796=CARTESIAN_POINT('Ctrl Pts',(78.407498131545,9.49643612376326,133.237072257336));
#67797=CARTESIAN_POINT('Ctrl Pts',(78.3846480814157,9.41611127630672,133.243182772986));
#67798=CARTESIAN_POINT('Ctrl Pts',(78.3513888497726,9.25379191329365,133.255206136156));
#67799=CARTESIAN_POINT('Ctrl Pts',(78.3408639956099,9.17204636037335,133.261103741288));
#67800=CARTESIAN_POINT('Ctrl Pts',(78.334817626086,9.06009551836616,133.26889834066));
#67801=CARTESIAN_POINT('Ctrl Pts',(78.3340091080431,9.03030376633059,133.270946591912));
#67802=CARTESIAN_POINT('Ctrl Pts',(78.3340000765189,9.00050493656018,133.272970309233));
#67803=CARTESIAN_POINT('Ctrl Pts',(78.3340000762184,9.0005039440939,133.272970376634));
#67804=CARTESIAN_POINT('Ctrl Pts',(78.3339976906018,8.99261728163465,133.273505980588));
#67805=CARTESIAN_POINT('Ctrl Pts',(78.3340513068531,8.98473055887474,133.274039846394));
#67806=CARTESIAN_POINT('Ctrl Pts',(78.3342826460377,8.96808778940267,133.275162829666));
#67807=CARTESIAN_POINT('Ctrl Pts',(78.3344734091631,8.95933216535589,133.275751521671));
#67808=CARTESIAN_POINT('Ctrl Pts',(78.3350069258589,8.9413552901423,133.276956035385));
#67809=CARTESIAN_POINT('Ctrl Pts',(78.3353572678109,8.93213455223497,133.277571598656));
#67810=CARTESIAN_POINT('Ctrl Pts',(78.3362616313914,8.91260940516593,133.278870483235));
#67811=CARTESIAN_POINT('Ctrl Pts',(78.3368348210835,8.90230623868865,133.279553178857));
#67812=CARTESIAN_POINT('Ctrl Pts',(78.3385195583362,8.87637013403552,133.281265291819));
#67813=CARTESIAN_POINT('Ctrl Pts',(78.3397560479465,8.8607460991998,133.282290776303));
#67814=CARTESIAN_POINT('Ctrl Pts',(78.3453906963644,8.80038986588423,133.286231969989));
#67815=CARTESIAN_POINT('Ctrl Pts',(78.3513780475261,8.7558230969127,133.289098279209));
#67816=CARTESIAN_POINT('Ctrl Pts',(78.3747357773466,8.6229534732413,133.29757661396));
#67817=CARTESIAN_POINT('Ctrl Pts',(78.397460520862,8.53576261080013,133.303042613918));
#67818=CARTESIAN_POINT('Ctrl Pts',(78.4582638678523,8.36161531908081,133.314314205));
#67819=CARTESIAN_POINT('Ctrl Pts',(78.4969421837066,8.27522597289918,133.320105329415));
#67820=CARTESIAN_POINT('Ctrl Pts',(78.5486304022539,8.181934737297,133.327074563826));
#67821=CARTESIAN_POINT('Ctrl Pts',(78.5546524440025,8.17134150318087,133.327877037898));
#67822=CARTESIAN_POINT('Ctrl Pts',(78.5640565095659,8.15521343058383,133.329117435649));
#67823=CARTESIAN_POINT('Ctrl Pts',(78.5673557102706,8.14963043849194,133.329550287636));
#67824=CARTESIAN_POINT('Ctrl Pts',(78.5735008530715,8.13936873575705,133.330352574247));
#67825=CARTESIAN_POINT('Ctrl Pts',(78.5763373699455,8.13468462286057,133.33072140944));
#67826=CARTESIAN_POINT('Ctrl Pts',(78.5828633261871,8.12402685924504,133.331566579186));
#67827=CARTESIAN_POINT('Ctrl Pts',(78.586567468122,8.11806249147503,133.332043840979));
#67828=CARTESIAN_POINT('Ctrl Pts',(78.5984572801371,8.0991849465474,133.333567619908));
#67829=CARTESIAN_POINT('Ctrl Pts',(78.6067827912849,8.08636138206777,133.334622530965));
#67830=CARTESIAN_POINT('Ctrl Pts',(78.6718552790283,7.98908990652449,133.342766654373));
#67831=CARTESIAN_POINT('Ctrl Pts',(78.7360499709074,7.90989242480569,133.350213830109));
#67832=CARTESIAN_POINT('Ctrl Pts',(78.8877362334637,7.75429427524032,133.366018514977));
#67833=CARTESIAN_POINT('Ctrl Pts',(78.9768190667109,7.68014256855238,133.374308265934));
#67834=CARTESIAN_POINT('Ctrl Pts',(79.0889714252201,7.60502396866075,133.383544518744));
#67835=CARTESIAN_POINT('Ctrl Pts',(79.1052522183433,7.59452582583626,133.384859482924));
#67836=CARTESIAN_POINT('Ctrl Pts',(79.1311511046681,7.57845824542435,133.386911916442));
#67837=CARTESIAN_POINT('Ctrl Pts',(79.1406477113292,7.57269729306556,133.387656374132));
#67838=CARTESIAN_POINT('Ctrl Pts',(79.1585629022349,7.56207298066403,133.389045905185));
#67839=CARTESIAN_POINT('Ctrl Pts',(79.1669677696563,7.55718753384629,133.389691760503));
#67840=CARTESIAN_POINT('Ctrl Pts',(79.185957562513,7.54637070897763,133.391137755132));
#67841=CARTESIAN_POINT('Ctrl Pts',(79.1965655630021,7.54048079005655,133.391936383075));
#67842=CARTESIAN_POINT('Ctrl Pts',(79.2280194530625,7.52346339045191,133.394278483317));
#67843=CARTESIAN_POINT('Ctrl Pts',(79.2490393430912,7.51266261193098,133.39581045891));
#67844=CARTESIAN_POINT('Ctrl Pts',(79.3674336652126,7.45497744089553,133.404270765032));
#67845=CARTESIAN_POINT('Ctrl Pts',(79.4689628593109,7.41720564843457,133.410878524406));
#67846=CARTESIAN_POINT('Ctrl Pts',(79.6460681417884,7.37029686375471,133.422065944804));
#67847=CARTESIAN_POINT('Ctrl Pts',(79.7199038650213,7.35599737471142,133.426643271146));
#67848=CARTESIAN_POINT('Ctrl Pts',(79.829951825236,7.34231494403922,133.433643316259));
#67849=CARTESIAN_POINT('Ctrl Pts',(79.8655873782694,7.33904577276688,133.435937755948));
#67850=CARTESIAN_POINT('Ctrl Pts',(79.91098881767,7.33635121984644,133.438927283502));
#67851=CARTESIAN_POINT('Ctrl Pts',(79.9206847846028,7.33586078114829,133.439569566155));
#67852=CARTESIAN_POINT('Ctrl Pts',(79.9363299482605,7.33520645774564,133.440612924074));
#67853=CARTESIAN_POINT('Ctrl Pts',(79.9422768741108,7.33498965415705,133.441011144881));
#67854=CARTESIAN_POINT('Ctrl Pts',(79.9537971150287,7.33463145968591,133.441785941147));
#67855=CARTESIAN_POINT('Ctrl Pts',(79.9593701742531,7.33448617677437,133.442162301269));
#67856=CARTESIAN_POINT('Ctrl Pts',(79.971828684925,7.33422396438118,133.443006954968));
#67857=CARTESIAN_POINT('Ctrl Pts',(79.9787143388054,7.33412175105805,133.443476036851));
#67858=CARTESIAN_POINT('Ctrl Pts',(79.9992891360013,7.33394391043794,133.444884026227));
#67859=CARTESIAN_POINT('Ctrl Pts',(80.0129784042471,7.33399431859728,133.445829204494));
#67860=CARTESIAN_POINT('Ctrl Pts',(80.1294256411956,7.33585833849934,133.4539321431));
#67861=CARTESIAN_POINT('Ctrl Pts',(80.2318047428464,7.3470082965904,133.461457592154));
#67862=CARTESIAN_POINT('Ctrl Pts',(80.4448668856639,7.39040352061597,133.477270424917));
#67863=CARTESIAN_POINT('Ctrl Pts',(80.5545948611097,7.42483615666219,133.485492956991));
#67864=CARTESIAN_POINT('Ctrl Pts',(80.6777392382939,7.47796133305972,133.49467001486));
#67865=CARTESIAN_POINT('Ctrl Pts',(80.6954131319735,7.48595481909441,133.495986743098));
#67866=CARTESIAN_POINT('Ctrl Pts',(80.7229874500541,7.49901078287701,133.498041289588));
#67867=CARTESIAN_POINT('Ctrl Pts',(80.7329831997019,7.50386660949968,133.498786120209));
#67868=CARTESIAN_POINT('Ctrl Pts',(80.751630419617,7.51315696763973,133.500175988367));
#67869=CARTESIAN_POINT('Ctrl Pts',(80.7602930577058,7.51756788896651,133.500821811555));
#67870=CARTESIAN_POINT('Ctrl Pts',(80.7796731770337,7.52765060040558,133.502267271415));
#67871=CARTESIAN_POINT('Ctrl Pts',(80.7903684174145,7.53336412317115,133.503065401678));
#67872=CARTESIAN_POINT('Ctrl Pts',(80.8216861517258,7.55053650848381,133.505404572047));
#67873=CARTESIAN_POINT('Ctrl Pts',(80.8421292587959,7.56231750854899,133.506934159587));
#67874=CARTESIAN_POINT('Ctrl Pts',(80.9502247758351,7.62770818984177,133.515050247536));
#67875=CARTESIAN_POINT('Ctrl Pts',(81.0330295487542,7.6889068623411,133.521350881295));
#67876=CARTESIAN_POINT('Ctrl Pts',(81.1688136589222,7.81016101826928,133.532469075745));
#67877=CARTESIAN_POINT('Ctrl Pts',(81.2241022440341,7.8671213138598,133.537288054666));
#67878=CARTESIAN_POINT('Ctrl Pts',(81.2910637399378,7.94675547761684,133.543848463834));
#67879=CARTESIAN_POINT('Ctrl Pts',(81.3065802203259,7.96606692551881,133.545427393132));
#67880=CARTESIAN_POINT('Ctrl Pts',(81.3321413301288,7.99937425055244,133.548144449112));
#67881=CARTESIAN_POINT('Ctrl Pts',(81.3424102336148,8.01319347291886,133.549270027772));
#67882=CARTESIAN_POINT('Ctrl Pts',(81.3568066038894,8.03320778833813,133.550901713761));
#67883=CARTESIAN_POINT('Ctrl Pts',(81.3611099608627,8.03927578874542,133.551396608904));
#67884=CARTESIAN_POINT('Ctrl Pts',(81.3685284940726,8.04988627106338,133.552262709149));
#67885=CARTESIAN_POINT('Ctrl Pts',(81.3716620131375,8.0544157056535,133.55263267084));
#67886=CARTESIAN_POINT('Ctrl Pts',(81.3783286277925,8.0641550254371,133.553428804293));
#67887=CARTESIAN_POINT('Ctrl Pts',(81.3818546168129,8.06936933356374,133.553855397039));
#67888=CARTESIAN_POINT('Ctrl Pts',(81.391455070299,8.08374154619191,133.555031906416));
#67889=CARTESIAN_POINT('Ctrl Pts',(81.3974684746196,8.09293957578421,133.555785620058));
#67890=CARTESIAN_POINT('Ctrl Pts',(81.4311433328127,8.14557798363366,133.5601002991));
#67891=CARTESIAN_POINT('Ctrl Pts',(81.4568672269784,8.1902191553164,133.563763837486));
#67892=CARTESIAN_POINT('Ctrl Pts',(81.5245100564812,8.32129316163141,133.574392839356));
#67893=CARTESIAN_POINT('Ctrl Pts',(81.5610830164513,8.41025873016334,133.581444794114));
#67894=CARTESIAN_POINT('Ctrl Pts',(81.605515542038,8.55206932932379,133.592131964013));
#67895=CARTESIAN_POINT('Ctrl Pts',(81.6188562365306,8.60297680582893,133.595867200292));
#67896=CARTESIAN_POINT('Ctrl Pts',(81.63471145473,8.67775367372426,133.601194518558));
#67897=CARTESIAN_POINT('Ctrl Pts',(81.6391550674477,8.70117731183862,133.602841254199));
#67898=CARTESIAN_POINT('Ctrl Pts',(81.6463013028563,8.74382709388512,133.605800365489));
#67899=CARTESIAN_POINT('Ctrl Pts',(81.6491734675297,8.76302011298758,133.607117734688));
#67900=CARTESIAN_POINT('Ctrl Pts',(81.6531623562786,8.7932785685513,133.609173048873));
#67901=CARTESIAN_POINT('Ctrl Pts',(81.6545046780016,8.80431196440993,133.609918014963));
#67902=CARTESIAN_POINT('Ctrl Pts',(81.6568138218278,8.82501872640462,133.611308005724));
#67903=CARTESIAN_POINT('Ctrl Pts',(81.6578065795981,8.83468866404034,133.611953817388));
#67904=CARTESIAN_POINT('Ctrl Pts',(81.6598470942018,8.85643617030607,133.613399083718));
#67905=CARTESIAN_POINT('Ctrl Pts',(81.6608477843686,8.86851768388437,133.61419703377));
#67906=CARTESIAN_POINT('Ctrl Pts',(81.663406183093,8.9041262700719,133.616535143697));
#67907=CARTESIAN_POINT('Ctrl Pts',(81.6645964743734,8.92767732745032,133.618063866961));
#67908=CARTESIAN_POINT('Ctrl Pts',(81.6683370307246,9.05544504806204,133.626275643631));
#67909=CARTESIAN_POINT('Ctrl Pts',(81.6616018430605,9.15970381562065,133.632663200137));
#67910=CARTESIAN_POINT('Ctrl Pts',(81.632845300703,9.33982027825646,133.643802078366));
#67911=CARTESIAN_POINT('Ctrl Pts',(81.6151137661839,9.41601371610997,133.6485544592));
#67912=CARTESIAN_POINT('Ctrl Pts',(81.584863594433,9.51416693766071,133.655032520303));
#67913=CARTESIAN_POINT('Ctrl Pts',(81.5771051039896,9.53749382917846,133.65659978726));
#67914=CARTESIAN_POINT('Ctrl Pts',(81.5630729797701,9.57675984626653,133.659298718012));
#67915=CARTESIAN_POINT('Ctrl Pts',(81.5570642676673,9.59278990453277,133.66041805248));
#67916=CARTESIAN_POINT('Ctrl Pts',(81.5480979086607,9.61563297300678,133.662042265941));
#67917=CARTESIAN_POINT('Ctrl Pts',(81.5453398245459,9.62252382582609,133.66253607295));
#67918=CARTESIAN_POINT('Ctrl Pts',(81.5404558248239,9.63449362926699,133.663400946802));
#67919=CARTESIAN_POINT('Ctrl Pts',(81.5383506316102,9.63958083696979,133.663770781289));
#67920=CARTESIAN_POINT('Ctrl Pts',(81.5337808304227,9.65047068038874,133.664567439537));
#67921=CARTESIAN_POINT('Ctrl Pts',(81.5313085340496,9.65626969460908,133.664994691331));
#67922=CARTESIAN_POINT('Ctrl Pts',(81.5244197079475,9.6721772405201,133.666174749137));
#67923=CARTESIAN_POINT('Ctrl Pts',(81.5199356908112,9.68225594037223,133.666931388306));
#67924=CARTESIAN_POINT('Ctrl Pts',(81.4936353726453,9.73982473044721,133.671301950198));
#67925=CARTESIAN_POINT('Ctrl Pts',(81.4696960734452,9.78630756238536,133.675021462593));
#67926=CARTESIAN_POINT('Ctrl Pts',(81.3925518833272,9.92022858523847,133.686163104619));
#67927=CARTESIAN_POINT('Ctrl Pts',(81.3334282287822,10.0039882219303,133.693682715429));
#67928=CARTESIAN_POINT('Ctrl Pts',(81.2198088715287,10.137058927403,133.706224759534));
#67929=CARTESIAN_POINT('Ctrl Pts',(81.1690523623575,10.1891828613474,133.711330843185));
#67930=CARTESIAN_POINT('Ctrl Pts',(81.1019642253685,10.249616292301,133.717492787095));
#67931=CARTESIAN_POINT('Ctrl Pts',(81.0886953332371,10.2611933018708,133.718685747098));
#67932=CARTESIAN_POINT('Ctrl Pts',(81.0670487487982,10.2794835309093,133.720591701858));
#67933=CARTESIAN_POINT('Ctrl Pts',(81.0587856766769,10.2863296771672,133.721310105985));
#67934=CARTESIAN_POINT('Ctrl Pts',(81.0428569413904,10.2992695160165,133.722677877021));
#67935=CARTESIAN_POINT('Ctrl Pts',(81.0352025995274,10.3053763673253,133.723327756611));
#67936=CARTESIAN_POINT('Ctrl Pts',(81.0176007656893,10.3191674132863,133.724805753231));
#67937=CARTESIAN_POINT('Ctrl Pts',(81.0076191828995,10.3268072879126,133.725632095427));
#67938=CARTESIAN_POINT('Ctrl Pts',(80.9807273846552,10.3469116774754,133.727827989257));
#67939=CARTESIAN_POINT('Ctrl Pts',(80.9636659512391,10.3591708014653,133.729189642396));
#67940=CARTESIAN_POINT('Ctrl Pts',(80.8469854273796,10.4397071305131,133.738304247379));
#67941=CARTESIAN_POINT('Ctrl Pts',(80.7404283258063,10.4973011311402,133.745639610053));
#67942=CARTESIAN_POINT('Ctrl Pts',(80.5671851459957,10.5678809492911,133.757070391546));
#67943=CARTESIAN_POINT('Ctrl Pts',(80.5043657798887,10.5892021750872,133.761131682327));
#67944=CARTESIAN_POINT('Ctrl Pts',(80.4187903515136,10.6126608373729,133.766747645376));
#67945=CARTESIAN_POINT('Ctrl Pts',(80.3970152165322,10.6181591862726,133.768183883208));
#67946=CARTESIAN_POINT('Ctrl Pts',(80.3595441017168,10.62681902944,133.77067807578));
#67947=CARTESIAN_POINT('Ctrl Pts',(80.343901062721,10.6301975734692,133.771726024234));
#67948=CARTESIAN_POINT('Ctrl Pts',(80.3211276038736,10.6347737716873,133.773264567756));
#67949=CARTESIAN_POINT('Ctrl Pts',(80.3140336848583,10.6361512957294,133.773745633039));
#67950=CARTESIAN_POINT('Ctrl Pts',(80.3015893065327,10.6384838810663,133.774593059245));
#67951=CARTESIAN_POINT('Ctrl Pts',(80.2962427951625,10.6394589788814,133.774958290382));
#67952=CARTESIAN_POINT('Ctrl Pts',(80.2845856993941,10.6415261170223,133.775757207788));
#67953=CARTESIAN_POINT('Ctrl Pts',(80.2782736606913,10.6426079201925,133.776191425318));
#67954=CARTESIAN_POINT('Ctrl Pts',(80.2606330000671,10.6455267095962,133.777409192905));
#67955=CARTESIAN_POINT('Ctrl Pts',(80.2492916556214,10.6472830251457,133.778196969373));
#67956=CARTESIAN_POINT('Ctrl Pts',(80.1727704439156,10.6583247589852,133.783540864829));
#67957=CARTESIAN_POINT('Ctrl Pts',(80.1071142619588,10.6638555325745,133.788263817613));
#67958=CARTESIAN_POINT('Ctrl Pts',(80.0205159427081,10.666003543698,133.794543326326));
#67959=CARTESIAN_POINT('Ctrl Pts',(79.9997129860433,10.6661298304552,133.796055813938));
#67960=CARTESIAN_POINT('Ctrl Pts',(79.9107607700668,10.6650038671956,133.802529662383));
#67961=CARTESIAN_POINT('Ctrl Pts',(79.8427218693291,10.6599596401399,133.807494384476));
#67962=CARTESIAN_POINT('Ctrl Pts',(79.7041211212561,10.6410834274608,133.817515485007));
#67963=CARTESIAN_POINT('Ctrl Pts',(79.6337528996968,10.6268265761426,133.82255224343));
#67964=CARTESIAN_POINT('Ctrl Pts',(79.5475739026474,10.6034882697754,133.828644654542));
#67965=CARTESIAN_POINT('Ctrl Pts',(79.5307070329419,10.598633215237,133.829833626625));
#67966=CARTESIAN_POINT('Ctrl Pts',(79.5036679138261,10.5903852781821,133.831734785228));
#67967=CARTESIAN_POINT('Ctrl Pts',(79.4934465879558,10.5871592619694,133.832452332212));
#67968=CARTESIAN_POINT('Ctrl Pts',(79.473944928724,10.5807966361743,133.833819460409));
#67969=CARTESIAN_POINT('Ctrl Pts',(79.4646597712293,10.5776763893161,133.834469544958));
#67970=CARTESIAN_POINT('Ctrl Pts',(79.4435003638077,10.5703575275151,133.835949359433));
#67971=CARTESIAN_POINT('Ctrl Pts',(79.4316450288256,10.5661057596879,133.836777298828));
#67972=CARTESIAN_POINT('Ctrl Pts',(79.4000644477015,10.5543739317494,133.838980466862));
#67973=CARTESIAN_POINT('Ctrl Pts',(79.3804307589017,10.5466528395429,133.840347711874));
#67974=CARTESIAN_POINT('Ctrl Pts',(79.2509904481143,10.4928889183974,133.849357420134));
#67975=CARTESIAN_POINT('Ctrl Pts',(79.1462430747107,10.4355610645967,133.856595880305));
#67976=CARTESIAN_POINT('Ctrl Pts',(78.9699041148057,10.3128689198404,133.869720206282));
#67977=CARTESIAN_POINT('Ctrl Pts',(78.8961850138629,10.2515229050092,133.875580330368));
#67978=CARTESIAN_POINT('Ctrl Pts',(78.8192428280163,10.175383162731,133.882648386722));
#67979=CARTESIAN_POINT('Ctrl Pts',(78.8104343491552,10.166467581056,133.883473288501));
#67980=CARTESIAN_POINT('Ctrl Pts',(78.7971720486753,10.1527375744529,133.88474115286));
#67981=CARTESIAN_POINT('Ctrl Pts',(78.7926444570711,10.1479945929044,133.885178690297));
#67982=CARTESIAN_POINT('Ctrl Pts',(78.7843920613262,10.1392467913437,133.885985145762));
#67983=CARTESIAN_POINT('Ctrl Pts',(78.7806588340017,10.1352502059921,133.886353413212));
#67984=CARTESIAN_POINT('Ctrl Pts',(78.7721628194211,10.1260645927159,133.887199406111));
#67985=CARTESIAN_POINT('Ctrl Pts',(78.7674132319093,10.1208637132067,133.887678076848));
#67986=CARTESIAN_POINT('Ctrl Pts',(78.7526487673841,10.1044890467979,133.889183682213));
#67987=CARTESIAN_POINT('Ctrl Pts',(78.7427521035009,10.093210336394,133.890218618129));
#67988=CARTESIAN_POINT('Ctrl Pts',(78.6650788248194,10.0022403777949,133.898538900544));
#67989=CARTESIAN_POINT('Ctrl Pts',(78.6047986749672,9.91646607616967,133.906204482806));
#67990=CARTESIAN_POINT('Ctrl Pts',(78.5073026724441,9.74558706254934,133.920508699118));
#67991=CARTESIAN_POINT('Ctrl Pts',(78.4683717547555,9.66193031557139,133.927135282778));
#67992=CARTESIAN_POINT('Ctrl Pts',(78.4365594251401,9.5755080962782,133.933539779158));
#67993=CARTESIAN_POINT('Origin',(80.,9.,134.));
#67994=CARTESIAN_POINT('',(78.4365593788086,9.57550797041272,134.632696244622));
#67995=CARTESIAN_POINT('',(78.4365593695155,9.57550794516687,134.440654960983));
#67996=CARTESIAN_POINT('',(78.4365593737638,9.57550795670799,134.));
#67997=CARTESIAN_POINT('Ctrl Pts',(78.4365593695155,9.57550794516687,134.440654960983));
#67998=CARTESIAN_POINT('Ctrl Pts',(78.4717534098169,9.67111703800434,134.433522190505));
#67999=CARTESIAN_POINT('Ctrl Pts',(78.5156454552651,9.76330196577179,134.426050259462));
#68000=CARTESIAN_POINT('Ctrl Pts',(78.6055725715436,9.91467496779458,134.413255774226));
#68001=CARTESIAN_POINT('Ctrl Pts',(78.6476779773201,9.97585109071723,134.407912451059));
#68002=CARTESIAN_POINT('Ctrl Pts',(78.7208950245598,10.0683458166058,134.399623746152));
#68003=CARTESIAN_POINT('Ctrl Pts',(78.7494092000487,10.101587755822,134.396595232034));
#68004=CARTESIAN_POINT('Ctrl Pts',(78.7882311734735,10.1433933553685,134.392717792511));
#68005=CARTESIAN_POINT('Ctrl Pts',(78.7973761238583,10.1530081891617,134.391820944744));
#68006=CARTESIAN_POINT('Ctrl Pts',(78.8138136955503,10.1698819958327,134.390237530461));
#68007=CARTESIAN_POINT('Ctrl Pts',(78.8210604278832,10.1771844912938,134.389549030466));
#68008=CARTESIAN_POINT('Ctrl Pts',(78.8353519540154,10.1913216413596,134.388209505794));
#68009=CARTESIAN_POINT('Ctrl Pts',(78.8423904069475,10.1981620763861,134.387558241358));
#68010=CARTESIAN_POINT('Ctrl Pts',(78.8586848634129,10.2137204861971,134.386069439706));
#68011=CARTESIAN_POINT('Ctrl Pts',(78.8679811180378,10.2223955682949,134.385233767959));
#68012=CARTESIAN_POINT('Ctrl Pts',(78.8983105698349,10.2500556642151,134.382550090482));
#68013=CARTESIAN_POINT('Ctrl Pts',(78.9197296884904,10.2686114338002,134.380719977311));
#68014=CARTESIAN_POINT('Ctrl Pts',(79.0426548317125,10.3697315291208,134.370548321813));
#68015=CARTESIAN_POINT('Ctrl Pts',(79.1531340971381,10.4406577670204,134.3626819129));
#68016=CARTESIAN_POINT('Ctrl Pts',(79.3349163426839,10.5291527269294,134.350277274017));
#68017=CARTESIAN_POINT('Ctrl Pts',(79.4009847355871,10.5562206511986,134.345855173336));
#68018=CARTESIAN_POINT('Ctrl Pts',(79.4835238801607,10.584000374267,134.340204787391));
#68019=CARTESIAN_POINT('Ctrl Pts',(79.4985423529536,10.5888187284823,134.339171656379));
#68020=CARTESIAN_POINT('Ctrl Pts',(79.5204991763432,10.5955207920101,134.33765087529));
#68021=CARTESIAN_POINT('Ctrl Pts',(79.52738540625,10.5975741230538,134.337172448045));
#68022=CARTESIAN_POINT('Ctrl Pts',(79.5395001725956,10.6011013139814,134.336327831701));
#68023=CARTESIAN_POINT('Ctrl Pts',(79.5447229565041,10.6025942471699,134.335962744969));
#68024=CARTESIAN_POINT('Ctrl Pts',(79.5561484430879,10.6057998628139,134.335161876589));
#68025=CARTESIAN_POINT('Ctrl Pts',(79.5623536995695,10.6075021356771,134.334725542647));
#68026=CARTESIAN_POINT('Ctrl Pts',(79.5797810505691,10.6121745538988,134.333496551393));
#68027=CARTESIAN_POINT('Ctrl Pts',(79.5910242985964,10.6150633469108,134.33269954875));
#68028=CARTESIAN_POINT('Ctrl Pts',(79.6770221111404,10.6362037307128,134.326576764937));
#68029=CARTESIAN_POINT('Ctrl Pts',(79.7529225796494,10.6493718284977,134.321023978802));
#68030=CARTESIAN_POINT('Ctrl Pts',(79.8863716847609,10.6631051806393,134.311272788271));
#68031=CARTESIAN_POINT('Ctrl Pts',(79.9435573553131,10.666026628933,134.307097168952));
#68032=CARTESIAN_POINT('Ctrl Pts',(80.0835683615011,10.665961027129,134.296979523559));
#68033=CARTESIAN_POINT('Ctrl Pts',(80.1662478239518,10.6597515104948,134.291100279272));
#68034=CARTESIAN_POINT('Ctrl Pts',(80.2707236121087,10.6440153912872,134.283836629884));
#68035=CARTESIAN_POINT('Ctrl Pts',(80.2932420642366,10.6401484879565,134.282280374805));
#68036=CARTESIAN_POINT('Ctrl Pts',(80.3272859169139,10.633578821394,134.279940686102));
#68037=CARTESIAN_POINT('Ctrl Pts',(80.3388730360393,10.6312145521252,134.279146661994));
#68038=CARTESIAN_POINT('Ctrl Pts',(80.3590024547347,10.6268835391473,134.277770999319));
#68039=CARTESIAN_POINT('Ctrl Pts',(80.3675561022312,10.6249724087513,134.277187615218));
#68040=CARTESIAN_POINT('Ctrl Pts',(80.3868119500423,10.6205102742645,134.275876783885));
#68041=CARTESIAN_POINT('Ctrl Pts',(80.3975048341847,10.6179205636449,134.275150604561));
#68042=CARTESIAN_POINT('Ctrl Pts',(80.426462197628,10.6106029639376,134.273188219848));
#68043=CARTESIAN_POINT('Ctrl Pts',(80.4446736378678,10.6056703635157,134.271958618735));
#68044=CARTESIAN_POINT('Ctrl Pts',(80.5580078175167,10.5728973886081,134.264327463464));
#68045=CARTESIAN_POINT('Ctrl Pts',(80.6505763286658,10.53692323142,134.258203402104));
#68046=CARTESIAN_POINT('Ctrl Pts',(80.8035679698344,10.4611505315518,134.247760058908));
#68047=CARTESIAN_POINT('Ctrl Pts',(80.8656108827619,10.425271703696,134.243418208718));
#68048=CARTESIAN_POINT('Ctrl Pts',(80.955803724873,10.3650471629056,134.236683650588));
#68049=CARTESIAN_POINT('Ctrl Pts',(80.985766829958,10.3435690989589,134.234368599642));
#68050=CARTESIAN_POINT('Ctrl Pts',(81.0273755962566,10.3116018045944,134.231003249736));
#68051=CARTESIAN_POINT('Ctrl Pts',(81.039625270246,10.3019136564475,134.229993002769));
#68052=CARTESIAN_POINT('Ctrl Pts',(81.0611431150497,10.2843980711431,134.228179755869));
#68053=CARTESIAN_POINT('Ctrl Pts',(81.0704655439687,10.2766387953932,134.227380910594));
#68054=CARTESIAN_POINT('Ctrl Pts',(81.0846327705929,10.2645828047962,134.226144889673));
#68055=CARTESIAN_POINT('Ctrl Pts',(81.0895388497703,10.2603582857805,134.225712728893));
#68056=CARTESIAN_POINT('Ctrl Pts',(81.0985512418213,10.2525059645829,134.224910922071));
#68057=CARTESIAN_POINT('Ctrl Pts',(81.1026644322755,10.2488863715036,134.224541866833));
#68058=CARTESIAN_POINT('Ctrl Pts',(81.1120218309677,10.2405696318755,134.223695163274));
#68059=CARTESIAN_POINT('Ctrl Pts',(81.1172541714244,10.235859488779,134.22321657594));
#68060=CARTESIAN_POINT('Ctrl Pts',(81.133827277232,10.2207491483756,134.221684661446));
#68061=CARTESIAN_POINT('Ctrl Pts',(81.1450534976661,10.2102252779089,134.220622820074));
#68062=CARTESIAN_POINT('Ctrl Pts',(81.2492013953704,10.1098468775308,134.210555269639));
#68063=CARTESIAN_POINT('Ctrl Pts',(81.3315103269491,10.0096247672927,134.200990320769));
#68064=CARTESIAN_POINT('Ctrl Pts',(81.4498942791623,9.82547168943415,134.1851748068));
#68065=CARTESIAN_POINT('Ctrl Pts',(81.4922220469123,9.74624058084547,134.178822287609));
#68066=CARTESIAN_POINT('Ctrl Pts',(81.5353121423154,9.64707956838064,134.171434710219));
#68067=CARTESIAN_POINT('Ctrl Pts',(81.5423733435618,9.63006337658953,134.170185456192));
#68068=CARTESIAN_POINT('Ctrl Pts',(81.5531637218669,9.60279134563995,134.168211714246));
#68069=CARTESIAN_POINT('Ctrl Pts',(81.5570767196664,9.59261037129318,134.167481109577));
#68070=CARTESIAN_POINT('Ctrl Pts',(81.5642994349045,9.57325249807744,134.166103419677));
#68071=CARTESIAN_POINT('Ctrl Pts',(81.567629063061,9.56408357195772,134.16545569432));
#68072=CARTESIAN_POINT('Ctrl Pts',(81.5750273495003,9.54313907051892,134.163986767324));
#68073=CARTESIAN_POINT('Ctrl Pts',(81.5790448685575,9.53134595013395,134.163167283554));
#68074=CARTESIAN_POINT('Ctrl Pts',(81.5910806614151,9.49467318798527,134.160641522239));
#68075=CARTESIAN_POINT('Ctrl Pts',(81.5986462271919,9.46964837359512,134.158949999286));
#68076=CARTESIAN_POINT('Ctrl Pts',(81.6411775401056,9.31600138516183,134.148736305119));
#68077=CARTESIAN_POINT('Ctrl Pts',(81.6611923991752,9.18374758227627,134.14072090391));
#68078=CARTESIAN_POINT('Ctrl Pts',(81.6674194862762,8.97846918028418,134.128123847904));
#68079=CARTESIAN_POINT('Ctrl Pts',(81.6649268959898,8.90636581012944,134.123658054442));
#68080=CARTESIAN_POINT('Ctrl Pts',(81.6562025417169,8.81889162830616,134.117955261184));
#68081=CARTESIAN_POINT('Ctrl Pts',(81.6544050883785,8.80314761834793,134.116917400582));
#68082=CARTESIAN_POINT('Ctrl Pts',(81.6514648583346,8.78029189447922,134.115390923116));
#68083=CARTESIAN_POINT('Ctrl Pts',(81.6505000343227,8.77315762769281,134.114911626281));
#68084=CARTESIAN_POINT('Ctrl Pts',(81.6487259548289,8.76065036311876,134.114066056469));
#68085=CARTESIAN_POINT('Ctrl Pts',(81.6479366085231,8.75527473396422,134.113700894662));
#68086=CARTESIAN_POINT('Ctrl Pts',(81.6461563682749,8.74355020220027,134.112900574557));
#68087=CARTESIAN_POINT('Ctrl Pts',(81.6451550526002,8.73720324008348,134.112464870509));
#68088=CARTESIAN_POINT('Ctrl Pts',(81.6422483126799,8.71944644920624,134.111239316501));
#68089=CARTESIAN_POINT('Ctrl Pts',(81.640260772931,8.70805070045029,134.110445158203));
#68090=CARTESIAN_POINT('Ctrl Pts',(81.6253827006515,8.62769878644319,134.104795786829));
#68091=CARTESIAN_POINT('Ctrl Pts',(81.6082679814573,8.55960358964008,134.099751553034));
#68092=CARTESIAN_POINT('Ctrl Pts',(81.5821724444974,8.47795678547016,134.09353028303));
#68093=CARTESIAN_POINT('Ctrl Pts',(81.5772210400791,8.46318294905379,134.092397282145));
#68094=CARTESIAN_POINT('Ctrl Pts',(81.5500165615117,8.38563866339634,134.08641730424));
#68095=CARTESIAN_POINT('Ctrl Pts',(81.524220608712,8.32417197039541,134.0815651552));
#68096=CARTESIAN_POINT('Ctrl Pts',(81.4622342756303,8.19820736482847,134.071496195681));
#68097=CARTESIAN_POINT('Ctrl Pts',(81.4252893935586,8.13423248932816,134.066308633628));
#68098=CARTESIAN_POINT('Ctrl Pts',(81.3743818047362,8.0582234247988,134.060064952454));
#68099=CARTESIAN_POINT('Ctrl Pts',(81.3643117476438,8.04369358475773,134.058867228155));
#68100=CARTESIAN_POINT('Ctrl Pts',(81.3477504420116,8.02059189175592,134.056955416699));
#68101=CARTESIAN_POINT('Ctrl Pts',(81.3414043902598,8.01191813720221,134.056235862665));
#68102=CARTESIAN_POINT('Ctrl Pts',(81.3291174349257,7.99546095138826,134.054866992511));
#68103=CARTESIAN_POINT('Ctrl Pts',(81.3231910023655,7.98766733024652,134.05421715313));
#68104=CARTESIAN_POINT('Ctrl Pts',(81.3095146325956,7.97000737072319,134.052740724637));
#68105=CARTESIAN_POINT('Ctrl Pts',(81.3017212023016,7.96017534403954,134.051915894276));
#68106=CARTESIAN_POINT('Ctrl Pts',(81.2806399739871,7.93418821513339,134.049727291466));
#68107=CARTESIAN_POINT('Ctrl Pts',(81.2671574883132,7.91819342487992,134.048371330096));
#68108=CARTESIAN_POINT('Ctrl Pts',(81.1728115718415,7.8104519499025,134.039163307409));
#68109=CARTESIAN_POINT('Ctrl Pts',(81.0823604792179,7.72759629044802,134.031741275172));
#68110=CARTESIAN_POINT('Ctrl Pts',(80.9309654286274,7.6168442623512,134.020277141289));
#68111=CARTESIAN_POINT('Ctrl Pts',(80.8760692804462,7.58143811939194,134.016275171723));
#68112=CARTESIAN_POINT('Ctrl Pts',(80.790461102991,7.53309175100642,134.010050577342));
#68113=CARTESIAN_POINT('Ctrl Pts',(80.7612045315729,7.51769912582214,134.007925635897));
#68114=CARTESIAN_POINT('Ctrl Pts',(80.7230090107625,7.49903246561289,134.005129409953));
#68115=CARTESIAN_POINT('Ctrl Pts',(80.7144710260588,7.49494959836549,134.004502972021));
#68116=CARTESIAN_POINT('Ctrl Pts',(80.7005562138335,7.48844061238148,134.003479042104));
#68117=CARTESIAN_POINT('Ctrl Pts',(80.6952003287852,7.48596985130118,134.003084213235));
#68118=CARTESIAN_POINT('Ctrl Pts',(80.6847248401779,7.48120463262235,134.002310368956));
#68119=CARTESIAN_POINT('Ctrl Pts',(80.6796065806318,7.47890750875482,134.001931519594));
#68120=CARTESIAN_POINT('Ctrl Pts',(80.6668202692552,7.47324630488577,134.000983382627));
#68121=CARTESIAN_POINT('Ctrl Pts',(80.6591383430751,7.46991413498947,134.000412230716));
#68122=CARTESIAN_POINT('Ctrl Pts',(80.6315242939161,7.45818259653272,133.998354540622));
#68123=CARTESIAN_POINT('Ctrl Pts',(80.6114550711116,7.45011406010067,133.996850570291));
#68124=CARTESIAN_POINT('Ctrl Pts',(80.4916245280058,7.40462750030144,133.987843672003));
#68125=CARTESIAN_POINT('Ctrl Pts',(80.388621751089,7.37646093642236,133.980010302708));
#68126=CARTESIAN_POINT('Ctrl Pts',(80.1990335284948,7.34370480911231,133.966054588333));
#68127=CARTESIAN_POINT('Ctrl Pts',(80.1134128065259,7.33564746488484,133.959912346471));
#68128=CARTESIAN_POINT('Ctrl Pts',(79.9985594831699,7.33374847760258,133.951957176601));
#68129=CARTESIAN_POINT('Ctrl Pts',(79.9695680245425,7.33402572411456,133.949972205689));
#68130=CARTESIAN_POINT('Ctrl Pts',(79.9276388698942,7.3355217058213,133.94713316799));
#68131=CARTESIAN_POINT('Ctrl Pts',(79.9146863464289,7.33613530539314,133.946260517242));
#68132=CARTESIAN_POINT('Ctrl Pts',(79.891940011496,7.33747918723407,133.944735342234));
#68133=CARTESIAN_POINT('Ctrl Pts',(79.8821431766625,7.33814495509189,133.944080837117));
#68134=CARTESIAN_POINT('Ctrl Pts',(79.8617332644356,7.33971335414146,133.942722033578));
#68135=CARTESIAN_POINT('Ctrl Pts',(79.8511217790143,7.34063122821057,133.942018242842));
#68136=CARTESIAN_POINT('Ctrl Pts',(79.8233708843971,7.34329998063211,133.940184256715));
#68137=CARTESIAN_POINT('Ctrl Pts',(79.8062482696252,7.34521508897377,133.939059229406));
#68138=CARTESIAN_POINT('Ctrl Pts',(79.729846399537,7.35496256964079,133.934064647661));
#68139=CARTESIAN_POINT('Ctrl Pts',(79.6709813137082,7.36571759223016,133.930286982939));
#68140=CARTESIAN_POINT('Ctrl Pts',(79.5110234161314,7.40393879256718,133.92006358903));
#68141=CARTESIAN_POINT('Ctrl Pts',(79.4117517666636,7.43779866347004,133.913776385343));
#68142=CARTESIAN_POINT('Ctrl Pts',(79.2771189196786,7.49838544137152,133.904658568878));
#68143=CARTESIAN_POINT('Ctrl Pts',(79.2386239628447,7.51753267652199,133.901975605468));
#68144=CARTESIAN_POINT('Ctrl Pts',(79.185772786292,7.54642239771882,133.89812611215));
#68145=CARTESIAN_POINT('Ctrl Pts',(79.1707606110715,7.55493398517142,133.897013152933));
#68146=CARTESIAN_POINT('Ctrl Pts',(79.144589270734,7.57031467942988,133.895033377468));
#68147=CARTESIAN_POINT('Ctrl Pts',(79.1333736616278,7.57708524674022,133.894171889332));
#68148=CARTESIAN_POINT('Ctrl Pts',(79.1165669096028,7.58750344509526,133.89285923895));
#68149=CARTESIAN_POINT('Ctrl Pts',(79.1109156271945,7.59105375652308,133.892414100823));
#68150=CARTESIAN_POINT('Ctrl Pts',(79.1006767501204,7.5975722664739,133.891600454173));
#68151=CARTESIAN_POINT('Ctrl Pts',(79.0960822335142,7.60052919843287,133.891232676755));
#68152=CARTESIAN_POINT('Ctrl Pts',(79.0857122386401,7.60727547479778,133.890396526846));
#68153=CARTESIAN_POINT('Ctrl Pts',(79.0799457689899,7.61107814424571,133.889927301711));
#68154=CARTESIAN_POINT('Ctrl Pts',(79.0623277990385,7.62285408349946,133.888480972167));
#68155=CARTESIAN_POINT('Ctrl Pts',(79.0505554172563,7.63094376228111,133.887496710809));
#68156=CARTESIAN_POINT('Ctrl Pts',(78.9457899123003,7.7049370416856,133.878586364187));
#68157=CARTESIAN_POINT('Ctrl Pts',(78.8596916831411,7.78006546219407,133.870204991479));
#68158=CARTESIAN_POINT('Ctrl Pts',(78.7209618818999,7.92873594493842,133.85544274897));
#68159=CARTESIAN_POINT('Ctrl Pts',(78.6653321864532,7.99889503028003,133.84903941248));
#68160=CARTESIAN_POINT('Ctrl Pts',(78.5994406429063,8.09731914270485,133.840836179085));
#68161=CARTESIAN_POINT('Ctrl Pts',(78.5839190152081,8.12186899017604,133.838847548913));
#68162=CARTESIAN_POINT('Ctrl Pts',(78.5624013561224,8.15795813791738,133.836004308962));
#68163=CARTESIAN_POINT('Ctrl Pts',(78.5558867540909,8.16918033972146,133.835131038241));
#68164=CARTESIAN_POINT('Ctrl Pts',(78.5446730298935,8.18902783685474,133.833605155122));
#68165=CARTESIAN_POINT('Ctrl Pts',(78.5399179056304,8.19762058593297,133.832950556056));
#68166=CARTESIAN_POINT('Ctrl Pts',(78.5301664535987,8.21561572017753,133.831591912922));
#68167=CARTESIAN_POINT('Ctrl Pts',(78.5251837085998,8.22502498874853,133.830888373463));
#68168=CARTESIAN_POINT('Ctrl Pts',(78.5123837571888,8.24976665037211,133.829055830354));
#68169=CARTESIAN_POINT('Ctrl Pts',(78.5047131914249,8.26517378864806,133.827931979447));
#68170=CARTESIAN_POINT('Ctrl Pts',(78.4715818485716,8.33438952014141,133.822955704477));
#68171=CARTESIAN_POINT('Ctrl Pts',(78.4487755266755,8.3894239231307,133.819194279212));
#68172=CARTESIAN_POINT('Ctrl Pts',(78.3874605661852,8.56316532165436,133.807739248082));
#68173=CARTESIAN_POINT('Ctrl Pts',(78.3592967448776,8.68504337033533,133.800310442124));
#68174=CARTESIAN_POINT('Ctrl Pts',(78.3415069564533,8.83912280758562,133.79060816018));
#68175=CARTESIAN_POINT('Ctrl Pts',(78.3388471401507,8.86941820951917,133.788684127488));
#68176=CARTESIAN_POINT('Ctrl Pts',(78.3358148753454,8.91972728041939,133.785437379776));
#68177=CARTESIAN_POINT('Ctrl Pts',(78.3349713560226,8.93970599466852,133.784134560203));
#68178=CARTESIAN_POINT('Ctrl Pts',(78.3342967629445,8.96758129161905,133.782291999451));
#68179=CARTESIAN_POINT('Ctrl Pts',(78.3341619212957,8.97546969345619,133.78176780665));
#68180=CARTESIAN_POINT('Ctrl Pts',(78.3340274107861,8.98893507310451,133.780867837847));
#68181=CARTESIAN_POINT('Ctrl Pts',(78.3339997062066,8.99451175506259,133.780493595106));
#68182=CARTESIAN_POINT('Ctrl Pts',(78.3340003253419,9.00617081158276,133.779707828496));
#68183=CARTESIAN_POINT('Ctrl Pts',(78.3340339570425,9.01225298347197,133.779296039333));
#68184=CARTESIAN_POINT('Ctrl Pts',(78.3342142740156,9.0286366550134,133.778181977064));
#68185=CARTESIAN_POINT('Ctrl Pts',(78.3344232112333,9.03893700301425,133.777476439763));
#68186=CARTESIAN_POINT('Ctrl Pts',(78.3360154195585,9.09279080067836,133.773763074316));
#68187=CARTESIAN_POINT('Ctrl Pts',(78.3390114485997,9.13627592012142,133.770680929117));
#68188=CARTESIAN_POINT('Ctrl Pts',(78.3559301549065,9.29231160739358,133.7594283155));
#68189=CARTESIAN_POINT('Ctrl Pts',(78.3796274787048,9.4034931184064,133.751070147562));
#68190=CARTESIAN_POINT('Ctrl Pts',(78.4213757555641,9.5329283937359,133.741325712562));
#68191=CARTESIAN_POINT('Ctrl Pts',(78.428752080249,9.5542984480888,133.739715322682));
#68192=CARTESIAN_POINT('Ctrl Pts',(78.4365593568556,9.5755079107748,133.73811642446));
#68193=CARTESIAN_POINT('Ctrl Pts',(78.4365594251401,9.5755080962782,133.933539779158));
#68194=CARTESIAN_POINT('Ctrl Pts',(78.4292827696383,9.55574014073706,133.935004724177));
#68195=CARTESIAN_POINT('Ctrl Pts',(78.4223785847212,9.5358275358506,133.936458722568));
#68196=CARTESIAN_POINT('Ctrl Pts',(78.4098685575793,9.49740473250551,133.939223437784));
#68197=CARTESIAN_POINT('Ctrl Pts',(78.4042055386525,9.47892542613148,133.940535321508));
#68198=CARTESIAN_POINT('Ctrl Pts',(78.3957986621001,9.44968569135736,133.942584064875));
#68199=CARTESIAN_POINT('Ctrl Pts',(78.3928387794976,9.43898972102187,133.943327871012));
#68200=CARTESIAN_POINT('Ctrl Pts',(78.3874866924185,9.41886914002329,133.944716814553));
#68201=CARTESIAN_POINT('Ctrl Pts',(78.3850697044886,9.40945167123947,133.945362727448));
#68202=CARTESIAN_POINT('Ctrl Pts',(78.379818829415,9.38822224508079,133.94680966347));
#68203=CARTESIAN_POINT('Ctrl Pts',(78.3770313841504,9.37639928547213,133.947609166515));
#68204=CARTESIAN_POINT('Ctrl Pts',(78.3691885495291,9.34142565176383,133.949956423171));
#68205=CARTESIAN_POINT('Ctrl Pts',(78.3644973321265,9.31819581511957,133.951492602172));
#68206=CARTESIAN_POINT('Ctrl Pts',(78.3427139805689,9.19706531134075,133.959398109159));
#68207=CARTESIAN_POINT('Ctrl Pts',(78.333910218766,9.09787589607775,133.965502739526));
#68208=CARTESIAN_POINT('Ctrl Pts',(78.3341019470699,8.88724216840797,133.978370404461));
#68209=CARTESIAN_POINT('Ctrl Pts',(78.3453445218236,8.77630641058436,133.985095466586));
#68210=CARTESIAN_POINT('Ctrl Pts',(78.3704604189554,8.65305748572697,133.993274686661));
#68211=CARTESIAN_POINT('Ctrl Pts',(78.373557302935,8.63881795150663,133.994230825064));
#68212=CARTESIAN_POINT('Ctrl Pts',(78.3784090194991,8.61783883427495,133.995658511274));
#68213=CARTESIAN_POINT('Ctrl Pts',(78.3800200632685,8.61106624615768,133.996122349285));
#68214=CARTESIAN_POINT('Ctrl Pts',(78.3829713986039,8.59899580431812,133.996954615568));
#68215=CARTESIAN_POINT('Ctrl Pts',(78.3842953744662,8.59369417438305,133.997322116891));
#68216=CARTESIAN_POINT('Ctrl Pts',(78.3872818226931,8.58198092045737,133.998138437268));
#68217=CARTESIAN_POINT('Ctrl Pts',(78.3889564365218,8.57557273526007,133.998587914231));
#68218=CARTESIAN_POINT('Ctrl Pts',(78.3939939260773,8.55675538646089,133.999915916189));
#68219=CARTESIAN_POINT('Ctrl Pts',(78.3974621993928,8.5443752977656,134.000800054597));
#68220=CARTESIAN_POINT('Ctrl Pts',(78.4058039318622,8.51587342677483,134.002857798219));
#68221=CARTESIAN_POINT('Ctrl Pts',(78.4107792279849,8.49978311450435,134.0040360492));
#68222=CARTESIAN_POINT('Ctrl Pts',(78.428821732205,8.44442122607083,134.008141407812));
#68223=CARTESIAN_POINT('Ctrl Pts',(78.4431072005666,8.40556472504274,134.011112642033));
#68224=CARTESIAN_POINT('Ctrl Pts',(78.5067069662335,8.25064794641112,134.023229987836));
#68225=CARTESIAN_POINT('Ctrl Pts',(78.5676843445167,8.13980698015248,134.032491073314));
#68226=CARTESIAN_POINT('Ctrl Pts',(78.6660831901528,8.00091694717258,134.044461408363));
#68227=CARTESIAN_POINT('Ctrl Pts',(78.6929988890228,7.96595468162453,134.047515227136));
#68228=CARTESIAN_POINT('Ctrl Pts',(78.7312816391157,7.9201141106541,134.051577554172));
#68229=CARTESIAN_POINT('Ctrl Pts',(78.7414587805668,7.90827025272771,134.052632795706));
#68230=CARTESIAN_POINT('Ctrl Pts',(78.7586276623913,7.88884881788925,134.054373205629));
#68231=CARTESIAN_POINT('Ctrl Pts',(78.7655257267966,7.88119013808065,134.055062190782));
#68232=CARTESIAN_POINT('Ctrl Pts',(78.7792396077382,7.86624535739449,134.05641218649));
#68233=CARTESIAN_POINT('Ctrl Pts',(78.7860506671652,7.85895550059733,134.05707335696));
#68234=CARTESIAN_POINT('Ctrl Pts',(78.8025323136292,7.84162986995193,134.058651505359));
#68235=CARTESIAN_POINT('Ctrl Pts',(78.8122642524354,7.83165329138682,134.059565793758));
#68236=CARTESIAN_POINT('Ctrl Pts',(78.8469171865273,7.79700979063132,134.062761953827));
#68237=CARTESIAN_POINT('Ctrl Pts',(78.8724915709273,7.77300756384942,134.065014972303));
#68238=CARTESIAN_POINT('Ctrl Pts',(78.9383230163171,7.71502094328138,134.070581454987));
#68239=CARTESIAN_POINT('Ctrl Pts',(78.9794700518876,7.6821045395804,134.073855840616));
#68240=CARTESIAN_POINT('Ctrl Pts',(79.0998222603495,7.59484888620787,134.083006360312));
#68241=CARTESIAN_POINT('Ctrl Pts',(79.1822547195393,7.54533134956343,134.088782132031));
#68242=CARTESIAN_POINT('Ctrl Pts',(79.314691453025,7.48060774315112,134.097952739101));
#68243=CARTESIAN_POINT('Ctrl Pts',(79.3619109959993,7.4601811976655,134.101205579418));
#68244=CARTESIAN_POINT('Ctrl Pts',(79.4202678761006,7.43808215511817,134.105293019905));
#68245=CARTESIAN_POINT('Ctrl Pts',(79.4305796641964,7.43429340073857,134.106017783195));
#68246=CARTESIAN_POINT('Ctrl Pts',(79.4468567163556,7.42849495057426,134.107166870708));
#68247=CARTESIAN_POINT('Ctrl Pts',(79.4527974057639,7.4264165321767,134.10758730846));
#68248=CARTESIAN_POINT('Ctrl Pts',(79.4639589770602,7.42258237566908,134.10837946313));
#68249=CARTESIAN_POINT('Ctrl Pts',(79.469176962349,7.42081880742468,134.108750720923));
#68250=CARTESIAN_POINT('Ctrl Pts',(79.4814640972008,7.41673379388088,134.109627046339));
#68251=CARTESIAN_POINT('Ctrl Pts',(79.4885401527792,7.41443379787537,134.110133324271));
#68252=CARTESIAN_POINT('Ctrl Pts',(79.5120478338653,7.40696660971541,134.111820031297));
#68253=CARTESIAN_POINT('Ctrl Pts',(79.5285435615917,7.40200705012318,134.113011324654));
#68254=CARTESIAN_POINT('Ctrl Pts',(79.5689576453855,7.39053645909651,134.115943816239));
#68255=CARTESIAN_POINT('Ctrl Pts',(79.5929497358112,7.38430189950451,134.117696397838));
#68256=CARTESIAN_POINT('Ctrl Pts',(79.6943259687317,7.36035958894112,134.125127285409));
#68257=CARTESIAN_POINT('Ctrl Pts',(79.7727835603266,7.34765949977901,134.130934681421));
#68258=CARTESIAN_POINT('Ctrl Pts',(79.9540430108181,7.3314761693961,134.144159920278));
#68259=CARTESIAN_POINT('Ctrl Pts',(80.0568808706016,7.33181091585703,134.151514475538));
#68260=CARTESIAN_POINT('Ctrl Pts',(80.1825333510307,7.34386166571305,134.160204110095));
#68261=CARTESIAN_POINT('Ctrl Pts',(80.2059685914751,7.34661267553775,134.161813033239));
#68262=CARTESIAN_POINT('Ctrl Pts',(80.2413484885229,7.35152982092665,134.1642253242));
#68263=CARTESIAN_POINT('Ctrl Pts',(80.253340092762,7.3533300770676,134.16504003577));
#68264=CARTESIAN_POINT('Ctrl Pts',(80.2749078495667,7.35680915130232,134.166500430426));
#68265=CARTESIAN_POINT('Ctrl Pts',(80.2844908825668,7.35844115682495,134.167147558405));
#68266=CARTESIAN_POINT('Ctrl Pts',(80.3049968846645,7.36211832573745,134.168528772613));
#68267=CARTESIAN_POINT('Ctrl Pts',(80.3159148288969,7.36418909727171,134.169262014424));
#68268=CARTESIAN_POINT('Ctrl Pts',(80.3458290817464,7.37017350912847,134.171265674622));
#68269=CARTESIAN_POINT('Ctrl Pts',(80.3647794256104,7.37430994167322,134.172528993386));
#68270=CARTESIAN_POINT('Ctrl Pts',(80.4949918326228,7.40512401197013,134.181177420844));
#68271=CARTESIAN_POINT('Ctrl Pts',(80.6033237838827,7.44287085822383,134.188181742833));
#68272=CARTESIAN_POINT('Ctrl Pts',(80.8003166559047,7.53518514326631,134.201466172693));
#68273=CARTESIAN_POINT('Ctrl Pts',(80.8894137990673,7.58751050261682,134.207730718492));
#68274=CARTESIAN_POINT('Ctrl Pts',(80.985371672674,7.65656128276603,134.215410054106));
#68275=CARTESIAN_POINT('Ctrl Pts',(80.9975311542382,7.6655651094126,134.216401997883));
#68276=CARTESIAN_POINT('Ctrl Pts',(81.0151872144262,7.67901519384399,134.217873010427));
#68277=CARTESIAN_POINT('Ctrl Pts',(81.0207812013519,7.68333312000774,134.218343681427));
#68278=CARTESIAN_POINT('Ctrl Pts',(81.0306567116587,7.69105665848395,134.219183150422));
#68279=CARTESIAN_POINT('Ctrl Pts',(81.0349491721654,7.69444795658702,134.219550951431));
#68280=CARTESIAN_POINT('Ctrl Pts',(81.0443358553451,7.70193937711952,134.220361760343));
#68281=CARTESIAN_POINT('Ctrl Pts',(81.0494226004676,7.7060483156635,134.220805366688));
#68282=CARTESIAN_POINT('Ctrl Pts',(81.0641202472575,7.718064357426,134.222099107279));
#68283=CARTESIAN_POINT('Ctrl Pts',(81.0736666537819,7.72604914307242,134.222954440932));
#68284=CARTESIAN_POINT('Ctrl Pts',(81.1511393244527,7.79233796605027,134.23001380237));
#68285=CARTESIAN_POINT('Ctrl Pts',(81.2143478908648,7.85591734582821,134.236517821913));
#68286=CARTESIAN_POINT('Ctrl Pts',(81.3536801647676,8.02068697694039,134.252224711899));
#68287=CARTESIAN_POINT('Ctrl Pts',(81.4240099031207,8.12609427616564,134.261361197319));
#68288=CARTESIAN_POINT('Ctrl Pts',(81.4911808132693,8.25679019836835,134.271464199248));
#68289=CARTESIAN_POINT('Ctrl Pts',(81.5002638658933,8.2753004582786,134.272869995471));
#68290=CARTESIAN_POINT('Ctrl Pts',(81.5143382192573,8.30538186762996,134.275115400431));
#68291=CARTESIAN_POINT('Ctrl Pts',(81.5195456956089,8.31684885552939,134.275962358245));
#68292=CARTESIAN_POINT('Ctrl Pts',(81.5285604575656,8.33731279343818,134.277458306956));
#68293=CARTESIAN_POINT('Ctrl Pts',(81.5324195237557,8.34628613570786,134.278109040574));
#68294=CARTESIAN_POINT('Ctrl Pts',(81.540389176041,8.36527612225781,134.27947541763));
#68295=CARTESIAN_POINT('Ctrl Pts',(81.5444814996683,8.37529997506769,134.280190418696));
#68296=CARTESIAN_POINT('Ctrl Pts',(81.5551375599044,8.40214615932136,134.282089272543));
#68297=CARTESIAN_POINT('Ctrl Pts',(81.5615261301565,8.41903680727938,134.283267247005));
#68298=CARTESIAN_POINT('Ctrl Pts',(81.5950770012891,8.51229623372557,134.289685905848));
#68299=CARTESIAN_POINT('Ctrl Pts',(81.6169146373465,8.59046963469517,134.294747577581));
#68300=CARTESIAN_POINT('Ctrl Pts',(81.6405770225901,8.70753636567241,134.302093818309));
#68301=CARTESIAN_POINT('Ctrl Pts',(81.6468769238953,8.74539360741391,134.304435841777));
#68302=CARTESIAN_POINT('Ctrl Pts',(81.6648733724003,8.88266271293565,134.312889590771));
#68303=CARTESIAN_POINT('Ctrl Pts',(81.6689133593665,8.98284781760037,134.318980025011));
#68304=CARTESIAN_POINT('Ctrl Pts',(81.6631858489151,9.09798325804285,134.326464228381));
#68305=CARTESIAN_POINT('Ctrl Pts',(81.6622208071392,9.11318054263232,134.327462062326));
#68306=CARTESIAN_POINT('Ctrl Pts',(81.6604995116557,9.13545472222088,134.32894198442));
#68307=CARTESIAN_POINT('Ctrl Pts',(81.6599059739023,9.14254389913312,134.329415593353));
#68308=CARTESIAN_POINT('Ctrl Pts',(81.6587744483283,9.15509163005926,134.330258819551));
#68309=CARTESIAN_POINT('Ctrl Pts',(81.6582548812689,9.16055164785982,134.330627414616));
#68310=CARTESIAN_POINT('Ctrl Pts',(81.6570687683985,9.17239575021775,134.331430717949));
#68311=CARTESIAN_POINT('Ctrl Pts',(81.6563922993576,9.17877848038597,134.331865938271));
#68312=CARTESIAN_POINT('Ctrl Pts',(81.6543599356357,9.19695193197278,134.333111456928));
#68313=CARTESIAN_POINT('Ctrl Pts',(81.6529149367816,9.20873200953898,134.333926396938));
#68314=CARTESIAN_POINT('Ctrl Pts',(81.6493342434214,9.23554872486521,134.335797389002));
#68315=CARTESIAN_POINT('Ctrl Pts',(81.6471185599384,9.25057346553193,134.336857041338));
#68316=CARTESIAN_POINT('Ctrl Pts',(81.6215515157509,9.40891522731972,134.348130798183));
#68317=CARTESIAN_POINT('Ctrl Pts',(81.5797647521216,9.54862355016414,134.35893263322));
#68318=CARTESIAN_POINT('Ctrl Pts',(81.4935541903558,9.74105368209058,134.373993201831));
#68319=CARTESIAN_POINT('Ctrl Pts',(81.4631973685814,9.79932477347735,134.378592525845));
#68320=CARTESIAN_POINT('Ctrl Pts',(81.4204118118372,9.87080296011738,134.384277892558));
#68321=CARTESIAN_POINT('Ctrl Pts',(81.4111065614483,9.88580236193422,134.385473753312));
#68322=CARTESIAN_POINT('Ctrl Pts',(81.3957586771143,9.90968623527289,134.38738319654));
#68323=CARTESIAN_POINT('Ctrl Pts',(81.3898656277605,9.91866472529193,134.388102224063));
#68324=CARTESIAN_POINT('Ctrl Pts',(81.3784357055735,9.93571728264751,134.389470466152));
#68325=CARTESIAN_POINT('Ctrl Pts',(81.3729137001607,9.94380072384735,134.39012020017));
#68326=CARTESIAN_POINT('Ctrl Pts',(81.3600278108871,9.96231143156325,134.391611003564));
#68327=CARTESIAN_POINT('Ctrl Pts',(81.3526146325724,9.97270376196015,134.39245015694));
#68328=CARTESIAN_POINT('Ctrl Pts',(81.3286529132681,10.0054913097682,134.395105720157));
#68329=CARTESIAN_POINT('Ctrl Pts',(81.3116615214287,10.0275580448526,134.396905031995));
#68330=CARTESIAN_POINT('Ctrl Pts',(81.2483226798764,10.1056834158241,134.403335698931));
#68331=CARTESIAN_POINT('Ctrl Pts',(81.1988686984716,10.1591206750026,134.407846467255));
#68332=CARTESIAN_POINT('Ctrl Pts',(81.0506790659567,10.299579119196,134.420372121352));
#68333=CARTESIAN_POINT('Ctrl Pts',(80.9449318739748,10.3783779499106,134.428212585468));
#68334=CARTESIAN_POINT('Ctrl Pts',(80.8182619913302,10.4512825090272,134.437709817667));
#68335=CARTESIAN_POINT('Ctrl Pts',(80.8053801951284,10.4584705386873,134.438677099889));
#68336=CARTESIAN_POINT('Ctrl Pts',(80.7862288879123,10.4688258697336,134.440119853789));
#68337=CARTESIAN_POINT('Ctrl Pts',(80.7800316637102,10.4721263189549,134.440587434949));
#68338=CARTESIAN_POINT('Ctrl Pts',(80.7689642403079,10.4779309814886,134.441424078927));
#68339=CARTESIAN_POINT('Ctrl Pts',(80.7641022939745,10.4804504962472,134.44179217973));
#68340=CARTESIAN_POINT('Ctrl Pts',(80.753455623245,10.4859013010626,134.442599551497));
#68341=CARTESIAN_POINT('Ctrl Pts',(80.7476662611274,10.4888227601342,134.443039382238));
#68342=CARTESIAN_POINT('Ctrl Pts',(80.7309504769168,10.4971358848322,134.444311311855));
#68343=CARTESIAN_POINT('Ctrl Pts',(80.7199820400186,10.5024414456951,134.445148354278));
#68344=CARTESIAN_POINT('Ctrl Pts',(80.6251959938193,10.5470143114208,134.452396553142));
#68345=CARTESIAN_POINT('Ctrl Pts',(80.5383071566729,10.5793495783025,134.459129988765));
#68346=CARTESIAN_POINT('Ctrl Pts',(80.3305015798915,10.637533839283,134.474838723062));
#68347=CARTESIAN_POINT('Ctrl Pts',(80.2084656950573,10.6574984451795,134.483746324709));
#68348=CARTESIAN_POINT('Ctrl Pts',(80.0645052553556,10.6648813030621,134.493660293738));
#68349=CARTESIAN_POINT('Ctrl Pts',(80.0436646238897,10.665558209756,134.495082319254));
#68350=CARTESIAN_POINT('Ctrl Pts',(80.0102924973982,10.6660152851486,134.49733917295));
#68351=CARTESIAN_POINT('Ctrl Pts',(79.997767239054,10.6660455862611,134.498181665826));
#68352=CARTESIAN_POINT('Ctrl Pts',(79.9754573623775,10.6658479570174,134.499674539596));
#68353=CARTESIAN_POINT('Ctrl Pts',(79.965672976613,10.6656750641851,134.500326605001));
#68354=CARTESIAN_POINT('Ctrl Pts',(79.9451414961652,10.665131276112,134.501689551222));
#68355=CARTESIAN_POINT('Ctrl Pts',(79.9343952942363,10.6647425187863,134.502399844363));
#68356=CARTESIAN_POINT('Ctrl Pts',(79.905959282621,10.6634380312737,134.504271723231));
#68357=CARTESIAN_POINT('Ctrl Pts',(79.8882787166219,10.6623441684622,134.505427729311));
#68358=CARTESIAN_POINT('Ctrl Pts',(79.796375038728,10.6551853055709,134.511400849813));
#68359=CARTESIAN_POINT('Ctrl Pts',(79.7225978722295,10.6444304813611,134.51606901182));
#68360=CARTESIAN_POINT('Ctrl Pts',(79.5852682836288,10.6149017989144,134.524734195293));
#68361=CARTESIAN_POINT('Ctrl Pts',(79.5216372751277,10.5972099006477,134.528740413662));
#68362=CARTESIAN_POINT('Ctrl Pts',(79.3843706418594,10.5501029584372,134.537624458055));
#68363=CARTESIAN_POINT('Ctrl Pts',(79.3114526527675,10.5191175787064,134.542505410142));
#68364=CARTESIAN_POINT('Ctrl Pts',(79.2269807790108,10.4758882291769,134.548662012659));
#68365=CARTESIAN_POINT('Ctrl Pts',(79.2130432063088,10.4685039127005,134.549695170748));
#68366=CARTESIAN_POINT('Ctrl Pts',(79.1929796770627,10.4575063395732,134.551210853761));
#68367=CARTESIAN_POINT('Ctrl Pts',(79.1867682276615,10.454049727965,134.551684103978));
#68368=CARTESIAN_POINT('Ctrl Pts',(79.1758041225414,10.4478560817909,134.55252693549));
#68369=CARTESIAN_POINT('Ctrl Pts',(79.1710425819683,10.4451351756224,134.55289549816));
#68370=CARTESIAN_POINT('Ctrl Pts',(79.1607340955242,10.4391768439629,134.553699030435));
#68371=CARTESIAN_POINT('Ctrl Pts',(79.1551924934083,10.4359308896811,134.554134514844));
#68372=CARTESIAN_POINT('Ctrl Pts',(79.1394483284626,10.4265861727884,134.55538153999));
#68373=CARTESIAN_POINT('Ctrl Pts',(79.1292923235012,10.4204102962432,134.556197739389));
#68374=CARTESIAN_POINT('Ctrl Pts',(79.0384128396547,10.3638055169821,134.563602268254));
#68375=CARTESIAN_POINT('Ctrl Pts',(78.9620914784457,10.3066588842547,134.570533367854));
#68376=CARTESIAN_POINT('Ctrl Pts',(78.8008697701194,10.162863868255,134.586259005378));
#68377=CARTESIAN_POINT('Ctrl Pts',(78.7196727220553,10.0728177145332,134.594986297006));
#68378=CARTESIAN_POINT('Ctrl Pts',(78.6366415339469,9.95773204050071,134.604748412558));
#68379=CARTESIAN_POINT('Ctrl Pts',(78.6246776784905,9.94047091927356,134.60618091296));
#68380=CARTESIAN_POINT('Ctrl Pts',(78.6060805321219,9.91252531414578,134.608451025808));
#68381=CARTESIAN_POINT('Ctrl Pts',(78.5992366254061,9.90198443185305,134.609296446346));
#68382=CARTESIAN_POINT('Ctrl Pts',(78.5872737879914,9.88309485330583,134.610792647012));
#68383=CARTESIAN_POINT('Ctrl Pts',(78.5821080271373,9.87477667456243,134.611445138275));
#68384=CARTESIAN_POINT('Ctrl Pts',(78.5714349500713,9.85724737267127,134.612807122053));
#68385=CARTESIAN_POINT('Ctrl Pts',(78.5659426808873,9.84802757880847,134.613516043089));
#68386=CARTESIAN_POINT('Ctrl Pts',(78.551672706782,9.82353764321999,134.615380058359));
#68387=CARTESIAN_POINT('Ctrl Pts',(78.5430472517491,9.80818000839586,134.61652965884));
#68388=CARTESIAN_POINT('Ctrl Pts',(78.5000523691766,9.72870127932335,134.622385815212));
#68389=CARTESIAN_POINT('Ctrl Pts',(78.4696638823641,9.66251168730783,134.626950764182));
#68390=CARTESIAN_POINT('Ctrl Pts',(78.4412789673489,9.5882097138014,134.631861484381));
#68391=CARTESIAN_POINT('Ctrl Pts',(78.4388996016047,9.58186548337547,134.632279173869));
#68392=CARTESIAN_POINT('Ctrl Pts',(78.4365593788086,9.57550797041271,134.632696244622));
#68393=CARTESIAN_POINT('Origin',(80.,9.,134.));
#68394=CARTESIAN_POINT('',(78.4365593737638,9.57550795670805,135.330578607084));
#68395=CARTESIAN_POINT('',(78.436559333852,9.57550784828241,135.139259993339));
#68396=CARTESIAN_POINT('',(78.4365593737638,9.57550795670799,134.));
#68397=CARTESIAN_POINT('',(78.3340007521426,9.00139877871345,134.47795709598));
#68398=CARTESIAN_POINT('Ctrl Pts',(78.436559333852,9.57550784828241,135.139259993339));
#68399=CARTESIAN_POINT('Ctrl Pts',(78.4595768295332,9.63803781879155,135.135190034949));
#68400=CARTESIAN_POINT('Ctrl Pts',(78.48633467882,9.69915708210112,135.131135418933));
#68401=CARTESIAN_POINT('Ctrl Pts',(78.5389125131787,9.80197250901578,135.123936741731));
#68402=CARTESIAN_POINT('Ctrl Pts',(78.5630224575881,9.84441170149945,135.120844198812));
#68403=CARTESIAN_POINT('Ctrl Pts',(78.5947306342489,9.89492566985977,135.116936366758));
#68404=CARTESIAN_POINT('Ctrl Pts',(78.600594089363,9.90406693714173,135.11621972521));
#68405=CARTESIAN_POINT('Ctrl Pts',(78.6099809912233,9.91839121479723,135.115080647939));
#68406=CARTESIAN_POINT('Ctrl Pts',(78.6134451542317,9.92361297339697,135.114661987101));
#68407=CARTESIAN_POINT('Ctrl Pts',(78.6200142168467,9.9333947030339,135.113871014238));
#68408=CARTESIAN_POINT('Ctrl Pts',(78.6231124072684,9.93795894725437,135.113499139384));
#68409=CARTESIAN_POINT('Ctrl Pts',(78.6304738652055,9.94868875603311,135.112618382558));
#68410=CARTESIAN_POINT('Ctrl Pts',(78.6347561394962,9.954841026381,135.112108254196));
#68411=CARTESIAN_POINT('Ctrl Pts',(78.6491993564279,9.97529555597973,135.110395607681));
#68412=CARTESIAN_POINT('Ctrl Pts',(78.6595442915055,9.98946562995298,135.109181781516));
#68413=CARTESIAN_POINT('Ctrl Pts',(78.6854148977695,10.0237517388748,135.106182152998));
#68414=CARTESIAN_POINT('Ctrl Pts',(78.7011804707563,10.0436806524863,135.104384326804));
#68415=CARTESIAN_POINT('Ctrl Pts',(78.770530949551,10.1273393577573,135.09662654426));
#68416=CARTESIAN_POINT('Ctrl Pts',(78.8283957107909,10.1873629637841,135.090528050799));
#68417=CARTESIAN_POINT('Ctrl Pts',(78.969608427744,10.3134284072819,135.07678436002));
#68418=CARTESIAN_POINT('Ctrl Pts',(79.0552882169735,10.3763459205111,135.069214044058));
#68419=CARTESIAN_POINT('Ctrl Pts',(79.1624700284796,10.4402952614068,135.060679223039));
#68420=CARTESIAN_POINT('Ctrl Pts',(79.1787177532822,10.4496214727164,135.059408011729));
#68421=CARTESIAN_POINT('Ctrl Pts',(79.2048192615853,10.4640240143684,135.057400675318));
#68422=CARTESIAN_POINT('Ctrl Pts',(79.2145719524751,10.4692792497745,135.056658220562));
#68423=CARTESIAN_POINT('Ctrl Pts',(79.2329037893004,10.4789226616873,135.055276467085));
#68424=CARTESIAN_POINT('Ctrl Pts',(79.2414699375459,10.4833344150064,135.054636357071));
#68425=CARTESIAN_POINT('Ctrl Pts',(79.260911613389,10.4931348418625,135.053195808424));
#68426=CARTESIAN_POINT('Ctrl Pts',(79.271808799099,10.498479525102,135.052396930061));
#68427=CARTESIAN_POINT('Ctrl Pts',(79.3048180336016,10.5142242530074,135.050001816641));
#68428=CARTESIAN_POINT('Ctrl Pts',(79.3271020192118,10.524257675576,135.04841816174));
#68429=CARTESIAN_POINT('Ctrl Pts',(79.3791778856433,10.5463402248736,135.044786816533));
#68430=CARTESIAN_POINT('Ctrl Pts',(79.4091140021764,10.5580250691894,135.04275081985));
#68431=CARTESIAN_POINT('Ctrl Pts',(79.5208019710125,10.5979371338126,135.035310974151));
#68432=CARTESIAN_POINT('Ctrl Pts',(79.6043765441966,10.6206532697851,135.030054517818));
#68433=CARTESIAN_POINT('Ctrl Pts',(79.6942272612181,10.6377068638952,135.024466413443));
#68434=CARTESIAN_POINT('Ctrl Pts',(79.699118059475,10.6386124610672,135.024162405358));
#68435=CARTESIAN_POINT('Ctrl Pts',(79.7870407308366,10.6544856197643,135.018699181239));
#68436=CARTESIAN_POINT('Ctrl Pts',(79.8710774225485,10.6631445377566,135.013513524576));
#68437=CARTESIAN_POINT('Ctrl Pts',(79.9712133501961,10.6658264270786,135.007014882455));
#68438=CARTESIAN_POINT('Ctrl Pts',(79.9870348609031,10.6660246747404,135.005978529663));
#68439=CARTESIAN_POINT('Ctrl Pts',(80.0099746926268,10.6659853481699,135.004458930245));
#68440=CARTESIAN_POINT('Ctrl Pts',(80.0170929929726,10.6659275193683,135.003985023274));
#68441=CARTESIAN_POINT('Ctrl Pts',(80.0296966550466,10.665744341872,135.003141378851));
#68442=CARTESIAN_POINT('Ctrl Pts',(80.035182089349,10.6656375125257,135.002772665828));
#68443=CARTESIAN_POINT('Ctrl Pts',(80.0470838781903,10.6653469034605,135.001969232211));
#68444=CARTESIAN_POINT('Ctrl Pts',(80.0534996296835,10.6651531420862,135.001534000457));
#68445=CARTESIAN_POINT('Ctrl Pts',(80.0717706408757,10.6644956407054,135.000288753083));
#68446=CARTESIAN_POINT('Ctrl Pts',(80.08362200275,10.6639423377607,134.999474100277));
#68447=CARTESIAN_POINT('Ctrl Pts',(80.1904844336595,10.6578087718802,134.992071838171));
#68448=CARTESIAN_POINT('Ctrl Pts',(80.2848507584234,10.6442233634993,134.985141304991));
#68449=CARTESIAN_POINT('Ctrl Pts',(80.4952998086151,10.595260035669,134.969412834063));
#68450=CARTESIAN_POINT('Ctrl Pts',(80.6097575305606,10.555114898904,134.960682148722));
#68451=CARTESIAN_POINT('Ctrl Pts',(80.7378176643581,10.4938614507758,134.950917010713));
#68452=CARTESIAN_POINT('Ctrl Pts',(80.7565884822857,10.4844429521204,134.949484556792));
#68453=CARTESIAN_POINT('Ctrl Pts',(80.786302232231,10.4688236010766,134.947214383048));
#68454=CARTESIAN_POINT('Ctrl Pts',(80.797361201076,10.4628496510365,134.946368857043));
#68455=CARTESIAN_POINT('Ctrl Pts',(80.8169154517957,10.4519989884945,134.944872389066));
#68456=CARTESIAN_POINT('Ctrl Pts',(80.8254372134439,10.447171493526,134.944219736213));
#68457=CARTESIAN_POINT('Ctrl Pts',(80.8432096442333,10.4368955219991,134.942857330438));
#68458=CARTESIAN_POINT('Ctrl Pts',(80.852451242863,10.4314321964071,134.942148150075));
#68459=CARTESIAN_POINT('Ctrl Pts',(80.876721843206,10.4167658062093,134.940283247379));
#68460=CARTESIAN_POINT('Ctrl Pts',(80.891659004499,10.4074128030831,134.939133025982));
#68461=CARTESIAN_POINT('Ctrl Pts',(80.9675789591181,10.3581810806092,134.9332690082));
#68462=CARTESIAN_POINT('Ctrl Pts',(81.0260502414299,10.3145675022484,134.928697289946));
#68463=CARTESIAN_POINT('Ctrl Pts',(81.1593619892043,10.2007988837498,134.917877567722));
#68464=CARTESIAN_POINT('Ctrl Pts',(81.2309443048808,10.127303340571,134.911729872304));
#68465=CARTESIAN_POINT('Ctrl Pts',(81.3280267478551,10.0072759803649,134.902129804689));
#68466=CARTESIAN_POINT('Ctrl Pts',(81.3588137561803,9.96534137660396,134.898842181923));
#68467=CARTESIAN_POINT('Ctrl Pts',(81.3936832742374,9.91286597158227,134.894715513996));
#68468=CARTESIAN_POINT('Ctrl Pts',(81.3996886516148,9.90363101625349,134.893988807344));
#68469=CARTESIAN_POINT('Ctrl Pts',(81.4089846636838,9.88902076959058,134.892837239411));
#68470=CARTESIAN_POINT('Ctrl Pts',(81.4123372547927,9.88368500423325,134.89241629075));
#68471=CARTESIAN_POINT('Ctrl Pts',(81.4185634844085,9.8736498055683,134.891623615563));
#68472=CARTESIAN_POINT('Ctrl Pts',(81.4214441854525,9.86895498512908,134.891252352986));
#68473=CARTESIAN_POINT('Ctrl Pts',(81.4281569679721,9.85789213274889,134.890376603875));
#68474=CARTESIAN_POINT('Ctrl Pts',(81.431969772634,9.85151265497805,134.889870913347));
#68475=CARTESIAN_POINT('Ctrl Pts',(81.444448788892,9.83031226637494,134.888188684681));
#68476=CARTESIAN_POINT('Ctrl Pts',(81.4529282546458,9.81538346376594,134.887001360695));
#68477=CARTESIAN_POINT('Ctrl Pts',(81.4730292090426,9.77868469899812,134.884080792212));
#68478=CARTESIAN_POINT('Ctrl Pts',(81.4844004177947,9.75678278312836,134.882336278665));
#68479=CARTESIAN_POINT('Ctrl Pts',(81.5299828212697,9.6640044249349,134.87496302992));
#68480=CARTESIAN_POINT('Ctrl Pts',(81.559635482426,9.59100389808208,134.869206879877));
#68481=CARTESIAN_POINT('Ctrl Pts',(81.6160813514976,9.41778818137742,134.85596512143));
#68482=CARTESIAN_POINT('Ctrl Pts',(81.6389125309935,9.31660417435719,134.848544516602));
#68483=CARTESIAN_POINT('Ctrl Pts',(81.6552351362672,9.190549172048,134.839794471824));
#68484=CARTESIAN_POINT('Ctrl Pts',(81.657767096704,9.16709486871849,134.838185936527));
#68485=CARTESIAN_POINT('Ctrl Pts',(81.6608454107353,9.13151260438395,134.835773974394));
#68486=CARTESIAN_POINT('Ctrl Pts',(81.6617586641462,9.1194202624968,134.834959211637));
#68487=CARTESIAN_POINT('Ctrl Pts',(81.6631661659548,9.09761579739518,134.833498601627));
#68488=CARTESIAN_POINT('Ctrl Pts',(81.6637075580421,9.08790738119863,134.83285131032));
#68489=CARTESIAN_POINT('Ctrl Pts',(81.6646857187853,9.06708983388079,134.831469611039));
#68490=CARTESIAN_POINT('Ctrl Pts',(81.6650963482185,9.05597990141252,134.830736049229));
#68491=CARTESIAN_POINT('Ctrl Pts',(81.6659184384813,9.02546477680437,134.828731145386));
#68492=CARTESIAN_POINT('Ctrl Pts',(81.6661020643355,9.00605481777819,134.827466915392));
#68493=CARTESIAN_POINT('Ctrl Pts',(81.6657553517935,8.96280345461606,134.824671427951));
#68494=CARTESIAN_POINT('Ctrl Pts',(81.6650524306856,8.93896752365867,134.823145477617));
#68495=CARTESIAN_POINT('Ctrl Pts',(81.6611589647097,8.86261631701194,134.818294478144));
#68496=CARTESIAN_POINT('Ctrl Pts',(81.6559928557438,8.81023259395848,134.815023390367));
#68497=CARTESIAN_POINT('Ctrl Pts',(81.6344255122983,8.66322093320718,134.805876838922));
#68498=CARTESIAN_POINT('Ctrl Pts',(81.612316427257,8.56964984982452,134.800101912622));
#68499=CARTESIAN_POINT('Ctrl Pts',(81.5661516753972,8.42958022776165,134.790927272234));
#68500=CARTESIAN_POINT('Ctrl Pts',(81.5477674300288,8.38143339017847,134.787669044119));
#68501=CARTESIAN_POINT('Ctrl Pts',(81.522792307153,8.32414468076876,134.783575439866));
#68502=CARTESIAN_POINT('Ctrl Pts',(81.5183001488764,8.3141126438614,134.782850283073));
#68503=CARTESIAN_POINT('Ctrl Pts',(81.5110793056081,8.2984054054304,134.781700638172));
#68504=CARTESIAN_POINT('Ctrl Pts',(81.5084170545687,8.29269976022694,134.781280041339));
#68505=CARTESIAN_POINT('Ctrl Pts',(81.50336467134,8.28202993069098,134.780487631935));
#68506=CARTESIAN_POINT('Ctrl Pts',(81.5009821783954,8.27706234566539,134.780116279215));
#68507=CARTESIAN_POINT('Ctrl Pts',(81.4953237456508,8.26541285384464,134.779239778075));
#68508=CARTESIAN_POINT('Ctrl Pts',(81.4920276294024,8.25874098493878,134.778733419276));
#68509=CARTESIAN_POINT('Ctrl Pts',(81.48095434106,8.23669997016199,134.77704663579));
#68510=CARTESIAN_POINT('Ctrl Pts',(81.4729838095861,8.22142994231128,134.775855347865));
#68511=CARTESIAN_POINT('Ctrl Pts',(81.4529702350702,8.18449536905194,134.772922993039));
#68512=CARTESIAN_POINT('Ctrl Pts',(81.4406778902115,8.16297109229459,134.77117054613));
#68513=CARTESIAN_POINT('Ctrl Pts',(81.3870267135645,8.07371117513843,134.763741238432));
#68514=CARTESIAN_POINT('Ctrl Pts',(81.341336430295,8.00870296076878,134.757935350165));
#68515=CARTESIAN_POINT('Ctrl Pts',(81.2263388287413,7.86766591825471,134.744710260202));
#68516=CARTESIAN_POINT('Ctrl Pts',(81.1542689103373,7.79428149358286,134.737354382563));
#68517=CARTESIAN_POINT('Ctrl Pts',(81.0578765739544,7.71275105004603,134.728663376349));
#68518=CARTESIAN_POINT('Ctrl Pts',(81.0395393957121,7.69789760444843,134.727054307098));
#68519=CARTESIAN_POINT('Ctrl Pts',(81.0113080575839,7.67600638428667,134.724641711067));
#68520=CARTESIAN_POINT('Ctrl Pts',(81.0016430053057,7.66867945813251,134.723826839451));
#68521=CARTESIAN_POINT('Ctrl Pts',(80.9840864605018,7.65566954206517,134.722366111667));
#68522=CARTESIAN_POINT('Ctrl Pts',(80.97622367182,7.64994893010276,134.721718810443));
#68523=CARTESIAN_POINT('Ctrl Pts',(80.9592655601433,7.63783659249082,134.720337172478));
#68524=CARTESIAN_POINT('Ctrl Pts',(80.9501554004482,7.6314663728264,134.719603681144));
#68525=CARTESIAN_POINT('Ctrl Pts',(80.9249698491532,7.61422827459938,134.717599184103));
#68526=CARTESIAN_POINT('Ctrl Pts',(80.9087669674189,7.60354908903928,134.716335285497));
#68527=CARTESIAN_POINT('Ctrl Pts',(80.8722537008129,7.58038823382266,134.713540641305));
#68528=CARTESIAN_POINT('Ctrl Pts',(80.8518543935338,7.56805437866129,134.712015197801));
#68529=CARTESIAN_POINT('Ctrl Pts',(80.7856299839704,7.52992994320918,134.707166428122));
#68530=CARTESIAN_POINT('Ctrl Pts',(80.7388449438088,7.50586840734171,134.703897004702));
#68531=CARTESIAN_POINT('Ctrl Pts',(80.603661743914,7.4442491239965,134.69475156433));
#68532=CARTESIAN_POINT('Ctrl Pts',(80.513053586177,7.41206331113077,134.688976222279));
#68533=CARTESIAN_POINT('Ctrl Pts',(80.3702990586206,7.37485630706935,134.679799176776));
#68534=CARTESIAN_POINT('Ctrl Pts',(80.3198439569555,7.36417845165627,134.676538811708));
#68535=CARTESIAN_POINT('Ctrl Pts',(80.2581314695191,7.35408232145139,134.672442808601));
#68536=CARTESIAN_POINT('Ctrl Pts',(80.2472651147339,7.3524148558345,134.671717543446));
#68537=CARTESIAN_POINT('Ctrl Pts',(80.230150472288,7.34996169503671,134.67056776409));
#68538=CARTESIAN_POINT('Ctrl Pts',(80.2239126446682,7.34910364588566,134.670147142652));
#68539=CARTESIAN_POINT('Ctrl Pts',(80.2122079664861,7.34756115590539,134.669354714707));
#68540=CARTESIAN_POINT('Ctrl Pts',(80.2067424029856,7.34686844752748,134.668983368338));
#68541=CARTESIAN_POINT('Ctrl Pts',(80.19388701471,7.34530389645441,134.668106919998));
#68542=CARTESIAN_POINT('Ctrl Pts',(80.1864946807959,7.34445444088535,134.667600608097));
#68543=CARTESIAN_POINT('Ctrl Pts',(80.1619759648962,7.34180328468377,134.665914144554));
#68544=CARTESIAN_POINT('Ctrl Pts',(80.1448279913955,7.34021767842525,134.66472313512));
#68545=CARTESIAN_POINT('Ctrl Pts',(80.1029546813816,7.33699962101212,134.661791608797));
#68546=CARTESIAN_POINT('Ctrl Pts',(80.0782119829312,7.33565247579054,134.660039719719));
#68547=CARTESIAN_POINT('Ctrl Pts',(79.9741769426422,7.3323130279938,134.652614366621));
#68548=CARTESIAN_POINT('Ctrl Pts',(79.8948266089783,7.33543267728944,134.646811988994));
#68549=CARTESIAN_POINT('Ctrl Pts',(79.7140227875555,7.3555239420664,134.633591198007));
#68550=CARTESIAN_POINT('Ctrl Pts',(79.6132923451326,7.37625491741082,134.626236039483));
#68551=CARTESIAN_POINT('Ctrl Pts',(79.4924794818541,7.41300983157092,134.617542352806));
#68552=CARTESIAN_POINT('Ctrl Pts',(79.470010608614,7.42037149447115,134.615930088245));
#68553=CARTESIAN_POINT('Ctrl Pts',(79.4362541554326,7.43223281902356,134.613513699278));
#68554=CARTESIAN_POINT('Ctrl Pts',(79.4248473719495,7.43638151105058,134.612698176615));
#68555=CARTESIAN_POINT('Ctrl Pts',(79.4043851854499,7.44407791036834,134.611236744118));
#68556=CARTESIAN_POINT('Ctrl Pts',(79.395313677967,7.44758091510655,134.610589383219));
#68557=CARTESIAN_POINT('Ctrl Pts',(79.3759451212478,7.45525570856294,134.609208110183));
#68558=CARTESIAN_POINT('Ctrl Pts',(79.3656580385916,7.45945149259336,134.608475038938));
#68559=CARTESIAN_POINT('Ctrl Pts',(79.337549692951,7.47124531524862,134.606472966311));
#68560=CARTESIAN_POINT('Ctrl Pts',(79.3198174265426,7.47905193612013,134.605211042645));
#68561=CARTESIAN_POINT('Ctrl Pts',(79.2002987474682,7.534178404984,134.596703849676));
#68562=CARTESIAN_POINT('Ctrl Pts',(79.1033803906839,7.59137206742112,134.589823415652));
#68563=CARTESIAN_POINT('Ctrl Pts',(78.9278811533166,7.72044313864304,134.576519626134));
#68564=CARTESIAN_POINT('Ctrl Pts',(78.8489726735374,7.79093652603735,134.57011457457));
#68565=CARTESIAN_POINT('Ctrl Pts',(78.7672402454537,7.87925129477731,134.562295530178));
#68566=CARTESIAN_POINT('Ctrl Pts',(78.7573504110862,7.8902269442982,134.56132680261));
#68567=CARTESIAN_POINT('Ctrl Pts',(78.7429742663424,7.90661457736231,134.559882215023));
#68568=CARTESIAN_POINT('Ctrl Pts',(78.7383738375851,7.91192610573639,134.559414272181));
#68569=CARTESIAN_POINT('Ctrl Pts',(78.7302470677872,7.9214298816747,134.558577143894));
#68570=CARTESIAN_POINT('Ctrl Pts',(78.7267076060679,7.92561064453025,134.558208923318));
#68571=CARTESIAN_POINT('Ctrl Pts',(78.7190235218901,7.93477828291706,134.557401479233));
#68572=CARTESIAN_POINT('Ctrl Pts',(78.7148874323616,7.93977185052571,134.556961697435));
#68573=CARTESIAN_POINT('Ctrl Pts',(78.7030686725898,7.95421159584004,134.555690391752));
#68574=CARTESIAN_POINT('Ctrl Pts',(78.6954604622114,7.96371778601726,134.554853933028));
#68575=CARTESIAN_POINT('Ctrl Pts',(78.62665966037,8.05164037652404,134.547128469293));
#68576=CARTESIAN_POINT('Ctrl Pts',(78.5725065577799,8.13529879337757,134.539869065089));
#68577=CARTESIAN_POINT('Ctrl Pts',(78.4880026369898,8.29564766771051,134.526677331998));
#68578=CARTESIAN_POINT('Ctrl Pts',(78.4552417606265,8.37073639724606,134.520753607426));
#68579=CARTESIAN_POINT('Ctrl Pts',(78.4124015647396,8.49271341237347,134.511636873155));
#68580=CARTESIAN_POINT('Ctrl Pts',(78.3985939950807,8.53814715393391,134.508344061591));
#68581=CARTESIAN_POINT('Ctrl Pts',(78.3827529244764,8.59959576188696,134.504024965509));
#68582=CARTESIAN_POINT('Ctrl Pts',(78.3789844705253,8.61513594432263,134.502943853637));
#68583=CARTESIAN_POINT('Ctrl Pts',(78.3731378917345,8.64085717013506,134.501172268919));
#68584=CARTESIAN_POINT('Ctrl Pts',(78.3709303090874,8.65100738955739,134.5004776961));
#68585=CARTESIAN_POINT('Ctrl Pts',(78.3667977765972,8.67090252478805,134.499124894524));
#68586=CARTESIAN_POINT('Ctrl Pts',(78.3648647659361,8.68064530015661,134.498466434605));
#68587=CARTESIAN_POINT('Ctrl Pts',(78.3611942719982,8.70005300453407,134.497162480892));
#68588=CARTESIAN_POINT('Ctrl Pts',(78.3594548795604,8.70971715708942,134.496516951246));
#68589=CARTESIAN_POINT('Ctrl Pts',(78.3555736685381,8.73243147202584,134.495008221625));
#68590=CARTESIAN_POINT('Ctrl Pts',(78.3535015709651,8.74549299401506,134.494147213189));
#68591=CARTESIAN_POINT('Ctrl Pts',(78.3474319850282,8.78693577934105,134.491434719267));
#68592=CARTESIAN_POINT('Ctrl Pts',(78.3440110778587,8.81539706561595,134.489600685518));
#68593=CARTESIAN_POINT('Ctrl Pts',(78.3364011152609,8.89627585539281,134.484454790613));
#68594=CARTESIAN_POINT('Ctrl Pts',(78.3339564019042,8.94882309198879,134.481190393475));
#68595=CARTESIAN_POINT('Ctrl Pts',(78.334000588343,9.00140012801338,134.477956726976));
#68596=CARTESIAN_POINT('Ctrl Pts',(78.334000587195,9.00139876132414,134.477956811032));
#68597=CARTESIAN_POINT('Ctrl Pts',(78.3341144029438,9.13695939446217,134.469619369734));
#68598=CARTESIAN_POINT('Ctrl Pts',(78.3507729491612,9.27198368688069,134.461562220848));
#68599=CARTESIAN_POINT('Ctrl Pts',(78.3865043312805,9.41512871033398,134.452015614116));
#68600=CARTESIAN_POINT('Ctrl Pts',(78.3895374774457,9.42674414342167,134.451233266144));
#68601=CARTESIAN_POINT('Ctrl Pts',(78.3952949355229,9.44785628193003,134.449795506627));
#68602=CARTESIAN_POINT('Ctrl Pts',(78.3979787300738,9.45736356674616,134.449142174374));
#68603=CARTESIAN_POINT('Ctrl Pts',(78.4024251895845,9.47259559702508,134.448085140636));
#68604=CARTESIAN_POINT('Ctrl Pts',(78.4041345039162,9.47833585352387,134.44768442901));
#68605=CARTESIAN_POINT('Ctrl Pts',(78.4074892318674,9.48938362278601,134.446908425406));
#68606=CARTESIAN_POINT('Ctrl Pts',(78.4091303015437,9.49469230413346,134.446533381212));
#68607=CARTESIAN_POINT('Ctrl Pts',(78.4128412140502,9.50648726034336,134.445695424521));
#68608=CARTESIAN_POINT('Ctrl Pts',(78.4149243241241,9.51296925290203,134.445231765119));
#68609=CARTESIAN_POINT('Ctrl Pts',(78.4212156623015,9.5321416841275,134.443851358949));
#68610=CARTESIAN_POINT('Ctrl Pts',(78.4255368765548,9.5447940916601,134.442928665735));
#68611=CARTESIAN_POINT('Ctrl Pts',(78.4321583095151,9.56344447363863,134.441552517316));
#68612=CARTESIAN_POINT('Ctrl Pts',(78.4343415699454,9.56948301017296,134.441104442064));
#68613=CARTESIAN_POINT('Ctrl Pts',(78.4365593695155,9.57550794516687,134.440654960983));
#68614=CARTESIAN_POINT('',(78.33399962793,9.00042833786235,134.670001209792));
#68615=CARTESIAN_POINT('Ctrl Pts',(78.4365593788086,9.57550797041271,134.632696244622));
#68616=CARTESIAN_POINT('Ctrl Pts',(78.3964895291875,9.46665312599119,134.639837428959));
#68617=CARTESIAN_POINT('Ctrl Pts',(78.3678945384663,9.35390299944845,134.646774484532));
#68618=CARTESIAN_POINT('Ctrl Pts',(78.3463552045929,9.20536770540159,134.656260408587));
#68619=CARTESIAN_POINT('Ctrl Pts',(78.342501337998,9.171507483015,134.658447247285));
#68620=CARTESIAN_POINT('Ctrl Pts',(78.338872193526,9.12770335501346,134.661335059154));
#68621=CARTESIAN_POINT('Ctrl Pts',(78.3381436654843,9.11784416823972,134.661988859751));
#68622=CARTESIAN_POINT('Ctrl Pts',(78.3371147150437,9.10200200404197,134.663046400438));
#68623=CARTESIAN_POINT('Ctrl Pts',(78.3367587310335,9.09602269583068,134.663447144266));
#68624=CARTESIAN_POINT('Ctrl Pts',(78.3361542697455,9.0848549763065,134.664198821945));
#68625=CARTESIAN_POINT('Ctrl Pts',(78.3358978010449,9.07966711689634,134.664549308398));
#68626=CARTESIAN_POINT('Ctrl Pts',(78.3354160271824,9.06890111970038,134.665279246728));
#68627=CARTESIAN_POINT('Ctrl Pts',(78.335194491578,9.06332285323331,134.665658898888));
#68628=CARTESIAN_POINT('Ctrl Pts',(78.3346997106691,9.04905618855536,134.666633389127));
#68629=CARTESIAN_POINT('Ctrl Pts',(78.3344664262952,9.04036669725143,134.667230258446));
#68630=CARTESIAN_POINT('Ctrl Pts',(78.3341030873326,9.02126033511182,134.668549398473));
#68631=CARTESIAN_POINT('Ctrl Pts',(78.3340027210372,9.01084335607688,134.669273015857));
#68632=CARTESIAN_POINT('Ctrl Pts',(78.3340000545804,9.00042645273249,134.670000601306));
#68633=CARTESIAN_POINT('Ctrl Pts',(78.3340000550508,9.00042828629872,134.670000473238));
#68634=CARTESIAN_POINT('Ctrl Pts',(78.3339655643716,8.86626226295517,134.679371509964));
#68635=CARTESIAN_POINT('Ctrl Pts',(78.3501373438938,8.73258081952499,134.689320485778));
#68636=CARTESIAN_POINT('Ctrl Pts',(78.3979867997652,8.53793954488717,134.70375480757));
#68637=CARTESIAN_POINT('Ctrl Pts',(78.4176301614395,8.47459188357303,134.708453036327));
#68638=CARTESIAN_POINT('Ctrl Pts',(78.4507577524891,8.38667242062074,134.714950171927));
#68639=CARTESIAN_POINT('Ctrl Pts',(78.4611626488001,8.36101484640449,134.716843815114));
#68640=CARTESIAN_POINT('Ctrl Pts',(78.4772814611657,8.32394789450348,134.719577511883));
#68641=CARTESIAN_POINT('Ctrl Pts',(78.4824941151857,8.31232703772465,134.720434277576));
#68642=CARTESIAN_POINT('Ctrl Pts',(78.4919466359459,8.29188503438602,134.721941261321));
#68643=CARTESIAN_POINT('Ctrl Pts',(78.4961318749502,8.28303945517025,134.722593313147));
#68644=CARTESIAN_POINT('Ctrl Pts',(78.5050794805669,8.26455164845712,134.723956291029));
#68645=CARTESIAN_POINT('Ctrl Pts',(78.5098577732733,8.25491759483874,134.724666628887));
#68646=CARTESIAN_POINT('Ctrl Pts',(78.5227541482814,8.22953614636296,134.726538763998));
#68647=CARTESIAN_POINT('Ctrl Pts',(78.531030845559,8.21387054585789,134.727694978796));
#68648=CARTESIAN_POINT('Ctrl Pts',(78.5717445858448,8.13969933644567,134.733177471293));
#68649=CARTESIAN_POINT('Ctrl Pts',(78.6074377376139,8.08304708015765,134.737386447034));
#68650=CARTESIAN_POINT('Ctrl Pts',(78.7306339541458,7.91136886111357,134.750467103729));
#68651=CARTESIAN_POINT('Ctrl Pts',(78.8297057385005,7.80550903048326,134.758995701262));
#68652=CARTESIAN_POINT('Ctrl Pts',(78.9526798341496,7.70427666301174,134.769227894363));
#68653=CARTESIAN_POINT('Ctrl Pts',(78.9643223946167,7.69495197031709,134.770194072015));
#68654=CARTESIAN_POINT('Ctrl Pts',(78.9827584636376,7.68058832899099,134.771722870912));
#68655=CARTESIAN_POINT('Ctrl Pts',(78.9894680948451,7.67544242763187,134.772279029694));
#68656=CARTESIAN_POINT('Ctrl Pts',(79.0019141360088,7.66604663756914,134.773310855872));
#68657=CARTESIAN_POINT('Ctrl Pts',(79.0076392904091,7.66178208707062,134.773785562536));
#68658=CARTESIAN_POINT('Ctrl Pts',(79.0134457612967,7.65751471567714,134.774267280301));
#68659=CARTESIAN_POINT('Ctrl Pts',(79.0134999791126,7.6574748742329,134.774271778355));
#68660=CARTESIAN_POINT('Ctrl Pts',(79.0136085086173,7.65739513248702,134.774280782299));
#68661=CARTESIAN_POINT('Ctrl Pts',(79.0136628203814,7.65735523214674,134.774285288196));
#68662=CARTESIAN_POINT('Ctrl Pts',(79.0137715540034,7.65727536074349,134.774294309169));
#68663=CARTESIAN_POINT('Ctrl Pts',(79.0138259757974,7.65723538974719,134.774298824242));
#68664=CARTESIAN_POINT('Ctrl Pts',(79.0139349458008,7.65715536510478,134.774307864923));
#68665=CARTESIAN_POINT('Ctrl Pts',(79.0139894941712,7.65711531136321,134.774312390546));
#68666=CARTESIAN_POINT('Ctrl Pts',(79.0140987341401,7.65703510895518,134.774321453723));
#68667=CARTESIAN_POINT('Ctrl Pts',(79.0141534256526,7.65699496037784,134.77432599127));
#68668=CARTESIAN_POINT('Ctrl Pts',(79.0142372940766,7.65693340115975,134.774332949553));
#68669=CARTESIAN_POINT('Ctrl Pts',(79.0142664693503,7.65691198804299,134.774335370135));
#68670=CARTESIAN_POINT('Ctrl Pts',(79.0143255417741,7.65686863495178,134.774340271206));
#68671=CARTESIAN_POINT('Ctrl Pts',(79.014355439047,7.65684669496034,134.774342751704));
#68672=CARTESIAN_POINT('Ctrl Pts',(79.0144159916862,7.65680226176421,134.774347775614));
#68673=CARTESIAN_POINT('Ctrl Pts',(79.0144466469614,7.65677976870502,134.774350319018));
#68674=CARTESIAN_POINT('Ctrl Pts',(79.01450875407,7.65673420138942,134.77435547193));
#68675=CARTESIAN_POINT('Ctrl Pts',(79.0145402059464,7.65671112718616,134.774358081442));
#68676=CARTESIAN_POINT('Ctrl Pts',(79.014603947371,7.65666436767768,134.774363369984));
#68677=CARTESIAN_POINT('Ctrl Pts',(79.0146362368861,7.65664068248822,134.774366049012));
#68678=CARTESIAN_POINT('Ctrl Pts',(79.014701697453,7.65659266910958,134.774371480224));
#68679=CARTESIAN_POINT('Ctrl Pts',(79.0147348686655,7.65656834090136,134.774374232423));
#68680=CARTESIAN_POINT('Ctrl Pts',(79.0148021397554,7.65651900722135,134.774379813891));
#68681=CARTESIAN_POINT('Ctrl Pts',(79.014836239638,7.65649400185285,134.774382643161));
#68682=CARTESIAN_POINT('Ctrl Pts',(79.0149054185573,7.65644327715413,134.774388382961));
#68683=CARTESIAN_POINT('Ctrl Pts',(79.0149404976944,7.65641755786645,134.7743912935));
#68684=CARTESIAN_POINT('Ctrl Pts',(79.0192893423312,7.65322933803952,134.774752121319));
#68685=CARTESIAN_POINT('Ctrl Pts',(79.0236181254127,7.6500877643364,134.775111452968));
#68686=CARTESIAN_POINT('Ctrl Pts',(79.0330801844961,7.64329008805398,134.775897371685));
#68687=CARTESIAN_POINT('Ctrl Pts',(79.0382190092707,7.63964231271351,134.77632447413));
#68688=CARTESIAN_POINT('Ctrl Pts',(79.0524019646582,7.62969512779834,134.77750372754));
#68689=CARTESIAN_POINT('Ctrl Pts',(79.0614879140347,7.62345631103728,134.778259703456));
#68690=CARTESIAN_POINT('Ctrl Pts',(79.1133508313759,7.58859706382759,134.782574758738));
#68691=CARTESIAN_POINT('Ctrl Pts',(79.1573702490982,7.56188351848903,134.786236178465));
#68692=CARTESIAN_POINT('Ctrl Pts',(79.2868521186522,7.49129355265541,134.79686349874));
#68693=CARTESIAN_POINT('Ctrl Pts',(79.374969956264,7.45270766917598,134.803915883256));
#68694=CARTESIAN_POINT('Ctrl Pts',(79.5157219516368,7.4050722027638,134.81460187366));
#68695=CARTESIAN_POINT('Ctrl Pts',(79.5662936761663,7.39058407485569,134.81833561118));
#68696=CARTESIAN_POINT('Ctrl Pts',(79.6406651938631,7.37303889138632,134.823661050877));
#68697=CARTESIAN_POINT('Ctrl Pts',(79.6639759107463,7.36806499446573,134.825307363598));
#68698=CARTESIAN_POINT('Ctrl Pts',(79.7064425619118,7.35995231119174,134.828265793654));
#68699=CARTESIAN_POINT('Ctrl Pts',(79.7255615497273,7.35664490044277,134.829582901039));
#68700=CARTESIAN_POINT('Ctrl Pts',(79.7557168877124,7.35196927526038,134.831637901646));
#68701=CARTESIAN_POINT('Ctrl Pts',(79.7667160914956,7.35037636503631,134.832382812402));
#68702=CARTESIAN_POINT('Ctrl Pts',(79.787364243718,7.34759674316542,134.833772753076));
#68703=CARTESIAN_POINT('Ctrl Pts',(79.7970091768313,7.34638419800633,134.834418569438));
#68704=CARTESIAN_POINT('Ctrl Pts',(79.8187058503884,7.34384921928543,134.83586391477));
#68705=CARTESIAN_POINT('Ctrl Pts',(79.8307626083924,7.34257377376927,134.836661938393));
#68706=CARTESIAN_POINT('Ctrl Pts',(79.8663104509477,7.33920522971412,134.839000481215));
#68707=CARTESIAN_POINT('Ctrl Pts',(79.8898338919031,7.33747911813372,134.840529557292));
#68708=CARTESIAN_POINT('Ctrl Pts',(80.0169191278567,7.33086319106281,134.848704969525));
#68709=CARTESIAN_POINT('Ctrl Pts',(80.120732423455,7.33514835686051,134.855059492965));
#68710=CARTESIAN_POINT('Ctrl Pts',(80.3013471321691,7.35959770217609,134.866190415333));
#68711=CARTESIAN_POINT('Ctrl Pts',(80.3783618299464,7.37563230934988,134.870968067021));
#68712=CARTESIAN_POINT('Ctrl Pts',(80.4776725496375,7.40375667796768,134.877477389854));
#68713=CARTESIAN_POINT('Ctrl Pts',(80.5012401771179,7.41099969654625,134.879049101299));
#68714=CARTESIAN_POINT('Ctrl Pts',(80.5409205188762,7.42416519602091,134.88175494137));
#68715=CARTESIAN_POINT('Ctrl Pts',(80.5571187043268,7.42981879060742,134.882876657556));
#68716=CARTESIAN_POINT('Ctrl Pts',(80.5802011360544,7.43827728810236,134.884503721651));
#68717=CARTESIAN_POINT('Ctrl Pts',(80.587159019503,7.4408799059292,134.884997944199));
#68718=CARTESIAN_POINT('Ctrl Pts',(80.5992436735831,7.44549257245466,134.885863286103));
#68719=CARTESIAN_POINT('Ctrl Pts',(80.604378255201,7.44748164382845,134.88623316888));
#68720=CARTESIAN_POINT('Ctrl Pts',(80.6153667197088,7.4518012090293,134.887029625428));
#68721=CARTESIAN_POINT('Ctrl Pts',(80.6212171751045,7.45413942603265,134.887456624532));
#68722=CARTESIAN_POINT('Ctrl Pts',(80.6372592945784,7.46065665748178,134.888635321439));
#68723=CARTESIAN_POINT('Ctrl Pts',(80.6474227784382,7.46490356510367,134.889390838519));
#68724=CARTESIAN_POINT('Ctrl Pts',(80.7053387281912,7.48978172973047,134.893743378003));
#68725=CARTESIAN_POINT('Ctrl Pts',(80.7521418935547,7.51253793236193,134.897445033514));
#68726=CARTESIAN_POINT('Ctrl Pts',(80.8876317634994,7.58644525919441,134.908569778452));
#68727=CARTESIAN_POINT('Ctrl Pts',(80.9727652378245,7.64362368216281,134.916091786867));
#68728=CARTESIAN_POINT('Ctrl Pts',(81.1086268706204,7.75428135027503,134.928652989111));
#68729=CARTESIAN_POINT('Ctrl Pts',(81.1620649880607,7.80397487713806,134.933774979999));
#68730=CARTESIAN_POINT('Ctrl Pts',(81.2241714733357,7.86983598770199,134.939952857166));
#68731=CARTESIAN_POINT('Ctrl Pts',(81.2360566858485,7.8828471896814,134.941146718081));
#68732=CARTESIAN_POINT('Ctrl Pts',(81.2548457660713,7.90408335100636,134.943053756302));
#68733=CARTESIAN_POINT('Ctrl Pts',(81.2618801817239,7.91219045119758,134.94377235405));
#68734=CARTESIAN_POINT('Ctrl Pts',(81.2751807585309,7.92782189281806,134.945140271076));
#68735=CARTESIAN_POINT('Ctrl Pts',(81.2814598683829,7.93533457219946,134.945790105141));
#68736=CARTESIAN_POINT('Ctrl Pts',(81.2956442187441,7.9526128219236,134.947267694861));
#68737=CARTESIAN_POINT('Ctrl Pts',(81.3035060145859,7.96241341244177,134.948093679199));
#68738=CARTESIAN_POINT('Ctrl Pts',(81.3242023253096,7.98882017335116,134.950287944473));
#68739=CARTESIAN_POINT('Ctrl Pts',(81.3368354399322,8.00558182350233,134.951648345913));
#68740=CARTESIAN_POINT('Ctrl Pts',(81.4202054119589,8.12065857266002,134.960784214748));
#68741=CARTESIAN_POINT('Ctrl Pts',(81.4803566264465,8.22619584699319,134.968139287296));
#68742=CARTESIAN_POINT('Ctrl Pts',(81.5548111698802,8.39793574788531,134.979577599606));
#68743=CARTESIAN_POINT('Ctrl Pts',(81.5774554675545,8.46004432938995,134.983625386728));
#68744=CARTESIAN_POINT('Ctrl Pts',(81.602764709373,8.5448037509964,134.989224360882));
#68745=CARTESIAN_POINT('Ctrl Pts',(81.6087430956234,8.56640584542373,134.990657848497));
#68746=CARTESIAN_POINT('Ctrl Pts',(81.6182342449221,8.60360463697743,134.993147721655));
#68747=CARTESIAN_POINT('Ctrl Pts',(81.6219617264688,8.61914377097646,134.994194147028));
#68748=CARTESIAN_POINT('Ctrl Pts',(81.6270484136842,8.64177992750096,134.995730857786));
#68749=CARTESIAN_POINT('Ctrl Pts',(81.6285859996696,8.64883650862056,134.996211645075));
#68750=CARTESIAN_POINT('Ctrl Pts',(81.6312000630023,8.66122000055998,134.997058764868));
#68751=CARTESIAN_POINT('Ctrl Pts',(81.6322964316461,8.66654251908276,134.997423970398));
#68752=CARTESIAN_POINT('Ctrl Pts',(81.6346286589376,8.67815190451848,134.998223055866));
#68753=CARTESIAN_POINT('Ctrl Pts',(81.6358542801932,8.6844404656776,134.998657469107));
#68754=CARTESIAN_POINT('Ctrl Pts',(81.6391763465296,8.70202532500559,134.99987630194));
#68755=CARTESIAN_POINT('Ctrl Pts',(81.6411922067568,8.71333621756289,135.000664959297));
#68756=CARTESIAN_POINT('Ctrl Pts',(81.6540547720352,8.7900954033791,135.006044639556));
#68757=CARTESIAN_POINT('Ctrl Pts',(81.6610996002016,8.85611365607817,135.010805013117));
#68758=CARTESIAN_POINT('Ctrl Pts',(81.665209496978,8.94421690254066,135.017199631535));
#68759=CARTESIAN_POINT('Ctrl Pts',(81.6657983350307,8.96608376369899,135.018790384712));
#68760=CARTESIAN_POINT('Ctrl Pts',(81.6664768275813,9.05993177730709,135.025620917735));
#68761=CARTESIAN_POINT('Ctrl Pts',(81.662332170408,9.13187027488392,135.0308608838));
#68762=CARTESIAN_POINT('Ctrl Pts',(81.6453814388771,9.2697271088658,135.040783878553));
#68763=CARTESIAN_POINT('Ctrl Pts',(81.6332219646552,9.33559034233666,135.045471709918));
#68764=CARTESIAN_POINT('Ctrl Pts',(81.6129873141637,9.41728292185814,135.051211768597));
#68765=CARTESIAN_POINT('Ctrl Pts',(81.608583542799,9.43394946380289,135.05237908819));
#68766=CARTESIAN_POINT('Ctrl Pts',(81.6010414288129,9.46079906787661,135.054254202118));
#68767=CARTESIAN_POINT('Ctrl Pts',(81.5980627804573,9.47102526106106,135.054967094336));
#68768=CARTESIAN_POINT('Ctrl Pts',(81.5921510532064,9.4906193687477,135.056330834542));
#68769=CARTESIAN_POINT('Ctrl Pts',(81.5892328582637,9.49999127038626,135.056982134395));
#68770=CARTESIAN_POINT('Ctrl Pts',(81.5823384505464,9.52146257453709,135.058472316146));
#68771=CARTESIAN_POINT('Ctrl Pts',(81.5783059521219,9.53354336766289,135.059309318231));
#68772=CARTESIAN_POINT('Ctrl Pts',(81.5648133893197,9.57247301044821,135.062002881108));
#68773=CARTESIAN_POINT('Ctrl Pts',(81.5548033520058,9.59912684920207,135.063841354955));
#68774=CARTESIAN_POINT('Ctrl Pts',(81.4950347547579,9.74666919824612,135.074012539877));
#68775=CARTESIAN_POINT('Ctrl Pts',(81.4318677430366,9.86162693812818,135.081871730983));
#68776=CARTESIAN_POINT('Ctrl Pts',(81.3144981211259,10.0260261801304,135.094265552378));
#68777=CARTESIAN_POINT('Ctrl Pts',(81.2694138767051,10.0813052834377,135.098683841434));
#68778=CARTESIAN_POINT('Ctrl Pts',(81.2102100137371,10.1450747715085,135.104329553291));
#68779=CARTESIAN_POINT('Ctrl Pts',(81.1993213311166,10.156474301575,135.105362159929));
#68780=CARTESIAN_POINT('Ctrl Pts',(81.1832381854639,10.1728405671852,135.106882232634));
#68781=CARTESIAN_POINT('Ctrl Pts',(81.1781703771917,10.177931304084,135.107360485816));
#68782=CARTESIAN_POINT('Ctrl Pts',(81.1692137682067,10.1868128141315,135.108204821734));
#68783=CARTESIAN_POINT('Ctrl Pts',(81.1653391169179,10.1906175846407,135.108569803132));
#68784=CARTESIAN_POINT('Ctrl Pts',(81.1568337888374,10.1988882221994,135.109370462327));
#68785=CARTESIAN_POINT('Ctrl Pts',(81.1521958984812,10.2033461648048,135.109806692327));
#68786=CARTESIAN_POINT('Ctrl Pts',(81.1391183099488,10.2157714354649,135.11103542964));
#68787=CARTESIAN_POINT('Ctrl Pts',(81.1306211943769,10.2236774098439,135.111832280922));
#68788=CARTESIAN_POINT('Ctrl Pts',(81.0651948577583,10.283288863595,135.117951756461));
#68789=CARTESIAN_POINT('Ctrl Pts',(81.0048352230073,10.331079969485,135.123501132967));
#68790=CARTESIAN_POINT('Ctrl Pts',(80.8942455523406,10.406821720891,135.133244006134));
#68791=CARTESIAN_POINT('Ctrl Pts',(80.8454599825917,10.4366698097108,135.137414680222));
#68792=CARTESIAN_POINT('Ctrl Pts',(80.7224007237856,10.5035170862845,135.147535074295));
#68793=CARTESIAN_POINT('Ctrl Pts',(80.6467054064323,10.5375962292472,135.153421747104));
#68794=CARTESIAN_POINT('Ctrl Pts',(80.5472951364979,10.5737046696924,135.160693101657));
#68795=CARTESIAN_POINT('Ctrl Pts',(80.5256541130962,10.5810648934162,135.162250076072));
#68796=CARTESIAN_POINT('Ctrl Pts',(80.492595949516,10.5915542938227,135.164590482353));
#68797=CARTESIAN_POINT('Ctrl Pts',(80.4812863703349,10.5950107466402,135.165384517732));
#68798=CARTESIAN_POINT('Ctrl Pts',(80.4615343328447,10.6008181768382,135.166760054414));
#68799=CARTESIAN_POINT('Ctrl Pts',(80.4531084734992,10.603223469129,135.167343302369));
#68800=CARTESIAN_POINT('Ctrl Pts',(80.4340667845741,10.60849710561,135.168653637365));
#68801=CARTESIAN_POINT('Ctrl Pts',(80.4234406749298,10.6113270669855,135.1693794589));
#68802=CARTESIAN_POINT('Ctrl Pts',(80.3945261603837,10.6187218356989,135.1713403868));
#68803=CARTESIAN_POINT('Ctrl Pts',(80.376186701251,10.6230819096126,135.172568903385));
#68804=CARTESIAN_POINT('Ctrl Pts',(80.257825845632,10.6491073300895,135.180407936744));
#68805=CARTESIAN_POINT('Ctrl Pts',(80.1560575540375,10.6618300337175,135.186720343809));
#68806=CARTESIAN_POINT('Ctrl Pts',(79.9711508904763,10.6677991590036,135.198030615194));
#68807=CARTESIAN_POINT('Ctrl Pts',(79.8884694665592,10.6643153573151,135.203037381399));
#68808=CARTESIAN_POINT('Ctrl Pts',(79.7785227195045,10.6514512508697,135.209983518382));
#68809=CARTESIAN_POINT('Ctrl Pts',(79.7507402310437,10.647486815931,135.211764281708));
#68810=CARTESIAN_POINT('Ctrl Pts',(79.704468073352,10.6396868145213,135.214792621852));
#68811=CARTESIAN_POINT('Ctrl Pts',(79.6859189679776,10.6362350079938,135.216023557846));
#68812=CARTESIAN_POINT('Ctrl Pts',(79.6598766766881,10.6309296734533,135.217780840331));
#68813=CARTESIAN_POINT('Ctrl Pts',(79.652330865977,10.6293377925579,135.218293479883));
#68814=CARTESIAN_POINT('Ctrl Pts',(79.6393774296913,10.6265110289581,135.219179887729));
#68815=CARTESIAN_POINT('Ctrl Pts',(79.6339644523312,10.625301431283,135.21955223185));
#68816=CARTESIAN_POINT('Ctrl Pts',(79.6225562905157,10.6226922518594,135.220341200459));
#68817=CARTESIAN_POINT('Ctrl Pts',(79.616562882159,10.6212864866049,135.220758140634));
#68818=CARTESIAN_POINT('Ctrl Pts',(79.600227109927,10.6173592548224,135.221900991594));
#68819=CARTESIAN_POINT('Ctrl Pts',(79.5899011146247,10.6147718762332,135.222630451623));
#68820=CARTESIAN_POINT('Ctrl Pts',(79.5378582464754,10.6012001597168,135.226340226601));
#68821=CARTESIAN_POINT('Ctrl Pts',(79.4965578283731,10.5886982831219,135.22939244255));
#68822=CARTESIAN_POINT('Ctrl Pts',(79.3705372398145,10.5451438203399,135.238953074695));
#68823=CARTESIAN_POINT('Ctrl Pts',(79.2878164753645,10.5088032830177,135.245574547554));
#68824=CARTESIAN_POINT('Ctrl Pts',(79.126556758386,10.4217290802034,135.258830502727));
#68825=CARTESIAN_POINT('Ctrl Pts',(79.0485067711148,10.3707233603725,135.26543372522));
#68826=CARTESIAN_POINT('Ctrl Pts',(78.9605025005847,10.3020539474665,135.273062215689));
#68827=CARTESIAN_POINT('Ctrl Pts',(78.9460807894463,10.2904084156567,135.27431932258));
#68828=CARTESIAN_POINT('Ctrl Pts',(78.9234687965993,10.2715172078411,135.276302367087));
#68829=CARTESIAN_POINT('Ctrl Pts',(78.9151506769188,10.264427695755,135.277034524169));
#68830=CARTESIAN_POINT('Ctrl Pts',(78.8995470943713,10.2508614659861,135.278413302258));
#68831=CARTESIAN_POINT('Ctrl Pts',(78.8922475758704,10.244401694923,135.279060581157));
#68832=CARTESIAN_POINT('Ctrl Pts',(78.8757834475827,10.2295719472118,135.280526008271));
#68833=CARTESIAN_POINT('Ctrl Pts',(78.8666547623747,10.2211628131991,135.281342467502));
#68834=CARTESIAN_POINT('Ctrl Pts',(78.8430725753683,10.1989472090883,135.283462807994));
#68835=CARTESIAN_POINT('Ctrl Pts',(78.8287717965673,10.1849810236034,135.284759832465));
#68836=CARTESIAN_POINT('Ctrl Pts',(78.7067132658651,10.061409291051,135.295942556402));
#68837=CARTESIAN_POINT('Ctrl Pts',(78.6143579187439,9.93764471136762,135.305096360121));
#68838=CARTESIAN_POINT('Ctrl Pts',(78.5113757384388,9.75043263522426,135.318278407621));
#68839=CARTESIAN_POINT('Ctrl Pts',(78.4853363743524,9.69637913181366,135.322029156211));
#68840=CARTESIAN_POINT('Ctrl Pts',(78.4566660025697,9.62760516086039,135.326874455342));
#68841=CARTESIAN_POINT('Ctrl Pts',(78.4512393376177,9.61409155740559,135.327829956955));
#68842=CARTESIAN_POINT('Ctrl Pts',(78.4434820923841,9.59401720648724,135.329256871534));
#68843=CARTESIAN_POINT('Ctrl Pts',(78.4410142084785,9.58750977509323,135.329720586687));
#68844=CARTESIAN_POINT('Ctrl Pts',(78.4379080630576,9.57916195781168,135.330317158519));
#68845=CARTESIAN_POINT('Ctrl Pts',(78.4372321137202,9.57733554043893,135.330447786867));
#68846=CARTESIAN_POINT('Ctrl Pts',(78.4365593737638,9.57550795670805,135.330578607084));
#68847=CARTESIAN_POINT('Origin',(80.,9.,134.));
#68848=CARTESIAN_POINT('',(78.4365593745323,9.57550795879571,136.032852165095));
#68849=CARTESIAN_POINT('',(78.4365593737294,9.5755079566144,135.837694135948));
#68850=CARTESIAN_POINT('',(78.4365593737638,9.57550795670799,134.));
#68851=CARTESIAN_POINT('Ctrl Pts',(78.4365593737294,9.5755079566144,135.837694135948));
#68852=CARTESIAN_POINT('Ctrl Pts',(78.4371889020499,9.57721815043606,135.837570608446));
#68853=CARTESIAN_POINT('Ctrl Pts',(78.4378212447466,9.57892733385798,135.837447172522));
#68854=CARTESIAN_POINT('Ctrl Pts',(78.4430078465044,9.59287602418787,135.836439956826));
#68855=CARTESIAN_POINT('Ctrl Pts',(78.4477031699583,9.60506290119926,135.835560896534));
#68856=CARTESIAN_POINT('Ctrl Pts',(78.456184053024,9.62632659361785,135.834028387693));
#68857=CARTESIAN_POINT('Ctrl Pts',(78.4599075277412,9.63542730821962,135.833372898105));
#68858=CARTESIAN_POINT('Ctrl Pts',(78.4678162009344,9.65427929313463,135.832015684355));
#68859=CARTESIAN_POINT('Ctrl Pts',(78.4720144386067,9.66402463848485,135.831314436495));
#68860=CARTESIAN_POINT('Ctrl Pts',(78.4831971227381,9.6893151977885,135.82949506286));
#68861=CARTESIAN_POINT('Ctrl Pts',(78.4903275987439,9.70479478308494,135.828381950611));
#68862=CARTESIAN_POINT('Ctrl Pts',(78.5220251521166,9.77091790502434,135.823625425996));
#68863=CARTESIAN_POINT('Ctrl Pts',(78.5489137951427,9.82041080652283,135.820062437349));
#68864=CARTESIAN_POINT('Ctrl Pts',(78.6423744983455,9.97341519189136,135.808892894365));
#68865=CARTESIAN_POINT('Ctrl Pts',(78.717911922364,10.0709491270467,135.801557481335));
#68866=CARTESIAN_POINT('Ctrl Pts',(78.8269160378371,10.18345392699,135.791796678314));
#68867=CARTESIAN_POINT('Ctrl Pts',(78.8510660309233,10.2069132665183,135.789674860879));
#68868=CARTESIAN_POINT('Ctrl Pts',(78.8867641540232,10.2395476136788,135.786566292188));
#68869=CARTESIAN_POINT('Ctrl Pts',(78.8977504725858,10.2493271317726,135.785613198198));
#68870=CARTESIAN_POINT('Ctrl Pts',(78.9151944838268,10.2644457919935,135.78410274589));
#68871=CARTESIAN_POINT('Ctrl Pts',(78.9215656914436,10.2698840908047,135.783551656952));
#68872=CARTESIAN_POINT('Ctrl Pts',(78.9333776871248,10.2798135064164,135.78253043967));
#68873=CARTESIAN_POINT('Ctrl Pts',(78.9388065511281,10.2843185855315,135.782061266588));
#68874=CARTESIAN_POINT('Ctrl Pts',(78.944311691745,10.2888282273662,135.781585494046));
#68875=CARTESIAN_POINT('Ctrl Pts',(78.944359643814,10.2888675037541,135.781581349868));
#68876=CARTESIAN_POINT('Ctrl Pts',(78.9444557602574,10.2889462214621,135.781573043163));
#68877=CARTESIAN_POINT('Ctrl Pts',(78.9445039246395,10.2889856627496,135.781568880635));
#68878=CARTESIAN_POINT('Ctrl Pts',(78.9446004792839,10.2890647212547,135.781560536056));
#68879=CARTESIAN_POINT('Ctrl Pts',(78.9446488698297,10.2891043386629,135.781556353981));
#68880=CARTESIAN_POINT('Ctrl Pts',(78.9447458910764,10.2891837609702,135.781547969073));
#68881=CARTESIAN_POINT('Ctrl Pts',(78.9447945217013,10.2892235657627,135.781543766247));
#68882=CARTESIAN_POINT('Ctrl Pts',(78.9448920376513,10.2893033746091,135.781535338581));
#68883=CARTESIAN_POINT('Ctrl Pts',(78.9449409229435,10.2893433785888,135.781531113744));
#68884=CARTESIAN_POINT('Ctrl Pts',(78.9450389629839,10.289423597741,135.78152264078));
#68885=CARTESIAN_POINT('Ctrl Pts',(78.9450881177422,10.2894638128714,135.781518392651));
#68886=CARTESIAN_POINT('Ctrl Pts',(78.9492752585669,10.2928890513312,135.781156525011));
#68887=CARTESIAN_POINT('Ctrl Pts',(78.9534293415932,10.2962540019012,135.780797496679));
#68888=CARTESIAN_POINT('Ctrl Pts',(78.9624494181203,10.3034889497047,135.780017748647));
#68889=CARTESIAN_POINT('Ctrl Pts',(78.9673208142496,10.3073516543394,135.779596563731));
#68890=CARTESIAN_POINT('Ctrl Pts',(78.9808088158269,10.3179243531187,135.7784304457));
#68891=CARTESIAN_POINT('Ctrl Pts',(78.9894697747196,10.3245768827743,135.777681728199));
#68892=CARTESIAN_POINT('Ctrl Pts',(79.0359779336887,10.3595784389727,135.773664349366));
#68893=CARTESIAN_POINT('Ctrl Pts',(79.0749506047345,10.3863891275557,135.770309329564));
#68894=CARTESIAN_POINT('Ctrl Pts',(79.1888177813669,10.4577823086992,135.7606469809));
#68895=CARTESIAN_POINT('Ctrl Pts',(79.2661448503083,10.4981997819734,135.754255358622));
#68896=CARTESIAN_POINT('Ctrl Pts',(79.4233562643577,10.5652668334709,135.74189897358));
#68897=CARTESIAN_POINT('Ctrl Pts',(79.5028145895219,10.5922903771581,135.735944638444));
#68898=CARTESIAN_POINT('Ctrl Pts',(79.6062258886722,10.6189582228513,135.728601378606));
#68899=CARTESIAN_POINT('Ctrl Pts',(79.6285887039478,10.6242344407781,135.727036168204));
#68900=CARTESIAN_POINT('Ctrl Pts',(79.6626425303537,10.6315288478536,135.724685904037));
#68901=CARTESIAN_POINT('Ctrl Pts',(79.6742569685117,10.6338873687392,135.723890113654));
#68902=CARTESIAN_POINT('Ctrl Pts',(79.6945054233707,10.6377746854809,135.72251250527));
#68903=CARTESIAN_POINT('Ctrl Pts',(79.7031280474857,10.6393596022848,135.721928925997));
#68904=CARTESIAN_POINT('Ctrl Pts',(79.7225806466558,10.642776654463,135.720619073461));
#68905=CARTESIAN_POINT('Ctrl Pts',(79.7334171079582,10.6445699150402,135.719894055633));
#68906=CARTESIAN_POINT('Ctrl Pts',(79.7628286326272,10.6491386990061,135.717938345507));
#68907=CARTESIAN_POINT('Ctrl Pts',(79.781434530142,10.6517075672982,135.716714179264));
#68908=CARTESIAN_POINT('Ctrl Pts',(79.8914918128947,10.6650105351748,135.709542605456));
#68909=CARTESIAN_POINT('Ctrl Pts',(79.9836672967324,10.6684635269506,135.70383092974));
#68910=CARTESIAN_POINT('Ctrl Pts',(80.1702715709164,10.6599795974664,135.692386144377));
#68911=CARTESIAN_POINT('Ctrl Pts',(80.2643313114565,10.6476198988377,135.686675985887));
#68912=CARTESIAN_POINT('Ctrl Pts',(80.3832678283266,10.621540816857,135.679024852909));
#68913=CARTESIAN_POINT('Ctrl Pts',(80.4095641042411,10.6150993561976,135.677304690945));
#68914=CARTESIAN_POINT('Ctrl Pts',(80.4534309272396,10.6032137196487,135.674369289443));
#68915=CARTESIAN_POINT('Ctrl Pts',(80.4710899431191,10.5981138989459,135.673169399217));
#68916=CARTESIAN_POINT('Ctrl Pts',(80.495958918979,10.5904839007493,135.671448951928));
#68917=CARTESIAN_POINT('Ctrl Pts',(80.5032421119597,10.5881944650987,135.670941340366));
#68918=CARTESIAN_POINT('Ctrl Pts',(80.5157789344344,10.5841586850526,135.670060658604));
#68919=CARTESIAN_POINT('Ctrl Pts',(80.5210400278227,10.5824360768028,135.669688960555));
#68920=CARTESIAN_POINT('Ctrl Pts',(80.5321708221944,10.5787300593399,135.668897925723));
#68921=CARTESIAN_POINT('Ctrl Pts',(80.5380379820997,10.5767401532695,135.668478244052));
#68922=CARTESIAN_POINT('Ctrl Pts',(80.5541224476665,10.5711847185626,135.667320493298));
#68923=CARTESIAN_POINT('Ctrl Pts',(80.5643161112282,10.5675523653185,135.666578725591));
#68924=CARTESIAN_POINT('Ctrl Pts',(80.6173642992726,10.548064989706,135.662679060297));
#68925=CARTESIAN_POINT('Ctrl Pts',(80.6595849349259,10.5305524484115,135.659440510941));
#68926=CARTESIAN_POINT('Ctrl Pts',(80.7954511837306,10.4675310484174,135.648683421257));
#68927=CARTESIAN_POINT('Ctrl Pts',(80.8855625271718,10.4149806455776,135.641024428585));
#68928=CARTESIAN_POINT('Ctrl Pts',(81.0332169965827,10.3092099344154,135.627972585677));
#68929=CARTESIAN_POINT('Ctrl Pts',(81.0930285014872,10.2597062551331,135.622511354908));
#68930=CARTESIAN_POINT('Ctrl Pts',(81.1621294348974,10.1938722759951,135.615995350205));
#68931=CARTESIAN_POINT('Ctrl Pts',(81.1748786032305,10.1813281279153,135.614783283866));
#68932=CARTESIAN_POINT('Ctrl Pts',(81.1949931638495,10.1608892250598,135.612854227821));
#68933=CARTESIAN_POINT('Ctrl Pts',(81.2024878104736,10.153124247273,135.612131593229));
#68934=CARTESIAN_POINT('Ctrl Pts',(81.2166293532872,10.13818480507,135.610760346202));
#68935=CARTESIAN_POINT('Ctrl Pts',(81.2232895281687,10.1310235943625,135.610111177375));
#68936=CARTESIAN_POINT('Ctrl Pts',(81.2382912286932,10.114605796552,135.608640963039));
#68937=CARTESIAN_POINT('Ctrl Pts',(81.246592802831,10.1053133703756,135.607821622425));
#68938=CARTESIAN_POINT('Ctrl Pts',(81.2724752762651,10.0756790851664,135.605247713919));
#68939=CARTESIAN_POINT('Ctrl Pts',(81.2896689976927,10.0550037108813,135.603508996473));
#68940=CARTESIAN_POINT('Ctrl Pts',(81.388552741998,9.93006435616154,135.593309988638));
#68941=CARTESIAN_POINT('Ctrl Pts',(81.4580714713327,9.8167794409514,135.585345574692));
#68942=CARTESIAN_POINT('Ctrl Pts',(81.5434655964223,9.63121112141915,135.57281469744));
#68943=CARTESIAN_POINT('Ctrl Pts',(81.5692342064941,9.56410563174356,135.568364281595));
#68944=CARTESIAN_POINT('Ctrl Pts',(81.595296918562,9.48045189419966,135.562679933504));
#68945=CARTESIAN_POINT('Ctrl Pts',(81.5997871089906,9.46528211039712,135.561643733308));
#68946=CARTESIAN_POINT('Ctrl Pts',(81.6060039428389,9.44312424672617,135.560119255425));
#68947=CARTESIAN_POINT('Ctrl Pts',(81.607902550172,9.43618476227067,135.559640263588));
#68948=CARTESIAN_POINT('Ctrl Pts',(81.6111558893842,9.42398374722654,135.558795028424));
#68949=CARTESIAN_POINT('Ctrl Pts',(81.6125299211568,9.41872756049863,135.558429893178));
#68950=CARTESIAN_POINT('Ctrl Pts',(81.6154737145086,9.4072370390653,135.557629381805));
#68951=CARTESIAN_POINT('Ctrl Pts',(81.6170330850204,9.40100040737403,135.557193457639));
#68952=CARTESIAN_POINT('Ctrl Pts',(81.6213006324686,9.38350280744024,135.555966702875));
#68953=CARTESIAN_POINT('Ctrl Pts',(81.6239274687256,9.37222265080472,135.555171551032));
#68954=CARTESIAN_POINT('Ctrl Pts',(81.6418716392339,9.29135891068976,135.54944506218));
#68955=CARTESIAN_POINT('Ctrl Pts',(81.6528271685414,9.22089036318195,135.544318813724));
#68956=CARTESIAN_POINT('Ctrl Pts',(81.6605271818987,9.13568532352874,135.538107697812));
#68957=CARTESIAN_POINT('Ctrl Pts',(81.6616320165991,9.1214086708507,135.537066427058));
#68958=CARTESIAN_POINT('Ctrl Pts',(81.6667939648985,9.04129254314559,135.531224458975));
#68959=CARTESIAN_POINT('Ctrl Pts',(81.6671221653112,8.97526858400889,135.52641825763));
#68960=CARTESIAN_POINT('Ctrl Pts',(81.6594838417457,8.83502385270356,135.516341107659));
#68961=CARTESIAN_POINT('Ctrl Pts',(81.6504498133135,8.76099797400832,135.511102797069));
#68962=CARTESIAN_POINT('Ctrl Pts',(81.6331693527157,8.67041276363314,135.504808441865));
#68963=CARTESIAN_POINT('Ctrl Pts',(81.6295720065072,8.65306340820967,135.503607945659));
#68964=CARTESIAN_POINT('Ctrl Pts',(81.6233470671427,8.62527879573648,135.50169280095));
#68965=CARTESIAN_POINT('Ctrl Pts',(81.62089403588,8.61480626282599,135.500972651338));
#68966=CARTESIAN_POINT('Ctrl Pts',(81.6160151736116,8.59484969448182,135.499603326994));
#68967=CARTESIAN_POINT('Ctrl Pts',(81.6136068461751,8.58536188747445,135.498953622558));
#68968=CARTESIAN_POINT('Ctrl Pts',(81.607925652204,8.56377979931247,135.49747842109));
#68969=CARTESIAN_POINT('Ctrl Pts',(81.6045996705743,8.55170001343006,135.496654672192));
#68970=CARTESIAN_POINT('Ctrl Pts',(81.5953745508907,8.51961363783677,135.494470982989));
#68971=CARTESIAN_POINT('Ctrl Pts',(81.589235335494,8.49967797878135,135.493118796825));
#68972=CARTESIAN_POINT('Ctrl Pts',(81.5442627613074,8.36283131153741,135.483856233414));
#68973=CARTESIAN_POINT('Ctrl Pts',(81.4929411815564,8.25042551509475,135.476383324012));
#68974=CARTESIAN_POINT('Ctrl Pts',(81.3823894100486,8.06563168265518,135.463221266979));
#68975=CARTESIAN_POINT('Ctrl Pts',(81.3286182436084,7.99063711854755,135.457567557998));
#68976=CARTESIAN_POINT('Ctrl Pts',(81.2608470093163,7.91097446152881,135.450737524056));
#68977=CARTESIAN_POINT('Ctrl Pts',(81.2526526459669,7.90155877259471,135.449915906257));
#68978=CARTESIAN_POINT('Ctrl Pts',(81.2399998363058,7.88734584060681,135.448651989517));
#68979=CARTESIAN_POINT('Ctrl Pts',(81.2356174078701,7.882481100754,135.448215062634));
#68980=CARTESIAN_POINT('Ctrl Pts',(81.2275203207019,7.87359873861287,135.44740904312));
#68981=CARTESIAN_POINT('Ctrl Pts',(81.2238144068862,7.86957342830091,135.447040593474));
#68982=CARTESIAN_POINT('Ctrl Pts',(81.2152813085664,7.86039604004827,135.446193269992));
#68983=CARTESIAN_POINT('Ctrl Pts',(81.2104411737599,7.85525635848035,135.445713440452));
#68984=CARTESIAN_POINT('Ctrl Pts',(81.195154867592,7.83922935100644,135.444200921511));
#68985=CARTESIAN_POINT('Ctrl Pts',(81.1845937089885,7.82845343159333,135.443160131475));
#68986=CARTESIAN_POINT('Ctrl Pts',(81.1004040028163,7.74485403017175,135.434906390445));
#68987=CARTESIAN_POINT('Ctrl Pts',(81.0202827741972,7.67890198977009,135.427321282152));
#68988=CARTESIAN_POINT('Ctrl Pts',(80.8402202887424,7.55688726559962,135.411504619801));
#68989=CARTESIAN_POINT('Ctrl Pts',(80.7395468894221,7.50279461738319,135.403335481153));
#68990=CARTESIAN_POINT('Ctrl Pts',(80.6161604699399,7.45200790544327,135.394204948353));
#68991=CARTESIAN_POINT('Ctrl Pts',(80.5980709950718,7.44492945826397,135.392886308833));
#68992=CARTESIAN_POINT('Ctrl Pts',(80.5694364482698,7.43429830858088,135.390829345355));
#68993=CARTESIAN_POINT('Ctrl Pts',(80.5589730075605,7.43053230605684,135.390083984161));
#68994=CARTESIAN_POINT('Ctrl Pts',(80.5392916128432,7.4236703741662,135.388693437174));
#68995=CARTESIAN_POINT('Ctrl Pts',(80.5300827980014,7.42054985293012,135.388047462111));
#68996=CARTESIAN_POINT('Ctrl Pts',(80.5093328045889,7.41372037989788,135.386602057814));
#68997=CARTESIAN_POINT('Ctrl Pts',(80.4977773224061,7.41005638802945,135.385804131618));
#68998=CARTESIAN_POINT('Ctrl Pts',(80.463642341964,7.39964155929411,135.383466789958));
#68999=CARTESIAN_POINT('Ctrl Pts',(80.4409578348283,7.39324313065237,135.381938796362));
#69000=CARTESIAN_POINT('Ctrl Pts',(80.3161449279824,7.36088081709177,135.3736550935));
#69001=CARTESIAN_POINT('Ctrl Pts',(80.2118627864795,7.34416881613139,135.367202248805));
#69002=CARTESIAN_POINT('Ctrl Pts',(80.0295733591696,7.33247099956887,135.356047607247));
#69003=CARTESIAN_POINT('Ctrl Pts',(79.9522106782296,7.33289410774803,135.351345341874));
#69004=CARTESIAN_POINT('Ctrl Pts',(79.8507929580685,7.34051498721274,135.344929256771));
#69005=CARTESIAN_POINT('Ctrl Pts',(79.8264674895346,7.34288214316547,135.34337078917));
#69006=CARTESIAN_POINT('Ctrl Pts',(79.7852787299223,7.34780711061536,135.340685489222));
#69007=CARTESIAN_POINT('Ctrl Pts',(79.7683861076351,7.3500904517831,135.339570821136));
#69008=CARTESIAN_POINT('Ctrl Pts',(79.7442041198344,7.35373775124611,135.337952115254));
#69009=CARTESIAN_POINT('Ctrl Pts',(79.7368835629395,7.35489190040628,135.337459044359));
#69010=CARTESIAN_POINT('Ctrl Pts',(79.7241384735539,7.35698851781325,135.336594912208));
#69011=CARTESIAN_POINT('Ctrl Pts',(79.7187105267668,7.35790909399508,135.336225075123));
#69012=CARTESIAN_POINT('Ctrl Pts',(79.7070675909919,7.35994315140387,135.335427754671));
#69013=CARTESIAN_POINT('Ctrl Pts',(79.7008544413295,7.36106504269217,135.334999837235));
#69014=CARTESIAN_POINT('Ctrl Pts',(79.6837663099493,7.3642510035482,135.333816498112));
#69015=CARTESIAN_POINT('Ctrl Pts',(79.6729055217632,7.36638813912674,135.333057211024));
#69016=CARTESIAN_POINT('Ctrl Pts',(79.6106135659066,7.37929173353919,135.328664026149));
#69017=CARTESIAN_POINT('Ctrl Pts',(79.5596980648687,7.39237748693745,135.324923475073));
#69018=CARTESIAN_POINT('Ctrl Pts',(79.4119690862255,7.43788958409844,135.31377785942));
#69019=CARTESIAN_POINT('Ctrl Pts',(79.3174062356663,7.47683327946542,135.306277611792));
#69020=CARTESIAN_POINT('Ctrl Pts',(79.1627104763143,7.55785936185751,135.293761005204));
#69021=CARTESIAN_POINT('Ctrl Pts',(79.1006811008133,7.59570249196534,135.288661579771));
#69022=CARTESIAN_POINT('Ctrl Pts',(79.0269119947805,7.64760742475122,135.282506098413));
#69023=CARTESIAN_POINT('Ctrl Pts',(79.0126747578349,7.65796615133012,135.281313313264));
#69024=CARTESIAN_POINT('Ctrl Pts',(78.9900273114165,7.6749994959794,135.279407441579));
#69025=CARTESIAN_POINT('Ctrl Pts',(78.9815130756263,7.68153287430435,135.278688948962));
#69026=CARTESIAN_POINT('Ctrl Pts',(78.9653497315866,7.69418578672538,135.277320881687));
#69027=CARTESIAN_POINT('Ctrl Pts',(78.9576903320825,7.70029137854909,135.276670795295));
#69028=CARTESIAN_POINT('Ctrl Pts',(78.9403207273325,7.71438964180317,135.27519214855));
#69029=CARTESIAN_POINT('Ctrl Pts',(78.9306462081757,7.72242548696557,135.274365366127));
#69030=CARTESIAN_POINT('Ctrl Pts',(78.9050436415752,7.74418608268522,135.272167883603));
#69031=CARTESIAN_POINT('Ctrl Pts',(78.8892825334564,7.75810435436498,135.270805098002));
#69032=CARTESIAN_POINT('Ctrl Pts',(78.785007142001,7.85376114434714,135.261708171914));
#69033=CARTESIAN_POINT('Ctrl Pts',(78.7053200499514,7.94459541896909,135.254389280659));
#69034=CARTESIAN_POINT('Ctrl Pts',(78.5979475730788,8.0976566520055,135.242965088757));
#69035=CARTESIAN_POINT('Ctrl Pts',(78.5630673382307,8.15430633410518,135.238892842738));
#69036=CARTESIAN_POINT('Ctrl Pts',(78.521038709007,8.23270897647865,135.233263027437));
#69037=CARTESIAN_POINT('Ctrl Pts',(78.5108140012874,8.25274704738411,135.231824481991));
#69038=CARTESIAN_POINT('Ctrl Pts',(78.4940058489315,8.28740306060595,135.22932661385));
#69039=CARTESIAN_POINT('Ctrl Pts',(78.4872217666789,8.301920669576,135.228277335055));
#69040=CARTESIAN_POINT('Ctrl Pts',(78.4776817992591,8.32312808515022,135.226737113721));
#69041=CARTESIAN_POINT('Ctrl Pts',(78.474758190257,8.32974205681834,135.226255727875));
#69042=CARTESIAN_POINT('Ctrl Pts',(78.4697121624634,8.34136148585165,135.22540785943));
#69043=CARTESIAN_POINT('Ctrl Pts',(78.4675710458501,8.34635861719915,135.225042509136));
#69044=CARTESIAN_POINT('Ctrl Pts',(78.4629609830329,8.35726516019802,135.224243469643));
#69045=CARTESIAN_POINT('Ctrl Pts',(78.4605016781524,8.36317826077445,135.223809250165));
#69046=CARTESIAN_POINT('Ctrl Pts',(78.453732180635,8.37972309185749,135.222591783484));
#69047=CARTESIAN_POINT('Ctrl Pts',(78.4494977200106,8.39038514328856,135.221804314434));
#69048=CARTESIAN_POINT('Ctrl Pts',(78.4217951048182,8.4622944255158,135.216477948403));
#69049=CARTESIAN_POINT('Ctrl Pts',(78.4018538499882,8.52483167063241,135.211773462402));
#69050=CARTESIAN_POINT('Ctrl Pts',(78.3800892829802,8.61018958902758,135.205388320628));
#69051=CARTESIAN_POINT('Ctrl Pts',(78.3749694611813,8.63211603112233,135.203751007043));
#69052=CARTESIAN_POINT('Ctrl Pts',(78.3556833935058,8.72299245558801,135.196989681015));
#69053=CARTESIAN_POINT('Ctrl Pts',(78.3454484854014,8.79270639435171,135.191865066245));
#69054=CARTESIAN_POINT('Ctrl Pts',(78.3359116036228,8.90817036100321,135.183580455327));
#69055=CARTESIAN_POINT('Ctrl Pts',(78.3340252029878,8.95361618722017,135.180369783187));
#69056=CARTESIAN_POINT('Ctrl Pts',(78.3339832799616,9.03001090103268,135.175064120421));
#69057=CARTESIAN_POINT('Ctrl Pts',(78.3348273798225,9.06093218182135,135.172941591376));
#69058=CARTESIAN_POINT('Ctrl Pts',(78.3372103810584,9.10410698033752,135.170011188523));
#69059=CARTESIAN_POINT('Ctrl Pts',(78.3380251523274,9.11639243985792,135.169181086744));
#69060=CARTESIAN_POINT('Ctrl Pts',(78.3396793292485,9.13774683111602,135.167744448532));
#69061=CARTESIAN_POINT('Ctrl Pts',(78.3404570351457,9.14681986477141,135.167136010918));
#69062=CARTESIAN_POINT('Ctrl Pts',(78.3422420221702,9.16581283062367,135.165866268476));
#69063=CARTESIAN_POINT('Ctrl Pts',(78.3432640475013,9.17573104138504,135.165205451804));
#69064=CARTESIAN_POINT('Ctrl Pts',(78.3459230598327,9.19944540806841,135.163630504336));
#69065=CARTESIAN_POINT('Ctrl Pts',(78.347643710537,9.21323158013467,135.162719032102));
#69066=CARTESIAN_POINT('Ctrl Pts',(78.3542717295818,9.26142340818167,135.159545705797));
#69067=CARTESIAN_POINT('Ctrl Pts',(78.3600831440737,9.29569699801195,135.157312135275));
#69068=CARTESIAN_POINT('Ctrl Pts',(78.377253028677,9.38072420582431,135.151806446648));
#69069=CARTESIAN_POINT('Ctrl Pts',(78.389923300544,9.43117546839901,135.148572236091));
#69070=CARTESIAN_POINT('Ctrl Pts',(78.4145339668366,9.51279575799008,135.143322369138));
#69071=CARTESIAN_POINT('Ctrl Pts',(78.4250816317236,9.54432720267512,135.141289483025));
#69072=CARTESIAN_POINT('Ctrl Pts',(78.436559333852,9.57550784828241,135.139259993339));
#69073=CARTESIAN_POINT('Ctrl Pts',(78.4365593737638,9.57550795670805,135.330578607084));
#69074=CARTESIAN_POINT('Ctrl Pts',(78.4355262723798,9.57270140528524,135.33077950276));
#69075=CARTESIAN_POINT('Ctrl Pts',(78.4345007395636,9.56989210354653,135.330980854609));
#69076=CARTESIAN_POINT('Ctrl Pts',(78.4313071287389,9.56106998627476,135.331613968312));
#69077=CARTESIAN_POINT('Ctrl Pts',(78.4291661450982,9.55504761120526,135.332047319095));
#69078=CARTESIAN_POINT('Ctrl Pts',(78.4232962754902,9.53823024994616,135.333260372946));
#69079=CARTESIAN_POINT('Ctrl Pts',(78.4196437447625,9.52740925797726,135.33404425235));
#69080=CARTESIAN_POINT('Ctrl Pts',(78.3963374997551,9.45594559517682,135.339239229933));
#69081=CARTESIAN_POINT('Ctrl Pts',(78.3800690873393,9.39426112985148,135.343806896006));
#69082=CARTESIAN_POINT('Ctrl Pts',(78.3452668265791,9.22301847979288,135.356465476987));
#69083=CARTESIAN_POINT('Ctrl Pts',(78.334083988153,9.11228258671161,135.364607419398));
#69084=CARTESIAN_POINT('Ctrl Pts',(78.3339601059339,8.9475905634631,135.37627703322));
#69085=CARTESIAN_POINT('Ctrl Pts',(78.3365124686746,8.89395279681553,135.380013427585));
#69086=CARTESIAN_POINT('Ctrl Pts',(78.3432447661313,8.82394431812517,135.384805757513));
#69087=CARTESIAN_POINT('Ctrl Pts',(78.3450880334805,8.80738658885369,135.385933100535));
#69088=CARTESIAN_POINT('Ctrl Pts',(78.3485009066364,8.78041502197843,135.387760125986));
#69089=CARTESIAN_POINT('Ctrl Pts',(78.3499213969916,8.76998384700473,135.388464434486));
#69090=CARTESIAN_POINT('Ctrl Pts',(78.3528637810574,8.74980904945305,135.38982244397));
#69091=CARTESIAN_POINT('Ctrl Pts',(78.3543734980957,8.74006412552131,135.390476498127));
#69092=CARTESIAN_POINT('Ctrl Pts',(78.3581156922323,8.71724976331965,135.392003588042));
#69093=CARTESIAN_POINT('Ctrl Pts',(78.3604178571507,8.7041923088771,135.392874387061));
#69094=CARTESIAN_POINT('Ctrl Pts',(78.3685721522937,8.66096687825507,135.39574766828));
#69095=CARTESIAN_POINT('Ctrl Pts',(78.3751032246534,8.63093233611292,135.397728715485));
#69096=CARTESIAN_POINT('Ctrl Pts',(78.3929307120513,8.55864300837883,135.402474127848));
#69097=CARTESIAN_POINT('Ctrl Pts',(78.4050672459156,8.51661856466896,135.405213399711));
#69098=CARTESIAN_POINT('Ctrl Pts',(78.4417660192211,8.40606709352683,135.412431961071));
#69099=CARTESIAN_POINT('Ctrl Pts',(78.4691873764116,8.33859052489656,135.416848633756));
#69100=CARTESIAN_POINT('Ctrl Pts',(78.5082913556486,8.25794485264148,135.422331579828));
#69101=CARTESIAN_POINT('Ctrl Pts',(78.5158807852211,8.24288001844525,135.423365202029));
#69102=CARTESIAN_POINT('Ctrl Pts',(78.5569119677471,8.16442251607549,135.428809918712));
#69103=CARTESIAN_POINT('Ctrl Pts',(78.594186073562,8.10312910721448,135.433275373539));
#69104=CARTESIAN_POINT('Ctrl Pts',(78.6419287132801,8.03494426001742,135.438720104484));
#69105=CARTESIAN_POINT('Ctrl Pts',(78.6486718058958,8.02552460550151,135.439483540475));
#69106=CARTESIAN_POINT('Ctrl Pts',(78.6593083991554,8.0109886991139,135.440680571152));
#69107=CARTESIAN_POINT('Ctrl Pts',(78.6631343644788,8.00582315911466,135.441109732105));
#69108=CARTESIAN_POINT('Ctrl Pts',(78.6702479503188,7.99633422592931,135.441905355014));
#69109=CARTESIAN_POINT('Ctrl Pts',(78.6735269361245,7.99200460944198,135.442271229362));
#69110=CARTESIAN_POINT('Ctrl Pts',(78.6811961254307,7.98198033279288,135.443124925565));
#69111=CARTESIAN_POINT('Ctrl Pts',(78.6856020646813,7.97629800956047,135.443613818828));
#69112=CARTESIAN_POINT('Ctrl Pts',(78.6998089939681,7.95821830353017,135.445184849795));
#69113=CARTESIAN_POINT('Ctrl Pts',(78.7097493242125,7.94593221112157,135.446275972561));
#69114=CARTESIAN_POINT('Ctrl Pts',(78.7657260411902,7.878724162347,135.4523678497));
#69115=CARTESIAN_POINT('Ctrl Pts',(78.815090538436,7.82668024068256,135.457545086332));
#69116=CARTESIAN_POINT('Ctrl Pts',(78.9644277739157,7.68830054279848,135.472346573717));
#69117=CARTESIAN_POINT('Ctrl Pts',(79.0715402208265,7.61041741960888,135.481955240158));
#69118=CARTESIAN_POINT('Ctrl Pts',(79.210581360526,7.53264839284583,135.492967592059));
#69119=CARTESIAN_POINT('Ctrl Pts',(79.2347530466752,7.51989872622275,135.494836149405));
#69120=CARTESIAN_POINT('Ctrl Pts',(79.2704570670618,7.50217482543893,135.497531655256));
#69121=CARTESIAN_POINT('Ctrl Pts',(79.2817482452908,7.49672771052085,135.498374914482));
#69122=CARTESIAN_POINT('Ctrl Pts',(79.3019624432637,7.48725568726848,135.499868658341));
#69123=CARTESIAN_POINT('Ctrl Pts',(79.3108613630338,7.48318104825195,135.500520834452));
#69124=CARTESIAN_POINT('Ctrl Pts',(79.329606366152,7.47479710343564,135.501883524849));
#69125=CARTESIAN_POINT('Ctrl Pts',(79.3394593108189,7.47050416572711,135.502593455724));
#69126=CARTESIAN_POINT('Ctrl Pts',(79.365634982382,7.45939952365756,135.504463258595));
#69127=CARTESIAN_POINT('Ctrl Pts',(79.3820261018241,7.45275176411336,135.505617573671));
#69128=CARTESIAN_POINT('Ctrl Pts',(79.4675358538586,7.41964720720809,135.511559328879));
#69129=CARTESIAN_POINT('Ctrl Pts',(79.5382595516358,7.39755475181327,135.516199808249));
#69130=CARTESIAN_POINT('Ctrl Pts',(79.6749399046776,7.36466444374126,135.524873926533));
#69131=CARTESIAN_POINT('Ctrl Pts',(79.7405293754179,7.3529840330421,135.528914746655));
#69132=CARTESIAN_POINT('Ctrl Pts',(79.8206920456076,7.34361696822805,135.53385549727));
#69133=CARTESIAN_POINT('Ctrl Pts',(79.8347620036837,7.34215426290705,135.534722882639));
#69134=CARTESIAN_POINT('Ctrl Pts',(79.919920544765,7.33439608424094,135.539982085897));
#69135=CARTESIAN_POINT('Ctrl Pts',(79.9913263135815,7.33249548365123,135.54442948329));
#69136=CARTESIAN_POINT('Ctrl Pts',(80.0741971893372,7.33561275340795,135.54985408425));
#69137=CARTESIAN_POINT('Ctrl Pts',(80.0857651839337,7.33616874523279,135.550617320797));
#69138=CARTESIAN_POINT('Ctrl Pts',(80.103742584287,7.3372207635344,135.551814104463));
#69139=CARTESIAN_POINT('Ctrl Pts',(80.110156765949,7.33763337483366,135.552243220755));
#69140=CARTESIAN_POINT('Ctrl Pts',(80.1219864120354,7.33846311626056,135.553038806115));
#69141=CARTESIAN_POINT('Ctrl Pts',(80.1274024210042,7.33886962559536,135.553404688075));
#69142=CARTESIAN_POINT('Ctrl Pts',(80.1399848731861,7.33987592262087,135.554258461848));
#69143=CARTESIAN_POINT('Ctrl Pts',(80.1471494855941,7.34049563390066,135.554747425744));
#69144=CARTESIAN_POINT('Ctrl Pts',(80.1700509906115,7.34262599477267,135.556318915199));
#69145=CARTESIAN_POINT('Ctrl Pts',(80.1857699441369,7.34431421607951,135.557410432914));
#69146=CARTESIAN_POINT('Ctrl Pts',(80.2726560108602,7.3548986234757,135.56350670515));
#69147=CARTESIAN_POINT('Ctrl Pts',(80.3432091811378,7.36815893093811,135.568688199619));
#69148=CARTESIAN_POINT('Ctrl Pts',(80.5406863706064,7.41864906966731,135.583506964158));
#69149=CARTESIAN_POINT('Ctrl Pts',(80.6643696174399,7.46649499200883,135.593128129855));
#69150=CARTESIAN_POINT('Ctrl Pts',(80.8027309224151,7.53993897976176,135.603954121002));
#69151=CARTESIAN_POINT('Ctrl Pts',(80.8240961288433,7.55189061297607,135.605629646067));
#69152=CARTESIAN_POINT('Ctrl Pts',(80.8557933317578,7.57055075849263,135.608122311018));
#69153=CARTESIAN_POINT('Ctrl Pts',(80.8663262234286,7.57690961304857,135.608951799932));
#69154=CARTESIAN_POINT('Ctrl Pts',(80.8845276031981,7.58817502206136,135.610387567001));
#69155=CARTESIAN_POINT('Ctrl Pts',(80.8922279884972,7.59302875958053,135.610995742188));
#69156=CARTESIAN_POINT('Ctrl Pts',(80.9082777442465,7.60333006208968,135.612265113588));
#69157=CARTESIAN_POINT('Ctrl Pts',(80.9166187988983,7.60878996517094,135.612925820588));
#69158=CARTESIAN_POINT('Ctrl Pts',(80.9364673964996,7.62203850458377,135.614500826786));
#69159=CARTESIAN_POINT('Ctrl Pts',(80.9479276130456,7.62989696471609,135.615412464521));
#69160=CARTESIAN_POINT('Ctrl Pts',(80.9877284052998,7.65792749639774,135.618588065335));
#69161=CARTESIAN_POINT('Ctrl Pts',(81.015535505028,7.67884371973154,135.620823683606));
#69162=CARTESIAN_POINT('Ctrl Pts',(81.0832734073492,7.73319888802652,135.626335958627));
#69163=CARTESIAN_POINT('Ctrl Pts',(81.1223302056246,7.76766812399154,135.629574577227));
#69164=CARTESIAN_POINT('Ctrl Pts',(81.2309739037552,7.87300760811763,135.638893173755));
#69165=CARTESIAN_POINT('Ctrl Pts',(81.2959154866832,7.94832989600981,135.644859765391));
#69166=CARTESIAN_POINT('Ctrl Pts',(81.3825097768175,8.06905684535266,135.654117567324));
#69167=CARTESIAN_POINT('Ctrl Pts',(81.4094588894118,8.11038599325179,135.657242339616));
#69168=CARTESIAN_POINT('Ctrl Pts',(81.4400674820342,8.1622171387033,135.661186180796));
#69169=CARTESIAN_POINT('Ctrl Pts',(81.4455101231757,8.17164322670767,135.661904399419));
#69170=CARTESIAN_POINT('Ctrl Pts',(81.4539421455483,8.18658278726268,135.663045365083));
#69171=CARTESIAN_POINT('Ctrl Pts',(81.4569935343459,8.19206116430724,135.66346431519));
#69172=CARTESIAN_POINT('Ctrl Pts',(81.4626695039906,8.2023883644143,135.664255362671));
#69173=CARTESIAN_POINT('Ctrl Pts',(81.4653010320628,8.2072331484142,135.664627018325));
#69174=CARTESIAN_POINT('Ctrl Pts',(81.4714469492169,8.21868325443794,135.665506598766));
#69175=CARTESIAN_POINT('Ctrl Pts',(81.4749409411293,8.22529928613699,135.666015761414));
#69176=CARTESIAN_POINT('Ctrl Pts',(81.4864437598857,8.24744029100124,135.667722237322));
#69177=CARTESIAN_POINT('Ctrl Pts',(81.4942526464905,8.26306707550487,135.668930754027));
#69178=CARTESIAN_POINT('Ctrl Pts',(81.5127500832846,8.30158649940001,135.671914618186));
#69179=CARTESIAN_POINT('Ctrl Pts',(81.5231661820241,8.32460465184501,135.673701839157));
#69180=CARTESIAN_POINT('Ctrl Pts',(81.5652864053762,8.42361949908233,135.681382280979));
#69181=CARTESIAN_POINT('Ctrl Pts',(81.5918557215902,8.5016722043508,135.68741180965));
#69182=CARTESIAN_POINT('Ctrl Pts',(81.6373024528799,8.67672963025059,135.700546199591));
#69183=CARTESIAN_POINT('Ctrl Pts',(81.6535550730723,8.77411413891817,135.707597502603));
#69184=CARTESIAN_POINT('Ctrl Pts',(81.6629257119012,8.89608075737983,135.71602037739));
#69185=CARTESIAN_POINT('Ctrl Pts',(81.6642393184605,8.91982067431672,135.7176418433));
#69186=CARTESIAN_POINT('Ctrl Pts',(81.6654563090048,8.95573707809814,135.720069018246));
#69187=CARTESIAN_POINT('Ctrl Pts',(81.665735071334,8.96789689741178,135.720886281368));
#69188=CARTESIAN_POINT('Ctrl Pts',(81.665997040466,8.98978188462742,135.722349441641));
#69189=CARTESIAN_POINT('Ctrl Pts',(81.6660283044952,8.99950580976594,135.722996807222));
#69190=CARTESIAN_POINT('Ctrl Pts',(81.6659130142133,9.02031603070605,135.724376609691));
#69191=CARTESIAN_POINT('Ctrl Pts',(81.66574093169,9.03140175975677,135.725108219727));
#69192=CARTESIAN_POINT('Ctrl Pts',(81.6649666818517,9.06175307058747,135.727102466855));
#69193=CARTESIAN_POINT('Ctrl Pts',(81.6641408185409,9.08101160115348,135.72835811806));
#69194=CARTESIAN_POINT('Ctrl Pts',(81.6615587931183,9.12384220092693,135.731131890408));
#69195=CARTESIAN_POINT('Ctrl Pts',(81.6596348364403,9.14740015750329,135.732644831843));
#69196=CARTESIAN_POINT('Ctrl Pts',(81.651886303822,9.22253291145368,135.737439086954));
#69197=CARTESIAN_POINT('Ctrl Pts',(81.6441529643126,9.27388116766472,135.740667914712));
#69198=CARTESIAN_POINT('Ctrl Pts',(81.6143575210505,9.42378454711294,135.750080428851));
#69199=CARTESIAN_POINT('Ctrl Pts',(81.5857260250495,9.52078278621531,135.756144397367));
#69200=CARTESIAN_POINT('Ctrl Pts',(81.530774782337,9.65923586281198,135.765435689647));
#69201=CARTESIAN_POINT('Ctrl Pts',(81.5111337397708,9.70309120762843,135.768482149024));
#69202=CARTESIAN_POINT('Ctrl Pts',(81.4847261831156,9.75582007881523,135.77234650148));
#69203=CARTESIAN_POINT('Ctrl Pts',(81.4797280760176,9.76555903475263,135.77306896099));
#69204=CARTESIAN_POINT('Ctrl Pts',(81.4717394179309,9.78075463082542,135.774211065236));
#69205=CARTESIAN_POINT('Ctrl Pts',(81.4688135424138,9.78624517951265,135.774626812462));
#69206=CARTESIAN_POINT('Ctrl Pts',(81.463230742399,9.79658165709692,135.77541556904));
#69207=CARTESIAN_POINT('Ctrl Pts',(81.4605803742529,9.80143091317351,135.775788174682));
#69208=CARTESIAN_POINT('Ctrl Pts',(81.454239459696,9.81289666766545,135.776675184424));
#69209=CARTESIAN_POINT('Ctrl Pts',(81.4505278485402,9.81950128338884,135.777190888842));
#69210=CARTESIAN_POINT('Ctrl Pts',(81.4378304522403,9.8417391122704,135.778942836025));
#69211=CARTESIAN_POINT('Ctrl Pts',(81.4286363033025,9.85725106568938,135.780191082515));
#69212=CARTESIAN_POINT('Ctrl Pts',(81.4053782746448,9.89507738748669,135.783294438228));
#69213=CARTESIAN_POINT('Ctrl Pts',(81.3910330153885,9.9172124186111,135.785162601277));
#69214=CARTESIAN_POINT('Ctrl Pts',(81.3256058612948,10.0131007982961,135.793459217994));
#69215=CARTESIAN_POINT('Ctrl Pts',(81.2691408661249,10.0829981997379,135.800041990791));
#69216=CARTESIAN_POINT('Ctrl Pts',(81.1397406665309,10.2190842941631,135.813648349463));
#69217=CARTESIAN_POINT('Ctrl Pts',(81.0660031271714,10.2840633393234,135.820625335516));
#69218=CARTESIAN_POINT('Ctrl Pts',(80.9717595732041,10.3533645055372,135.82862382769));
#69219=CARTESIAN_POINT('Ctrl Pts',(80.9563662710091,10.3642858056406,135.829904297675));
#69220=CARTESIAN_POINT('Ctrl Pts',(80.9317110782607,10.381155852343,135.831915381344));
#69221=CARTESIAN_POINT('Ctrl Pts',(80.9225705091458,10.3872781579476,135.832652520586));
#69222=CARTESIAN_POINT('Ctrl Pts',(80.9060423576129,10.3981130176164,135.833970623002));
#69223=CARTESIAN_POINT('Ctrl Pts',(80.8986770458846,10.4028586300952,135.834552805803));
#69224=CARTESIAN_POINT('Ctrl Pts',(80.8812895413516,10.4138686004615,135.835915252056));
#69225=CARTESIAN_POINT('Ctrl Pts',(80.8712373615092,10.4200849083835,135.836693722761));
#69226=CARTESIAN_POINT('Ctrl Pts',(80.8415842486195,10.4379891213393,135.838964119111));
#69227=CARTESIAN_POINT('Ctrl Pts',(80.8218078298927,10.4493821900743,135.840445372837));
#69228=CARTESIAN_POINT('Ctrl Pts',(80.7293814862687,10.5001281731556,135.847228376951));
#69229=CARTESIAN_POINT('Ctrl Pts',(80.654098593684,10.5344507911214,135.852354049634));
#69230=CARTESIAN_POINT('Ctrl Pts',(80.5227686740386,10.582895324556,135.86093616232));
#69231=CARTESIAN_POINT('Ctrl Pts',(80.4679769501478,10.5999506848582,135.864419714101));
#69232=CARTESIAN_POINT('Ctrl Pts',(80.3377702569209,10.633218563853,135.872667132635));
#69233=CARTESIAN_POINT('Ctrl Pts',(80.2619015467661,10.6470871492649,135.877449139394));
#69234=CARTESIAN_POINT('Ctrl Pts',(80.173821971105,10.6569479918808,135.883246274229));
#69235=CARTESIAN_POINT('Ctrl Pts',(80.1622741205884,10.658118758322,135.884011169932));
#69236=CARTESIAN_POINT('Ctrl Pts',(80.1443085207512,10.6597507154383,135.885210008354));
#69237=CARTESIAN_POINT('Ctrl Pts',(80.1378984781843,10.6602955739268,135.885639496073));
#69238=CARTESIAN_POINT('Ctrl Pts',(80.1260198425192,10.6612360039375,135.886438895678));
#69239=CARTESIAN_POINT('Ctrl Pts',(80.1205522586141,10.6616417216824,135.886808245399));
#69240=CARTESIAN_POINT('Ctrl Pts',(80.1078860378463,10.6625187652172,135.887667066783));
#69241=CARTESIAN_POINT('Ctrl Pts',(80.1006862709663,10.6629703280143,135.888157598022));
#69242=CARTESIAN_POINT('Ctrl Pts',(80.077574998257,10.6642692133135,135.889739284605));
#69243=CARTESIAN_POINT('Ctrl Pts',(80.0616547356785,10.6649349962972,135.890839590619));
#69244=CARTESIAN_POINT('Ctrl Pts',(80.0234091746146,10.6659851504276,135.893504900459));
#69245=CARTESIAN_POINT('Ctrl Pts',(80.0010812613823,10.6661492253617,135.895078907019));
#69246=CARTESIAN_POINT('Ctrl Pts',(79.9131523002241,10.6650280120699,135.901332136934));
#69247=CARTESIAN_POINT('Ctrl Pts',(79.8476567622816,10.6603166690618,135.906107479269));
#69248=CARTESIAN_POINT('Ctrl Pts',(79.6619254928567,10.6358727075662,135.919744178876));
#69249=CARTESIAN_POINT('Ctrl Pts',(79.5433200779141,10.6068066586641,135.92853648176));
#69250=CARTESIAN_POINT('Ctrl Pts',(79.4092286288398,10.5578783178132,135.938355106246));
#69251=CARTESIAN_POINT('Ctrl Pts',(79.3896674785021,10.5503193053925,135.939785442954));
#69252=CARTESIAN_POINT('Ctrl Pts',(79.3586268708904,10.5376456746956,135.942052817809));
#69253=CARTESIAN_POINT('Ctrl Pts',(79.3470540734671,10.5327672177043,135.942897634334));
#69254=CARTESIAN_POINT('Ctrl Pts',(79.3265595088388,10.523853585934,135.944393147976));
#69255=CARTESIAN_POINT('Ctrl Pts',(79.3176161856124,10.519869791592,135.945045550733));
#69256=CARTESIAN_POINT('Ctrl Pts',(79.2989405155616,10.5113526569068,135.946407729794));
#69257=CARTESIAN_POINT('Ctrl Pts',(79.2892157983496,10.5068035977015,135.947116931299));
#69258=CARTESIAN_POINT('Ctrl Pts',(79.2636366710297,10.4945353687164,135.948982554098));
#69259=CARTESIAN_POINT('Ctrl Pts',(79.2478593963666,10.4866578192775,135.950133464123));
#69260=CARTESIAN_POINT('Ctrl Pts',(79.1673402747877,10.4448448283746,135.956013131467));
#69261=CARTESIAN_POINT('Ctrl Pts',(79.1047536180214,10.4069238260739,135.960598823203));
#69262=CARTESIAN_POINT('Ctrl Pts',(78.9618238360485,10.3069107756024,135.971367229113));
#69263=CARTESIAN_POINT('Ctrl Pts',(78.8842717425862,10.2413599753503,135.977454361145));
#69264=CARTESIAN_POINT('Ctrl Pts',(78.7959791055502,10.1517330206466,135.985274076365));
#69265=CARTESIAN_POINT('Ctrl Pts',(78.7791866299631,10.1339179362806,135.986807656105));
#69266=CARTESIAN_POINT('Ctrl Pts',(78.741903796181,10.0925762592732,135.990337665404));
#69267=CARTESIAN_POINT('Ctrl Pts',(78.7216703511934,10.0688320524545,135.992344934213));
#69268=CARTESIAN_POINT('Ctrl Pts',(78.6961022820835,10.037062565829,135.995026271725));
#69269=CARTESIAN_POINT('Ctrl Pts',(78.6901526190616,10.0295376885197,135.995661063656));
#69270=CARTESIAN_POINT('Ctrl Pts',(78.680633553061,10.0172823066178,135.996695201466));
#69271=CARTESIAN_POINT('Ctrl Pts',(78.6770237243328,10.0125832725887,135.997091783689));
#69272=CARTESIAN_POINT('Ctrl Pts',(78.6700171507486,10.0033611596313,135.997870449096));
#69273=CARTESIAN_POINT('Ctrl Pts',(78.6666182534952,9.99883988229195,135.998252377929));
#69274=CARTESIAN_POINT('Ctrl Pts',(78.6582720049682,9.98761903026825,135.999200510252));
#69275=CARTESIAN_POINT('Ctrl Pts',(78.653351783978,9.98089955478689,135.999768517035));
#69276=CARTESIAN_POINT('Ctrl Pts',(78.6350024287481,9.95544183230182,136.001920485684));
#69277=CARTESIAN_POINT('Ctrl Pts',(78.6219130226321,9.93646335570433,136.003524716942));
#69278=CARTESIAN_POINT('Ctrl Pts',(78.5887353552704,9.88615620575833,136.007764765068));
#69279=CARTESIAN_POINT('Ctrl Pts',(78.5692960739808,9.85441596795094,136.010427614625));
#69280=CARTESIAN_POINT('Ctrl Pts',(78.5061596399335,9.74312315643574,136.019662196131));
#69281=CARTESIAN_POINT('Ctrl Pts',(78.4679062115829,9.66066563172754,136.026320752444));
#69282=CARTESIAN_POINT('Ctrl Pts',(78.4365593745323,9.57550795879571,136.032852165095));
#69283=CARTESIAN_POINT('Origin',(80.,9.,134.));
#69284=CARTESIAN_POINT('',(78.436559386885,9.57550799235334,136.733447166179));
#69285=CARTESIAN_POINT('',(78.4365593610507,9.57550792217121,136.539851329404));
#69286=CARTESIAN_POINT('',(78.4365593737638,9.57550795670799,134.));
#69287=CARTESIAN_POINT('',(78.3340002443602,8.99909766519367,135.879690700183));
#69288=CARTESIAN_POINT('Ctrl Pts',(78.4365593610507,9.57550792217122,136.539851329404));
#69289=CARTESIAN_POINT('Ctrl Pts',(78.4458980275004,9.60087760011751,136.537889809312));
#69290=CARTESIAN_POINT('Ctrl Pts',(78.4558546510834,9.62602120168908,136.535921262459));
#69291=CARTESIAN_POINT('Ctrl Pts',(78.513413053214,9.76163062536091,136.525197504869));
#69292=CARTESIAN_POINT('Ctrl Pts',(78.5722644735132,9.86695051212577,136.516515201914));
#69293=CARTESIAN_POINT('Ctrl Pts',(78.6541410523814,9.98217214453261,136.506791241766));
#69294=CARTESIAN_POINT('Ctrl Pts',(78.6666490069173,9.99908639648936,136.505356318561));
#69295=CARTESIAN_POINT('Ctrl Pts',(78.6871436490772,10.0257301910071,136.503083020575));
#69296=CARTESIAN_POINT('Ctrl Pts',(78.694925708194,10.0356135045628,136.502236805642));
#69297=CARTESIAN_POINT('Ctrl Pts',(78.7089655592686,10.0530346707326,136.500739553739));
#69298=CARTESIAN_POINT('Ctrl Pts',(78.7151792245619,10.060607150158,136.500086799618));
#69299=CARTESIAN_POINT('Ctrl Pts',(78.7283389195473,10.0763592497235,136.498724614947));
#69300=CARTESIAN_POINT('Ctrl Pts',(78.7352979370172,10.0845274726714,136.498015753178));
#69301=CARTESIAN_POINT('Ctrl Pts',(78.7538775446772,10.1059134442187,136.496152676661));
#69302=CARTESIAN_POINT('Ctrl Pts',(78.7656296915254,10.1190155047002,136.495003942963));
#69303=CARTESIAN_POINT('Ctrl Pts',(78.8268276349446,10.185105430601,136.489166463528));
#69304=CARTESIAN_POINT('Ctrl Pts',(78.879488287366,10.2350156611454,136.484618156925));
#69305=CARTESIAN_POINT('Ctrl Pts',(79.0133919326892,10.3462861007539,136.473867741119));
#69306=CARTESIAN_POINT('Ctrl Pts',(79.0973198710174,10.4039405144166,136.467764442186));
#69307=CARTESIAN_POINT('Ctrl Pts',(79.2322433804078,10.4794992547448,136.458155545519));
#69308=CARTESIAN_POINT('Ctrl Pts',(79.2797188993223,10.5031840215815,136.454805680345));
#69309=CARTESIAN_POINT('Ctrl Pts',(79.3384037901551,10.529042145102,136.450606265239));
#69310=CARTESIAN_POINT('Ctrl Pts',(79.3486145731024,10.5334198497632,136.44987349627));
#69311=CARTESIAN_POINT('Ctrl Pts',(79.3647039479201,10.5401282105118,136.448714407541));
#69312=CARTESIAN_POINT('Ctrl Pts',(79.370553547515,10.5425281646531,136.448292084374));
#69313=CARTESIAN_POINT('Ctrl Pts',(79.3810077458325,10.5467479118295,136.44753545195));
#69314=CARTESIAN_POINT('Ctrl Pts',(79.3856069953906,10.5485805587497,136.447201917851));
#69315=CARTESIAN_POINT('Ctrl Pts',(79.3967884586408,10.552978345497,136.446389492731));
#69316=CARTESIAN_POINT('Ctrl Pts',(79.4033788396736,10.5555221283219,136.445909364363));
#69317=CARTESIAN_POINT('Ctrl Pts',(79.4241170173408,10.56337556062,136.444394953272));
#69318=CARTESIAN_POINT('Ctrl Pts',(79.438320538265,10.5685345057026,136.443352542089));
#69319=CARTESIAN_POINT('Ctrl Pts',(79.5139094505476,10.5948313099461,136.437784753802));
#69320=CARTESIAN_POINT('Ctrl Pts',(79.5764159518748,10.6125587759403,136.433112458027));
#69321=CARTESIAN_POINT('Ctrl Pts',(79.749410282889,10.6508684561015,136.420251466739));
#69322=CARTESIAN_POINT('Ctrl Pts',(79.861217992052,10.6640032544479,136.412036239531));
#69323=CARTESIAN_POINT('Ctrl Pts',(80.0204682490802,10.666536310738,136.400809113303));
#69324=CARTESIAN_POINT('Ctrl Pts',(80.0674469135898,10.6652969361736,136.397551199577));
#69325=CARTESIAN_POINT('Ctrl Pts',(80.1302143102675,10.6609799004612,136.393269371992));
#69326=CARTESIAN_POINT('Ctrl Pts',(80.1460979604029,10.6596582217318,136.392191852024));
#69327=CARTESIAN_POINT('Ctrl Pts',(80.172287697451,10.6571000615169,136.390424580544));
#69328=CARTESIAN_POINT('Ctrl Pts',(80.1826052506413,10.6559948657601,136.389730768935));
#69329=CARTESIAN_POINT('Ctrl Pts',(80.2027836034663,10.6536425196755,136.388378339198));
#69330=CARTESIAN_POINT('Ctrl Pts',(80.2126448787324,10.6524033816069,136.387719499716));
#69331=CARTESIAN_POINT('Ctrl Pts',(80.2360839112888,10.6492447993141,136.386158204223));
#69332=CARTESIAN_POINT('Ctrl Pts',(80.2496503598245,10.6472458036534,136.385258285195));
#69333=CARTESIAN_POINT('Ctrl Pts',(80.2963336744391,10.6397770917644,136.382173098446));
#69334=CARTESIAN_POINT('Ctrl Pts',(80.3293102520229,10.6334740770935,136.380013993463));
#69335=CARTESIAN_POINT('Ctrl Pts',(80.4103597203438,10.6154280592734,136.3747374412));
#69336=CARTESIAN_POINT('Ctrl Pts',(80.4581431700007,10.6025318396699,136.371653699907));
#69337=CARTESIAN_POINT('Ctrl Pts',(80.5681771776301,10.5675097634719,136.364530377955));
#69338=CARTESIAN_POINT('Ctrl Pts',(80.6298245739275,10.5437724303144,136.36052327146));
#69339=CARTESIAN_POINT('Ctrl Pts',(80.7032614684615,10.5103624497923,136.355584336946));
#69340=CARTESIAN_POINT('Ctrl Pts',(80.7165401282959,10.5041082605296,136.35468429641));
#69341=CARTESIAN_POINT('Ctrl Pts',(80.7934727348447,10.4666233640757,136.349419896146));
#69342=CARTESIAN_POINT('Ctrl Pts',(80.8551559140994,10.4315337576631,136.344999977038));
#69343=CARTESIAN_POINT('Ctrl Pts',(80.9240868982668,10.3862732260957,136.339605906287));
#69344=CARTESIAN_POINT('Ctrl Pts',(80.9336983409376,10.3798179019983,136.338842882871));
#69345=CARTESIAN_POINT('Ctrl Pts',(80.9485397695367,10.369623898227,136.337646293559));
#69346=CARTESIAN_POINT('Ctrl Pts',(80.953816932243,10.3659540890121,136.337217154765));
#69347=CARTESIAN_POINT('Ctrl Pts',(80.9635152417125,10.3591261526397,136.336421427271));
#69348=CARTESIAN_POINT('Ctrl Pts',(80.9679423382045,10.3559768237714,136.336055424912));
#69349=CARTESIAN_POINT('Ctrl Pts',(80.9781970595739,10.3486060558101,136.335201225032));
#69350=CARTESIAN_POINT('Ctrl Pts',(80.9840127922328,10.3443684766607,136.334711953221));
#69351=CARTESIAN_POINT('Ctrl Pts',(81.0025319991253,10.330690083646,136.333138896977));
#69352=CARTESIAN_POINT('Ctrl Pts',(81.015128026274,10.3211061852551,136.332046098187));
#69353=CARTESIAN_POINT('Ctrl Pts',(81.0841690520176,10.2670048330408,136.325936764934));
#69354=CARTESIAN_POINT('Ctrl Pts',(81.1378185215559,10.2190532234388,136.3207427415));
#69355=CARTESIAN_POINT('Ctrl Pts',(81.2811849946705,10.0731816316372,136.305872598001));
#69356=CARTESIAN_POINT('Ctrl Pts',(81.3625569574922,9.96778336794194,136.296214151952));
#69357=CARTESIAN_POINT('Ctrl Pts',(81.4442407137162,9.83092508232392,136.285205243351));
#69358=CARTESIAN_POINT('Ctrl Pts',(81.4573618852194,9.80769066449269,136.283381715138));
#69359=CARTESIAN_POINT('Ctrl Pts',(81.4758303629881,9.77307077235363,136.280729067577));
#69360=CARTESIAN_POINT('Ctrl Pts',(81.4816153784461,9.76192490753418,136.279884613378));
#69361=CARTESIAN_POINT('Ctrl Pts',(81.4916744330505,9.74199646418387,136.278391315488));
#69362=CARTESIAN_POINT('Ctrl Pts',(81.4959982425564,9.73323981910587,136.277740753512));
#69363=CARTESIAN_POINT('Ctrl Pts',(81.5049633818357,9.71467402722417,136.276372962746));
#69364=CARTESIAN_POINT('Ctrl Pts',(81.5095863899686,9.70485650061991,136.275656392404));
#69365=CARTESIAN_POINT('Ctrl Pts',(81.5216898386558,9.67848795092658,136.273749143768));
#69366=CARTESIAN_POINT('Ctrl Pts',(81.528996238272,9.66185830061692,136.272564435488));
#69367=CARTESIAN_POINT('Ctrl Pts',(81.5682750111704,9.56833445083818,136.265996175822));
#69368=CARTESIAN_POINT('Ctrl Pts',(81.5947210065873,9.48924235382752,136.260802471226));
#69369=CARTESIAN_POINT('Ctrl Pts',(81.6324281079547,9.34015279512863,136.251351667603));
#69370=CARTESIAN_POINT('Ctrl Pts',(81.6453576294033,9.27078321913306,136.247080789718));
#69371=CARTESIAN_POINT('Ctrl Pts',(81.6624622758917,9.1299065981701,136.238353015175));
#69372=CARTESIAN_POINT('Ctrl Pts',(81.6665015166774,9.05853763611416,136.233902556347));
#69373=CARTESIAN_POINT('Ctrl Pts',(81.6658609443739,8.97555613782454,136.228474420203));
#69374=CARTESIAN_POINT('Ctrl Pts',(81.6656507162538,8.96397415633981,136.227711019224));
#69375=CARTESIAN_POINT('Ctrl Pts',(81.6651360325248,8.9459692040301,136.226513962298));
#69376=CARTESIAN_POINT('Ctrl Pts',(81.6649151318616,8.93954395020537,136.226084738945));
#69377=CARTESIAN_POINT('Ctrl Pts',(81.6644389495642,8.92769162615402,136.225288940422));
#69378=CARTESIAN_POINT('Ctrl Pts',(81.664194303583,8.92226432882691,136.224922952537));
#69379=CARTESIAN_POINT('Ctrl Pts',(81.6635640161367,8.90965334753726,136.224068899793));
#69380=CARTESIAN_POINT('Ctrl Pts',(81.663158387874,8.90247089955206,136.223579761925));
#69381=CARTESIAN_POINT('Ctrl Pts',(81.6617121751876,8.87950594198288,136.222007575483));
#69382=CARTESIAN_POINT('Ctrl Pts',(81.6604933809911,8.86373607440735,136.220915526025));
#69383=CARTESIAN_POINT('Ctrl Pts',(81.6525008293375,8.77650657570113,136.214814543334));
#69384=CARTESIAN_POINT('Ctrl Pts',(81.6413392147133,8.70553122657962,136.209628611462));
#69385=CARTESIAN_POINT('Ctrl Pts',(81.5966894584062,8.50639479706589,136.194791421912));
#69386=CARTESIAN_POINT('Ctrl Pts',(81.5524567974861,8.38116773129696,136.185156833187));
#69387=CARTESIAN_POINT('Ctrl Pts',(81.4819160569234,8.23828547885221,136.174146397751));
#69388=CARTESIAN_POINT('Ctrl Pts',(81.4693832552013,8.21438100318894,136.172301411733));
#69389=CARTESIAN_POINT('Ctrl Pts',(81.4502138693321,8.17988328371215,136.169633008825));
#69390=CARTESIAN_POINT('Ctrl Pts',(81.4440306759922,8.169044455681,136.168793745769));
#69391=CARTESIAN_POINT('Ctrl Pts',(81.4327841307596,8.14983453727094,136.167304384201));
#69392=CARTESIAN_POINT('Ctrl Pts',(81.4277677824247,8.1414367548883,136.166652631738));
#69393=CARTESIAN_POINT('Ctrl Pts',(81.4170672044347,8.1238762711815,136.165288113281));
#69394=CARTESIAN_POINT('Ctrl Pts',(81.4113673827893,8.11472356289231,136.164575954843));
#69395=CARTESIAN_POINT('Ctrl Pts',(81.3960019106015,8.09057549888803,136.1626939861));
#69396=CARTESIAN_POINT('Ctrl Pts',(81.3861834043846,8.07567869924814,136.161529863921));
#69397=CARTESIAN_POINT('Ctrl Pts',(81.3328896409876,7.99758022478432,136.155404556238));
#69398=CARTESIAN_POINT('Ctrl Pts',(81.2853248028695,7.93727589449194,136.150602200035));
#69399=CARTESIAN_POINT('Ctrl Pts',(81.1619942589528,7.80136202703497,136.139292518966));
#69400=CARTESIAN_POINT('Ctrl Pts',(81.0827859129208,7.72935611213826,136.132888141231));
#69401=CARTESIAN_POINT('Ctrl Pts',(80.9619007348197,7.63902654463295,136.123444441762));
#69402=CARTESIAN_POINT('Ctrl Pts',(80.9255337584337,7.61403885768261,136.12063792134));
#69403=CARTESIAN_POINT('Ctrl Pts',(80.8791641576979,7.58481767525403,136.117044303455));
#69404=CARTESIAN_POINT('Ctrl Pts',(80.8700517176677,7.57919719092472,136.116337384099));
#69405=CARTESIAN_POINT('Ctrl Pts',(80.8556032078558,7.57047657391985,136.115214342057));
#69406=CARTESIAN_POINT('Ctrl Pts',(80.8503028131598,7.56731748183787,136.114801903797));
#69407=CARTESIAN_POINT('Ctrl Pts',(80.8402069969403,7.56137602564292,136.114015220141));
#69408=CARTESIAN_POINT('Ctrl Pts',(80.835415081637,7.55858806203347,136.113641337107));
#69409=CARTESIAN_POINT('Ctrl Pts',(80.823945821088,7.55199158285998,136.11274541065));
#69410=CARTESIAN_POINT('Ctrl Pts',(80.8172559187656,7.54820530045358,136.112221993922));
#69411=CARTESIAN_POINT('Ctrl Pts',(80.7941987094058,7.53536548380102,136.110415779378));
#69412=CARTESIAN_POINT('Ctrl Pts',(80.7777059411348,7.52654173717698,136.109119988525));
#69413=CARTESIAN_POINT('Ctrl Pts',(80.7364041228524,7.5053315541547,136.105871934395));
#69414=CARTESIAN_POINT('Ctrl Pts',(80.7114282203446,7.49328353415353,136.103905115514));
#69415=CARTESIAN_POINT('Ctrl Pts',(80.6071193867698,7.44613815221024,136.095711658995));
#69416=CARTESIAN_POINT('Ctrl Pts',(80.5254062658984,7.41664014416357,136.089349800247));
#69417=CARTESIAN_POINT('Ctrl Pts',(80.3465548666147,7.36745376822056,136.075907222767));
#69418=CARTESIAN_POINT('Ctrl Pts',(80.2491871353681,7.34978201894724,136.068880472038));
#69419=CARTESIAN_POINT('Ctrl Pts',(80.1320200842002,7.33913192770637,136.060836249827));
#69420=CARTESIAN_POINT('Ctrl Pts',(80.1131998031606,7.33774312707843,136.059555958063));
#69421=CARTESIAN_POINT('Ctrl Pts',(80.0833746162996,7.33605116518116,136.057544960696));
#69422=CARTESIAN_POINT('Ctrl Pts',(80.0723838103143,7.33553682960693,136.056807733068));
#69423=CARTESIAN_POINT('Ctrl Pts',(80.0526302741536,7.33480846003855,136.055489367396));
#69424=CARTESIAN_POINT('Ctrl Pts',(80.0438695133671,7.33455462973606,136.054907010221));
#69425=CARTESIAN_POINT('Ctrl Pts',(80.0232854957997,7.33412077387957,136.053544016591));
#69426=CARTESIAN_POINT('Ctrl Pts',(80.011461414904,7.3339974614781,136.052765175393));
#69427=CARTESIAN_POINT('Ctrl Pts',(79.9767976902504,7.33400501918422,136.050493189432));
#69428=CARTESIAN_POINT('Ctrl Pts',(79.9539602954211,7.33447964568401,136.049010736823));
#69429=CARTESIAN_POINT('Ctrl Pts',(79.8484624695344,7.33884393409024,136.04221843503));
#69430=CARTESIAN_POINT('Ctrl Pts',(79.7661508423424,7.34841894270687,136.037085242915));
#69431=CARTESIAN_POINT('Ctrl Pts',(79.6286599096413,7.37490279584805,136.028501166937));
#69432=CARTESIAN_POINT('Ctrl Pts',(79.5730324592314,7.38862387123253,136.025023027446));
#69433=CARTESIAN_POINT('Ctrl Pts',(79.444500014626,7.42745215560983,136.016782791305));
#69434=CARTESIAN_POINT('Ctrl Pts',(79.3724200242907,7.45480512372725,136.012002410027));
#69435=CARTESIAN_POINT('Ctrl Pts',(79.2919795314778,7.49188951860505,136.00620841966));
#69436=CARTESIAN_POINT('Ctrl Pts',(79.281510138081,7.49684914002765,136.005444964198));
#69437=CARTESIAN_POINT('Ctrl Pts',(79.2653123770348,7.50473031435706,136.004247839794));
#69438=CARTESIAN_POINT('Ctrl Pts',(79.2595475269933,7.5075766458903,136.003818604241));
#69439=CARTESIAN_POINT('Ctrl Pts',(79.2489418620964,7.51288965071559,136.003022795464));
#69440=CARTESIAN_POINT('Ctrl Pts',(79.2440964610611,7.51534672257244,136.002656809662));
#69441=CARTESIAN_POINT('Ctrl Pts',(79.2328632502145,7.52111225695536,136.001802778125));
#69442=CARTESIAN_POINT('Ctrl Pts',(79.2264847928044,7.52443842255551,136.001313659565));
#69443=CARTESIAN_POINT('Ctrl Pts',(79.2061527485013,7.53520900332105,135.999741598483));
#69444=CARTESIAN_POINT('Ctrl Pts',(79.1922840230788,7.5428105895762,135.998649657017));
#69445=CARTESIAN_POINT('Ctrl Pts',(79.1160927714381,7.58599360479228,135.992549877015));
#69446=CARTESIAN_POINT('Ctrl Pts',(79.056016814999,7.62537285193159,135.987365110413));
#69447=CARTESIAN_POINT('Ctrl Pts',(78.8929628019962,7.74799401685066,135.972532659081));
#69448=CARTESIAN_POINT('Ctrl Pts',(78.7970750631929,7.83981291272444,135.962901499605));
#69449=CARTESIAN_POINT('Ctrl Pts',(78.6958864665773,7.96290092295109,135.951890834227));
#69450=CARTESIAN_POINT('Ctrl Pts',(78.6792313709984,7.98419638691527,135.950042753144));
#69451=CARTESIAN_POINT('Ctrl Pts',(78.6556507015866,8.01590810574452,135.947370770852));
#69452=CARTESIAN_POINT('Ctrl Pts',(78.6483131203581,8.02601104389264,135.946530963027));
#69453=CARTESIAN_POINT('Ctrl Pts',(78.6354302502559,8.04417517413303,135.945040984802));
#69454=CARTESIAN_POINT('Ctrl Pts',(78.6298411583723,8.05220442320869,135.944389155505));
#69455=CARTESIAN_POINT('Ctrl Pts',(78.6182437384799,8.06918219062246,135.943024828332));
#69456=CARTESIAN_POINT('Ctrl Pts',(78.612250854005,8.07814074962577,135.942312934921));
#69457=CARTESIAN_POINT('Ctrl Pts',(78.5965809579962,8.10206427868909,135.940432484722));
#69458=CARTESIAN_POINT('Ctrl Pts',(78.5870562300029,8.11712769340393,135.939269599304));
#69459=CARTESIAN_POINT('Ctrl Pts',(78.5380114395936,8.19751962447847,135.933168598142));
#69460=CARTESIAN_POINT('Ctrl Pts',(78.5027728281628,8.2653584214726,135.92838770591));
#69461=CARTESIAN_POINT('Ctrl Pts',(78.4371865697683,8.41611517413024,135.91825484369));
#69462=CARTESIAN_POINT('Ctrl Pts',(78.408519948634,8.49950227648941,135.912944595744));
#69463=CARTESIAN_POINT('Ctrl Pts',(78.3742897727855,8.63250494513716,135.904457920536));
#69464=CARTESIAN_POINT('Ctrl Pts',(78.3641286570108,8.68076577835562,135.90137319221));
#69465=CARTESIAN_POINT('Ctrl Pts',(78.3529714810313,8.74854529491676,135.896946601538));
#69466=CARTESIAN_POINT('Ctrl Pts',(78.3501550515473,8.7677415701127,135.895682464896));
#69467=CARTESIAN_POINT('Ctrl Pts',(78.3466497920386,8.7949309109591,135.893871644247));
#69468=CARTESIAN_POINT('Ctrl Pts',(78.3456823718366,8.80288729081993,135.893339297453));
#69469=CARTESIAN_POINT('Ctrl Pts',(78.3441430496019,8.81635771375061,135.892433404305));
#69470=CARTESIAN_POINT('Ctrl Pts',(78.3435411760049,8.82186832690684,135.892061506298));
#69471=CARTESIAN_POINT('Ctrl Pts',(78.342438082413,8.83245737806811,135.891344210993));
#69472=CARTESIAN_POINT('Ctrl Pts',(78.3419326783328,8.83753524738031,135.890999078881));
#69473=CARTESIAN_POINT('Ctrl Pts',(78.340884149257,8.84858484071975,135.890245654511));
#69474=CARTESIAN_POINT('Ctrl Pts',(78.3403499229025,8.85455731196778,135.88983689008));
#69475=CARTESIAN_POINT('Ctrl Pts',(78.3391176720687,8.86922540738591,135.888829448641));
#69476=CARTESIAN_POINT('Ctrl Pts',(78.3384556917618,8.87792377279871,135.888228975868));
#69477=CARTESIAN_POINT('Ctrl Pts',(78.3353083420516,8.92406629268983,135.88502886214));
#69478=CARTESIAN_POINT('Ctrl Pts',(78.3340205656214,8.96157809269317,135.88237599935));
#69479=CARTESIAN_POINT('Ctrl Pts',(78.3340002443602,8.99909766519367,135.879690700183));
#69480=CARTESIAN_POINT('Ctrl Pts',(78.3340002456947,8.99909520463398,135.879690876287));
#69481=CARTESIAN_POINT('Ctrl Pts',(78.3339311639518,9.12629542146476,135.870587082321));
#69482=CARTESIAN_POINT('Ctrl Pts',(78.3484291209228,9.25309503966349,135.86118595031));
#69483=CARTESIAN_POINT('Ctrl Pts',(78.3865895332018,9.41734411656879,135.849173887942));
#69484=CARTESIAN_POINT('Ctrl Pts',(78.3974571739415,9.45730340847634,135.846260812617));
#69485=CARTESIAN_POINT('Ctrl Pts',(78.4180656644503,9.52326615740673,135.841471980529));
#69486=CARTESIAN_POINT('Ctrl Pts',(78.4269871736021,9.54950385642816,135.83957241518));
#69487=CARTESIAN_POINT('Ctrl Pts',(78.4365593737294,9.5755079566144,135.837694135948));
#69488=CARTESIAN_POINT('',(78.3340003883633,8.99886244719965,136.072462051176));
#69489=CARTESIAN_POINT('Ctrl Pts',(78.4365593745323,9.57550795879571,136.032852165095));
#69490=CARTESIAN_POINT('Ctrl Pts',(78.4356277148595,9.57297698670518,136.033046285279));
#69491=CARTESIAN_POINT('Ctrl Pts',(78.4347021561404,9.57044363022435,136.03324030345));
#69492=CARTESIAN_POINT('Ctrl Pts',(78.4095803158231,9.50116081178708,136.038538509474));
#69493=CARTESIAN_POINT('Ctrl Pts',(78.3896669089255,9.43292796125389,136.043552730623));
#69494=CARTESIAN_POINT('Ctrl Pts',(78.3698143382183,9.34416329481746,136.049800240416));
#69495=CARTESIAN_POINT('Ctrl Pts',(78.365811465529,9.32462525924818,136.051159038004));
#69496=CARTESIAN_POINT('Ctrl Pts',(78.3598903716904,9.29283119587528,136.053344580382));
#69497=CARTESIAN_POINT('Ctrl Pts',(78.3577566142742,9.28061785155142,136.054178056609));
#69498=CARTESIAN_POINT('Ctrl Pts',(78.3541893803237,9.25876317691845,136.055658992162));
#69499=CARTESIAN_POINT('Ctrl Pts',(78.3527038212801,9.24913105802732,136.056308069511));
#69500=CARTESIAN_POINT('Ctrl Pts',(78.3499924352749,9.23046504336666,136.057559132773));
#69501=CARTESIAN_POINT('Ctrl Pts',(78.3487560728268,9.22143305627928,136.058161428655));
#69502=CARTESIAN_POINT('Ctrl Pts',(78.3462230634299,9.20172621449645,136.059469152917));
#69503=CARTESIAN_POINT('Ctrl Pts',(78.344955499794,9.19104798557724,136.060173652948));
#69504=CARTESIAN_POINT('Ctrl Pts',(78.3412526870132,9.15704544821936,136.0624046368));
#69505=CARTESIAN_POINT('Ctrl Pts',(78.33920639662,9.13368101662976,136.063919147197));
#69506=CARTESIAN_POINT('Ctrl Pts',(78.3351936433969,9.07319343063213,136.067799234268));
#69507=CARTESIAN_POINT('Ctrl Pts',(78.3339750077718,9.03603351786301,136.070143150966));
#69508=CARTESIAN_POINT('Ctrl Pts',(78.3340003883633,8.99886244719965,136.072462051176));
#69509=CARTESIAN_POINT('Ctrl Pts',(78.3340003869984,8.99886444785471,136.072461926366));
#69510=CARTESIAN_POINT('Ctrl Pts',(78.3340531441327,8.92146301309155,136.077290581301));
#69511=CARTESIAN_POINT('Ctrl Pts',(78.3394999121662,8.84415419702371,136.081997861543));
#69512=CARTESIAN_POINT('Ctrl Pts',(78.3596031876968,8.70151152241477,136.090799621358));
#69513=CARTESIAN_POINT('Ctrl Pts',(78.3728537644019,8.63614436901105,136.0948817902));
#69514=CARTESIAN_POINT('Ctrl Pts',(78.395771922399,8.54998256302621,136.100524008562));
#69515=CARTESIAN_POINT('Ctrl Pts',(78.4020028876724,8.52833428565311,136.101964483626));
#69516=CARTESIAN_POINT('Ctrl Pts',(78.4134188217244,8.49149881699858,136.104465329264));
#69517=CARTESIAN_POINT('Ctrl Pts',(78.4183879553125,8.47624759472493,136.105515622285));
#69518=CARTESIAN_POINT('Ctrl Pts',(78.4259160897696,8.45422700585422,136.107056986682));
#69519=CARTESIAN_POINT('Ctrl Pts',(78.4283003909941,8.44739828827664,136.10753847939));
#69520=CARTESIAN_POINT('Ctrl Pts',(78.4325542090003,8.43546546783966,136.108386377101));
#69521=CARTESIAN_POINT('Ctrl Pts',(78.4344043529058,8.43035465917388,136.108751647994));
#69522=CARTESIAN_POINT('Ctrl Pts',(78.438487381553,8.41924592080844,136.109550308729));
#69523=CARTESIAN_POINT('Ctrl Pts',(78.4407297901262,8.41325187071367,136.109984226704));
#69524=CARTESIAN_POINT('Ctrl Pts',(78.4470829225921,8.39656332434912,136.111200364459));
#69525=CARTESIAN_POINT('Ctrl Pts',(78.4512694246017,8.385898332915,136.111986793306));
#69526=CARTESIAN_POINT('Ctrl Pts',(78.4799752666411,8.31493192506949,136.117277844626));
#69527=CARTESIAN_POINT('Ctrl Pts',(78.507898388204,8.25607503662913,136.121945620769));
#69528=CARTESIAN_POINT('Ctrl Pts',(78.5496654896484,8.17990204110557,136.128241573454));
#69529=CARTESIAN_POINT('Ctrl Pts',(78.5605161495456,8.16100233712507,136.129825995778));
#69530=CARTESIAN_POINT('Ctrl Pts',(78.607265245597,8.08315253400646,136.136434473902));
#69531=CARTESIAN_POINT('Ctrl Pts',(78.64644051915,8.02624589460323,136.141461378754));
#69532=CARTESIAN_POINT('Ctrl Pts',(78.7180407219012,7.93494324859615,136.14976933578));
#69533=CARTESIAN_POINT('Ctrl Pts',(78.748601331274,7.89919687992975,136.153093131371));
#69534=CARTESIAN_POINT('Ctrl Pts',(78.7957310356929,7.84857346821893,136.157900575771));
#69535=CARTESIAN_POINT('Ctrl Pts',(78.8111492200505,7.83266084637885,136.159427611635));
#69536=CARTESIAN_POINT('Ctrl Pts',(78.8396995303685,7.80434756730253,136.162174621035));
#69537=CARTESIAN_POINT('Ctrl Pts',(78.8527244032876,7.79184410387257,136.163398921305));
#69538=CARTESIAN_POINT('Ctrl Pts',(78.8736862199784,7.7723661856787,136.165324871146));
#69539=CARTESIAN_POINT('Ctrl Pts',(78.8814903602932,7.76525156088244,136.166032473925));
#69540=CARTESIAN_POINT('Ctrl Pts',(78.8966095250413,7.75172919220106,136.167385612255));
#69541=CARTESIAN_POINT('Ctrl Pts',(78.9039140122308,7.74531037140608,136.168031596976));
#69542=CARTESIAN_POINT('Ctrl Pts',(78.9204810008802,7.73100722187497,136.169479679248));
#69543=CARTESIAN_POINT('Ctrl Pts',(78.9297745554825,7.72315958264297,136.170280246122));
#69544=CARTESIAN_POINT('Ctrl Pts',(78.957486111298,7.70027461065848,136.172633779232));
#69545=CARTESIAN_POINT('Ctrl Pts',(78.976141478408,7.68552857954004,136.174175075683));
#69546=CARTESIAN_POINT('Ctrl Pts',(79.0768085212832,7.60940081325571,136.182281295892));
#69547=CARTESIAN_POINT('Ctrl Pts',(79.1640373786691,7.55527912932194,136.188562885749));
#69548=CARTESIAN_POINT('Ctrl Pts',(79.3266333773447,7.47408365318616,136.199662664586));
#69549=CARTESIAN_POINT('Ctrl Pts',(79.4000062528873,7.44377088487217,136.204482058647));
#69550=CARTESIAN_POINT('Ctrl Pts',(79.4987636390716,7.41099661009946,136.211042980748));
#69551=CARTESIAN_POINT('Ctrl Pts',(79.5224448305711,7.40371976366654,136.212621982234));
#69552=CARTESIAN_POINT('Ctrl Pts',(79.5628446199963,7.3922849728829,136.215339150357));
#69553=CARTESIAN_POINT('Ctrl Pts',(79.5794819977325,7.38785329831413,136.216464767613));
#69554=CARTESIAN_POINT('Ctrl Pts',(79.6034016650233,7.3818772904637,136.21809649978));
#69555=CARTESIAN_POINT('Ctrl Pts',(79.6106308998602,7.38012252283014,136.218591401636));
#69556=CARTESIAN_POINT('Ctrl Pts',(79.6232325458451,7.37715292691006,136.219457509455));
#69557=CARTESIAN_POINT('Ctrl Pts',(79.6285996162931,7.37591623026215,136.219827471938));
#69558=CARTESIAN_POINT('Ctrl Pts',(79.6401136592124,7.37332319018451,136.220623602186));
#69559=CARTESIAN_POINT('Ctrl Pts',(79.64626211335,7.3719750843008,136.221050190894));
#69560=CARTESIAN_POINT('Ctrl Pts',(79.663165244482,7.36836918738495,136.222226678532));
#69561=CARTESIAN_POINT('Ctrl Pts',(79.6739346251001,7.36618296116407,136.222980374254));
#69562=CARTESIAN_POINT('Ctrl Pts',(79.7352883383868,7.35435866547006,136.227294660842));
#69563=CARTESIAN_POINT('Ctrl Pts',(79.786271870605,7.34696434852525,136.230957803344));
#69564=CARTESIAN_POINT('Ctrl Pts',(79.9330610803652,7.33257898529598,136.241586302096));
#69565=CARTESIAN_POINT('Ctrl Pts',(80.0292434301914,7.33149182043701,136.248638173744));
#69566=CARTESIAN_POINT('Ctrl Pts',(80.1774362924461,7.3426409991384,136.259325602428));
#69567=CARTESIAN_POINT('Ctrl Pts',(80.2296730923483,7.34906885175078,136.263061157461));
#69568=CARTESIAN_POINT('Ctrl Pts',(80.3050186510509,7.36198659414462,136.268388875245));
#69569=CARTESIAN_POINT('Ctrl Pts',(80.328426569488,7.36651893711743,136.27003570082));
#69570=CARTESIAN_POINT('Ctrl Pts',(80.3706981806889,7.37564922888482,136.272994956971));
#69571=CARTESIAN_POINT('Ctrl Pts',(80.3895937887019,7.38007737720623,136.274312381842));
#69572=CARTESIAN_POINT('Ctrl Pts',(80.41918371063,7.38755944389731,136.276367762707));
#69573=CARTESIAN_POINT('Ctrl Pts',(80.4299316748906,7.39039188138417,136.277112740561));
#69574=CARTESIAN_POINT('Ctrl Pts',(80.4500249318149,7.39590273153883,136.278502741974));
#69575=CARTESIAN_POINT('Ctrl Pts',(80.4593766296121,7.39855577526023,136.279148552641));
#69576=CARTESIAN_POINT('Ctrl Pts',(80.4803371515214,7.40470091698071,136.280593802181));
#69577=CARTESIAN_POINT('Ctrl Pts',(80.4919322395702,7.40823819996467,136.281391736597));
#69578=CARTESIAN_POINT('Ctrl Pts',(80.5259619131412,7.41902690972052,136.283729754519));
#69579=CARTESIAN_POINT('Ctrl Pts',(80.5482829454949,7.42662854120583,136.2852584028));
#69580=CARTESIAN_POINT('Ctrl Pts',(80.6684827181651,7.4704325131571,136.29347727327));
#69581=CARTESIAN_POINT('Ctrl Pts',(80.7629594290216,7.5152972863955,136.299871275994));
#69582=CARTESIAN_POINT('Ctrl Pts',(80.919683081142,7.60865842096054,136.311011723616));
#69583=CARTESIAN_POINT('Ctrl Pts',(80.983845328925,7.65326505081037,136.315759181713));
#69584=CARTESIAN_POINT('Ctrl Pts',(81.0637776959932,7.71760514161585,136.322231150989));
#69585=CARTESIAN_POINT('Ctrl Pts',(81.082571443264,7.73343041943481,136.323797549425));
#69586=CARTESIAN_POINT('Ctrl Pts',(81.1138497761565,7.76097316930884,136.326495129723));
#69587=CARTESIAN_POINT('Ctrl Pts',(81.1265165492664,7.77247842400972,136.327613998469));
#69588=CARTESIAN_POINT('Ctrl Pts',(81.1444191234065,7.7892498425877,136.329237654458));
#69589=CARTESIAN_POINT('Ctrl Pts',(81.1498008982252,7.79435952169334,136.32973138014));
#69590=CARTESIAN_POINT('Ctrl Pts',(81.1591155133244,7.80332229114611,136.330596162431));
#69591=CARTESIAN_POINT('Ctrl Pts',(81.1630636771064,7.80715919164722,136.330965987508));
#69592=CARTESIAN_POINT('Ctrl Pts',(81.1714924574114,7.81543207327504,136.331762685419));
#69593=CARTESIAN_POINT('Ctrl Pts',(81.1759668595373,7.81987386573971,136.332189986815));
#69594=CARTESIAN_POINT('Ctrl Pts',(81.188202586242,7.83215909805313,136.333370311814));
#69595=CARTESIAN_POINT('Ctrl Pts',(81.1959112004824,7.84005425019851,136.334127171301));
#69596=CARTESIAN_POINT('Ctrl Pts',(81.2397026746054,7.88580595563019,136.338500511347));
#69597=CARTESIAN_POINT('Ctrl Pts',(81.2740621717922,7.92526489625351,136.342222723922));
#69598=CARTESIAN_POINT('Ctrl Pts',(81.36972325798,8.0461685123325,136.353337187766));
#69599=CARTESIAN_POINT('Ctrl Pts',(81.4254825206518,8.13170417319068,136.360825746992));
#69600=CARTESIAN_POINT('Ctrl Pts',(81.5071779949745,8.28634739173715,136.373364231176));
#69601=CARTESIAN_POINT('Ctrl Pts',(81.5370027634574,8.35307596322642,136.378494736779));
#69602=CARTESIAN_POINT('Ctrl Pts',(81.5684768422049,8.4380861890499,136.384681139292));
#69603=CARTESIAN_POINT('Ctrl Pts',(81.5743347196586,8.45471386648205,136.385875480287));
#69604=CARTESIAN_POINT('Ctrl Pts',(81.5833335102568,8.48161189689634,136.387783095859));
#69605=CARTESIAN_POINT('Ctrl Pts',(81.5866408293228,8.49182471705531,136.388501796782));
#69606=CARTESIAN_POINT('Ctrl Pts',(81.5927754208663,8.51141192076544,136.389869791718));
#69607=CARTESIAN_POINT('Ctrl Pts',(81.5956192040493,8.52078061898938,136.390519601639));
#69608=CARTESIAN_POINT('Ctrl Pts',(81.6019224727224,8.5422247721688,136.391996975092));
#69609=CARTESIAN_POINT('Ctrl Pts',(81.6053283402842,8.5543154679845,136.392822769176));
#69610=CARTESIAN_POINT('Ctrl Pts',(81.614056014618,8.5866972282222,136.395016168822));
#69611=CARTESIAN_POINT('Ctrl Pts',(81.6191319958297,8.60705262120181,136.396375904976));
#69612=CARTESIAN_POINT('Ctrl Pts',(81.6509426179813,8.74572292910676,136.405522797681));
#69613=CARTESIAN_POINT('Ctrl Pts',(81.6650720831742,8.86655650291308,136.41288809779));
#69614=CARTESIAN_POINT('Ctrl Pts',(81.6664361104077,9.05379667937085,136.424330348604));
#69615=CARTESIAN_POINT('Ctrl Pts',(81.6630018453198,9.11969544808851,136.428371150736));
#69616=CARTESIAN_POINT('Ctrl Pts',(81.6531837064261,9.20746310136646,136.433961334851));
#69617=CARTESIAN_POINT('Ctrl Pts',(81.6502464055033,9.22966063418458,136.435393396896));
#69618=CARTESIAN_POINT('Ctrl Pts',(81.6444495977984,9.26757518884687,136.437881030727));
#69619=CARTESIAN_POINT('Ctrl Pts',(81.6418096589256,9.28332306541428,136.438926666206));
#69620=CARTESIAN_POINT('Ctrl Pts',(81.6376479925338,9.30613262049103,136.44046242638));
#69621=CARTESIAN_POINT('Ctrl Pts',(81.6363059433073,9.31322672916653,136.440943069394));
#69622=CARTESIAN_POINT('Ctrl Pts',(81.633873045942,9.32564459283121,136.441790030242));
#69623=CARTESIAN_POINT('Ctrl Pts',(81.6328021976409,9.33097207322808,136.44215522256));
#69624=CARTESIAN_POINT('Ctrl Pts',(81.6304116884145,9.34257086014009,136.442954395602));
#69625=CARTESIAN_POINT('Ctrl Pts',(81.6290819233892,9.34883972159588,136.44338891069));
#69626=CARTESIAN_POINT('Ctrl Pts',(81.6252657802977,9.36633222086151,136.444608298));
#69627=CARTESIAN_POINT('Ctrl Pts',(81.6226994066407,9.37753777297932,136.445397413902));
#69628=CARTESIAN_POINT('Ctrl Pts',(81.6044757219645,9.45348711802887,136.450796223447));
#69629=CARTESIAN_POINT('Ctrl Pts',(81.5850651386949,9.51726147192289,136.455576621685));
#69630=CARTESIAN_POINT('Ctrl Pts',(81.5543651901998,9.59997740745913,136.461973961768));
#69631=CARTESIAN_POINT('Ctrl Pts',(81.5464431899345,9.62011085810467,136.463547373611));
#69632=CARTESIAN_POINT('Ctrl Pts',(81.5104525822664,9.70659681239344,136.470365206775));
#69633=CARTESIAN_POINT('Ctrl Pts',(81.4784869358484,9.77124809500272,136.475609756227));
#69634=CARTESIAN_POINT('Ctrl Pts',(81.4090013952113,9.89147934437659,136.485530128629));
#69635=CARTESIAN_POINT('Ctrl Pts',(81.3721150591305,9.94727117582283,136.490211221038));
#69636=CARTESIAN_POINT('Ctrl Pts',(81.3216223477074,10.0144788123303,136.495944434571));
#69637=CARTESIAN_POINT('Ctrl Pts',(81.3110592185517,10.0280936994288,136.497111309044));
#69638=CARTESIAN_POINT('Ctrl Pts',(81.2936287115666,10.0498543541593,136.498985887513));
#69639=CARTESIAN_POINT('Ctrl Pts',(81.2868913353451,10.0581021257214,136.499698684046));
#69640=CARTESIAN_POINT('Ctrl Pts',(81.273792821711,10.0738268935684,136.501062356521));
#69641=CARTESIAN_POINT('Ctrl Pts',(81.2674437998601,10.0813133547781,136.501713683256));
#69642=CARTESIAN_POINT('Ctrl Pts',(81.2527042578371,10.0983853185433,136.503204087334));
#69643=CARTESIAN_POINT('Ctrl Pts',(81.2442691547377,10.1079316545407,136.504041282955));
#69644=CARTESIAN_POINT('Ctrl Pts',(81.2166216463029,10.138507382077,136.506736170426));
#69645=CARTESIAN_POINT('Ctrl Pts',(81.1969786102493,10.159141773007,136.508575749744));
#69646=CARTESIAN_POINT('Ctrl Pts',(81.0842992880271,10.271587167455,136.518746647065));
#69647=CARTESIAN_POINT('Ctrl Pts',(80.9812427320881,10.3527024702783,136.52660468837));
#69648=CARTESIAN_POINT('Ctrl Pts',(80.8089796364339,10.4581447509026,136.538997006382));
#69649=CARTESIAN_POINT('Ctrl Pts',(80.745882777515,10.491405619886,136.54341493937));
#69650=CARTESIAN_POINT('Ctrl Pts',(80.6664719944726,10.5269641682872,136.549060224161));
#69651=CARTESIAN_POINT('Ctrl Pts',(80.6519948407415,10.5332016090782,136.550092792081));
#69652=CARTESIAN_POINT('Ctrl Pts',(80.6307954172729,10.5419807844289,136.551612818145));
#69653=CARTESIAN_POINT('Ctrl Pts',(80.6241412643118,10.5446861414027,136.552091064196));
#69654=CARTESIAN_POINT('Ctrl Pts',(80.6124261410438,10.5493610661181,136.552935392305));
#69655=CARTESIAN_POINT('Ctrl Pts',(80.607372724284,10.5513490464612,136.553300373097));
#69656=CARTESIAN_POINT('Ctrl Pts',(80.5963115518121,10.555638106521,136.554101036828));
#69657=CARTESIAN_POINT('Ctrl Pts',(80.5903002527089,10.5579290720182,136.554537272025));
#69658=CARTESIAN_POINT('Ctrl Pts',(80.5734064698385,10.5642556490202,136.555766037709));
#69659=CARTESIAN_POINT('Ctrl Pts',(80.5624951096833,10.5682123414605,136.556562912473));
#69660=CARTESIAN_POINT('Ctrl Pts',(80.4788922277897,10.5975437926729,136.562688499604));
#69661=CARTESIAN_POINT('Ctrl Pts',(80.4045691098785,10.6179632513618,136.568244476519));
#69662=CARTESIAN_POINT('Ctrl Pts',(80.2729626348254,10.644484111067,136.578002871392));
#69663=CARTESIAN_POINT('Ctrl Pts',(80.216267404747,10.6528960245061,136.582182529251));
#69664=CARTESIAN_POINT('Ctrl Pts',(80.0769170039275,10.6662776354405,136.592298421443));
#69665=CARTESIAN_POINT('Ctrl Pts',(79.994098936278,10.6680426113408,136.598172072534));
#69666=CARTESIAN_POINT('Ctrl Pts',(79.8886810548849,10.662433584049,136.605429609091));
#69667=CARTESIAN_POINT('Ctrl Pts',(79.8659071031743,10.6607517917005,136.606985022737));
#69668=CARTESIAN_POINT('Ctrl Pts',(79.8314054840249,10.6574895544519,136.609323585377));
#69669=CARTESIAN_POINT('Ctrl Pts',(79.8196489842142,10.6562515683095,136.610117312495));
#69670=CARTESIAN_POINT('Ctrl Pts',(79.7992030873229,10.6538782808652,136.611492509951));
#69671=CARTESIAN_POINT('Ctrl Pts',(79.7905077515289,10.6527993740684,136.612075724195));
#69672=CARTESIAN_POINT('Ctrl Pts',(79.770916709222,10.6502114496122,136.613386231962));
#69673=CARTESIAN_POINT('Ctrl Pts',(79.7600265500876,10.6486630145815,136.614112257789));
#69674=CARTESIAN_POINT('Ctrl Pts',(79.7305036901016,10.6441665295293,136.616074359909));
#69675=CARTESIAN_POINT('Ctrl Pts',(79.7119040793561,10.6410096359875,136.617303832634));
#69676=CARTESIAN_POINT('Ctrl Pts',(79.5960403487304,10.6193134693007,136.624928541129));
#69677=CARTESIAN_POINT('Ctrl Pts',(79.5005320938761,10.5924493635285,136.631046890396));
#69678=CARTESIAN_POINT('Ctrl Pts',(79.3412551908745,10.5318957765152,136.641470337049));
#69679=CARTESIAN_POINT('Ctrl Pts',(79.2762465790241,10.5022748303543,136.645798286387));
#69680=CARTESIAN_POINT('Ctrl Pts',(79.1806609743707,10.4510733646507,136.652530398233));
#69681=CARTESIAN_POINT('Ctrl Pts',(79.1485772869746,10.4324836322335,136.654858373179));
#69682=CARTESIAN_POINT('Ctrl Pts',(79.1038484739672,10.4045334396655,136.658240769282));
#69683=CARTESIAN_POINT('Ctrl Pts',(79.0906728703663,10.3960393524008,136.659254690725));
#69684=CARTESIAN_POINT('Ctrl Pts',(79.0674902914687,10.3806265241495,136.661073882843));
#69685=CARTESIAN_POINT('Ctrl Pts',(79.0574353909328,10.3737816028056,136.661874958807));
#69686=CARTESIAN_POINT('Ctrl Pts',(79.0421399378135,10.3631221875605,136.663113642967));
#69687=CARTESIAN_POINT('Ctrl Pts',(79.0368449483351,10.3593860157656,136.663546201151));
#69688=CARTESIAN_POINT('Ctrl Pts',(79.027115580287,10.3524355440393,136.664348231931));
#69689=CARTESIAN_POINT('Ctrl Pts',(79.0226750903932,10.3492301556437,136.664717108332));
#69690=CARTESIAN_POINT('Ctrl Pts',(79.0125730778852,10.3418619357556,136.665562738655));
#69691=CARTESIAN_POINT('Ctrl Pts',(79.0069220354718,10.3376851397204,136.666040423824));
#69692=CARTESIAN_POINT('Ctrl Pts',(78.9890335633866,10.324287597794,136.667566932692));
#69693=CARTESIAN_POINT('Ctrl Pts',(78.9768972461405,10.3149340253902,136.668624191239));
#69694=CARTESIAN_POINT('Ctrl Pts',(78.8854012954304,10.2423837757863,136.676750572399));
#69695=CARTESIAN_POINT('Ctrl Pts',(78.8118406528033,10.1722293634422,136.684175373678));
#69696=CARTESIAN_POINT('Ctrl Pts',(78.6690376031109,10.0086999071987,136.699966323611));
#69697=CARTESIAN_POINT('Ctrl Pts',(78.6022200081783,9.91386921074871,136.708264360951));
#69698=CARTESIAN_POINT('Ctrl Pts',(78.5362713505037,9.79588488873858,136.717513992661));
#69699=CARTESIAN_POINT('Ctrl Pts',(78.527079001614,9.77874135861699,136.718834533187));
#69700=CARTESIAN_POINT('Ctrl Pts',(78.5131044699187,9.75154602302515,136.720893645411));
#69701=CARTESIAN_POINT('Ctrl Pts',(78.5081194252236,9.74160104038382,136.721639281496));
#69702=CARTESIAN_POINT('Ctrl Pts',(78.4989661081055,9.72287462326264,136.723029879778));
#69703=CARTESIAN_POINT('Ctrl Pts',(78.4947743800461,9.71410524816181,136.723675635595));
#69704=CARTESIAN_POINT('Ctrl Pts',(78.4855334627877,9.69432969248777,136.72511995042));
#69705=CARTESIAN_POINT('Ctrl Pts',(78.4805270036655,9.68330406155704,136.725917013648));
#69706=CARTESIAN_POINT('Ctrl Pts',(78.4661546710695,9.65071287997985,136.72824990872));
#69707=CARTESIAN_POINT('Ctrl Pts',(78.45712432468,9.62900197491221,136.729774382256));
#69708=CARTESIAN_POINT('Ctrl Pts',(78.4444496037559,9.59661206619143,136.732009064827));
#69709=CARTESIAN_POINT('Ctrl Pts',(78.4404505189736,9.58607874726763,136.732729698797));
#69710=CARTESIAN_POINT('Ctrl Pts',(78.436559386885,9.57550799235334,136.733447166179));
#69711=CARTESIAN_POINT('Origin',(80.,9.,134.));
#69712=CARTESIAN_POINT('',(78.4365593900224,9.5755080008764,137.430947520545));
#69713=CARTESIAN_POINT('',(78.4365593610394,9.57550792214055,137.240217191853));
#69714=CARTESIAN_POINT('',(78.4365593737638,9.57550795670799,134.));
#69715=CARTESIAN_POINT('Ctrl Pts',(78.4365593610394,9.57550792214055,137.240217191853));
#69716=CARTESIAN_POINT('Ctrl Pts',(78.4441567507286,9.59614719978225,137.238854438564));
#69717=CARTESIAN_POINT('Ctrl Pts',(78.452164058202,9.61663935851914,137.23748249975));
#69718=CARTESIAN_POINT('Ctrl Pts',(78.4751003999289,9.67207150003121,137.233704427405));
#69719=CARTESIAN_POINT('Ctrl Pts',(78.4908185278503,9.70666093137332,137.231273238148));
#69720=CARTESIAN_POINT('Ctrl Pts',(78.5121018738559,9.7495418921171,137.228128061239));
#69721=CARTESIAN_POINT('Ctrl Pts',(78.5165791146514,9.75836425742755,137.227473783099));
#69722=CARTESIAN_POINT('Ctrl Pts',(78.5238939653149,9.77246545940252,137.22641558442));
#69723=CARTESIAN_POINT('Ctrl Pts',(78.5266820284786,9.77776992970115,137.226014665493));
#69724=CARTESIAN_POINT('Ctrl Pts',(78.5321095974894,9.78796232448249,137.225238569216));
#69725=CARTESIAN_POINT('Ctrl Pts',(78.5347450217788,9.79285225846006,137.224863642427));
#69726=CARTESIAN_POINT('Ctrl Pts',(78.5412736012842,9.80482207728492,137.223939667203));
#69727=CARTESIAN_POINT('Ctrl Pts',(78.5451938711188,9.8118869398309,137.223388953042));
#69728=CARTESIAN_POINT('Ctrl Pts',(78.558908288206,9.83618392116839,137.221477110259));
#69729=CARTESIAN_POINT('Ctrl Pts',(78.5689580529981,9.85326885122324,137.220101504471));
#69730=CARTESIAN_POINT('Ctrl Pts',(78.6358228215016,9.96243624264813,137.211127292575));
#69731=CARTESIAN_POINT('Ctrl Pts',(78.7011862165201,10.0489724589298,137.203171911928));
#69732=CARTESIAN_POINT('Ctrl Pts',(78.8422075956884,10.2021111029538,137.188068368296));
#69733=CARTESIAN_POINT('Ctrl Pts',(78.9164366201114,10.2694293964965,137.180934778744));
#69734=CARTESIAN_POINT('Ctrl Pts',(79.0126836258733,10.3420824796925,137.172669483643));
#69735=CARTESIAN_POINT('Ctrl Pts',(79.029327568455,10.3541691553361,137.17127149212));
#69736=CARTESIAN_POINT('Ctrl Pts',(79.053897604199,10.3713258513728,137.169251906349));
#69737=CARTESIAN_POINT('Ctrl Pts',(79.0616490111354,10.3766414790926,137.168621001937));
#69738=CARTESIAN_POINT('Ctrl Pts',(79.0773649264363,10.3872244542846,137.167354179846));
#69739=CARTESIAN_POINT('Ctrl Pts',(79.0853305657053,10.3924894965559,137.166718365568));
#69740=CARTESIAN_POINT('Ctrl Pts',(79.1025455082022,10.4036565835148,137.165357454539));
#69741=CARTESIAN_POINT('Ctrl Pts',(79.1118087782443,10.4095363537644,137.16463320721));
#69742=CARTESIAN_POINT('Ctrl Pts',(79.1370363126506,10.4252018319677,137.162681922915));
#69743=CARTESIAN_POINT('Ctrl Pts',(79.1531088633351,10.4348108015295,137.161461360357));
#69744=CARTESIAN_POINT('Ctrl Pts',(79.255317963956,10.4936004893069,137.153832918091));
#69745=CARTESIAN_POINT('Ctrl Pts',(79.3455445039721,10.5352802477523,137.147703388719));
#69746=CARTESIAN_POINT('Ctrl Pts',(79.5059607040737,10.5926535732133,137.137281713342));
#69747=CARTESIAN_POINT('Ctrl Pts',(79.5744316013533,10.6122999311012,137.132966095825));
#69748=CARTESIAN_POINT('Ctrl Pts',(79.6803413395232,10.6354700730709,137.126236506467));
#69749=CARTESIAN_POINT('Ctrl Pts',(79.7169912342135,10.6422087862814,137.123897445164));
#69750=CARTESIAN_POINT('Ctrl Pts',(79.7693891997842,10.6500369799307,137.120500313191));
#69751=CARTESIAN_POINT('Ctrl Pts',(79.7849762807276,10.6521404714815,137.119483123625));
#69752=CARTESIAN_POINT('Ctrl Pts',(79.8126981119374,10.6554826291982,137.117658570102));
#69753=CARTESIAN_POINT('Ctrl Pts',(79.8248212730772,10.6568093206845,137.116855435411));
#69754=CARTESIAN_POINT('Ctrl Pts',(79.8434145542836,10.6586377227587,137.115614156822));
#69755=CARTESIAN_POINT('Ctrl Pts',(79.8498751598587,10.6592349520136,137.115181094226));
#69756=CARTESIAN_POINT('Ctrl Pts',(79.8617961764518,10.660266757952,137.114378503731));
#69757=CARTESIAN_POINT('Ctrl Pts',(79.867255441798,10.6607121615801,137.114009576577));
#69758=CARTESIAN_POINT('Ctrl Pts',(79.879717665427,10.6616670725899,137.113164293621));
#69759=CARTESIAN_POINT('Ctrl Pts',(79.8867217125316,10.6621592358291,137.112687011154));
#69760=CARTESIAN_POINT('Ctrl Pts',(79.9089820012279,10.6635820820643,137.111163518315));
#69761=CARTESIAN_POINT('Ctrl Pts',(79.9242475335512,10.6643470618944,137.11010892025));
#69762=CARTESIAN_POINT('Ctrl Pts',(80.0412447323588,10.668597104661,137.10196180995));
#69763=CARTESIAN_POINT('Ctrl Pts',(80.1430844532501,10.6629614691322,137.09451097101));
#69764=CARTESIAN_POINT('Ctrl Pts',(80.3581200602769,10.631155894574,137.07870094813));
#69765=CARTESIAN_POINT('Ctrl Pts',(80.470425302254,10.6023822883109,137.070409584079));
#69766=CARTESIAN_POINT('Ctrl Pts',(80.5969898265088,10.5554847758582,137.061174597286));
#69767=CARTESIAN_POINT('Ctrl Pts',(80.6150000626136,10.5484523623587,137.059862232195));
#69768=CARTESIAN_POINT('Ctrl Pts',(80.6431531455503,10.5368907768096,137.057812784356));
#69769=CARTESIAN_POINT('Ctrl Pts',(80.6533796047633,10.5325711503486,137.057068749769));
#69770=CARTESIAN_POINT('Ctrl Pts',(80.6724826551113,10.5242761081943,137.055679401051));
#69771=CARTESIAN_POINT('Ctrl Pts',(80.6813690377307,10.5203245761071,137.055033310805));
#69772=CARTESIAN_POINT('Ctrl Pts',(80.7012782375894,10.5112618713821,137.053585999822));
#69773=CARTESIAN_POINT('Ctrl Pts',(80.7122808458653,10.5061074397518,137.052786299797));
#69774=CARTESIAN_POINT('Ctrl Pts',(80.7445770879048,10.4905444205572,137.050438512168));
#69775=CARTESIAN_POINT('Ctrl Pts',(80.7657066730077,10.4798010309386,137.048902004));
#69776=CARTESIAN_POINT('Ctrl Pts',(80.8741629807096,10.4217108576275,137.040999131004));
#69777=CARTESIAN_POINT('Ctrl Pts',(80.95735954906,10.3670729803495,137.034897172586));
#69778=CARTESIAN_POINT('Ctrl Pts',(81.0992953801532,10.254510936634,137.023830527725));
#69779=CARTESIAN_POINT('Ctrl Pts',(81.1595555584995,10.1990317287867,137.01886543544));
#69780=CARTESIAN_POINT('Ctrl Pts',(81.2327128834758,10.1209857011942,137.012124713097));
#69781=CARTESIAN_POINT('Ctrl Pts',(81.249513077078,10.1022281660943,137.010520676842));
#69782=CARTESIAN_POINT('Ctrl Pts',(81.2772104621868,10.0698565956479,137.00776459678));
#69783=CARTESIAN_POINT('Ctrl Pts',(81.2883310684674,10.0564386869723,137.00662557701));
#69784=CARTESIAN_POINT('Ctrl Pts',(81.3039183880279,10.0370191561546,137.004977737447));
#69785=CARTESIAN_POINT('Ctrl Pts',(81.3085587520806,10.0311575436909,137.004480433655));
#69786=CARTESIAN_POINT('Ctrl Pts',(81.3165527052162,10.020918889011,137.003611524914));
#69787=CARTESIAN_POINT('Ctrl Pts',(81.3199242697735,10.0165561099329,137.003241187156));
#69788=CARTESIAN_POINT('Ctrl Pts',(81.3270879085903,10.0071906900113,137.002445881928));
#69789=CARTESIAN_POINT('Ctrl Pts',(81.3308733237961,10.0021834143096,137.002020507632));
#69790=CARTESIAN_POINT('Ctrl Pts',(81.3411588937267,9.98841681493098,137.000850854266));
#69791=CARTESIAN_POINT('Ctrl Pts',(81.3476013271066,9.97961503953268,137.000102848898));
#69792=CARTESIAN_POINT('Ctrl Pts',(81.3829464792416,9.93031732360164,136.995915217375));
#69793=CARTESIAN_POINT('Ctrl Pts',(81.4101077302643,9.8886092939543,136.99237983895));
#69794=CARTESIAN_POINT('Ctrl Pts',(81.4861778279224,9.75950789100241,136.98159180925));
#69795=CARTESIAN_POINT('Ctrl Pts',(81.5291201290991,9.66885700191761,136.974233533431));
#69796=CARTESIAN_POINT('Ctrl Pts',(81.5902754412872,9.50252003513767,136.961501041081));
#69797=CARTESIAN_POINT('Ctrl Pts',(81.6118311849855,9.42837563872173,136.956070830108));
#69798=CARTESIAN_POINT('Ctrl Pts',(81.6319586796834,9.33553822559325,136.949585577354));
#69799=CARTESIAN_POINT('Ctrl Pts',(81.6354623509377,9.31802197222772,136.948375063007));
#69800=CARTESIAN_POINT('Ctrl Pts',(81.6406290638025,9.2898424152369,136.946447872807));
#69801=CARTESIAN_POINT('Ctrl Pts',(81.6424713083734,9.27921382720119,136.945725571437));
#69802=CARTESIAN_POINT('Ctrl Pts',(81.64578689093,9.25891536543541,136.944354584762));
#69803=CARTESIAN_POINT('Ctrl Pts',(81.6472785455074,9.2492489865344,136.943705346627));
#69804=CARTESIAN_POINT('Ctrl Pts',(81.6504780457373,9.22723048957915,136.942234475678));
#69805=CARTESIAN_POINT('Ctrl Pts',(81.652132528817,9.21487111519411,136.94141455346));
#69806=CARTESIAN_POINT('Ctrl Pts',(81.656922081295,9.17575769578835,136.938836791272));
#69807=CARTESIAN_POINT('Ctrl Pts',(81.6595472699879,9.14894475857101,136.937094871233));
#69808=CARTESIAN_POINT('Ctrl Pts',(81.6712224189802,8.99004308033938,136.926896824456));
#69809=CARTESIAN_POINT('Ctrl Pts',(81.6651515597865,8.85732401881156,136.918935842363));
#69810=CARTESIAN_POINT('Ctrl Pts',(81.6316554657435,8.65589040181983,136.906409426386));
#69811=CARTESIAN_POINT('Ctrl Pts',(81.6153131106448,8.58590802729544,136.901960051444));
#69812=CARTESIAN_POINT('Ctrl Pts',(81.5899272799326,8.50206680169757,136.896276951877));
#69813=CARTESIAN_POINT('Ctrl Pts',(81.5851280112728,8.4869937927546,136.895240864237));
#69814=CARTESIAN_POINT('Ctrl Pts',(81.5778349735574,8.46516866762161,136.89371652191));
#69815=CARTESIAN_POINT('Ctrl Pts',(81.5755107528314,8.45836024811325,136.89323755076));
#69816=CARTESIAN_POINT('Ctrl Pts',(81.5713540664811,8.44643707202731,136.892392338283));
#69817=CARTESIAN_POINT('Ctrl Pts',(81.5695405691288,8.44131590494413,136.892027204831));
#69818=CARTESIAN_POINT('Ctrl Pts',(81.5655263782726,8.4301539769805,136.891226680444));
#69819=CARTESIAN_POINT('Ctrl Pts',(81.5633157933471,8.42411714923985,136.890790741317));
#69820=CARTESIAN_POINT('Ctrl Pts',(81.5570246087822,8.4072399016705,136.889563904925));
#69821=CARTESIAN_POINT('Ctrl Pts',(81.5528659058478,8.39642926986835,136.888768685536));
#69822=CARTESIAN_POINT('Ctrl Pts',(81.5222892163702,8.31935279925682,136.883036021022));
#69823=CARTESIAN_POINT('Ctrl Pts',(81.4917543439312,8.25480757612961,136.877903187313));
#69824=CARTESIAN_POINT('Ctrl Pts',(81.4502898035044,8.17998923869833,136.871692828559));
#69825=CARTESIAN_POINT('Ctrl Pts',(81.4432387155267,8.16764180305702,136.870658858038));
#69826=CARTESIAN_POINT('Ctrl Pts',(81.4020137165864,8.09755017501308,136.864741651403));
#69827=CARTESIAN_POINT('Ctrl Pts',(81.3645323426622,8.04181919621046,136.859852864129));
#69828=CARTESIAN_POINT('Ctrl Pts',(81.279182604106,7.93011871742011,136.849772279195));
#69829=CARTESIAN_POINT('Ctrl Pts',(81.2307568765635,7.87474700498699,136.844607678291));
#69830=CARTESIAN_POINT('Ctrl Pts',(81.1663483333201,7.81025238864768,136.8383869511));
#69831=CARTESIAN_POINT('Ctrl Pts',(81.1536721564451,7.79795656880646,136.837190498154));
#69832=CARTESIAN_POINT('Ctrl Pts',(81.1329732538303,7.7785078724003,136.835280215567));
#69833=CARTESIAN_POINT('Ctrl Pts',(81.1250729326946,7.77122731266041,136.834560934724));
#69834=CARTESIAN_POINT('Ctrl Pts',(81.1098383097247,7.75745792706753,136.833192272027));
#69835=CARTESIAN_POINT('Ctrl Pts',(81.1025161719375,7.75095637612602,136.832542369872));
#69836=CARTESIAN_POINT('Ctrl Pts',(81.0856769838456,7.7362678007032,136.831065374322));
#69837=CARTESIAN_POINT('Ctrl Pts',(81.0761237914023,7.72812296792738,136.830240044582));
#69838=CARTESIAN_POINT('Ctrl Pts',(81.0503887938214,7.70667945261632,136.828049171444));
#69839=CARTESIAN_POINT('Ctrl Pts',(81.0340464230124,7.69357636496063,136.826691465504));
#69840=CARTESIAN_POINT('Ctrl Pts',(80.9209696590145,7.60636456397531,136.817510131877));
#69841=CARTESIAN_POINT('Ctrl Pts',(80.8166041346293,7.54275383490075,136.810112937507));
#69842=CARTESIAN_POINT('Ctrl Pts',(80.6468474133552,7.46330148471858,136.798658618166));
#69843=CARTESIAN_POINT('Ctrl Pts',(80.5858862609422,7.43904197648147,136.794639866934));
#69844=CARTESIAN_POINT('Ctrl Pts',(80.5024725214716,7.41142344598125,136.789077368489));
#69845=CARTESIAN_POINT('Ctrl Pts',(80.4811476814525,7.40483514568857,136.78764973846));
#69846=CARTESIAN_POINT('Ctrl Pts',(80.4443864797406,7.39428196086315,136.785169016454));
#69847=CARTESIAN_POINT('Ctrl Pts',(80.4290133520928,7.3901064436533,136.784125785631));
#69848=CARTESIAN_POINT('Ctrl Pts',(80.406594820929,7.38436121002614,136.782592842662));
#69849=CARTESIAN_POINT('Ctrl Pts',(80.3995948267126,7.38261568644368,136.782112561499));
#69850=CARTESIAN_POINT('Ctrl Pts',(80.3872541589689,7.37962341033284,136.781262619434));
#69851=CARTESIAN_POINT('Ctrl Pts',(80.381918337216,7.37835748132305,136.780894052722));
#69852=CARTESIAN_POINT('Ctrl Pts',(80.3703065362092,7.37566305993886,136.780089559));
#69853=CARTESIAN_POINT('Ctrl Pts',(80.3640285949764,7.37424460507,136.779653108145));
#69854=CARTESIAN_POINT('Ctrl Pts',(80.3463976223474,7.37036825622229,136.778423478526));
#69855=CARTESIAN_POINT('Ctrl Pts',(80.3350271334523,7.36799272854395,136.777625947544));
#69856=CARTESIAN_POINT('Ctrl Pts',(80.2466940468641,7.3505001320761,136.771400025706));
#69857=CARTESIAN_POINT('Ctrl Pts',(80.1687834258318,7.34071788543422,136.765735938482));
#69858=CARTESIAN_POINT('Ctrl Pts',(80.0841050236893,7.33611203704654,136.759570310174));
#69859=CARTESIAN_POINT('Ctrl Pts',(80.0777243878536,7.33580177639229,136.759105630035));
#69860=CARTESIAN_POINT('Ctrl Pts',(80.0049687431653,7.33268334361355,136.753806824493));
#69861=CARTESIAN_POINT('Ctrl Pts',(79.9384815145451,7.333811005712,136.748965503485));
#69862=CARTESIAN_POINT('Ctrl Pts',(79.7977697960227,7.34463383993467,136.738838859056));
#69863=CARTESIAN_POINT('Ctrl Pts',(79.7237636951394,7.3553631071429,136.73358567604));
#69864=CARTESIAN_POINT('Ctrl Pts',(79.6333835584968,7.37474227366125,136.727276485483));
#69865=CARTESIAN_POINT('Ctrl Pts',(79.6161091430804,7.3787356340346,136.726075186789));
#69866=CARTESIAN_POINT('Ctrl Pts',(79.588459588512,7.38559415740954,136.724159077109));
#69867=CARTESIAN_POINT('Ctrl Pts',(79.5780431392189,7.38828533793717,136.723438755088));
#69868=CARTESIAN_POINT('Ctrl Pts',(79.5582009220473,7.39361730171117,136.722069298777));
#69869=CARTESIAN_POINT('Ctrl Pts',(79.5487709702345,7.39624061395898,136.721419632922));
#69870=CARTESIAN_POINT('Ctrl Pts',(79.5273289595814,7.40240964810455,136.719944784321));
#69871=CARTESIAN_POINT('Ctrl Pts',(79.5153325728377,7.40600804763197,136.719121346653));
#69872=CARTESIAN_POINT('Ctrl Pts',(79.4834852018927,7.41595367384657,136.716939070755));
#69873=CARTESIAN_POINT('Ctrl Pts',(79.4637104247722,7.42253879498198,136.715587970325));
#69874=CARTESIAN_POINT('Ctrl Pts',(79.3277038545238,7.47068312921476,136.706310434162));
#69875=CARTESIAN_POINT('Ctrl Pts',(79.2162803033471,7.52467647500018,136.698823529851));
#69876=CARTESIAN_POINT('Ctrl Pts',(79.0335694217868,7.63980673795968,136.685623092476));
#69877=CARTESIAN_POINT('Ctrl Pts',(78.9595576862316,7.69555042192493,136.679945541948));
#69878=CARTESIAN_POINT('Ctrl Pts',(78.8815147889027,7.76521500198143,136.673108825756));
#69879=CARTESIAN_POINT('Ctrl Pts',(78.8725537632234,7.77339161877224,136.672309866105));
#69880=CARTESIAN_POINT('Ctrl Pts',(78.8589482264551,7.78608123331161,136.671073704971));
#69881=CARTESIAN_POINT('Ctrl Pts',(78.8542391888395,7.79052487330223,136.670641520119));
#69882=CARTESIAN_POINT('Ctrl Pts',(78.8455932049895,7.79877938189214,136.669839692465));
#69883=CARTESIAN_POINT('Ctrl Pts',(78.8416490114791,7.80258235939275,136.669470640732));
#69884=CARTESIAN_POINT('Ctrl Pts',(78.832680139837,7.81131589518588,136.668623975459));
#69885=CARTESIAN_POINT('Ctrl Pts',(78.8276679044773,7.81625889221227,136.668145423239));
#69886=CARTESIAN_POINT('Ctrl Pts',(78.8118018459658,7.83210538182189,136.666613735772));
#69887=CARTESIAN_POINT('Ctrl Pts',(78.801068026262,7.84312715792007,136.665552089735));
#69888=CARTESIAN_POINT('Ctrl Pts',(78.7015875533203,7.94814790205874,136.655483836516));
#69889=CARTESIAN_POINT('Ctrl Pts',(78.6239167938436,8.05202297935756,136.645917844602));
#69890=CARTESIAN_POINT('Ctrl Pts',(78.5140361434025,8.24137836753594,136.630102035964));
#69891=CARTESIAN_POINT('Ctrl Pts',(78.4753621461088,8.322445951564,136.623750161606));
#69892=CARTESIAN_POINT('Ctrl Pts',(78.4368323551965,8.42345664111919,136.616363206657));
#69893=CARTESIAN_POINT('Ctrl Pts',(78.4305529141594,8.44077623220499,136.615113974666));
#69894=CARTESIAN_POINT('Ctrl Pts',(78.421014869428,8.46851066873512,136.613140259184));
#69895=CARTESIAN_POINT('Ctrl Pts',(78.4175692373393,8.4788590948793,136.612409659228));
#69896=CARTESIAN_POINT('Ctrl Pts',(78.4112349102624,8.49852553556778,136.611031973253));
#69897=CARTESIAN_POINT('Ctrl Pts',(78.4083259638667,8.50783649215256,136.610384247156));
#69898=CARTESIAN_POINT('Ctrl Pts',(78.4018883932622,8.52909608521878,136.608915311756));
#69899=CARTESIAN_POINT('Ctrl Pts',(78.3984116560258,8.54105992217274,136.608095820398));
#69900=CARTESIAN_POINT('Ctrl Pts',(78.3896655882493,8.57246658091112,136.605962403692));
#69901=CARTESIAN_POINT('Ctrl Pts',(78.3846140015559,8.59196829271555,136.60465547565));
#69902=CARTESIAN_POINT('Ctrl Pts',(78.3492974616268,8.73926351182668,136.594905585127));
#69903=CARTESIAN_POINT('Ctrl Pts',(78.3338838504094,8.87014160580966,136.586972037662));
#69904=CARTESIAN_POINT('Ctrl Pts',(78.3340197490512,9.02294677687804,136.577620043621));
#69905=CARTESIAN_POINT('Ctrl Pts',(78.3344536791785,9.04440920217299,136.576303249206));
#69906=CARTESIAN_POINT('Ctrl Pts',(78.3378839391261,9.13111758901513,136.570951054929));
#69907=CARTESIAN_POINT('Ctrl Pts',(78.3443007902142,9.19616240125983,136.566863007183));
#69908=CARTESIAN_POINT('Ctrl Pts',(78.3563104862453,9.27197837462577,136.56184054762));
#69909=CARTESIAN_POINT('Ctrl Pts',(78.3582210861192,9.2832833103782,136.561084807116));
#69910=CARTESIAN_POINT('Ctrl Pts',(78.361380210246,9.30086903943918,136.559897239663));
#69911=CARTESIAN_POINT('Ctrl Pts',(78.3625485693222,9.30716413041022,136.559469734436));
#69912=CARTESIAN_POINT('Ctrl Pts',(78.3647761199494,9.31879213203793,136.558675366611));
#69913=CARTESIAN_POINT('Ctrl Pts',(78.3658251665951,9.32412678388195,136.55830907206));
#69914=CARTESIAN_POINT('Ctrl Pts',(78.36833079584,9.33654707787777,136.557451973668));
#69915=CARTESIAN_POINT('Ctrl Pts',(78.3698074289554,9.34362843866692,136.556960070411));
#69916=CARTESIAN_POINT('Ctrl Pts',(78.374706053551,9.36637793164341,136.555369859755));
#69917=CARTESIAN_POINT('Ctrl Pts',(78.3783080674557,9.38200579814046,136.554262270216));
#69918=CARTESIAN_POINT('Ctrl Pts',(78.3875090109046,9.41944717148081,136.551575936862));
#69919=CARTESIAN_POINT('Ctrl Pts',(78.3933256591598,9.44120355757371,136.549988014995));
#69920=CARTESIAN_POINT('Ctrl Pts',(78.4105689193626,9.50082844584118,136.545573123226));
#69921=CARTESIAN_POINT('Ctrl Pts',(78.422903446365,9.53840988900929,136.542719656609));
#69922=CARTESIAN_POINT('Ctrl Pts',(78.4365593610507,9.57550792217122,136.539851329404));
#69923=CARTESIAN_POINT('Ctrl Pts',(78.436559386885,9.57550799235334,136.733447166179));
#69924=CARTESIAN_POINT('Ctrl Pts',(78.4030736853152,9.48453982772584,136.7396214358));
#69925=CARTESIAN_POINT('Ctrl Pts',(78.3775820235553,9.3907985152114,136.745546815303));
#69926=CARTESIAN_POINT('Ctrl Pts',(78.3470673792254,9.22139434210338,136.756057559526));
#69927=CARTESIAN_POINT('Ctrl Pts',(78.3387660613633,9.14663529075277,136.760635517436));
#69928=CARTESIAN_POINT('Ctrl Pts',(78.3345040615497,9.04752667892352,136.766897315785));
#69929=CARTESIAN_POINT('Ctrl Pts',(78.3339912587269,9.02345761297898,136.768433258204));
#69930=CARTESIAN_POINT('Ctrl Pts',(78.3340063127332,8.98253179884407,136.771083427609));
#69931=CARTESIAN_POINT('Ctrl Pts',(78.3342683081362,8.96567826665469,136.772185903033));
#69932=CARTESIAN_POINT('Ctrl Pts',(78.3350100826247,8.94153772320898,136.773784708654));
#69933=CARTESIAN_POINT('Ctrl Pts',(78.3352821544608,8.93424475258736,136.774270287832));
#69934=CARTESIAN_POINT('Ctrl Pts',(78.3358435545575,8.92145291171762,136.77512687663));
#69935=CARTESIAN_POINT('Ctrl Pts',(78.336112240968,8.91595332062918,136.775496744943));
#69936=CARTESIAN_POINT('Ctrl Pts',(78.3367468940995,8.90416255723736,136.776293261581));
#69937=CARTESIAN_POINT('Ctrl Pts',(78.3371212853714,8.89787220329512,136.776720336044));
#69938=CARTESIAN_POINT('Ctrl Pts',(78.3382678817186,8.88029006601136,136.777919737365));
#69939=CARTESIAN_POINT('Ctrl Pts',(78.3391194664742,8.86900405722907,136.778696199416));
#69940=CARTESIAN_POINT('Ctrl Pts',(78.345620941244,8.79315013695945,136.783955179707));
#69941=CARTESIAN_POINT('Ctrl Pts',(78.3549191936476,8.72895721360702,136.788600550031));
#69942=CARTESIAN_POINT('Ctrl Pts',(78.3892328775846,8.56154782536482,136.800982578253));
#69943=CARTESIAN_POINT('Ctrl Pts',(78.4204160779959,8.45988032602276,136.808760913248));
#69944=CARTESIAN_POINT('Ctrl Pts',(78.4829024545348,8.30918647951376,136.820349849389));
#69945=CARTESIAN_POINT('Ctrl Pts',(78.5074387888753,8.25765869026001,136.824328711338));
#69946=CARTESIAN_POINT('Ctrl Pts',(78.5427106751217,8.19243793920472,136.829384750903));
#69947=CARTESIAN_POINT('Ctrl Pts',(78.5510801249017,8.17751602332318,136.830543104393));
#69948=CARTESIAN_POINT('Ctrl Pts',(78.565016929048,8.15354123986161,136.832407432349));
#69949=CARTESIAN_POINT('Ctrl Pts',(78.5704434701634,8.14440840141322,136.833118397418));
#69950=CARTESIAN_POINT('Ctrl Pts',(78.5810561805067,8.12693015172603,136.834480789204));
#69951=CARTESIAN_POINT('Ctrl Pts',(78.5862295314058,8.11857751785878,136.835132646085));
#69952=CARTESIAN_POINT('Ctrl Pts',(78.5984298129583,8.09926334226122,136.836642101561));
#69953=CARTESIAN_POINT('Ctrl Pts',(78.6055120194309,8.0883373409974,136.837497619059));
#69954=CARTESIAN_POINT('Ctrl Pts',(78.6289517611519,8.05308826193487,136.840264121129));
#69955=CARTESIAN_POINT('Ctrl Pts',(78.6458237677389,8.02911277069109,136.842155863237));
#69956=CARTESIAN_POINT('Ctrl Pts',(78.687779516564,7.97271591149635,136.846642829469));
#69957=CARTESIAN_POINT('Ctrl Pts',(78.7134443739473,7.94075018576501,136.849216611562));
#69958=CARTESIAN_POINT('Ctrl Pts',(78.7883700637603,7.85417587290556,136.856329726646));
#69959=CARTESIAN_POINT('Ctrl Pts',(78.8401043991311,7.80183360512246,136.860796614085));
#69960=CARTESIAN_POINT('Ctrl Pts',(78.9595934886699,7.69595660826427,136.870555998891));
#69961=CARTESIAN_POINT('Ctrl Pts',(79.0283848665807,7.64392655417022,136.875844112729));
#69962=CARTESIAN_POINT('Ctrl Pts',(79.1141666863909,7.58893498888015,136.882455019426));
#69963=CARTESIAN_POINT('Ctrl Pts',(79.127574218344,7.5806063490936,136.883488876303));
#69964=CARTESIAN_POINT('Ctrl Pts',(79.1471901595856,7.56880401922944,136.88500539939));
#69965=CARTESIAN_POINT('Ctrl Pts',(79.1533061405205,7.56517734092202,136.885478776532));
#69966=CARTESIAN_POINT('Ctrl Pts',(79.1641803132638,7.55882286604679,136.886321747656));
#69967=CARTESIAN_POINT('Ctrl Pts',(79.1689290337283,7.55607925150957,136.886690321747));
#69968=CARTESIAN_POINT('Ctrl Pts',(79.1792668997422,7.55017435272811,136.887493772831));
#69969=CARTESIAN_POINT('Ctrl Pts',(79.1848607139052,7.54702196502059,136.887929163654));
#69970=CARTESIAN_POINT('Ctrl Pts',(79.2008557751368,7.53812940244398,136.88917565485));
#69971=CARTESIAN_POINT('Ctrl Pts',(79.2113001410009,7.53246817806658,136.889991407863));
#69972=CARTESIAN_POINT('Ctrl Pts',(79.2352491944495,7.51981641808843,136.891864572921));
#69973=CARTESIAN_POINT('Ctrl Pts',(79.2487907110497,7.51289818820773,136.892925596629));
#69974=CARTESIAN_POINT('Ctrl Pts',(79.3926812392006,7.44185269648364,136.904205504012));
#69975=CARTESIAN_POINT('Ctrl Pts',(79.5307891946342,7.39485083645149,136.91501211988));
#69976=CARTESIAN_POINT('Ctrl Pts',(79.7375241832035,7.35350096951997,136.930069769281));
#69977=CARTESIAN_POINT('Ctrl Pts',(79.8025087289686,7.34444820210943,136.934662444953));
#69978=CARTESIAN_POINT('Ctrl Pts',(79.88545485719,7.33784875794428,136.940341161207));
#69979=CARTESIAN_POINT('Ctrl Pts',(79.903065819285,7.33672878116685,136.94153669007));
#69980=CARTESIAN_POINT('Ctrl Pts',(79.9314178969884,7.3353775790235,136.943445734171));
#69981=CARTESIAN_POINT('Ctrl Pts',(79.9421488409848,7.3349701017669,136.944164690372));
#69982=CARTESIAN_POINT('Ctrl Pts',(79.9626687076319,7.33438953908708,136.945532878419));
#69983=CARTESIAN_POINT('Ctrl Pts',(79.9724566431502,7.33419893043463,136.946182628945));
#69984=CARTESIAN_POINT('Ctrl Pts',(79.9950119682409,7.33395855055136,136.947673585971));
#69985=CARTESIAN_POINT('Ctrl Pts',(80.0077794925974,7.33396924208447,136.948512875108));
#69986=CARTESIAN_POINT('Ctrl Pts',(80.0484006518734,7.33447024037042,136.951169344954));
#69987=CARTESIAN_POINT('Ctrl Pts',(80.076243568615,7.33551237129322,136.952969410681));
#69988=CARTESIAN_POINT('Ctrl Pts',(80.1770792879234,7.34182229840092,136.959429254076));
#69989=CARTESIAN_POINT('Ctrl Pts',(80.2497335226601,7.35119888417629,136.963966667801));
#69990=CARTESIAN_POINT('Ctrl Pts',(80.4498370468105,7.39055937721553,136.976475842704));
#69991=CARTESIAN_POINT('Ctrl Pts',(80.5746952596342,7.43080668921727,136.984278205149));
#69992=CARTESIAN_POINT('Ctrl Pts',(80.7072561045526,7.49150001316877,136.993749635824));
#69993=CARTESIAN_POINT('Ctrl Pts',(80.7208808831035,7.49796334230454,136.994738366762));
#69994=CARTESIAN_POINT('Ctrl Pts',(80.7407501115925,7.50772151433877,136.996205496484));
#69995=CARTESIAN_POINT('Ctrl Pts',(80.7470647878348,7.51087273718508,136.996675560369));
#69996=CARTESIAN_POINT('Ctrl Pts',(80.7582379682765,7.516537460813,136.997514382947));
#69997=CARTESIAN_POINT('Ctrl Pts',(80.7631043855971,7.51903490358137,136.997882150861));
#69998=CARTESIAN_POINT('Ctrl Pts',(80.7737677952332,7.5245738742949,136.998693420935));
#69999=CARTESIAN_POINT('Ctrl Pts',(80.7795591139725,7.52762557835944,136.999137526626));
#70000=CARTESIAN_POINT('Ctrl Pts',(80.7963388836133,7.53659433490796,137.000434164659));
#70001=CARTESIAN_POINT('Ctrl Pts',(80.8072787359053,7.5426006801379,137.001291930846));
#70002=CARTESIAN_POINT('Ctrl Pts',(80.8322664331978,7.55668742064324,137.003278070515));
#70003=CARTESIAN_POINT('Ctrl Pts',(80.846265765879,7.56485093877536,137.00441067271));
#70004=CARTESIAN_POINT('Ctrl Pts',(80.8935450089723,7.59335346502885,137.008298515055));
#70005=CARTESIAN_POINT('Ctrl Pts',(80.9262273734105,7.61465541325279,137.011093449451));
#70006=CARTESIAN_POINT('Ctrl Pts',(81.0157500518482,7.67758981040091,137.019000471824));
#70007=CARTESIAN_POINT('Ctrl Pts',(81.0707431456563,7.72170971288379,137.024153825553));
#70008=CARTESIAN_POINT('Ctrl Pts',(81.1942227452502,7.83435010290942,137.036260037415));
#70009=CARTESIAN_POINT('Ctrl Pts',(81.2598665593812,7.90562817839676,137.043136301701));
#70010=CARTESIAN_POINT('Ctrl Pts',(81.3304312911098,7.99707379042736,137.05103540341));
#70011=CARTESIAN_POINT('Ctrl Pts',(81.3416480347789,8.01212905548655,137.052309403241));
#70012=CARTESIAN_POINT('Ctrl Pts',(81.3590799344955,8.03637112370215,137.054319988779));
#70013=CARTESIAN_POINT('Ctrl Pts',(81.3654616852998,8.0454355569973,137.055062941595));
#70014=CARTESIAN_POINT('Ctrl Pts',(81.3772182215592,8.06249334398771,137.056444941151));
#70015=CARTESIAN_POINT('Ctrl Pts',(81.3826150441936,8.07047086861635,137.057084805771));
#70016=CARTESIAN_POINT('Ctrl Pts',(81.394645433703,8.08859066904249,137.058523918968));
#70017=CARTESIAN_POINT('Ctrl Pts',(81.4012381752752,8.09875949746397,137.059321617668));
#70018=CARTESIAN_POINT('Ctrl Pts',(81.4207421221415,8.12957439531984,137.061710067042));
#70019=CARTESIAN_POINT('Ctrl Pts',(81.4333125873483,8.15043303020283,137.063288340336));
#70020=CARTESIAN_POINT('Ctrl Pts',(81.4613258109241,8.19930917774067,137.066905332146));
#70021=CARTESIAN_POINT('Ctrl Pts',(81.4764281202986,8.22751109276889,137.068932489297));
#70022=CARTESIAN_POINT('Ctrl Pts',(81.5290033459996,8.33287168606672,137.076320011856));
#70023=CARTESIAN_POINT('Ctrl Pts',(81.5613147843599,8.41245538300326,137.081535407693));
#70024=CARTESIAN_POINT('Ctrl Pts',(81.6148198800948,8.58036312745446,137.092302034073));
#70025=CARTESIAN_POINT('Ctrl Pts',(81.6352154788742,8.66863238517132,137.097840102902));
#70026=CARTESIAN_POINT('Ctrl Pts',(81.6506322174938,8.77368769325163,137.104729507002));
#70027=CARTESIAN_POINT('Ctrl Pts',(81.652697507866,8.78929907209232,137.105761031409));
#70028=CARTESIAN_POINT('Ctrl Pts',(81.6553728835853,8.8119918009125,137.107274750262));
#70029=CARTESIAN_POINT('Ctrl Pts',(81.6561594996812,8.81905201392687,137.10774770353));
#70030=CARTESIAN_POINT('Ctrl Pts',(81.6574732822563,8.83157081142447,137.108590208591));
#70031=CARTESIAN_POINT('Ctrl Pts',(81.6580186866952,8.83702728371803,137.10895874472));
#70032=CARTESIAN_POINT('Ctrl Pts',(81.6591446599214,8.84888320875113,137.109762467733));
#70033=CARTESIAN_POINT('Ctrl Pts',(81.6597151408411,8.85528325970895,137.110198171706));
#70034=CARTESIAN_POINT('Ctrl Pts',(81.661236646562,8.87354665634267,137.111446449934));
#70035=CARTESIAN_POINT('Ctrl Pts',(81.6620975663473,8.88541682635254,137.112263697002));
#70036=CARTESIAN_POINT('Ctrl Pts',(81.6686518303634,8.99153249930862,137.11961669387));
#70037=CARTESIAN_POINT('Ctrl Pts',(81.6664502117914,9.08608453758049,137.126489790719));
#70038=CARTESIAN_POINT('Ctrl Pts',(81.6431119020496,9.30091395812051,137.142220075137));
#70039=CARTESIAN_POINT('Ctrl Pts',(81.616749530842,9.42011567995595,137.151009721228));
#70040=CARTESIAN_POINT('Ctrl Pts',(81.5708940626847,9.55523578336539,137.160824648851));
#70041=CARTESIAN_POINT('Ctrl Pts',(81.5637873314049,9.5749471129144,137.162253763344));
#70042=CARTESIAN_POINT('Ctrl Pts',(81.5518306590445,9.6062468085746,137.16451959139));
#70043=CARTESIAN_POINT('Ctrl Pts',(81.547218424341,9.61792293177251,137.165364066556));
#70044=CARTESIAN_POINT('Ctrl Pts',(81.5387753200797,9.63860969892447,137.166859192072));
#70045=CARTESIAN_POINT('Ctrl Pts',(81.5349962149629,9.64764068767145,137.167511544957));
#70046=CARTESIAN_POINT('Ctrl Pts',(81.5269053177683,9.66650690800216,137.16887383513));
#70047=CARTESIAN_POINT('Ctrl Pts',(81.5225775820687,9.67633484571877,137.169583195738));
#70048=CARTESIAN_POINT('Ctrl Pts',(81.5108883537846,9.702199197676,137.171449730414));
#70049=CARTESIAN_POINT('Ctrl Pts',(81.5033664766593,9.71816196390955,137.172601383266));
#70050=CARTESIAN_POINT('Ctrl Pts',(81.4633015131445,9.79979769045396,137.178494476378));
#70051=CARTESIAN_POINT('Ctrl Pts',(81.4267022120965,9.86339470417785,137.18309201408));
#70052=CARTESIAN_POINT('Ctrl Pts',(81.3312272227854,10.006551182847,137.193712905817));
#70053=CARTESIAN_POINT('Ctrl Pts',(81.2692294400598,10.0836819981732,137.199650714628));
#70054=CARTESIAN_POINT('Ctrl Pts',(81.1627542193764,10.1943893051936,137.209183141753));
#70055=CARTESIAN_POINT('Ctrl Pts',(81.1228165717532,10.2320084490749,137.2126423618));
#70056=CARTESIAN_POINT('Ctrl Pts',(81.0725947826126,10.2748417351893,137.216964011017));
#70057=CARTESIAN_POINT('Ctrl Pts',(81.064015015251,10.2820113291743,137.217701391912));
#70058=CARTESIAN_POINT('Ctrl Pts',(81.0504599681644,10.2931086668703,137.218866131505));
#70059=CARTESIAN_POINT('Ctrl Pts',(81.0455331445941,10.2970954511045,137.219289428603));
#70060=CARTESIAN_POINT('Ctrl Pts',(81.0367206717318,10.3041436726657,137.220046729303));
#70061=CARTESIAN_POINT('Ctrl Pts',(81.0328439664583,10.3072160528096,137.220379946082));
#70062=CARTESIAN_POINT('Ctrl Pts',(81.0234193004885,10.3146172269441,137.221190164059));
#70063=CARTESIAN_POINT('Ctrl Pts',(81.0178575820266,10.3189281467118,137.221668385616));
#70064=CARTESIAN_POINT('Ctrl Pts',(81.0003786265952,10.3322997865969,137.223171157498));
#70065=CARTESIAN_POINT('Ctrl Pts',(80.9883668463439,10.3412348996587,137.224203667787));
#70066=CARTESIAN_POINT('Ctrl Pts',(80.9246734000024,10.3872938528503,137.22967064186));
#70067=CARTESIAN_POINT('Ctrl Pts',(80.8710209325088,10.4215927877309,137.234246628945));
#70068=CARTESIAN_POINT('Ctrl Pts',(80.7207611093635,10.5059464438477,137.246749508099));
#70069=CARTESIAN_POINT('Ctrl Pts',(80.6209860253325,10.5497587407792,137.254707430096));
#70070=CARTESIAN_POINT('Ctrl Pts',(80.4690607933605,10.5994220790315,137.266011218455));
#70071=CARTESIAN_POINT('Ctrl Pts',(80.4197640777349,10.6130617125935,137.269565251839));
#70072=CARTESIAN_POINT('Ctrl Pts',(80.3539378517031,10.6280517334369,137.274163338005));
#70073=CARTESIAN_POINT('Ctrl Pts',(80.3379091313229,10.6314539227006,137.275271741466));
#70074=CARTESIAN_POINT('Ctrl Pts',(80.31156082702,10.6366415136901,137.277075992327));
#70075=CARTESIAN_POINT('Ctrl Pts',(80.3012703047201,10.6385669975331,137.27777624808));
#70076=CARTESIAN_POINT('Ctrl Pts',(80.2812275607659,10.6421220423068,137.279131825288));
#70077=CARTESIAN_POINT('Ctrl Pts',(80.2714776606844,10.6437620356028,137.27978745126));
#70078=CARTESIAN_POINT('Ctrl Pts',(80.2484623751338,10.6474229829796,137.281326461368));
#70079=CARTESIAN_POINT('Ctrl Pts',(80.2351859027425,10.6493706815928,137.282207503514));
#70080=CARTESIAN_POINT('Ctrl Pts',(80.1904607809732,10.6553809635095,137.285154198034));
#70081=CARTESIAN_POINT('Ctrl Pts',(80.1589188923718,10.6587062542882,137.287196833749));
#70082=CARTESIAN_POINT('Ctrl Pts',(80.0817652431223,10.6646188745619,137.292123523469));
#70083=CARTESIAN_POINT('Ctrl Pts',(80.0361045469151,10.6662348184673,137.294979714829));
#70084=CARTESIAN_POINT('Ctrl Pts',(79.9202871807467,10.6655696888832,137.302145286982));
#70085=CARTESIAN_POINT('Ctrl Pts',(79.850236043801,10.6607370501646,137.30640394688));
#70086=CARTESIAN_POINT('Ctrl Pts',(79.7581933805297,10.6485147712397,137.312085024652));
#70087=CARTESIAN_POINT('Ctrl Pts',(79.7357524450302,10.645066743442,137.31347727211));
#70088=CARTESIAN_POINT('Ctrl Pts',(79.6490469979864,10.6299245969132,137.318906036174));
#70089=CARTESIAN_POINT('Ctrl Pts',(79.5854286126961,10.6149150765957,137.322994359479));
#70090=CARTESIAN_POINT('Ctrl Pts',(79.5118803014772,10.5929301840218,137.328017006247));
#70091=CARTESIAN_POINT('Ctrl Pts',(79.5009315690447,10.5895339237011,137.32877262626));
#70092=CARTESIAN_POINT('Ctrl Pts',(79.4839251983947,10.584065584103,137.329959974923));
#70093=CARTESIAN_POINT('Ctrl Pts',(79.4778427368079,10.5820710365412,137.330387382962));
#70094=CARTESIAN_POINT('Ctrl Pts',(79.4666170529393,10.5783181478392,137.331181545506));
#70095=CARTESIAN_POINT('Ctrl Pts',(79.4614707563206,10.5765696288291,137.33154773202));
#70096=CARTESIAN_POINT('Ctrl Pts',(79.4494980113515,10.5724362778149,137.332404532393));
#70097=CARTESIAN_POINT('Ctrl Pts',(79.4426784654646,10.570032161951,137.332896244569));
#70098=CARTESIAN_POINT('Ctrl Pts',(79.4207932614516,10.562156352059,137.334485643967));
#70099=CARTESIAN_POINT('Ctrl Pts',(79.405791369107,10.5565117956628,137.335592602676));
#70100=CARTESIAN_POINT('Ctrl Pts',(79.3699279742725,10.5424239612572,137.338277211525));
#70101=CARTESIAN_POINT('Ctrl Pts',(79.349151891389,10.5337728223931,137.33986402686));
#70102=CARTESIAN_POINT('Ctrl Pts',(79.267674636542,10.4978922777206,137.346196413881));
#70103=CARTESIAN_POINT('Ctrl Pts',(79.2084545190922,10.4674592182152,137.351040247954));
#70104=CARTESIAN_POINT('Ctrl Pts',(79.0474882485134,10.3721546951768,137.364657209239));
#70105=CARTESIAN_POINT('Ctrl Pts',(78.9507143056559,10.2996525362347,137.373359192585));
#70106=CARTESIAN_POINT('Ctrl Pts',(78.847302217206,10.2030304697436,137.383094040994));
#70107=CARTESIAN_POINT('Ctrl Pts',(78.8322718237093,10.1884466605559,137.384522420273));
#70108=CARTESIAN_POINT('Ctrl Pts',(78.808678873446,10.1646748412572,137.386787317785));
#70109=CARTESIAN_POINT('Ctrl Pts',(78.7999387177852,10.1556671001299,137.387631587554));
#70110=CARTESIAN_POINT('Ctrl Pts',(78.7845640397795,10.1394591927282,137.389126479589));
#70111=CARTESIAN_POINT('Ctrl Pts',(78.7778897106595,10.1322977845993,137.389778802522));
#70112=CARTESIAN_POINT('Ctrl Pts',(78.7640260963101,10.1171570388989,137.391141159827));
#70113=CARTESIAN_POINT('Ctrl Pts',(78.7568500483043,10.1091661493547,137.391850616386));
#70114=CARTESIAN_POINT('Ctrl Pts',(78.7407313745033,10.0908642412796,137.393454409272));
#70115=CARTESIAN_POINT('Ctrl Pts',(78.7318371039949,10.0805115229938,137.394346731238));
#70116=CARTESIAN_POINT('Ctrl Pts',(78.6919672881274,10.0329334559382,137.398382610261));
#70117=CARTESIAN_POINT('Ctrl Pts',(78.6624949279325,9.99447571999671,137.401465951503));
#70118=CARTESIAN_POINT('Ctrl Pts',(78.5842718581045,9.88262336604409,137.410024479372));
#70119=CARTESIAN_POINT('Ctrl Pts',(78.539605694465,9.80657283152094,137.415372364282));
#70120=CARTESIAN_POINT('Ctrl Pts',(78.4771203097745,9.67780902984256,137.424120149123));
#70121=CARTESIAN_POINT('Ctrl Pts',(78.4555629954577,9.62713370969076,137.427494595459));
#70122=CARTESIAN_POINT('Ctrl Pts',(78.4365593900224,9.5755080008764,137.430947520545));
#70123=CARTESIAN_POINT('Origin',(80.,9.,134.));
#70124=CARTESIAN_POINT('',(78.4365594482967,9.57550815918599,138.131873589273));
#70125=CARTESIAN_POINT('',(78.4365593728781,9.57550795430191,137.937814872615));
#70126=CARTESIAN_POINT('',(78.4365593737638,9.57550795670799,134.));
#70127=CARTESIAN_POINT('',(78.3340004536037,8.99997160195063,137.276979806444));
#70128=CARTESIAN_POINT('Ctrl Pts',(78.4365593728781,9.5755079543019,137.937814872615));
#70129=CARTESIAN_POINT('Ctrl Pts',(78.4603180243237,9.64005135572325,137.933372005971));
#70130=CARTESIAN_POINT('Ctrl Pts',(78.4880535272684,9.70306961636733,137.929060117645));
#70131=CARTESIAN_POINT('Ctrl Pts',(78.5665915402355,9.85521111305201,137.918489348387));
#70132=CARTESIAN_POINT('Ctrl Pts',(78.6218618578815,9.94168978399369,137.912339466934));
#70133=CARTESIAN_POINT('Ctrl Pts',(78.7166757234652,10.0636472777365,137.902733472706));
#70134=CARTESIAN_POINT('Ctrl Pts',(78.7505375248075,10.1032266780965,137.899441897796));
#70135=CARTESIAN_POINT('Ctrl Pts',(78.7937404694485,10.1491803062351,137.895310756722));
#70136=CARTESIAN_POINT('Ctrl Pts',(78.8013677233108,10.1571335621185,137.894583814464));
#70137=CARTESIAN_POINT('Ctrl Pts',(78.8134803147446,10.1695156083388,137.893431954189));
#70138=CARTESIAN_POINT('Ctrl Pts',(78.8179130109011,10.1739957702526,137.89301095204));
#70139=CARTESIAN_POINT('Ctrl Pts',(78.8262671585949,10.1823440941879,137.892218236306));
#70140=CARTESIAN_POINT('Ctrl Pts',(78.830182502229,10.1862180905868,137.89184698729));
#70141=CARTESIAN_POINT('Ctrl Pts',(78.8394248791861,10.1952726065343,137.890971351862));
#70142=CARTESIAN_POINT('Ctrl Pts',(78.8447674349128,10.2004369747196,137.890465762424));
#70143=CARTESIAN_POINT('Ctrl Pts',(78.8625618331006,10.2174090883994,137.888784221988));
#70144=CARTESIAN_POINT('Ctrl Pts',(78.8751610930413,10.2290597415161,137.887597496814));
#70145=CARTESIAN_POINT('Ctrl Pts',(78.906299149686,10.256973567291,137.884678707655));
#70146=CARTESIAN_POINT('Ctrl Pts',(78.9250231240445,10.2730234425448,137.882935391324));
#70147=CARTESIAN_POINT('Ctrl Pts',(79.0048908929729,10.3384661040631,137.875570568485));
#70148=CARTESIAN_POINT('Ctrl Pts',(79.0691330440637,10.3839145534009,137.869821889228));
#70149=CARTESIAN_POINT('Ctrl Pts',(79.2249486631411,10.4783735349723,137.856577618796));
#70150=CARTESIAN_POINT('Ctrl Pts',(79.3183881013215,10.523714118291,137.849147271953));
#70151=CARTESIAN_POINT('Ctrl Pts',(79.4375354745546,10.5683577223649,137.840388347377));
#70152=CARTESIAN_POINT('Ctrl Pts',(79.4597959030243,10.5761636717191,137.838779894225));
#70153=CARTESIAN_POINT('Ctrl Pts',(79.4937410006874,10.5872633250951,137.836368029617));
#70154=CARTESIAN_POINT('Ctrl Pts',(79.505307451961,10.5909061361305,137.835553283614));
#70155=CARTESIAN_POINT('Ctrl Pts',(79.5262182959437,10.5972418213938,137.834092691733));
#70156=CARTESIAN_POINT('Ctrl Pts',(79.5355483451059,10.5999797518256,137.833445401957));
#70157=CARTESIAN_POINT('Ctrl Pts',(79.5555963636861,10.6056727561798,137.83206369325));
#70158=CARTESIAN_POINT('Ctrl Pts',(79.5663210667442,10.6086025565167,137.831330120601));
#70159=CARTESIAN_POINT('Ctrl Pts',(79.595848217657,10.6163520861527,137.829325154166));
#70160=CARTESIAN_POINT('Ctrl Pts',(79.6147071949879,10.6209510279663,137.82806087318));
#70161=CARTESIAN_POINT('Ctrl Pts',(79.6569032110071,10.6304628571024,137.825265255981));
#70162=CARTESIAN_POINT('Ctrl Pts',(79.6802742251072,10.6352064239638,137.823739227656));
#70163=CARTESIAN_POINT('Ctrl Pts',(79.7555116219636,10.6488023737964,137.818887885018));
#70164=CARTESIAN_POINT('Ctrl Pts',(79.8076998245706,10.6557007887152,137.815616541092));
#70165=CARTESIAN_POINT('Ctrl Pts',(79.9557638262409,10.6681756114588,137.806469809281));
#70166=CARTESIAN_POINT('Ctrl Pts',(80.0519101902268,10.6679540340626,137.800694938082));
#70167=CARTESIAN_POINT('Ctrl Pts',(80.1988056810736,10.6548974336841,137.791520665853));
#70168=CARTESIAN_POINT('Ctrl Pts',(80.2498684314536,10.6479605163513,137.788262774791));
#70169=CARTESIAN_POINT('Ctrl Pts',(80.3113335506969,10.6366881919472,137.784169548875));
#70170=CARTESIAN_POINT('Ctrl Pts',(80.3221247004967,10.6345985681234,137.783444409162));
#70171=CARTESIAN_POINT('Ctrl Pts',(80.3390632597283,10.6311443063431,137.782294785459));
#70172=CARTESIAN_POINT('Ctrl Pts',(80.34522518396,10.6298512850267,137.78187419251));
#70173=CARTESIAN_POINT('Ctrl Pts',(80.3567651574653,10.6273613544703,137.781081786038));
#70174=CARTESIAN_POINT('Ctrl Pts',(80.3621447783337,10.6261726573734,137.780710432324));
#70175=CARTESIAN_POINT('Ctrl Pts',(80.3747768455679,10.6233156492839,137.77983392288));
#70176=CARTESIAN_POINT('Ctrl Pts',(80.3820241120107,10.6216254048738,137.779327556701));
#70177=CARTESIAN_POINT('Ctrl Pts',(80.406008334227,10.6158619835251,137.77764072285));
#70178=CARTESIAN_POINT('Ctrl Pts',(80.4226928029456,10.6115779390934,137.77644939108));
#70179=CARTESIAN_POINT('Ctrl Pts',(80.4632161898438,10.6005002744246,137.773516905807));
#70180=CARTESIAN_POINT('Ctrl Pts',(80.486975284828,10.5934319274754,137.771764371064));
#70181=CARTESIAN_POINT('Ctrl Pts',(80.5861154510812,10.5615133489777,137.764334440491));
#70182=CARTESIAN_POINT('Ctrl Pts',(80.659826748801,10.5318234463411,137.758527999245));
#70183=CARTESIAN_POINT('Ctrl Pts',(80.8233419338781,10.4519619417108,137.745303094737));
#70184=CARTESIAN_POINT('Ctrl Pts',(80.9112011989396,10.398500708682,137.737947936093));
#70185=CARTESIAN_POINT('Ctrl Pts',(81.0125321908413,10.323212481663,137.729257585613));
#70186=CARTESIAN_POINT('Ctrl Pts',(81.031171164287,10.3087394079502,137.727648510103));
#70187=CARTESIAN_POINT('Ctrl Pts',(81.058916096021,10.2862347312287,137.725235906644));
#70188=CARTESIAN_POINT('Ctrl Pts',(81.0682514393932,10.2784920640967,137.724421033757));
#70189=CARTESIAN_POINT('Ctrl Pts',(81.0849174965081,10.2643593506877,137.722960304602));
#70190=CARTESIAN_POINT('Ctrl Pts',(81.0922783077409,10.2580058216151,137.722313003266));
#70191=CARTESIAN_POINT('Ctrl Pts',(81.1079340706472,10.2442514450235,137.720931366033));
#70192=CARTESIAN_POINT('Ctrl Pts',(81.1162114601229,10.236831253529,137.720197875534));
#70193=CARTESIAN_POINT('Ctrl Pts',(81.1387318021035,10.2162328630918,137.718193383288));
#70194=CARTESIAN_POINT('Ctrl Pts',(81.152820052104,10.2028875562101,137.716929488585));
#70195=CARTESIAN_POINT('Ctrl Pts',(81.1836870087352,10.1726078398235,137.714134854323));
#70196=CARTESIAN_POINT('Ctrl Pts',(81.2003420349938,10.1555531855752,137.712609416785));
#70197=CARTESIAN_POINT('Ctrl Pts',(81.2525450193666,10.0997506005858,137.70776067334));
#70198=CARTESIAN_POINT('Ctrl Pts',(81.2866279749678,10.0596742360916,137.704491269499));
#70199=CARTESIAN_POINT('Ctrl Pts',(81.3774118913886,9.94207472581671,137.695345841588));
#70200=CARTESIAN_POINT('Ctrl Pts',(81.4293852737237,9.86117632790724,137.689570494069));
#70201=CARTESIAN_POINT('Ctrl Pts',(81.4981227772977,9.73064464780243,137.680393420181));
#70202=CARTESIAN_POINT('Ctrl Pts',(81.5200097938617,9.68394631594964,137.677133030546));
#70203=CARTESIAN_POINT('Ctrl Pts',(81.5438938451707,9.62615385919302,137.673036999861));
#70204=CARTESIAN_POINT('Ctrl Pts',(81.5479919678399,9.61595268662903,137.672311733463));
#70205=CARTESIAN_POINT('Ctrl Pts',(81.5542779886716,9.59984629841822,137.671161952565));
#70206=CARTESIAN_POINT('Ctrl Pts',(81.5565339582423,9.59396774437959,137.670741330847));
#70207=CARTESIAN_POINT('Ctrl Pts',(81.5607012833398,9.58292182896472,137.66994890269));
#70208=CARTESIAN_POINT('Ctrl Pts',(81.5626203961725,9.57775760352184,137.669577556394));
#70209=CARTESIAN_POINT('Ctrl Pts',(81.5670712353594,9.56559624535191,137.668701108659));
#70210=CARTESIAN_POINT('Ctrl Pts',(81.5695817342217,9.55859157150085,137.668194797296));
#70211=CARTESIAN_POINT('Ctrl Pts',(81.5777465593237,9.53532079435447,137.666508337432));
#70212=CARTESIAN_POINT('Ctrl Pts',(81.5831953865827,9.51898445876916,137.6653173312));
#70213=CARTESIAN_POINT('Ctrl Pts',(81.5958641434518,9.47894421199637,137.662385814406));
#70214=CARTESIAN_POINT('Ctrl Pts',(81.6028102189478,9.45515842657444,137.660633931746));
#70215=CARTESIAN_POINT('Ctrl Pts',(81.6297523872076,9.35461773490232,137.653208624139));
#70216=CARTESIAN_POINT('Ctrl Pts',(81.6447841101506,9.27664229544041,137.647406286896));
#70217=CARTESIAN_POINT('Ctrl Pts',(81.6664020734281,9.09593859837252,137.634180006056));
#70218=CARTESIAN_POINT('Ctrl Pts',(81.6691489838036,8.99305708989231,137.62681951096));
#70219=CARTESIAN_POINT('Ctrl Pts',(81.6608518954632,8.86702007947374,137.618124293289));
#70220=CARTESIAN_POINT('Ctrl Pts',(81.6588020259686,8.84351161250257,137.616515263834));
#70221=CARTESIAN_POINT('Ctrl Pts',(81.6549434674822,8.80799687927613,137.614102715043));
#70222=CARTESIAN_POINT('Ctrl Pts',(81.6535019120037,8.79595461430971,137.613287851536));
#70223=CARTESIAN_POINT('Ctrl Pts',(81.6506679017083,8.77428774963148,137.611827132523));
#70224=CARTESIAN_POINT('Ctrl Pts',(81.6493224477173,8.76465767055056,137.611179832034));
#70225=CARTESIAN_POINT('Ctrl Pts',(81.646258296431,8.74404456072636,137.609798189491));
#70226=CARTESIAN_POINT('Ctrl Pts',(81.6445138201669,8.7330657930999,137.609064692901));
#70227=CARTESIAN_POINT('Ctrl Pts',(81.6394229111241,8.70297301421987,137.607060165533));
#70228=CARTESIAN_POINT('Ctrl Pts',(81.6358521643053,8.68389834012931,137.605796242225));
#70229=CARTESIAN_POINT('Ctrl Pts',(81.6271545090234,8.64154174850958,137.60300153518));
#70230=CARTESIAN_POINT('Ctrl Pts',(81.6218594829965,8.61829852407933,137.601476053899));
#70231=CARTESIAN_POINT('Ctrl Pts',(81.6032907977022,8.54417187390974,137.596627118047));
#70232=CARTESIAN_POINT('Ctrl Pts',(81.5881062991737,8.49379878635708,137.593357570595));
#70233=CARTESIAN_POINT('Ctrl Pts',(81.5385449084026,8.35374328700117,137.584212050977));
#70234=CARTESIAN_POINT('Ctrl Pts',(81.4987685533963,8.26620192264929,137.57843674328));
#70235=CARTESIAN_POINT('Ctrl Pts',(81.4263874947732,8.13765907838286,137.569259877718));
#70236=CARTESIAN_POINT('Ctrl Pts',(81.3990272130029,8.09394542818712,137.565999668745));
#70237=CARTESIAN_POINT('Ctrl Pts',(81.3634298489296,8.04253673466349,137.561903840873));
#70238=CARTESIAN_POINT('Ctrl Pts',(81.357082326405,8.03356096886301,137.561178583639));
#70239=CARTESIAN_POINT('Ctrl Pts',(81.3469603297793,8.01954422976199,137.560028814107));
#70240=CARTESIAN_POINT('Ctrl Pts',(81.3432451735803,8.01446052957018,137.559608194465));
#70241=CARTESIAN_POINT('Ctrl Pts',(81.3362254231235,8.00496835568891,137.558815767872));
#70242=CARTESIAN_POINT('Ctrl Pts',(81.3329276705251,8.00055506595402,137.558444421038));
#70243=CARTESIAN_POINT('Ctrl Pts',(81.325124518436,7.99021963727935,137.557567968835));
#70244=CARTESIAN_POINT('Ctrl Pts',(81.3206012694709,7.98431124251789,137.557061653504));
#70245=CARTESIAN_POINT('Ctrl Pts',(81.3054789153626,7.96482978627866,137.555375166562));
#70246=CARTESIAN_POINT('Ctrl Pts',(81.2947093396599,7.951391284682,137.554184136761));
#70247=CARTESIAN_POINT('Ctrl Pts',(81.2679408337498,7.919030066635,137.551252549849));
#70248=CARTESIAN_POINT('Ctrl Pts',(81.2517245712348,7.90029302940611,137.549500619978));
#70249=CARTESIAN_POINT('Ctrl Pts',(81.1818666631113,7.82312345585774,137.542074977754));
#70250=CARTESIAN_POINT('Ctrl Pts',(81.1245066502778,7.76820003645204,137.536272343468));
#70251=CARTESIAN_POINT('Ctrl Pts',(80.9844165234301,7.65202999601314,137.523046162218));
#70252=CARTESIAN_POINT('Ctrl Pts',(80.8994762689304,7.59392464172677,137.515686053372));
#70253=CARTESIAN_POINT('Ctrl Pts',(80.7890927180304,7.53253778157291,137.506991188015));
#70254=CARTESIAN_POINT('Ctrl Pts',(80.7682306276826,7.52150939072891,137.505382155263));
#70255=CARTESIAN_POINT('Ctrl Pts',(80.7363006692908,7.50548857362456,137.502969602562));
#70256=CARTESIAN_POINT('Ctrl Pts',(80.7254016843756,7.5001681797742,137.502154738387));
#70257=CARTESIAN_POINT('Ctrl Pts',(80.705661514236,7.49079743936208,137.500694018656));
#70258=CARTESIAN_POINT('Ctrl Pts',(80.6968412180264,7.48670463377182,137.500046718111));
#70259=CARTESIAN_POINT('Ctrl Pts',(80.677861533278,7.47809878539718,137.49866507596));
#70260=CARTESIAN_POINT('Ctrl Pts',(80.6676917443785,7.47360971246924,137.497931579813));
#70261=CARTESIAN_POINT('Ctrl Pts',(80.6396486332997,7.46156503664912,137.495927054985));
#70262=CARTESIAN_POINT('Ctrl Pts',(80.6216866964267,7.45421922218457,137.494663133743));
#70263=CARTESIAN_POINT('Ctrl Pts',(80.581384165052,7.43855305421675,137.491868431954));
#70264=CARTESIAN_POINT('Ctrl Pts',(80.5589848945867,7.4303949272185,137.490342953831));
#70265=CARTESIAN_POINT('Ctrl Pts',(80.4866375721685,7.4057903156756,137.485494031866));
#70266=CARTESIAN_POINT('Ctrl Pts',(80.436081874529,7.39122597404735,137.482224494779));
#70267=CARTESIAN_POINT('Ctrl Pts',(80.291535630357,7.35690074541331,137.473078981691));
#70268=CARTESIAN_POINT('Ctrl Pts',(80.1964152774299,7.34283741180767,137.467303671037));
#70269=CARTESIAN_POINT('Ctrl Pts',(80.049163857556,7.33392794644519,137.45812679033));
#70270=CARTESIAN_POINT('Ctrl Pts',(79.9975986803697,7.33320478592516,137.454866568298));
#70271=CARTESIAN_POINT('Ctrl Pts',(79.9351010014767,7.33522825058939,137.450770725768));
#70272=CARTESIAN_POINT('Ctrl Pts',(79.9241173822381,7.33569273567307,137.450045467875));
#70273=CARTESIAN_POINT('Ctrl Pts',(79.9068514718617,7.33659415681977,137.448895697529));
#70274=CARTESIAN_POINT('Ctrl Pts',(79.9005654573009,7.33695808355034,137.448475077741));
#70275=CARTESIAN_POINT('Ctrl Pts',(79.8887833918301,7.33770723979103,137.447682651039));
#70276=CARTESIAN_POINT('Ctrl Pts',(79.8832870055806,7.33808410923743,137.447311304246));
#70277=CARTESIAN_POINT('Ctrl Pts',(79.870371598657,7.33903406181835,137.446434852372));
#70278=CARTESIAN_POINT('Ctrl Pts',(79.8629544437138,7.33962959540837,137.445928537331));
#70279=CARTESIAN_POINT('Ctrl Pts',(79.8383853890871,7.34176802390877,137.444242052367));
#70280=CARTESIAN_POINT('Ctrl Pts',(79.8212540776608,7.34352711870955,137.443051024286));
#70281=CARTESIAN_POINT('Ctrl Pts',(79.7795477081114,7.34846412712838,137.440119442494));
#70282=CARTESIAN_POINT('Ctrl Pts',(79.7550107682784,7.35192533621856,137.438367516069));
#70283=CARTESIAN_POINT('Ctrl Pts',(79.6522888318208,7.36875994801261,137.430941898269));
#70284=CARTESIAN_POINT('Ctrl Pts',(79.5750351830167,7.38716051164576,137.425139285665));
#70285=CARTESIAN_POINT('Ctrl Pts',(79.4015807794382,7.44180668854913,137.411922708435));
#70286=CARTESIAN_POINT('Ctrl Pts',(79.3068122953559,7.48158991550364,137.404571845428));
#70287=CARTESIAN_POINT('Ctrl Pts',(79.1953997081614,7.54098152746416,137.395879555419));
#70288=CARTESIAN_POINT('Ctrl Pts',(79.1747461884986,7.55256337641308,137.394264843608));
#70289=CARTESIAN_POINT('Ctrl Pts',(79.1438820430329,7.57074651293147,137.391845550211));
#70290=CARTESIAN_POINT('Ctrl Pts',(79.1334859649914,7.57702532446266,137.391029529376));
#70291=CARTESIAN_POINT('Ctrl Pts',(79.1148905181638,7.58853559284854,137.38956755723));
#70292=CARTESIAN_POINT('Ctrl Pts',(79.1066666315337,7.59372617632354,137.388920150257));
#70293=CARTESIAN_POINT('Ctrl Pts',(79.0908010514225,7.60393523127913,137.387669294185));
#70294=CARTESIAN_POINT('Ctrl Pts',(79.0831543084549,7.60894516640444,137.387065559858));
#70295=CARTESIAN_POINT('Ctrl Pts',(79.0613035831744,7.62351961376397,137.385337573908));
#70296=CARTESIAN_POINT('Ctrl Pts',(79.0472050347962,7.63324069184258,137.384219211252));
#70297=CARTESIAN_POINT('Ctrl Pts',(78.9801076315827,7.68104787299922,137.378875786567));
#70298=CARTESIAN_POINT('Ctrl Pts',(78.9292242924007,7.72201094963783,137.374762688965));
#70299=CARTESIAN_POINT('Ctrl Pts',(78.8264135681483,7.81524048778105,137.366159302839));
#70300=CARTESIAN_POINT('Ctrl Pts',(78.7752832935954,7.86817423451628,137.361697125596));
#70301=CARTESIAN_POINT('Ctrl Pts',(78.7157297954127,7.93860636357451,137.356054407551));
#70302=CARTESIAN_POINT('Ctrl Pts',(78.7038852369026,7.95310319767985,137.354907078642));
#70303=CARTESIAN_POINT('Ctrl Pts',(78.6490951958397,8.02251742219506,137.349464305369));
#70304=CARTESIAN_POINT('Ctrl Pts',(78.6093852501464,8.07988904640922,137.345114750604));
#70305=CARTESIAN_POINT('Ctrl Pts',(78.567418680568,8.14947050178401,137.339799275742));
#70306=CARTESIAN_POINT('Ctrl Pts',(78.5615510904945,8.15943210830667,137.339037337228));
#70307=CARTESIAN_POINT('Ctrl Pts',(78.5525852701964,8.17502250403875,137.33784209163));
#70308=CARTESIAN_POINT('Ctrl Pts',(78.5494149920936,8.18060973872479,137.337413195881));
#70309=CARTESIAN_POINT('Ctrl Pts',(78.5436229645985,8.19095645574832,137.336617672193));
#70310=CARTESIAN_POINT('Ctrl Pts',(78.5409920890399,8.19571060035635,137.336251627882));
#70311=CARTESIAN_POINT('Ctrl Pts',(78.5349285124989,8.20679548813728,137.335397003523));
#70312=CARTESIAN_POINT('Ctrl Pts',(78.5315135705612,8.21313567696747,137.334907345496));
#70313=CARTESIAN_POINT('Ctrl Pts',(78.5207105506204,8.23350785641826,137.333331779417));
#70314=CARTESIAN_POINT('Ctrl Pts',(78.5134819306624,8.2476227907738,137.332236818073));
#70315=CARTESIAN_POINT('Ctrl Pts',(78.4744667230697,8.32656335934003,137.326103332673));
#70316=CARTESIAN_POINT('Ctrl Pts',(78.4467215596323,8.39329354004269,137.320885898191));
#70317=CARTESIAN_POINT('Ctrl Pts',(78.3781212144582,8.59417900957207,137.305451726776));
#70318=CARTESIAN_POINT('Ctrl Pts',(78.3497413654723,8.7319640815458,137.295262916405));
#70319=CARTESIAN_POINT('Ctrl Pts',(78.3373025928241,8.89299608217247,137.284174441421));
#70320=CARTESIAN_POINT('Ctrl Pts',(78.3360669841584,8.91432912615348,137.28272012647));
#70321=CARTESIAN_POINT('Ctrl Pts',(78.3347977471238,8.94718053836917,137.280502133071));
#70322=CARTESIAN_POINT('Ctrl Pts',(78.3344726075072,8.95868468939974,137.279729470816));
#70323=CARTESIAN_POINT('Ctrl Pts',(78.3341612575565,8.97608330710807,137.278566801402));
#70324=CARTESIAN_POINT('Ctrl Pts',(78.3340870825413,8.98197565526008,137.27817406287));
#70325=CARTESIAN_POINT('Ctrl Pts',(78.3340147926857,8.99190271330143,137.277514077583));
#70326=CARTESIAN_POINT('Ctrl Pts',(78.3340000686845,8.99593720572022,137.277246316743));
#70327=CARTESIAN_POINT('Ctrl Pts',(78.3340000002397,8.99997173673522,137.276979010776));
#70328=CARTESIAN_POINT('Ctrl Pts',(78.3340000002429,8.99997155004477,137.276979023145));
#70329=CARTESIAN_POINT('Ctrl Pts',(78.3339999112415,9.00518337813501,137.276633715891));
#70330=CARTESIAN_POINT('Ctrl Pts',(78.3340242788548,9.01039523950057,137.276289169831));
#70331=CARTESIAN_POINT('Ctrl Pts',(78.3341549983631,9.02434857171807,137.275368731287));
#70332=CARTESIAN_POINT('Ctrl Pts',(78.3343056973382,9.03308953525333,137.274794220308));
#70333=CARTESIAN_POINT('Ctrl Pts',(78.3350293907745,9.06190427622381,137.2729068771));
#70334=CARTESIAN_POINT('Ctrl Pts',(78.3358965351355,9.08196940223928,137.271603123381));
#70335=CARTESIAN_POINT('Ctrl Pts',(78.3432383809184,9.20164398891471,137.263880528597));
#70336=CARTESIAN_POINT('Ctrl Pts',(78.3582917109302,9.30052728128795,137.257736897948));
#70337=CARTESIAN_POINT('Ctrl Pts',(78.3969323077997,9.45780953315502,137.247839398521));
#70338=CARTESIAN_POINT('Ctrl Pts',(78.4151125289883,9.51724486873033,137.244064136938));
#70339=CARTESIAN_POINT('Ctrl Pts',(78.4365593610394,9.57550792214055,137.240217191853));
#70340=CARTESIAN_POINT('',(78.3340007164138,9.00153000900957,137.471592617802));
#70341=CARTESIAN_POINT('Ctrl Pts',(78.4365593900224,9.5755080008764,137.430947520545));
#70342=CARTESIAN_POINT('Ctrl Pts',(78.4254741421113,9.54539351640444,137.432961692578));
#70343=CARTESIAN_POINT('Ctrl Pts',(78.4152578407775,9.51495565961625,137.435002791709));
#70344=CARTESIAN_POINT('Ctrl Pts',(78.401326629796,9.46909459877583,137.43811228276));
#70345=CARTESIAN_POINT('Ctrl Pts',(78.396944381392,9.45389307791809,137.439148496163));
#70346=CARTESIAN_POINT('Ctrl Pts',(78.3909056497913,9.43176616931305,137.440667851912));
#70347=CARTESIAN_POINT('Ctrl Pts',(78.3890758906659,9.42488841146042,137.441141656688));
#70348=CARTESIAN_POINT('Ctrl Pts',(78.3859140581865,9.41268954428143,137.44198509852));
#70349=CARTESIAN_POINT('Ctrl Pts',(78.3845641129672,9.40737327005085,137.442353711423));
#70350=CARTESIAN_POINT('Ctrl Pts',(78.3816919415351,9.39582344462313,137.443156890438));
#70351=CARTESIAN_POINT('Ctrl Pts',(78.3801794888434,9.38958783293473,137.443591967108));
#70352=CARTESIAN_POINT('Ctrl Pts',(78.3771195253297,9.37664616117294,137.44449772603));
#70353=CARTESIAN_POINT('Ctrl Pts',(78.3755774747087,9.3699389423902,137.444968691075));
#70354=CARTESIAN_POINT('Ctrl Pts',(78.3716952592679,9.35256066034583,137.446192601775));
#70355=CARTESIAN_POINT('Ctrl Pts',(78.369418460985,9.34187596857764,137.446948646952));
#70356=CARTESIAN_POINT('Ctrl Pts',(78.345237229499,9.22265629376286,137.45541838206));
#70357=CARTESIAN_POINT('Ctrl Pts',(78.3341023880633,9.11223104855113,137.463553888552));
#70358=CARTESIAN_POINT('Ctrl Pts',(78.3340007028448,9.00153031966764,137.471592615215));
#70359=CARTESIAN_POINT('Ctrl Pts',(78.3340007025608,9.00153001046496,137.471592637669));
#70360=CARTESIAN_POINT('Ctrl Pts',(78.3339287513718,8.92318372917125,137.47728188952));
#70361=CARTESIAN_POINT('Ctrl Pts',(78.3393833622202,8.84492220646431,137.482910887098));
#70362=CARTESIAN_POINT('Ctrl Pts',(78.3549525496431,8.73453511273653,137.490701819754));
#70363=CARTESIAN_POINT('Ctrl Pts',(78.3605546094469,8.70188626702482,137.492988332332));
#70364=CARTESIAN_POINT('Ctrl Pts',(78.3695663929548,8.65737273930555,137.49608242935));
#70365=CARTESIAN_POINT('Ctrl Pts',(78.3721395827095,8.64534853356166,137.496915889869));
#70366=CARTESIAN_POINT('Ctrl Pts',(78.3769359582418,8.62408867414977,137.498385630189));
#70367=CARTESIAN_POINT('Ctrl Pts',(78.3791054258978,8.61484159793951,137.499023588584));
#70368=CARTESIAN_POINT('Ctrl Pts',(78.3836666407023,8.59612140612928,137.500312608937));
#70369=CARTESIAN_POINT('Ctrl Pts',(78.3860628785508,8.58664975872747,137.500963498353));
#70370=CARTESIAN_POINT('Ctrl Pts',(78.391287589648,8.56673634341967,137.502329436818));
#70371=CARTESIAN_POINT('Ctrl Pts',(78.3941347336951,8.55629990859409,137.503043850255));
#70372=CARTESIAN_POINT('Ctrl Pts',(78.4019934698906,8.52856005056862,137.504939337139));
#70373=CARTESIAN_POINT('Ctrl Pts',(78.40718448228,8.51130862107592,137.506114569891));
#70374=CARTESIAN_POINT('Ctrl Pts',(78.4343862111914,8.42595120347724,137.511916816552));
#70375=CARTESIAN_POINT('Ctrl Pts',(78.46049114693,8.35922478435311,137.516407989382));
#70376=CARTESIAN_POINT('Ctrl Pts',(78.5371894315996,8.1951819621097,137.52759031137));
#70377=CARTESIAN_POINT('Ctrl Pts',(78.5932321632432,8.10080659771329,137.534149370386));
#70378=CARTESIAN_POINT('Ctrl Pts',(78.6841730731729,7.97721594606461,137.543736304128));
#70379=CARTESIAN_POINT('Ctrl Pts',(78.711609931341,7.9428632827288,137.54652636555));
#70380=CARTESIAN_POINT('Ctrl Pts',(78.7479791615948,7.90084805569639,137.550159052374));
#70381=CARTESIAN_POINT('Ctrl Pts',(78.7556800360156,7.89213765062358,137.550924784073));
#70382=CARTESIAN_POINT('Ctrl Pts',(78.767867220488,7.87864018135803,137.552132599807));
#70383=CARTESIAN_POINT('Ctrl Pts',(78.7722918866621,7.87379761410806,137.55257030158));
#70384=CARTESIAN_POINT('Ctrl Pts',(78.7804577469815,7.86496581416413,137.553376906155));
#70385=CARTESIAN_POINT('Ctrl Pts',(78.7841901274287,7.86096871823972,137.5537451566));
#70386=CARTESIAN_POINT('Ctrl Pts',(78.7927722180932,7.85186819306799,137.554590910183));
#70387=CARTESIAN_POINT('Ctrl Pts',(78.7976346243268,7.84677709771279,137.555069356436));
#70388=CARTESIAN_POINT('Ctrl Pts',(78.812949288948,7.83094429383044,137.556573545334));
#70389=CARTESIAN_POINT('Ctrl Pts',(78.8235139908239,7.82031306444383,137.557607268595));
#70390=CARTESIAN_POINT('Ctrl Pts',(78.9091693881078,7.73641326926946,137.565946867398));
#70391=CARTESIAN_POINT('Ctrl Pts',(78.9908790518476,7.67025030826881,137.573635216038));
#70392=CARTESIAN_POINT('Ctrl Pts',(79.1721446481223,7.54985705249177,137.58945608513));
#70393=CARTESIAN_POINT('Ctrl Pts',(79.272131820779,7.49717740518232,137.597530761659));
#70394=CARTESIAN_POINT('Ctrl Pts',(79.3947319766863,7.44771616568219,137.606577657256));
#70395=CARTESIAN_POINT('Ctrl Pts',(79.4129004286917,7.44075382592577,137.607898495035));
#70396=CARTESIAN_POINT('Ctrl Pts',(79.4416437058296,7.43031276647969,137.609957963222));
#70397=CARTESIAN_POINT('Ctrl Pts',(79.4521380532596,7.4266192259896,137.61070366208));
#70398=CARTESIAN_POINT('Ctrl Pts',(79.4718686805701,7.41989627774148,137.612094317371));
#70399=CARTESIAN_POINT('Ctrl Pts',(79.481095943743,7.41684206381599,137.612740068047));
#70400=CARTESIAN_POINT('Ctrl Pts',(79.5018762998957,7.41016498895068,137.614184294179));
#70401=CARTESIAN_POINT('Ctrl Pts',(79.513443300426,7.40658694181847,137.61498127468));
#70402=CARTESIAN_POINT('Ctrl Pts',(79.5475774495274,7.39643450794926,137.617313683611));
#70403=CARTESIAN_POINT('Ctrl Pts',(79.5702464859399,7.39021105195353,137.618837761028));
#70404=CARTESIAN_POINT('Ctrl Pts',(79.6830467970281,7.3617961508521,137.626311547409));
#70405=CARTESIAN_POINT('Ctrl Pts',(79.7747948485177,7.34668313218989,137.632034142422));
#70406=CARTESIAN_POINT('Ctrl Pts',(79.9437118458753,7.33318910940777,137.642395696399));
#70407=CARTESIAN_POINT('Ctrl Pts',(80.0204164978586,7.33236425947121,137.647040535184));
#70408=CARTESIAN_POINT('Ctrl Pts',(80.1292101070493,7.3387028727825,137.653841168167));
#70409=CARTESIAN_POINT('Ctrl Pts',(80.1614551903792,7.3415261947357,137.655884159614));
#70410=CARTESIAN_POINT('Ctrl Pts',(80.2143589252237,7.34771574145885,137.659310584514));
#70411=CARTESIAN_POINT('Ctrl Pts',(80.2350736061321,7.3505354438978,137.660671196879));
#70412=CARTESIAN_POINT('Ctrl Pts',(80.2636582052659,7.35497576089786,137.662581896315));
#70413=CARTESIAN_POINT('Ctrl Pts',(80.2715786388843,7.35626479235752,137.663114869811));
#70414=CARTESIAN_POINT('Ctrl Pts',(80.285009157298,7.3585502956289,137.664025119953));
#70415=CARTESIAN_POINT('Ctrl Pts',(80.290524224223,7.35951744114007,137.664400771594));
#70416=CARTESIAN_POINT('Ctrl Pts',(80.3019657698684,7.36158338531573,137.665184157333));
#70417=CARTESIAN_POINT('Ctrl Pts',(80.3078912684435,7.36268656227587,137.66559211338));
#70418=CARTESIAN_POINT('Ctrl Pts',(80.3236871490699,7.36571613070729,137.666685384723));
#70419=CARTESIAN_POINT('Ctrl Pts',(80.333546110018,7.36769974702247,137.667373766445));
#70420=CARTESIAN_POINT('Ctrl Pts',(80.378503331374,7.37716940001516,137.670538517282));
#70421=CARTESIAN_POINT('Ctrl Pts',(80.4133694492256,7.3856985426999,137.673064548523));
#70422=CARTESIAN_POINT('Ctrl Pts',(80.5397860150075,7.42098699538215,137.682424452084));
#70423=CARTESIAN_POINT('Ctrl Pts',(80.6292683281143,7.45446713406057,137.689430037614));
#70424=CARTESIAN_POINT('Ctrl Pts',(80.8021709727264,7.53667825828746,137.703292062072));
#70425=CARTESIAN_POINT('Ctrl Pts',(80.8852284541493,7.58537458060474,137.710119491605));
#70426=CARTESIAN_POINT('Ctrl Pts',(80.9788302865691,7.6517440023957,137.717962194055));
#70427=CARTESIAN_POINT('Ctrl Pts',(80.9938439023537,7.66277252809275,137.719225694971));
#70428=CARTESIAN_POINT('Ctrl Pts',(81.017383868299,7.68067974389455,137.721216415677));
#70429=CARTESIAN_POINT('Ctrl Pts',(81.0260324088749,7.68739443110717,137.721949938113));
#70430=CARTESIAN_POINT('Ctrl Pts',(81.0422513000252,7.70024495962461,137.723329872008));
#70431=CARTESIAN_POINT('Ctrl Pts',(81.0498351960297,7.70636287721292,137.723976955361));
#70432=CARTESIAN_POINT('Ctrl Pts',(81.0669304055423,7.72040290784581,137.725440040069));
#70433=CARTESIAN_POINT('Ctrl Pts',(81.0764080507875,7.7283652527157,137.726254373629));
#70434=CARTESIAN_POINT('Ctrl Pts',(81.1053015397203,7.75319372240697,137.728747786565));
#70435=CARTESIAN_POINT('Ctrl Pts',(81.1244168571189,7.77040484955706,137.730412662811));
#70436=CARTESIAN_POINT('Ctrl Pts',(81.2404340440021,7.87983397813105,137.740635202132));
#70437=CARTESIAN_POINT('Ctrl Pts',(81.3263327863133,7.98299817522528,137.748679835144));
#70438=CARTESIAN_POINT('Ctrl Pts',(81.4381964934003,8.15598342027225,137.761314867289));
#70439=CARTESIAN_POINT('Ctrl Pts',(81.473428334307,8.21911608842373,137.765789522364));
#70440=CARTESIAN_POINT('Ctrl Pts',(81.5112621464553,8.29864827394566,137.771502842678));
#70441=CARTESIAN_POINT('Ctrl Pts',(81.5178697891846,8.31306566758462,137.772541547719));
#70442=CARTESIAN_POINT('Ctrl Pts',(81.5271765651335,8.33416249251169,137.774068965174));
#70443=CARTESIAN_POINT('Ctrl Pts',(81.5300400073809,8.34076907042324,137.774548339349));
#70444=CARTESIAN_POINT('Ctrl Pts',(81.5350076882618,8.35243730498534,137.775397199345));
#70445=CARTESIAN_POINT('Ctrl Pts',(81.5371299066947,8.35749109295909,137.775765599455));
#70446=CARTESIAN_POINT('Ctrl Pts',(81.5416921792717,8.36850753872899,137.776570348652));
#70447=CARTESIAN_POINT('Ctrl Pts',(81.544122563974,8.37447381494852,137.777007227026));
#70448=CARTESIAN_POINT('Ctrl Pts',(81.5508499438202,8.39126677958626,137.778239506254));
#70449=CARTESIAN_POINT('Ctrl Pts',(81.5550679850582,8.4021244069886,137.779039289344));
#70450=CARTESIAN_POINT('Ctrl Pts',(81.5878017294627,8.48907449138211,137.785463319868));
#70451=CARTESIAN_POINT('Ctrl Pts',(81.6108262378961,8.56710848663504,137.791340103224));
#70452=CARTESIAN_POINT('Ctrl Pts',(81.6310452013371,8.66022818212903,137.79827098935));
#70453=CARTESIAN_POINT('Ctrl Pts',(81.6338521471435,8.67399310328744,137.799293625379));
#70454=CARTESIAN_POINT('Ctrl Pts',(81.6455914630325,8.73552644289922,137.803853633398));
#70455=CARTESIAN_POINT('Ctrl Pts',(81.6526056327334,8.78363815439648,137.807387361721));
#70456=CARTESIAN_POINT('Ctrl Pts',(81.66570866662,8.91290568798445,137.816741005222));
#70457=CARTESIAN_POINT('Ctrl Pts',(81.6679754656164,8.99432400382189,137.822479946779));
#70458=CARTESIAN_POINT('Ctrl Pts',(81.6634641980402,9.09364501107874,137.829269764892));
#70459=CARTESIAN_POINT('Ctrl Pts',(81.662350622459,9.11168249155662,137.830494710364));
#70460=CARTESIAN_POINT('Ctrl Pts',(81.6601006884897,9.14049548262302,137.832439120203));
#70461=CARTESIAN_POINT('Ctrl Pts',(81.6591523447306,9.15128378339317,137.833164392343));
#70462=CARTESIAN_POINT('Ctrl Pts',(81.6571487606078,9.17178294113825,137.8345375067));
#70463=CARTESIAN_POINT('Ctrl Pts',(81.6561131865902,9.18149521698174,137.83518593514));
#70464=CARTESIAN_POINT('Ctrl Pts',(81.6535475865648,9.20370281359891,137.836663983932));
#70465=CARTESIAN_POINT('Ctrl Pts',(81.6519612191109,9.21619112454287,137.837491801894));
#70466=CARTESIAN_POINT('Ctrl Pts',(81.6474063716617,9.24906326446204,137.839662789551));
#70467=CARTESIAN_POINT('Ctrl Pts',(81.6442010948644,9.26941247645857,137.840998540815));
#70468=CARTESIAN_POINT('Ctrl Pts',(81.6186182888777,9.4142932730626,137.850462352303));
#70469=CARTESIAN_POINT('Ctrl Pts',(81.5824965813417,9.53597810194223,137.858124406919));
#70470=CARTESIAN_POINT('Ctrl Pts',(81.4979964629142,9.73452480618185,137.871319775353));
#70471=CARTESIAN_POINT('Ctrl Pts',(81.4565123747977,9.81368752299305,137.87680683921));
#70472=CARTESIAN_POINT('Ctrl Pts',(81.4022259737074,9.89970805908838,137.883449050135));
#70473=CARTESIAN_POINT('Ctrl Pts',(81.395435760577,9.91020398158919,137.884271877212));
#70474=CARTESIAN_POINT('Ctrl Pts',(81.3849085623913,9.92608162862454,137.885537202478));
#70475=CARTESIAN_POINT('Ctrl Pts',(81.3812567023457,9.93151963351911,137.885974308671));
#70476=CARTESIAN_POINT('Ctrl Pts',(81.3744968329581,9.94145864187024,137.886780373674));
#70477=CARTESIAN_POINT('Ctrl Pts',(81.3713986110425,9.94596604850566,137.887148686581));
#70478=CARTESIAN_POINT('Ctrl Pts',(81.3642551315529,9.9562497921903,137.887995311226));
#70479=CARTESIAN_POINT('Ctrl Pts',(81.3601953706312,9.9620157369843,137.888474573981));
#70480=CARTESIAN_POINT('Ctrl Pts',(81.3473565354114,9.98000657517159,137.889983919264));
#70481=CARTESIAN_POINT('Ctrl Pts',(81.3384486144671,9.992137988303,137.891022057793));
#70482=CARTESIAN_POINT('Ctrl Pts',(81.2667091256282,10.0871130683613,137.899301629979));
#70483=CARTESIAN_POINT('Ctrl Pts',(81.1964164928546,10.1640235873545,137.906918442772));
#70484=CARTESIAN_POINT('Ctrl Pts',(81.0352408581541,10.3102487629109,137.922742541798));
#70485=CARTESIAN_POINT('Ctrl Pts',(80.9434500740638,10.3778194409555,137.930888542775));
#70486=CARTESIAN_POINT('Ctrl Pts',(80.8287674670517,10.4453638055376,137.939995778718));
#70487=CARTESIAN_POINT('Ctrl Pts',(80.8118871670219,10.4549128248653,137.941312267555));
#70488=CARTESIAN_POINT('Ctrl Pts',(80.7850779599095,10.4694665914661,137.943366527283));
#70489=CARTESIAN_POINT('Ctrl Pts',(80.7752595745072,10.4746701560225,137.944111307281));
#70490=CARTESIAN_POINT('Ctrl Pts',(80.7567555227279,10.4842410757629,137.945501129611));
#70491=CARTESIAN_POINT('Ctrl Pts',(80.7480823187248,10.4886313658591,137.946146957093));
#70492=CARTESIAN_POINT('Ctrl Pts',(80.7285044915405,10.4983271501057,137.947592489253));
#70493=CARTESIAN_POINT('Ctrl Pts',(80.7175792934883,10.5035900416917,137.948390686852));
#70494=CARTESIAN_POINT('Ctrl Pts',(80.6852284939717,10.5187411552836,137.950730253628));
#70495=CARTESIAN_POINT('Ctrl Pts',(80.6636486154599,10.5282942748456,137.95226016427));
#70496=CARTESIAN_POINT('Ctrl Pts',(80.5475559826864,10.5767639656207,137.960342116054));
#70497=CARTESIAN_POINT('Ctrl Pts',(80.4498125073947,10.6073811523825,137.966611684753));
#70498=CARTESIAN_POINT('Ctrl Pts',(80.2719511564401,10.6455849840024,137.977722604372));
#70499=CARTESIAN_POINT('Ctrl Pts',(80.1929377981737,10.6567077628697,137.982565383274));
#70500=CARTESIAN_POINT('Ctrl Pts',(80.08865782956,10.6638247270237,137.989155191184));
#70501=CARTESIAN_POINT('Ctrl Pts',(80.06384390888,10.6649614883015,137.990738248872));
#70502=CARTESIAN_POINT('Ctrl Pts',(80.0217687601418,10.6659470953656,137.993461717335));
#70503=CARTESIAN_POINT('Ctrl Pts',(80.0045178912742,10.66608317173,137.994589502206));
#70504=CARTESIAN_POINT('Ctrl Pts',(79.979824035363,10.6658944621728,137.996223827633));
#70505=CARTESIAN_POINT('Ctrl Pts',(79.9723798522388,10.6657876667918,137.996719106262));
#70506=CARTESIAN_POINT('Ctrl Pts',(79.9594293769094,10.6655150464119,137.997585639382));
#70507=CARTESIAN_POINT('Ctrl Pts',(79.9539227914281,10.6653718008705,137.997955646565));
#70508=CARTESIAN_POINT('Ctrl Pts',(79.9421285358687,10.6650064488473,137.998751598054));
#70509=CARTESIAN_POINT('Ctrl Pts',(79.93584148749,10.6647760399084,137.999177960879));
#70510=CARTESIAN_POINT('Ctrl Pts',(79.9185910485487,10.6640459815483,138.000353232378));
#70511=CARTESIAN_POINT('Ctrl Pts',(79.9076312849937,10.663473609809,138.001105925484));
#70512=CARTESIAN_POINT('Ctrl Pts',(79.8455854960802,10.6596182451507,138.005398170394));
#70513=CARTESIAN_POINT('Ctrl Pts',(79.7946711079838,10.6540905455986,138.009039077295));
#70514=CARTESIAN_POINT('Ctrl Pts',(79.6484020627057,10.631353365934,138.019704308045));
#70515=CARTESIAN_POINT('Ctrl Pts',(79.554184957195,10.6081619860541,138.026818643538));
#70516=CARTESIAN_POINT('Ctrl Pts',(79.4130223831853,10.5600471704601,138.037541472249));
#70517=CARTESIAN_POINT('Ctrl Pts',(79.3643495247312,10.5408566599295,138.041254083757));
#70518=CARTESIAN_POINT('Ctrl Pts',(79.2949977090718,10.5096660990511,138.046553032325));
#70519=CARTESIAN_POINT('Ctrl Pts',(79.2735493110557,10.4994630556862,138.048193373808));
#70520=CARTESIAN_POINT('Ctrl Pts',(79.2350357843055,10.4801216409016,138.051142183353));
#70521=CARTESIAN_POINT('Ctrl Pts',(79.2178981042715,10.4711379957743,138.052455592176));
#70522=CARTESIAN_POINT('Ctrl Pts',(79.1911784230002,10.4565324966649,138.054506162777));
#70523=CARTESIAN_POINT('Ctrl Pts',(79.1814899617597,10.4511101215595,138.055250291754));
#70524=CARTESIAN_POINT('Ctrl Pts',(79.1634206093619,10.4407586322126,138.056639526508));
#70525=CARTESIAN_POINT('Ctrl Pts',(79.1550273102227,10.4358522464081,138.057285410977));
#70526=CARTESIAN_POINT('Ctrl Pts',(79.1362508773537,10.4246546339289,138.058731880603));
#70527=CARTESIAN_POINT('Ctrl Pts',(79.1258925211453,10.4183227775366,138.059530949999));
#70528=CARTESIAN_POINT('Ctrl Pts',(79.095551065719,10.3993169870543,138.061875649637));
#70529=CARTESIAN_POINT('Ctrl Pts',(79.0757671930687,10.3863295834404,138.063409743942));
#70530=CARTESIAN_POINT('Ctrl Pts',(78.9739598577287,10.3163482767935,138.071345537865));
#70531=CARTESIAN_POINT('Ctrl Pts',(78.8969042495098,10.2524831793467,138.077479404025));
#70532=CARTESIAN_POINT('Ctrl Pts',(78.7682487685487,10.1247114646343,138.088555960527));
#70533=CARTESIAN_POINT('Ctrl Pts',(78.7147591971933,10.0631750674789,138.093499383091));
#70534=CARTESIAN_POINT('Ctrl Pts',(78.6509400881766,9.97786721061838,138.100213338924));
#70535=CARTESIAN_POINT('Ctrl Pts',(78.6363511293087,9.95741764666495,138.101813627696));
#70536=CARTESIAN_POINT('Ctrl Pts',(78.6124511771225,9.9222618100677,138.10456383958));
#70537=CARTESIAN_POINT('Ctrl Pts',(78.6028979092562,9.90772477759486,138.105700809082));
#70538=CARTESIAN_POINT('Ctrl Pts',(78.589570516647,9.88673584902199,138.107346118212));
#70539=CARTESIAN_POINT('Ctrl Pts',(78.5856091176666,9.88040344168236,138.107842987693));
#70540=CARTESIAN_POINT('Ctrl Pts',(78.5787988305795,9.86935241191356,138.108711319212));
#70541=CARTESIAN_POINT('Ctrl Pts',(78.5759305606735,9.86464594549603,138.109081517776));
#70542=CARTESIAN_POINT('Ctrl Pts',(78.5698452684304,9.85454833355674,138.109876726172));
#70543=CARTESIAN_POINT('Ctrl Pts',(78.5666353998263,9.84915330201386,138.110302144389));
#70544=CARTESIAN_POINT('Ctrl Pts',(78.5579283427053,9.83432875449606,138.111472338454));
#70545=CARTESIAN_POINT('Ctrl Pts',(78.5524933254307,9.82486335028105,138.112220847355));
#70546=CARTESIAN_POINT('Ctrl Pts',(78.5227117142183,9.77179608591075,138.11642191868));
#70547=CARTESIAN_POINT('Ctrl Pts',(78.5002443780857,9.72717394337924,138.119970955635));
#70548=CARTESIAN_POINT('Ctrl Pts',(78.4641777346591,9.64673575538072,138.12631815485));
#70549=CARTESIAN_POINT('Ctrl Pts',(78.4497513016068,9.61134549370152,138.129094408613));
#70550=CARTESIAN_POINT('Ctrl Pts',(78.4365594482967,9.57550815918599,138.131873589273));
#70551=CARTESIAN_POINT('Origin',(80.,9.,134.));
#70552=CARTESIAN_POINT('',(78.4365593737687,9.57550795672114,138.833737829798));
#70553=CARTESIAN_POINT('',(78.4365593294404,9.57550783629781,138.638847722432));
#70554=CARTESIAN_POINT('',(78.4365593737638,9.57550795670799,134.));
#70555=CARTESIAN_POINT('Ctrl Pts',(78.4365593294404,9.57550783629781,138.638847722432));
#70556=CARTESIAN_POINT('Ctrl Pts',(78.4698751475928,9.66601451889556,138.631860971438));
#70557=CARTESIAN_POINT('Ctrl Pts',(78.5110043344498,9.75350400925092,138.624997573652));
#70558=CARTESIAN_POINT('Ctrl Pts',(78.56925966871,9.85376521116878,138.617062797006));
#70559=CARTESIAN_POINT('Ctrl Pts',(78.5793064228173,9.87038080542856,138.615744725277));
#70560=CARTESIAN_POINT('Ctrl Pts',(78.595560026213,9.89622986845154,138.61368844008));
#70561=CARTESIAN_POINT('Ctrl Pts',(78.6015725411225,9.90558283426176,138.612943197163));
#70562=CARTESIAN_POINT('Ctrl Pts',(78.6130177193405,9.92300091580669,138.61155275464));
#70563=CARTESIAN_POINT('Ctrl Pts',(78.6184282007808,9.93107996858373,138.610906766962));
#70564=CARTESIAN_POINT('Ctrl Pts',(78.6307436256256,9.94912590423244,138.609461184705));
#70565=CARTESIAN_POINT('Ctrl Pts',(78.6376873154159,9.95906577628718,138.608663094773));
#70566=CARTESIAN_POINT('Ctrl Pts',(78.6584519768842,9.98810973039291,138.606324798227));
#70567=CARTESIAN_POINT('Ctrl Pts',(78.6725710537013,10.0069977257062,138.604796027743));
#70568=CARTESIAN_POINT('Ctrl Pts',(78.7513426715646,10.1078384642751,138.596575410555));
#70569=CARTESIAN_POINT('Ctrl Pts',(78.8231888943482,10.1838793037918,138.590179940072));
#70570=CARTESIAN_POINT('Ctrl Pts',(78.9603567424553,10.304141881122,138.579039582531));
#70571=CARTESIAN_POINT('Ctrl Pts',(79.0225638155637,10.3513922269045,138.574293696002));
#70572=CARTESIAN_POINT('Ctrl Pts',(79.1084026561718,10.4075558902805,138.567823600148));
#70573=CARTESIAN_POINT('Ctrl Pts',(79.1292519552094,10.4205481770095,138.566257394367));
#70574=CARTESIAN_POINT('Ctrl Pts',(79.1650984130671,10.441800307635,138.563560057599));
#70575=CARTESIAN_POINT('Ctrl Pts',(79.1799499811963,10.4502988305529,138.562441234675));
#70576=CARTESIAN_POINT('Ctrl Pts',(79.2014272070227,10.4621534065749,138.560817553085));
#70577=CARTESIAN_POINT('Ctrl Pts',(79.2079490717549,10.4656965620156,138.560323754007));
#70578=CARTESIAN_POINT('Ctrl Pts',(79.2193507606788,10.4717924761891,138.559458801605));
#70579=CARTESIAN_POINT('Ctrl Pts',(79.224219912497,10.4743648064948,138.559088879836));
#70580=CARTESIAN_POINT('Ctrl Pts',(79.2346933188503,10.4798315668086,138.558291914412));
#70581=CARTESIAN_POINT('Ctrl Pts',(79.2403011901216,10.4827182798151,138.557864441443));
#70582=CARTESIAN_POINT('Ctrl Pts',(79.2557703539077,10.4905704058508,138.556683498593));
#70583=CARTESIAN_POINT('Ctrl Pts',(79.2656646161706,10.4954696348169,138.555926187831));
#70584=CARTESIAN_POINT('Ctrl Pts',(79.3227321057375,10.523024220578,138.551550041503));
#70585=CARTESIAN_POINT('Ctrl Pts',(79.3708990178427,10.5435431320813,138.547825355627));
#70586=CARTESIAN_POINT('Ctrl Pts',(79.5154078606454,10.5972152414325,138.536711882098));
#70587=CARTESIAN_POINT('Ctrl Pts',(79.6139265359875,10.6238457737905,138.529227113014));
#70588=CARTESIAN_POINT('Ctrl Pts',(79.7861823776582,10.6538342419194,138.516692139568));
#70589=CARTESIAN_POINT('Ctrl Pts',(79.8588582831123,10.6616158826775,138.511561555687));
#70590=CARTESIAN_POINT('Ctrl Pts',(79.9494358320328,10.6653258261224,138.505374865551));
#70591=CARTESIAN_POINT('Ctrl Pts',(79.967062684725,10.6657676959816,138.504180316125));
#70592=CARTESIAN_POINT('Ctrl Pts',(79.9954304593155,10.666028332329,138.502272322725));
#70593=CARTESIAN_POINT('Ctrl Pts',(80.0061679972251,10.6660231841036,138.501553450984));
#70594=CARTESIAN_POINT('Ctrl Pts',(80.0266977190896,10.665814857622,138.500185097982));
#70595=CARTESIAN_POINT('Ctrl Pts',(80.0364895890604,10.6656291378804,138.499535100863));
#70596=CARTESIAN_POINT('Ctrl Pts',(80.0588395816359,10.6650080428592,138.498057251417));
#70597=CARTESIAN_POINT('Ctrl Pts',(80.0713956557027,10.6645169130661,138.497231170131));
#70598=CARTESIAN_POINT('Ctrl Pts',(80.1049042047268,10.6628263598905,138.495036878493));
#70599=CARTESIAN_POINT('Ctrl Pts',(80.1258420023163,10.6613730011019,138.493676545403));
#70600=CARTESIAN_POINT('Ctrl Pts',(80.2674420411157,10.6488516692777,138.484537467913));
#70601=CARTESIAN_POINT('Ctrl Pts',(80.3866140790496,10.6250447616171,138.477179522494));
#70602=CARTESIAN_POINT('Ctrl Pts',(80.5651040283222,10.5686208468811,138.465740446354));
#70603=CARTESIAN_POINT('Ctrl Pts',(80.6268057216803,10.5450007293215,138.46169497969));
#70604=CARTESIAN_POINT('Ctrl Pts',(80.7073518884925,10.5085461089418,138.456098851407));
#70605=CARTESIAN_POINT('Ctrl Pts',(80.7275756528225,10.4988968030965,138.454665755171));
#70606=CARTESIAN_POINT('Ctrl Pts',(80.7618759593436,10.4816734783529,138.452176444966));
#70607=CARTESIAN_POINT('Ctrl Pts',(80.7760497639094,10.4742991527802,138.451130183467));
#70608=CARTESIAN_POINT('Ctrl Pts',(80.7964736589637,10.4632969218808,138.44959359307));
#70609=CARTESIAN_POINT('Ctrl Pts',(80.8028101492682,10.4598301375242,138.44911275806));
#70610=CARTESIAN_POINT('Ctrl Pts',(80.8138754647173,10.4536823162074,138.448265497098));
#70611=CARTESIAN_POINT('Ctrl Pts',(80.8186140150488,10.451019173433,138.447900197882));
#70612=CARTESIAN_POINT('Ctrl Pts',(80.8289118836179,10.4451651028096,138.447100826664));
#70613=CARTESIAN_POINT('Ctrl Pts',(80.8344657583841,10.4419653185167,138.446666220341));
#70614=CARTESIAN_POINT('Ctrl Pts',(80.8499296717283,10.4329367526867,138.445446647146));
#70615=CARTESIAN_POINT('Ctrl Pts',(80.8597978180775,10.4270374479311,138.444657435966));
#70616=CARTESIAN_POINT('Ctrl Pts',(80.9263981430245,10.3862813619017,138.439260270069));
#70617=CARTESIAN_POINT('Ctrl Pts',(80.9810517778842,10.348156133496,138.434481746895));
#70618=CARTESIAN_POINT('Ctrl Pts',(81.0502562035274,10.2934398789512,138.428084980723));
#70619=CARTESIAN_POINT('Ctrl Pts',(81.0669773043952,10.2796812991607,138.426510261427));
#70620=CARTESIAN_POINT('Ctrl Pts',(81.1371848469924,10.219579705752,138.419783885405));
#70621=CARTESIAN_POINT('Ctrl Pts',(81.1879605471258,10.1701772831467,138.414631882007));
#70622=CARTESIAN_POINT('Ctrl Pts',(81.2810227128656,10.0673109733487,138.404715591331));
#70623=CARTESIAN_POINT('Ctrl Pts',(81.3234830320867,10.01418278992,138.399952975223));
#70624=CARTESIAN_POINT('Ctrl Pts',(81.3725447586744,9.944445091565,138.394136853282));
#70625=CARTESIAN_POINT('Ctrl Pts',(81.3822840009549,9.93013258491287,138.392964465253));
#70626=CARTESIAN_POINT('Ctrl Pts',(81.397662282159,9.90675793808567,138.391083127421));
#70627=CARTESIAN_POINT('Ctrl Pts',(81.4034402037986,9.89778918280856,138.390369019844));
#70628=CARTESIAN_POINT('Ctrl Pts',(81.4143668755396,9.88046501591153,138.389004176543));
#70629=CARTESIAN_POINT('Ctrl Pts',(81.4195287092893,9.87211842853965,138.388352977357));
#70630=CARTESIAN_POINT('Ctrl Pts',(81.4312045339081,9.85286051276188,138.386864718679));
#70631=CARTESIAN_POINT('Ctrl Pts',(81.4376680921694,9.84191920261341,138.386029519993));
#70632=CARTESIAN_POINT('Ctrl Pts',(81.4581156391399,9.80638398624396,138.383349066478));
#70633=CARTESIAN_POINT('Ctrl Pts',(81.4715990360857,9.78150673601723,138.381521642392));
#70634=CARTESIAN_POINT('Ctrl Pts',(81.5438698071603,9.63965525522469,138.371347682696));
#70635=CARTESIAN_POINT('Ctrl Pts',(81.5893418100884,9.51641830732505,138.363477085657));
#70636=CARTESIAN_POINT('Ctrl Pts',(81.636579003702,9.31976948397194,138.351068475344));
#70637=CARTESIAN_POINT('Ctrl Pts',(81.6487655171531,9.24942593473739,138.346646775582));
#70638=CARTESIAN_POINT('Ctrl Pts',(81.6580970524159,9.16284628102584,138.340996870565));
#70639=CARTESIAN_POINT('Ctrl Pts',(81.6595643024016,9.14714288426201,138.339963783403));
#70640=CARTESIAN_POINT('Ctrl Pts',(81.6613751850065,9.12425832140393,138.338443055351));
#70641=CARTESIAN_POINT('Ctrl Pts',(81.6618956694207,9.11709148135974,138.337964636403));
#70642=CARTESIAN_POINT('Ctrl Pts',(81.6627281742232,9.10450132613928,138.337120029267));
#70643=CARTESIAN_POINT('Ctrl Pts',(81.6630600580564,9.09907951625501,138.336754943365));
#70644=CARTESIAN_POINT('Ctrl Pts',(81.6637271597607,9.08723154786881,138.335954070026));
#70645=CARTESIAN_POINT('Ctrl Pts',(81.6640516611493,9.08080513966375,138.335517730234));
#70646=CARTESIAN_POINT('Ctrl Pts',(81.6648571887898,9.06277983209842,138.334288707313));
#70647=CARTESIAN_POINT('Ctrl Pts',(81.665254208477,9.05117781458003,138.333491678512));
#70648=CARTESIAN_POINT('Ctrl Pts',(81.6673600431489,8.96254844721634,138.32736223425));
#70649=CARTESIAN_POINT('Ctrl Pts',(81.6638445707235,8.88549809884345,138.321802255384));
#70650=CARTESIAN_POINT('Ctrl Pts',(81.6484360905783,8.75199969873759,138.312034124754));
#70651=CARTESIAN_POINT('Ctrl Pts',(81.6389215378767,8.69539836439753,138.307848689915));
#70652=CARTESIAN_POINT('Ctrl Pts',(81.608628840787,8.55876150375631,138.297735945525));
#70653=CARTESIAN_POINT('Ctrl Pts',(81.5847771185521,8.47955478599375,138.291870908533));
#70654=CARTESIAN_POINT('Ctrl Pts',(81.5469582248326,8.38113247558281,138.284622337968));
#70655=CARTESIAN_POINT('Ctrl Pts',(81.5383358630638,8.36000029365466,138.283067787426));
#70656=CARTESIAN_POINT('Ctrl Pts',(81.524592182781,8.32820062675729,138.280730112098));
#70657=CARTESIAN_POINT('Ctrl Pts',(81.5197872560296,8.31740024129588,138.279936424551));
#70658=CARTESIAN_POINT('Ctrl Pts',(81.5112203994609,8.2986828759621,138.278561131887));
#70659=CARTESIAN_POINT('Ctrl Pts',(81.5075102403455,8.29074286432606,138.277977784237));
#70660=CARTESIAN_POINT('Ctrl Pts',(81.4990001690529,8.27289917888247,138.276666762775));
#70661=CARTESIAN_POINT('Ctrl Pts',(81.494164399837,8.26301298048575,138.275940359269));
#70662=CARTESIAN_POINT('Ctrl Pts',(81.480766566296,8.23629658245513,138.273976686895));
#70663=CARTESIAN_POINT('Ctrl Pts',(81.4720156051569,8.2195625334724,138.272746037432));
#70664=CARTESIAN_POINT('Ctrl Pts',(81.4174770794252,8.11945350495147,138.265372266942));
#70665=CARTESIAN_POINT('Ctrl Pts',(81.3649004322941,8.03997208345693,138.259482296623));
#70666=CARTESIAN_POINT('Ctrl Pts',(81.2486346798971,7.89322663979722,138.248020525256));
#70667=CARTESIAN_POINT('Ctrl Pts',(81.1855669134947,7.82591962859444,138.242461164671));
#70668=CARTESIAN_POINT('Ctrl Pts',(81.0974522237328,7.74625834087843,138.234993167515));
#70669=CARTESIAN_POINT('Ctrl Pts',(81.0772105399731,7.72882462809436,138.233295021015));
#70670=CARTESIAN_POINT('Ctrl Pts',(81.0424867113786,7.7003428333551,138.230393501992));
#70671=CARTESIAN_POINT('Ctrl Pts',(81.0282262033174,7.68903161642448,138.229205023145));
#70672=CARTESIAN_POINT('Ctrl Pts',(81.0077487757175,7.673328885167,138.227498164455));
#70673=CARTESIAN_POINT('Ctrl Pts',(81.0016820985551,7.66874239542077,138.226992455909));
#70674=CARTESIAN_POINT('Ctrl Pts',(80.9911489474787,7.660891951698,138.226113961521));
#70675=CARTESIAN_POINT('Ctrl Pts',(80.9866972650644,7.65760843739858,138.225742528422));
#70676=CARTESIAN_POINT('Ctrl Pts',(80.9772133866843,7.65068589299375,138.224950768147));
#70677=CARTESIAN_POINT('Ctrl Pts',(80.972177254307,7.64705286669271,138.224530085084));
#70678=CARTESIAN_POINT('Ctrl Pts',(80.9582555253865,7.6371277046653,138.223366762406));
#70679=CARTESIAN_POINT('Ctrl Pts',(80.949328562139,7.63089452169851,138.222620367147));
#70680=CARTESIAN_POINT('Ctrl Pts',(80.9016376259835,7.59828536161688,138.218633231472));
#70681=CARTESIAN_POINT('Ctrl Pts',(80.8618374981891,7.57346938281445,138.215307560432));
#70682=CARTESIAN_POINT('Ctrl Pts',(80.7448733383006,7.50722280179509,138.205645885225));
#70683=CARTESIAN_POINT('Ctrl Pts',(80.6654169334357,7.47015018279518,138.199222597692));
#70684=CARTESIAN_POINT('Ctrl Pts',(80.5121119517632,7.41283519098589,138.18739024551));
#70685=CARTESIAN_POINT('Ctrl Pts',(80.4390579909328,7.39109305294282,138.181970522357));
#70686=CARTESIAN_POINT('Ctrl Pts',(80.3375008399328,7.36830459358104,138.174770807004));
#70687=CARTESIAN_POINT('Ctrl Pts',(80.3100865663232,7.36287349267407,138.172858984433));
#70688=CARTESIAN_POINT('Ctrl Pts',(80.2699484838518,7.35596616727004,138.170104156736));
#70689=CARTESIAN_POINT('Ctrl Pts',(80.2573249825108,7.3539431066078,138.169244075488));
#70690=CARTESIAN_POINT('Ctrl Pts',(80.2349914171841,7.35062710259901,138.167733194048));
#70691=CARTESIAN_POINT('Ctrl Pts',(80.2252910321334,7.34927413580797,138.167080530441));
#70692=CARTESIAN_POINT('Ctrl Pts',(80.2049346504632,7.34661770215669,138.165718148428));
#70693=CARTESIAN_POINT('Ctrl Pts',(80.194276820789,7.34533152571712,138.165009002177));
#70694=CARTESIAN_POINT('Ctrl Pts',(80.1660947666925,7.34220659288969,138.163144294905));
#70695=CARTESIAN_POINT('Ctrl Pts',(80.1485522221125,7.340542640482,138.161994232691));
#70696=CARTESIAN_POINT('Ctrl Pts',(80.0661765790623,7.33404590401942,138.156639177914));
#70697=CARTESIAN_POINT('Ctrl Pts',(80.0011191323809,7.33273200050666,138.152544385492));
#70698=CARTESIAN_POINT('Ctrl Pts',(79.7905807369824,7.34080750592639,138.139488284622));
#70699=CARTESIAN_POINT('Ctrl Pts',(79.6463990940175,7.36545665094281,138.130891323677));
#70700=CARTESIAN_POINT('Ctrl Pts',(79.4858549650214,7.41516124815858,138.120104771471));
#70701=CARTESIAN_POINT('Ctrl Pts',(79.4645682704295,7.42222570358287,138.118647577626));
#70702=CARTESIAN_POINT('Ctrl Pts',(79.435661751426,7.43247127561186,138.116623277611));
#70703=CARTESIAN_POINT('Ctrl Pts',(79.4279123143807,7.43528289025306,138.11607606326));
#70704=CARTESIAN_POINT('Ctrl Pts',(79.4148958097335,7.44011509760981,138.11514876498));
#70705=CARTESIAN_POINT('Ctrl Pts',(79.4096174245005,7.44210519111252,138.114770455316));
#70706=CARTESIAN_POINT('Ctrl Pts',(79.3987883762957,7.44625097279439,138.113989445477));
#70707=CARTESIAN_POINT('Ctrl Pts',(79.393239034047,7.44840965992862,138.113586586177));
#70708=CARTESIAN_POINT('Ctrl Pts',(79.3786618957416,7.45417030825552,138.112521630125));
#70709=CARTESIAN_POINT('Ctrl Pts',(79.3696540024839,7.45782154478325,138.111856731377));
#70710=CARTESIAN_POINT('Ctrl Pts',(79.3307794633611,7.47397633421778,138.108959257332));
#70711=CARTESIAN_POINT('Ctrl Pts',(79.3012509123767,7.48726944246051,138.106686390145));
#70712=CARTESIAN_POINT('Ctrl Pts',(79.2485890456955,7.51284750779756,138.102524107678));
#70713=CARTESIAN_POINT('Ctrl Pts',(79.2253208989838,7.52483453793934,138.100645156923));
#70714=CARTESIAN_POINT('Ctrl Pts',(79.1163595061494,7.58425706699978,138.091683336236));
#70715=CARTESIAN_POINT('Ctrl Pts',(79.0346701850194,7.63864458735291,138.08449167424));
#70716=CARTESIAN_POINT('Ctrl Pts',(78.9010169556137,7.7457401561245,138.072211211653));
#70717=CARTESIAN_POINT('Ctrl Pts',(78.8468840825302,7.79531836101649,138.067057827598));
#70718=CARTESIAN_POINT('Ctrl Pts',(78.7839868269093,7.86106213638394,138.060848319867));
#70719=CARTESIAN_POINT('Ctrl Pts',(78.7719891260512,7.87400851273935,138.059652491979));
#70720=CARTESIAN_POINT('Ctrl Pts',(78.7530241926725,7.89513679310415,138.057742961111));
#70721=CARTESIAN_POINT('Ctrl Pts',(78.7459267067906,7.90319940070358,138.057023814628));
#70722=CARTESIAN_POINT('Ctrl Pts',(78.7325087096955,7.91874253020877,138.055655253828));
#70723=CARTESIAN_POINT('Ctrl Pts',(78.7261752349649,7.92621121166902,138.055005320669));
#70724=CARTESIAN_POINT('Ctrl Pts',(78.7118711209733,7.9433838576828,138.053528045512));
#70725=CARTESIAN_POINT('Ctrl Pts',(78.7039435452367,7.9531230437098,138.052702469588));
#70726=CARTESIAN_POINT('Ctrl Pts',(78.6830809368851,7.97935343687659,138.050510476768));
#70727=CARTESIAN_POINT('Ctrl Pts',(78.6703454409366,7.99600097512323,138.049151910357));
#70728=CARTESIAN_POINT('Ctrl Pts',(78.5858580460651,8.1108693065002,138.03998413505));
#70729=CARTESIAN_POINT('Ctrl Pts',(78.5247346361114,8.21645241547501,138.032599543878));
#70730=CARTESIAN_POINT('Ctrl Pts',(78.4491360791845,8.38787732964649,138.021150156936));
#70731=CARTESIAN_POINT('Ctrl Pts',(78.4262054996706,8.44950686764995,138.017122855687));
#70732=CARTESIAN_POINT('Ctrl Pts',(78.4004337782013,8.53369187129784,138.011549591999));
#70733=CARTESIAN_POINT('Ctrl Pts',(78.394323335799,8.55518799531768,138.010120209386));
#70734=CARTESIAN_POINT('Ctrl Pts',(78.3845969613144,8.59222154197438,138.007636733414));
#70735=CARTESIAN_POINT('Ctrl Pts',(78.3807683358447,8.60770034367379,138.006592530437));
#70736=CARTESIAN_POINT('Ctrl Pts',(78.3755304552818,8.6302611924448,138.005058417337));
#70737=CARTESIAN_POINT('Ctrl Pts',(78.3739440164941,8.63730174906978,138.004577958352));
#70738=CARTESIAN_POINT('Ctrl Pts',(78.3712431197804,8.6496622096962,138.00373111118));
#70739=CARTESIAN_POINT('Ctrl Pts',(78.370108874352,8.65497759567742,138.003365845923));
#70740=CARTESIAN_POINT('Ctrl Pts',(78.3676928823558,8.66657743321451,138.002566244546));
#70741=CARTESIAN_POINT('Ctrl Pts',(78.3664214283584,8.67286366579006,138.002131371326));
#70742=CARTESIAN_POINT('Ctrl Pts',(78.3629688718115,8.6904557147033,138.000910345724));
#70743=CARTESIAN_POINT('Ctrl Pts',(78.3608686842504,8.70177677730762,138.000119933529));
#70744=CARTESIAN_POINT('Ctrl Pts',(78.3472941136256,8.77943044674238,137.994670723471));
#70745=CARTESIAN_POINT('Ctrl Pts',(78.3397332555545,8.84637714545199,137.989837644452));
#70746=CARTESIAN_POINT('Ctrl Pts',(78.3347732333155,8.94187762843282,137.982902275693));
#70747=CARTESIAN_POINT('Ctrl Pts',(78.3340257364443,8.97019868153111,137.980840122181));
#70748=CARTESIAN_POINT('Ctrl Pts',(78.3338937192958,9.11928312173196,137.969987770784));
#70749=CARTESIAN_POINT('Ctrl Pts',(78.346916648822,9.23971673357786,137.961268923042));
#70750=CARTESIAN_POINT('Ctrl Pts',(78.3773635453077,9.37821719681774,137.951513842782));
#70751=CARTESIAN_POINT('Ctrl Pts',(78.3822617974017,9.39864832833047,137.950080771153));
#70752=CARTESIAN_POINT('Ctrl Pts',(78.3907068943763,9.43114931819787,137.94780981578));
#70753=CARTESIAN_POINT('Ctrl Pts',(78.3940061035281,9.44328055892653,137.946964117364));
#70754=CARTESIAN_POINT('Ctrl Pts',(78.4001194494637,9.46479473827414,137.945467453211));
#70755=CARTESIAN_POINT('Ctrl Pts',(78.402879583022,9.47419226630688,137.944814775025));
#70756=CARTESIAN_POINT('Ctrl Pts',(78.4088380738411,9.49383696006755,137.943452424694));
#70757=CARTESIAN_POINT('Ctrl Pts',(78.4120529265984,9.50407868389715,137.942743324161));
#70758=CARTESIAN_POINT('Ctrl Pts',(78.4208047007412,9.53104476374886,137.940878879167));
#70759=CARTESIAN_POINT('Ctrl Pts',(78.4265083827096,9.54771388805996,137.939729030653));
#70760=CARTESIAN_POINT('Ctrl Pts',(78.433823501066,9.56803434018546,137.938329395143));
#70761=CARTESIAN_POINT('Ctrl Pts',(78.4351847809449,9.57177370031289,137.938071921239));
#70762=CARTESIAN_POINT('Ctrl Pts',(78.4365593728781,9.5755079543019,137.937814872615));
#70763=CARTESIAN_POINT('Ctrl Pts',(78.4365594482967,9.57550815918599,138.131873589273));
#70764=CARTESIAN_POINT('Ctrl Pts',(78.414637849384,9.51595536892372,138.136491900461));
#70765=CARTESIAN_POINT('Ctrl Pts',(78.3961254178195,9.45516788459882,138.14111638968));
#70766=CARTESIAN_POINT('Ctrl Pts',(78.3633053651022,9.32012388879201,138.151092520531));
#70767=CARTESIAN_POINT('Ctrl Pts',(78.3504862686607,9.24567456191019,138.156401286859));
#70768=CARTESIAN_POINT('Ctrl Pts',(78.3409385833685,9.15292782700929,138.162765649055));
#70769=CARTESIAN_POINT('Ctrl Pts',(78.3394018998885,9.13522461606615,138.163969701031));
#70770=CARTESIAN_POINT('Ctrl Pts',(78.3373894606692,9.10676175426065,138.165888993768));
#70771=CARTESIAN_POINT('Ctrl Pts',(78.3367343264427,9.09601659357096,138.166609780825));
#70772=CARTESIAN_POINT('Ctrl Pts',(78.3356827063292,9.07549597672171,138.167979367341));
#70773=CARTESIAN_POINT('Ctrl Pts',(78.3352680907964,9.06572194426203,138.168628705263));
#70774=CARTESIAN_POINT('Ctrl Pts',(78.3345197768597,9.04345014518695,138.170101784909));
#70775=CARTESIAN_POINT('Ctrl Pts',(78.3342406128081,9.0309510410592,138.170923794325));
#70776=CARTESIAN_POINT('Ctrl Pts',(78.3338721747492,8.99768326344809,138.173100002262));
#70777=CARTESIAN_POINT('Ctrl Pts',(78.3340304986832,8.97691365807849,138.174446530418));
#70778=CARTESIAN_POINT('Ctrl Pts',(78.3378513864377,8.83179078941756,138.183782698973));
#70779=CARTESIAN_POINT('Ctrl Pts',(78.3550437260773,8.70818656399838,138.191324616436));
#70780=CARTESIAN_POINT('Ctrl Pts',(78.4084928740364,8.49896359949546,138.204525774198));
#70781=CARTESIAN_POINT('Ctrl Pts',(78.4384117498405,8.41231826870576,138.210146095496));
#70782=CARTESIAN_POINT('Ctrl Pts',(78.4802104555524,8.31739833167442,138.216922874802));
#70783=CARTESIAN_POINT('Ctrl Pts',(78.485257448758,8.30627074519,138.217727500129));
#70784=CARTESIAN_POINT('Ctrl Pts',(78.4931726195924,8.28931765787036,138.21897053404));
#70785=CARTESIAN_POINT('Ctrl Pts',(78.4959533468624,8.2834514619487,138.219403837487));
#70786=CARTESIAN_POINT('Ctrl Pts',(78.5011424516177,8.27266786802886,138.220206518164));
#70787=CARTESIAN_POINT('Ctrl Pts',(78.5035408713517,8.26774590899586,138.220575290997));
#70788=CARTESIAN_POINT('Ctrl Pts',(78.5090660378454,8.25654785934247,138.221419757373));
#70789=CARTESIAN_POINT('Ctrl Pts',(78.5122081713514,8.25027962872683,138.221896372034));
#70790=CARTESIAN_POINT('Ctrl Pts',(78.5223042246101,8.23045247212741,138.223415985597));
#70791=CARTESIAN_POINT('Ctrl Pts',(78.5294044201984,8.2169694756745,138.224467316182));
#70792=CARTESIAN_POINT('Ctrl Pts',(78.5855325897473,8.1138408899625,138.232637376182));
#70793=CARTESIAN_POINT('Ctrl Pts',(78.6425252244934,8.02878693163967,138.240117459765));
#70794=CARTESIAN_POINT('Ctrl Pts',(78.7795628508592,7.86010829693086,138.255923485067));
#70795=CARTESIAN_POINT('Ctrl Pts',(78.8612687627697,7.77847618599563,138.264182945378));
#70796=CARTESIAN_POINT('Ctrl Pts',(78.9658258335971,7.69370139811592,138.273393669623));
#70797=CARTESIAN_POINT('Ctrl Pts',(78.9811053750318,7.6817488698564,138.274710513945));
#70798=CARTESIAN_POINT('Ctrl Pts',(79.0054617482289,7.66337246904914,138.276765199439));
#70799=CARTESIAN_POINT('Ctrl Pts',(79.0143996700174,7.65676826622106,138.277510054563));
#70800=CARTESIAN_POINT('Ctrl Pts',(79.0312785371243,7.64455571226963,138.278899944832));
#70801=CARTESIAN_POINT('Ctrl Pts',(79.0392037391194,7.63892651127807,138.279545765869));
#70802=CARTESIAN_POINT('Ctrl Pts',(79.0571237790144,7.62643258739501,138.280991190476));
#70803=CARTESIAN_POINT('Ctrl Pts',(79.0671452704098,7.61960691412703,138.281789287962));
#70804=CARTESIAN_POINT('Ctrl Pts',(79.0968805489473,7.59982583747257,138.284128265636));
#70805=CARTESIAN_POINT('Ctrl Pts',(79.1167964965988,7.58717867746819,138.28565769616));
#70806=CARTESIAN_POINT('Ctrl Pts',(79.225102628248,7.52158699880848,138.293792071544));
#70807=CARTESIAN_POINT('Ctrl Pts',(79.317994307088,7.4765031953814,138.300109324374));
#70808=CARTESIAN_POINT('Ctrl Pts',(79.4884867459653,7.41249832585567,138.311231414377));
#70809=CARTESIAN_POINT('Ctrl Pts',(79.5643873148481,7.39001639114764,138.316037638715));
#70810=CARTESIAN_POINT('Ctrl Pts',(79.6657466595042,7.36768798256059,138.322582286372));
#70811=CARTESIAN_POINT('Ctrl Pts',(79.6900166995516,7.36290560993512,138.324158994922));
#70812=CARTESIAN_POINT('Ctrl Pts',(79.7313263464648,7.3557171038693,138.326872600835));
#70813=CARTESIAN_POINT('Ctrl Pts',(79.7483136567872,7.35303135951741,138.327996991992));
#70814=CARTESIAN_POINT('Ctrl Pts',(79.7727005126892,7.34956180462178,138.329627257385));
#70815=CARTESIAN_POINT('Ctrl Pts',(79.7800691084418,7.34856374891355,138.33012194618));
#70816=CARTESIAN_POINT('Ctrl Pts',(79.7929064676546,7.34691240354196,138.330987814442));
#70817=CARTESIAN_POINT('Ctrl Pts',(79.7983721830943,7.34623685034833,138.331357752602));
#70818=CARTESIAN_POINT('Ctrl Pts',(79.8100939733911,7.34484703225218,138.33215398822));
#70819=CARTESIAN_POINT('Ctrl Pts',(79.816350673941,7.34414113906587,138.33258070801));
#70820=CARTESIAN_POINT('Ctrl Pts',(79.8335459591911,7.34229978744588,138.333757895499));
#70821=CARTESIAN_POINT('Ctrl Pts',(79.8444917892242,7.34123717106693,138.334512167061));
#70822=CARTESIAN_POINT('Ctrl Pts',(79.9069181891597,7.3358001443225,138.338838958122));
#70823=CARTESIAN_POINT('Ctrl Pts',(79.9585650469178,7.33371448078588,138.342514709301));
#70824=CARTESIAN_POINT('Ctrl Pts',(80.1062897031846,7.33462066696945,138.353161094629));
#70825=CARTESIAN_POINT('Ctrl Pts',(80.2021297567767,7.34351864753318,138.360217535047));
#70826=CARTESIAN_POINT('Ctrl Pts',(80.3482770337563,7.36996643463314,138.370897266388));
#70827=CARTESIAN_POINT('Ctrl Pts',(80.3994163169786,7.38173741146202,138.374621449589));
#70828=CARTESIAN_POINT('Ctrl Pts',(80.4728290324852,7.40232830237056,138.379934912268));
#70829=CARTESIAN_POINT('Ctrl Pts',(80.4955994412264,7.40924438087714,138.381578527507));
#70830=CARTESIAN_POINT('Ctrl Pts',(80.5366303837534,7.42267337305199,138.384532612724));
#70831=CARTESIAN_POINT('Ctrl Pts',(80.554939950649,7.42902159052957,138.385848050426));
#70832=CARTESIAN_POINT('Ctrl Pts',(80.583565628269,7.43950951519255,138.387901052862));
#70833=CARTESIAN_POINT('Ctrl Pts',(80.5939576958954,7.44343530121392,138.388645612348));
#70834=CARTESIAN_POINT('Ctrl Pts',(80.6133689848682,7.45099096569337,138.390035238025));
#70835=CARTESIAN_POINT('Ctrl Pts',(80.6223971505771,7.45459639777722,138.390681087156));
#70836=CARTESIAN_POINT('Ctrl Pts',(80.6426192887695,7.46287814195678,138.392126944959));
#70837=CARTESIAN_POINT('Ctrl Pts',(80.6537948611912,7.46759814368206,138.392925443575));
#70838=CARTESIAN_POINT('Ctrl Pts',(80.6865744247106,7.48186647011733,138.395266773831));
#70839=CARTESIAN_POINT('Ctrl Pts',(80.7080286210067,7.49175286609609,138.396798120448));
#70840=CARTESIAN_POINT('Ctrl Pts',(80.8199922498526,7.54626310536275,138.404797826564));
#70841=CARTESIAN_POINT('Ctrl Pts',(80.9065217582138,7.59858650179525,138.410991884992));
#70842=CARTESIAN_POINT('Ctrl Pts',(81.05276059186,7.70626109595913,138.422084629955));
#70843=CARTESIAN_POINT('Ctrl Pts',(81.1141641228485,7.75874993612572,138.426984504078));
#70844=CARTESIAN_POINT('Ctrl Pts',(81.1892927783001,7.83305373898671,138.433644775243));
#70845=CARTESIAN_POINT('Ctrl Pts',(81.2066673559814,7.85102887431014,138.435237653497));
#70846=CARTESIAN_POINT('Ctrl Pts',(81.2353929821131,7.88211779770212,138.437976368323));
#70847=CARTESIAN_POINT('Ctrl Pts',(81.2469559886809,7.89503070495842,138.43910939277));
#70848=CARTESIAN_POINT('Ctrl Pts',(81.2632034314202,7.91375475706185,138.440749985354));
#70849=CARTESIAN_POINT('Ctrl Pts',(81.268053988071,7.91942112040923,138.441246173031));
#70850=CARTESIAN_POINT('Ctrl Pts',(81.2764214767593,7.92932984601704,138.442113732601));
#70851=CARTESIAN_POINT('Ctrl Pts',(81.2799556739122,7.93355739170006,138.442483847944));
#70852=CARTESIAN_POINT('Ctrl Pts',(81.2874751356204,7.94264326842464,138.443279368357));
#70853=CARTESIAN_POINT('Ctrl Pts',(81.2914538419781,7.94750655421665,138.443705186116));
#70854=CARTESIAN_POINT('Ctrl Pts',(81.302284331078,7.96089884401729,138.444877535578));
#70855=CARTESIAN_POINT('Ctrl Pts',(81.3090796168231,7.96947283769105,138.445627822173));
#70856=CARTESIAN_POINT('Ctrl Pts',(81.3467455593922,8.01797179417796,138.449867410779));
#70857=CARTESIAN_POINT('Ctrl Pts',(81.3758712214113,8.05921291139832,138.453455236175));
#70858=CARTESIAN_POINT('Ctrl Pts',(81.454966856042,8.18275540357339,138.464020380551));
#70859=CARTESIAN_POINT('Ctrl Pts',(81.499736688283,8.26814746189261,138.471089924749));
#70860=CARTESIAN_POINT('Ctrl Pts',(81.5573988258966,8.40595520346095,138.481837139326));
#70861=CARTESIAN_POINT('Ctrl Pts',(81.5755563232026,8.45593795418796,138.485613081212));
#70862=CARTESIAN_POINT('Ctrl Pts',(81.6017424851114,8.54041095075611,138.491778221743));
#70863=CARTESIAN_POINT('Ctrl Pts',(81.6111176165792,8.57443985920846,138.494205727242));
#70864=CARTESIAN_POINT('Ctrl Pts',(81.6226860975378,8.62232161223749,138.497546023901));
#70865=CARTESIAN_POINT('Ctrl Pts',(81.6257958881495,8.63594109481123,138.498487778727));
#70866=CARTESIAN_POINT('Ctrl Pts',(81.630833587254,8.65935729333653,138.500093088662));
#70867=CARTESIAN_POINT('Ctrl Pts',(81.6328453675909,8.66913498835969,138.500759288286));
#70868=CARTESIAN_POINT('Ctrl Pts',(81.6365205099671,8.68784746929808,138.502026634361));
#70869=CARTESIAN_POINT('Ctrl Pts',(81.6381988751599,8.69677890419265,138.502628236285));
#70870=CARTESIAN_POINT('Ctrl Pts',(81.6423784664736,8.72006896456704,138.50418869879));
#70871=CARTESIAN_POINT('Ctrl Pts',(81.6447645414857,8.73444767558111,138.505143893466));
#70872=CARTESIAN_POINT('Ctrl Pts',(81.652506158067,8.78521599040884,138.508489501857));
#70873=CARTESIAN_POINT('Ctrl Pts',(81.6568453408311,8.82175128228929,138.510848200184));
#70874=CARTESIAN_POINT('Ctrl Pts',(81.6703115006988,8.97961742097151,138.520878132781));
#70875=CARTESIAN_POINT('Ctrl Pts',(81.667343736401,9.10159783692041,138.528188075259));
#70876=CARTESIAN_POINT('Ctrl Pts',(81.6411898648129,9.29596637601409,138.540236404648));
#70877=CARTESIAN_POINT('Ctrl Pts',(81.6263253019061,9.36900325051639,138.544867531466));
#70878=CARTESIAN_POINT('Ctrl Pts',(81.6035664506266,9.45195651606326,138.550495984455));
#70879=CARTESIAN_POINT('Ctrl Pts',(81.6003868868736,9.46308945989816,138.551259258554));
#70880=CARTESIAN_POINT('Ctrl Pts',(81.5952822719424,9.48028208892552,138.55245155244));
#70881=CARTESIAN_POINT('Ctrl Pts',(81.5934380574184,9.48636567100102,138.552876092584));
#70882=CARTESIAN_POINT('Ctrl Pts',(81.5899348447478,9.4976880410318,138.553671426601));
#70883=CARTESIAN_POINT('Ctrl Pts',(81.5882846901683,9.50292935519285,138.554041714052));
#70884=CARTESIAN_POINT('Ctrl Pts',(81.5844103219732,9.5150260917976,138.554901151823));
#70885=CARTESIAN_POINT('Ctrl Pts',(81.5821675232111,9.52187533691655,138.555391351295));
#70886=CARTESIAN_POINT('Ctrl Pts',(81.5748930757631,9.54361270621935,138.556958027052));
#70887=CARTESIAN_POINT('Ctrl Pts',(81.5696953432664,9.55844378346109,138.558043326547));
#70888=CARTESIAN_POINT('Ctrl Pts',(81.5345844752285,9.65426319935507,138.565152192615));
#70889=CARTESIAN_POINT('Ctrl Pts',(81.4986263975882,9.73288878810961,138.571431825343));
#70890=CARTESIAN_POINT('Ctrl Pts',(81.4212058917595,9.87240697068342,138.58304676143));
#70891=CARTESIAN_POINT('Ctrl Pts',(81.3814820678671,9.93403898360383,138.588369654603));
#70892=CARTESIAN_POINT('Ctrl Pts',(81.3134507173293,10.025707793532,138.596497657231));
#70893=CARTESIAN_POINT('Ctrl Pts',(81.2878698570919,10.0576487845835,138.599375111348));
#70894=CARTESIAN_POINT('Ctrl Pts',(81.2420094106939,10.1107769901602,138.604237184161));
#70895=CARTESIAN_POINT('Ctrl Pts',(81.2222999374128,10.1324292245238,138.606242214442));
#70896=CARTESIAN_POINT('Ctrl Pts',(81.1930184007679,10.1629412899006,138.609104133544));
#70897=CARTESIAN_POINT('Ctrl Pts',(81.18389790651,10.172224855551,138.609980031773));
#70898=CARTESIAN_POINT('Ctrl Pts',(81.1677031341513,10.1883273518583,138.611508775063));
#70899=CARTESIAN_POINT('Ctrl Pts',(81.1606756730323,10.195192241366,138.612163632632));
#70900=CARTESIAN_POINT('Ctrl Pts',(81.1459214810457,10.2093522501043,138.613521175951));
#70901=CARTESIAN_POINT('Ctrl Pts',(81.1381848320589,10.2166364298585,138.614223371539));
#70902=CARTESIAN_POINT('Ctrl Pts',(81.1178023519147,10.23546226283,138.616048792409));
#70903=CARTESIAN_POINT('Ctrl Pts',(81.1050471662243,10.2468840750931,138.61716693801));
#70904=CARTESIAN_POINT('Ctrl Pts',(81.048942768151,10.2955862776625,138.62198550762));
#70905=CARTESIAN_POINT('Ctrl Pts',(81.0038643175851,10.3308201250184,138.625602725255));
#70906=CARTESIAN_POINT('Ctrl Pts',(80.8703213163117,10.4245441518146,138.635760662698));
#70907=CARTESIAN_POINT('Ctrl Pts',(80.7779759666654,10.4770031489307,138.642126353889));
#70908=CARTESIAN_POINT('Ctrl Pts',(80.6269437164868,10.5446818877417,138.652339500227));
#70909=CARTESIAN_POINT('Ctrl Pts',(80.5713525655898,10.5660955565402,138.65606496528));
#70910=CARTESIAN_POINT('Ctrl Pts',(80.5009374305427,10.5889708463977,138.660879948062));
#70911=CARTESIAN_POINT('Ctrl Pts',(80.4870760012602,10.5932744879666,138.661832344571));
#70912=CARTESIAN_POINT('Ctrl Pts',(80.4664963302561,10.599370340004,138.663255498536));
#70913=CARTESIAN_POINT('Ctrl Pts',(80.4598198222796,10.6013026064257,138.663718616607));
#70914=CARTESIAN_POINT('Ctrl Pts',(80.4483802827232,10.60453591428,138.664514851499));
#70915=CARTESIAN_POINT('Ctrl Pts',(80.4436232513506,10.6058576487229,138.664846772434));
#70916=CARTESIAN_POINT('Ctrl Pts',(80.4326875975321,10.608843804261,138.665611735535));
#70917=CARTESIAN_POINT('Ctrl Pts',(80.4265053484731,10.6104937528121,138.66604557398));
#70918=CARTESIAN_POINT('Ctrl Pts',(80.4092327514541,10.6149971187187,138.667261232166));
#70919=CARTESIAN_POINT('Ctrl Pts',(80.3981225082043,10.6177717974687,138.668047255481));
#70920=CARTESIAN_POINT('Ctrl Pts',(80.3238895414408,10.6354998147202,138.67332221061));
#70921=CARTESIAN_POINT('Ctrl Pts',(80.2599746108758,10.6468683642374,138.677973173226));
#70922=CARTESIAN_POINT('Ctrl Pts',(80.1726390973349,10.6571918445905,138.684346254378));
#70923=CARTESIAN_POINT('Ctrl Pts',(80.149656848923,10.6594251631363,138.686025218517));
#70924=CARTESIAN_POINT('Ctrl Pts',(80.0553326270621,10.666615732976,138.692909975694));
#70925=CARTESIAN_POINT('Ctrl Pts',(79.9837491995658,10.6674551721576,138.698116437658));
#70926=CARTESIAN_POINT('Ctrl Pts',(79.8674834373629,10.661328437191,138.706437658304));
#70927=CARTESIAN_POINT('Ctrl Pts',(79.822747614529,10.6571526768007,138.709607725067));
#70928=CARTESIAN_POINT('Ctrl Pts',(79.7471814059211,10.6470034241371,138.71490139837));
#70929=CARTESIAN_POINT('Ctrl Pts',(79.7162531253605,10.6419578133436,138.717050629039));
#70930=CARTESIAN_POINT('Ctrl Pts',(79.6723672323591,10.6335210951386,138.720077218468));
#70931=CARTESIAN_POINT('Ctrl Pts',(79.6592812856565,10.6308418606453,138.720976763044));
#70932=CARTESIAN_POINT('Ctrl Pts',(79.6365771357627,10.6259081683505,138.722532760185));
#70933=CARTESIAN_POINT('Ctrl Pts',(79.6269443021032,10.623725039425,138.723191448666));
#70934=CARTESIAN_POINT('Ctrl Pts',(79.6083520929794,10.6193372203495,138.724460123332));
#70935=CARTESIAN_POINT('Ctrl Pts',(79.5993905232437,10.617143521526,138.725070434654));
#70936=CARTESIAN_POINT('Ctrl Pts',(79.5755792743885,10.6111046924307,138.726689157048));
#70937=CARTESIAN_POINT('Ctrl Pts',(79.5607634601316,10.6071286725431,138.727693334503));
#70938=CARTESIAN_POINT('Ctrl Pts',(79.505572949772,10.5914973175549,138.731424960401));
#70939=CARTESIAN_POINT('Ctrl Pts',(79.465587071244,10.578519907278,138.734109837021));
#70940=CARTESIAN_POINT('Ctrl Pts',(79.3592437811039,10.5395011582675,138.74124610156));
#70941=CARTESIAN_POINT('Ctrl Pts',(79.2939954713438,10.5106922254269,138.745617493715));
#70942=CARTESIAN_POINT('Ctrl Pts',(79.1302274333835,10.4254487935235,138.756898446319));
#70943=CARTESIAN_POINT('Ctrl Pts',(79.0352854784983,10.3629846025207,138.763743707595));
#70944=CARTESIAN_POINT('Ctrl Pts',(78.9363102086356,10.2823127455362,138.772050382616));
#70945=CARTESIAN_POINT('Ctrl Pts',(78.925304322394,10.2731029480145,138.772992294661));
#70946=CARTESIAN_POINT('Ctrl Pts',(78.9091705562749,10.2592438213694,138.774402735372));
#70947=CARTESIAN_POINT('Ctrl Pts',(78.9039501303199,10.2547025766547,138.774863819975));
#70948=CARTESIAN_POINT('Ctrl Pts',(78.8946591181166,10.2465181012451,138.775693220494));
#70949=CARTESIAN_POINT('Ctrl Pts',(78.890577956397,10.242887190852,138.776060637702));
#70950=CARTESIAN_POINT('Ctrl Pts',(78.8815611664521,10.2347853751436,138.776879346046));
#70951=CARTESIAN_POINT('Ctrl Pts',(78.8766345121527,10.2303049719124,138.777331320272));
#70952=CARTESIAN_POINT('Ctrl Pts',(78.8621441286129,10.2169675135089,138.778674130992));
#70953=CARTESIAN_POINT('Ctrl Pts',(78.8526575987415,10.2080278560539,138.779570765341));
#70954=CARTESIAN_POINT('Ctrl Pts',(78.830937882052,10.1870736052995,138.781662644502));
#70955=CARTESIAN_POINT('Ctrl Pts',(78.8187834772551,10.1749797684339,138.782862741672));
#70956=CARTESIAN_POINT('Ctrl Pts',(78.7771190701015,10.1322231168403,138.787074156149));
#70957=CARTESIAN_POINT('Ctrl Pts',(78.7486002214435,10.100620318275,138.79013183154));
#70958=CARTESIAN_POINT('Ctrl Pts',(78.6545313762142,9.98799134945566,138.800756752041));
#70959=CARTESIAN_POINT('Ctrl Pts',(78.5953819310225,9.90192232857178,138.808400266586));
#70960=CARTESIAN_POINT('Ctrl Pts',(78.5150811796408,9.75780283068197,138.820148096467));
#70961=CARTESIAN_POINT('Ctrl Pts',(78.4884265097267,9.70313312068178,138.824395576988));
#70962=CARTESIAN_POINT('Ctrl Pts',(78.4581005186763,9.63119009899751,138.829720882919));
#70963=CARTESIAN_POINT('Ctrl Pts',(78.4516327232602,9.6151534499893,138.830891885378));
#70964=CARTESIAN_POINT('Ctrl Pts',(78.442404467417,9.59120410005916,138.832617607355));
#70965=CARTESIAN_POINT('Ctrl Pts',(78.4394523293198,9.58336703874729,138.8331787035));
#70966=CARTESIAN_POINT('Ctrl Pts',(78.4365593737687,9.57550795672114,138.833737829798));
#70967=CARTESIAN_POINT('Origin',(80.,9.,134.));
#70968=CARTESIAN_POINT('',(78.4365593737676,9.57550795671827,139.531855288841));
#70969=CARTESIAN_POINT('',(78.4365593737638,9.57550795670799,139.340802412607));
#70970=CARTESIAN_POINT('',(78.4365593737638,9.57550795670799,134.));
#70971=CARTESIAN_POINT('',(81.2690708798525,10.0793586530483,140.));
#70972=CARTESIAN_POINT('Ctrl Pts',(78.4365593737676,9.57550795671827,139.531855288841));
#70973=CARTESIAN_POINT('Ctrl Pts',(78.4053667308162,9.49076917133665,139.537370123103));
#70974=CARTESIAN_POINT('Ctrl Pts',(78.3811187428276,9.40364475628102,139.542897610453));
#70975=CARTESIAN_POINT('Ctrl Pts',(78.3610876164748,9.29961255398156,139.549772227858));
#70976=CARTESIAN_POINT('Ctrl Pts',(78.3583425323577,9.28418690792652,139.550798653398));
#70977=CARTESIAN_POINT('Ctrl Pts',(78.3546746539356,9.26174516760808,139.552305209109));
#70978=CARTESIAN_POINT('Ctrl Pts',(78.3535782721426,9.25475776074172,139.552776147149));
#70979=CARTESIAN_POINT('Ctrl Pts',(78.3517117452004,9.24234652681836,139.55361628133));
#70980=CARTESIAN_POINT('Ctrl Pts',(78.3509238114044,9.23692558411675,139.55398447884));
#70981=CARTESIAN_POINT('Ctrl Pts',(78.3492663990445,9.22511369656628,139.554789527723));
#70982=CARTESIAN_POINT('Ctrl Pts',(78.3484073002293,9.21872162274131,139.555226917024));
#70983=CARTESIAN_POINT('Ctrl Pts',(78.3460625052061,9.2004732948317,139.556480224361));
#70984=CARTESIAN_POINT('Ctrl Pts',(78.3446672560414,9.18860611061177,139.557300839175));
#70985=CARTESIAN_POINT('Ctrl Pts',(78.333364075957,9.0826516048928,139.564671223018));
#70986=CARTESIAN_POINT('Ctrl Pts',(78.3313608875267,8.98790384756586,139.571558498935));
#70987=CARTESIAN_POINT('Ctrl Pts',(78.3451972873752,8.77188127659991,139.58731651004));
#70988=CARTESIAN_POINT('Ctrl Pts',(78.3663122964101,8.65145308166225,139.596119420761));
#70989=CARTESIAN_POINT('Ctrl Pts',(78.4062640967921,8.51419734399615,139.605954073373));
#70990=CARTESIAN_POINT('Ctrl Pts',(78.4125241826993,8.49411567631456,139.607388987131));
#70991=CARTESIAN_POINT('Ctrl Pts',(78.4231442968658,8.46218851940609,139.609664788115));
#70992=CARTESIAN_POINT('Ctrl Pts',(78.4272613658869,8.4502652448208,139.610513451837));
#70993=CARTESIAN_POINT('Ctrl Pts',(78.4348319556892,8.42912181998497,139.612016513195));
#70994=CARTESIAN_POINT('Ctrl Pts',(78.4382324971456,8.41988347938466,139.612672616458));
#70995=CARTESIAN_POINT('Ctrl Pts',(78.4455376008314,8.40056740148135,139.614043338092));
#70996=CARTESIAN_POINT('Ctrl Pts',(78.4494587539753,8.39049639524773,139.614757370607));
#70997=CARTESIAN_POINT('Ctrl Pts',(78.4600904688232,8.36395687939928,139.616637826442));
#70998=CARTESIAN_POINT('Ctrl Pts',(78.4669672952011,8.34755614732925,139.617798664051));
#70999=CARTESIAN_POINT('Ctrl Pts',(78.5040857977424,8.26286014614947,139.623792192387));
#71000=CARTESIAN_POINT('Ctrl Pts',(78.5386341911395,8.19654093875735,139.628475965896));
#71001=CARTESIAN_POINT('Ctrl Pts',(78.6273025671526,8.05110419380196,139.638990034171));
#71002=CARTESIAN_POINT('Ctrl Pts',(78.6840202632315,7.97389190749445,139.644750830598));
#71003=CARTESIAN_POINT('Ctrl Pts',(78.7788109362275,7.86572660845065,139.65367678295));
#71004=CARTESIAN_POINT('Ctrl Pts',(78.812131143485,7.83087827413104,139.656709975096));
#71005=CARTESIAN_POINT('Ctrl Pts',(78.857393958366,7.7874743897082,139.660776866668));
#71006=CARTESIAN_POINT('Ctrl Pts',(78.8680069505943,7.77756038009546,139.661726901642));
#71007=CARTESIAN_POINT('Ctrl Pts',(78.8840134712842,7.76299524890752,139.663156978034));
#71008=CARTESIAN_POINT('Ctrl Pts',(78.8893097257908,7.75823762466625,139.66362972244));
#71009=CARTESIAN_POINT('Ctrl Pts',(78.8988844390412,7.7497469210675,139.664483924752));
#71010=CARTESIAN_POINT('Ctrl Pts',(78.9031518593805,7.74600143721624,139.664864490509));
#71011=CARTESIAN_POINT('Ctrl Pts',(78.9119754231542,7.73833655872414,139.66565123698));
#71012=CARTESIAN_POINT('Ctrl Pts',(78.9165337119192,7.73441992800407,139.6660575779));
#71013=CARTESIAN_POINT('Ctrl Pts',(78.9284546333327,7.72428868574962,139.667119774126));
#71014=CARTESIAN_POINT('Ctrl Pts',(78.9358500406632,7.71811323302088,139.667778264676));
#71015=CARTESIAN_POINT('Ctrl Pts',(78.9693822239564,7.69060268948958,139.670760313008));
#71016=CARTESIAN_POINT('Ctrl Pts',(78.9961081467314,7.67000183951041,139.673127018181));
#71017=CARTESIAN_POINT('Ctrl Pts',(79.078295038691,7.61053954222738,139.680332728223));
#71018=CARTESIAN_POINT('Ctrl Pts',(79.1355172652143,7.57423383202161,139.685252406462));
#71019=CARTESIAN_POINT('Ctrl Pts',(79.2942426688896,7.48660346930289,139.698407037452));
#71020=CARTESIAN_POINT('Ctrl Pts',(79.3990703762787,7.44200311167996,139.706573674443));
#71021=CARTESIAN_POINT('Ctrl Pts',(79.5277093152694,7.40220809819103,139.71583196675));
#71022=CARTESIAN_POINT('Ctrl Pts',(79.5478979744556,7.3963786982033,139.717264747969));
#71023=CARTESIAN_POINT('Ctrl Pts',(79.5803929030306,7.38765839275512,139.719539488006));
#71024=CARTESIAN_POINT('Ctrl Pts',(79.5926306120503,7.38452305150594,139.720389118694));
#71025=CARTESIAN_POINT('Ctrl Pts',(79.6145046399116,7.37918322722211,139.721895582784));
#71026=CARTESIAN_POINT('Ctrl Pts',(79.6241270252903,7.37692477142474,139.722554103203));
#71027=CARTESIAN_POINT('Ctrl Pts',(79.6443814771264,7.37236066433221,139.723931733666));
#71028=CARTESIAN_POINT('Ctrl Pts',(79.6550172081869,7.37007324595036,139.724650237993));
#71029=CARTESIAN_POINT('Ctrl Pts',(79.6832792183942,7.36428398969517,139.726547021515));
#71030=CARTESIAN_POINT('Ctrl Pts',(79.7009413603169,7.36096281600217,139.727719579448));
#71031=CARTESIAN_POINT('Ctrl Pts',(79.7944212245474,7.34494637327114,139.733863415645));
#71032=CARTESIAN_POINT('Ctrl Pts',(79.8710008794541,7.33722323910122,139.738675901439));
#71033=CARTESIAN_POINT('Ctrl Pts',(80.0546353883884,7.33147201806204,139.749995122743));
#71034=CARTESIAN_POINT('Ctrl Pts',(80.1614895001244,7.33840756221315,139.756398196994));
#71035=CARTESIAN_POINT('Ctrl Pts',(80.3114471576711,7.36274926557926,139.765895226437));
#71036=CARTESIAN_POINT('Ctrl Pts',(80.355640800178,7.37177761697455,139.768761519963));
#71037=CARTESIAN_POINT('Ctrl Pts',(80.409741442029,7.38513740138604,139.772414688513));
#71038=CARTESIAN_POINT('Ctrl Pts',(80.4200485064856,7.38778770027444,139.773117257217));
#71039=CARTESIAN_POINT('Ctrl Pts',(80.436323379197,7.39213918253426,139.774238093289));
#71040=CARTESIAN_POINT('Ctrl Pts',(80.4423084959807,7.39377532990872,139.774652754427));
#71041=CARTESIAN_POINT('Ctrl Pts',(80.4534063064654,7.39687586103046,139.775426471519));
#71042=CARTESIAN_POINT('Ctrl Pts',(80.4585214575859,7.3983313839014,139.775785009602));
#71043=CARTESIAN_POINT('Ctrl Pts',(80.4704166120831,7.4017778182161,139.776623426204));
#71044=CARTESIAN_POINT('Ctrl Pts',(80.4771909418797,7.40378737900399,139.777104405194));
#71045=CARTESIAN_POINT('Ctrl Pts',(80.4996779315145,7.41061393702509,139.778712154311));
#71046=CARTESIAN_POINT('Ctrl Pts',(80.5153314671278,7.41562014743402,139.779849528432));
#71047=CARTESIAN_POINT('Ctrl Pts',(80.55322384788,7.4283595574259,139.782642847223));
#71048=CARTESIAN_POINT('Ctrl Pts',(80.5753773386563,7.43633408313875,139.784309913187));
#71049=CARTESIAN_POINT('Ctrl Pts',(80.6654046790929,7.4709130715592,139.791204241041));
#71050=CARTESIAN_POINT('Ctrl Pts',(80.7316635856436,7.50148824087596,139.796557027201));
#71051=CARTESIAN_POINT('Ctrl Pts',(80.9013281874108,7.59372222585803,139.810707967327));
#71052=CARTESIAN_POINT('Ctrl Pts',(81.0004470399118,7.66241778458007,139.819419383229));
#71053=CARTESIAN_POINT('Ctrl Pts',(81.1092751016174,7.75676652829245,139.829342478444));
#71054=CARTESIAN_POINT('Ctrl Pts',(81.1268962507127,7.77271614438428,139.830963459691));
#71055=CARTESIAN_POINT('Ctrl Pts',(81.1526837625225,7.7970813390071,139.833358730681));
#71056=CARTESIAN_POINT('Ctrl Pts',(81.1611116817903,7.80521431360711,139.83414539553));
#71057=CARTESIAN_POINT('Ctrl Pts',(81.1760953042924,7.81998186305234,139.835551254031));
#71058=CARTESIAN_POINT('Ctrl Pts',(81.1826823077608,7.82658381913668,139.836171886201));
#71059=CARTESIAN_POINT('Ctrl Pts',(81.1966248066269,7.84079464412579,139.837491383799));
#71060=CARTESIAN_POINT('Ctrl Pts',(81.2039639681868,7.8484190183791,139.83818949429));
#71061=CARTESIAN_POINT('Ctrl Pts',(81.2237527349007,7.86937279243841,139.840082081726));
#71062=CARTESIAN_POINT('Ctrl Pts',(81.2360571416266,7.88283778028323,139.841270150687));
#71063=CARTESIAN_POINT('Ctrl Pts',(81.3155034313595,7.97269749339213,139.849024342637));
#71064=CARTESIAN_POINT('Ctrl Pts',(81.3757536331803,8.05490450313513,139.855287060513));
#71065=CARTESIAN_POINT('Ctrl Pts',(81.4828978778062,8.23326696583813,139.867989113746));
#71066=CARTESIAN_POINT('Ctrl Pts',(81.5287990176698,8.32945273557691,139.874398074938));
#71067=CARTESIAN_POINT('Ctrl Pts',(81.5722470710693,8.44862322547404,139.882558428744));
#71068=CARTESIAN_POINT('Ctrl Pts',(81.5789196238383,8.468032025565,139.883894545287));
#71069=CARTESIAN_POINT('Ctrl Pts',(81.5877128975135,8.49523388460554,139.885783694033));
#71070=CARTESIAN_POINT('Ctrl Pts',(81.5901383567808,8.50292749457657,139.886319835288));
#71071=CARTESIAN_POINT('Ctrl Pts',(81.5941215369148,8.5158897763245,139.887226693119));
#71072=CARTESIAN_POINT('Ctrl Pts',(81.5957092256296,8.52114903315197,139.887595635095));
#71073=CARTESIAN_POINT('Ctrl Pts',(81.5989613818557,8.53211768075396,139.888367229068));
#71074=CARTESIAN_POINT('Ctrl Pts',(81.600621290968,8.53782812135838,139.888770105643));
#71075=CARTESIAN_POINT('Ctrl Pts',(81.6045716412018,8.55169472712968,139.889751057349));
#71076=CARTESIAN_POINT('Ctrl Pts',(81.606830482858,8.55985961202684,139.890330872933));
#71077=CARTESIAN_POINT('Ctrl Pts',(81.6162178053412,8.59482695740804,139.892822511523));
#71078=CARTESIAN_POINT('Ctrl Pts',(81.622738220569,8.62178625974415,139.89476473738));
#71079=CARTESIAN_POINT('Ctrl Pts',(81.6388046100089,8.69630909345912,139.900170835777));
#71080=CARTESIAN_POINT('Ctrl Pts',(81.6469506220005,8.74414514010715,139.903681742951));
#71081=CARTESIAN_POINT('Ctrl Pts',(81.6663865506929,8.89880131909011,139.915050442486));
#71082=CARTESIAN_POINT('Ctrl Pts',(81.6694453861322,9.00639326269799,139.92296815897));
#71083=CARTESIAN_POINT('Ctrl Pts',(81.6574866644886,9.18146727647585,139.935529580012));
#71084=CARTESIAN_POINT('Ctrl Pts',(81.6486856361659,9.24905865828822,139.940304728758));
#71085=CARTESIAN_POINT('Ctrl Pts',(81.6321457760444,9.33469610208402,139.946265985266));
#71086=CARTESIAN_POINT('Ctrl Pts',(81.6281984719859,9.35339934954393,139.947562687596));
#71087=CARTESIAN_POINT('Ctrl Pts',(81.6212939304409,9.38353793248474,139.949644961515));
#71088=CARTESIAN_POINT('Ctrl Pts',(81.6185355334317,9.395016573005,139.950436311492));
#71089=CARTESIAN_POINT('Ctrl Pts',(81.6129949985425,9.41703960326716,139.951951763404));
#71090=CARTESIAN_POINT('Ctrl Pts',(81.610230892546,9.42758785929924,139.952676349238));
#71091=CARTESIAN_POINT('Ctrl Pts',(81.6035551209315,9.4520804060029,139.954356363082));
#71092=CARTESIAN_POINT('Ctrl Pts',(81.5995647671019,9.46600246207649,139.955309460251));
#71093=CARTESIAN_POINT('Ctrl Pts',(81.5858025496379,9.51175673215393,139.958437569274));
#71094=CARTESIAN_POINT('Ctrl Pts',(81.5752576500616,9.54334907755491,139.960590535652));
#71095=CARTESIAN_POINT('Ctrl Pts',(81.5337731745299,9.65624785971019,139.968291296163));
#71096=CARTESIAN_POINT('Ctrl Pts',(81.4974257178194,9.73541750188746,139.973698039324));
#71097=CARTESIAN_POINT('Ctrl Pts',(81.4141641539465,9.88472987117062,139.98435684324));
#71098=CARTESIAN_POINT('Ctrl Pts',(81.3677849887947,9.95486588117745,139.989595164794));
#71099=CARTESIAN_POINT('Ctrl Pts',(81.3077170231935,10.0322932224563,139.995972388889));
#71100=CARTESIAN_POINT('Ctrl Pts',(81.298971634533,10.0432764629132,139.99689214452));
#71101=CARTESIAN_POINT('Ctrl Pts',(81.2863139832169,10.0587671730338,139.998213014843));
#71102=CARTESIAN_POINT('Ctrl Pts',(81.2825144776254,10.0633664479793,139.99860821659));
#71103=CARTESIAN_POINT('Ctrl Pts',(81.2755009163509,10.0717640454966,139.999335560135));
#71104=CARTESIAN_POINT('Ctrl Pts',(81.2722943743604,10.075568584752,139.999667279677));
#71105=CARTESIAN_POINT('Ctrl Pts',(81.2690708798525,10.0793586530483,140.));
#71106=CARTESIAN_POINT('',(78.7475355302757,10.0985848861505,140.));
#71107=CARTESIAN_POINT('Origin',(80.,9.,140.));
#71108=CARTESIAN_POINT('Ctrl Pts',(78.7475355302756,10.0985848861504,140.));
#71109=CARTESIAN_POINT('Ctrl Pts',(78.7492750986987,10.1005681171869,139.999818410898));
#71110=CARTESIAN_POINT('Ctrl Pts',(78.7510193658275,10.1025472028964,139.999636522787));
#71111=CARTESIAN_POINT('Ctrl Pts',(78.770908215588,10.1250057874456,139.997564813153));
#71112=CARTESIAN_POINT('Ctrl Pts',(78.7895488081928,10.1450381433428,139.995644440404));
#71113=CARTESIAN_POINT('Ctrl Pts',(78.8882628677563,10.2460175613479,139.98562143943));
#71114=CARTESIAN_POINT('Ctrl Pts',(78.9759871769111,10.3190590992091,139.977218838742));
#71115=CARTESIAN_POINT('Ctrl Pts',(79.1419499639817,10.4306376570869,139.962791329009));
#71116=CARTESIAN_POINT('Ctrl Pts',(79.2170533914007,10.4730827499196,139.956701369571));
#71117=CARTESIAN_POINT('Ctrl Pts',(79.3118014922645,10.5173259355423,139.949558030066));
#71118=CARTESIAN_POINT('Ctrl Pts',(79.3286173003773,10.5248411387034,139.948309317913));
#71119=CARTESIAN_POINT('Ctrl Pts',(79.3556487262977,10.5363879435193,139.946331440542));
#71120=CARTESIAN_POINT('Ctrl Pts',(79.3657851517762,10.5405998874096,139.945596259446));
#71121=CARTESIAN_POINT('Ctrl Pts',(79.3851089845753,10.5484063894291,139.944206726716));
#71122=CARTESIAN_POINT('Ctrl Pts',(79.394288092677,10.5520201029836,139.94355176061));
#71123=CARTESIAN_POINT('Ctrl Pts',(79.4153287694979,10.5600884833331,139.942061691837));
#71124=CARTESIAN_POINT('Ctrl Pts',(79.4272102356773,10.5644898286818,139.941228374794));
#71125=CARTESIAN_POINT('Ctrl Pts',(79.4585943042953,10.5757102123304,139.939047594908));
#71126=CARTESIAN_POINT('Ctrl Pts',(79.4781758977839,10.5823028996122,139.937707454102));
#71127=CARTESIAN_POINT('Ctrl Pts',(79.6370549675723,10.6325235681068,139.926984125458));
#71128=CARTESIAN_POINT('Ctrl Pts',(79.7814057183628,10.6580351361542,139.918235640159));
#71129=CARTESIAN_POINT('Ctrl Pts',(79.9881845593757,10.6670746420004,139.90544526783));
#71130=CARTESIAN_POINT('Ctrl Pts',(80.0492243989363,10.6663891718741,139.9016274265));
#71131=CARTESIAN_POINT('Ctrl Pts',(80.1248166860646,10.6613834150736,139.896700584619));
#71132=CARTESIAN_POINT('Ctrl Pts',(80.1395369390971,10.6602118731241,139.89573171006));
#71133=CARTESIAN_POINT('Ctrl Pts',(80.1599038879926,10.6583181583504,139.894375639909));
#71134=CARTESIAN_POINT('Ctrl Pts',(80.1655658804903,10.6577624391401,139.893996986679));
#71135=CARTESIAN_POINT('Ctrl Pts',(80.1714021636216,10.6571594160172,139.893604854225));
#71136=CARTESIAN_POINT('Ctrl Pts',(80.171579509769,10.6571410632821,139.893592936825));
#71137=CARTESIAN_POINT('Ctrl Pts',(80.1719340651294,10.6571043144563,139.893569107748));
#71138=CARTESIAN_POINT('Ctrl Pts',(80.1721112743328,10.6570859184089,139.893557196074));
#71139=CARTESIAN_POINT('Ctrl Pts',(80.1724681775636,10.6570488104965,139.893533202193));
#71140=CARTESIAN_POINT('Ctrl Pts',(80.1726478715362,10.6570300978238,139.893521119941));
#71141=CARTESIAN_POINT('Ctrl Pts',(80.1730128166048,10.6569920337717,139.893496578145));
#71142=CARTESIAN_POINT('Ctrl Pts',(80.1731980674868,10.6569726805567,139.893484118503));
#71143=CARTESIAN_POINT('Ctrl Pts',(80.1735779686894,10.6569329277586,139.893458563112));
#71144=CARTESIAN_POINT('Ctrl Pts',(80.1737726186638,10.6569125249414,139.893445467188));
#71145=CARTESIAN_POINT('Ctrl Pts',(80.1741764645885,10.6568701226802,139.893418292312));
#71146=CARTESIAN_POINT('Ctrl Pts',(80.1743856599498,10.6568481179187,139.893404213072));
#71147=CARTESIAN_POINT('Ctrl Pts',(80.1748260242303,10.6568017127244,139.893374570582));
#71148=CARTESIAN_POINT('Ctrl Pts',(80.175057192188,10.6567773035316,139.893359006855));
#71149=CARTESIAN_POINT('Ctrl Pts',(80.1755531972879,10.6567248250234,139.893325606149));
#71150=CARTESIAN_POINT('Ctrl Pts',(80.1758180327483,10.6566967405916,139.893307768348));
#71151=CARTESIAN_POINT('Ctrl Pts',(80.1764020011204,10.6566346721597,139.893268426891));
#71152=CARTESIAN_POINT('Ctrl Pts',(80.176721130876,10.6566006594537,139.893246921666));
#71153=CARTESIAN_POINT('Ctrl Pts',(80.1774569200864,10.6565220243359,139.893197325737));
#71154=CARTESIAN_POINT('Ctrl Pts',(80.1778735723233,10.6564773369607,139.893169231475));
#71155=CARTESIAN_POINT('Ctrl Pts',(80.1786073295496,10.6563983589592,139.89311973797));
#71156=CARTESIAN_POINT('Ctrl Pts',(80.1789244418834,10.6563641344306,139.893098342367));
#71157=CARTESIAN_POINT('Ctrl Pts',(80.1845614758536,10.6557541166304,139.892717909549));
#71158=CARTESIAN_POINT('Ctrl Pts',(80.1898783580145,10.6551528146369,139.892357455688));
#71159=CARTESIAN_POINT('Ctrl Pts',(80.2022343165761,10.653695123613,139.891516011902));
#71160=CARTESIAN_POINT('Ctrl Pts',(80.2092708314008,10.6528194079281,139.891033993502));
#71161=CARTESIAN_POINT('Ctrl Pts',(80.2319915260492,10.6498443361182,139.889468874148));
#71162=CARTESIAN_POINT('Ctrl Pts',(80.2476509081041,10.6475665037098,139.888376764884));
#71163=CARTESIAN_POINT('Ctrl Pts',(80.3411772974491,10.6325986329934,139.881782820596));
#71164=CARTESIAN_POINT('Ctrl Pts',(80.418088524781,10.614614450719,139.876068361954));
#71165=CARTESIAN_POINT('Ctrl Pts',(80.5564340513755,10.5717151770512,139.865536547396));
#71166=CARTESIAN_POINT('Ctrl Pts',(80.6182268478162,10.5484520551824,139.860733731884));
#71167=CARTESIAN_POINT('Ctrl Pts',(80.7461488655859,10.4914112409354,139.850690609429));
#71168=CARTESIAN_POINT('Ctrl Pts',(80.8117374630785,10.4567534612047,139.845481557463));
#71169=CARTESIAN_POINT('Ctrl Pts',(80.8899158582108,10.4085172618325,139.839211264558));
#71170=CARTESIAN_POINT('Ctrl Pts',(80.9048735959079,10.3989549417533,139.838008313772));
#71171=CARTESIAN_POINT('Ctrl Pts',(80.9286833317609,10.3831919451638,139.836087464075));
#71172=CARTESIAN_POINT('Ctrl Pts',(80.937632473553,10.3771412570411,139.83536409414));
#71173=CARTESIAN_POINT('Ctrl Pts',(80.9546271750259,10.3654083472983,139.833987438966));
#71174=CARTESIAN_POINT('Ctrl Pts',(80.9626824004861,10.3597410051297,139.833333632863));
#71175=CARTESIAN_POINT('Ctrl Pts',(80.9809536269438,10.346642326696,139.831847381941));
#71176=CARTESIAN_POINT('Ctrl Pts',(80.9911363918032,10.3391655019623,139.831016715976));
#71177=CARTESIAN_POINT('Ctrl Pts',(81.0180920377573,10.3188970796573,139.828810584563));
#71178=CARTESIAN_POINT('Ctrl Pts',(81.0347090196051,10.30590130274,139.827443034891));
#71179=CARTESIAN_POINT('Ctrl Pts',(81.1448734339632,10.2163208233676,139.818312653203));
#71180=CARTESIAN_POINT('Ctrl Pts',(81.2300929659983,10.1300649017884,139.810966409533));
#71181=CARTESIAN_POINT('Ctrl Pts',(81.3644670124966,9.96066167524757,139.797749486242));
#71182=CARTESIAN_POINT('Ctrl Pts',(81.4171750095174,9.88105099238715,139.791907767027));
#71183=CARTESIAN_POINT('Ctrl Pts',(81.4685531305597,9.78679926524852,139.784889721542));
#71184=CARTESIAN_POINT('Ctrl Pts',(81.4742087798991,9.77615065143372,139.784095347322));
#71185=CARTESIAN_POINT('Ctrl Pts',(81.4827223790021,9.75969220912737,139.782863862527));
#71186=CARTESIAN_POINT('Ctrl Pts',(81.4856630076555,9.75392528141965,139.782431667568));
#71187=CARTESIAN_POINT('Ctrl Pts',(81.4910294417248,9.74324773934362,139.781629910425));
#71188=CARTESIAN_POINT('Ctrl Pts',(81.4934647279951,9.73834213053225,139.781260939473));
#71189=CARTESIAN_POINT('Ctrl Pts',(81.4989767863981,9.72709986391266,139.78041395824));
#71190=CARTESIAN_POINT('Ctrl Pts',(81.5020375687078,9.72075568393222,139.779935008673));
#71191=CARTESIAN_POINT('Ctrl Pts',(81.5114663439987,9.70089145713497,139.778432744825));
#71192=CARTESIAN_POINT('Ctrl Pts',(81.5176925032422,9.68730544199477,139.777401506352));
#71193=CARTESIAN_POINT('Ctrl Pts',(81.5653593419637,9.57948550333323,139.769198242541));
#71194=CARTESIAN_POINT('Ctrl Pts',(81.5981641547459,9.48168577394389,139.761657185607));
#71195=CARTESIAN_POINT('Ctrl Pts',(81.6480358012736,9.26968123022381,139.74581391735));
#71196=CARTESIAN_POINT('Ctrl Pts',(81.6627089976902,9.15542873537538,139.737577113301));
#71197=CARTESIAN_POINT('Ctrl Pts',(81.6659732073318,9.02138184528976,139.728404304849));
#71198=CARTESIAN_POINT('Ctrl Pts',(81.6661089783952,9.00219922893443,139.727102401817));
#71199=CARTESIAN_POINT('Ctrl Pts',(81.6658009943218,8.97198667939606,139.725068057421));
#71200=CARTESIAN_POINT('Ctrl Pts',(81.6655789773034,8.96095669877791,139.724328745244));
#71201=CARTESIAN_POINT('Ctrl Pts',(81.6649566872603,8.94026054187571,139.722947618986));
#71202=CARTESIAN_POINT('Ctrl Pts',(81.6645817507167,8.93059412650554,139.722305038663));
#71203=CARTESIAN_POINT('Ctrl Pts',(81.6635486081921,8.90885003708972,139.720864934414));
#71204=CARTESIAN_POINT('Ctrl Pts',(81.6628430220334,8.89677507769214,139.720068930335));
#71205=CARTESIAN_POINT('Ctrl Pts',(81.6603716121573,8.86114797964545,139.717730493693));
#71206=CARTESIAN_POINT('Ctrl Pts',(81.6582363706974,8.83762388309946,139.716199637637));
#71207=CARTESIAN_POINT('Ctrl Pts',(81.6442645692347,8.71315789442467,139.708156235552));
#71208=CARTESIAN_POINT('Ctrl Pts',(81.6237101542136,8.61340845804988,139.701924276533));
#71209=CARTESIAN_POINT('Ctrl Pts',(81.5707057125444,8.43877123795905,139.690787681328));
#71210=CARTESIAN_POINT('Ctrl Pts',(81.5416217936874,8.36321544518455,139.685881605787));
#71211=CARTESIAN_POINT('Ctrl Pts',(81.4965111736758,8.2674455312216,139.679212331265));
#71212=CARTESIAN_POINT('Ctrl Pts',(81.4853439508587,8.24505963413609,139.677618983377));
#71213=CARTESIAN_POINT('Ctrl Pts',(81.4655964689787,8.20760920551813,139.674880336749));
#71214=CARTESIAN_POINT('Ctrl Pts',(81.4572771121725,8.19241127962502,139.673747993319));
#71215=CARTESIAN_POINT('Ctrl Pts',(81.4450533848761,8.1708848495053,139.672109901386));
#71216=CARTESIAN_POINT('Ctrl Pts',(81.4413409920195,8.16444787272541,139.671615621108));
#71217=CARTESIAN_POINT('Ctrl Pts',(81.4348113091426,8.15329896353987,139.6707513724));
#71218=CARTESIAN_POINT('Ctrl Pts',(81.4320135987525,8.14857578744658,139.670382656971));
#71219=CARTESIAN_POINT('Ctrl Pts',(81.4259695167432,8.13848605742688,139.669589357307));
#71220=CARTESIAN_POINT('Ctrl Pts',(81.4227162194236,8.13312406212703,139.669164355312));
#71221=CARTESIAN_POINT('Ctrl Pts',(81.4137344797883,8.118507353448,139.667996697368));
#71222=CARTESIAN_POINT('Ctrl Pts',(81.407945615409,8.10929039880981,139.667250335225));
#71223=CARTESIAN_POINT('Ctrl Pts',(81.3754565030873,8.05866978534001,139.663098084314));
#71224=CARTESIAN_POINT('Ctrl Pts',(81.3470224720968,8.01841319804142,139.659598300316));
#71225=CARTESIAN_POINT('Ctrl Pts',(81.2642198516651,7.91156707465608,139.649869030341));
#71226=CARTESIAN_POINT('Ctrl Pts',(81.2064152620534,7.84782792978545,139.643566876989));
#71227=CARTESIAN_POINT('Ctrl Pts',(81.0835143179181,7.73174766910833,139.631348866015));
#71228=CARTESIAN_POINT('Ctrl Pts',(81.0188815933741,7.67926111943427,139.625444129004));
#71229=CARTESIAN_POINT('Ctrl Pts',(80.9317796281978,7.61874426909228,139.618152116356));
#71230=CARTESIAN_POINT('Ctrl Pts',(80.9127002713673,7.60606349685692,139.616591653707));
#71231=CARTESIAN_POINT('Ctrl Pts',(80.8833640619185,7.58742635245284,139.614246262621));
#71232=CARTESIAN_POINT('Ctrl Pts',(80.873295797785,7.58117977257087,139.613450695429));
#71233=CARTESIAN_POINT('Ctrl Pts',(80.8556535575413,7.57049307713706,139.612072572033));
#71234=CARTESIAN_POINT('Ctrl Pts',(80.8481096451488,7.56600450213261,139.611488264746));
#71235=CARTESIAN_POINT('Ctrl Pts',(80.8310200940209,7.55601837457729,139.610175603773));
#71236=CARTESIAN_POINT('Ctrl Pts',(80.821454637414,7.55055540992867,139.609448517601));
#71237=CARTESIAN_POINT('Ctrl Pts',(80.7953476009133,7.53598678289165,139.607484166069));
#71238=CARTESIAN_POINT('Ctrl Pts',(80.7787039561566,7.52706663359772,139.606253500638));
#71239=CARTESIAN_POINT('Ctrl Pts',(80.6672312942661,7.46974069865266,139.598145144544));
#71240=CARTESIAN_POINT('Ctrl Pts',(80.5680972936347,7.43023547044236,139.591592283712));
#71241=CARTESIAN_POINT('Ctrl Pts',(80.3866011081683,7.37737548465106,139.580037400198));
#71242=CARTESIAN_POINT('Ctrl Pts',(80.3057421837066,7.36021629637196,139.575027261048));
#71243=CARTESIAN_POINT('Ctrl Pts',(80.1866818205355,7.34406507866575,139.567456166848));
#71244=CARTESIAN_POINT('Ctrl Pts',(80.149255105943,7.34027321812248,139.565047941981));
#71245=CARTESIAN_POINT('Ctrl Pts',(80.1018795857936,7.33708865866905,139.561928092699));
#71246=CARTESIAN_POINT('Ctrl Pts',(80.0920182106946,7.33651383645002,139.561274784604));
#71247=CARTESIAN_POINT('Ctrl Pts',(80.0761608197798,7.3357309356564,139.560217137779));
#71248=CARTESIAN_POINT('Ctrl Pts',(80.0701675992035,7.33546748479596,139.559815775111));
#71249=CARTESIAN_POINT('Ctrl Pts',(80.0586099431458,7.33502196097285,139.559038396566));
#71250=CARTESIAN_POINT('Ctrl Pts',(80.0530458311416,7.3348354039381,139.5586626271));
#71251=CARTESIAN_POINT('Ctrl Pts',(80.0406526779747,7.33448205531283,139.557822405884));
#71252=CARTESIAN_POINT('Ctrl Pts',(80.0338233404751,7.33432937173224,139.557357199541));
#71253=CARTESIAN_POINT('Ctrl Pts',(80.0135473697047,7.33400080666893,139.555969883116));
#71254=CARTESIAN_POINT('Ctrl Pts',(80.0000996997849,7.33394573753342,139.555041755501));
#71255=CARTESIAN_POINT('Ctrl Pts',(79.8797815025852,7.33490965958925,139.546674444081));
#71256=CARTESIAN_POINT('Ctrl Pts',(79.7732490591185,7.3460475246641,139.538836936621));
#71257=CARTESIAN_POINT('Ctrl Pts',(79.5949919508074,7.3822377378563,139.525617369195));
#71258=CARTESIAN_POINT('Ctrl Pts',(79.5225431689758,7.40211911086728,139.52020977534));
#71259=CARTESIAN_POINT('Ctrl Pts',(79.4099453776348,7.44136454264681,139.511829421572));
#71260=CARTESIAN_POINT('Ctrl Pts',(79.3688075776359,7.4575650095866,139.508771661348));
#71261=CARTESIAN_POINT('Ctrl Pts',(79.3144889245214,7.48149406073892,139.504737646618));
#71262=CARTESIAN_POINT('Ctrl Pts',(79.3007022349305,7.48779353780562,139.503714000649));
#71263=CARTESIAN_POINT('Ctrl Pts',(79.27776794372,7.49865351527179,139.502011045577));
#71264=CARTESIAN_POINT('Ctrl Pts',(79.2685731154254,7.50311151688941,139.501328263302));
#71265=CARTESIAN_POINT('Ctrl Pts',(79.2505173739298,7.51207172159102,139.499987186907));
#71266=CARTESIAN_POINT('Ctrl Pts',(79.2416545925398,7.51656917292258,139.499328762384));
#71267=CARTESIAN_POINT('Ctrl Pts',(79.2201912948159,7.52770343183762,139.49773354055));
#71268=CARTESIAN_POINT('Ctrl Pts',(79.2076344596344,7.534423092265,139.496799692401));
#71269=CARTESIAN_POINT('Ctrl Pts',(79.1648697993957,7.55801846394256,139.493615639117));
#71270=CARTESIAN_POINT('Ctrl Pts',(79.1351011633426,7.57567438042733,139.491393086056));
#71271=CARTESIAN_POINT('Ctrl Pts',(79.0013945651311,7.66071538902914,139.481340113618));
#71272=CARTESIAN_POINT('Ctrl Pts',(78.9046264916226,7.7386299123878,139.473897338724));
#71273=CARTESIAN_POINT('Ctrl Pts',(78.7643433145804,7.88000915540193,139.461665691532));
#71274=CARTESIAN_POINT('Ctrl Pts',(78.7149939414714,7.93699322549024,139.456984746963));
#71275=CARTESIAN_POINT('Ctrl Pts',(78.6626904070687,8.00637349674128,139.451299675603));
#71276=CARTESIAN_POINT('Ctrl Pts',(78.6558042869799,8.01570916803908,139.450534934193));
#71277=CARTESIAN_POINT('Ctrl Pts',(78.6452926771124,8.0302760365412,139.449340714995));
#71278=CARTESIAN_POINT('Ctrl Pts',(78.6415985710281,8.03545759533834,139.448915736125));
#71279=CARTESIAN_POINT('Ctrl Pts',(78.6347704093569,8.04515218274614,139.448120005445));
#71280=CARTESIAN_POINT('Ctrl Pts',(78.6316288854985,8.04965970361618,139.447749764622));
#71281=CARTESIAN_POINT('Ctrl Pts',(78.6244223298619,8.06010962891752,139.446890876136));
#71282=CARTESIAN_POINT('Ctrl Pts',(78.6203734702877,8.06606291971006,139.446401184483));
#71283=CARTESIAN_POINT('Ctrl Pts',(78.6076290978192,8.08506548486369,139.4448373713));
#71284=CARTESIAN_POINT('Ctrl Pts',(78.5990794698452,8.09821093365397,139.443754464852));
#71285=CARTESIAN_POINT('Ctrl Pts',(78.5460191682421,8.18236943841616,139.436824183178));
#71286=CARTESIAN_POINT('Ctrl Pts',(78.5067388158411,8.25652951784427,139.430735061346));
#71287=CARTESIAN_POINT('Ctrl Pts',(78.4427463578755,8.40308167274243,139.419094545706));
#71288=CARTESIAN_POINT('Ctrl Pts',(78.4171000601497,8.47485264748105,139.413558033869));
#71289=CARTESIAN_POINT('Ctrl Pts',(78.385402981615,8.58733593744271,139.405238400553));
#71290=CARTESIAN_POINT('Ctrl Pts',(78.3757958706539,8.62693625566892,139.402373492433));
#71291=CARTESIAN_POINT('Ctrl Pts',(78.3618143819876,8.69544236650391,139.397530264804));
#71292=CARTESIAN_POINT('Ctrl Pts',(78.3567311470748,8.72418278881758,139.395531728685));
#71293=CARTESIAN_POINT('Ctrl Pts',(78.3504789670484,8.76589483573377,139.39267745763));
#71294=CARTESIAN_POINT('Ctrl Pts',(78.3487030801407,8.77876852581196,139.391802837263));
#71295=CARTESIAN_POINT('Ctrl Pts',(78.345850162255,8.80140314295193,139.390275746978));
#71296=CARTESIAN_POINT('Ctrl Pts',(78.3447084797235,8.81115512359756,139.389621273678));
#71297=CARTESIAN_POINT('Ctrl Pts',(78.3425106275818,8.83148313808281,139.388263988864));
#71298=CARTESIAN_POINT('Ctrl Pts',(78.3414693157658,8.84206035732694,139.387561672131));
#71299=CARTESIAN_POINT('Ctrl Pts',(78.3390131433626,8.86972146348093,139.385734767674));
#71300=CARTESIAN_POINT('Ctrl Pts',(78.3377605825241,8.88681877531719,139.384615282217));
#71301=CARTESIAN_POINT('Ctrl Pts',(78.333402225627,8.96227584006357,139.379713452031));
#71302=CARTESIAN_POINT('Ctrl Pts',(78.3331042628764,9.02075953004453,139.376018566448));
#71303=CARTESIAN_POINT('Ctrl Pts',(78.3408872562269,9.18441018408281,139.36582617507));
#71304=CARTESIAN_POINT('Ctrl Pts',(78.3558701181429,9.28896149901275,139.359496157283));
#71305=CARTESIAN_POINT('Ctrl Pts',(78.3957051395104,9.45377587821222,139.3490300654));
#71306=CARTESIAN_POINT('Ctrl Pts',(78.4143721582719,9.51522510607317,139.345008208124));
#71307=CARTESIAN_POINT('Ctrl Pts',(78.4365419166502,9.5754605308294,139.340805721476));
#71308=CARTESIAN_POINT('Ctrl Pts',(78.4365506449801,9.5754842438558,139.340804067081));
#71309=CARTESIAN_POINT('Ctrl Pts',(78.4365593737638,9.57550795670799,139.340802412607));
#71310=CARTESIAN_POINT('Origin',(80.,-9.,141.545925280538));
#71311=CARTESIAN_POINT('',(81.2520391107128,-7.37076839346109,129.106054343781));
#71312=CARTESIAN_POINT('',(81.2492121870567,-7.37445590553645,129.047846843673));
#71313=CARTESIAN_POINT('',(81.2520391107129,-7.37076839346111,141.545925280538));
#71314=CARTESIAN_POINT('',(81.8174278887594,-8.04137941204074,129.));
#71315=CARTESIAN_POINT('Ctrl Pts',(81.2492121870567,-7.37445590553645,129.047846843673));
#71316=CARTESIAN_POINT('Ctrl Pts',(81.4831295299336,-7.55380834072825,129.031897895782));
#71317=CARTESIAN_POINT('Ctrl Pts',(81.6801942371869,-7.78120112171703,129.015948947891));
#71318=CARTESIAN_POINT('Ctrl Pts',(81.8174278887595,-8.04137941204082,129.));
#71319=CARTESIAN_POINT('',(82.0533682620167,-9.07534150942548,129.000000008563));
#71320=CARTESIAN_POINT('Origin',(80.,-9.,129.));
#71321=CARTESIAN_POINT('Ctrl Pts',(81.2520391107129,-7.37076839346109,129.106054343781));
#71322=CARTESIAN_POINT('Ctrl Pts',(81.3081324823019,-7.41387527574805,129.102199425929));
#71323=CARTESIAN_POINT('Ctrl Pts',(81.3621028898732,-7.45996383129776,129.098344508077));
#71324=CARTESIAN_POINT('Ctrl Pts',(81.4136153569759,-7.50879606189431,129.094489590225));
#71325=CARTESIAN_POINT('Ctrl Pts',(81.4662255514254,-7.55866890417088,129.090552524322));
#71326=CARTESIAN_POINT('Ctrl Pts',(81.5162713772154,-7.61140346509638,129.08661545842));
#71327=CARTESIAN_POINT('Ctrl Pts',(81.5634292255428,-7.66670085156455,129.082678392517));
#71328=CARTESIAN_POINT('Ctrl Pts',(81.6094922174622,-7.72071440723755,129.078832732859));
#71329=CARTESIAN_POINT('Ctrl Pts',(81.6527995488012,-7.77717267636535,129.074987073202));
#71330=CARTESIAN_POINT('Ctrl Pts',(81.6930864251896,-7.83575950966368,129.071141413544));
#71331=CARTESIAN_POINT('Ctrl Pts',(81.7333528037562,-7.89431653418604,129.067297710544));
#71332=CARTESIAN_POINT('Ctrl Pts',(81.7706014995003,-7.95499957180025,129.063454007545));
#71333=CARTESIAN_POINT('Ctrl Pts',(81.804609430456,-8.01746126488105,129.059610304545));
#71334=CARTESIAN_POINT('Ctrl Pts',(81.8386116248341,-8.07991242170324,129.055767249915));
#71335=CARTESIAN_POINT('Ctrl Pts',(81.8693739064979,-8.14414120838439,129.051924195285));
#71336=CARTESIAN_POINT('Ctrl Pts',(81.8967186837959,-8.20977484408587,129.048081140655));
#71337=CARTESIAN_POINT('Ctrl Pts',(81.9252282934647,-8.27820434031468,129.044074379647));
#71338=CARTESIAN_POINT('Ctrl Pts',(81.9500224558933,-8.348160541956,129.04006761864));
#71339=CARTESIAN_POINT('Ctrl Pts',(81.9709560850656,-8.41919911050101,129.036060857632));
#71340=CARTESIAN_POINT('Ctrl Pts',(81.9910610267401,-8.48742551622748,129.03221270996));
#71341=CARTESIAN_POINT('Ctrl Pts',(82.0076052835568,-8.55664969729867,129.028364562288));
#71342=CARTESIAN_POINT('Ctrl Pts',(82.0205122847536,-8.62646597255455,129.024516414616));
#71343=CARTESIAN_POINT('Ctrl Pts',(82.0334284198522,-8.6963316547163,129.020665543725));
#71344=CARTESIAN_POINT('Ctrl Pts',(82.0427021171196,-8.7667897800782,129.016814672833));
#71345=CARTESIAN_POINT('Ctrl Pts',(82.0483086557833,-8.83742935952861,129.012963801941));
#71346=CARTESIAN_POINT('Ctrl Pts',(82.0539242775961,-8.90818338210834,129.009106692256));
#71347=CARTESIAN_POINT('Ctrl Pts',(82.0558608834404,-8.9791189577832,129.005249582572));
#71348=CARTESIAN_POINT('Ctrl Pts',(82.0541457913538,-9.04982600087946,129.001392472887));
#71349=CARTESIAN_POINT('Ctrl Pts',(82.0539394015318,-9.05833470670729,129.000928318112));
#71350=CARTESIAN_POINT('Ctrl Pts',(82.05368019249,-9.06684011174075,129.000464163338));
#71351=CARTESIAN_POINT('Ctrl Pts',(82.0533682620167,-9.07534150942548,129.000000008563));
#71352=CARTESIAN_POINT('Origin',(80.,-9.,141.545925280538));
#71353=CARTESIAN_POINT('',(81.2520391107129,-7.37076839346111,129.806138766351));
#71354=CARTESIAN_POINT('',(81.2520391107129,-7.37076839346113,129.747865110012));
#71355=CARTESIAN_POINT('',(81.2520391107129,-7.37076839346111,141.545925280538));
#71356=CARTESIAN_POINT('',(77.9454433123729,-9.00149860204779,129.295925300346));
#71357=CARTESIAN_POINT('Ctrl Pts',(81.2520391107129,-7.37076839346113,129.747865110012));
#71358=CARTESIAN_POINT('Ctrl Pts',(81.3085193358146,-7.41417256664642,129.744007244271));
#71359=CARTESIAN_POINT('Ctrl Pts',(81.3627900147932,-7.46055568534263,129.740149378531));
#71360=CARTESIAN_POINT('Ctrl Pts',(81.4145261450971,-7.50965998935252,129.73629151279));
#71361=CARTESIAN_POINT('Ctrl Pts',(81.4662398813796,-7.55874303852898,129.732435316929));
#71362=CARTESIAN_POINT('Ctrl Pts',(81.5154208944419,-7.61054460151153,129.728579121068));
#71363=CARTESIAN_POINT('Ctrl Pts',(81.5617787946249,-7.66476797553387,129.724722925207));
#71364=CARTESIAN_POINT('Ctrl Pts',(81.6081321217098,-7.71898600054751,129.720867109751));
#71365=CARTESIAN_POINT('Ctrl Pts',(81.6516625743354,-7.77562499232182,129.717011294294));
#71366=CARTESIAN_POINT('Ctrl Pts',(81.6921192009196,-7.83435418227522,129.713155478838));
#71367=CARTESIAN_POINT('Ctrl Pts',(81.7326518844035,-7.89319378084367,129.709292414597));
#71368=CARTESIAN_POINT('Ctrl Pts',(81.7700988981036,-7.95413104048772,129.705429350357));
#71369=CARTESIAN_POINT('Ctrl Pts',(81.8042518642402,-8.01680481445141,129.701566286116));
#71370=CARTESIAN_POINT('Ctrl Pts',(81.8383883949273,-8.07944842788261,129.6977050809));
#71371=CARTESIAN_POINT('Ctrl Pts',(81.8692338552675,-8.14382643622838,129.693843875683));
#71372=CARTESIAN_POINT('Ctrl Pts',(81.8966275669693,-8.2095561786488,129.689982670467));
#71373=CARTESIAN_POINT('Ctrl Pts',(81.9240726505379,-8.2754091851093,129.68611422427));
#71374=CARTESIAN_POINT('Ctrl Pts',(81.94805288481,-8.34261853290929,129.682245778074));
#71375=CARTESIAN_POINT('Ctrl Pts',(81.9684568199746,-8.41078415636068,129.678377331878));
#71376=CARTESIAN_POINT('Ctrl Pts',(81.9888137867372,-8.47879286741362,129.674517790568));
#71377=CARTESIAN_POINT('Ctrl Pts',(82.0056108665842,-8.5477529730635,129.670658249259));
#71378=CARTESIAN_POINT('Ctrl Pts',(82.0187884996638,-8.61725915278709,129.666798707949));
#71379=CARTESIAN_POINT('Ctrl Pts',(82.0319999878966,-8.68694390345363,129.662929250947));
#71380=CARTESIAN_POINT('Ctrl Pts',(82.0416249747741,-8.75744965513442,129.659059793944));
#71381=CARTESIAN_POINT('Ctrl Pts',(82.0475698224613,-8.82837428908914,129.655190336942));
#71382=CARTESIAN_POINT('Ctrl Pts',(82.0535058275942,-8.89919342750028,129.651326635492));
#71383=CARTESIAN_POINT('Ctrl Pts',(82.0557725190415,-8.97042973138174,129.647462934043));
#71384=CARTESIAN_POINT('Ctrl Pts',(82.0543273941934,-9.04167157264538,129.643599232593));
#71385=CARTESIAN_POINT('Ctrl Pts',(82.0528839599576,-9.11283007000717,129.639740051183));
#71386=CARTESIAN_POINT('Ctrl Pts',(82.0477373446454,-9.18399360866671,129.635880869773));
#71387=CARTESIAN_POINT('Ctrl Pts',(82.0388970253626,-9.25474788020187,129.632021688364));
#71388=CARTESIAN_POINT('Ctrl Pts',(82.030062258362,-9.32545771356014,129.628164930765));
#71389=CARTESIAN_POINT('Ctrl Pts',(82.0175384501078,-9.39575830898987,129.624308173166));
#71390=CARTESIAN_POINT('Ctrl Pts',(82.0013870127015,-9.4652392802525,129.620451415567));
#71391=CARTESIAN_POINT('Ctrl Pts',(81.9852403197715,-9.53469984151569,129.616595790889));
#71392=CARTESIAN_POINT('Ctrl Pts',(81.9654682231559,-9.60334078380567,129.612740166211));
#71393=CARTESIAN_POINT('Ctrl Pts',(81.9421831305996,-9.67076243910528,129.608884541532));
#71394=CARTESIAN_POINT('Ctrl Pts',(81.9188970937224,-9.73818682867246,129.60502876049));
#71395=CARTESIAN_POINT('Ctrl Pts',(81.8920979386739,-9.80439137473934,129.601172979448));
#71396=CARTESIAN_POINT('Ctrl Pts',(81.8619472202092,-9.86899373510695,129.597317198406));
#71397=CARTESIAN_POINT('Ctrl Pts',(81.831764901583,-9.9336638034805,129.593457376223));
#71398=CARTESIAN_POINT('Ctrl Pts',(81.7982242132673,-9.9967278930938,129.58959755404));
#71399=CARTESIAN_POINT('Ctrl Pts',(81.7615335686011,-10.0578265685789,129.585737731857));
#71400=CARTESIAN_POINT('Ctrl Pts',(81.7248221155494,-10.1189598949895,129.581875720651));
#71401=CARTESIAN_POINT('Ctrl Pts',(81.6849574213982,-10.1781251853909,129.578013709445));
#71402=CARTESIAN_POINT('Ctrl Pts',(81.6421907782822,-10.2349927166687,129.574151698238));
#71403=CARTESIAN_POINT('Ctrl Pts',(81.5993493071618,-10.2919597480142,129.570282929743));
#71404=CARTESIAN_POINT('Ctrl Pts',(81.5535960615509,-10.3466206209628,129.566414161247));
#71405=CARTESIAN_POINT('Ctrl Pts',(81.5052216076061,-10.3986799042296,129.562545392751));
#71406=CARTESIAN_POINT('Ctrl Pts',(81.4765469614202,-10.4295387854496,129.560252125153));
#71407=CARTESIAN_POINT('Ctrl Pts',(81.4469520009933,-10.4594842601665,129.557958857556));
#71408=CARTESIAN_POINT('Ctrl Pts',(81.4165027389574,-10.4884614717977,129.555665589958));
#71409=CARTESIAN_POINT('Ctrl Pts',(81.3651794348254,-10.5373035831004,129.551800206612));
#71410=CARTESIAN_POINT('Ctrl Pts',(81.31122528226,-10.5835848618398,129.547934823266));
#71411=CARTESIAN_POINT('Ctrl Pts',(81.254926402395,-10.6270086929921,129.544069439919));
#71412=CARTESIAN_POINT('Ctrl Pts',(81.1987116344752,-10.6703676478465,129.540209831553));
#71413=CARTESIAN_POINT('Ctrl Pts',(81.1401594746294,-10.7108773337765,129.536350223187));
#71414=CARTESIAN_POINT('Ctrl Pts',(81.0795918236439,-10.7482788841661,129.532490614821));
#71415=CARTESIAN_POINT('Ctrl Pts',(81.019095246917,-10.7856365449972,129.528635535586));
#71416=CARTESIAN_POINT('Ctrl Pts',(80.9565882888255,-10.819893060054,129.524780456351));
#71417=CARTESIAN_POINT('Ctrl Pts',(80.892423346155,-10.850831741066,129.520925377115));
#71418=CARTESIAN_POINT('Ctrl Pts',(80.8282988035791,-10.8817509421941,129.517072725149));
#71419=CARTESIAN_POINT('Ctrl Pts',(80.762518784844,-10.9093562425956,129.513220073182));
#71420=CARTESIAN_POINT('Ctrl Pts',(80.6954606021694,-10.9334766906612,129.509367421215));
#71421=CARTESIAN_POINT('Ctrl Pts',(80.6284220946006,-10.9575900617029,129.50551589963));
#71422=CARTESIAN_POINT('Ctrl Pts',(80.5601066253927,-10.9782204454682,129.501664378046));
#71423=CARTESIAN_POINT('Ctrl Pts',(80.4909101913095,-10.9952455354087,129.497812856461));
#71424=CARTESIAN_POINT('Ctrl Pts',(80.421710794651,-11.0122713542612,129.493961169977));
#71425=CARTESIAN_POINT('Ctrl Pts',(80.3516308314874,-11.0256914586866,129.490109483493));
#71426=CARTESIAN_POINT('Ctrl Pts',(80.2810784152267,-11.0354342256614,129.486257797009));
#71427=CARTESIAN_POINT('Ctrl Pts',(80.2104512222903,-11.045187318742,129.482402028222));
#71428=CARTESIAN_POINT('Ctrl Pts',(80.1393510599224,-11.0512552274711,129.478546259435));
#71429=CARTESIAN_POINT('Ctrl Pts',(80.0681922209285,-11.0536181201735,129.474690490649));
#71430=CARTESIAN_POINT('Ctrl Pts',(79.9969926693478,-11.0559823647736,129.470832515835));
#71431=CARTESIAN_POINT('Ctrl Pts',(79.9257348612537,-11.0546373832113,129.466974541022));
#71432=CARTESIAN_POINT('Ctrl Pts',(79.8548313680584,-11.0496154836457,129.463116566208));
#71433=CARTESIAN_POINT('Ctrl Pts',(79.7838023847573,-11.0445846959607,129.459251763273));
#71434=CARTESIAN_POINT('Ctrl Pts',(79.7131294516034,-11.0358640575065,129.455386960338));
#71435=CARTESIAN_POINT('Ctrl Pts',(79.6432176148211,-11.0235374699091,129.451522157403));
#71436=CARTESIAN_POINT('Ctrl Pts',(79.6010712876026,-11.0161063907345,129.449192262257));
#71437=CARTESIAN_POINT('Ctrl Pts',(79.5592013425454,-11.0073657984892,129.446862367112));
#71438=CARTESIAN_POINT('Ctrl Pts',(79.5176937268385,-10.9973427901512,129.444532471966));
#71439=CARTESIAN_POINT('Ctrl Pts',(79.4486461692916,-10.980669602997,129.440656711665));
#71440=CARTESIAN_POINT('Ctrl Pts',(79.3803310897322,-10.9603796507532,129.436780951364));
#71441=CARTESIAN_POINT('Ctrl Pts',(79.3131544468131,-10.9365538331189,129.432905191063));
#71442=CARTESIAN_POINT('Ctrl Pts',(79.2460779854487,-10.9127635472906,129.429035210743));
#71443=CARTESIAN_POINT('Ctrl Pts',(79.1801370428466,-10.8854480245579,129.425165230423));
#71444=CARTESIAN_POINT('Ctrl Pts',(79.1157251296031,-10.8547386651721,129.421295250102));
#71445=CARTESIAN_POINT('Ctrl Pts',(79.0513895511559,-10.8240656995616,129.41742985611));
#71446=CARTESIAN_POINT('Ctrl Pts',(78.9885798369927,-10.7900070947805,129.413564462118));
#71447=CARTESIAN_POINT('Ctrl Pts',(78.9276704924502,-10.752742704945,129.409699068125));
#71448=CARTESIAN_POINT('Ctrl Pts',(78.8668000421066,-10.7155021106142,129.405836142414));
#71449=CARTESIAN_POINT('Ctrl Pts',(78.8078279653701,-10.6750600450864,129.401973216703));
#71450=CARTESIAN_POINT('Ctrl Pts',(78.7511037956164,-10.6316420665012,129.398110290992));
#71451=CARTESIAN_POINT('Ctrl Pts',(78.6943970463681,-10.5882374219697,129.394248551621));
#71452=CARTESIAN_POINT('Ctrl Pts',(78.6399372174938,-10.5418589729753,129.390386812249));
#71453=CARTESIAN_POINT('Ctrl Pts',(78.5880430834521,-10.4927743393804,129.386525072878));
#71454=CARTESIAN_POINT('Ctrl Pts',(78.5361476869729,-10.4436885116952,129.382663239561));
#71455=CARTESIAN_POINT('Ctrl Pts',(78.4868184593472,-10.3918967028469,129.378801406244));
#71456=CARTESIAN_POINT('Ctrl Pts',(78.4403381714333,-10.3377042060979,129.374939572927));
#71457=CARTESIAN_POINT('Ctrl Pts',(78.393810886182,-10.2834569140116,129.371073834818));
#71458=CARTESIAN_POINT('Ctrl Pts',(78.3501386070332,-10.2268044562488,129.367208096709));
#71459=CARTESIAN_POINT('Ctrl Pts',(78.3095639575526,-10.1680854202047,129.3633423586));
#71460=CARTESIAN_POINT('Ctrl Pts',(78.2689670491438,-10.109334171367,129.359474499777));
#71461=CARTESIAN_POINT('Ctrl Pts',(78.2314714082485,-10.0485144990275,129.355606640955));
#71462=CARTESIAN_POINT('Ctrl Pts',(78.1972749688131,-9.98599189876595,129.351738782133));
#71463=CARTESIAN_POINT('Ctrl Pts',(78.1630202938598,-9.92336282437823,129.347864336462));
#71464=CARTESIAN_POINT('Ctrl Pts',(78.1320762482958,-9.859025468056,129.343989890791));
#71465=CARTESIAN_POINT('Ctrl Pts',(78.1045933769319,-9.79336706241788,129.340115445121));
#71466=CARTESIAN_POINT('Ctrl Pts',(78.0887134735239,-9.75542891812244,129.337876748072));
#71467=CARTESIAN_POINT('Ctrl Pts',(78.0739882226127,-9.71705005416845,129.335638051023));
#71468=CARTESIAN_POINT('Ctrl Pts',(78.0604390161882,-9.67830727002969,129.333399353975));
#71469=CARTESIAN_POINT('Ctrl Pts',(78.0332608353717,-9.60059361214667,129.328908780042));
#71470=CARTESIAN_POINT('Ctrl Pts',(78.0107314285335,-9.52117080928538,129.324418206109));
#71471=CARTESIAN_POINT('Ctrl Pts',(77.9930364419773,-9.44056195849032,129.319927632176));
#71472=CARTESIAN_POINT('Ctrl Pts',(77.9754996317223,-9.36067367393154,129.315477199691));
#71473=CARTESIAN_POINT('Ctrl Pts',(77.9627112852818,-9.27962060760744,129.311026767205));
#71474=CARTESIAN_POINT('Ctrl Pts',(77.9548055732078,-9.19793261256783,129.30657633472));
#71475=CARTESIAN_POINT('Ctrl Pts',(77.9484987710017,-9.13276580374609,129.303025990722));
#71476=CARTESIAN_POINT('Ctrl Pts',(77.9452984673716,-9.06719534548324,129.299475646723));
#71477=CARTESIAN_POINT('Ctrl Pts',(77.9452505466265,-9.00149878663961,129.295925302725));
#71478=CARTESIAN_POINT('Ctrl Pts',(77.94704827473,-9.00149706514133,129.295925280538));
#71479=CARTESIAN_POINT('Ctrl Pts',(77.9500644504662,-8.54755626783022,129.271372265686));
#71480=CARTESIAN_POINT('Ctrl Pts',(78.3217621619307,-7.40396017493601,129.209774878171));
#71481=CARTESIAN_POINT('Ctrl Pts',(79.9094070337756,-6.71505827450504,129.127082065883));
#71482=CARTESIAN_POINT('Ctrl Pts',(80.9398133637899,-7.13722923514124,129.068942268446));
#71483=CARTESIAN_POINT('Ctrl Pts',(81.2492121870567,-7.37445590553645,129.047846843673));
#71484=CARTESIAN_POINT('',(77.9452508134305,-8.99817166960857,129.354074719499));
#71485=CARTESIAN_POINT('Ctrl Pts',(77.9452508134311,-8.99817166892661,129.354074719462));
#71486=CARTESIAN_POINT('Ctrl Pts',(77.9453406300956,-8.89723222694866,129.34859460346));
#71487=CARTESIAN_POINT('Ctrl Pts',(77.952871897115,-8.79661291965776,129.343114487457));
#71488=CARTESIAN_POINT('Ctrl Pts',(77.9676835787623,-8.69720051772217,129.337634371454));
#71489=CARTESIAN_POINT('Ctrl Pts',(77.9734619030679,-8.65841781147318,129.335496471906));
#71490=CARTESIAN_POINT('Ctrl Pts',(77.9803477788761,-8.61981845206601,129.333358572358));
#71491=CARTESIAN_POINT('Ctrl Pts',(77.988329837195,-8.58145404245158,129.331220672811));
#71492=CARTESIAN_POINT('Ctrl Pts',(78.0027616152757,-8.51209014862456,129.327355292404));
#71493=CARTESIAN_POINT('Ctrl Pts',(78.0208137903994,-8.44333610135341,129.323489911997));
#71494=CARTESIAN_POINT('Ctrl Pts',(78.042419743995,-8.3755986036216,129.31962453159));
#71495=CARTESIAN_POINT('Ctrl Pts',(78.0639934177053,-8.3079623075629,129.315764926167));
#71496=CARTESIAN_POINT('Ctrl Pts',(78.0891101847324,-8.24134000650113,129.311905320744));
#71497=CARTESIAN_POINT('Ctrl Pts',(78.1176525274556,-8.17612770704076,129.308045715321));
#71498=CARTESIAN_POINT('Ctrl Pts',(78.1461613766581,-8.11099193211538,129.30419063902));
#71499=CARTESIAN_POINT('Ctrl Pts',(78.17808762317,-8.04726331621047,129.30033556272));
#71500=CARTESIAN_POINT('Ctrl Pts',(78.2132646763425,-7.98532052070883,129.29648048642));
#71501=CARTESIAN_POINT('Ctrl Pts',(78.24841958107,-7.92341672610333,129.292627837382));
#71502=CARTESIAN_POINT('Ctrl Pts',(78.2868209921103,-7.8632969435781,129.288775188345));
#71503=CARTESIAN_POINT('Ctrl Pts',(78.3282558117856,-7.80531638846454,129.284922539307));
#71504=CARTESIAN_POINT('Ctrl Pts',(78.369678474441,-7.74735284490711,129.281071020641));
#71505=CARTESIAN_POINT('Ctrl Pts',(78.4141324960515,-7.69152767864704,129.277219501974));
#71506=CARTESIAN_POINT('Ctrl Pts',(78.4613617424586,-7.63816672278501,129.273367983308));
#71507=CARTESIAN_POINT('Ctrl Pts',(78.5085930111155,-7.58480348212737,129.269516299728));
#71508=CARTESIAN_POINT('Ctrl Pts',(78.5585994161696,-7.53390502441321,129.265664616149));
#71509=CARTESIAN_POINT('Ctrl Pts',(78.6110860295267,-7.4857623881556,129.261812932569));
#71510=CARTESIAN_POINT('Ctrl Pts',(78.6636282726897,-7.43756872621102,129.257957166645));
#71511=CARTESIAN_POINT('Ctrl Pts',(78.7186556121075,-7.39213704604406,129.254101400722));
#71512=CARTESIAN_POINT('Ctrl Pts',(78.7758385789269,-7.34971930337404,129.250245634798));
#71513=CARTESIAN_POINT('Ctrl Pts',(78.8330542625269,-7.30727729172922,129.246387662829));
#71514=CARTESIAN_POINT('Ctrl Pts',(78.8924276226871,-7.26785291933302,129.242529690859));
#71515=CARTESIAN_POINT('Ctrl Pts',(78.9536009498714,-7.23165427860104,129.23867171889));
#71516=CARTESIAN_POINT('Ctrl Pts',(79.0148825470524,-7.19539157029434,129.234806918738));
#71517=CARTESIAN_POINT('Ctrl Pts',(79.0779700401004,-7.16236621772688,129.230942118587));
#71518=CARTESIAN_POINT('Ctrl Pts',(79.1424825630927,-7.13273959826168,129.227077318435));
#71519=CARTESIAN_POINT('Ctrl Pts',(79.1813743788247,-7.11487898807997,129.22474739723));
#71520=CARTESIAN_POINT('Ctrl Pts',(79.2207837219093,-7.09825266193998,129.222417476024));
#71521=CARTESIAN_POINT('Ctrl Pts',(79.2606244867228,-7.08288721957572,129.220087554819));
#71522=CARTESIAN_POINT('Ctrl Pts',(79.3268985355705,-7.05732721633333,129.216211793083));
#71523=CARTESIAN_POINT('Ctrl Pts',(79.3946273063918,-7.03515857174183,129.212336031348));
#71524=CARTESIAN_POINT('Ctrl Pts',(79.4634308896462,-7.01654565156791,129.208460269612));
#71525=CARTESIAN_POINT('Ctrl Pts',(79.5321318648481,-6.99796048918509,129.204590287872));
#71526=CARTESIAN_POINT('Ctrl Pts',(79.6019040070276,-6.98292064977586,129.200720306131));
#71527=CARTESIAN_POINT('Ctrl Pts',(79.6723489208654,-6.97154188289679,129.196850324391));
#71528=CARTESIAN_POINT('Ctrl Pts',(79.742710349704,-6.96017660111254,129.192984929006));
#71529=CARTESIAN_POINT('Ctrl Pts',(79.8137424907851,-6.95246384924864,129.189119533621));
#71530=CARTESIAN_POINT('Ctrl Pts',(79.8850350203369,-6.94846871436211,129.185254138236));
#71531=CARTESIAN_POINT('Ctrl Pts',(79.9562820251037,-6.94447613062165,129.18139121115));
#71532=CARTESIAN_POINT('Ctrl Pts',(80.0277886063581,-6.94419648043532,129.177528284064));
#71533=CARTESIAN_POINT('Ctrl Pts',(80.0991389834618,-6.94764305627453,129.173665356978));
#71534=CARTESIAN_POINT('Ctrl Pts',(80.1704674478651,-6.95108857362201,129.169803616252));
#71535=CARTESIAN_POINT('Ctrl Pts',(80.2416393202463,-6.95825802149985,129.165941875525));
#71536=CARTESIAN_POINT('Ctrl Pts',(80.3122401944723,-6.96911260197522,129.162080134798));
#71537=CARTESIAN_POINT('Ctrl Pts',(80.3828427858252,-6.97996744645144,129.158218300147));
#71538=CARTESIAN_POINT('Ctrl Pts',(80.4528738734421,-6.99450752577777,129.154356465497));
#71539=CARTESIAN_POINT('Ctrl Pts',(80.5219272353851,-7.01264257782771,129.150494630846));
#71540=CARTESIAN_POINT('Ctrl Pts',(80.5910504180819,-7.03079596646503,129.146628891445));
#71541=CARTESIAN_POINT('Ctrl Pts',(80.6591934325206,-7.05255146114117,129.142763152043));
#71542=CARTESIAN_POINT('Ctrl Pts',(80.7259641399556,-7.07776858052977,129.138897412641));
#71543=CARTESIAN_POINT('Ctrl Pts',(80.792771476884,-7.10299953368385,129.135029552548));
#71544=CARTESIAN_POINT('Ctrl Pts',(80.858204564293,-7.13169569834081,129.131161692454));
#71545=CARTESIAN_POINT('Ctrl Pts',(80.9218927148622,-7.16366904268754,129.127293832361));
#71546=CARTESIAN_POINT('Ctrl Pts',(80.9856893236471,-7.1956968362819,129.123419385466));
#71547=CARTESIAN_POINT('Ctrl Pts',(81.0477346416405,-7.23101271315047,129.119544938571));
#71548=CARTESIAN_POINT('Ctrl Pts',(81.1076845945461,-7.2693838087244,129.115670491676));
#71549=CARTESIAN_POINT('Ctrl Pts',(81.1423241343156,-7.29155492023849,129.113431806726));
#71550=CARTESIAN_POINT('Ctrl Pts',(81.1762646743719,-7.31474525825012,129.111193121777));
#71551=CARTESIAN_POINT('Ctrl Pts',(81.2094449384984,-7.33890382480706,129.108954436827));
#71552=CARTESIAN_POINT('Ctrl Pts',(81.2237726733701,-7.34933585558259,129.107987739145));
#71553=CARTESIAN_POINT('Ctrl Pts',(81.2379725769056,-7.35995848134784,129.107021041463));
#71554=CARTESIAN_POINT('Ctrl Pts',(81.2520391107129,-7.37076839346109,129.106054343781));
#71555=CARTESIAN_POINT('Ctrl Pts',(81.2520391107129,-7.37076839346111,129.806138766351));
#71556=CARTESIAN_POINT('Ctrl Pts',(81.3085777008962,-7.41421741930245,129.80227718848));
#71557=CARTESIAN_POINT('Ctrl Pts',(81.3628020023102,-7.46057451897514,129.798415610609));
#71558=CARTESIAN_POINT('Ctrl Pts',(81.4144129914842,-7.50955260004903,129.794554032738));
#71559=CARTESIAN_POINT('Ctrl Pts',(81.4661146722451,-7.55861674612496,129.790685669245));
#71560=CARTESIAN_POINT('Ctrl Pts',(81.5151935371269,-7.61031071703995,129.786817305753));
#71561=CARTESIAN_POINT('Ctrl Pts',(81.5613890771163,-7.66431226989174,129.78294894226));
#71562=CARTESIAN_POINT('Ctrl Pts',(81.590032865033,-7.69779621720377,129.780550343099));
#71563=CARTESIAN_POINT('Ctrl Pts',(81.6175689183534,-7.73216671299117,129.778151743938));
#71564=CARTESIAN_POINT('Ctrl Pts',(81.6439435864093,-7.76734147177588,129.775753144777));
#71565=CARTESIAN_POINT('Ctrl Pts',(81.6864883346646,-7.82408157004983,129.771883985277));
#71566=CARTESIAN_POINT('Ctrl Pts',(81.7261753868327,-7.88313796797225,129.768014825776));
#71567=CARTESIAN_POINT('Ctrl Pts',(81.7627435659047,-7.94419098158735,129.764145666276));
#71568=CARTESIAN_POINT('Ctrl Pts',(81.7992572713571,-8.00515304786175,129.760282270452));
#71569=CARTESIAN_POINT('Ctrl Pts',(81.8326610783687,-8.06810541268281,129.756418874627));
#71570=CARTESIAN_POINT('Ctrl Pts',(81.8627355243751,-8.1326973257674,129.752555478803));
#71571=CARTESIAN_POINT('Ctrl Pts',(81.8927747030353,-8.1972134939701,129.748696613459));
#71572=CARTESIAN_POINT('Ctrl Pts',(81.9194920717898,-8.26336495317575,129.744837748116));
#71573=CARTESIAN_POINT('Ctrl Pts',(81.9427136505352,-8.33077564709266,129.740978882773));
#71574=CARTESIAN_POINT('Ctrl Pts',(81.9659206058334,-8.39814389011814,129.737122447493));
#71575=CARTESIAN_POINT('Ctrl Pts',(81.9856359808804,-8.46676933639469,129.733266012214));
#71576=CARTESIAN_POINT('Ctrl Pts',(82.0017341467539,-8.53625657069942,129.729409576934));
#71577=CARTESIAN_POINT('Ctrl Pts',(82.0178275595263,-8.60572328839044,129.725554280295));
#71578=CARTESIAN_POINT('Ctrl Pts',(82.030305773847,-8.67605081598735,129.721698983657));
#71579=CARTESIAN_POINT('Ctrl Pts',(82.0390936631195,-8.74683089539595,129.717843687018));
#71580=CARTESIAN_POINT('Ctrl Pts',(82.0478818969737,-8.81761375016064,129.713988239209));
#71581=CARTESIAN_POINT('Ctrl Pts',(82.0529794608286,-8.88884870963739,129.7101327914));
#71582=CARTESIAN_POINT('Ctrl Pts',(82.0543629818976,-8.9601214204246,129.706277343591));
#71583=CARTESIAN_POINT('Ctrl Pts',(82.0557479511442,-9.0314687347381,129.702417860156));
#71584=CARTESIAN_POINT('Ctrl Pts',(82.0534111076121,-9.10285339258064,129.698558376722));
#71585=CARTESIAN_POINT('Ctrl Pts',(82.04738123642,-9.17386096530035,129.694698893287));
#71586=CARTESIAN_POINT('Ctrl Pts',(82.0413479508545,-9.24490874557463,129.690837224446));
#71587=CARTESIAN_POINT('Ctrl Pts',(82.0316175410741,-9.31557853422141,129.686975555605));
#71588=CARTESIAN_POINT('Ctrl Pts',(82.0182703747424,-9.38546369081551,129.683113886764));
#71589=CARTESIAN_POINT('Ctrl Pts',(82.0048998596312,-9.45547110055874,129.679245462537));
#71590=CARTESIAN_POINT('Ctrl Pts',(81.987900071923,-9.52469066594064,129.675377038311));
#71591=CARTESIAN_POINT('Ctrl Pts',(81.9674017425439,-9.59272923492526,129.671508614084));
#71592=CARTESIAN_POINT('Ctrl Pts',(81.9552344686409,-9.63311515562621,129.669212418318));
#71593=CARTESIAN_POINT('Ctrl Pts',(81.9418354955515,-9.67308530827785,129.666916222551));
#71594=CARTESIAN_POINT('Ctrl Pts',(81.9272400721396,-9.7125610618322,129.664620026785));
#71595=CARTESIAN_POINT('Ctrl Pts',(81.9026497177558,-9.77906977090307,129.660751398515));
#71596=CARTESIAN_POINT('Ctrl Pts',(81.8745642853651,-9.84443451853481,129.656882770244));
#71597=CARTESIAN_POINT('Ctrl Pts',(81.8431105990524,-9.9082625623468,129.653014141974));
#71598=CARTESIAN_POINT('Ctrl Pts',(81.8117037902735,-9.97199547895319,129.649151279379));
#71599=CARTESIAN_POINT('Ctrl Pts',(81.7769389049626,-10.0341958054905,129.645288416785));
#71600=CARTESIAN_POINT('Ctrl Pts',(81.7389914953888,-10.0944889864523,129.64142555419));
#71601=CARTESIAN_POINT('Ctrl Pts',(81.7010885954797,-10.1547114477181,129.637567222464));
#71602=CARTESIAN_POINT('Ctrl Pts',(81.6600108435754,-10.213030797469,129.633708890737));
#71603=CARTESIAN_POINT('Ctrl Pts',(81.6159797248073,-10.2690969590664,129.629850559011));
#71604=CARTESIAN_POINT('Ctrl Pts',(81.5719763372501,-10.3251278096703,129.625994657298));
#71605=CARTESIAN_POINT('Ctrl Pts',(81.5250235725302,-10.3789079062814,129.622138755585));
#71606=CARTESIAN_POINT('Ctrl Pts',(81.4753854079039,-10.4301172891215,129.618282853872));
#71607=CARTESIAN_POINT('Ctrl Pts',(81.4257618905939,-10.4813115610074,129.614428089966));
#71608=CARTESIAN_POINT('Ctrl Pts',(81.3734548845351,-10.5299362763718,129.610573326059));
#71609=CARTESIAN_POINT('Ctrl Pts',(81.3187665507146,-10.575706935701,129.606718562153));
#71610=CARTESIAN_POINT('Ctrl Pts',(81.2640760492417,-10.6214794092176,129.602863645457));
#71611=CARTESIAN_POINT('Ctrl Pts',(81.2070044066542,-10.6643972919325,129.599008728761));
#71612=CARTESIAN_POINT('Ctrl Pts',(81.1478869763645,-10.7042162574019,129.595153812065));
#71613=CARTESIAN_POINT('Ctrl Pts',(81.0887075634526,-10.744076971707,129.59129485362));
#71614=CARTESIAN_POINT('Ctrl Pts',(81.0274784849117,-10.7808320108207,129.587435895174));
#71615=CARTESIAN_POINT('Ctrl Pts',(80.964563447489,-10.8142808267377,129.583576936729));
#71616=CARTESIAN_POINT('Ctrl Pts',(80.9016127366326,-10.8477486084563,129.579715790217));
#71617=CARTESIAN_POINT('Ctrl Pts',(80.8369746044577,-10.8779062296208,129.575854643705));
#71618=CARTESIAN_POINT('Ctrl Pts',(80.7710341896528,-10.9046007037924,129.571993497193));
#71619=CARTESIAN_POINT('Ctrl Pts',(80.7049782381157,-10.9313419503769,129.568125585417));
#71620=CARTESIAN_POINT('Ctrl Pts',(80.6376159077565,-10.9546077765723,129.564257673642));
#71621=CARTESIAN_POINT('Ctrl Pts',(80.5693483188029,-10.9742948245833,129.560389761867));
#71622=CARTESIAN_POINT('Ctrl Pts',(80.528737160153,-10.9860062947315,129.558088810843));
#71623=CARTESIAN_POINT('Ctrl Pts',(80.4878058768319,-10.9964522641733,129.555787859818));
#71624=CARTESIAN_POINT('Ctrl Pts',(80.446640193328,-11.0056196299907,129.553486908794));
#71625=CARTESIAN_POINT('Ctrl Pts',(80.3774071770919,-11.0210374326956,129.549617137516));
#71626=CARTESIAN_POINT('Ctrl Pts',(80.3072395029954,-11.0328963456036,129.545747366239));
#71627=CARTESIAN_POINT('Ctrl Pts',(80.2365361341041,-11.041089958763,129.541877594962));
#71628=CARTESIAN_POINT('Ctrl Pts',(80.1659381343249,-11.0492713609945,129.538013590798));
#71629=CARTESIAN_POINT('Ctrl Pts',(80.0948065029077,-11.0537982508364,129.534149586634));
#71630=CARTESIAN_POINT('Ctrl Pts',(80.0235513380866,-11.0546150240311,129.53028558247));
#71631=CARTESIAN_POINT('Ctrl Pts',(79.95237986535,-11.0554308378926,129.526426116736));
#71632=CARTESIAN_POINT('Ctrl Pts',(79.8810856306334,-11.0525451855223,129.522566651002));
#71633=CARTESIAN_POINT('Ctrl Pts',(79.8100830674483,-11.0459543301917,129.518707185268));
#71634=CARTESIAN_POINT('Ctrl Pts',(79.7391253061563,-11.0393676336235,129.514850154818));
#71635=CARTESIAN_POINT('Ctrl Pts',(79.6684593336303,-11.0290804173782,129.510993124368));
#71636=CARTESIAN_POINT('Ctrl Pts',(79.5984973212508,-11.0151409780601,129.507136093917));
#71637=CARTESIAN_POINT('Ctrl Pts',(79.5285560722597,-11.0012056757013,129.50328020816));
#71638=CARTESIAN_POINT('Ctrl Pts',(79.4593188446184,-10.9836203969911,129.499424322402));
#71639=CARTESIAN_POINT('Ctrl Pts',(79.3911887258673,-10.9624847502564,129.495568436644));
#71640=CARTESIAN_POINT('Ctrl Pts',(79.3230560578231,-10.941348312668,129.491712406607));
#71641=CARTESIAN_POINT('Ctrl Pts',(79.2560310440557,-10.9166613892836,129.48785637657));
#71642=CARTESIAN_POINT('Ctrl Pts',(79.1905010257898,-10.8885732639357,129.484000346533));
#71643=CARTESIAN_POINT('Ctrl Pts',(79.1249026706106,-10.8604558473432,129.480140295298));
#71644=CARTESIAN_POINT('Ctrl Pts',(79.0608028703654,-10.8289303400641,129.476280244063));
#71645=CARTESIAN_POINT('Ctrl Pts',(78.998567567296,-10.7941935919037,129.472420192828));
#71646=CARTESIAN_POINT('Ctrl Pts',(78.9362971464976,-10.7594372427188,129.468557963468));
#71647=CARTESIAN_POINT('Ctrl Pts',(78.8758937286265,-10.7214663039507,129.464695734108));
#71648=CARTESIAN_POINT('Ctrl Pts',(78.8176949311995,-10.6805214330049,129.460833504749));
#71649=CARTESIAN_POINT('Ctrl Pts',(78.7593946027653,-10.6395051314768,129.456964537517));
#71650=CARTESIAN_POINT('Ctrl Pts',(78.7033069558238,-10.595504839164,129.453095570286));
#71651=CARTESIAN_POINT('Ctrl Pts',(78.6497365892073,-10.5488015637823,129.449226603054));
#71652=CARTESIAN_POINT('Ctrl Pts',(78.6180158870127,-10.521147082705,129.446935665637));
#71653=CARTESIAN_POINT('Ctrl Pts',(78.5871771037121,-10.4925456023546,129.444644728219));
#71654=CARTESIAN_POINT('Ctrl Pts',(78.5572770056771,-10.4630611484664,129.442353790802));
#71655=CARTESIAN_POINT('Ctrl Pts',(78.5075191974749,-10.4139950283555,129.438541361007));
#71656=CARTESIAN_POINT('Ctrl Pts',(78.4601566106289,-10.3622781813274,129.434728931212));
#71657=CARTESIAN_POINT('Ctrl Pts',(78.4154907210218,-10.3081773225874,129.430916501417));
#71658=CARTESIAN_POINT('Ctrl Pts',(78.370884322811,-10.2541485218687,129.427109149474));
#71659=CARTESIAN_POINT('Ctrl Pts',(78.328967820547,-10.1977423834135,129.423301797531));
#71660=CARTESIAN_POINT('Ctrl Pts',(78.2900066717981,-10.1392630863875,129.419494445588));
#71661=CARTESIAN_POINT('Ctrl Pts',(78.2510834935506,-10.080840781732,129.415690804189));
#71662=CARTESIAN_POINT('Ctrl Pts',(78.2151102356859,-10.0203497381726,129.41188716279));
#71663=CARTESIAN_POINT('Ctrl Pts',(78.182311540293,-9.958126414388,129.408083521391));
#71664=CARTESIAN_POINT('Ctrl Pts',(78.1495330966884,-9.89594151083817,129.404282228577));
#71665=CARTESIAN_POINT('Ctrl Pts',(78.1199255604223,-9.83202689089695,129.400480935764));
#71666=CARTESIAN_POINT('Ctrl Pts',(78.093668727308,-9.76674548662288,129.39667964295));
#71667=CARTESIAN_POINT('Ctrl Pts',(78.0674079984643,-9.70145439653907,129.392877786139));
#71668=CARTESIAN_POINT('Ctrl Pts',(78.044499168057,-9.63479657590548,129.389075929327));
#71669=CARTESIAN_POINT('Ctrl Pts',(78.0250741537879,-9.56715559105353,129.385274072515));
#71670=CARTESIAN_POINT('Ctrl Pts',(78.0056484039667,-9.49951204489265,129.381472071741));
#71671=CARTESIAN_POINT('Ctrl Pts',(77.9897068601131,-9.4308857455588,129.377670070968));
#71672=CARTESIAN_POINT('Ctrl Pts',(77.9773310417072,-9.36167367565081,129.373868070194));
#71673=CARTESIAN_POINT('Ctrl Pts',(77.9649417578525,-9.29238629988788,129.370061932672));
#71674=CARTESIAN_POINT('Ctrl Pts',(77.9561260209403,-9.22251237727799,129.36625579515));
#71675=CARTESIAN_POINT('Ctrl Pts',(77.9509136980301,-9.15245618904848,129.362449657627));
#71676=CARTESIAN_POINT('Ctrl Pts',(77.9470906725768,-9.10107284320192,129.359658011585));
#71677=CARTESIAN_POINT('Ctrl Pts',(77.9452050596103,-9.04959160188904,129.356866365542));
#71678=CARTESIAN_POINT('Ctrl Pts',(77.9452508134305,-8.99817166960858,129.354074719499));
#71679=CARTESIAN_POINT('Origin',(80.,-9.,141.545925280538));
#71680=CARTESIAN_POINT('',(81.2520391107129,-7.37076839346111,130.506052881321));
#71681=CARTESIAN_POINT('',(81.2520391107129,-7.37076839346112,130.44794571257));
#71682=CARTESIAN_POINT('',(81.2520391107129,-7.37076839346111,141.545925280538));
#71683=CARTESIAN_POINT('',(77.9452500565798,-9.00048219782007,129.995925280508));
#71684=CARTESIAN_POINT('Ctrl Pts',(81.2520391107129,-7.37076839346111,130.44794571257));
#71685=CARTESIAN_POINT('Ctrl Pts',(81.2676313194312,-7.38275076297777,130.446873986343));
#71686=CARTESIAN_POINT('Ctrl Pts',(81.2830435643931,-7.39495088616389,130.445802260117));
#71687=CARTESIAN_POINT('Ctrl Pts',(81.2982695699414,-7.40736266329582,130.44473053389));
#71688=CARTESIAN_POINT('Ctrl Pts',(81.3532376875177,-7.45217100272229,130.440861444716));
#71689=CARTESIAN_POINT('Ctrl Pts',(81.4059909768369,-7.49991619016276,130.436992355542));
#71690=CARTESIAN_POINT('Ctrl Pts',(81.4561988949054,-7.55035095937804,130.433123266368));
#71691=CARTESIAN_POINT('Ctrl Pts',(81.5063320052026,-7.60071058282287,130.429259941981));
#71692=CARTESIAN_POINT('Ctrl Pts',(81.553926932326,-7.65375149205841,130.425396617594));
#71693=CARTESIAN_POINT('Ctrl Pts',(81.5986861257916,-7.70918621261568,130.421533293207));
#71694=CARTESIAN_POINT('Ctrl Pts',(81.6433928156937,-7.76455590697052,130.417674500588));
#71695=CARTESIAN_POINT('Ctrl Pts',(81.6852700755659,-7.8223134588909,130.413815707969));
#71696=CARTESIAN_POINT('Ctrl Pts',(81.7240583935174,-7.88213586771812,130.40995691535));
#71697=CARTESIAN_POINT('Ctrl Pts',(81.7628222770737,-7.94192059189048,130.406100553547));
#71698=CARTESIAN_POINT('Ctrl Pts',(81.7985008155955,-8.0037671856847,130.402244191744));
#71699=CARTESIAN_POINT('Ctrl Pts',(81.8308767539392,-8.06732220226645,130.398387829941));
#71700=CARTESIAN_POINT('Ctrl Pts',(81.8632431275178,-8.13085844290422,130.394532607416));
#71701=CARTESIAN_POINT('Ctrl Pts',(81.892308617534,-8.19610167170972,130.390677384892));
#71702=CARTESIAN_POINT('Ctrl Pts',(81.9179018845683,-8.2626738010423,130.386822162367));
#71703=CARTESIAN_POINT('Ctrl Pts',(81.9434961516872,-8.32924853175284,130.382966789195));
#71704=CARTESIAN_POINT('Ctrl Pts',(81.9656177541859,-8.39715181186872,130.379111416023));
#71705=CARTESIAN_POINT('Ctrl Pts',(81.9841441099778,-8.4659871599481,130.375256042851));
#71706=CARTESIAN_POINT('Ctrl Pts',(82.0026898570007,-8.53489455685084,130.371396634324));
#71707=CARTESIAN_POINT('Ctrl Pts',(82.0176327188452,-8.60473549914392,130.367537225796));
#71708=CARTESIAN_POINT('Ctrl Pts',(82.0289007144961,-8.67510085685347,130.363677817269));
#71709=CARTESIAN_POINT('Ctrl Pts',(82.0401750899228,-8.74550605440905,130.3598162236));
#71710=CARTESIAN_POINT('Ctrl Pts',(82.0477704054632,-8.81643577520147,130.355954629932));
#71711=CARTESIAN_POINT('Ctrl Pts',(82.0516666187413,-8.8874760112566,130.352093036263));
#71712=CARTESIAN_POINT('Ctrl Pts',(82.0555696483801,-8.95864053102955,130.348224686801));
#71713=CARTESIAN_POINT('Ctrl Pts',(82.0557606538846,-9.02991546614981,130.344356337338));
#71714=CARTESIAN_POINT('Ctrl Pts',(82.0522717225159,-9.10088775674808,130.340487987875));
#71715=CARTESIAN_POINT('Ctrl Pts',(82.0502001471195,-9.14302800987866,130.33819113055));
#71716=CARTESIAN_POINT('Ctrl Pts',(82.0468322168565,-9.1850616621623,130.335894273224));
#71717=CARTESIAN_POINT('Ctrl Pts',(82.0421831982172,-9.22690382856912,130.333597415899));
#71718=CARTESIAN_POINT('Ctrl Pts',(82.0343518468729,-9.29738767291675,130.329728320484));
#71719=CARTESIAN_POINT('Ctrl Pts',(82.0228518583727,-9.36760364829802,130.325859225068));
#71720=CARTESIAN_POINT('Ctrl Pts',(82.0077116910824,-9.43713994096954,130.321990129653));
#71721=CARTESIAN_POINT('Ctrl Pts',(81.9925940813417,-9.50657263053435,130.318126798858));
#71722=CARTESIAN_POINT('Ctrl Pts',(81.9738471609236,-9.57532717671738,130.314263468062));
#71723=CARTESIAN_POINT('Ctrl Pts',(81.951551062922,-9.64299767597408,130.310400137267));
#71724=CARTESIAN_POINT('Ctrl Pts',(81.9292811174798,-9.71058880005251,130.306541338027));
#71725=CARTESIAN_POINT('Ctrl Pts',(81.9034704149883,-9.77709794379142,130.302682538786));
#71726=CARTESIAN_POINT('Ctrl Pts',(81.8742495666074,-9.84213189262258,130.298823739545));
#71727=CARTESIAN_POINT('Ctrl Pts',(81.8450471246696,-9.90712487605568,130.294967370993));
#71728=CARTESIAN_POINT('Ctrl Pts',(81.8124389972207,-9.97064406611448,130.29111100244));
#71729=CARTESIAN_POINT('Ctrl Pts',(81.7766042934178,-10.032315236306,130.287254633888));
#71730=CARTESIAN_POINT('Ctrl Pts',(81.7407801750932,-10.0939681889942,130.283399404497));
#71731=CARTESIAN_POINT('Ctrl Pts',(81.7017316165523,-10.1537737857869,130.279544175106));
#71732=CARTESIAN_POINT('Ctrl Pts',(81.6596833322111,-10.2113830109757,130.275688945714));
#71733=CARTESIAN_POINT('Ctrl Pts',(81.6176334036367,-10.2689944888843,130.27183356557));
#71734=CARTESIAN_POINT('Ctrl Pts',(81.5725838045506,-10.3244090335942,130.267978185426));
#71735=CARTESIAN_POINT('Ctrl Pts',(81.5248011475405,-10.3773086157283,130.264122805282));
#71736=CARTESIAN_POINT('Ctrl Pts',(81.4769684759247,-10.4302635684068,130.260263389672));
#71737=CARTESIAN_POINT('Ctrl Pts',(81.4263973620334,-10.4806979423454,130.256403974061));
#71738=CARTESIAN_POINT('Ctrl Pts',(81.3733924898514,-10.5283293595688,130.252544558451));
#71739=CARTESIAN_POINT('Ctrl Pts',(81.3203576061274,-10.5759877458653,130.248682957626));
#71740=CARTESIAN_POINT('Ctrl Pts',(81.2648865988595,-10.6208397105533,130.244821356801));
#71741=CARTESIAN_POINT('Ctrl Pts',(81.2073164206213,-10.6626438653536,130.240959755975));
#71742=CARTESIAN_POINT('Ctrl Pts',(81.1496455239559,-10.7045211560874,130.23709139932));
#71743=CARTESIAN_POINT('Ctrl Pts',(81.0898685316552,-10.7433397265681,130.233223042664));
#71744=CARTESIAN_POINT('Ctrl Pts',(81.0283498737814,-10.7789024986192,130.229354686009));
#71745=CARTESIAN_POINT('Ctrl Pts',(80.991823818404,-10.8000175200812,130.227057889975));
#71746=CARTESIAN_POINT('Ctrl Pts',(80.9546842389192,-10.8199856735525,130.224761093941));
#71747=CARTESIAN_POINT('Ctrl Pts',(80.9170107237101,-10.8387737476647,130.222464297907));
#71748=CARTESIAN_POINT('Ctrl Pts',(80.8535484476817,-10.870422876734,130.218595269411));
#71749=CARTESIAN_POINT('Ctrl Pts',(80.7883214528133,-10.8988447018783,130.214726240915));
#71750=CARTESIAN_POINT('Ctrl Pts',(80.7216911380469,-10.9238397708137,130.210857212419));
#71751=CARTESIAN_POINT('Ctrl Pts',(80.6551601017931,-10.9487975973426,130.206993948738));
#71752=CARTESIAN_POINT('Ctrl Pts',(80.5872303472227,-10.9703386333542,130.203130685056));
#71753=CARTESIAN_POINT('Ctrl Pts',(80.5182863363069,-10.988310045264,130.199267421374));
#71754=CARTESIAN_POINT('Ctrl Pts',(80.4494231951227,-11.0062603771229,130.195408689212));
#71755=CARTESIAN_POINT('Ctrl Pts',(80.3795486285444,-11.0206492799013,130.191549957049));
#71756=CARTESIAN_POINT('Ctrl Pts',(80.3090638173179,-11.0313732102509,130.187691224887));
#71757=CARTESIAN_POINT('Ctrl Pts',(80.2386234047366,-11.0420903855567,130.183834923354));
#71758=CARTESIAN_POINT('Ctrl Pts',(80.1675739892765,-11.0491470957167,130.179978621821));
#71759=CARTESIAN_POINT('Ctrl Pts',(80.0963271041859,-11.0524908407833,130.176122320288));
#71760=CARTESIAN_POINT('Ctrl Pts',(80.0251012627136,-11.0558335982348,130.17226715776));
#71761=CARTESIAN_POINT('Ctrl Pts',(79.9536785524018,-11.0554655450204,130.168411995232));
#71762=CARTESIAN_POINT('Ctrl Pts',(79.882474061892,-11.0513861694893,130.164556832704));
#71763=CARTESIAN_POINT('Ctrl Pts',(79.8112667822854,-11.047306634168,130.160701519168));
#71764=CARTESIAN_POINT('Ctrl Pts',(79.740278224328,-11.0395155178963,130.156846205632));
#71765=CARTESIAN_POINT('Ctrl Pts',(79.6699201689214,-11.0280643154533,130.152990892097));
#71766=CARTESIAN_POINT('Ctrl Pts',(79.5994884522895,-11.0166011241969,130.149131542248));
#71767=CARTESIAN_POINT('Ctrl Pts',(79.5296890363937,-11.0014702756004,130.145272192399));
#71768=CARTESIAN_POINT('Ctrl Pts',(79.4609243994404,-10.9827745861245,130.141412842551));
#71769=CARTESIAN_POINT('Ctrl Pts',(79.392120820313,-10.964068309073,130.13755130711));
#71770=CARTESIAN_POINT('Ctrl Pts',(79.3243536484091,-10.9417933240919,130.133689771669));
#71771=CARTESIAN_POINT('Ctrl Pts',(79.2580084266242,-10.9161017894515,130.129828236228));
#71772=CARTESIAN_POINT('Ctrl Pts',(79.1915471101499,-10.8903652982844,130.12595994365));
#71773=CARTESIAN_POINT('Ctrl Pts',(79.12651315498,-10.8612005201156,130.122091651072));
#71774=CARTESIAN_POINT('Ctrl Pts',(79.0632697805276,-10.8288067307475,130.118223358494));
#71775=CARTESIAN_POINT('Ctrl Pts',(79.0257093132346,-10.809567942865,130.115925965634));
#71776=CARTESIAN_POINT('Ctrl Pts',(78.9887799256528,-10.7891910807889,130.113628572775));
#71777=CARTESIAN_POINT('Ctrl Pts',(78.9525527426241,-10.7677250367395,130.111331179916));
#71778=CARTESIAN_POINT('Ctrl Pts',(78.8915407846791,-10.7315730296748,130.107462029052));
#71779=CARTESIAN_POINT('Ctrl Pts',(78.8322831872935,-10.6921878298015,130.103592878188));
#71780=CARTESIAN_POINT('Ctrl Pts',(78.7751435457919,-10.6497649011555,130.099723727324));
#71781=CARTESIAN_POINT('Ctrl Pts',(78.7180890430305,-10.6074051831739,130.095860341541));
#71782=CARTESIAN_POINT('Ctrl Pts',(78.6631466188576,-10.5620170081236,130.091996955758));
#71783=CARTESIAN_POINT('Ctrl Pts',(78.6106532103293,-10.5138405003605,130.088133569974));
#71784=CARTESIAN_POINT('Ctrl Pts',(78.5582213866318,-10.4657205128761,130.084274716683));
#71785=CARTESIAN_POINT('Ctrl Pts',(78.5082332276439,-10.4148190173584,130.080415863392));
#71786=CARTESIAN_POINT('Ctrl Pts',(78.4609933270415,-10.3614169174391,130.0765570101));
#71787=CARTESIAN_POINT('Ctrl Pts',(78.4137831902294,-10.3080484638416,130.072700588103));
#71788=CARTESIAN_POINT('Ctrl Pts',(78.369318197509,-10.2521828946335,130.068844166106));
#71789=CARTESIAN_POINT('Ctrl Pts',(78.327865673879,-10.1941374953949,130.064987744109));
#71790=CARTESIAN_POINT('Ctrl Pts',(78.2864254023504,-10.1361092526054,130.061132461953));
#71791=CARTESIAN_POINT('Ctrl Pts',(78.2479961143842,-10.0759028539788,130.057277179797));
#71792=CARTESIAN_POINT('Ctrl Pts',(78.2128033861742,-10.0138667693684,130.05342189764));
#71793=CARTESIAN_POINT('Ctrl Pts',(78.177609288703,-9.95182827108889,130.049566465484));
#71794=CARTESIAN_POINT('Ctrl Pts',(78.1456522387718,-9.88796036908939,130.045711033329));
#71795=CARTESIAN_POINT('Ctrl Pts',(78.117112326338,-9.82263696177101,130.041855601173));
#71796=CARTESIAN_POINT('Ctrl Pts',(78.0885425523607,-9.7572452060379,130.037996135047));
#71797=CARTESIAN_POINT('Ctrl Pts',(78.0633972480212,-9.69039535096697,130.034136668921));
#71798=CARTESIAN_POINT('Ctrl Pts',(78.0418083407976,-9.62248131564733,130.030277202795));
#71799=CARTESIAN_POINT('Ctrl Pts',(78.0202072143132,-9.55452884117498,130.026415552222));
#71800=CARTESIAN_POINT('Ctrl Pts',(78.0021666149461,-9.48551145760912,130.02255390165));
#71801=CARTESIAN_POINT('Ctrl Pts',(77.9877678314391,-9.41583561933637,130.018692251077));
#71802=CARTESIAN_POINT('Ctrl Pts',(77.9733438642384,-9.34603791695104,130.014823846418));
#71803=CARTESIAN_POINT('Ctrl Pts',(77.9625745033955,-9.27557994090165,130.010955441758));
#71804=CARTESIAN_POINT('Ctrl Pts',(77.9554893450192,-9.20487494763926,130.007087037099));
#71805=CARTESIAN_POINT('Ctrl Pts',(77.9512835216487,-9.16290373157261,130.004790712041));
#71806=CARTESIAN_POINT('Ctrl Pts',(77.948374915081,-9.12084552646747,130.002494386983));
#71807=CARTESIAN_POINT('Ctrl Pts',(77.9467610336941,-9.07878648198151,130.000198061924));
#71808=CARTESIAN_POINT('Ctrl Pts',(77.9457600484714,-9.05270000353759,129.998773801462));
#71809=CARTESIAN_POINT('Ctrl Pts',(77.9452561844424,-9.02659432475927,129.997349541));
#71810=CARTESIAN_POINT('Ctrl Pts',(77.9452500565799,-9.00048219837867,129.995925280538));
#71811=CARTESIAN_POINT('Ctrl Pts',(77.9452500565798,-9.00048219782009,129.995925280508));
#71812=CARTESIAN_POINT('Ctrl Pts',(77.9452335129531,-8.92998620069327,129.99208014511));
#71813=CARTESIAN_POINT('Ctrl Pts',(77.94884919308,-8.85934488793869,129.988235009713));
#71814=CARTESIAN_POINT('Ctrl Pts',(77.9561158551286,-8.78896643668981,129.984389874316));
#71815=CARTESIAN_POINT('Ctrl Pts',(77.9636220283225,-8.71626829266497,129.980418002216));
#71816=CARTESIAN_POINT('Ctrl Pts',(77.9750241783424,-8.64385116603616,129.976446130117));
#71817=CARTESIAN_POINT('Ctrl Pts',(77.9902844923641,-8.57216692406059,129.972474258018));
#71818=CARTESIAN_POINT('Ctrl Pts',(78.005019200792,-8.50295167705567,129.968639187703));
#71819=CARTESIAN_POINT('Ctrl Pts',(78.0233505262677,-8.43442018110653,129.964804117388));
#71820=CARTESIAN_POINT('Ctrl Pts',(78.0451918525315,-8.36697340570031,129.960969047074));
#71821=CARTESIAN_POINT('Ctrl Pts',(78.0670205792052,-8.29956553826654,129.957136189093));
#71822=CARTESIAN_POINT('Ctrl Pts',(78.0923551392775,-8.23324161778643,129.953303331113));
#71823=CARTESIAN_POINT('Ctrl Pts',(78.121058669008,-8.1683888906526,129.949470473133));
#71824=CARTESIAN_POINT('Ctrl Pts',(78.1497555440784,-8.10355119905121,129.945638503767));
#71825=CARTESIAN_POINT('Ctrl Pts',(78.1818196388573,-8.040184473733,129.941806534401));
#71826=CARTESIAN_POINT('Ctrl Pts',(78.2170660967416,-7.97865566085095,129.937974565034));
#71827=CARTESIAN_POINT('Ctrl Pts',(78.2523165439689,-7.91711988387786,129.93414216195));
#71828=CARTESIAN_POINT('Ctrl Pts',(78.2907498217624,-7.85742285789769,129.930309758865));
#71829=CARTESIAN_POINT('Ctrl Pts',(78.332136214679,-7.7999050220442,129.926477355781));
#71830=CARTESIAN_POINT('Ctrl Pts',(78.3735674182597,-7.74232490938332,129.922640803204));
#71831=CARTESIAN_POINT('Ctrl Pts',(78.4179578264847,-7.68692909327009,129.918804250627));
#71832=CARTESIAN_POINT('Ctrl Pts',(78.4650362993757,-7.63402635447611,129.91496769805));
#71833=CARTESIAN_POINT('Ctrl Pts',(78.5121454593173,-7.58108913221403,129.911128644702));
#71834=CARTESIAN_POINT('Ctrl Pts',(78.5619458225972,-7.53064856875079,129.907289591353));
#71835=CARTESIAN_POINT('Ctrl Pts',(78.6141300949471,-7.48297588391985,129.903450538005));
#71836=CARTESIAN_POINT('Ctrl Pts',(78.6664000147489,-7.4352249562814,129.89960518381));
#71837=CARTESIAN_POINT('Ctrl Pts',(78.7210612665847,-7.39025127784402,129.895759829614));
#71838=CARTESIAN_POINT('Ctrl Pts',(78.7777751369244,-7.34828454430555,129.891914475419));
#71839=CARTESIAN_POINT('Ctrl Pts',(78.7917840726457,-7.33791830992497,129.89096463159));
#71840=CARTESIAN_POINT('Ctrl Pts',(78.8059181218404,-7.32773532710005,129.890014787761));
#71841=CARTESIAN_POINT('Ctrl Pts',(78.8201719453355,-7.3177386279396,129.889064943932));
#71842=CARTESIAN_POINT('Ctrl Pts',(78.8782264908607,-7.27702296826328,129.885196315152));
#71843=CARTESIAN_POINT('Ctrl Pts',(78.9385050111917,-7.2392361583561,129.881327686372));
#71844=CARTESIAN_POINT('Ctrl Pts',(79.0006798082348,-7.20462908655889,129.877459057592));
#71845=CARTESIAN_POINT('Ctrl Pts',(79.0627619420393,-7.17007359198433,129.873596194486));
#71846=CARTESIAN_POINT('Ctrl Pts',(79.1267343216675,-7.13868866324636,129.869733331381));
#71847=CARTESIAN_POINT('Ctrl Pts',(79.192239515353,-7.11068251425472,129.865870468276));
#71848=CARTESIAN_POINT('Ctrl Pts',(79.257667876001,-7.08270921452855,129.86201213604));
#71849=CARTESIAN_POINT('Ctrl Pts',(79.3246250349128,-7.05810701269977,129.858153803805));
#71850=CARTESIAN_POINT('Ctrl Pts',(79.3927297045678,-7.03703786312989,129.854295471569));
#71851=CARTESIAN_POINT('Ctrl Pts',(79.4607914812494,-7.01598198311225,129.850439569349));
#71852=CARTESIAN_POINT('Ctrl Pts',(79.5299988717297,-6.99845488399779,129.846583667128));
#71853=CARTESIAN_POINT('Ctrl Pts',(79.5999527695071,-6.98456958049281,129.842727764907));
#71854=CARTESIAN_POINT('Ctrl Pts',(79.6698860251347,-6.97068837429367,129.838873000494));
#71855=CARTESIAN_POINT('Ctrl Pts',(79.7405648743919,-6.96044692483719,129.835018236082));
#71856=CARTESIAN_POINT('Ctrl Pts',(79.8115789746446,-6.95390736287332,129.831163471669));
#71857=CARTESIAN_POINT('Ctrl Pts',(79.8825958895971,-6.94736754170876,129.827308554469));
#71858=CARTESIAN_POINT('Ctrl Pts',(79.9539475978615,-6.94452994170624,129.82345363727));
#71859=CARTESIAN_POINT('Ctrl Pts',(80.0252193065267,-6.94540477244828,129.819598720071));
#71860=CARTESIAN_POINT('Ctrl Pts',(80.0965657410168,-6.94628052041891,129.815739761129));
#71861=CARTESIAN_POINT('Ctrl Pts',(80.1678315216015,-6.95087646314228,129.811880802188));
#71862=CARTESIAN_POINT('Ctrl Pts',(80.2386034358576,-6.9591506760917,129.808021843246));
#71863=CARTESIAN_POINT('Ctrl Pts',(80.3094154784047,-6.96742958059185,129.804160696241));
#71864=CARTESIAN_POINT('Ctrl Pts',(80.3797326179328,-6.97939082554255,129.800299549237));
#71865=CARTESIAN_POINT('Ctrl Pts',(80.4491510670373,-6.99494117755133,129.796438402232));
#71866=CARTESIAN_POINT('Ctrl Pts',(80.5186911466634,-7.01051877588222,129.792570489975));
#71867=CARTESIAN_POINT('Ctrl Pts',(80.5873289239613,-7.02969790579128,129.788702577718));
#71868=CARTESIAN_POINT('Ctrl Pts',(80.6546756951435,-7.05233542500554,129.784834665461));
#71869=CARTESIAN_POINT('Ctrl Pts',(80.6947389922348,-7.06580204919211,129.782533718954));
#71870=CARTESIAN_POINT('Ctrl Pts',(80.7343457867761,-7.08049160587811,129.780232772447));
#71871=CARTESIAN_POINT('Ctrl Pts',(80.7734181194189,-7.09636611317867,129.777931825941));
#71872=CARTESIAN_POINT('Ctrl Pts',(80.8391271617478,-7.12306271923229,129.774062259392));
#71873=CARTESIAN_POINT('Ctrl Pts',(80.9035808241524,-7.15321771156363,129.770192692842));
#71874=CARTESIAN_POINT('Ctrl Pts',(80.9663905023612,-7.18669170865896,129.766323126293));
#71875=CARTESIAN_POINT('Ctrl Pts',(81.0291002102201,-7.22011242722627,129.762459718698));
#71876=CARTESIAN_POINT('Ctrl Pts',(81.0901707053912,-7.25684143326172,129.758596311103));
#71877=CARTESIAN_POINT('Ctrl Pts',(81.1492332295155,-7.29669129436928,129.754732903508));
#71878=CARTESIAN_POINT('Ctrl Pts',(81.1842307637733,-7.32030435358001,129.752443639009));
#71879=CARTESIAN_POINT('Ctrl Pts',(81.2185236431271,-7.34501227869952,129.750154374511));
#71880=CARTESIAN_POINT('Ctrl Pts',(81.2520391107129,-7.37076839346113,129.747865110012));
#71881=CARTESIAN_POINT('',(77.9452500005989,-9.00004961080126,130.054074719503));
#71882=CARTESIAN_POINT('Ctrl Pts',(77.9452500005989,-9.0000496100482,130.054074719462));
#71883=CARTESIAN_POINT('Ctrl Pts',(77.9452481959175,-8.92530327730347,130.05004413849));
#71884=CARTESIAN_POINT('Ctrl Pts',(77.9493293030799,-8.85063229326303,130.046013557518));
#71885=CARTESIAN_POINT('Ctrl Pts',(77.9574429753664,-8.77648632341645,130.041982976546));
#71886=CARTESIAN_POINT('Ctrl Pts',(77.9655784946025,-8.70214070744002,130.037941542793));
#71887=CARTESIAN_POINT('Ctrl Pts',(77.977768229183,-8.62832334710428,130.033900109041));
#71888=CARTESIAN_POINT('Ctrl Pts',(77.9939102844703,-8.55547596718978,130.029858675289));
#71889=CARTESIAN_POINT('Ctrl Pts',(78.0100750999784,-8.48252587281739,130.025811543135));
#71890=CARTESIAN_POINT('Ctrl Pts',(78.0302032326271,-8.41054888741118,130.021764410981));
#71891=CARTESIAN_POINT('Ctrl Pts',(78.0541430544742,-8.33997097787378,130.017717278826));
#71892=CARTESIAN_POINT('Ctrl Pts',(78.0781473948008,-8.26920285892522,130.013659239539));
#71893=CARTESIAN_POINT('Ctrl Pts',(78.1059838015981,-8.19984174114008,130.009601200252));
#71894=CARTESIAN_POINT('Ctrl Pts',(78.1374525227725,-8.13229356486568,130.005543160965));
#71895=CARTESIAN_POINT('Ctrl Pts',(78.1569006457639,-8.0905478188995,130.00303523423));
#71896=CARTESIAN_POINT('Ctrl Pts',(78.1777351877113,-8.04949402479317,130.000527307495));
#71897=CARTESIAN_POINT('Ctrl Pts',(78.1999006272447,-8.00922262303484,129.99801938076));
#71898=CARTESIAN_POINT('Ctrl Pts',(78.234095691327,-7.94709513119158,129.994150352343));
#71899=CARTESIAN_POINT('Ctrl Pts',(78.2715778605616,-7.88661829432888,129.990281323926));
#71900=CARTESIAN_POINT('Ctrl Pts',(78.312163336166,-7.82816171818907,129.986412295509));
#71901=CARTESIAN_POINT('Ctrl Pts',(78.3526883398097,-7.76979224177453,129.982549031907));
#71902=CARTESIAN_POINT('Ctrl Pts',(78.3963071967288,-7.71343744678505,129.978685768304));
#71903=CARTESIAN_POINT('Ctrl Pts',(78.4427906230037,-7.65944171380172,129.974822504702));
#71904=CARTESIAN_POINT('Ctrl Pts',(78.4892195252959,-7.60550931656296,129.970963772618));
#71905=CARTESIAN_POINT('Ctrl Pts',(78.5385060073011,-7.55393085126767,129.967105040534));
#71906=CARTESIAN_POINT('Ctrl Pts',(78.5903789984731,-7.50501966750249,129.963246308451));
#71907=CARTESIAN_POINT('Ctrl Pts',(78.6422193146569,-7.45613929307212,129.959390006997));
#71908=CARTESIAN_POINT('Ctrl Pts',(78.6966425549832,-7.40992319930734,129.955533705543));
#71909=CARTESIAN_POINT('Ctrl Pts',(78.7533401012571,-7.36664864179006,129.951677404088));
#71910=CARTESIAN_POINT('Ctrl Pts',(78.8100209012381,-7.32338686592666,129.947822241639));
#71911=CARTESIAN_POINT('Ctrl Pts',(78.8689742876135,-7.28306519605176,129.943967079189));
#71912=CARTESIAN_POINT('Ctrl Pts',(78.929859147609,-7.24592015046527,129.940111916739));
#71913=CARTESIAN_POINT('Ctrl Pts',(78.990746392486,-7.20877364989418,129.936256603281));
#71914=CARTESIAN_POINT('Ctrl Pts',(79.0535648453302,-7.17480427177923,129.932401289823));
#71915=CARTESIAN_POINT('Ctrl Pts',(79.117946533292,-7.1442038785555,129.928545976366));
#71916=CARTESIAN_POINT('Ctrl Pts',(79.1823956255543,-7.11357144830132,129.924686626594));
#71917=CARTESIAN_POINT('Ctrl Pts',(79.2484107803471,-7.08631525289264,129.920827276822));
#71918=CARTESIAN_POINT('Ctrl Pts',(79.3156024849781,-7.06257965223553,129.91696792705));
#71919=CARTESIAN_POINT('Ctrl Pts',(79.3828322410247,-7.03883060984165,129.913106391685));
#71920=CARTESIAN_POINT('Ctrl Pts',(79.4512394072066,-7.01860626893441,129.90924485632));
#71921=CARTESIAN_POINT('Ctrl Pts',(79.5204203348216,-7.00200077396226,129.905383320956));
#71922=CARTESIAN_POINT('Ctrl Pts',(79.5897223192403,-6.98536622173092,129.901515028452));
#71923=CARTESIAN_POINT('Ctrl Pts',(79.6598002905396,-6.9723632470331,129.897646735948));
#71924=CARTESIAN_POINT('Ctrl Pts',(79.7302421608351,-6.96303454356508,129.893778443445));
#71925=CARTESIAN_POINT('Ctrl Pts',(79.7720778542155,-6.9574941912677,129.891481049886));
#71926=CARTESIAN_POINT('Ctrl Pts',(79.8140418177163,-6.95324883831699,129.889183656327));
#71927=CARTESIAN_POINT('Ctrl Pts',(79.856047742892,-6.95029872660099,129.886886262768));
#71928=CARTESIAN_POINT('Ctrl Pts',(79.9267744990955,-6.94533152658724,129.883018065759));
#71929=CARTESIAN_POINT('Ctrl Pts',(79.9978971276319,-6.94401963059411,129.87914986875));
#71930=CARTESIAN_POINT('Ctrl Pts',(80.0690057038552,-6.94640905355145,129.87528167174));
#71931=CARTESIAN_POINT('Ctrl Pts',(80.1400164928976,-6.94879519061914,129.871418794203));
#71932=CARTESIAN_POINT('Ctrl Pts',(80.2110127869314,-6.95487253311624,129.867555916666));
#71933=CARTESIAN_POINT('Ctrl Pts',(80.2815810444504,-6.96463524696279,129.863693039128));
#71934=CARTESIAN_POINT('Ctrl Pts',(80.3520758709569,-6.97438780204975,129.859834181175));
#71935=CARTESIAN_POINT('Ctrl Pts',(80.4221430662193,-6.98781805163217,129.855975323221));
#71936=CARTESIAN_POINT('Ctrl Pts',(80.4913723285457,-7.00486822559522,129.852116465267));
#71937=CARTESIAN_POINT('Ctrl Pts',(80.5605648400204,-7.02190934835083,129.848259655816));
#71938=CARTESIAN_POINT('Ctrl Pts',(80.6289198289698,-7.04256647320145,129.844402846365));
#71939=CARTESIAN_POINT('Ctrl Pts',(80.6960368317509,-7.06673067283781,129.840546036914));
#71940=CARTESIAN_POINT('Ctrl Pts',(80.7631293991516,-7.09088607498043,129.836690631616));
#71941=CARTESIAN_POINT('Ctrl Pts',(80.828984419639,-7.11854584861426,129.832835226319));
#71942=CARTESIAN_POINT('Ctrl Pts',(80.8932181129685,-7.14955168535705,129.828979821022));
#71943=CARTESIAN_POINT('Ctrl Pts',(80.9574849838627,-7.18057353703062,129.825122424356));
#71944=CARTESIAN_POINT('Ctrl Pts',(81.0201284140811,-7.21494469754726,129.82126502769));
#71945=CARTESIAN_POINT('Ctrl Pts',(81.0807870621434,-7.25245976046229,129.817407631025));
#71946=CARTESIAN_POINT('Ctrl Pts',(81.1398557515114,-7.2889914944976,129.8136513428));
#71947=CARTESIAN_POINT('Ctrl Pts',(81.1970420997478,-7.32850404723543,129.809895054576));
#71948=CARTESIAN_POINT('Ctrl Pts',(81.2520391107129,-7.37076839346111,129.806138766351));
#71949=CARTESIAN_POINT('Ctrl Pts',(81.2520391107129,-7.37076839346111,130.506052881321));
#71950=CARTESIAN_POINT('Ctrl Pts',(81.3085807246794,-7.41421974303275,130.50219771141));
#71951=CARTESIAN_POINT('Ctrl Pts',(81.362873206473,-7.46062977900589,130.498342541498));
#71952=CARTESIAN_POINT('Ctrl Pts',(81.4145999487785,-7.5097300421011,130.494487371586));
#71953=CARTESIAN_POINT('Ctrl Pts',(81.4663306422551,-7.55883405574272,130.490631907195));
#71954=CARTESIAN_POINT('Ctrl Pts',(81.5154948564782,-7.6106283683093,130.486776442805));
#71955=CARTESIAN_POINT('Ctrl Pts',(81.561812211972,-7.66480706374127,130.482920978414));
#71956=CARTESIAN_POINT('Ctrl Pts',(81.6081791212523,-7.71904372361176,130.479061389158));
#71957=CARTESIAN_POINT('Ctrl Pts',(81.651692776919,-7.77566948756278,130.475201799901));
#71958=CARTESIAN_POINT('Ctrl Pts',(81.6921131557005,-7.83434540673269,130.471342210645));
#71959=CARTESIAN_POINT('Ctrl Pts',(81.7325577723832,-7.89305651065771,130.467480307003));
#71960=CARTESIAN_POINT('Ctrl Pts',(81.7699051661614,-7.95381980266632,130.463618403362));
#71961=CARTESIAN_POINT('Ctrl Pts',(81.8039601860705,-8.01626974755644,130.45975649972));
#71962=CARTESIAN_POINT('Ctrl Pts',(81.8380736285783,-8.0788268275497,130.455887970845));
#71963=CARTESIAN_POINT('Ctrl Pts',(81.8688832138848,-8.14307589792443,130.45201944197));
#71964=CARTESIAN_POINT('Ctrl Pts',(81.8962413478652,-8.20863010346207,130.448150913095));
#71965=CARTESIAN_POINT('Ctrl Pts',(81.9094401501915,-8.24025641983182,130.446284559639));
#71966=CARTESIAN_POINT('Ctrl Pts',(81.9218363544097,-8.27218626462339,130.444418206182));
#71967=CARTESIAN_POINT('Ctrl Pts',(81.9334175758367,-8.30437507236593,130.442551852726));
#71968=CARTESIAN_POINT('Ctrl Pts',(81.9574262793432,-8.37110478185256,130.438682768014));
#71969=CARTESIAN_POINT('Ctrl Pts',(81.9780233007512,-8.43920959718742,130.434813683301));
#71970=CARTESIAN_POINT('Ctrl Pts',(81.9950528338328,-8.50830725781688,130.430944598589));
#71971=CARTESIAN_POINT('Ctrl Pts',(82.0120569938305,-8.57730196666607,130.427081278604));
#71972=CARTESIAN_POINT('Ctrl Pts',(82.0255041010556,-8.64728611664166,130.423217958619));
#71973=CARTESIAN_POINT('Ctrl Pts',(82.0352873460395,-8.71785999654176,130.419354638634));
#71974=CARTESIAN_POINT('Ctrl Pts',(82.0450591153133,-8.78835109354143,130.415495850309));
#71975=CARTESIAN_POINT('Ctrl Pts',(82.0511754926477,-8.85943006756781,130.411637061983));
#71976=CARTESIAN_POINT('Ctrl Pts',(82.053580576256,-8.93068636985202,130.407778273658));
#71977=CARTESIAN_POINT('Ctrl Pts',(82.0559841448421,-9.00189778601412,130.40392191608));
#71978=CARTESIAN_POINT('Ctrl Pts',(82.0546810415849,-9.07328582445763,130.400065558502));
#71979=CARTESIAN_POINT('Ctrl Pts',(82.0496672686969,-9.14443562625877,130.396209200924));
#71980=CARTESIAN_POINT('Ctrl Pts',(82.0446549769234,-9.21556440975503,130.39235398255));
#71981=CARTESIAN_POINT('Ctrl Pts',(82.0359342258414,-9.28645461201044,130.388498764175));
#71982=CARTESIAN_POINT('Ctrl Pts',(82.0235530649265,-9.3566939247121,130.3846435458));
#71983=CARTESIAN_POINT('Ctrl Pts',(82.0111714199462,-9.42693598355592,130.380788176699));
#71984=CARTESIAN_POINT('Ctrl Pts',(81.9951291675039,-9.49652662429819,130.376932807597));
#71985=CARTESIAN_POINT('Ctrl Pts',(81.9755256195375,-9.56506290716236,130.373077438495));
#71986=CARTESIAN_POINT('Ctrl Pts',(81.9559015520805,-9.63367092855154,130.369218033888));
#71987=CARTESIAN_POINT('Ctrl Pts',(81.9327088816582,-9.70122192097859,130.365358629282));
#71988=CARTESIAN_POINT('Ctrl Pts',(81.9060968013722,-9.7673281868266,130.361499224675));
#71989=CARTESIAN_POINT('Ctrl Pts',(81.8794696531574,-9.83347188246193,130.357637634849));
#71990=CARTESIAN_POINT('Ctrl Pts',(81.8494194456522,-9.89816878232024,130.353776045023));
#71991=CARTESIAN_POINT('Ctrl Pts',(81.8161423941771,-9.96105377923019,130.349914455197));
#71992=CARTESIAN_POINT('Ctrl Pts',(81.7828071235772,-10.0240487951869,130.346046109413));
#71993=CARTESIAN_POINT('Ctrl Pts',(81.7462339870473,-10.0852251621662,130.342177763628));
#71994=CARTESIAN_POINT('Ctrl Pts',(81.7066633828725,-10.1442454544643,130.338309417844));
#71995=CARTESIAN_POINT('Ctrl Pts',(81.683167681349,-10.1792897304005,130.336012523474));
#71996=CARTESIAN_POINT('Ctrl Pts',(81.6586159996239,-10.2135744578996,130.333715629104));
#71997=CARTESIAN_POINT('Ctrl Pts',(81.6330651749265,-10.2470347617216,130.331418734734));
#71998=CARTESIAN_POINT('Ctrl Pts',(81.5900252789422,-10.3033980303506,130.327549658259));
#71999=CARTESIAN_POINT('Ctrl Pts',(81.5439796921779,-10.3576408743815,130.323680581783));
#72000=CARTESIAN_POINT('Ctrl Pts',(81.4951650564802,-10.4094250658977,130.319811505308));
#72001=CARTESIAN_POINT('Ctrl Pts',(81.4464231523288,-10.4611321013668,130.315948193577));
#72002=CARTESIAN_POINT('Ctrl Pts',(81.3949207192542,-10.5103874052188,130.312084881846));
#72003=CARTESIAN_POINT('Ctrl Pts',(81.3409356349291,-10.5568844483382,130.308221570115));
#72004=CARTESIAN_POINT('Ctrl Pts',(81.2870138748539,-10.6033269506447,130.304362790031));
#72005=CARTESIAN_POINT('Ctrl Pts',(81.2306156143129,-10.647017303385,130.300504009947));
#72006=CARTESIAN_POINT('Ctrl Pts',(81.1720554473805,-10.6876858685092,130.296645229862));
#72007=CARTESIAN_POINT('Ctrl Pts',(81.113532168842,-10.7283288155703,130.292788880512));
#72008=CARTESIAN_POINT('Ctrl Pts',(81.0528500838303,-10.7659534750732,130.288932531162));
#72009=CARTESIAN_POINT('Ctrl Pts',(80.9903555592917,-10.8003314774452,130.285076181812));
#72010=CARTESIAN_POINT('Ctrl Pts',(80.9278794958464,-10.8346993244394,130.281220971641));
#72011=CARTESIAN_POINT('Ctrl Pts',(80.8635924811966,-10.8658221843169,130.277365761469));
#72012=CARTESIAN_POINT('Ctrl Pts',(80.7978669688866,-10.8935167975119,130.273510551298));
#72013=CARTESIAN_POINT('Ctrl Pts',(80.7321388862765,-10.9212124937485,130.269655190362));
#72014=CARTESIAN_POINT('Ctrl Pts',(80.6649726428412,-10.9454794905282,130.265799829427));
#72015=CARTESIAN_POINT('Ctrl Pts',(80.5967606250719,-10.9661826768802,130.261944468491));
#72016=CARTESIAN_POINT('Ctrl Pts',(80.528477206057,-10.9869075343884,130.258085071938));
#72017=CARTESIAN_POINT('Ctrl Pts',(80.4591462933012,-11.0040609933093,130.254225675386));
#72018=CARTESIAN_POINT('Ctrl Pts',(80.3891745224171,-11.0175581165363,130.250366278833));
#72019=CARTESIAN_POINT('Ctrl Pts',(80.3191631320623,-11.0310628821149,130.24650469701));
#72020=CARTESIAN_POINT('Ctrl Pts',(80.2485106425874,-11.0409071236151,130.242643115187));
#72021=CARTESIAN_POINT('Ctrl Pts',(80.1776302144995,-11.0470576614734,130.238781533364));
#72022=CARTESIAN_POINT('Ctrl Pts',(80.106625775804,-11.0532189601575,130.234913195415));
#72023=CARTESIAN_POINT('Ctrl Pts',(80.035393087939,-11.0556736360794,130.231044857466));
#72024=CARTESIAN_POINT('Ctrl Pts',(79.9643460192144,-11.0544406431324,130.227176519517));
#72025=CARTESIAN_POINT('Ctrl Pts',(79.9221592153547,-11.05370850833,130.224879551926));
#72026=CARTESIAN_POINT('Ctrl Pts',(79.8800377937428,-11.051677162781,130.222582584334));
#72027=CARTESIAN_POINT('Ctrl Pts',(79.8380670939317,-11.0483591717353,130.220285616743));
#72028=CARTESIAN_POINT('Ctrl Pts',(79.7673702407754,-11.0427702364356,130.216416527563));
#72029=CARTESIAN_POINT('Ctrl Pts',(79.6968246044294,-11.03350602237,130.212547438383));
#72030=CARTESIAN_POINT('Ctrl Pts',(79.6268426933459,-11.0205818931661,130.208678349203));
#72031=CARTESIAN_POINT('Ctrl Pts',(79.5569650524864,-11.0076770203932,130.20481502481));
#72032=CARTESIAN_POINT('Ctrl Pts',(79.4876499434675,-10.9911231442897,130.200951700417));
#72033=CARTESIAN_POINT('Ctrl Pts',(79.41930560889,-10.9709874648595,130.197088376024));
#72034=CARTESIAN_POINT('Ctrl Pts',(79.3510414437919,-10.9508754050453,130.193229583399));
#72035=CARTESIAN_POINT('Ctrl Pts',(79.283746254927,-10.9271900242032,130.189370790774));
#72036=CARTESIAN_POINT('Ctrl Pts',(79.2178172056323,-10.9000493779623,130.18551199815));
#72037=CARTESIAN_POINT('Ctrl Pts',(79.151929687824,-10.8729258287583,130.181655636341));
#72038=CARTESIAN_POINT('Ctrl Pts',(79.0874070503361,-10.8423515170163,130.177799274533));
#72039=CARTESIAN_POINT('Ctrl Pts',(79.0246290184254,-10.8084935749961,130.173942912724));
#72040=CARTESIAN_POINT('Ctrl Pts',(78.9618695329172,-10.7746456355676,130.170087690194));
#72041=CARTESIAN_POINT('Ctrl Pts',(78.9008540570915,-10.7375162222038,130.166232467664));
#72042=CARTESIAN_POINT('Ctrl Pts',(78.8419385666496,-10.6973188501535,130.162377245133));
#72043=CARTESIAN_POINT('Ctrl Pts',(78.7830207740229,-10.6571199073485,130.158521871956));
#72044=CARTESIAN_POINT('Ctrl Pts',(78.7262035297341,-10.6138530434507,130.154666498779));
#72045=CARTESIAN_POINT('Ctrl Pts',(78.6718131695291,-10.5677746349089,130.150811125601));
#72046=CARTESIAN_POINT('Ctrl Pts',(78.6173658798344,-10.5216479968595,130.146951717069));
#72047=CARTESIAN_POINT('Ctrl Pts',(78.5653509164017,-10.4727042543346,130.143092308536));
#72048=CARTESIAN_POINT('Ctrl Pts',(78.5160601907348,-10.4212389682871,130.139232900004));
#72049=CARTESIAN_POINT('Ctrl Pts',(78.4667415573744,-10.3697445433417,130.13537130633));
#72050=CARTESIAN_POINT('Ctrl Pts',(78.4201505496984,-10.3157261008707,130.131509712656));
#72051=CARTESIAN_POINT('Ctrl Pts',(78.3765391350539,-10.2595127559848,130.127648118983));
#72052=CARTESIAN_POINT('Ctrl Pts',(78.3328514229635,-10.2032010667853,130.123779769515));
#72053=CARTESIAN_POINT('Ctrl Pts',(78.2921539887692,-10.1446872075429,130.119911420047));
#72054=CARTESIAN_POINT('Ctrl Pts',(78.2546553847502,-10.0843291642848,130.11604307058));
#72055=CARTESIAN_POINT('Ctrl Pts',(78.2323903484066,-10.0484911894607,130.113746213303));
#72056=CARTESIAN_POINT('Ctrl Pts',(78.2112521765726,-10.0120035409388,130.111449356027));
#72057=CARTESIAN_POINT('Ctrl Pts',(78.1912765943959,-9.97494471869947,130.109152498751));
#72058=CARTESIAN_POINT('Ctrl Pts',(78.155830663704,-9.9091852112667,130.105076810588));
#72059=CARTESIAN_POINT('Ctrl Pts',(78.1239212019008,-9.84139127309731,130.101001122426));
#72060=CARTESIAN_POINT('Ctrl Pts',(78.0957732939458,-9.77195739160262,130.096925434263));
#72061=CARTESIAN_POINT('Ctrl Pts',(78.0677085507469,-9.70272865685746,130.092861787976));
#72062=CARTESIAN_POINT('Ctrl Pts',(78.0433833815986,-9.63187000592221,130.088798141689));
#72063=CARTESIAN_POINT('Ctrl Pts',(78.0229762170244,-9.55979864598709,130.084734495402));
#72064=CARTESIAN_POINT('Ctrl Pts',(78.0026057685884,-9.4878569553155,130.080678160342));
#72065=CARTESIAN_POINT('Ctrl Pts',(77.9861394179744,-9.41470728619444,130.076621825281));
#72066=CARTESIAN_POINT('Ctrl Pts',(77.9737071028153,-9.34078535373292,130.07256549022));
#72067=CARTESIAN_POINT('Ctrl Pts',(77.96130303065,-9.26703135271886,130.0685183701));
#72068=CARTESIAN_POINT('Ctrl Pts',(77.9529148139121,-9.19250898403491,130.06447124998));
#72069=CARTESIAN_POINT('Ctrl Pts',(77.9486218581334,-9.11766597457222,130.06042412986));
#72070=CARTESIAN_POINT('Ctrl Pts',(77.946376826516,-9.07852629290516,130.058307659741));
#72071=CARTESIAN_POINT('Ctrl Pts',(77.9452509482569,-9.03929913360494,130.056191189622));
#72072=CARTESIAN_POINT('Ctrl Pts',(77.9452500005989,-9.00004961080127,130.054074719503));
#72073=CARTESIAN_POINT('Origin',(80.,-9.,141.545925280538));
#72074=CARTESIAN_POINT('',(81.2520391107129,-7.37076839346111,131.206019331682));
#72075=CARTESIAN_POINT('',(81.2520391107129,-7.3707683934611,131.147979657963));
#72076=CARTESIAN_POINT('',(81.2520391107129,-7.37076839346111,141.545925280538));
#72077=CARTESIAN_POINT('',(77.9452508472645,-8.99813403300313,130.695925280507));
#72078=CARTESIAN_POINT('Ctrl Pts',(81.2520391107129,-7.3707683934611,131.147979657963));
#72079=CARTESIAN_POINT('Ctrl Pts',(81.3086037747096,-7.4142374566219,131.144119415677));
#72080=CARTESIAN_POINT('Ctrl Pts',(81.362864049299,-7.46062653621925,131.14025917339));
#72081=CARTESIAN_POINT('Ctrl Pts',(81.4145173037714,-7.50965159783651,131.136398931104));
#72082=CARTESIAN_POINT('Ctrl Pts',(81.4662067801097,-7.55871103829843,131.132535981821));
#72083=CARTESIAN_POINT('Ctrl Pts',(81.5152852658367,-7.61040978588829,131.128673032539));
#72084=CARTESIAN_POINT('Ctrl Pts',(81.5614888520647,-7.66442891339409,131.124810083256));
#72085=CARTESIAN_POINT('Ctrl Pts',(81.607767173866,-7.71853541832652,131.120940885546));
#72086=CARTESIAN_POINT('Ctrl Pts',(81.6511610284125,-7.77496940355062,131.117071687836));
#72087=CARTESIAN_POINT('Ctrl Pts',(81.6914490147046,-7.83338189918263,131.113202490127));
#72088=CARTESIAN_POINT('Ctrl Pts',(81.6972565756089,-7.8418021295584,131.112644740698));
#72089=CARTESIAN_POINT('Ctrl Pts',(81.7029996757573,-7.85026343058691,131.112086991269));
#72090=CARTESIAN_POINT('Ctrl Pts',(81.7086777314096,-7.85876471633363,131.11152924184));
#72091=CARTESIAN_POINT('Ctrl Pts',(81.748066149928,-7.91773775595226,131.107660158956));
#72092=CARTESIAN_POINT('Ctrl Pts',(81.7844750515849,-7.97886786377236,131.103791076072));
#72093=CARTESIAN_POINT('Ctrl Pts',(81.8176610664465,-8.04182161889099,131.099921993188));
#72094=CARTESIAN_POINT('Ctrl Pts',(81.8507976357948,-8.10468157604252,131.096058675046));
#72095=CARTESIAN_POINT('Ctrl Pts',(81.8807206253814,-8.16935936080732,131.092195356903));
#72096=CARTESIAN_POINT('Ctrl Pts',(81.9072300095338,-8.2354928036743,131.088332038761));
#72097=CARTESIAN_POINT('Ctrl Pts',(81.9337082981801,-8.30154867201683,131.08447325229));
#72098=CARTESIAN_POINT('Ctrl Pts',(81.9567807551404,-8.36905635809634,131.080614465819));
#72099=CARTESIAN_POINT('Ctrl Pts',(81.9762941479208,-8.43763090110313,131.076755679349));
#72100=CARTESIAN_POINT('Ctrl Pts',(81.9957952486906,-8.50616224716216,131.072899323631));
#72101=CARTESIAN_POINT('Ctrl Pts',(82.0117416006339,-8.57575865069783,131.069042967914));
#72102=CARTESIAN_POINT('Ctrl Pts',(82.0240293050706,-8.64601845427297,131.065186612197));
#72103=CARTESIAN_POINT('Ctrl Pts',(82.0363133795937,-8.71625750238318,131.061331395686));
#72104=CARTESIAN_POINT('Ctrl Pts',(82.0449408686595,-8.78715908320829,131.057476179176));
#72105=CARTESIAN_POINT('Ctrl Pts',(82.0498590005135,-8.8583114665404,131.053620962666));
#72106=CARTESIAN_POINT('Ctrl Pts',(82.0547773246505,-8.92946663170095,131.049765595429));
#72107=CARTESIAN_POINT('Ctrl Pts',(82.0559859723494,-9.00087213405753,131.045910228192));
#72108=CARTESIAN_POINT('Ctrl Pts',(82.0534841808734,-9.07211297666065,131.042054860955));
#72109=CARTESIAN_POINT('Ctrl Pts',(82.0509797707049,-9.14342838896989,131.038195458202));
#72110=CARTESIAN_POINT('Ctrl Pts',(82.0447571854772,-9.21457831099044,131.034336055448));
#72111=CARTESIAN_POINT('Ctrl Pts',(82.0348677469965,-9.28515051242027,131.030476652695));
#72112=CARTESIAN_POINT('Ctrl Pts',(82.0249727090402,-9.35576267236917,131.026615064718));
#72113=CARTESIAN_POINT('Ctrl Pts',(82.0114067771824,-9.42579598340886,131.022753476741));
#72114=CARTESIAN_POINT('Ctrl Pts',(81.9942723547638,-9.49484880269107,131.018891888764));
#72115=CARTESIAN_POINT('Ctrl Pts',(81.9771079550666,-9.56402243232522,131.015023544803));
#72116=CARTESIAN_POINT('Ctrl Pts',(81.9563627415182,-9.63221168044898,131.011155200841));
#72117=CARTESIAN_POINT('Ctrl Pts',(81.9321886708894,-9.69903111703738,131.007286856879));
#72118=CARTESIAN_POINT('Ctrl Pts',(81.9178348053739,-9.73870657018487,131.004989945869));
#72119=CARTESIAN_POINT('Ctrl Pts',(81.9022729705369,-9.77789946020317,131.002693034859));
#72120=CARTESIAN_POINT('Ctrl Pts',(81.8855426871365,-9.81653312087521,131.000396123848));
#72121=CARTESIAN_POINT('Ctrl Pts',(81.8573609872102,-9.88161045435812,130.996527040743));
#72122=CARTESIAN_POINT('Ctrl Pts',(81.8257510312545,-9.94535454821874,130.992657957637));
#72123=CARTESIAN_POINT('Ctrl Pts',(81.7908609381868,-10.0073800983624,130.988788874532));
#72124=CARTESIAN_POINT('Ctrl Pts',(81.7560228296013,-10.0693132335588,130.984925556166));
#72125=CARTESIAN_POINT('Ctrl Pts',(81.7179145211625,-10.1295324877013,130.9810622378));
#72126=CARTESIAN_POINT('Ctrl Pts',(81.6767317935167,-10.1876733789685,130.977198919433));
#72127=CARTESIAN_POINT('Ctrl Pts',(81.635597373182,-10.2457460710103,130.973340132737));
#72128=CARTESIAN_POINT('Ctrl Pts',(81.5913959763829,-10.3017448482196,130.96948134604));
#72129=CARTESIAN_POINT('Ctrl Pts',(81.5443679111866,-10.3553321797246,130.965622559344));
#72130=CARTESIAN_POINT('Ctrl Pts',(81.4973694702163,-10.4088857551478,130.961766203399));
#72131=CARTESIAN_POINT('Ctrl Pts',(81.4475482131879,-10.4600305343499,130.957909847455));
#72132=CARTESIAN_POINT('Ctrl Pts',(81.395185233245,-10.5084613775086,130.954053491511));
#72133=CARTESIAN_POINT('Ctrl Pts',(81.3428377218496,-10.5568779137122,130.950198274772));
#72134=CARTESIAN_POINT('Ctrl Pts',(81.2879503346217,-10.6025817758474,130.946343058034));
#72135=CARTESIAN_POINT('Ctrl Pts',(81.2308403574089,-10.6453053142422,130.942487841296));
#72136=CARTESIAN_POINT('Ctrl Pts',(81.1737281473731,-10.6880305229949,130.93863247383));
#72137=CARTESIAN_POINT('Ctrl Pts',(81.1143935651329,-10.7277748874385,130.934777106365));
#72138=CARTESIAN_POINT('Ctrl Pts',(81.0531848497,-10.764312680582,130.9309217389));
#72139=CARTESIAN_POINT('Ctrl Pts',(80.991912065475,-10.8008887188063,130.927062335918));
#72140=CARTESIAN_POINT('Ctrl Pts',(80.9287616500267,-10.8342512360934,130.923202932937));
#72141=CARTESIAN_POINT('Ctrl Pts',(80.8641077676447,-10.8642197639753,130.919343529956));
#72142=CARTESIAN_POINT('Ctrl Pts',(80.7994172777452,-10.8942052602645,130.915481941752));
#72143=CARTESIAN_POINT('Ctrl Pts',(80.7332220772815,-10.9207927604884,130.911620353548));
#72144=CARTESIAN_POINT('Ctrl Pts',(80.6659151412917,-10.9438504538926,130.907758765343));
#72145=CARTESIAN_POINT('Ctrl Pts',(80.598490449488,-10.9669484875295,130.903890421157));
#72146=CARTESIAN_POINT('Ctrl Pts',(80.5299506061597,-10.9865042514215,130.90002207697));
#72147=CARTESIAN_POINT('Ctrl Pts',(80.4607018422215,-11.0024363598062,130.896153732784));
#72148=CARTESIAN_POINT('Ctrl Pts',(80.4195839634142,-11.0118963770606,130.893856823808));
#72149=CARTESIAN_POINT('Ctrl Pts',(80.3782163235417,-11.0200798088441,130.891559914832));
#72150=CARTESIAN_POINT('Ctrl Pts',(80.3366847674755,-11.0269782756236,130.889263005857));
#72151=CARTESIAN_POINT('Ctrl Pts',(80.2667259651641,-11.0385985595567,130.885393923738));
#72152=CARTESIAN_POINT('Ctrl Pts',(80.196027842885,-11.0466155311481,130.881524841618));
#72153=CARTESIAN_POINT('Ctrl Pts',(80.124994443943,-11.0509446485665,130.877655759499));
#72154=CARTESIAN_POINT('Ctrl Pts',(80.0540668812426,-11.0552673158145,130.873792442121));
#72155=CARTESIAN_POINT('Ctrl Pts',(79.9828055143971,-11.0559130064459,130.869929124742));
#72156=CARTESIAN_POINT('Ctrl Pts',(79.9116227440299,-11.0528485144129,130.866065807363));
#72157=CARTESIAN_POINT('Ctrl Pts',(79.840523470976,-11.0497876170257,130.862207021652));
#72158=CARTESIAN_POINT('Ctrl Pts',(79.7695030942512,-11.0430252023924,130.85834823594));
#72159=CARTESIAN_POINT('Ctrl Pts',(79.6989755229046,-11.0325800910885,130.854489450228));
#72160=CARTESIAN_POINT('Ctrl Pts',(79.628492378718,-11.0221415594332,130.850633095267));
#72161=CARTESIAN_POINT('Ctrl Pts',(79.5585019034254,-11.0080250046074,130.846776740305));
#72162=CARTESIAN_POINT('Ctrl Pts',(79.489412914315,-10.9903010803473,130.842920385343));
#72163=CARTESIAN_POINT('Ctrl Pts',(79.4203443347233,-10.9725823918964,130.839065169584));
#72164=CARTESIAN_POINT('Ctrl Pts',(79.35217718291,-10.9512585702692,130.835209953825));
#72165=CARTESIAN_POINT('Ctrl Pts',(79.2853084096626,-10.9264510098108,130.831354738066));
#72166=CARTESIAN_POINT('Ctrl Pts',(79.2184370219655,-10.901642479421,130.827499371575));
#72167=CARTESIAN_POINT('Ctrl Pts',(79.1528645683048,-10.8733501108095,130.823644005084));
#72168=CARTESIAN_POINT('Ctrl Pts',(79.0889695672252,-10.8417440411355,130.819788638592));
#72169=CARTESIAN_POINT('Ctrl Pts',(79.0250076852926,-10.8101048884212,130.815929236571));
#72170=CARTESIAN_POINT('Ctrl Pts',(78.9627271973097,-10.7751453264637,130.81206983455));
#72171=CARTESIAN_POINT('Ctrl Pts',(78.9024826599988,-10.7370818204382,130.808210432529));
#72172=CARTESIAN_POINT('Ctrl Pts',(78.842204011663,-10.6989967624967,130.804348845277));
#72173=CARTESIAN_POINT('Ctrl Pts',(78.7839640056126,-10.6578045425288,130.800487258026));
#72174=CARTESIAN_POINT('Ctrl Pts',(78.7280865221899,-10.6137638202243,130.796625670775));
#72175=CARTESIAN_POINT('Ctrl Pts',(78.672111278851,-10.5696460468958,130.792757327521));
#72176=CARTESIAN_POINT('Ctrl Pts',(78.6185071759079,-10.5226701416633,130.788888984267));
#72177=CARTESIAN_POINT('Ctrl Pts',(78.5675629197205,-10.473133250436,130.785020641013));
#72178=CARTESIAN_POINT('Ctrl Pts',(78.5373135967212,-10.4437195827283,130.782723723297));
#72179=CARTESIAN_POINT('Ctrl Pts',(78.5080013169699,-10.4134036807332,130.780426805581));
#72180=CARTESIAN_POINT('Ctrl Pts',(78.4796796815619,-10.3822531214811,130.778129887865));
#72181=CARTESIAN_POINT('Ctrl Pts',(78.432491033328,-10.3303510063079,130.774302833369));
#72182=CARTESIAN_POINT('Ctrl Pts',(78.3878608320509,-10.2759167409365,130.770475778873));
#72183=CARTESIAN_POINT('Ctrl Pts',(78.3460767383655,-10.2192355831111,130.766648724377));
#72184=CARTESIAN_POINT('Ctrl Pts',(78.3043498473697,-10.1626320221507,130.762826909143));
#72185=CARTESIAN_POINT('Ctrl Pts',(78.2654616325306,-10.1037880620617,130.759005093909));
#72186=CARTESIAN_POINT('Ctrl Pts',(78.2296616569659,-10.043024311166,130.755183278674));
#72187=CARTESIAN_POINT('Ctrl Pts',(78.1938980883374,-9.98232235422308,130.751365350051));
#72188=CARTESIAN_POINT('Ctrl Pts',(78.1612167818143,-9.91970490401357,130.747547421428));
#72189=CARTESIAN_POINT('Ctrl Pts',(78.1318247421453,-9.85552251194209,130.743729492805));
#72190=CARTESIAN_POINT('Ctrl Pts',(78.1011566442909,-9.78855363524112,130.73974580845));
#72191=CARTESIAN_POINT('Ctrl Pts',(78.0740702736535,-9.71988128861933,130.735762124094));
#72192=CARTESIAN_POINT('Ctrl Pts',(78.0507474289142,-9.6499322861771,130.731778439738));
#72193=CARTESIAN_POINT('Ctrl Pts',(78.0284112294296,-9.58294239323039,130.72796328042));
#72194=CARTESIAN_POINT('Ctrl Pts',(78.0095266831817,-9.5147822055705,130.724148121101));
#72195=CARTESIAN_POINT('Ctrl Pts',(77.9942033860666,-9.44584471067081,130.720332961782));
#72196=CARTESIAN_POINT('Ctrl Pts',(77.978879928244,-9.37690649276972,130.71651776245));
#72197=CARTESIAN_POINT('Ctrl Pts',(77.9671178912741,-9.30719143896892,130.712702563119));
#72198=CARTESIAN_POINT('Ctrl Pts',(77.958975811088,-9.23710297926417,130.708887363787));
#72199=CARTESIAN_POINT('Ctrl Pts',(77.9508281237988,-9.16696625262999,130.705069537091));
#72200=CARTESIAN_POINT('Ctrl Pts',(77.9463054071666,-9.09645610237582,130.701251710395));
#72201=CARTESIAN_POINT('Ctrl Pts',(77.9454142484556,-9.0259798393166,130.697433883698));
#72202=CARTESIAN_POINT('Ctrl Pts',(77.9452968688612,-9.01669700891443,130.696931015978));
#72203=CARTESIAN_POINT('Ctrl Pts',(77.9452424192122,-9.00741476447613,130.696428148258));
#72204=CARTESIAN_POINT('Ctrl Pts',(77.945250847264,-8.99813403357328,130.695925280538));
#72205=CARTESIAN_POINT('Ctrl Pts',(77.9452508472645,-8.99813403300313,130.695925280507));
#72206=CARTESIAN_POINT('Ctrl Pts',(77.9453334654873,-8.90715722391885,130.690995787233));
#72207=CARTESIAN_POINT('Ctrl Pts',(77.9514620741457,-8.81644963145446,130.686066293958));
#72208=CARTESIAN_POINT('Ctrl Pts',(77.9635073127305,-8.72669596197999,130.681136800683));
#72209=CARTESIAN_POINT('Ctrl Pts',(77.9750243886388,-8.64087783416966,130.67642345708));
#72210=CARTESIAN_POINT('Ctrl Pts',(77.9919501516155,-8.55593137583548,130.671710113477));
#72211=CARTESIAN_POINT('Ctrl Pts',(78.014131603958,-8.47243552422342,130.666996769874));
#72212=CARTESIAN_POINT('Ctrl Pts',(78.0323398920176,-8.40389553439494,130.663127685166));
#72213=CARTESIAN_POINT('Ctrl Pts',(78.0541363781932,-8.33616506606054,130.659258600459));
#72214=CARTESIAN_POINT('Ctrl Pts',(78.079431785375,-8.26964714317534,130.655389515751));
#72215=CARTESIAN_POINT('Ctrl Pts',(78.1046895037667,-8.20322832840126,130.651526195771));
#72216=CARTESIAN_POINT('Ctrl Pts',(78.133435623837,-8.13801892333169,130.64766287579));
#72217=CARTESIAN_POINT('Ctrl Pts',(78.1655306436996,-8.0744084360288,130.64379955581));
#72218=CARTESIAN_POINT('Ctrl Pts',(78.1975880162222,-8.01087256359274,130.639940767489));
#72219=CARTESIAN_POINT('Ctrl Pts',(78.2329862679424,-7.94893231509545,130.636081979169));
#72220=CARTESIAN_POINT('Ctrl Pts',(78.2715378619355,-7.88895715664184,130.632223190848));
#72221=CARTESIAN_POINT('Ctrl Pts',(78.3100651713178,-7.82901977803666,130.628366833275));
#72222=CARTESIAN_POINT('Ctrl Pts',(78.3517416199971,-7.77104544125757,130.624510475702));
#72223=CARTESIAN_POINT('Ctrl Pts',(78.39633452927,-7.71537763506611,130.620654118128));
#72224=CARTESIAN_POINT('Ctrl Pts',(78.4409142653881,-7.65972627365573,130.616798899759));
#72225=CARTESIAN_POINT('Ctrl Pts',(78.4884084481412,-7.60638046905467,130.612943681389));
#72226=CARTESIAN_POINT('Ctrl Pts',(78.538543041537,-7.55565200832347,130.609088463019));
#72227=CARTESIAN_POINT('Ctrl Pts',(78.588679595042,-7.50492156426463,130.605233093922));
#72228=CARTESIAN_POINT('Ctrl Pts',(78.6414564211046,-7.45680901120684,130.601377724824));
#72229=CARTESIAN_POINT('Ctrl Pts',(78.6965626498843,-7.41158927325979,130.597522355727));
#72230=CARTESIAN_POINT('Ctrl Pts',(78.7517265596389,-7.36632220275835,130.593662951125));
#72231=CARTESIAN_POINT('Ctrl Pts',(78.8092243630841,-7.32395430067749,130.589803546523));
#72232=CARTESIAN_POINT('Ctrl Pts',(78.8687128334742,-7.28471958288035,130.585944141922));
#72233=CARTESIAN_POINT('Ctrl Pts',(78.9282349866143,-7.24546265013672,130.5820825521));
#72234=CARTESIAN_POINT('Ctrl Pts',(78.9897496313597,-7.20934267930978,130.578220962279));
#72235=CARTESIAN_POINT('Ctrl Pts',(79.0528877151142,-7.1765483603017,130.574359372458));
#72236=CARTESIAN_POINT('Ctrl Pts',(79.1161362606994,-7.14369666672193,130.570491026678));
#72237=CARTESIAN_POINT('Ctrl Pts',(79.1810134736196,-7.11418244262259,130.566622680898));
#72238=CARTESIAN_POINT('Ctrl Pts',(79.2471297063824,-7.08814647959419,130.562754335118));
#72239=CARTESIAN_POINT('Ctrl Pts',(79.2863873152439,-7.07268719508579,130.560457440706));
#72240=CARTESIAN_POINT('Ctrl Pts',(79.3260814289308,-7.0584532561107,130.558160546294));
#72241=CARTESIAN_POINT('Ctrl Pts',(79.3661283994563,-7.04546569318312,130.555863651882));
#72242=CARTESIAN_POINT('Ctrl Pts',(79.4335880972261,-7.02358795665611,130.551994500213));
#72243=CARTESIAN_POINT('Ctrl Pts',(79.5023139048528,-7.00516397119918,130.548125348544));
#72244=CARTESIAN_POINT('Ctrl Pts',(79.5719187854035,-6.9903373327323,130.544256196876));
#72245=CARTESIAN_POINT('Ctrl Pts',(79.6441103182617,-6.97495970763487,130.54024326003));
#72246=CARTESIAN_POINT('Ctrl Pts',(79.7172470800461,-6.96345231053239,130.536230323184));
#72247=CARTESIAN_POINT('Ctrl Pts',(79.7908772299262,-6.95591946598558,130.532217386337));
#72248=CARTESIAN_POINT('Ctrl Pts',(79.8616761607451,-6.94867627361388,130.528358754532));
#72249=CARTESIAN_POINT('Ctrl Pts',(79.9329306947213,-6.94510762601367,130.524500122727));
#72250=CARTESIAN_POINT('Ctrl Pts',(80.004228495175,-6.9452543509406,130.520641490922));
#72251=CARTESIAN_POINT('Ctrl Pts',(80.0754817362487,-6.94540098416803,130.516785270667));
#72252=CARTESIAN_POINT('Ctrl Pts',(80.1467777054929,-6.94925838149796,130.512929050412));
#72253=CARTESIAN_POINT('Ctrl Pts',(80.2177016824627,-6.95681534364784,130.509072830158));
#72254=CARTESIAN_POINT('Ctrl Pts',(80.2886050591163,-6.96437011083043,130.505217729966));
#72255=CARTESIAN_POINT('Ctrl Pts',(80.3591361753002,-6.9756222575018,130.501362629775));
#72256=CARTESIAN_POINT('Ctrl Pts',(80.4288847876532,-6.99050867097674,130.497507529584));
#72257=CARTESIAN_POINT('Ctrl Pts',(80.4986364724683,-7.00539574020581,130.493652259574));
#72258=CARTESIAN_POINT('Ctrl Pts',(80.5676051105877,-7.02391728997555,130.489796989563));
#72259=CARTESIAN_POINT('Ctrl Pts',(80.6353917187032,-7.04595933350828,130.485941719553));
#72260=CARTESIAN_POINT('Ctrl Pts',(80.7032436165698,-7.06802260718628,130.482082736278));
#72261=CARTESIAN_POINT('Ctrl Pts',(80.7699107501882,-7.09361298979535,130.478223753003));
#72262=CARTESIAN_POINT('Ctrl Pts',(80.8350113131769,-7.12256726635372,130.474364769728));
#72263=CARTESIAN_POINT('Ctrl Pts',(80.9001492847591,-7.1515381808444,130.470503568973));
#72264=CARTESIAN_POINT('Ctrl Pts',(80.9637184610631,-7.18387661662423,130.466642368219));
#72265=CARTESIAN_POINT('Ctrl Pts',(81.025361334346,-7.21937322930149,130.462781167465));
#72266=CARTESIAN_POINT('Ctrl Pts',(81.0870986711808,-7.25492423814713,130.458914049681));
#72267=CARTESIAN_POINT('Ctrl Pts',(81.1469034085351,-7.29364281593865,130.455046931896));
#72268=CARTESIAN_POINT('Ctrl Pts',(81.2044475328565,-7.33527668872698,130.451179814112));
#72269=CARTESIAN_POINT('Ctrl Pts',(81.2204890700428,-7.34688293569694,130.450101780265));
#72270=CARTESIAN_POINT('Ctrl Pts',(81.2363551343962,-7.35871550197462,130.449023746417));
#72271=CARTESIAN_POINT('Ctrl Pts',(81.2520391107129,-7.37076839346111,130.44794571257));
#72272=CARTESIAN_POINT('',(77.9452507933687,-9.00180564337554,130.754074719418));
#72273=CARTESIAN_POINT('Ctrl Pts',(77.9452507933687,-9.00180564337555,130.754074719418));
#72274=CARTESIAN_POINT('Ctrl Pts',(77.9451892124666,-8.93172906490193,130.75026907596));
#72275=CARTESIAN_POINT('Ctrl Pts',(77.9487167666403,-8.86153512362492,130.746463432502));
#72276=CARTESIAN_POINT('Ctrl Pts',(77.9558428519795,-8.79162745695133,130.742657789045));
#72277=CARTESIAN_POINT('Ctrl Pts',(77.9629627689979,-8.72178030217006,130.738855439742));
#72278=CARTESIAN_POINT('Ctrl Pts',(77.9736749941492,-8.65221942719567,130.735053090439));
#72279=CARTESIAN_POINT('Ctrl Pts',(77.9879368905025,-8.5833471398165,130.731250741136));
#72280=CARTESIAN_POINT('Ctrl Pts',(78.0021915378923,-8.51450985848987,130.727450324471));
#72281=CARTESIAN_POINT('Ctrl Pts',(78.0199921779358,-8.44636096084695,130.723649907807));
#72282=CARTESIAN_POINT('Ctrl Pts',(78.0412447589193,-8.37929437892127,130.719849491143));
#72283=CARTESIAN_POINT('Ctrl Pts',(78.0624941303822,-8.31223792525093,130.716049648409));
#72284=CARTESIAN_POINT('Ctrl Pts',(78.0871942556725,-8.24626394027792,130.712249805676));
#72285=CARTESIAN_POINT('Ctrl Pts',(78.1152012631972,-8.18175108662069,130.708449962943));
#72286=CARTESIAN_POINT('Ctrl Pts',(78.1432332471445,-8.11718070092245,130.70464673154));
#72287=CARTESIAN_POINT('Ctrl Pts',(78.1745778040796,-8.05407451019606,130.700843500138));
#72288=CARTESIAN_POINT('Ctrl Pts',(78.2090433737826,-7.99279002908629,130.697040268735));
#72289=CARTESIAN_POINT('Ctrl Pts',(78.2435240047018,-7.93147876708109,130.693235375347));
#72290=CARTESIAN_POINT('Ctrl Pts',(78.281128094716,-7.87199122326443,130.689430481959));
#72291=CARTESIAN_POINT('Ctrl Pts',(78.3216202127564,-7.81465665215848,130.685625588571));
#72292=CARTESIAN_POINT('Ctrl Pts',(78.3621848365631,-7.75721941694875,130.681813882086));
#72293=CARTESIAN_POINT('Ctrl Pts',(78.4056475048417,-7.70194324737498,130.678002175601));
#72294=CARTESIAN_POINT('Ctrl Pts',(78.4517323843917,-7.64912437546652,130.674190469116));
#72295=CARTESIAN_POINT('Ctrl Pts',(78.4895041823922,-7.60583330516712,130.671066342314));
#72296=CARTESIAN_POINT('Ctrl Pts',(78.5290366712978,-7.56419239373585,130.667942215512));
#72297=CARTESIAN_POINT('Ctrl Pts',(78.5701610019991,-7.52434489046531,130.664818088709));
#72298=CARTESIAN_POINT('Ctrl Pts',(78.6210915251772,-7.47499565719387,130.660949006592));
#72299=CARTESIAN_POINT('Ctrl Pts',(78.6746796484665,-7.42818957462096,130.657079924474));
#72300=CARTESIAN_POINT('Ctrl Pts',(78.7306411390617,-7.38422599208386,130.653210842356));
#72301=CARTESIAN_POINT('Ctrl Pts',(78.7865192498114,-7.34032791310425,130.649347524979));
#72302=CARTESIAN_POINT('Ctrl Pts',(78.8447633297201,-7.29926422509389,130.645484207602));
#72303=CARTESIAN_POINT('Ctrl Pts',(78.9050530730376,-7.2612968080677,130.641620890225));
#72304=CARTESIAN_POINT('Ctrl Pts',(78.9652720965509,-7.22337392678093,130.637762104515));
#72305=CARTESIAN_POINT('Ctrl Pts',(79.0275316080639,-7.18854035986118,130.633903318805));
#72306=CARTESIAN_POINT('Ctrl Pts',(79.0914804690462,-7.15701605422743,130.630044533095));
#72307=CARTESIAN_POINT('Ctrl Pts',(79.1553890469699,-7.12551160657752,130.626188178135));
#72308=CARTESIAN_POINT('Ctrl Pts',(79.2209844283878,-7.09731249870358,130.622331823175));
#72309=CARTESIAN_POINT('Ctrl Pts',(79.2878901805766,-7.07259314944127,130.618475468214));
#72310=CARTESIAN_POINT('Ctrl Pts',(79.354776168195,-7.04788110250054,130.614620252457));
#72311=CARTESIAN_POINT('Ctrl Pts',(79.4229713026635,-7.02664694166551,130.610765036699));
#72312=CARTESIAN_POINT('Ctrl Pts',(79.4920800506123,-7.00901660290348,130.606909820942));
#72313=CARTESIAN_POINT('Ctrl Pts',(79.5611915005902,-6.99138557482657,130.603054454452));
#72314=CARTESIAN_POINT('Ctrl Pts',(79.6312161637148,-6.97735876651486,130.599199087962));
#72315=CARTESIAN_POINT('Ctrl Pts',(79.70174594251,-6.96701153970546,130.595343721472));
#72316=CARTESIAN_POINT('Ctrl Pts',(79.7723495469836,-6.95665348213704,130.591484319453));
#72317=CARTESIAN_POINT('Ctrl Pts',(79.8434588409484,-6.94998276524663,130.587624917433));
#72318=CARTESIAN_POINT('Ctrl Pts',(79.9146590843218,-6.94702301751549,130.583765515413));
#72319=CARTESIAN_POINT('Ctrl Pts',(79.9858996419443,-6.94406159394727,130.579903928163));
#72320=CARTESIAN_POINT('Ctrl Pts',(80.0572307655028,-6.94481531721578,130.576042340914));
#72321=CARTESIAN_POINT('Ctrl Pts',(80.1282389460113,-6.94925566312475,130.572180753664));
#72322=CARTESIAN_POINT('Ctrl Pts',(80.199371358203,-6.95370377759844,130.568312410411));
#72323=CARTESIAN_POINT('Ctrl Pts',(80.2701792165508,-6.96185133656276,130.564444067159));
#72324=CARTESIAN_POINT('Ctrl Pts',(80.3402560516066,-6.97361815497545,130.560575723906));
#72325=CARTESIAN_POINT('Ctrl Pts',(80.381865783308,-6.98060497389702,130.558278806176));
#72326=CARTESIAN_POINT('Ctrl Pts',(80.4232179919651,-6.9888668452408,130.555981888447));
#72327=CARTESIAN_POINT('Ctrl Pts',(80.4642301545167,-6.99837867563882,130.553684970717));
#72328=CARTESIAN_POINT('Ctrl Pts',(80.5351039378127,-7.01481622402536,130.549715629934));
#72329=CARTESIAN_POINT('Ctrl Pts',(80.605246038444,-7.03505572659329,130.545746289151));
#72330=CARTESIAN_POINT('Ctrl Pts',(80.6742185442106,-7.05901393174951,130.541776948368));
#72331=CARTESIAN_POINT('Ctrl Pts',(80.7413369803834,-7.08232810956167,130.537914308567));
#72332=CARTESIAN_POINT('Ctrl Pts',(80.8073474059089,-7.10916343562223,130.534051668765));
#72333=CARTESIAN_POINT('Ctrl Pts',(80.8718566425127,-7.13939161632369,130.530189028963));
#72334=CARTESIAN_POINT('Ctrl Pts',(80.939038869302,-7.17087232510634,130.52616633769));
#72335=CARTESIAN_POINT('Ctrl Pts',(81.0045922551066,-7.20603309031259,130.522143646416));
#72336=CARTESIAN_POINT('Ctrl Pts',(81.068092810446,-7.24467230672629,130.518120955142));
#72337=CARTESIAN_POINT('Ctrl Pts',(81.1315933657854,-7.28331152314,130.514098263869));
#72338=CARTESIAN_POINT('Ctrl Pts',(81.1930405549278,-7.32542892237426,130.510075572595));
#72339=CARTESIAN_POINT('Ctrl Pts',(81.2520391107129,-7.37076839346111,130.506052881321));
#72340=CARTESIAN_POINT('Ctrl Pts',(81.2520391107129,-7.37076839346111,131.206019331682));
#72341=CARTESIAN_POINT('Ctrl Pts',(81.3108254762814,-7.41594479967191,131.201991466223));
#72342=CARTESIAN_POINT('Ctrl Pts',(81.3672518683302,-7.46437480581457,131.197963600765));
#72343=CARTESIAN_POINT('Ctrl Pts',(81.420942732416,-7.51577652838455,131.193935735306));
#72344=CARTESIAN_POINT('Ctrl Pts',(81.4723686497498,-7.56500987153721,131.190077785176));
#72345=CARTESIAN_POINT('Ctrl Pts',(81.5212847957304,-7.61696888104173,131.186219835045));
#72346=CARTESIAN_POINT('Ctrl Pts',(81.5673942501132,-7.67136429853329,131.182361884915));
#72347=CARTESIAN_POINT('Ctrl Pts',(81.6134791222044,-7.72573071624524,131.17850599157));
#72348=CARTESIAN_POINT('Ctrl Pts',(81.6567599581888,-7.78253059464984,131.174650098225));
#72349=CARTESIAN_POINT('Ctrl Pts',(81.6969781583872,-7.84143938766383,131.17079420488));
#72350=CARTESIAN_POINT('Ctrl Pts',(81.7371883706359,-7.90033648049054,131.166939077374));
#72351=CARTESIAN_POINT('Ctrl Pts',(81.7743368814707,-7.96134125486396,131.163083949868));
#72352=CARTESIAN_POINT('Ctrl Pts',(81.8082077333116,-8.02409920806872,131.159228822363));
#72353=CARTESIAN_POINT('Ctrl Pts',(81.8420831878268,-8.0868656893855,131.155373170988));
#72354=CARTESIAN_POINT('Ctrl Pts',(81.8726798707601,-8.15138539377557,131.151517519613));
#72355=CARTESIAN_POINT('Ctrl Pts',(81.899828028585,-8.21727972793427,131.147661868238));
#72356=CARTESIAN_POINT('Ctrl Pts',(81.9270062103126,-8.28324693646923,131.143801952791));
#72357=CARTESIAN_POINT('Ctrl Pts',(81.9507280728954,-8.35059135785771,131.139942037344));
#72358=CARTESIAN_POINT('Ctrl Pts',(81.9708725888309,-8.41891583992077,131.136082121897));
#72359=CARTESIAN_POINT('Ctrl Pts',(81.9910302592243,-8.4872849381727,131.132219685908));
#72360=CARTESIAN_POINT('Ctrl Pts',(82.0076058223155,-8.55663489829064,131.12835724992));
#72361=CARTESIAN_POINT('Ctrl Pts',(82.0205292093832,-8.62655753250442,131.124494813931));
#72362=CARTESIAN_POINT('Ctrl Pts',(82.0334740890637,-8.69659645357762,131.120625954406));
#72363=CARTESIAN_POINT('Ctrl Pts',(82.0427546124962,-8.76720946810902,131.116757094882));
#72364=CARTESIAN_POINT('Ctrl Pts',(82.0483525478946,-8.83798332791455,131.112888235357));
#72365=CARTESIAN_POINT('Ctrl Pts',(82.0500587935554,-8.85955513655416,131.111709010463));
#72366=CARTESIAN_POINT('Ctrl Pts',(82.051423284175,-8.88114189500333,131.110529785569));
#72367=CARTESIAN_POINT('Ctrl Pts',(82.0524464644487,-8.90273195246212,131.109350560675));
#72368=CARTESIAN_POINT('Ctrl Pts',(82.0558035588436,-8.97356977326592,131.105481477794));
#72369=CARTESIAN_POINT('Ctrl Pts',(82.055495594845,-9.04472034164982,131.101612394913));
#72370=CARTESIAN_POINT('Ctrl Pts',(82.0514858739564,-9.1157724987093,131.097743312031));
#72371=CARTESIAN_POINT('Ctrl Pts',(82.0474821273517,-9.18671879160199,131.09387999389));
#72372=CARTESIAN_POINT('Ctrl Pts',(82.0397875989869,-9.25756648316244,131.090016675749));
#72373=CARTESIAN_POINT('Ctrl Pts',(82.0284175513188,-9.32790211954455,131.086153357608));
#72374=CARTESIAN_POINT('Ctrl Pts',(82.017060840712,-9.398155252254,131.082294571138));
#72375=CARTESIAN_POINT('Ctrl Pts',(82.002037251814,-9.46789704563033,131.078435784667));
#72376=CARTESIAN_POINT('Ctrl Pts',(81.9834138929834,-9.53671863356917,131.074576998197));
#72377=CARTESIAN_POINT('Ctrl Pts',(81.9648022655031,-9.60549686895472,131.070720642479));
#72378=CARTESIAN_POINT('Ctrl Pts',(81.9425954935463,-9.67335558113362,131.066864286761));
#72379=CARTESIAN_POINT('Ctrl Pts',(81.9169115671826,-9.73989702398478,131.063007931043));
#72380=CARTESIAN_POINT('Ctrl Pts',(81.8912352281081,-9.80641880982698,131.059152714531));
#72381=CARTESIAN_POINT('Ctrl Pts',(81.8620839487075,-9.87162364593301,131.05529749802));
#72382=CARTESIAN_POINT('Ctrl Pts',(81.8296247232369,-9.93513150659159,131.051442281508));
#72383=CARTESIAN_POINT('Ctrl Pts',(81.7971642287085,-9.99864185021608,131.047586914269));
#72384=CARTESIAN_POINT('Ctrl Pts',(81.7613957543859,-10.0604546551141,131.043731547029));
#72385=CARTESIAN_POINT('Ctrl Pts',(81.7225325466069,-10.1202139029578,131.03987617979));
#72386=CARTESIAN_POINT('Ctrl Pts',(81.683628659651,-10.1800357024321,131.036016777033));
#72387=CARTESIAN_POINT('Ctrl Pts',(81.6416238381699,-10.2377992458656,131.032157374276));
#72388=CARTESIAN_POINT('Ctrl Pts',(81.5967745355417,-10.2931777314606,131.02829797152));
#72389=CARTESIAN_POINT('Ctrl Pts',(81.5518998388882,-10.3485875727865,131.024436383539));
#72390=CARTESIAN_POINT('Ctrl Pts',(81.5041777800796,-10.4016093067255,131.020574795558));
#72391=CARTESIAN_POINT('Ctrl Pts',(81.4539031289799,-10.4519515329522,131.016713207577));
#72392=CARTESIAN_POINT('Ctrl Pts',(81.403540520585,-10.5023818346994,131.01284486361));
#72393=CARTESIAN_POINT('Ctrl Pts',(81.3506167645223,-10.5501229437333,131.008976519643));
#72394=CARTESIAN_POINT('Ctrl Pts',(81.2954607381983,-10.5949228941509,131.005108175676));
#72395=CARTESIAN_POINT('Ctrl Pts',(81.2627106817069,-10.6215238116711,131.002811264679));
#72396=CARTESIAN_POINT('Ctrl Pts',(81.2291741999367,-10.6470885862042,131.000514353681));
#72397=CARTESIAN_POINT('Ctrl Pts',(81.1949246752987,-10.6715718898277,130.998217442684));
#72398=CARTESIAN_POINT('Ctrl Pts',(81.1372323025235,-10.712813334617,130.994348359918));
#72399=CARTESIAN_POINT('Ctrl Pts',(81.0772893247062,-10.7511452709508,130.990479277153));
#72400=CARTESIAN_POINT('Ctrl Pts',(81.0154212654763,-10.7863138627124,130.986610194388));
#72401=CARTESIAN_POINT('Ctrl Pts',(80.9536453865701,-10.8214300550256,130.982746876363));
#72402=CARTESIAN_POINT('Ctrl Pts',(80.8899505385777,-10.8533920202796,130.978883558338));
#72403=CARTESIAN_POINT('Ctrl Pts',(80.8246923557848,-10.8819883317412,130.975020240313));
#72404=CARTESIAN_POINT('Ctrl Pts',(80.7595107208086,-10.9105510997434,130.971161453958));
#72405=CARTESIAN_POINT('Ctrl Pts',(80.6927698363414,-10.9357558618127,130.967302667603));
#72406=CARTESIAN_POINT('Ctrl Pts',(80.6248496025533,-10.9574372369731,130.963443881248));
#72407=CARTESIAN_POINT('Ctrl Pts',(80.5569721535271,-10.9791049544587,130.959587525646));
#72408=CARTESIAN_POINT('Ctrl Pts',(80.4879172907714,-10.9972535410618,130.955731170043));
#72409=CARTESIAN_POINT('Ctrl Pts',(80.4180831694305,-11.011766394475,130.951874814441));
#72410=CARTESIAN_POINT('Ctrl Pts',(80.3482696777804,-11.0262749606476,130.948019598044));
#72411=CARTESIAN_POINT('Ctrl Pts',(80.2776778599192,-11.0371498270919,130.944164381647));
#72412=CARTESIAN_POINT('Ctrl Pts',(80.2067175623955,-11.0443251727397,130.94030916525));
#72413=CARTESIAN_POINT('Ctrl Pts',(80.1357544905257,-11.0515007989232,130.936453798125));
#72414=CARTESIAN_POINT('Ctrl Pts',(80.0644233939313,-11.0549765704646,130.932598431));
#72415=CARTESIAN_POINT('Ctrl Pts',(79.9931390359827,-11.0547385453319,130.928743063875));
#72416=CARTESIAN_POINT('Ctrl Pts',(79.9217800627219,-11.0545002710517,130.92488366123));
#72417=CARTESIAN_POINT('Ctrl Pts',(79.850468412543,-11.0505404417333,130.921024258585));
#72418=CARTESIAN_POINT('Ctrl Pts',(79.7796177376916,-11.0428972614793,130.917164855941));
#72419=CARTESIAN_POINT('Ctrl Pts',(79.7087269466182,-11.0352497535952,130.913303268072));
#72420=CARTESIAN_POINT('Ctrl Pts',(79.6382981302969,-11.0239148203288,130.909441680202));
#72421=CARTESIAN_POINT('Ctrl Pts',(79.568735981132,-11.0089820577919,130.905580092333));
#72422=CARTESIAN_POINT('Ctrl Pts',(79.4990521304568,-10.9940231698437,130.901711748475));
#72423=CARTESIAN_POINT('Ctrl Pts',(79.4302384433608,-10.9754540120118,130.897843404617));
#72424=CARTESIAN_POINT('Ctrl Pts',(79.3626849813448,-10.9534142237366,130.893975060759));
#72425=CARTESIAN_POINT('Ctrl Pts',(79.322573666333,-10.940327627374,130.891678148737));
#72426=CARTESIAN_POINT('Ctrl Pts',(79.282906308109,-10.9260183444643,130.889381236715));
#72427=CARTESIAN_POINT('Ctrl Pts',(79.2437607894409,-10.9105234410791,130.887084324692));
#72428=CARTESIAN_POINT('Ctrl Pts',(79.1778212781382,-10.8844227176334,130.883215241808));
#72429=CARTESIAN_POINT('Ctrl Pts',(79.1131054573431,-10.8548531261454,130.879346158925));
#72430=CARTESIAN_POINT('Ctrl Pts',(79.0500031407997,-10.8219504740826,130.875477076041));
#72431=CARTESIAN_POINT('Ctrl Pts',(78.9869948435725,-10.7890968453364,130.871613757898));
#72432=CARTESIAN_POINT('Ctrl Pts',(78.9255957058774,-10.7529202363441,130.867750439756));
#72433=CARTESIAN_POINT('Ctrl Pts',(78.8661762433591,-10.7136047535464,130.863887121613));
#72434=CARTESIAN_POINT('Ctrl Pts',(78.8068264798667,-10.6743353878076,130.860028335142));
#72435=CARTESIAN_POINT('Ctrl Pts',(78.7494521821209,-10.6319347285184,130.856169548672));
#72436=CARTESIAN_POINT('Ctrl Pts',(78.6943983425402,-10.5866322430035,130.852310762201));
#72437=CARTESIAN_POINT('Ctrl Pts',(78.6393791828529,-10.5413582947419,130.848454406484));
#72438=CARTESIAN_POINT('Ctrl Pts',(78.5866779555273,-10.493186454796,130.844598050766));
#72439=CARTESIAN_POINT('Ctrl Pts',(78.5366085735479,-10.4423879836876,130.840741695049));
#72440=CARTESIAN_POINT('Ctrl Pts',(78.4865539825763,-10.3916045189674,130.836886478539));
#72441=CARTESIAN_POINT('Ctrl Pts',(78.4391300342721,-10.3381963093146,130.833031262028));
#72442=CARTESIAN_POINT('Ctrl Pts',(78.3946143198086,-10.2824719803318,130.829176045518));
#72443=CARTESIAN_POINT('Ctrl Pts',(78.3500968649242,-10.2267454727075,130.825320678281));
#72444=CARTESIAN_POINT('Ctrl Pts',(78.3084881711024,-10.1687030468921,130.821465311044));
#72445=CARTESIAN_POINT('Ctrl Pts',(78.2700249110102,-10.1086855974418,130.817609943807));
#72446=CARTESIAN_POINT('Ctrl Pts',(78.2315213903893,-10.048605326113,130.813750541054));
#72447=CARTESIAN_POINT('Ctrl Pts',(78.1961701385383,-9.98654631417253,130.8098911383));
#72448=CARTESIAN_POINT('Ctrl Pts',(78.1641634157798,-9.92287680572152,130.806031735547));
#72449=CARTESIAN_POINT('Ctrl Pts',(78.1321385705706,-9.85917124710896,130.80217014757));
#72450=CARTESIAN_POINT('Ctrl Pts',(78.103462219597,-9.7938538217371,130.798308559593));
#72451=CARTESIAN_POINT('Ctrl Pts',(78.0782785874139,-9.72731312026404,130.794446971617));
#72452=CARTESIAN_POINT('Ctrl Pts',(78.0530508955748,-9.66065600347805,130.790578627655));
#72453=CARTESIAN_POINT('Ctrl Pts',(78.0313282706817,-9.59277180050978,130.786710283693));
#72454=CARTESIAN_POINT('Ctrl Pts',(78.0132049587201,-9.52406395262953,130.782841939732));
#72455=CARTESIAN_POINT('Ctrl Pts',(78.0024438590867,-9.48326721535527,130.780545028721));
#72456=CARTESIAN_POINT('Ctrl Pts',(77.9929507711792,-9.44218030000125,130.778248117711));
#72457=CARTESIAN_POINT('Ctrl Pts',(77.9847367966347,-9.40088874224893,130.775951206701));
#72458=CARTESIAN_POINT('Ctrl Pts',(77.9647646110824,-9.3004887898615,130.77036629374));
#72459=CARTESIAN_POINT('Ctrl Pts',(77.9522903129557,-9.19855146660896,130.764781380779));
#72460=CARTESIAN_POINT('Ctrl Pts',(77.9474937711085,-9.09599866072768,130.759196467817));
#72461=CARTESIAN_POINT('Ctrl Pts',(77.9460275184567,-9.06464934108068,130.757489218366));
#72462=CARTESIAN_POINT('Ctrl Pts',(77.945278419186,-9.03324269326322,130.755781968914));
#72463=CARTESIAN_POINT('Ctrl Pts',(77.9452507933694,-9.00180564418067,130.754074719462));
#72464=CARTESIAN_POINT('Origin',(80.,-9.,141.545925280538));
#72465=CARTESIAN_POINT('',(81.2520391107129,-7.3707683934611,131.906140964161));
#72466=CARTESIAN_POINT('',(81.2520391107129,-7.37076839346113,131.847886939579));
#72467=CARTESIAN_POINT('',(81.2520391107129,-7.37076839346111,141.545925280538));
#72468=CARTESIAN_POINT('',(77.9452501035681,-9.00065239039587,131.39592528057));
#72469=CARTESIAN_POINT('Ctrl Pts',(81.2520391107129,-7.37076839346113,131.847886939579));
#72470=CARTESIAN_POINT('Ctrl Pts',(81.3085634825606,-7.41420649273306,131.844031409821));
#72471=CARTESIAN_POINT('Ctrl Pts',(81.3628520478468,-7.46061066578053,131.840175880064));
#72472=CARTESIAN_POINT('Ctrl Pts',(81.4145852360442,-7.50971607655934,131.836320350307));
#72473=CARTESIAN_POINT('Ctrl Pts',(81.4663133131985,-7.55881663590943,131.832465201462));
#72474=CARTESIAN_POINT('Ctrl Pts',(81.5154861631145,-7.6106175677554,131.828610052616));
#72475=CARTESIAN_POINT('Ctrl Pts',(81.5618198988355,-7.66481605533116,131.824754903771));
#72476=CARTESIAN_POINT('Ctrl Pts',(81.6083190592735,-7.71920804704219,131.820885990939));
#72477=CARTESIAN_POINT('Ctrl Pts',(81.6519584670128,-7.77601437920203,131.817017078107));
#72478=CARTESIAN_POINT('Ctrl Pts',(81.6924922190995,-7.83489586268532,131.813148165275));
#72479=CARTESIAN_POINT('Ctrl Pts',(81.7329383906802,-7.89365012206901,131.80928761193));
#72480=CARTESIAN_POINT('Ctrl Pts',(81.7702920867994,-7.95447014009036,131.805427058584));
#72481=CARTESIAN_POINT('Ctrl Pts',(81.8043538921319,-8.01699206796262,131.801566505239));
#72482=CARTESIAN_POINT('Ctrl Pts',(81.8385263315502,-8.07971706951997,131.797693412664));
#72483=CARTESIAN_POINT('Ctrl Pts',(81.8693852591814,-8.14415460682124,131.793820320089));
#72484=CARTESIAN_POINT('Ctrl Pts',(81.8967778292422,-8.2099168214706,131.789947227514));
#72485=CARTESIAN_POINT('Ctrl Pts',(81.9241703993031,-8.27567903611997,131.786074134939));
#72486=CARTESIAN_POINT('Ctrl Pts',(81.9480965076543,-8.3427654484236,131.782201042364));
#72487=CARTESIAN_POINT('Ctrl Pts',(81.9684540117226,-8.41077477461233,131.778327949789));
#72488=CARTESIAN_POINT('Ctrl Pts',(81.9887904401113,-8.47871369222997,131.774458866942));
#72489=CARTESIAN_POINT('Ctrl Pts',(82.0056453207931,-8.54783974469615,131.770589784096));
#72490=CARTESIAN_POINT('Ctrl Pts',(82.0188839110767,-8.61776274894318,131.766720701249));
#72491=CARTESIAN_POINT('Ctrl Pts',(82.0321027765211,-8.68758157140082,131.762857383143));
#72492=CARTESIAN_POINT('Ctrl Pts',(82.0417159571494,-8.75819451523129,131.758994065037));
#72493=CARTESIAN_POINT('Ctrl Pts',(82.0476385852171,-8.82919664280217,131.75513074693));
#72494=CARTESIAN_POINT('Ctrl Pts',(82.0535542660443,-8.90011548490451,131.751271960495));
#72495=CARTESIAN_POINT('Ctrl Pts',(82.0557879530187,-8.97142212220669,131.747413174059));
#72496=CARTESIAN_POINT('Ctrl Pts',(82.0543062010365,-9.04270356991117,131.743554387624));
#72497=CARTESIAN_POINT('Ctrl Pts',(82.0528253824494,-9.11394011553025,131.739698031941));
#72498=CARTESIAN_POINT('Ctrl Pts',(82.0476337784022,-9.18515101850258,131.735841676258));
#72499=CARTESIAN_POINT('Ctrl Pts',(82.0387500055478,-9.25592181888014,131.731985320575));
#72500=CARTESIAN_POINT('Ctrl Pts',(82.0298688570489,-9.32667171285441,131.728130104098));
#72501=CARTESIAN_POINT('Ctrl Pts',(82.0172977655642,-9.39698128060341,131.724274887621));
#72502=CARTESIAN_POINT('Ctrl Pts',(82.001107178664,-9.46644144541354,131.720419671144));
#72503=CARTESIAN_POINT('Ctrl Pts',(81.9849159587603,-9.53590432590819,131.71656430394));
#72504=CARTESIAN_POINT('Ctrl Pts',(81.9651050749101,-9.60451726493085,131.712708936735));
#72505=CARTESIAN_POINT('Ctrl Pts',(81.941795650409,-9.67188333403389,131.708853569531));
#72506=CARTESIAN_POINT('Ctrl Pts',(81.9184618272967,-9.73931991704135,131.704994166809));
#72507=CARTESIAN_POINT('Ctrl Pts',(81.8916223124967,-9.80550656477264,131.701134764086));
#72508=CARTESIAN_POINT('Ctrl Pts',(81.8614472056882,-9.8700642866682,131.697275361364));
#72509=CARTESIAN_POINT('Ctrl Pts',(81.8312550134973,-9.93465856165302,131.693413773417));
#72510=CARTESIAN_POINT('Ctrl Pts',(81.7977236980533,-9.99762164579254,131.68955218547));
#72511=CARTESIAN_POINT('Ctrl Pts',(81.7610690802575,-10.0585996679864,131.685690597524));
#72512=CARTESIAN_POINT('Ctrl Pts',(81.7243503338942,-10.1196843734156,131.68182225359));
#72513=CARTESIAN_POINT('Ctrl Pts',(81.684497647197,-10.1787766802047,131.677953909657));
#72514=CARTESIAN_POINT('Ctrl Pts',(81.6417694498063,-10.2355527654384,131.674085565724));
#72515=CARTESIAN_POINT('Ctrl Pts',(81.6163986757783,-10.2692647710139,131.671788654415));
#72516=CARTESIAN_POINT('Ctrl Pts',(81.5900148690266,-10.3021607970392,131.669491743107));
#72517=CARTESIAN_POINT('Ctrl Pts',(81.5626783192385,-10.3341791607884,131.667194831798));
#72518=CARTESIAN_POINT('Ctrl Pts',(81.516630665768,-10.3881131989183,131.663325748947));
#72519=CARTESIAN_POINT('Ctrl Pts',(81.4676973380779,-10.4397661522298,131.659456666095));
#72520=CARTESIAN_POINT('Ctrl Pts',(81.4161330600869,-10.4888131913134,131.655587583244));
#72521=CARTESIAN_POINT('Ctrl Pts',(81.3646456102982,-10.5377871527552,131.651724265133));
#72522=CARTESIAN_POINT('Ctrl Pts',(81.310535340387,-10.5841625749118,131.647860947022));
#72523=CARTESIAN_POINT('Ctrl Pts',(81.254096421259,-10.6276485273809,131.643997628911));
#72524=CARTESIAN_POINT('Ctrl Pts',(81.1977237049614,-10.6710834708446,131.640138842471));
#72525=CARTESIAN_POINT('Ctrl Pts',(81.1390281480807,-10.711635381957,131.636280056031));
#72526=CARTESIAN_POINT('Ctrl Pts',(81.0783385728406,-10.7490521675536,131.632421269591));
#72527=CARTESIAN_POINT('Ctrl Pts',(81.0176872275828,-10.786445383319,131.628564913903));
#72528=CARTESIAN_POINT('Ctrl Pts',(80.9550447685521,-10.8207071373998,131.624708558215));
#72529=CARTESIAN_POINT('Ctrl Pts',(80.8907694945673,-10.8516282753426,131.620852202528));
#72530=CARTESIAN_POINT('Ctrl Pts',(80.8265132081422,-10.8825402788716,131.616996986046));
#72531=CARTESIAN_POINT('Ctrl Pts',(80.760625501884,-10.9101134149559,131.613141769564));
#72532=CARTESIAN_POINT('Ctrl Pts',(80.6934882640478,-10.9341849937707,131.609286553083));
#72533=CARTESIAN_POINT('Ctrl Pts',(80.6263484013468,-10.9582575137122,131.605431185874));
#72534=CARTESIAN_POINT('Ctrl Pts',(80.5579593680992,-10.9788280427057,131.601575818665));
#72535=CARTESIAN_POINT('Ctrl Pts',(80.4887203319164,-10.99578305426,131.597720451456));
#72536=CARTESIAN_POINT('Ctrl Pts',(80.4194088213442,-11.0127558130878,131.593861048728));
#72537=CARTESIAN_POINT('Ctrl Pts',(80.3492460045624,-11.0261053840647,131.590001646001));
#72538=CARTESIAN_POINT('Ctrl Pts',(80.2786425427956,-11.0357691165366,131.586142243274));
#72539=CARTESIAN_POINT('Ctrl Pts',(80.2079991047945,-11.0454383206898,131.582280655323));
#72540=CARTESIAN_POINT('Ctrl Pts',(80.1369150094404,-11.0514174911261,131.578419067372));
#72541=CARTESIAN_POINT('Ctrl Pts',(80.0658046125601,-11.0536960134026,131.57455747942));
#72542=CARTESIAN_POINT('Ctrl Pts',(79.9945698054933,-11.0559785220355,131.570689135483));
#72543=CARTESIAN_POINT('Ctrl Pts',(79.9233090908679,-11.0545474659095,131.566820791545));
#72544=CARTESIAN_POINT('Ctrl Pts',(79.8524346901784,-11.0494443251372,131.562952447607));
#72545=CARTESIAN_POINT('Ctrl Pts',(79.810351511404,-11.0464142270575,131.56065553634));
#72546=CARTESIAN_POINT('Ctrl Pts',(79.7684044150229,-11.0420904754752,131.558358625073));
#72547=CARTESIAN_POINT('Ctrl Pts',(79.7266779226688,-11.036490266253,131.556061713806));
#72548=CARTESIAN_POINT('Ctrl Pts',(79.6563908124203,-11.0270568703262,131.552192630968));
#72549=CARTESIAN_POINT('Ctrl Pts',(79.5864549840659,-11.0139619085453,131.54832354813));
#72550=CARTESIAN_POINT('Ctrl Pts',(79.5172814947751,-10.9972432018193,131.544454465292));
#72551=CARTESIAN_POINT('Ctrl Pts',(79.4482110705339,-10.9805494051327,131.540591147194));
#72552=CARTESIAN_POINT('Ctrl Pts',(79.3799011990718,-10.9602426939566,131.536727829097));
#72553=CARTESIAN_POINT('Ctrl Pts',(79.3127558531514,-10.9364124160732,131.532864510999));
#72554=CARTESIAN_POINT('Ctrl Pts',(79.2456892686947,-10.9126100910961,131.529005724572));
#72555=CARTESIAN_POINT('Ctrl Pts',(79.179784952049,-10.8852925709212,131.525146938145));
#72556=CARTESIAN_POINT('Ctrl Pts',(79.1154330417219,-10.8545993796027,131.521288151718));
#72557=CARTESIAN_POINT('Ctrl Pts',(79.0511216683789,-10.8239255227437,131.517431796044));
#72558=CARTESIAN_POINT('Ctrl Pts',(78.9883611986391,-10.78988042217,131.513575440369));
#72559=CARTESIAN_POINT('Ctrl Pts',(78.9275216843035,-10.75265165531,131.509719084695));
#72560=CARTESIAN_POINT('Ctrl Pts',(78.8667001425688,-10.7154338861999,131.505863868226));
#72561=CARTESIAN_POINT('Ctrl Pts',(78.8077988437895,-10.6750345713477,131.502008651758));
#72562=CARTESIAN_POINT('Ctrl Pts',(78.7511615977412,-10.6316863079476,131.498153435289));
#72563=CARTESIAN_POINT('Ctrl Pts',(78.6945221373449,-10.5883363497592,131.494298068093));
#72564=CARTESIAN_POINT('Ctrl Pts',(78.6401472898436,-10.5420375111187,131.490442700897));
#72565=CARTESIAN_POINT('Ctrl Pts',(78.588348933253,-10.4930635714034,131.486587333701));
#72566=CARTESIAN_POINT('Ctrl Pts',(78.5364963579054,-10.4440383693257,131.482727930987));
#72567=CARTESIAN_POINT('Ctrl Pts',(78.487226010765,-10.3923328109689,131.478868528272));
#72568=CARTESIAN_POINT('Ctrl Pts',(78.4408132612832,-10.3382579259282,131.475009125558));
#72569=CARTESIAN_POINT('Ctrl Pts',(78.3943742325369,-10.2841524232615,131.471147537619));
#72570=CARTESIAN_POINT('Ctrl Pts',(78.3507963192775,-10.2276753081196,131.467285949681));
#72571=CARTESIAN_POINT('Ctrl Pts',(78.310313177494,-10.169168937472,131.463424361742));
#72572=CARTESIAN_POINT('Ctrl Pts',(78.2697592090004,-10.1105602078285,131.459556017817));
#72573=CARTESIAN_POINT('Ctrl Pts',(78.2323110773254,-10.0499155479552,131.455687673892));
#72574=CARTESIAN_POINT('Ctrl Pts',(78.1981575144787,-9.98760377675981,131.451819329966));
#72575=CARTESIAN_POINT('Ctrl Pts',(78.1778781109871,-9.95060483887392,131.449522418582));
#72576=CARTESIAN_POINT('Ctrl Pts',(78.1587593571235,-9.91301857604652,131.447225507198));
#72577=CARTESIAN_POINT('Ctrl Pts',(78.1408326489501,-9.87492532440782,131.444928595814));
#72578=CARTESIAN_POINT('Ctrl Pts',(78.1081554784628,-9.80548816582994,131.440741738743));
#72579=CARTESIAN_POINT('Ctrl Pts',(78.0793295383054,-9.73412774208689,131.436554881671));
#72580=CARTESIAN_POINT('Ctrl Pts',(78.0545656017943,-9.66127344176059,131.432368024599));
#72581=CARTESIAN_POINT('Ctrl Pts',(78.0298638437661,-9.58860206751596,131.42819168009));
#72582=CARTESIAN_POINT('Ctrl Pts',(78.0092039024853,-9.51444461665576,131.42401533558));
#72583=CARTESIAN_POINT('Ctrl Pts',(77.9927491649568,-9.43925123530684,131.41983899107));
#72584=CARTESIAN_POINT('Ctrl Pts',(77.9763607882809,-9.36436110382013,131.415679489478));
#72585=CARTESIAN_POINT('Ctrl Pts',(77.964143907639,-9.28844370983482,131.411519987886));
#72586=CARTESIAN_POINT('Ctrl Pts',(77.9562120164592,-9.21196282889739,131.407360486294));
#72587=CARTESIAN_POINT('Ctrl Pts',(77.948943292438,-9.14187633832032,131.403548751052));
#72588=CARTESIAN_POINT('Ctrl Pts',(77.9452725398498,-9.07131705349499,131.399737015811));
#72589=CARTESIAN_POINT('Ctrl Pts',(77.9452501035681,-9.00065239039586,131.39592528057));
#72590=CARTESIAN_POINT('Ctrl Pts',(77.9452501035679,-9.00065238980674,131.395925280538));
#72591=CARTESIAN_POINT('Ctrl Pts',(77.9452268384226,-8.92737709575494,131.391972724785));
#72592=CARTESIAN_POINT('Ctrl Pts',(77.9491275646018,-8.85413490590009,131.388020169032));
#72593=CARTESIAN_POINT('Ctrl Pts',(77.9569155176319,-8.78136020397297,131.384067613279));
#72594=CARTESIAN_POINT('Ctrl Pts',(77.9647095603039,-8.70852859725101,131.3801119669));
#72595=CARTESIAN_POINT('Ctrl Pts',(77.9763968270617,-8.63616565292411,131.376156320522));
#72596=CARTESIAN_POINT('Ctrl Pts',(77.9918890690412,-8.56469774700355,131.372200674143));
#72597=CARTESIAN_POINT('Ctrl Pts',(78.0074099266821,-8.49309783298509,131.368237721305));
#72598=CARTESIAN_POINT('Ctrl Pts',(78.0267496922354,-8.42239669799367,131.364274768467));
#72599=CARTESIAN_POINT('Ctrl Pts',(78.0497697059512,-8.35300744774416,131.360311815629));
#72600=CARTESIAN_POINT('Ctrl Pts',(78.0728143784025,-8.28354386864407,131.356344617728));
#72601=CARTESIAN_POINT('Ctrl Pts',(78.0995469862571,-8.21539539157083,131.352377419827));
#72602=CARTESIAN_POINT('Ctrl Pts',(78.1297809942058,-8.14895450599507,131.348410221926));
#72603=CARTESIAN_POINT('Ctrl Pts',(78.160077328868,-8.08237665405856,131.344434845737));
#72604=CARTESIAN_POINT('Ctrl Pts',(78.1938892656029,-8.01751381958153,131.340459469549));
#72605=CARTESIAN_POINT('Ctrl Pts',(78.2309848912298,-7.95473299705641,131.336484093361));
#72606=CARTESIAN_POINT('Ctrl Pts',(78.2393476952122,-7.94057974572926,131.335587888181));
#72607=CARTESIAN_POINT('Ctrl Pts',(78.2478772169343,-7.92653218314774,131.334691683002));
#72608=CARTESIAN_POINT('Ctrl Pts',(78.2565705111978,-7.9125942891106,131.333795477822));
#72609=CARTESIAN_POINT('Ctrl Pts',(78.2941010642335,-7.85242183255806,131.329926394941));
#72610=CARTESIAN_POINT('Ctrl Pts',(78.3348239566215,-7.79407678770886,131.32605731206));
#72611=CARTESIAN_POINT('Ctrl Pts',(78.3785355099981,-7.73791819989232,131.322188229179));
#72612=CARTESIAN_POINT('Ctrl Pts',(78.4221819353426,-7.68184328556781,131.318324911038));
#72613=CARTESIAN_POINT('Ctrl Pts',(78.4688078867317,-7.62794874203111,131.314461592897));
#72614=CARTESIAN_POINT('Ctrl Pts',(78.518165643408,-7.57656594739218,131.310598274756));
#72615=CARTESIAN_POINT('Ctrl Pts',(78.5674655034558,-7.52524342475045,131.306739488286));
#72616=CARTESIAN_POINT('Ctrl Pts',(78.61949046886,-7.47642714733036,131.302880701815));
#72617=CARTESIAN_POINT('Ctrl Pts',(78.6739527858865,-7.43041523056516,131.299021915345));
#72618=CARTESIAN_POINT('Ctrl Pts',(78.7283807956474,-7.38443229793316,131.295165559627));
#72619=CARTESIAN_POINT('Ctrl Pts',(78.7852427407113,-7.34125053392767,131.291309203909));
#72620=CARTESIAN_POINT('Ctrl Pts',(78.8442153428599,-7.30112996706057,131.287452848192));
#72621=CARTESIAN_POINT('Ctrl Pts',(78.903170523911,-7.26102125221097,131.28359763168));
#72622=CARTESIAN_POINT('Ctrl Pts',(78.9642347227805,-7.22397221229798,131.279742415168));
#72623=CARTESIAN_POINT('Ctrl Pts',(79.0270544352444,-7.19020042807984,131.275887198657));
#72624=CARTESIAN_POINT('Ctrl Pts',(79.0898766037698,-7.1564273234867,131.272031831417));
#72625=CARTESIAN_POINT('Ctrl Pts',(79.1544539932407,-7.12593195705841,131.268176464178));
#72626=CARTESIAN_POINT('Ctrl Pts',(79.2204087129456,-7.09888585622828,131.264321096939));
#72627=CARTESIAN_POINT('Ctrl Pts',(79.2864324692501,-7.07181144550855,131.260461694183));
#72628=CARTESIAN_POINT('Ctrl Pts',(79.3538359833414,-7.04819369232281,131.256602291426));
#72629=CARTESIAN_POINT('Ctrl Pts',(79.4222224454191,-7.02815551832237,131.252742888669));
#72630=CARTESIAN_POINT('Ctrl Pts',(79.4906476284457,-7.00810599855131,131.248881300688));
#72631=CARTESIAN_POINT('Ctrl Pts',(79.5600563944949,-6.99164020485382,131.245019712707));
#72632=CARTESIAN_POINT('Ctrl Pts',(79.6300405550026,-6.97883014777154,131.241158124726));
#72633=CARTESIAN_POINT('Ctrl Pts',(79.7001471552952,-6.96599767903749,131.23728978076));
#72634=CARTESIAN_POINT('Ctrl Pts',(79.770830677994,-6.95683377887449,131.233421436793));
#72635=CARTESIAN_POINT('Ctrl Pts',(79.8416773114535,-6.95135862367485,131.229553092826));
#72636=CARTESIAN_POINT('Ctrl Pts',(79.8837439976099,-6.9481076345425,131.227256181828));
#72637=CARTESIAN_POINT('Ctrl Pts',(79.9258681602479,-6.94615616588539,131.224959270829));
#72638=CARTESIAN_POINT('Ctrl Pts',(79.9679636615179,-6.94549976015658,131.222662359831));
#72639=CARTESIAN_POINT('Ctrl Pts',(80.0388583887718,-6.94439428086052,131.21879403961));
#72640=CARTESIAN_POINT('Ctrl Pts',(80.1099492315829,-6.9469604939641,131.21492571939));
#72641=CARTESIAN_POINT('Ctrl Pts',(80.1808243171314,-6.95322201281283,131.211057399169));
#72642=CARTESIAN_POINT('Ctrl Pts',(80.2516008675007,-6.95947482648855,131.20719445694));
#72643=CARTESIAN_POINT('Ctrl Pts',(80.3221617761498,-6.96941271114748,131.203331514712));
#72644=CARTESIAN_POINT('Ctrl Pts',(80.3920944026438,-6.98300730246355,131.199468572483));
#72645=CARTESIAN_POINT('Ctrl Pts',(80.4619532083238,-6.99658754334194,131.195609707972));
#72646=CARTESIAN_POINT('Ctrl Pts',(80.5311845737719,-7.01381673726949,131.191750843462));
#72647=CARTESIAN_POINT('Ctrl Pts',(80.5993819433181,-7.03461483456188,131.187891978951));
#72648=CARTESIAN_POINT('Ctrl Pts',(80.6675362532688,-7.05539980000383,131.184035550915));
#72649=CARTESIAN_POINT('Ctrl Pts',(80.734657399007,-7.07974905664672,131.180179122878));
#72650=CARTESIAN_POINT('Ctrl Pts',(80.800351555953,-7.10753204799037,131.176322694842));
#72651=CARTESIAN_POINT('Ctrl Pts',(80.8660214074106,-7.13530476019795,131.172467693605));
#72652=CARTESIAN_POINT('Ctrl Pts',(80.9302648728479,-7.16650849170464,131.168612692368));
#72653=CARTESIAN_POINT('Ctrl Pts',(80.9927074781101,-7.2009643068009,131.164757691131));
#72654=CARTESIAN_POINT('Ctrl Pts',(81.0551657820356,-7.23542878441596,131.16090172071));
#72655=CARTESIAN_POINT('Ctrl Pts',(81.1158218958355,-7.27314674404535,131.157045750289));
#72656=CARTESIAN_POINT('Ctrl Pts',(81.1743265826277,-7.31389364515938,131.153189779868));
#72657=CARTESIAN_POINT('Ctrl Pts',(81.2006767631621,-7.33224581930889,131.151453072566));
#72658=CARTESIAN_POINT('Ctrl Pts',(81.2265908984792,-7.3512118387721,131.149716365264));
#72659=CARTESIAN_POINT('Ctrl Pts',(81.2520391107129,-7.3707683934611,131.147979657963));
#72660=CARTESIAN_POINT('',(77.9452503396332,-8.99881859296011,131.454074719514));
#72661=CARTESIAN_POINT('Ctrl Pts',(77.9452503396338,-8.99881859201236,131.454074719462));
#72662=CARTESIAN_POINT('Ctrl Pts',(77.9452901831621,-8.92952121357853,131.450299784525));
#72663=CARTESIAN_POINT('Ctrl Pts',(77.9488353855607,-8.86032618901156,131.446524849588));
#72664=CARTESIAN_POINT('Ctrl Pts',(77.955856695627,-8.7914916939617,131.44274991465));
#72665=CARTESIAN_POINT('Ctrl Pts',(77.9630531190942,-8.72094044770435,131.438880831799));
#72666=CARTESIAN_POINT('Ctrl Pts',(77.9739204176304,-8.65062402026964,131.435011748947));
#72667=CARTESIAN_POINT('Ctrl Pts',(77.9884338439667,-8.58095446261622,131.431142666096));
#72668=CARTESIAN_POINT('Ctrl Pts',(78.0029256460216,-8.5113887091287,131.427279347985));
#72669=CARTESIAN_POINT('Ctrl Pts',(78.0210526941546,-8.44246838399812,131.423416029874));
#72670=CARTESIAN_POINT('Ctrl Pts',(78.0427385152252,-8.37460009376617,131.419552711764));
#72671=CARTESIAN_POINT('Ctrl Pts',(78.0643988988361,-8.30681141301247,131.415693925323));
#72672=CARTESIAN_POINT('Ctrl Pts',(78.0896096163957,-8.24007277643222,131.411835138883));
#72673=CARTESIAN_POINT('Ctrl Pts',(78.1182436044466,-8.1747785568141,131.407976352443));
#72674=CARTESIAN_POINT('Ctrl Pts',(78.1468595551847,-8.1095254677665,131.404119996755));
#72675=CARTESIAN_POINT('Ctrl Pts',(78.1788943034942,-8.04571543433216,131.400263641067));
#72676=CARTESIAN_POINT('Ctrl Pts',(78.2141721188595,-7.98372427882916,131.39640728538));
#72677=CARTESIAN_POINT('Ctrl Pts',(78.2494395128048,-7.92175143613432,131.392552068898));
#72678=CARTESIAN_POINT('Ctrl Pts',(78.2879478317048,-7.86159682662655,131.388696852416));
#72679=CARTESIAN_POINT('Ctrl Pts',(78.3294755145793,-7.80361147359645,131.384841635935));
#72680=CARTESIAN_POINT('Ctrl Pts',(78.3710048210619,-7.74562385351272,131.380986268726));
#72681=CARTESIAN_POINT('Ctrl Pts',(78.4155534412473,-7.68980605195061,131.377130901517));
#72682=CARTESIAN_POINT('Ctrl Pts',(78.4628576386407,-7.63647848443282,131.373275534308));
#72683=CARTESIAN_POINT('Ctrl Pts',(78.5102113506287,-7.58309509749437,131.36941613158));
#72684=CARTESIAN_POINT('Ctrl Pts',(78.5603260745858,-7.53220751210493,131.365556728853));
#72685=CARTESIAN_POINT('Ctrl Pts',(78.6128996831315,-7.48410083665061,131.361697326126));
#72686=CARTESIAN_POINT('Ctrl Pts',(78.6655030592671,-7.43596692281909,131.357835738175));
#72687=CARTESIAN_POINT('Ctrl Pts',(78.7205677163503,-7.39061736238294,131.353974150224));
#72688=CARTESIAN_POINT('Ctrl Pts',(78.7777588906715,-7.34829656621796,131.350112562272));
#72689=CARTESIAN_POINT('Ctrl Pts',(78.8350501230007,-7.30590172830415,131.346244218335));
#72690=CARTESIAN_POINT('Ctrl Pts',(78.8944748953435,-7.26654650244283,131.342375874397));
#72691=CARTESIAN_POINT('Ctrl Pts',(78.9556705686811,-7.23043123858347,131.338507530459));
#72692=CARTESIAN_POINT('Ctrl Pts',(78.9920067977859,-7.20898703460304,131.336210619192));
#72693=CARTESIAN_POINT('Ctrl Pts',(79.0289669160089,-7.18868424210409,131.333913707925));
#72694=CARTESIAN_POINT('Ctrl Pts',(79.0664716248486,-7.16955679266272,131.331616796658));
#72695=CARTESIAN_POINT('Ctrl Pts',(79.129647258756,-7.13733713862794,131.32774771382));
#72696=CARTESIAN_POINT('Ctrl Pts',(79.1946166239916,-7.10832886924695,131.323878630982));
#72697=CARTESIAN_POINT('Ctrl Pts',(79.2610201204866,-7.08273468185169,131.320009548144));
#72698=CARTESIAN_POINT('Ctrl Pts',(79.3273246790835,-7.05717862851921,131.316146230047));
#72699=CARTESIAN_POINT('Ctrl Pts',(79.395058677896,-7.03502673327756,131.312282911949));
#72700=CARTESIAN_POINT('Ctrl Pts',(79.4638390357952,-7.01643528389846,131.308419593851));
#72701=CARTESIAN_POINT('Ctrl Pts',(79.532538714362,-6.99786564228206,131.304560807425));
#72702=CARTESIAN_POINT('Ctrl Pts',(79.602281847348,-6.98284827692435,131.300702020998));
#72703=CARTESIAN_POINT('Ctrl Pts',(79.6726681924121,-6.9714903376515,131.296843234571));
#72704=CARTESIAN_POINT('Ctrl Pts',(79.7430101992408,-6.96013955304743,131.292986878896));
#72705=CARTESIAN_POINT('Ctrl Pts',(79.8139941358381,-6.95244369831161,131.289130523222));
#72706=CARTESIAN_POINT('Ctrl Pts',(79.8852089486723,-6.94845897505434,131.285274167547));
#72707=CARTESIAN_POINT('Ctrl Pts',(79.9564027239387,-6.94447542892417,131.281418951079));
#72708=CARTESIAN_POINT('Ctrl Pts',(80.0278267552795,-6.94420086492617,131.27756373461));
#72709=CARTESIAN_POINT('Ctrl Pts',(80.0990659661041,-6.9476395304772,131.273708518142));
#72710=CARTESIAN_POINT('Ctrl Pts',(80.17030796217,-6.95107833046982,131.269853150946));
#72711=CARTESIAN_POINT('Ctrl Pts',(80.2413646382617,-6.95823062261835,131.26599778375));
#72712=CARTESIAN_POINT('Ctrl Pts',(80.3118237572176,-6.96904862024353,131.262142416554));
#72713=CARTESIAN_POINT('Ctrl Pts',(80.3823566276609,-6.97987794136278,131.258283013839));
#72714=CARTESIAN_POINT('Ctrl Pts',(80.452290211231,-6.9943805535867,131.254423611125));
#72715=CARTESIAN_POINT('Ctrl Pts',(80.521221110999,-7.01245726688732,131.250564208411));
#72716=CARTESIAN_POINT('Ctrl Pts',(80.5901910399853,-7.0305442153654,131.246702620472));
#72717=CARTESIAN_POINT('Ctrl Pts',(80.6581566919426,-7.05220914584597,131.242841032534));
#72718=CARTESIAN_POINT('Ctrl Pts',(80.7247311599638,-7.0773033759125,131.238979444595));
#72719=CARTESIAN_POINT('Ctrl Pts',(80.7914221024071,-7.1024415092355,131.23511110067));
#72720=CARTESIAN_POINT('Ctrl Pts',(80.8567165563495,-7.13102072583423,131.231242756745));
#72721=CARTESIAN_POINT('Ctrl Pts',(80.9202495129067,-7.16284502654378,131.227374412819));
#72722=CARTESIAN_POINT('Ctrl Pts',(80.9579735555477,-7.18174138116103,131.225077501435));
#72723=CARTESIAN_POINT('Ctrl Pts',(80.9950770457654,-7.20178096490513,131.222780590051));
#72724=CARTESIAN_POINT('Ctrl Pts',(81.0314884665626,-7.22291556029309,131.220483678667));
#72725=CARTESIAN_POINT('Ctrl Pts',(81.0928208329711,-7.25851523533601,131.216614699991));
#72726=CARTESIAN_POINT('Ctrl Pts',(81.1524281864619,-7.29736350009924,131.212745721315));
#72727=CARTESIAN_POINT('Ctrl Pts',(81.2099452235106,-7.3392681978706,131.208876742639));
#72728=CARTESIAN_POINT('Ctrl Pts',(81.2241048442314,-7.34958435213222,131.20792427232));
#72729=CARTESIAN_POINT('Ctrl Pts',(81.238137884631,-7.36008551775973,131.206971802001));
#72730=CARTESIAN_POINT('Ctrl Pts',(81.2520391107129,-7.37076839346111,131.206019331682));
#72731=CARTESIAN_POINT('Ctrl Pts',(81.2520391107129,-7.3707683934611,131.906140964161));
#72732=CARTESIAN_POINT('Ctrl Pts',(81.3085547243609,-7.41419976219301,131.902272668884));
#72733=CARTESIAN_POINT('Ctrl Pts',(81.3627348190519,-7.46051906654932,131.898404373607));
#72734=CARTESIAN_POINT('Ctrl Pts',(81.4142868175889,-7.50943287299956,131.89453607833));
#72735=CARTESIAN_POINT('Ctrl Pts',(81.4465096511469,-7.54000669144819,131.892118181092));
#72736=CARTESIAN_POINT('Ctrl Pts',(81.4777064491362,-7.57159343467494,131.889700283854));
#72737=CARTESIAN_POINT('Ctrl Pts',(81.5078138187364,-7.60411495798271,131.887282386616));
#72738=CARTESIAN_POINT('Ctrl Pts',(81.5559911794038,-7.65615541115613,131.883413303769));
#72739=CARTESIAN_POINT('Ctrl Pts',(81.6015655640654,-7.71079489866968,131.879544220922));
#72740=CARTESIAN_POINT('Ctrl Pts',(81.6442441695771,-7.76774244846634,131.875675138076));
#72741=CARTESIAN_POINT('Ctrl Pts',(81.686859186095,-7.82460514925387,131.871811819969));
#72742=CARTESIAN_POINT('Ctrl Pts',(81.7265866988018,-7.88376870064298,131.867948501863));
#72743=CARTESIAN_POINT('Ctrl Pts',(81.763172185142,-7.94490691972623,131.864085183757));
#72744=CARTESIAN_POINT('Ctrl Pts',(81.7997147567208,-8.00597342370201,131.860226397321));
#72745=CARTESIAN_POINT('Ctrl Pts',(81.8331223745401,-8.06900957962136,131.856367610885));
#72746=CARTESIAN_POINT('Ctrl Pts',(81.8631831399905,-8.13365933412124,131.852508824449));
#72747=CARTESIAN_POINT('Ctrl Pts',(81.8932249693628,-8.19826836401633,131.848652468766));
#72748=CARTESIAN_POINT('Ctrl Pts',(81.9199239248084,-8.26448853642176,131.844796113083));
#72749=CARTESIAN_POINT('Ctrl Pts',(81.9431141996678,-8.33193954648609,131.8409397574));
#72750=CARTESIAN_POINT('Ctrl Pts',(81.9662976238879,-8.39937063084663,131.837084540923));
#72751=CARTESIAN_POINT('Ctrl Pts',(81.9859742674042,-8.46803137187562,131.833229324446));
#72752=CARTESIAN_POINT('Ctrl Pts',(82.0020272285703,-8.53752347241913,131.829374107968));
#72753=CARTESIAN_POINT('Ctrl Pts',(82.0180808173591,-8.6070182898959,131.825518740764));
#72754=CARTESIAN_POINT('Ctrl Pts',(82.0305103353282,-8.67734405760476,131.821663373559));
#72755=CARTESIAN_POINT('Ctrl Pts',(82.0392497279014,-8.74809106853049,131.817808006355));
#72756=CARTESIAN_POINT('Ctrl Pts',(82.0479982682355,-8.81891213228487,131.813948603632));
#72757=CARTESIAN_POINT('Ctrl Pts',(82.0530489129702,-8.89015483633853,131.810089200909));
#72758=CARTESIAN_POINT('Ctrl Pts',(82.054387478561,-8.96140401015755,131.806229798187));
#72759=CARTESIAN_POINT('Ctrl Pts',(82.0557268020581,-9.03269352581846,131.80236821024));
#72760=CARTESIAN_POINT('Ctrl Pts',(82.0533498785534,-9.10398903279388,131.798506622293));
#72761=CARTESIAN_POINT('Ctrl Pts',(82.0472946356544,-9.17487777823574,131.794645034346));
#72762=CARTESIAN_POINT('Ctrl Pts',(82.0412287988909,-9.24589054607866,131.790776690413));
#72763=CARTESIAN_POINT('Ctrl Pts',(82.0314718608921,-9.31649465020871,131.786908346479));
#72764=CARTESIAN_POINT('Ctrl Pts',(82.0181132365229,-9.38628555120693,131.783040002546));
#72765=CARTESIAN_POINT('Ctrl Pts',(82.0101812697978,-9.42772537982472,131.780743091239));
#72766=CARTESIAN_POINT('Ctrl Pts',(82.0009804488129,-9.46887873542872,131.778446179932));
#72767=CARTESIAN_POINT('Ctrl Pts',(81.9905377382803,-9.50966368811404,131.776149268625));
#72768=CARTESIAN_POINT('Ctrl Pts',(81.972947284492,-9.57836480007402,131.772280185777));
#72769=CARTESIAN_POINT('Ctrl Pts',(81.9517614930239,-9.64628873086806,131.76841110293));
#72770=CARTESIAN_POINT('Ctrl Pts',(81.9270660084628,-9.71303166937197,131.764542020082));
#72771=CARTESIAN_POINT('Ctrl Pts',(81.902407318942,-9.77967516422618,131.760678701975));
#72772=CARTESIAN_POINT('Ctrl Pts',(81.8742494834813,-9.84514070770194,131.756815383868));
#72773=CARTESIAN_POINT('Ctrl Pts',(81.8427284911057,-9.90903755179161,131.752952065761));
#72774=CARTESIAN_POINT('Ctrl Pts',(81.811244472842,-9.97285944490778,131.749093279325));
#72775=CARTESIAN_POINT('Ctrl Pts',(81.7764053476041,-10.0351158601245,131.745234492889));
#72776=CARTESIAN_POINT('Ctrl Pts',(81.7383953179643,-10.0954356580739,131.741375706452));
#72777=CARTESIAN_POINT('Ctrl Pts',(81.700409231856,-10.1557174589736,131.737519350769));
#72778=CARTESIAN_POINT('Ctrl Pts',(81.6592564626003,-10.2140646529026,131.733662995085));
#72779=CARTESIAN_POINT('Ctrl Pts',(81.6151665866136,-10.2701316703346,131.729806639401));
#72780=CARTESIAN_POINT('Ctrl Pts',(81.5710897352177,-10.3261821250083,131.725951422923));
#72781=CARTESIAN_POINT('Ctrl Pts',(81.5240777997389,-10.3799533587932,131.722096206445));
#72782=CARTESIAN_POINT('Ctrl Pts',(81.4744019976384,-10.4311311302113,131.718240989968));
#72783=CARTESIAN_POINT('Ctrl Pts',(81.4247242533627,-10.4823109025271,131.714385622762));
#72784=CARTESIAN_POINT('Ctrl Pts',(81.3723827756188,-10.5308966641232,131.710530255557));
#72785=CARTESIAN_POINT('Ctrl Pts',(81.3176859461205,-10.5766107033433,131.706674888352));
#72786=CARTESIAN_POINT('Ctrl Pts',(81.2629318639568,-10.6223725926967,131.702815485629));
#72787=CARTESIAN_POINT('Ctrl Pts',(81.2058178820311,-10.6652564470385,131.698956082905));
#72788=CARTESIAN_POINT('Ctrl Pts',(81.1466851059664,-10.7050251699769,131.695096680182));
#72789=CARTESIAN_POINT('Ctrl Pts',(81.0875188484595,-10.7448164102786,131.691235092235));
#72790=CARTESIAN_POINT('Ctrl Pts',(81.026331938212,-10.7814887581191,131.687373504287));
#72791=CARTESIAN_POINT('Ctrl Pts',(80.9634917137323,-10.814850208714,131.68351191634));
#72792=CARTESIAN_POINT('Ctrl Pts',(80.9005415480276,-10.8482700263625,131.679643572406));
#72793=CARTESIAN_POINT('Ctrl Pts',(80.8359327335556,-10.8783671766135,131.675775228472));
#72794=CARTESIAN_POINT('Ctrl Pts',(80.7700536341266,-10.904997365633,131.671906884538));
#72795=CARTESIAN_POINT('Ctrl Pts',(80.73093652081,-10.9208096054866,131.669609973236));
#72796=CARTESIAN_POINT('Ctrl Pts',(80.6913718813707,-10.9354004615867,131.667313061935));
#72797=CARTESIAN_POINT('Ctrl Pts',(80.6514431729604,-10.948748150712,131.665016150633));
#72798=CARTESIAN_POINT('Ctrl Pts',(80.5841843803941,-10.9712319597269,131.661147067787));
#72799=CARTESIAN_POINT('Ctrl Pts',(80.515628483031,-10.9902736788646,131.657277984941));
#72800=CARTESIAN_POINT('Ctrl Pts',(80.446161187892,-11.0057262417685,131.653408902095));
#72801=CARTESIAN_POINT('Ctrl Pts',(80.3767973955581,-11.0211557811243,131.64954558399));
#72802=CARTESIAN_POINT('Ctrl Pts',(80.3065253712461,-11.0330066745891,131.645682265884));
#72803=CARTESIAN_POINT('Ctrl Pts',(80.2357471530527,-11.0411812370114,131.641818947779));
#72804=CARTESIAN_POINT('Ctrl Pts',(80.1650519576818,-11.0493462106752,131.637960161344));
#72805=CARTESIAN_POINT('Ctrl Pts',(80.0938522280816,-11.053843363589,131.634101374909));
#72806=CARTESIAN_POINT('Ctrl Pts',(80.0225596785612,-11.0546261517374,131.630242588474));
#72807=CARTESIAN_POINT('Ctrl Pts',(79.9513120381194,-11.0554084467867,131.626386232792));
#72808=CARTESIAN_POINT('Ctrl Pts',(79.879972178366,-11.0524810138315,131.622529877109));
#72809=CARTESIAN_POINT('Ctrl Pts',(79.8089549414209,-11.0458492975028,131.618673521427));
#72810=CARTESIAN_POINT('Ctrl Pts',(79.7379586836785,-11.0392195402494,131.614818304951));
#72811=CARTESIAN_POINT('Ctrl Pts',(79.6672853429508,-11.0288877172192,131.610963088474));
#72812=CARTESIAN_POINT('Ctrl Pts',(79.5973460269111,-11.0149112487789,131.607107871998));
#72813=CARTESIAN_POINT('Ctrl Pts',(79.5274039764532,-11.0009342339005,131.603252504794));
#72814=CARTESIAN_POINT('Ctrl Pts',(79.4581964835926,-10.983312388063,131.599397137591));
#72815=CARTESIAN_POINT('Ctrl Pts',(79.3901241232501,-10.9621541676073,131.595541770387));
#72816=CARTESIAN_POINT('Ctrl Pts',(79.3219805097085,-10.9409738002642,131.591682367665));
#72817=CARTESIAN_POINT('Ctrl Pts',(79.2549748653891,-10.9162498135222,131.587822964943));
#72818=CARTESIAN_POINT('Ctrl Pts',(79.1894913917903,-10.8881401850811,131.583963562221));
#72819=CARTESIAN_POINT('Ctrl Pts',(79.1239708409342,-10.8600146407475,131.580101974275));
#72820=CARTESIAN_POINT('Ctrl Pts',(79.0599746125186,-10.8284998533183,131.576240386329));
#72821=CARTESIAN_POINT('Ctrl Pts',(78.9978632532916,-10.7938002964089,131.572378798383));
#72822=CARTESIAN_POINT('Ctrl Pts',(78.935643228015,-10.7590400313807,131.568510454451));
#72823=CARTESIAN_POINT('Ctrl Pts',(78.875315067074,-10.721084131254,131.564642110518));
#72824=CARTESIAN_POINT('Ctrl Pts',(78.8172106373791,-10.6801806111757,131.560773766585));
#72825=CARTESIAN_POINT('Ctrl Pts',(78.7827098989956,-10.6558932779622,131.558476855271));
#72826=CARTESIAN_POINT('Ctrl Pts',(78.748992556151,-10.6305675087266,131.556179943956));
#72827=CARTESIAN_POINT('Ctrl Pts',(78.7161221751681,-10.6042616037931,131.553883032642));
#72828=CARTESIAN_POINT('Ctrl Pts',(78.6614508986843,-10.5605086152737,131.550062721779));
#72829=CARTESIAN_POINT('Ctrl Pts',(78.608898578427,-10.5138612905726,131.546242410916));
#72830=CARTESIAN_POINT('Ctrl Pts',(78.5587935921191,-10.464555103908,131.542422100053));
#72831=CARTESIAN_POINT('Ctrl Pts',(78.5087739526719,-10.4153329034604,131.538608296557));
#72832=CARTESIAN_POINT('Ctrl Pts',(78.4611937228879,-10.3634611802395,131.534794493061));
#72833=CARTESIAN_POINT('Ctrl Pts',(78.4163489115401,-10.3092160984802,131.530980689565));
#72834=CARTESIAN_POINT('Ctrl Pts',(78.3715467866426,-10.2550226510107,131.527170516316));
#72835=CARTESIAN_POINT('Ctrl Pts',(78.329475236033,-10.1984607050715,131.523360343067));
#72836=CARTESIAN_POINT('Ctrl Pts',(78.2903930042303,-10.1398427446431,131.519550169818));
#72837=CARTESIAN_POINT('Ctrl Pts',(78.2513341075912,-10.0812597837433,131.515742271541));
#72838=CARTESIAN_POINT('Ctrl Pts',(78.2152612668582,-10.0206236570601,131.511934373265));
#72839=CARTESIAN_POINT('Ctrl Pts',(78.1823913627716,-9.95827783255842,131.508126474989));
#72840=CARTESIAN_POINT('Ctrl Pts',(78.1495294250015,-9.8959471181271,131.504319499591));
#72841=CARTESIAN_POINT('Ctrl Pts',(78.1198691151505,-9.83190797011655,131.500512524193));
#72842=CARTESIAN_POINT('Ctrl Pts',(78.0935816345597,-9.76652891557465,131.496705548795));
#72843=CARTESIAN_POINT('Ctrl Pts',(78.0672753510514,-9.7011030966816,131.492895850343));
#72844=CARTESIAN_POINT('Ctrl Pts',(78.0443469047302,-9.63433592002832,131.48908615189));
#72845=CARTESIAN_POINT('Ctrl Pts',(78.0249190681298,-9.56661527958821,131.485276453437));
#72846=CARTESIAN_POINT('Ctrl Pts',(78.0054843153251,-9.4988705309676,131.481465398753));
#72847=CARTESIAN_POINT('Ctrl Pts',(77.9895527685954,-9.43017212917455,131.477654344068));
#72848=CARTESIAN_POINT('Ctrl Pts',(77.9771963820948,-9.36091977763721,131.473843289384));
#72849=CARTESIAN_POINT('Ctrl Pts',(77.9648204879244,-9.29155809381223,131.470026217989));
#72850=CARTESIAN_POINT('Ctrl Pts',(77.9560310883201,-9.22164120977054,131.466209146595));
#72851=CARTESIAN_POINT('Ctrl Pts',(77.9508483050221,-9.15157471249978,131.4623920752));
#72852=CARTESIAN_POINT('Ctrl Pts',(77.947083896162,-9.10068334236886,131.459619623304));
#72853=CARTESIAN_POINT('Ctrl Pts',(77.9452210770952,-9.04971315177238,131.456847171409));
#72854=CARTESIAN_POINT('Ctrl Pts',(77.9452503396332,-8.99881859296011,131.454074719514));
#72855=CARTESIAN_POINT('Origin',(80.,-9.,141.545925280538));
#72856=CARTESIAN_POINT('',(81.2520391107129,-7.37076839346111,132.606087908702));
#72857=CARTESIAN_POINT('',(81.2520391107129,-7.3707683934611,132.547886797565));
#72858=CARTESIAN_POINT('',(81.2520391107129,-7.37076839346111,141.545925280538));
#72859=CARTESIAN_POINT('',(77.9452505617457,-9.00151937274232,132.095925280492));
#72860=CARTESIAN_POINT('Ctrl Pts',(81.2520391107129,-7.3707683934611,132.547886797565));
#72861=CARTESIAN_POINT('Ctrl Pts',(81.3083538607612,-7.41404540164551,132.544022016873));
#72862=CARTESIAN_POINT('Ctrl Pts',(81.3625154605356,-7.4603173375776,132.540157236181));
#72863=CARTESIAN_POINT('Ctrl Pts',(81.4141896923186,-7.50934072416269,132.536292455488));
#72864=CARTESIAN_POINT('Ctrl Pts',(81.4657959242599,-7.55829959924148,132.53243276059));
#72865=CARTESIAN_POINT('Ctrl Pts',(81.5149209399992,-7.61000240004589,132.528573065691));
#72866=CARTESIAN_POINT('Ctrl Pts',(81.5612632581667,-7.66416520437648,132.524713370792));
#72867=CARTESIAN_POINT('Ctrl Pts',(81.6075720611851,-7.71828883771727,132.520856467256));
#72868=CARTESIAN_POINT('Ctrl Pts',(81.6511018440891,-7.77486857728232,132.516999563721));
#72869=CARTESIAN_POINT('Ctrl Pts',(81.69158870253,-7.83358445484778,132.513142660186));
#72870=CARTESIAN_POINT('Ctrl Pts',(81.7320598241879,-7.89227751021701,132.509287255785));
#72871=CARTESIAN_POINT('Ctrl Pts',(81.7694900933409,-7.95310465610614,132.505431851384));
#72872=CARTESIAN_POINT('Ctrl Pts',(81.8036576222462,-8.01571511023833,132.501576446984));
#72873=CARTESIAN_POINT('Ctrl Pts',(81.8378232999895,-8.07832217219966,132.497721251465));
#72874=CARTESIAN_POINT('Ctrl Pts',(81.8687263571848,-8.14271192338244,132.493866055946));
#72875=CARTESIAN_POINT('Ctrl Pts',(81.8961906155537,-8.20850855217127,132.490010860427));
#72876=CARTESIAN_POINT('Ctrl Pts',(81.9236819791242,-8.27437011738988,132.486151860114));
#72877=CARTESIAN_POINT('Ctrl Pts',(81.9477275771208,-8.34164088432177,132.482292859801));
#72878=CARTESIAN_POINT('Ctrl Pts',(81.9681995653047,-8.4099253999414,132.478433859488));
#72879=CARTESIAN_POINT('Ctrl Pts',(81.9886814325063,-8.47824286712054,132.474572996965));
#72880=CARTESIAN_POINT('Ctrl Pts',(82.0055861392755,-8.54757458485537,132.470712134443));
#72881=CARTESIAN_POINT('Ctrl Pts',(82.0188366084774,-8.61751299267635,132.46685127192));
#72882=CARTESIAN_POINT('Ctrl Pts',(82.0321114365273,-8.68757997096613,132.462983311825));
#72883=CARTESIAN_POINT('Ctrl Pts',(82.0417185398173,-8.75825538508629,132.459115351731));
#72884=CARTESIAN_POINT('Ctrl Pts',(82.0476326158688,-8.82912509566834,132.455247391636));
#72885=CARTESIAN_POINT('Ctrl Pts',(82.05279078611,-8.89093661600497,132.45187381367));
#72886=CARTESIAN_POINT('Ctrl Pts',(82.055140463518,-8.95289567740437,132.448500235704));
#72887=CARTESIAN_POINT('Ctrl Pts',(82.0546972072604,-9.01472918789744,132.445126657738));
#72888=CARTESIAN_POINT('Ctrl Pts',(82.0541888463451,-9.08564468984679,132.441257574891));
#72889=CARTESIAN_POINT('Ctrl Pts',(82.0500038297876,-9.15667273902183,132.437388492044));
#72890=CARTESIAN_POINT('Ctrl Pts',(82.0421279206532,-9.22740078757216,132.433519409197));
#72891=CARTESIAN_POINT('Ctrl Pts',(82.0342637462307,-9.29802345485751,132.429656091091));
#72892=CARTESIAN_POINT('Ctrl Pts',(82.0227196484063,-9.36834652990705,132.425792772985));
#72893=CARTESIAN_POINT('Ctrl Pts',(82.007533399049,-9.43795800506769,132.421929454878));
#72894=CARTESIAN_POINT('Ctrl Pts',(81.9923649631563,-9.50748782599476,132.418070668442));
#72895=CARTESIAN_POINT('Ctrl Pts',(81.9735629648898,-9.57630723272567,132.414211882007));
#72896=CARTESIAN_POINT('Ctrl Pts',(81.9512166949537,-9.64401162398986,132.410353095571));
#72897=CARTESIAN_POINT('Ctrl Pts',(81.928884501529,-9.7116733664521,132.406496739888));
#72898=CARTESIAN_POINT('Ctrl Pts',(81.9030126178373,-9.7782210267392,132.402640384204));
#72899=CARTESIAN_POINT('Ctrl Pts',(81.8737405346709,-9.8432638799516,132.398784028521));
#72900=CARTESIAN_POINT('Ctrl Pts',(81.8444770987711,-9.90828751885387,132.394928812044));
#72901=CARTESIAN_POINT('Ctrl Pts',(81.8118156567702,-9.97180679045934,132.391073595567));
#72902=CARTESIAN_POINT('Ctrl Pts',(81.7759436651096,-10.0334513345375,132.38721837909));
#72903=CARTESIAN_POINT('Ctrl Pts',(81.7400702709614,-10.0950982887329,132.383363011885));
#72904=CARTESIAN_POINT('Ctrl Pts',(81.7009863241764,-10.1548699511211,132.37950764468));
#72905=CARTESIAN_POINT('Ctrl Pts',(81.6589241562073,-10.2124224537891,132.375652277476));
#72906=CARTESIAN_POINT('Ctrl Pts',(81.616817960618,-10.2700351982336,132.371792874753));
#72907=CARTESIAN_POINT('Ctrl Pts',(81.5717276080723,-10.3254237530131,132.36793347203));
#72908=CARTESIAN_POINT('Ctrl Pts',(81.5239269806332,-10.3782757779915,132.364074069307));
#72909=CARTESIAN_POINT('Ctrl Pts',(81.4760992881035,-10.4311577282016,132.360212481361));
#72910=CARTESIAN_POINT('Ctrl Pts',(81.4255586101456,-10.4814999465868,132.356350893414));
#72911=CARTESIAN_POINT('Ctrl Pts',(81.3726151590844,-10.5290275300176,132.352489305467));
#72912=CARTESIAN_POINT('Ctrl Pts',(81.3195790815579,-10.5766382646591,132.348620961533));
#72913=CARTESIAN_POINT('Ctrl Pts',(81.2641322160707,-10.6214242274925,132.3447526176));
#72914=CARTESIAN_POINT('Ctrl Pts',(81.2066166827356,-10.6631517499748,132.340884273666));
#72915=CARTESIAN_POINT('Ctrl Pts',(81.1724656141925,-10.6879283520124,132.33858736236));
#72916=CARTESIAN_POINT('Ctrl Pts',(81.1375857558048,-10.7116274925515,132.336290451053));
#72917=CARTESIAN_POINT('Ctrl Pts',(81.1020528512105,-10.7342079101535,132.333993539747));
#72918=CARTESIAN_POINT('Ctrl Pts',(81.0421986673429,-10.7722439919877,132.3301244569));
#72919=CARTESIAN_POINT('Ctrl Pts',(80.9802557831637,-10.8072522372018,132.326255374053));
#72920=CARTESIAN_POINT('Ctrl Pts',(80.9165630719349,-10.8389969270407,132.322386291206));
#72921=CARTESIAN_POINT('Ctrl Pts',(80.8529652596694,-10.870694318875,132.318522973099));
#72922=CARTESIAN_POINT('Ctrl Pts',(80.7876232267181,-10.8991375924029,132.314659654993));
#72923=CARTESIAN_POINT('Ctrl Pts',(80.7209036010568,-10.9241350161783,132.310796336886));
#72924=CARTESIAN_POINT('Ctrl Pts',(80.6542622374908,-10.9491031179851,132.30693755045));
#72925=CARTESIAN_POINT('Ctrl Pts',(80.586246943666,-10.9706332291725,132.303078764015));
#72926=CARTESIAN_POINT('Ctrl Pts',(80.517246068014,-10.9885809180478,132.299219977579));
#72927=CARTESIAN_POINT('Ctrl Pts',(80.4482886578541,-11.0065173011952,132.295363621895));
#72928=CARTESIAN_POINT('Ctrl Pts',(80.3783473666403,-11.0208756172173,132.291507266212));
#72929=CARTESIAN_POINT('Ctrl Pts',(80.3078261123459,-11.0315611354468,132.287650910529));
#72930=CARTESIAN_POINT('Ctrl Pts',(80.2373256907361,-11.0422434970673,132.283795694051));
#72931=CARTESIAN_POINT('Ctrl Pts',(80.1662461262163,-11.0492551421476,132.279940477574));
#72932=CARTESIAN_POINT('Ctrl Pts',(80.0950002433515,-11.0525526829446,132.276085261097));
#72933=CARTESIAN_POINT('Ctrl Pts',(80.0237515749859,-11.0558503526656,132.272229893892));
#72934=CARTESIAN_POINT('Ctrl Pts',(79.9523370607307,-11.0554336095476,132.268374526687));
#72935=CARTESIAN_POINT('Ctrl Pts',(79.8811716074018,-11.0513111357404,132.264519159483));
#72936=CARTESIAN_POINT('Ctrl Pts',(79.809931663249,-11.0471843468272,132.26065975676));
#72937=CARTESIAN_POINT('Ctrl Pts',(79.7389417863995,-11.0393441122429,132.256800354037));
#72938=CARTESIAN_POINT('Ctrl Pts',(79.668612932374,-11.0278511222253,132.252940951314));
#72939=CARTESIAN_POINT('Ctrl Pts',(79.598244257599,-11.0163516247864,132.249079363367));
#72940=CARTESIAN_POINT('Ctrl Pts',(79.5285378256335,-11.0011953579895,132.24521777542));
#72941=CARTESIAN_POINT('Ctrl Pts',(79.4598928447498,-10.9824938394224,132.241356187473));
#72942=CARTESIAN_POINT('Ctrl Pts',(79.3911277670117,-10.9637596018781,132.23748784354));
#72943=CARTESIAN_POINT('Ctrl Pts',(79.3234283095606,-10.9414678809868,132.233619499606));
#72944=CARTESIAN_POINT('Ctrl Pts',(79.257176344285,-10.9157793659527,132.229751155673));
#72945=CARTESIAN_POINT('Ctrl Pts',(79.2178378338809,-10.9005262649808,132.227454244367));
#72946=CARTESIAN_POINT('Ctrl Pts',(79.1790092532521,-10.8840764896419,132.225157333061));
#72947=CARTESIAN_POINT('Ctrl Pts',(79.1407663493566,-10.8664712952794,132.222860421755));
#72948=CARTESIAN_POINT('Ctrl Pts',(79.0763472474527,-10.836815837818,132.218991338908));
#72949=CARTESIAN_POINT('Ctrl Pts',(79.0133390613033,-10.8037633551402,132.215122256061));
#72950=CARTESIAN_POINT('Ctrl Pts',(78.95212362422,-10.7674706966686,132.211253173215));
#72951=CARTESIAN_POINT('Ctrl Pts',(78.8909993950849,-10.7312321124482,132.207389855108));
#72952=CARTESIAN_POINT('Ctrl Pts',(78.8316630274035,-10.691763181006,132.203526537002));
#72953=CARTESIAN_POINT('Ctrl Pts',(78.7744744529048,-10.6492679272686,132.199663218896));
#72954=CARTESIAN_POINT('Ctrl Pts',(78.717352960582,-10.6068225204476,132.19580443246));
#72955=CARTESIAN_POINT('Ctrl Pts',(78.6623746451655,-10.5613581309169,132.191945646024));
#72956=CARTESIAN_POINT('Ctrl Pts',(78.6098714810446,-10.5131226861318,132.188086859589));
#72957=CARTESIAN_POINT('Ctrl Pts',(78.5574013900671,-10.46491762614,132.184230503905));
#72958=CARTESIAN_POINT('Ctrl Pts',(78.5074037139146,-10.4139453019374,132.180374148222));
#72959=CARTESIAN_POINT('Ctrl Pts',(78.4601771161138,-10.3604936783243,132.176517792539));
#72960=CARTESIAN_POINT('Ctrl Pts',(78.4129644695228,-10.307057844856,132.172662576062));
#72961=CARTESIAN_POINT('Ctrl Pts',(78.3685215975989,-10.2511445298601,132.168807359585));
#72962=CARTESIAN_POINT('Ctrl Pts',(78.3271088597401,-10.1930770282508,132.164952143108));
#72963=CARTESIAN_POINT('Ctrl Pts',(78.285694502767,-10.1350072563759,132.161096775903));
#72964=CARTESIAN_POINT('Ctrl Pts',(78.2473107953373,-10.0747835274586,132.157241408699));
#72965=CARTESIAN_POINT('Ctrl Pts',(78.2121754805814,-10.012759127466,132.153386041494));
#72966=CARTESIAN_POINT('Ctrl Pts',(78.1770033887319,-9.95066980483986,132.149526638771));
#72967=CARTESIAN_POINT('Ctrl Pts',(78.1450867170067,-9.88677647217476,132.145667236049));
#72968=CARTESIAN_POINT('Ctrl Pts',(78.1165973717166,-9.8214573039879,132.141807833326));
#72969=CARTESIAN_POINT('Ctrl Pts',(78.0880918955353,-9.7561011515749,132.137946245379));
#72970=CARTESIAN_POINT('Ctrl Pts',(78.0630177797161,-9.68931801151647,132.134084657432));
#72971=CARTESIAN_POINT('Ctrl Pts',(78.0414978573553,-9.62150375683197,132.130223069485));
#72972=CARTESIAN_POINT('Ctrl Pts',(78.019940285119,-9.55357085867815,132.126354725552));
#72973=CARTESIAN_POINT('Ctrl Pts',(78.0019494437881,-9.48460371441895,132.122486381619));
#72974=CARTESIAN_POINT('Ctrl Pts',(77.9875974528442,-9.41501030192132,132.118618037685));
#72975=CARTESIAN_POINT('Ctrl Pts',(77.9790756536328,-9.37368773628851,132.116321126378));
#72976=CARTESIAN_POINT('Ctrl Pts',(77.9718357960167,-9.33214452690067,132.114024215071));
#72977=CARTESIAN_POINT('Ctrl Pts',(77.9658843036767,-9.29046668736917,132.111727303764));
#72978=CARTESIAN_POINT('Ctrl Pts',(77.9522361754433,-9.19488990327605,132.106459962688));
#72979=CARTESIAN_POINT('Ctrl Pts',(77.9453221472454,-9.09832918085083,132.101192621613));
#72980=CARTESIAN_POINT('Ctrl Pts',(77.9452505617463,-9.00151937358667,132.095925280538));
#72981=CARTESIAN_POINT('Ctrl Pts',(77.9452505617457,-9.00151937274232,132.095925280492));
#72982=CARTESIAN_POINT('Ctrl Pts',(77.9451965787833,-8.92851460007613,132.091953151545));
#72983=CARTESIAN_POINT('Ctrl Pts',(77.9490383631329,-8.85536232529461,132.087981022599));
#72984=CARTESIAN_POINT('Ctrl Pts',(77.9567917436018,-8.78251992393294,132.084008893652));
#72985=CARTESIAN_POINT('Ctrl Pts',(77.9642163077101,-8.71276672648809,132.080205220386));
#72986=CARTESIAN_POINT('Ctrl Pts',(77.9752273595376,-8.64329821470206,132.07640154712));
#72987=CARTESIAN_POINT('Ctrl Pts',(77.989785708765,-8.57451666799445,132.072597873854));
#72988=CARTESIAN_POINT('Ctrl Pts',(78.0043341072356,-8.50578213406467,132.068796800431));
#72989=CARTESIAN_POINT('Ctrl Pts',(78.0224248939572,-8.4377341234779,132.064995727008));
#72990=CARTESIAN_POINT('Ctrl Pts',(78.0439673846338,-8.37076715746578,132.061194653586));
#72991=CARTESIAN_POINT('Ctrl Pts',(78.0655028484981,-8.30382203499575,132.057394820012));
#72992=CARTESIAN_POINT('Ctrl Pts',(78.090487629481,-8.23795773444723,132.053594986438));
#72993=CARTESIAN_POINT('Ctrl Pts',(78.1187810484404,-8.17355410413447,132.049795152864));
#72994=CARTESIAN_POINT('Ctrl Pts',(78.1470753477331,-8.10914846994011,132.04599520106));
#72995=CARTESIAN_POINT('Ctrl Pts',(78.1786782846806,-8.04620405373723,132.042195249257));
#72996=CARTESIAN_POINT('Ctrl Pts',(78.2134016340244,-7.9850793916797,132.038395297453));
#72997=CARTESIAN_POINT('Ctrl Pts',(78.2481601793031,-7.92389277305208,132.03459149398));
#72998=CARTESIAN_POINT('Ctrl Pts',(78.2860451976124,-7.8645300241073,132.030787690508));
#72999=CARTESIAN_POINT('Ctrl Pts',(78.3268238180267,-7.80732274836095,132.026983887035));
#73000=CARTESIAN_POINT('Ctrl Pts',(78.3676269245136,-7.7500811217344,132.023177799517));
#73001=CARTESIAN_POINT('Ctrl Pts',(78.4113267751391,-7.69499793290784,132.019371711999));
#73002=CARTESIAN_POINT('Ctrl Pts',(78.4576505098363,-7.64237132739038,132.015565624481));
#73003=CARTESIAN_POINT('Ctrl Pts',(78.5040502056943,-7.58965842533244,132.011753295782));
#73004=CARTESIAN_POINT('Ctrl Pts',(78.5530820149241,-7.53941049549435,132.007940967083));
#73005=CARTESIAN_POINT('Ctrl Pts',(78.6044374301091,-7.4918877110707,132.004128638384));
#73006=CARTESIAN_POINT('Ctrl Pts',(78.6203081568685,-7.47720140927148,132.002950487513));
#73007=CARTESIAN_POINT('Ctrl Pts',(78.6364005734966,-7.4627750674,132.001772336643));
#73008=CARTESIAN_POINT('Ctrl Pts',(78.6527050052883,-7.44861553452252,132.000594185772));
#73009=CARTESIAN_POINT('Ctrl Pts',(78.7062492490401,-7.40211520323282,131.996725102925));
#73010=CARTESIAN_POINT('Ctrl Pts',(78.7623085494611,-7.35829907639647,131.992856020077));
#73011=CARTESIAN_POINT('Ctrl Pts',(78.8205827822767,-7.3174505686198,131.98898693723));
#73012=CARTESIAN_POINT('Ctrl Pts',(78.8787701893918,-7.27666292308245,131.985123619123));
#73013=CARTESIAN_POINT('Ctrl Pts',(78.9391655836702,-7.23883439640809,131.981260301016));
#73014=CARTESIAN_POINT('Ctrl Pts',(79.0014348634829,-7.20420902367991,131.977396982909));
#73015=CARTESIAN_POINT('Ctrl Pts',(79.0636311014544,-7.1696242665006,131.973538196473));
#73016=CARTESIAN_POINT('Ctrl Pts',(79.1276964363551,-7.13823543493536,131.969679410036));
#73017=CARTESIAN_POINT('Ctrl Pts',(79.1932682648411,-7.11024301298091,131.9658206236));
#73018=CARTESIAN_POINT('Ctrl Pts',(79.2587987878832,-7.08226822419972,131.961964267916));
#73019=CARTESIAN_POINT('Ctrl Pts',(79.3258334760286,-7.05768579059293,131.958107912232));
#73020=CARTESIAN_POINT('Ctrl Pts',(79.3939869504898,-7.03664935726617,131.954251556549));
#73021=CARTESIAN_POINT('Ctrl Pts',(79.4621202917322,-7.01561913831244,131.950396340071));
#73022=CARTESIAN_POINT('Ctrl Pts',(79.5313712992331,-6.99813298320813,131.946541123593));
#73023=CARTESIAN_POINT('Ctrl Pts',(79.6013381641286,-6.98429508530646,131.942685907115));
#73024=CARTESIAN_POINT('Ctrl Pts',(79.6713077645193,-6.97045664638438,131.93883053991));
#73025=CARTESIAN_POINT('Ctrl Pts',(79.7419928008914,-6.9602668399403,131.934975172705));
#73026=CARTESIAN_POINT('Ctrl Pts',(79.8129816751026,-6.95377867554544,131.9311198055));
#73027=CARTESIAN_POINT('Ctrl Pts',(79.8840448553072,-6.94728371981171,131.927260402776));
#73028=CARTESIAN_POINT('Ctrl Pts',(79.9554120234629,-6.94449818502207,131.923401000053));
#73029=CARTESIAN_POINT('Ctrl Pts',(80.0266677680113,-6.945423062368,131.91954159733));
#73030=CARTESIAN_POINT('Ctrl Pts',(80.0979638581219,-6.94634846338675,131.915680009382));
#73031=CARTESIAN_POINT('Ctrl Pts',(80.1691479140509,-6.95098842710182,131.911818421435));
#73032=CARTESIAN_POINT('Ctrl Pts',(80.2398085956787,-6.95929193662136,131.907956833487));
#73033=CARTESIAN_POINT('Ctrl Pts',(80.3105929007015,-6.9676099734284,131.904088489553));
#73034=CARTESIAN_POINT('Ctrl Pts',(80.3808515242713,-6.97960427102286,131.90022014562));
#73035=CARTESIAN_POINT('Ctrl Pts',(80.4501829707131,-6.99517261207356,131.896351801686));
#73036=CARTESIAN_POINT('Ctrl Pts',(80.4913499883317,-7.00441664495069,131.894054890384));
#73037=CARTESIAN_POINT('Ctrl Pts',(80.5321903805204,-7.01491979407838,131.891757979082));
#73038=CARTESIAN_POINT('Ctrl Pts',(80.5726231150619,-7.02665250637483,131.889461067781));
#73039=CARTESIAN_POINT('Ctrl Pts',(80.6407129225889,-7.04641070801747,131.885593007651));
#73040=CARTESIAN_POINT('Ctrl Pts',(80.7079122298124,-7.06973586291902,131.881724947521));
#73041=CARTESIAN_POINT('Ctrl Pts',(80.7738204657345,-7.09652963004138,131.877856887391));
#73042=CARTESIAN_POINT('Ctrl Pts',(80.8396428369124,-7.12328849044943,131.87399386654));
#73043=CARTESIAN_POINT('Ctrl Pts',(80.9041770260992,-7.15350682139415,131.870130845689));
#73044=CARTESIAN_POINT('Ctrl Pts',(80.967036885349,-7.18703634209772,131.866267824838));
#73045=CARTESIAN_POINT('Ctrl Pts',(81.0298266373812,-7.22052846753132,131.86240911239));
#73046=CARTESIAN_POINT('Ctrl Pts',(81.0909453409531,-7.25732422244068,131.858550399943));
#73047=CARTESIAN_POINT('Ctrl Pts',(81.1500279067684,-7.29722773802429,131.854691687496));
#73048=CARTESIAN_POINT('Ctrl Pts',(81.184758141456,-7.32068403925214,131.85242343819));
#73049=CARTESIAN_POINT('Ctrl Pts',(81.2187852194779,-7.34521329605046,131.850155188884));
#73050=CARTESIAN_POINT('Ctrl Pts',(81.2520391107129,-7.37076839346113,131.847886939579));
#73051=CARTESIAN_POINT('',(77.945250271645,-8.99894343713344,132.154074719416));
#73052=CARTESIAN_POINT('Ctrl Pts',(77.945250271645,-8.99894343713344,132.154074719416));
#73053=CARTESIAN_POINT('Ctrl Pts',(77.945290872253,-8.91998543955825,132.14981310901));
#73054=CARTESIAN_POINT('Ctrl Pts',(77.9498868100455,-8.84118478791793,132.145551498605));
#73055=CARTESIAN_POINT('Ctrl Pts',(77.9589591217714,-8.76304072944942,132.141289888199));
#73056=CARTESIAN_POINT('Ctrl Pts',(77.9680642943239,-8.68461362533253,132.137012841811));
#73057=CARTESIAN_POINT('Ctrl Pts',(77.981678191433,-8.60684816261152,132.132735795423));
#73058=CARTESIAN_POINT('Ctrl Pts',(77.999671050668,-8.53023233725138,132.128458749035));
#73059=CARTESIAN_POINT('Ctrl Pts',(78.017750965159,-8.45324581981796,132.124161008917));
#73060=CARTESIAN_POINT('Ctrl Pts',(78.0402521766357,-8.37742036596183,132.119863268799));
#73061=CARTESIAN_POINT('Ctrl Pts',(78.0669947748154,-8.30323005094278,132.115565528682));
#73062=CARTESIAN_POINT('Ctrl Pts',(78.0794747989853,-8.2686075016157,132.113559893321));
#73063=CARTESIAN_POINT('Ctrl Pts',(78.0928778545041,-8.23434073399828,132.11155425796));
#73064=CARTESIAN_POINT('Ctrl Pts',(78.1071822245976,-8.20047612191953,132.109548622599));
#73065=CARTESIAN_POINT('Ctrl Pts',(78.1347768681954,-8.13514770166873,132.105679539752));
#73066=CARTESIAN_POINT('Ctrl Pts',(78.1658116320372,-8.07112160100121,132.101810456905));
#73067=CARTESIAN_POINT('Ctrl Pts',(78.2001418722771,-8.00878444192498,132.097941374058));
#73068=CARTESIAN_POINT('Ctrl Pts',(78.2344209621713,-7.94654016210686,132.094078055952));
#73069=CARTESIAN_POINT('Ctrl Pts',(78.2719855496262,-7.8859802508739,132.090214737845));
#73070=CARTESIAN_POINT('Ctrl Pts',(78.3126431435273,-7.8274709379233,132.086351419739));
#73071=CARTESIAN_POINT('Ctrl Pts',(78.3532530460864,-7.76903025637427,132.082492633303));
#73072=CARTESIAN_POINT('Ctrl Pts',(78.3969484726024,-7.71263579225423,132.078633846867));
#73073=CARTESIAN_POINT('Ctrl Pts',(78.4434921636943,-7.65862722630175,132.074775060431));
#73074=CARTESIAN_POINT('Ctrl Pts',(78.4900065356737,-7.60465268178554,132.070918704748));
#73075=CARTESIAN_POINT('Ctrl Pts',(78.5393652961915,-7.55306142074469,132.067062349065));
#73076=CARTESIAN_POINT('Ctrl Pts',(78.5912901108142,-7.50416110138486,132.063205993381));
#73077=CARTESIAN_POINT('Ctrl Pts',(78.6431995863267,-7.45527522766904,132.059350776904));
#73078=CARTESIAN_POINT('Ctrl Pts',(78.6976732575751,-7.40907905034047,132.055495560427));
#73079=CARTESIAN_POINT('Ctrl Pts',(78.7543962613515,-7.36584306482982,132.05164034395));
#73080=CARTESIAN_POINT('Ctrl Pts',(78.8111214828275,-7.3226053889215,132.047784976745));
#73081=CARTESIAN_POINT('Ctrl Pts',(78.870095823747,-7.28232842734014,132.04392960954));
#73082=CARTESIAN_POINT('Ctrl Pts',(78.9309730915482,-7.2452410332168,132.040074242335));
#73083=CARTESIAN_POINT('Ctrl Pts',(78.9919140812485,-7.20811481870503,132.036214839613));
#73084=CARTESIAN_POINT('Ctrl Pts',(79.0547615582912,-7.17418508951644,132.03235543689));
#73085=CARTESIAN_POINT('Ctrl Pts',(79.11914299841,-7.14363567550713,132.028496034167));
#73086=CARTESIAN_POINT('Ctrl Pts',(79.1835608918059,-7.11306896417964,132.02463444622));
#73087=CARTESIAN_POINT('Ctrl Pts',(79.2495140279317,-7.08588656333384,132.020772858273));
#73088=CARTESIAN_POINT('Ctrl Pts',(79.3166106344542,-7.06222381644346,132.016911270326));
#73089=CARTESIAN_POINT('Ctrl Pts',(79.3838246288948,-7.03851967072926,132.013042926392));
#73090=CARTESIAN_POINT('Ctrl Pts',(79.4521856218024,-7.01834761064219,132.009174582459));
#73091=CARTESIAN_POINT('Ctrl Pts',(79.5212881315132,-7.00179267605439,132.005306238525));
#73092=CARTESIAN_POINT('Ctrl Pts',(79.5623192131711,-6.99196283230839,132.00300932722));
#73093=CARTESIAN_POINT('Ctrl Pts',(79.6036115398418,-6.98340727619076,132.000712415914));
#73094=CARTESIAN_POINT('Ctrl Pts',(79.6450793453083,-6.97613515980606,131.998415504608));
#73095=CARTESIAN_POINT('Ctrl Pts',(79.7149081391761,-6.96388944025815,131.994547671615));
#73096=CARTESIAN_POINT('Ctrl Pts',(79.7855081655632,-6.95523790608877,131.990679838623));
#73097=CARTESIAN_POINT('Ctrl Pts',(79.8564765514174,-6.95026865609003,131.98681200563));
#73098=CARTESIAN_POINT('Ctrl Pts',(79.9273493904374,-6.94530609633936,131.982949380016));
#73099=CARTESIAN_POINT('Ctrl Pts',(79.9985891252929,-6.9440160213747,131.979086754401));
#73100=CARTESIAN_POINT('Ctrl Pts',(80.0697838953175,-6.94643535031051,131.975224128786));
#73101=CARTESIAN_POINT('Ctrl Pts',(80.1409066359354,-6.9488522315549,131.97136541108));
#73102=CARTESIAN_POINT('Ctrl Pts',(80.2119840191086,-6.9549710540467,131.967506693374));
#73103=CARTESIAN_POINT('Ctrl Pts',(80.2826020050066,-6.96477675198364,131.963647975667));
#73104=CARTESIAN_POINT('Ctrl Pts',(80.353172170657,-6.97457580981471,131.959791870962));
#73105=CARTESIAN_POINT('Ctrl Pts',(80.4232830766715,-6.98805672020389,131.955935766256));
#73106=CARTESIAN_POINT('Ctrl Pts',(80.4925253618697,-7.00515255460095,131.95207966155));
#73107=CARTESIAN_POINT('Ctrl Pts',(80.561770301311,-7.02224904432734,131.948223409029));
#73108=CARTESIAN_POINT('Ctrl Pts',(80.6301460772589,-7.0429606369905,131.944367156508));
#73109=CARTESIAN_POINT('Ctrl Pts',(80.6972543344538,-7.06716944467827,131.940510903988));
#73110=CARTESIAN_POINT('Ctrl Pts',(80.7643590610103,-7.09137697871429,131.936654854349));
#73111=CARTESIAN_POINT('Ctrl Pts',(80.8301959465034,-7.11908118996674,131.93279880471));
#73112=CARTESIAN_POINT('Ctrl Pts',(80.894384749111,-7.15011527844093,131.928942755071));
#73113=CARTESIAN_POINT('Ctrl Pts',(80.9586397009929,-7.18118134885509,131.925082731609));
#73114=CARTESIAN_POINT('Ctrl Pts',(81.0212427411819,-7.21558393418775,131.921222708148));
#73115=CARTESIAN_POINT('Ctrl Pts',(81.0818372046269,-7.25310966996064,131.917362684687));
#73116=CARTESIAN_POINT('Ctrl Pts',(81.140556548437,-7.28947415699949,131.913622111178));
#73117=CARTESIAN_POINT('Ctrl Pts',(81.1973895061473,-7.32877102364184,131.90988153767));
#73118=CARTESIAN_POINT('Ctrl Pts',(81.2520391107129,-7.3707683934611,131.906140964161));
#73119=CARTESIAN_POINT('Ctrl Pts',(81.2520391107129,-7.37076839346111,132.606087908702));
#73120=CARTESIAN_POINT('Ctrl Pts',(81.3085934782384,-7.4142295439442,132.602232450567));
#73121=CARTESIAN_POINT('Ctrl Pts',(81.3628750382077,-7.46063328907426,132.598376992433));
#73122=CARTESIAN_POINT('Ctrl Pts',(81.4145730951239,-7.50970455242875,132.594521534299));
#73123=CARTESIAN_POINT('Ctrl Pts',(81.4663263971359,-7.55882825385944,132.590661956181));
#73124=CARTESIAN_POINT('Ctrl Pts',(81.5154903332362,-7.61062482749505,132.586802378063));
#73125=CARTESIAN_POINT('Ctrl Pts',(81.5617909053502,-7.66478214119745,132.582942799945));
#73126=CARTESIAN_POINT('Ctrl Pts',(81.6081191558986,-7.71897183008615,132.579080914575));
#73127=CARTESIAN_POINT('Ctrl Pts',(81.6515803396647,-7.77552468259948,132.575219029205));
#73128=CARTESIAN_POINT('Ctrl Pts',(81.6919423194437,-7.83409745253926,132.571357143836));
#73129=CARTESIAN_POINT('Ctrl Pts',(81.7323736167915,-7.89277081521586,132.567488626073));
#73130=CARTESIAN_POINT('Ctrl Pts',(81.7696948321811,-7.95347060574031,132.56362010831));
#73131=CARTESIAN_POINT('Ctrl Pts',(81.8037189057658,-8.01582741783614,132.559751590548));
#73132=CARTESIAN_POINT('Ctrl Pts',(81.8203431345088,-8.04629507790004,132.55786142522));
#73133=CARTESIAN_POINT('Ctrl Pts',(81.8361809521596,-8.07715799347721,132.555971259893));
#73134=CARTESIAN_POINT('Ctrl Pts',(81.8512147628779,-8.10837145390982,132.554081094566));
#73135=CARTESIAN_POINT('Ctrl Pts',(81.8819882927562,-8.1722639942131,132.550212011719));
#73136=CARTESIAN_POINT('Ctrl Pts',(81.9095104472025,-8.23787671514327,132.546342928872));
#73137=CARTESIAN_POINT('Ctrl Pts',(81.9335867653229,-8.3048454966928,132.542473846025));
#73138=CARTESIAN_POINT('Ctrl Pts',(81.9576272109299,-8.37171449809755,132.538610527919));
#73139=CARTESIAN_POINT('Ctrl Pts',(81.9782318482963,-8.43993509614539,132.534747209812));
#73140=CARTESIAN_POINT('Ctrl Pts',(81.9952531484605,-8.5091207520598,132.530883891706));
#73141=CARTESIAN_POINT('Ctrl Pts',(82.0122544826462,-8.57822525322665,132.52702510527));
#73142=CARTESIAN_POINT('Ctrl Pts',(82.0256807132234,-8.64829209427239,132.523166318834));
#73143=CARTESIAN_POINT('Ctrl Pts',(82.0354338270112,-8.71891869795672,132.519307532398));
#73144=CARTESIAN_POINT('Ctrl Pts',(82.0451807970526,-8.78950081205954,132.515451176715));
#73145=CARTESIAN_POINT('Ctrl Pts',(82.0512591745401,-8.86064150915053,132.511594821032));
#73146=CARTESIAN_POINT('Ctrl Pts',(82.053622127359,-8.9319285631008,132.507738465349));
#73147=CARTESIAN_POINT('Ctrl Pts',(82.0559843821379,-9.00319455814147,132.503883248871));
#73148=CARTESIAN_POINT('Ctrl Pts',(82.0546333751519,-9.07460633895539,132.500028032394));
#73149=CARTESIAN_POINT('Ctrl Pts',(82.0495743065814,-9.14574883979362,132.496172815917));
#73150=CARTESIAN_POINT('Ctrl Pts',(82.0445150402166,-9.2168941220909,132.492317448712));
#73151=CARTESIAN_POINT('Ctrl Pts',(82.0357474610954,-9.28776961910727,132.488462081508));
#73152=CARTESIAN_POINT('Ctrl Pts',(82.0233287253966,-9.35796428800237,132.484606714303));
#73153=CARTESIAN_POINT('Ctrl Pts',(82.0108969906679,-9.42823243157463,132.48074731158));
#73154=CARTESIAN_POINT('Ctrl Pts',(81.9948065550646,-9.4978178450992,132.476887908857));
#73155=CARTESIAN_POINT('Ctrl Pts',(81.9751657636102,-9.56631949353887,132.473028506135));
#73156=CARTESIAN_POINT('Ctrl Pts',(81.9555138513854,-9.63485992814995,132.469166918188));
#73157=CARTESIAN_POINT('Ctrl Pts',(81.9323077396484,-9.70231491653813,132.465305330241));
#73158=CARTESIAN_POINT('Ctrl Pts',(81.9057048777051,-9.76830103578668,132.461443742294));
#73159=CARTESIAN_POINT('Ctrl Pts',(81.8790554731013,-9.83440260011612,132.45757539836));
#73160=CARTESIAN_POINT('Ctrl Pts',(81.8489976583775,-9.89902972393679,132.453707054427));
#73161=CARTESIAN_POINT('Ctrl Pts',(81.8157356889678,-9.96182195353851,132.449838710493));
#73162=CARTESIAN_POINT('Ctrl Pts',(81.7959856887283,-9.99910617247326,132.447541799187));
#73163=CARTESIAN_POINT('Ctrl Pts',(81.7751068783501,-10.0357439816394,132.44524488788));
#73164=CARTESIAN_POINT('Ctrl Pts',(81.7531490904376,-10.0716649799251,132.442947976574));
#73165=CARTESIAN_POINT('Ctrl Pts',(81.7161618108983,-10.1321728967617,132.439078893727));
#73166=CARTESIAN_POINT('Ctrl Pts',(81.6759658686669,-10.1908822176689,132.43520981088));
#73167=CARTESIAN_POINT('Ctrl Pts',(81.632761701244,-10.2474320780912,132.431340728033));
#73168=CARTESIAN_POINT('Ctrl Pts',(81.5896219058757,-10.3038976820418,132.427477409927));
#73169=CARTESIAN_POINT('Ctrl Pts',(81.5434830746863,-10.3582098292608,132.42361409182));
#73170=CARTESIAN_POINT('Ctrl Pts',(81.494589934882,-10.4100349247623,132.419750773714));
#73171=CARTESIAN_POINT('Ctrl Pts',(81.445754146712,-10.4617992294466,132.415891987278));
#73172=CARTESIAN_POINT('Ctrl Pts',(81.3941707991378,-10.5110819255448,132.412033200842));
#73173=CARTESIAN_POINT('Ctrl Pts',(81.3401249501949,-10.5575823189691,132.408174414406));
#73174=CARTESIAN_POINT('Ctrl Pts',(81.2861131461739,-10.6040534205552,132.404318058723));
#73175=CARTESIAN_POINT('Ctrl Pts',(81.2296422857039,-10.6477453806082,132.40046170304));
#73176=CARTESIAN_POINT('Ctrl Pts',(81.1710332927739,-10.6883952705795,132.396605347356));
#73177=CARTESIAN_POINT('Ctrl Pts',(81.1124416135272,-10.7290331521662,132.392750130879));
#73178=CARTESIAN_POINT('Ctrl Pts',(81.0517134547251,-10.7666304710523,132.388894914402));
#73179=CARTESIAN_POINT('Ctrl Pts',(80.9892003473083,-10.8009664725877,132.385039697925));
#73180=CARTESIAN_POINT('Ctrl Pts',(80.9266847958159,-10.8353038165582,132.38118433072));
#73181=CARTESIAN_POINT('Ctrl Pts',(80.8623845840018,-10.8663793580925,132.377328963515));
#73182=CARTESIAN_POINT('Ctrl Pts',(80.796676042939,-10.8940181744395,132.373473596311));
#73183=CARTESIAN_POINT('Ctrl Pts',(80.7308987229515,-10.9216859210905,132.369614193588));
#73184=CARTESIAN_POINT('Ctrl Pts',(80.6637105797083,-10.9459095727734,132.365754790865));
#73185=CARTESIAN_POINT('Ctrl Pts',(80.5955073002182,-10.9665626402144,132.361895388142));
#73186=CARTESIAN_POINT('Ctrl Pts',(80.5272654034954,-10.9872274015843,132.358033800195));
#73187=CARTESIAN_POINT('Ctrl Pts',(80.4580076981792,-11.0043174377093,132.354172212249));
#73188=CARTESIAN_POINT('Ctrl Pts',(80.3881417079494,-11.017757065915,132.350310624302));
#73189=CARTESIAN_POINT('Ctrl Pts',(80.3181534846656,-11.031220207232,132.346442280368));
#73190=CARTESIAN_POINT('Ctrl Pts',(80.247555333052,-11.0410201229495,132.342573936435));
#73191=CARTESIAN_POINT('Ctrl Pts',(80.1767608663214,-11.0471329118153,132.338705592501));
#73192=CARTESIAN_POINT('Ctrl Pts',(80.1347251492659,-11.0507625099329,132.336408681195));
#73193=CARTESIAN_POINT('Ctrl Pts',(80.0926202580343,-11.0530931573773,132.334111769889));
#73194=CARTESIAN_POINT('Ctrl Pts',(80.0505323671532,-11.0541285359904,132.331814858582));
#73195=CARTESIAN_POINT('Ctrl Pts',(79.9796364922361,-11.0558726023028,132.327945775735));
#73196=CARTESIAN_POINT('Ctrl Pts',(79.9085113617542,-11.0539454419162,132.324076692888));
#73197=CARTESIAN_POINT('Ctrl Pts',(79.8375688633132,-11.0483197231718,132.320207610042));
#73198=CARTESIAN_POINT('Ctrl Pts',(79.7667320656567,-11.0427023864678,132.316344291935));
#73199=CARTESIAN_POINT('Ctrl Pts',(79.6960778402228,-11.0333974680175,132.312480973829));
#73200=CARTESIAN_POINT('Ctrl Pts',(79.6260191864144,-11.0204296358868,132.308617655722));
#73201=CARTESIAN_POINT('Ctrl Pts',(79.5560427113801,-11.0074770150183,132.304758869287));
#73202=CARTESIAN_POINT('Ctrl Pts',(79.4866608956555,-10.9908701029518,132.300900082851));
#73203=CARTESIAN_POINT('Ctrl Pts',(79.4182809721587,-10.9706852958165,132.297041296415));
#73204=CARTESIAN_POINT('Ctrl Pts',(79.3499441229995,-10.9505132036296,132.293184940732));
#73205=CARTESIAN_POINT('Ctrl Pts',(79.2826083787457,-10.9267678251053,132.289328585049));
#73206=CARTESIAN_POINT('Ctrl Pts',(79.2166686972241,-10.8995761718318,132.285472229365));
#73207=CARTESIAN_POINT('Ctrl Pts',(79.1507484949446,-10.872392551245,132.281617012888));
#73208=CARTESIAN_POINT('Ctrl Pts',(79.0862239854993,-10.8417648621427,132.277761796411));
#73209=CARTESIAN_POINT('Ctrl Pts',(79.0234712956362,-10.8078687043183,132.273906579934));
#73210=CARTESIAN_POINT('Ctrl Pts',(78.9607161523306,-10.7739712212555,132.270051212729));
#73211=CARTESIAN_POINT('Ctrl Pts',(78.8997333925077,-10.7368052485742,132.266195845525));
#73212=CARTESIAN_POINT('Ctrl Pts',(78.8408740891248,-10.6965920797993,132.26234047832));
#73213=CARTESIAN_POINT('Ctrl Pts',(78.7819531761015,-10.6563368188023,132.258481075597));
#73214=CARTESIAN_POINT('Ctrl Pts',(78.7251605584144,-10.6130282691899,132.254621672874));
#73215=CARTESIAN_POINT('Ctrl Pts',(78.6708171167331,-10.5669302554135,132.250762270152));
#73216=CARTESIAN_POINT('Ctrl Pts',(78.6164429053683,-10.5208061405797,132.246900682205));
#73217=CARTESIAN_POINT('Ctrl Pts',(78.5645209843352,-10.4718897507229,132.243039094258));
#73218=CARTESIAN_POINT('Ctrl Pts',(78.5153359699761,-10.4204824111735,132.239177506311));
#73219=CARTESIAN_POINT('Ctrl Pts',(78.4660649046714,-10.3689851326409,132.235309162378));
#73220=CARTESIAN_POINT('Ctrl Pts',(78.4195406232412,-10.31498857167,132.231440818444));
#73221=CARTESIAN_POINT('Ctrl Pts',(78.3760075415848,-10.2588272548331,132.227572474511));
#73222=CARTESIAN_POINT('Ctrl Pts',(78.3501588504697,-10.2254802810766,132.225275563204));
#73223=CARTESIAN_POINT('Ctrl Pts',(78.3253639320698,-10.1913706665246,132.222978651898));
#73224=CARTESIAN_POINT('Ctrl Pts',(78.3016664325153,-10.1565728062058,132.220681740591));
#73225=CARTESIAN_POINT('Ctrl Pts',(78.2611561583561,-10.0970867469942,132.216755228997));
#73226=CARTESIAN_POINT('Ctrl Pts',(78.22369963522,-10.0353595220403,132.212828717404));
#73227=CARTESIAN_POINT('Ctrl Pts',(78.1895485268499,-9.97173197223746,132.20890220581));
#73228=CARTESIAN_POINT('Ctrl Pts',(78.1554524650247,-9.90820698065173,132.204982023173));
#73229=CARTESIAN_POINT('Ctrl Pts',(78.1246514562146,-9.8427881549543,132.201061840536));
#73230=CARTESIAN_POINT('Ctrl Pts',(78.0973541022689,-9.77584544230588,132.1971416579));
#73231=CARTESIAN_POINT('Ctrl Pts',(78.0700989505557,-9.70900622437492,132.19322753594));
#73232=CARTESIAN_POINT('Ctrl Pts',(78.0463368576597,-9.64064823422256,132.189313413981));
#73233=CARTESIAN_POINT('Ctrl Pts',(78.0262298521903,-9.57116457008041,132.185399292022));
#73234=CARTESIAN_POINT('Ctrl Pts',(78.0061411816448,-9.5017442658303,132.181488739223));
#73235=CARTESIAN_POINT('Ctrl Pts',(77.9897011084485,-9.43120077295633,132.177578186424));
#73236=CARTESIAN_POINT('Ctrl Pts',(77.977022638429,-9.35994465834536,132.173667633625));
#73237=CARTESIAN_POINT('Ctrl Pts',(77.9643515390457,-9.28872996851899,132.169759354228));
#73238=CARTESIAN_POINT('Ctrl Pts',(77.9554377814959,-9.21680393863984,132.165851074832));
#73239=CARTESIAN_POINT('Ctrl Pts',(77.9503434953968,-9.14458829702956,132.161942795435));
#73240=CARTESIAN_POINT('Ctrl Pts',(77.9469249211355,-9.09612723126452,132.159320103444));
#73241=CARTESIAN_POINT('Ctrl Pts',(77.9452252851269,-9.04753598590096,132.156697411453));
#73242=CARTESIAN_POINT('Ctrl Pts',(77.9452502716446,-8.99894343798261,132.154074719462));
#73243=CARTESIAN_POINT('Origin',(80.,-9.,141.545925280538));
#73244=CARTESIAN_POINT('',(81.2520391107129,-7.37076839346112,133.306011340568));
#73245=CARTESIAN_POINT('',(81.2520391107129,-7.3707683934611,133.247993489751));
#73246=CARTESIAN_POINT('',(81.2520391107129,-7.37076839346111,141.545925280538));
#73247=CARTESIAN_POINT('',(77.9452506345969,-8.99838510821483,132.795925280579));
#73248=CARTESIAN_POINT('Ctrl Pts',(81.2520391107129,-7.3707683934611,133.247993489751));
#73249=CARTESIAN_POINT('Ctrl Pts',(81.3085458581026,-7.4141929486116,133.244130558908));
#73250=CARTESIAN_POINT('Ctrl Pts',(81.362730023197,-7.46051391564537,133.240267628065));
#73251=CARTESIAN_POINT('Ctrl Pts',(81.4142959525366,-7.50944154051626,133.236404697222));
#73252=CARTESIAN_POINT('Ctrl Pts',(81.4659453720001,-7.55844838384621,133.232535511929));
#73253=CARTESIAN_POINT('Ctrl Pts',(81.5149677691851,-7.61006994974573,133.228666326635));
#73254=CARTESIAN_POINT('Ctrl Pts',(81.5611066401294,-7.66398217802155,133.224797141341));
#73255=CARTESIAN_POINT('Ctrl Pts',(81.5680176300305,-7.67205751357997,133.224217588787));
#73256=CARTESIAN_POINT('Ctrl Pts',(81.5748640036943,-7.6801841888825,133.223638036233));
#73257=CARTESIAN_POINT('Ctrl Pts',(81.5816449834366,-7.68836106002075,133.223058483679));
#73258=CARTESIAN_POINT('Ctrl Pts',(81.6269146871557,-7.74294971060641,133.219189400832));
#73259=CARTESIAN_POINT('Ctrl Pts',(81.6694436428744,-7.79999167812778,133.215320317985));
#73260=CARTESIAN_POINT('Ctrl Pts',(81.7089553397541,-7.85918046596933,133.211451235138));
#73261=CARTESIAN_POINT('Ctrl Pts',(81.7484081661759,-7.9182810654689,133.207587917032));
#73262=CARTESIAN_POINT('Ctrl Pts',(81.7848523898165,-7.97952173530745,133.203724598926));
#73263=CARTESIAN_POINT('Ctrl Pts',(81.8180516424325,-8.04256290653195,133.199861280819));
#73264=CARTESIAN_POINT('Ctrl Pts',(81.8512119523379,-8.10553013048689,133.196002494383));
#73265=CARTESIAN_POINT('Ctrl Pts',(81.8811346266599,-8.17029323296865,133.192143707948));
#73266=CARTESIAN_POINT('Ctrl Pts',(81.9076274856162,-8.23648514184629,133.188284921512));
#73267=CARTESIAN_POINT('Ctrl Pts',(81.934103656014,-8.30263535467497,133.184428565829));
#73268=CARTESIAN_POINT('Ctrl Pts',(81.9571541174251,-8.37021213829343,133.180572210145));
#73269=CARTESIAN_POINT('Ctrl Pts',(81.9766340351603,-8.43882671700644,133.176715854462));
#73270=CARTESIAN_POINT('Ctrl Pts',(81.9961081983328,-8.50742102628585,133.172860637985));
#73271=CARTESIAN_POINT('Ctrl Pts',(82.0120137792493,-8.57705205496281,133.169005421508));
#73272=CARTESIAN_POINT('Ctrl Pts',(82.0242557560878,-8.6473157269663,133.16515020503));
#73273=CARTESIAN_POINT('Ctrl Pts',(82.036498211551,-8.71758214606921,133.161294837826));
#73274=CARTESIAN_POINT('Ctrl Pts',(82.0450766973487,-8.78848077865394,133.157439470621));
#73275=CARTESIAN_POINT('Ctrl Pts',(82.0499475849728,-8.85959892676965,133.153584103417));
#73276=CARTESIAN_POINT('Ctrl Pts',(82.054823571088,-8.93079151619345,133.149724700694));
#73277=CARTESIAN_POINT('Ctrl Pts',(82.055984178733,-9.00220359418581,133.145865297971));
#73278=CARTESIAN_POINT('Ctrl Pts',(82.0534378710938,-9.073419834225,133.142005895248));
#73279=CARTESIAN_POINT('Ctrl Pts',(82.0508901217152,-9.14467639745873,133.138144307301));
#73280=CARTESIAN_POINT('Ctrl Pts',(82.0446313214623,-9.21573641786266,133.134282719354));
#73281=CARTESIAN_POINT('Ctrl Pts',(82.0347218354742,-9.28618982292246,133.130421131407));
#73282=CARTESIAN_POINT('Ctrl Pts',(82.0247950124852,-9.35676648873972,133.126552787474));
#73283=CARTESIAN_POINT('Ctrl Pts',(82.0112048445784,-9.42673394328516,133.122684443541));
#73284=CARTESIAN_POINT('Ctrl Pts',(81.9940626600268,-9.49569312118169,133.118816099607));
#73285=CARTESIAN_POINT('Ctrl Pts',(81.9838841241492,-9.53663909654412,133.116519188301));
#73286=CARTESIAN_POINT('Ctrl Pts',(81.972454231622,-9.57722987554718,133.114222276994));
#73287=CARTESIAN_POINT('Ctrl Pts',(81.9598043720399,-9.61738511954302,133.111925365688));
#73288=CARTESIAN_POINT('Ctrl Pts',(81.9384960374134,-9.68502550483927,133.108056282841));
#73289=CARTESIAN_POINT('Ctrl Pts',(81.9136400623009,-9.75169392790778,133.104187199994));
#73290=CARTESIAN_POINT('Ctrl Pts',(81.8853439706104,-9.81699184511425,133.100318117147));
#73291=CARTESIAN_POINT('Ctrl Pts',(81.8570900386852,-9.88219247168061,133.096454799041));
#73292=CARTESIAN_POINT('Ctrl Pts',(81.8254063559398,-9.94602620356839,133.092591480934));
#73293=CARTESIAN_POINT('Ctrl Pts',(81.7904500040003,-10.0081102844804,133.088728162828));
#73294=CARTESIAN_POINT('Ctrl Pts',(81.7555346558482,-10.0701215407895,133.084869376392));
#73295=CARTESIAN_POINT('Ctrl Pts',(81.7173545009176,-10.1303868015217,133.081010589956));
#73296=CARTESIAN_POINT('Ctrl Pts',(81.6761136941161,-10.1885455173853,133.07715180352));
#73297=CARTESIAN_POINT('Ctrl Pts',(81.6348988659987,-10.2466675975224,133.073295447837));
#73298=CARTESIAN_POINT('Ctrl Pts',(81.5906274914361,-10.3026853701469,133.069439092154));
#73299=CARTESIAN_POINT('Ctrl Pts',(81.5435476382644,-10.3562662905596,133.065582736471));
#73300=CARTESIAN_POINT('Ctrl Pts',(81.4964816929528,-10.4098313826319,133.061727519993));
#73301=CARTESIAN_POINT('Ctrl Pts',(81.4466092365965,-10.4609606869092,133.057872303516));
#73302=CARTESIAN_POINT('Ctrl Pts',(81.3942182089022,-10.5093552095069,133.054017087039));
#73303=CARTESIAN_POINT('Ctrl Pts',(81.3418251328754,-10.5577516241857,133.050161719834));
#73304=CARTESIAN_POINT('Ctrl Pts',(81.28691364835,-10.6034127169036,133.04630635263));
#73305=CARTESIAN_POINT('Ctrl Pts',(81.2298068132815,-10.6460779946608,133.042450985425));
#73306=CARTESIAN_POINT('Ctrl Pts',(81.1726402029288,-10.6887879313296,133.038591582702));
#73307=CARTESIAN_POINT('Ctrl Pts',(81.1132740448054,-10.7284955019295,133.034732179979));
#73308=CARTESIAN_POINT('Ctrl Pts',(81.0520618587254,-10.7649825517311,133.030872777257));
#73309=CARTESIAN_POINT('Ctrl Pts',(80.9908150138248,-10.8014902607869,133.02701118931));
#73310=CARTESIAN_POINT('Ctrl Pts',(80.9277204900953,-10.8347735922872,133.023149601363));
#73311=CARTESIAN_POINT('Ctrl Pts',(80.8631555438839,-10.8646608457204,133.019288013416));
#73312=CARTESIAN_POINT('Ctrl Pts',(80.7984776389848,-10.8946003879747,133.015419669482));
#73313=CARTESIAN_POINT('Ctrl Pts',(80.732324626437,-10.9211318087839,133.011551325549));
#73314=CARTESIAN_POINT('Ctrl Pts',(80.6650921565283,-10.9441321935055,133.007682981616));
#73315=CARTESIAN_POINT('Ctrl Pts',(80.6251714506786,-10.9577891600597,133.005386070309));
#73316=CARTESIAN_POINT('Ctrl Pts',(80.5848704458191,-10.9702021689855,133.003089159003));
#73317=CARTESIAN_POINT('Ctrl Pts',(80.5442736622039,-10.981354017618,133.000792247696));
#73318=CARTESIAN_POINT('Ctrl Pts',(80.4758895157697,-11.0001389947021,132.996923164849));
#73319=CARTESIAN_POINT('Ctrl Pts',(80.4063977765706,-11.0154163084819,132.993054082002));
#73320=CARTESIAN_POINT('Ctrl Pts',(80.3361915931483,-11.027060131125,132.989184999155));
#73321=CARTESIAN_POINT('Ctrl Pts',(80.266090013438,-11.038686605053,132.985321681049));
#73322=CARTESIAN_POINT('Ctrl Pts',(80.1952765778128,-11.0466902550951,132.981458362943));
#73323=CARTESIAN_POINT('Ctrl Pts',(80.1241580504815,-11.0509954512384,132.977595044836));
#73324=CARTESIAN_POINT('Ctrl Pts',(80.0531229451553,-11.0552955973883,132.9737362584));
#73325=CARTESIAN_POINT('Ctrl Pts',(79.9817839415209,-11.0559058777313,132.969877471965));
#73326=CARTESIAN_POINT('Ctrl Pts',(79.9105546785685,-11.0528022547177,132.966018685529));
#73327=CARTESIAN_POINT('Ctrl Pts',(79.8393702848288,-11.049700586759,132.962162329846));
#73328=CARTESIAN_POINT('Ctrl Pts',(79.7682959787965,-11.0428896780456,132.958305974162));
#73329=CARTESIAN_POINT('Ctrl Pts',(79.6977456893856,-11.0323975728718,132.954449618479));
#73330=CARTESIAN_POINT('Ctrl Pts',(79.6272162412367,-11.0219085671709,132.950594402002));
#73331=CARTESIAN_POINT('Ctrl Pts',(79.5572109826255,-11.0077405953441,132.946739185525));
#73332=CARTESIAN_POINT('Ctrl Pts',(79.4881372810349,-10.9899733966648,132.942883969048));
#73333=CARTESIAN_POINT('Ctrl Pts',(79.4190608788692,-10.9722055033412,132.939028601843));
#73334=CARTESIAN_POINT('Ctrl Pts',(79.3509165759533,-10.9508382269336,132.935173234638));
#73335=CARTESIAN_POINT('Ctrl Pts',(79.28409844135,-10.92600169284,132.931317867434));
#73336=CARTESIAN_POINT('Ctrl Pts',(79.2172103663801,-10.9011391616677,132.927458464711));
#73337=CARTESIAN_POINT('Ctrl Pts',(79.1516516870319,-10.8728002933874,132.923599061988));
#73338=CARTESIAN_POINT('Ctrl Pts',(79.0877974244997,-10.8411637688567,132.919739659265));
#73339=CARTESIAN_POINT('Ctrl Pts',(79.0239070071824,-10.8095093314772,132.915878071318));
#73340=CARTESIAN_POINT('Ctrl Pts',(78.9617233514698,-10.7745537590656,132.912016483371));
#73341=CARTESIAN_POINT('Ctrl Pts',(78.9015953250592,-10.7365208701793,132.908154895425));
#73342=CARTESIAN_POINT('Ctrl Pts',(78.8413621025112,-10.6984214413906,132.904286551491));
#73343=CARTESIAN_POINT('Ctrl Pts',(78.7831920861634,-10.6572342278724,132.900418207558));
#73344=CARTESIAN_POINT('Ctrl Pts',(78.7274031336022,-10.6132249620355,132.896549863624));
#73345=CARTESIAN_POINT('Ctrl Pts',(78.6942772590379,-10.5870935264582,132.894252952318));
#73346=CARTESIAN_POINT('Ctrl Pts',(78.661990207726,-10.5599678909665,132.891956041011));
#73347=CARTESIAN_POINT('Ctrl Pts',(78.6306022743163,-10.5319097334348,132.889659129705));
#73348=CARTESIAN_POINT('Ctrl Pts',(78.5772314750468,-10.4842007532368,132.885753552658));
#73349=CARTESIAN_POINT('Ctrl Pts',(78.5262345230158,-10.4335895840301,132.881847975611));
#73350=CARTESIAN_POINT('Ctrl Pts',(78.4779491498061,-10.3803473374206,132.877942398564));
#73351=CARTESIAN_POINT('Ctrl Pts',(78.4309056772216,-10.3284744823049,132.874137273026));
#73352=CARTESIAN_POINT('Ctrl Pts',(78.386436362009,-10.2741046430855,132.870332147487));
#73353=CARTESIAN_POINT('Ctrl Pts',(78.3448201620121,-10.2175291645042,132.866527021949));
#73354=CARTESIAN_POINT('Ctrl Pts',(78.3032434930469,-10.1610074267026,132.862725510881));
#73355=CARTESIAN_POINT('Ctrl Pts',(78.264514863504,-10.102284603711,132.858923999814));
#73356=CARTESIAN_POINT('Ctrl Pts',(78.2288739527537,-10.0416861750382,132.855122488746));
#73357=CARTESIAN_POINT('Ctrl Pts',(78.1932541443473,-9.981123625608,132.851323228485));
#73358=CARTESIAN_POINT('Ctrl Pts',(78.1607186828808,-9.91868810415967,132.847523968224));
#73359=CARTESIAN_POINT('Ctrl Pts',(78.1314636677263,-9.85473360614478,132.843724707962));
#73360=CARTESIAN_POINT('Ctrl Pts',(78.1007916228991,-9.78768133426415,132.839741422347));
#73361=CARTESIAN_POINT('Ctrl Pts',(78.073726197892,-9.71895970058232,132.835758136732));
#73362=CARTESIAN_POINT('Ctrl Pts',(78.0504379098929,-9.64900325062141,132.831774851116));
#73363=CARTESIAN_POINT('Ctrl Pts',(78.02821733148,-9.58225412840588,132.827974189155));
#73364=CARTESIAN_POINT('Ctrl Pts',(78.0094352320241,-9.51438146381125,132.824173527193));
#73365=CARTESIAN_POINT('Ctrl Pts',(77.9941886715373,-9.44577850678409,132.820372865231));
#73366=CARTESIAN_POINT('Ctrl Pts',(77.9789361563188,-9.37714875602829,132.816570718874));
#73367=CARTESIAN_POINT('Ctrl Pts',(77.967222012663,-9.30778863950404,132.812768572516));
#73368=CARTESIAN_POINT('Ctrl Pts',(77.9590918603005,-9.23809982740112,132.808966426159));
#73369=CARTESIAN_POINT('Ctrl Pts',(77.9509517006751,-9.16832523655263,132.805159599806));
#73370=CARTESIAN_POINT('Ctrl Pts',(77.9464043599199,-9.09822164285832,132.801352773453));
#73371=CARTESIAN_POINT('Ctrl Pts',(77.9454434209989,-9.02819266187148,132.797545947101));
#73372=CARTESIAN_POINT('Ctrl Pts',(77.9453070553061,-9.01825493294981,132.797005724927));
#73373=CARTESIAN_POINT('Ctrl Pts',(77.9452428274764,-9.00831870003405,132.796465502753));
#73374=CARTESIAN_POINT('Ctrl Pts',(77.9452506345969,-8.99838510821483,132.795925280579));
#73375=CARTESIAN_POINT('Ctrl Pts',(77.9452506345975,-8.99838510746551,132.795925280538));
#73376=CARTESIAN_POINT('Ctrl Pts',(77.9453344508848,-8.8917393341807,132.790125524263));
#73377=CARTESIAN_POINT('Ctrl Pts',(77.9537227446016,-8.7854126555166,132.784325767988));
#73378=CARTESIAN_POINT('Ctrl Pts',(77.9702575839437,-8.68040136583243,132.778526011713));
#73379=CARTESIAN_POINT('Ctrl Pts',(77.9812881618236,-8.61034714969089,132.774656928866));
#73380=CARTESIAN_POINT('Ctrl Pts',(77.9959713625728,-8.54072745600456,132.770787846019));
#73381=CARTESIAN_POINT('Ctrl Pts',(78.0142600200556,-8.47195237473287,132.766918763172));
#73382=CARTESIAN_POINT('Ctrl Pts',(78.0325214283508,-8.40327976490233,132.763055445066));
#73383=CARTESIAN_POINT('Ctrl Pts',(78.0543775063822,-8.33544973518021,132.75919212696));
#73384=CARTESIAN_POINT('Ctrl Pts',(78.0797297357171,-8.26886412028216,132.755328808853));
#73385=CARTESIAN_POINT('Ctrl Pts',(78.1050522268967,-8.20235661028468,132.751470022417));
#73386=CARTESIAN_POINT('Ctrl Pts',(78.1338625514209,-8.13709106744276,132.747611235982));
#73387=CARTESIAN_POINT('Ctrl Pts',(78.1660123424268,-8.07345435386632,132.743752449546));
#73388=CARTESIAN_POINT('Ctrl Pts',(78.1981418814219,-8.00985772675313,132.739896093862));
#73389=CARTESIAN_POINT('Ctrl Pts',(78.2336064948159,-7.94788832581778,132.736039738179));
#73390=CARTESIAN_POINT('Ctrl Pts',(78.2722102319604,-7.88791183804621,132.732183382496));
#73391=CARTESIAN_POINT('Ctrl Pts',(78.3108025651744,-7.82795306792971,132.728328166019));
#73392=CARTESIAN_POINT('Ctrl Pts',(78.352531918358,-7.76998645045226,132.724472949542));
#73393=CARTESIAN_POINT('Ctrl Pts',(78.3971579299849,-7.71435041279142,132.720617733064));
#73394=CARTESIAN_POINT('Ctrl Pts',(78.4417856863553,-7.65871219992794,132.71676236586));
#73395=CARTESIAN_POINT('Ctrl Pts',(78.4893100203424,-7.60540512535013,132.712906998655));
#73396=CARTESIAN_POINT('Ctrl Pts',(78.5394501256201,-7.55473475550368,132.709051631451));
#73397=CARTESIAN_POINT('Ctrl Pts',(78.5896427139156,-7.50401134759714,132.705192228728));
#73398=CARTESIAN_POINT('Ctrl Pts',(78.6424561967729,-7.45593049983249,132.701332826005));
#73399=CARTESIAN_POINT('Ctrl Pts',(78.6975733581745,-7.41076043179036,132.697473423282));
#73400=CARTESIAN_POINT('Ctrl Pts',(78.7527217273459,-7.36556478810086,132.693611835335));
#73401=CARTESIAN_POINT('Ctrl Pts',(78.8101759802005,-7.32328349307188,132.689750247388));
#73402=CARTESIAN_POINT('Ctrl Pts',(78.8695885307939,-7.28414235066328,132.685888659441));
#73403=CARTESIAN_POINT('Ctrl Pts',(78.9291050257741,-7.24493272942309,132.682020315508));
#73404=CARTESIAN_POINT('Ctrl Pts',(78.9905862396583,-7.20887447518602,132.678151971575));
#73405=CARTESIAN_POINT('Ctrl Pts',(79.0536591538174,-7.1761478773359,132.674283627641));
#73406=CARTESIAN_POINT('Ctrl Pts',(79.091110035165,-7.1567157653218,132.671986716335));
#73407=CARTESIAN_POINT('Ctrl Pts',(79.1291216747153,-7.13845736884238,132.669689805028));
#73408=CARTESIAN_POINT('Ctrl Pts',(79.1676130426289,-7.1214022474999,132.667392893722));
#73409=CARTESIAN_POINT('Ctrl Pts',(79.2324506752053,-7.0926733726614,132.663523810875));
#73410=CARTESIAN_POINT('Ctrl Pts',(79.2989043618555,-7.06724886354418,132.659654728028));
#73411=CARTESIAN_POINT('Ctrl Pts',(79.3666039904559,-7.04531151904103,132.655785645181));
#73412=CARTESIAN_POINT('Ctrl Pts',(79.4342027499861,-7.02340686008714,132.651922327075));
#73413=CARTESIAN_POINT('Ctrl Pts',(79.503043308219,-7.0049792009511,132.648059008968));
#73414=CARTESIAN_POINT('Ctrl Pts',(79.5727346360592,-6.99016372028054,132.644195690862));
#73415=CARTESIAN_POINT('Ctrl Pts',(79.6423442159988,-6.97536561816309,132.640336904426));
#73416=CARTESIAN_POINT('Ctrl Pts',(79.7128021104156,-6.96417137875143,132.63647811799));
#73417=CARTESIAN_POINT('Ctrl Pts',(79.7837028323883,-6.95666618053164,132.632619331554));
#73418=CARTESIAN_POINT('Ctrl Pts',(79.8545588921051,-6.94916571003639,132.628762975871));
#73419=CARTESIAN_POINT('Ctrl Pts',(79.9258567440053,-6.9453497213157,132.624906620188));
#73420=CARTESIAN_POINT('Ctrl Pts',(79.9971828825805,-6.94525193117272,132.621050264504));
#73421=CARTESIAN_POINT('Ctrl Pts',(80.0684879507002,-6.94515416991792,132.617195048027));
#73422=CARTESIAN_POINT('Ctrl Pts',(80.1398208033875,-6.9487724272913,132.61333983155));
#73423=CARTESIAN_POINT('Ctrl Pts',(80.2107667494145,-6.95608832386494,132.609484615073));
#73424=CARTESIAN_POINT('Ctrl Pts',(80.2817154692159,-6.96340450646825,132.605629247868));
#73425=CARTESIAN_POINT('Ctrl Pts',(80.3522767693298,-6.97441856326924,132.601773880663));
#73426=CARTESIAN_POINT('Ctrl Pts',(80.422041629453,-6.98906031281177,132.597918513459));
#73427=CARTESIAN_POINT('Ctrl Pts',(80.4918795143608,-7.00371738827347,132.594059110736));
#73428=CARTESIAN_POINT('Ctrl Pts',(80.5609188187151,-7.02200963656564,132.590199708013));
#73429=CARTESIAN_POINT('Ctrl Pts',(80.6287621506491,-7.04381603104128,132.58634030529));
#73430=CARTESIAN_POINT('Ctrl Pts',(80.6966438960106,-7.06563477246877,132.582478717343));
#73431=CARTESIAN_POINT('Ctrl Pts',(80.7633278665928,-7.09097144841154,132.578617129396));
#73432=CARTESIAN_POINT('Ctrl Pts',(80.8284358332442,-7.11965651204441,132.57475554145));
#73433=CARTESIAN_POINT('Ctrl Pts',(80.8936577086169,-7.14839176122426,132.570887197516));
#73434=CARTESIAN_POINT('Ctrl Pts',(80.9572976411984,-7.18048687518794,132.567018853583));
#73435=CARTESIAN_POINT('Ctrl Pts',(81.0190018459504,-7.21572625406032,132.563150509649));
#73436=CARTESIAN_POINT('Ctrl Pts',(81.0556400270383,-7.23665038313284,132.560853598343));
#73437=CARTESIAN_POINT('Ctrl Pts',(81.0915962750952,-7.25868222392753,132.558556687036));
#73438=CARTESIAN_POINT('Ctrl Pts',(81.1268018071313,-7.28176973314236,132.55625977573));
#73439=CARTESIAN_POINT('Ctrl Pts',(81.1695802911759,-7.3098235243353,132.553468783008));
#73440=CARTESIAN_POINT('Ctrl Pts',(81.211370811523,-7.33951543903302,132.550677790287));
#73441=CARTESIAN_POINT('Ctrl Pts',(81.2520391107129,-7.3707683934611,132.547886797565));
#73442=CARTESIAN_POINT('',(77.9452507493435,-9.00175482953772,132.854074719498));
#73443=CARTESIAN_POINT('Ctrl Pts',(77.945250749343,-9.00175482886545,132.854074719462));
#73444=CARTESIAN_POINT('Ctrl Pts',(77.9451902335234,-8.93089616152734,132.850240467841));
#73445=CARTESIAN_POINT('Ctrl Pts',(77.9487993838056,-8.85997312348533,132.846406216221));
#73446=CARTESIAN_POINT('Ctrl Pts',(77.9560714877068,-8.78939658327859,132.8425719646));
#73447=CARTESIAN_POINT('Ctrl Pts',(77.9633409049725,-8.7188461171535,132.838739129521));
#73448=CARTESIAN_POINT('Ctrl Pts',(77.9742705404255,-8.64864238372495,132.834906294442));
#73449=CARTESIAN_POINT('Ctrl Pts',(77.9888017188309,-8.57919239987539,132.831073459363));
#73450=CARTESIAN_POINT('Ctrl Pts',(78.0033325301935,-8.50974417026249,132.827240721097));
#73451=CARTESIAN_POINT('Ctrl Pts',(78.0214646012841,-8.4410501334779,132.823407982832));
#73452=CARTESIAN_POINT('Ctrl Pts',(78.0430882613476,-8.37350657655141,132.819575244566));
#73453=CARTESIAN_POINT('Ctrl Pts',(78.0647340638347,-8.30589385566048,132.815738581613));
#73454=CARTESIAN_POINT('Ctrl Pts',(78.0898784440367,-8.23943443646795,132.811901918659));
#73455=CARTESIAN_POINT('Ctrl Pts',(78.1183622815556,-8.17450798972523,132.808065255706));
#73456=CARTESIAN_POINT('Ctrl Pts',(78.1468610721472,-8.10954745874536,132.804226578632));
#73457=CARTESIAN_POINT('Ctrl Pts',(78.178702588492,-8.04612194192218,132.800387901557));
#73458=CARTESIAN_POINT('Ctrl Pts',(78.2136813665786,-7.98458712712931,132.796549224483));
#73459=CARTESIAN_POINT('Ctrl Pts',(78.2487243400167,-7.92293937960173,132.792703502416));
#73460=CARTESIAN_POINT('Ctrl Pts',(78.2869158076438,-7.86318967817087,132.788857780349));
#73461=CARTESIAN_POINT('Ctrl Pts',(78.3280069113267,-7.80566475647388,132.785012058282));
#73462=CARTESIAN_POINT('Ctrl Pts',(78.3588674553701,-7.76246196510268,132.782123815704));
#73463=CARTESIAN_POINT('Ctrl Pts',(78.3913626087628,-7.72051343395676,132.779235573126));
#73464=CARTESIAN_POINT('Ctrl Pts',(78.4253729722412,-7.67994421104584,132.776347330549));
#73465=CARTESIAN_POINT('Ctrl Pts',(78.4709331737854,-7.62559777709811,132.772478247702));
#73466=CARTESIAN_POINT('Ctrl Pts',(78.5193994699273,-7.57350635485296,132.768609164855));
#73467=CARTESIAN_POINT('Ctrl Pts',(78.5705200716172,-7.52399705391533,132.764740082008));
#73468=CARTESIAN_POINT('Ctrl Pts',(78.62156450616,-7.47456151936696,132.760876763902));
#73469=CARTESIAN_POINT('Ctrl Pts',(78.675255050003,-7.42770080468091,132.757013445795));
#73470=CARTESIAN_POINT('Ctrl Pts',(78.7313001635042,-7.38370847698331,132.753150127689));
#73471=CARTESIAN_POINT('Ctrl Pts',(78.7872795361089,-7.33976775226914,132.749291341253));
#73472=CARTESIAN_POINT('Ctrl Pts',(78.8456076120165,-7.29868902976494,132.745432554817));
#73473=CARTESIAN_POINT('Ctrl Pts',(78.905957852007,-7.26072735291014,132.741573768381));
#73474=CARTESIAN_POINT('Ctrl Pts',(78.9662700757718,-7.22278958912815,132.737717412698));
#73475=CARTESIAN_POINT('Ctrl Pts',(79.0286015261643,-7.18796523346361,132.733861057015));
#73476=CARTESIAN_POINT('Ctrl Pts',(79.0925958019738,-7.15646665777254,132.730004701331));
#73477=CARTESIAN_POINT('Ctrl Pts',(79.1565711732334,-7.1249773870761,132.726149484854));
#73478=CARTESIAN_POINT('Ctrl Pts',(79.2222079591014,-7.09681216029129,132.722294268377));
#73479=CARTESIAN_POINT('Ctrl Pts',(79.2891257515506,-7.07213709891199,132.7184390519));
#73480=CARTESIAN_POINT('Ctrl Pts',(79.3560461602854,-7.04746107281158,132.714583684695));
#73481=CARTESIAN_POINT('Ctrl Pts',(79.424247218489,-7.02627564902794,132.710728317491));
#73482=CARTESIAN_POINT('Ctrl Pts',(79.4933307968454,-7.00869794328568,132.706872950286));
#73483=CARTESIAN_POINT('Ctrl Pts',(79.56248668687,-6.99110183847875,132.703013547563));
#73484=CARTESIAN_POINT('Ctrl Pts',(79.6325264693278,-6.97712111008018,132.69915414484));
#73485=CARTESIAN_POINT('Ctrl Pts',(79.7030400637036,-6.96682210352,132.695294742118));
#73486=CARTESIAN_POINT('Ctrl Pts',(79.7735935834305,-6.9565172655814,132.691433154171));
#73487=CARTESIAN_POINT('Ctrl Pts',(79.8446209652136,-6.94989834441169,132.687571566224));
#73488=CARTESIAN_POINT('Ctrl Pts',(79.9157079655863,-6.94697968460261,132.683709978277));
#73489=CARTESIAN_POINT('Ctrl Pts',(79.9869193352142,-6.94405591849357,132.679841634343));
#73490=CARTESIAN_POINT('Ctrl Pts',(80.0581900457724,-6.94484533336773,132.67597329041));
#73491=CARTESIAN_POINT('Ctrl Pts',(80.129107519016,-6.94931016215676,132.672104946476));
#73492=CARTESIAN_POINT('Ctrl Pts',(80.1712162738,-6.95196124900504,132.66980803517));
#73493=CARTESIAN_POINT('Ctrl Pts',(80.2132005988818,-6.95590716216112,132.667511123864));
#73494=CARTESIAN_POINT('Ctrl Pts',(80.2549758212292,-6.96113146743384,132.665214212557));
#73495=CARTESIAN_POINT('Ctrl Pts',(80.3253420978987,-6.96993129875895,132.661345290086));
#73496=CARTESIAN_POINT('Ctrl Pts',(80.3953900995648,-6.98239540609979,132.657476367615));
#73497=CARTESIAN_POINT('Ctrl Pts',(80.4647084963175,-6.99848967628185,132.653607445144));
#73498=CARTESIAN_POINT('Ctrl Pts',(80.5356580114459,-7.01496265775943,132.649647483774));
#73499=CARTESIAN_POINT('Ctrl Pts',(80.6058426319329,-7.03523884401316,132.645687522404));
#73500=CARTESIAN_POINT('Ctrl Pts',(80.6748265781646,-7.05922524441845,132.641727561034));
#73501=CARTESIAN_POINT('Ctrl Pts',(80.7420453191852,-7.08259786551268,132.63786892968));
#73502=CARTESIAN_POINT('Ctrl Pts',(80.8081236067996,-7.10949292659595,132.634010298327));
#73503=CARTESIAN_POINT('Ctrl Pts',(80.872670498717,-7.1397731957718,132.630151666974));
#73504=CARTESIAN_POINT('Ctrl Pts',(80.9397599518661,-7.17124623250323,132.626141040595));
#73505=CARTESIAN_POINT('Ctrl Pts',(81.0051943257724,-7.20637657914342,132.622130414216));
#73506=CARTESIAN_POINT('Ctrl Pts',(81.0685566253344,-7.24495461569964,132.618119787838));
#73507=CARTESIAN_POINT('Ctrl Pts',(81.1319189248964,-7.28353265225587,132.614109161459));
#73508=CARTESIAN_POINT('Ctrl Pts',(81.1932086344546,-7.3255580888724,132.61009853508));
#73509=CARTESIAN_POINT('Ctrl Pts',(81.2520391107129,-7.37076839346111,132.606087908702));
#73510=CARTESIAN_POINT('Ctrl Pts',(81.2520391107129,-7.37076839346111,133.306011340568));
#73511=CARTESIAN_POINT('Ctrl Pts',(81.3084857799458,-7.41414677948397,133.302153261449));
#73512=CARTESIAN_POINT('Ctrl Pts',(81.3627336375113,-7.46050680788434,133.298295182331));
#73513=CARTESIAN_POINT('Ctrl Pts',(81.414455974713,-7.50959339168848,133.294437103213));
#73514=CARTESIAN_POINT('Ctrl Pts',(81.4661499207835,-7.55865303116414,133.29058114185));
#73515=CARTESIAN_POINT('Ctrl Pts',(81.5153207454392,-7.61043592261164,133.286725180486));
#73516=CARTESIAN_POINT('Ctrl Pts',(81.5616759656113,-7.66464770905503,133.282869219123));
#73517=CARTESIAN_POINT('Ctrl Pts',(81.6080212472215,-7.71884787248822,133.279014084478));
#73518=CARTESIAN_POINT('Ctrl Pts',(81.6515518076407,-7.77547552757596,133.275158949833));
#73519=CARTESIAN_POINT('Ctrl Pts',(81.6920142694605,-7.83420187234587,133.271303815188));
#73520=CARTESIAN_POINT('Ctrl Pts',(81.7324815910096,-7.89293527042191,133.267448217523));
#73521=CARTESIAN_POINT('Ctrl Pts',(81.7698798089391,-7.95376745712211,133.263592619859));
#73522=CARTESIAN_POINT('Ctrl Pts',(81.8039988352567,-8.0163406255758,133.259737022194));
#73523=CARTESIAN_POINT('Ctrl Pts',(81.8381552721333,-8.07898240376049,133.255877196974));
#73524=CARTESIAN_POINT('Ctrl Pts',(81.8690251105619,-8.14336854525437,133.252017371755));
#73525=CARTESIAN_POINT('Ctrl Pts',(81.8964446627459,-8.20911745268799,133.248157546535));
#73526=CARTESIAN_POINT('Ctrl Pts',(81.9238817319164,-8.27490836382467,133.244295255465));
#73527=CARTESIAN_POINT('Ctrl Pts',(81.9478639656512,-8.342063315957,133.240432964395));
#73528=CARTESIAN_POINT('Ctrl Pts',(81.968277124051,-8.41018415972663,133.236570673326));
#73529=CARTESIAN_POINT('Ctrl Pts',(81.9887245108757,-8.47841922732844,133.232701906034));
#73530=CARTESIAN_POINT('Ctrl Pts',(82.005590767028,-8.54762294683034,133.228833138743));
#73531=CARTESIAN_POINT('Ctrl Pts',(82.0188126251097,-8.61738642575352,133.224964371451));
#73532=CARTESIAN_POINT('Ctrl Pts',(82.023465751608,-8.64193806519704,133.223602848472));
#73533=CARTESIAN_POINT('Ctrl Pts',(82.0276679805648,-8.66655898766611,133.222241325494));
#73534=CARTESIAN_POINT('Ctrl Pts',(82.0314180869268,-8.69123128622436,133.220879802515));
#73535=CARTESIAN_POINT('Ctrl Pts',(82.0420748826076,-8.7613433362115,133.217010719668));
#73536=CARTESIAN_POINT('Ctrl Pts',(82.0491185350753,-8.83214506707416,133.213141636821));
#73537=CARTESIAN_POINT('Ctrl Pts',(82.0524700687833,-8.90323131059755,133.209272553974));
#73538=CARTESIAN_POINT('Ctrl Pts',(82.0558166088733,-8.97421163916328,133.205409235868));
#73539=CARTESIAN_POINT('Ctrl Pts',(82.0554819269895,-9.0454751576497,133.201545917761));
#73540=CARTESIAN_POINT('Ctrl Pts',(82.0514384934808,-9.11660904752696,133.197682599655));
#73541=CARTESIAN_POINT('Ctrl Pts',(82.0473998029181,-9.18765949737885,133.193823813219));
#73542=CARTESIAN_POINT('Ctrl Pts',(82.0396610294618,-9.2585801380065,133.189965026783));
#73543=CARTESIAN_POINT('Ctrl Pts',(82.0282466859119,-9.32895735831159,133.186106240347));
#73544=CARTESIAN_POINT('Ctrl Pts',(82.0168395325615,-9.39929024612842,133.182249884664));
#73545=CARTESIAN_POINT('Ctrl Pts',(82.0017614803033,-9.46907991438652,133.178393528981));
#73546=CARTESIAN_POINT('Ctrl Pts',(81.9830888001475,-9.53791855631631,133.174537173298));
#73547=CARTESIAN_POINT('Ctrl Pts',(81.9644216360885,-9.60673686262192,133.17068195682));
#73548=CARTESIAN_POINT('Ctrl Pts',(81.9421620793816,-9.67460423176284,133.166826740343));
#73549=CARTESIAN_POINT('Ctrl Pts',(81.9164369736022,-9.74112542036437,133.162971523866));
#73550=CARTESIAN_POINT('Ctrl Pts',(81.8907108620482,-9.8076492097454,133.159116156661));
#73551=CARTESIAN_POINT('Ctrl Pts',(81.8615191096899,-9.87282626180524,133.155260789457));
#73552=CARTESIAN_POINT('Ctrl Pts',(81.8290370447409,-9.9362804341999,133.151405422252));
#73553=CARTESIAN_POINT('Ctrl Pts',(81.7965209799272,-9.99980102581,133.147546019529));
#73554=CARTESIAN_POINT('Ctrl Pts',(81.7607079492157,-10.0615947044879,133.143686616806));
#73555=CARTESIAN_POINT('Ctrl Pts',(81.7218192748204,-10.1213099247562,133.139827214084));
#73556=CARTESIAN_POINT('Ctrl Pts',(81.6829085813523,-10.1810589562513,133.135965626137));
#73557=CARTESIAN_POINT('Ctrl Pts',(81.6409190635822,-10.2387267937158,133.13210403819));
#73558=CARTESIAN_POINT('Ctrl Pts',(81.5961138122492,-10.2939931455951,133.128242450243));
#73559=CARTESIAN_POINT('Ctrl Pts',(81.551230172523,-10.349356187938,133.124374106309));
#73560=CARTESIAN_POINT('Ctrl Pts',(81.5035212891509,-10.4023089952922,133.120505762376));
#73561=CARTESIAN_POINT('Ctrl Pts',(81.4532882515811,-10.4525669761895,133.116637418443));
#73562=CARTESIAN_POINT('Ctrl Pts',(81.4234613194531,-10.4824087189476,133.114340507136));
#73563=CARTESIAN_POINT('Ctrl Pts',(81.392745133871,-10.5113011007561,133.11204359583));
#73564=CARTESIAN_POINT('Ctrl Pts',(81.3612080022368,-10.5391914556502,133.109746684523));
#73565=CARTESIAN_POINT('Ctrl Pts',(81.3080845861498,-10.5861719783254,133.105877601676));
#73566=CARTESIAN_POINT('Ctrl Pts',(81.2524220485734,-10.6304910492068,133.102008518829));
#73567=CARTESIAN_POINT('Ctrl Pts',(81.1945179499447,-10.6718625630595,133.098139435982));
#73568=CARTESIAN_POINT('Ctrl Pts',(81.136700125535,-10.7131724354199,133.094276117876));
#73569=CARTESIAN_POINT('Ctrl Pts',(81.0766477615528,-10.7515431880736,133.09041279977));
#73570=CARTESIAN_POINT('Ctrl Pts',(81.0146927489592,-10.7867277878036,133.086549481663));
#73571=CARTESIAN_POINT('Ctrl Pts',(80.9528104095716,-10.8218711160117,133.082690695227));
#73572=CARTESIAN_POINT('Ctrl Pts',(80.8890302750626,-10.8538354762219,133.078831908792));
#73573=CARTESIAN_POINT('Ctrl Pts',(80.8237131290574,-10.8824171279285,133.074973122356));
#73574=CARTESIAN_POINT('Ctrl Pts',(80.7584371280646,-10.9109807752904,133.071116766673));
#73575=CARTESIAN_POINT('Ctrl Pts',(80.6916264804665,-10.9361657474567,133.067260410989));
#73576=CARTESIAN_POINT('Ctrl Pts',(80.6236651661146,-10.9578149358597,133.063404055306));
#73577=CARTESIAN_POINT('Ctrl Pts',(80.5557239282157,-10.9794577288756,133.059548838829));
#73578=CARTESIAN_POINT('Ctrl Pts',(80.486633161009,-10.9975666643961,133.055693622352));
#73579=CARTESIAN_POINT('Ctrl Pts',(80.4167937189864,-11.0120339356764,133.051838405874));
#73580=CARTESIAN_POINT('Ctrl Pts',(80.3469515464505,-11.0265017725837,133.04798303867));
#73581=CARTESIAN_POINT('Ctrl Pts',(80.2763611171161,-11.0373275661965,133.044127671465));
#73582=CARTESIAN_POINT('Ctrl Pts',(80.2054335351808,-11.0444546033412,133.040272304261));
#73583=CARTESIAN_POINT('Ctrl Pts',(80.1344317114082,-11.0515891005504,133.036412901538));
#73584=CARTESIAN_POINT('Ctrl Pts',(80.0630925148929,-11.0550170640636,133.032553498815));
#73585=CARTESIAN_POINT('Ctrl Pts',(79.9918313314322,-11.0547337626451,133.028694096092));
#73586=CARTESIAN_POINT('Ctrl Pts',(79.9205297993297,-11.0544503008192,133.024832508145));
#73587=CARTESIAN_POINT('Ctrl Pts',(79.8493068534627,-11.050451418172,133.020970920198));
#73588=CARTESIAN_POINT('Ctrl Pts',(79.7785742766001,-11.0427844261,133.017109332251));
#73589=CARTESIAN_POINT('Ctrl Pts',(79.7077179505589,-11.0351040203506,133.013240988318));
#73590=CARTESIAN_POINT('Ctrl Pts',(79.6373541861036,-11.0237427699366,133.009372644385));
#73591=CARTESIAN_POINT('Ctrl Pts',(79.5678853829314,-11.0087992732515,133.005504300451));
#73592=CARTESIAN_POINT('Ctrl Pts',(79.526636806746,-10.9999262549563,133.003207389145));
#73593=CARTESIAN_POINT('Ctrl Pts',(79.4857035065239,-10.989791230724,133.000910477838));
#73594=CARTESIAN_POINT('Ctrl Pts',(79.4451667772748,-10.9784230228797,132.998613566532));
#73595=CARTESIAN_POINT('Ctrl Pts',(79.3768837907402,-10.9592735947553,132.994744483685));
#73596=CARTESIAN_POINT('Ctrl Pts',(79.309459608366,-10.9365474476032,132.990875400838));
#73597=CARTESIAN_POINT('Ctrl Pts',(79.2432959875487,-10.9103393939403,132.987006317991));
#73598=CARTESIAN_POINT('Ctrl Pts',(79.1772309472266,-10.8841703889702,132.983142999885));
#73599=CARTESIAN_POINT('Ctrl Pts',(79.1124231883006,-10.8545299527042,132.979279681778));
#73600=CARTESIAN_POINT('Ctrl Pts',(79.0492602626734,-10.8215629317617,132.975416363672));
#73601=CARTESIAN_POINT('Ctrl Pts',(78.9861714271336,-10.7886345811219,132.971557577236));
#73602=CARTESIAN_POINT('Ctrl Pts',(78.9247240210361,-10.7523876203454,132.9676987908));
#73603=CARTESIAN_POINT('Ctrl Pts',(78.8652848954573,-10.7130146508488,132.963840004364));
#73604=CARTESIAN_POINT('Ctrl Pts',(78.8058832121691,-10.6736664834359,132.959983648681));
#73605=CARTESIAN_POINT('Ctrl Pts',(78.7484877035544,-10.6311964817129,132.956127292998));
#73606=CARTESIAN_POINT('Ctrl Pts',(78.6934386248326,-10.5858420272589,132.952270937314));
#73607=CARTESIAN_POINT('Ctrl Pts',(78.6384058081598,-10.5405009709649,132.948415720837));
#73608=CARTESIAN_POINT('Ctrl Pts',(78.5857184199869,-10.4922774623159,132.94456050436));
#73609=CARTESIAN_POINT('Ctrl Pts',(78.5356844479139,-10.441449800173,132.940705287883));
#73610=CARTESIAN_POINT('Ctrl Pts',(78.4856485196625,-10.3906201508208,132.936849920678));
#73611=CARTESIAN_POINT('Ctrl Pts',(78.4382665526913,-10.3371864935733,132.932994553474));
#73612=CARTESIAN_POINT('Ctrl Pts',(78.3938091684396,-10.2814634505562,132.929139186269));
#73613=CARTESIAN_POINT('Ctrl Pts',(78.3493052494292,-10.2256820807076,132.925279783546));
#73614=CARTESIAN_POINT('Ctrl Pts',(78.3077323276445,-10.1676069219255,132.921420380823));
#73615=CARTESIAN_POINT('Ctrl Pts',(78.2693196750343,-10.1075843874291,132.917560978101));
#73616=CARTESIAN_POINT('Ctrl Pts',(78.2308852728786,-10.0475278677022,132.913699390154));
#73617=CARTESIAN_POINT('Ctrl Pts',(78.1956149422799,-9.98552219973657,132.909837802207));
#73618=CARTESIAN_POINT('Ctrl Pts',(78.1636922782394,-9.92193899662742,132.90597621426));
#73619=CARTESIAN_POINT('Ctrl Pts',(78.1317137643539,-9.85824455242537,132.902107870326));
#73620=CARTESIAN_POINT('Ctrl Pts',(78.1030948055356,-9.79296750779668,132.898239526393));
#73621=CARTESIAN_POINT('Ctrl Pts',(78.0779708196895,-9.72649940986562,132.894371182459));
#73622=CARTESIAN_POINT('Ctrl Pts',(78.0630529198994,-9.68703256609916,132.892074271153));
#73623=CARTESIAN_POINT('Ctrl Pts',(78.0493662725192,-9.64714610891388,132.889777359846));
#73624=CARTESIAN_POINT('Ctrl Pts',(78.0369307557737,-9.60692396959823,132.88748044854));
#73625=CARTESIAN_POINT('Ctrl Pts',(78.0114354604795,-9.52446054325239,132.88277132119));
#73626=CARTESIAN_POINT('Ctrl Pts',(77.9911203973392,-9.44032478764207,132.878062193839));
#73627=CARTESIAN_POINT('Ctrl Pts',(77.9761678835394,-9.35510720477408,132.873353066489));
#73628=CARTESIAN_POINT('Ctrl Pts',(77.9614177985698,-9.27104330722287,132.868707691839));
#73629=CARTESIAN_POINT('Ctrl Pts',(77.951886094498,-9.18592667450051,132.86406231719));
#73630=CARTESIAN_POINT('Ctrl Pts',(77.9477016670826,-9.10034498096334,132.85941694254));
#73631=CARTESIAN_POINT('Ctrl Pts',(77.9460976239039,-9.06753840598652,132.857636201526));
#73632=CARTESIAN_POINT('Ctrl Pts',(77.945278854709,-9.03466371179541,132.855855460512));
#73633=CARTESIAN_POINT('Ctrl Pts',(77.9452507493435,-9.00175482953773,132.854074719498));
#73634=CARTESIAN_POINT('Origin',(80.,-9.,141.545925280538));
#73635=CARTESIAN_POINT('',(81.2520391107129,-7.3707683934611,134.006113615385));
#73636=CARTESIAN_POINT('',(81.2520391107129,-7.37076839346111,133.947919788834));
#73637=CARTESIAN_POINT('',(81.2520391107129,-7.37076839346111,141.545925280538));
#73638=CARTESIAN_POINT('',(77.94525006034,-8.99950203698838,133.495925280488));
#73639=CARTESIAN_POINT('Ctrl Pts',(81.2520391107129,-7.37076839346111,133.947919788834));
#73640=CARTESIAN_POINT('Ctrl Pts',(81.3085900102766,-7.41422687886956,133.944064641566));
#73641=CARTESIAN_POINT('Ctrl Pts',(81.3628803154506,-7.46063677639288,133.940209494297));
#73642=CARTESIAN_POINT('Ctrl Pts',(81.4145961687758,-7.50972645404108,133.936354347029));
#73643=CARTESIAN_POINT('Ctrl Pts',(81.4665751616528,-7.5590659087875,133.932479584079));
#73644=CARTESIAN_POINT('Ctrl Pts',(81.5159530604065,-7.61111216160157,133.928604821129));
#73645=CARTESIAN_POINT('Ctrl Pts',(81.5624487563918,-7.66555200695202,133.924730058179));
#73646=CARTESIAN_POINT('Ctrl Pts',(81.6087738176557,-7.71979206331893,133.920869515235));
#73647=CARTESIAN_POINT('Ctrl Pts',(81.652237532106,-7.77640775807705,133.917008972292));
#73648=CARTESIAN_POINT('Ctrl Pts',(81.6926037674573,-7.83505792037144,133.913148429348));
#73649=CARTESIAN_POINT('Ctrl Pts',(81.7331930315904,-7.89403213255886,133.909266556395));
#73650=CARTESIAN_POINT('Ctrl Pts',(81.7706502273261,-7.95506293762194,133.905384683441));
#73651=CARTESIAN_POINT('Ctrl Pts',(81.8047817874466,-8.01777789568704,133.901502810488));
#73652=CARTESIAN_POINT('Ctrl Pts',(81.8389133475671,-8.08049285375215,133.897620937535));
#73653=CARTESIAN_POINT('Ctrl Pts',(81.8697191170293,-8.14489149318802,133.893739064581));
#73654=CARTESIAN_POINT('Ctrl Pts',(81.8970550143789,-8.21058259778507,133.889857191628));
#73655=CARTESIAN_POINT('Ctrl Pts',(81.9243008446297,-8.2760572614461,133.885988108781));
#73656=CARTESIAN_POINT('Ctrl Pts',(81.9482063861372,-8.34307235839047,133.882119025934));
#73657=CARTESIAN_POINT('Ctrl Pts',(81.9685973105307,-8.41125371213795,133.878249943087));
#73658=CARTESIAN_POINT('Ctrl Pts',(81.9889578534638,-8.47933347906872,133.874386624981));
#73659=CARTESIAN_POINT('Ctrl Pts',(82.0058140357402,-8.54857559196324,133.870523306875));
#73660=CARTESIAN_POINT('Ctrl Pts',(82.0190396129381,-8.61858604654963,133.866659988768));
#73661=CARTESIAN_POINT('Ctrl Pts',(82.0322496765391,-8.68851437889975,133.862801202332));
#73662=CARTESIAN_POINT('Ctrl Pts',(82.0418375045425,-8.7592087877014,133.858942415897));
#73663=CARTESIAN_POINT('Ctrl Pts',(82.0477271687752,-8.83026195252723,133.855083629461));
#73664=CARTESIAN_POINT('Ctrl Pts',(82.0536131229513,-8.9012703590693,133.851227273778));
#73665=CARTESIAN_POINT('Ctrl Pts',(82.0558054951567,-8.97263659029657,133.847370918094));
#73666=CARTESIAN_POINT('Ctrl Pts',(82.0542799880628,-9.04394648045941,133.843514562411));
#73667=CARTESIAN_POINT('Ctrl Pts',(82.052754931619,-9.11523530496674,133.839659345934));
#73668=CARTESIAN_POINT('Ctrl Pts',(82.047514186688,-9.1864673360446,133.835804129457));
#73669=CARTESIAN_POINT('Ctrl Pts',(82.0385855656644,-9.25722840816021,133.831948912979));
#73670=CARTESIAN_POINT('Ctrl Pts',(82.0296565955584,-9.32799224682206,133.828093545775));
#73671=CARTESIAN_POINT('Ctrl Pts',(82.017039526099,-9.3982846082792,133.82423817857));
#73672=CARTESIAN_POINT('Ctrl Pts',(82.0008138292302,-9.46769817538806,133.820382811366));
#73673=CARTESIAN_POINT('Ctrl Pts',(81.9845711484813,-9.53718439957352,133.816523408643));
#73674=CARTESIAN_POINT('Ctrl Pts',(81.9647124108874,-9.60578951916727,133.81266400592));
#73675=CARTESIAN_POINT('Ctrl Pts',(81.9413676557693,-9.67311899960777,133.808804603197));
#73676=CARTESIAN_POINT('Ctrl Pts',(81.9180096826674,-9.74048660252897,133.80494301525));
#73677=CARTESIAN_POINT('Ctrl Pts',(81.8911619457095,-9.80657667818826,133.801081427303));
#73678=CARTESIAN_POINT('Ctrl Pts',(81.8610025557139,-9.87101495401993,133.797219839356));
#73679=CARTESIAN_POINT('Ctrl Pts',(81.8307904007844,-9.93556596692488,133.793351495423));
#73680=CARTESIAN_POINT('Ctrl Pts',(81.7972552538553,-9.99845898147934,133.78948315149));
#73681=CARTESIAN_POINT('Ctrl Pts',(81.7606207105567,-10.0593452109953,133.785614807556));
#73682=CARTESIAN_POINT('Ctrl Pts',(81.7388681729964,-10.0954977019287,133.78331789625));
#73683=CARTESIAN_POINT('Ctrl Pts',(81.7160237303534,-10.1309432266616,133.781020984943));
#73684=CARTESIAN_POINT('Ctrl Pts',(81.6921409778438,-10.165614204444,133.778724073637));
#73685=CARTESIAN_POINT('Ctrl Pts',(81.6519111492854,-10.2240164967084,133.77485499079));
#73686=CARTESIAN_POINT('Ctrl Pts',(81.6085754448934,-10.2804480026079,133.770985907943));
#73687=CARTESIAN_POINT('Ctrl Pts',(81.5623536704284,-10.3345593171527,133.767116825096));
#73688=CARTESIAN_POINT('Ctrl Pts',(81.5162007641022,-10.3885900085374,133.76325350699));
#73689=CARTESIAN_POINT('Ctrl Pts',(81.4671706362291,-10.4403070041942,133.759390188883));
#73690=CARTESIAN_POINT('Ctrl Pts',(81.4155258303407,-10.4893905418453,133.755526870777));
#73691=CARTESIAN_POINT('Ctrl Pts',(81.3639416037897,-10.5384165045258,133.751668084341));
#73692=CARTESIAN_POINT('Ctrl Pts',(81.3097491417684,-10.5848148120564,133.747809297905));
#73693=CARTESIAN_POINT('Ctrl Pts',(81.2532494656944,-10.6283007520838,133.743950511469));
#73694=CARTESIAN_POINT('Ctrl Pts',(81.1967853802733,-10.6717592991577,133.740094155786));
#73695=CARTESIAN_POINT('Ctrl Pts',(81.1380173483262,-10.71230882291,133.736237800103));
#73696=CARTESIAN_POINT('Ctrl Pts',(81.0772801458063,-10.7497042749995,133.73238144442));
#73697=CARTESIAN_POINT('Ctrl Pts',(81.0165608856641,-10.787088680098,133.728526227942));
#73698=CARTESIAN_POINT('Ctrl Pts',(80.9538740232493,-10.8213206087536,133.724671011465));
#73699=CARTESIAN_POINT('Ctrl Pts',(80.8895825976209,-10.8521987918444,133.720815794988));
#73700=CARTESIAN_POINT('Ctrl Pts',(80.8252886583901,-10.8830781821799,133.716960427783));
#73701=CARTESIAN_POINT('Ctrl Pts',(80.7593904702462,-10.9106033582973,133.713105060579));
#73702=CARTESIAN_POINT('Ctrl Pts',(80.692273337813,-10.934620166403,133.709249693374));
#73703=CARTESIAN_POINT('Ctrl Pts',(80.625085952044,-10.9586621135578,133.705390290651));
#73704=CARTESIAN_POINT('Ctrl Pts',(80.5566775333181,-10.9791881979556,133.701530887928));
#73705=CARTESIAN_POINT('Ctrl Pts',(80.487450073939,-10.9960936821494,133.697671485206));
#73706=CARTESIAN_POINT('Ctrl Pts',(80.4181834174287,-11.0130087383612,133.693809897259));
#73707=CARTESIAN_POINT('Ctrl Pts',(80.3480972745911,-11.0262990228787,133.689948309312));
#73708=CARTESIAN_POINT('Ctrl Pts',(80.2776026879915,-11.035911174418,133.686086721365));
#73709=CARTESIAN_POINT('Ctrl Pts',(80.2069847685858,-11.0455401427608,133.682218377431));
#73710=CARTESIAN_POINT('Ctrl Pts',(80.1359574629724,-11.0514780899316,133.678350033498));
#73711=CARTESIAN_POINT('Ctrl Pts',(80.0649350722543,-11.0537236909797,133.674481689565));
#73712=CARTESIAN_POINT('Ctrl Pts',(80.0227640204922,-11.0550570642593,133.672184778258));
#73713=CARTESIAN_POINT('Ctrl Pts',(79.9805946865914,-11.055089647407,133.669887866952));
#73714=CARTESIAN_POINT('Ctrl Pts',(79.9385129163662,-11.0538298130678,133.667590955645));
#73715=CARTESIAN_POINT('Ctrl Pts',(79.8676273515257,-11.0517076573634,133.663721872798));
#73716=CARTESIAN_POINT('Ctrl Pts',(79.7967129435705,-11.0459072368963,133.659852789951));
#73717=CARTESIAN_POINT('Ctrl Pts',(79.7261824575087,-11.0364237073664,133.655983707104));
#73718=CARTESIAN_POINT('Ctrl Pts',(79.6557570583534,-11.0269543078226,133.652120388998));
#73719=CARTESIAN_POINT('Ctrl Pts',(79.585714923167,-11.0138127562554,133.648257070892));
#73720=CARTESIAN_POINT('Ctrl Pts',(79.5164670932608,-10.9970461914038,133.644393752785));
#73721=CARTESIAN_POINT('Ctrl Pts',(79.4473004910326,-10.9802992937263,133.640534966349));
#73722=CARTESIAN_POINT('Ctrl Pts',(79.3789268132231,-10.9599359427143,133.636676179914));
#73723=CARTESIAN_POINT('Ctrl Pts',(79.3117485241908,-10.9360546140402,133.632817393478));
#73724=CARTESIAN_POINT('Ctrl Pts',(79.2446125525545,-10.9121883288521,133.628961037795));
#73725=CARTESIAN_POINT('Ctrl Pts',(79.1786709323801,-10.8848086249775,133.625104682111));
#73726=CARTESIAN_POINT('Ctrl Pts',(79.1143111127732,-10.8540638493706,133.621248326428));
#73727=CARTESIAN_POINT('Ctrl Pts',(79.0499703057015,-10.8233281560783,133.617393109951));
#73728=CARTESIAN_POINT('Ctrl Pts',(78.9872108096157,-10.7892295738504,133.613537893474));
#73729=CARTESIAN_POINT('Ctrl Pts',(78.9263986226034,-10.7519639393983,133.609682676996));
#73730=CARTESIAN_POINT('Ctrl Pts',(78.8655840580166,-10.7146968479715,133.605827309792));
#73731=CARTESIAN_POINT('Ctrl Pts',(78.8067173667049,-10.6742627141862,133.601971942587));
#73732=CARTESIAN_POINT('Ctrl Pts',(78.7501370400148,-10.6309016352181,133.598116575382));
#73733=CARTESIAN_POINT('Ctrl Pts',(78.6934974891512,-10.5874951690243,133.59425717266));
#73734=CARTESIAN_POINT('Ctrl Pts',(78.6391494666403,-10.5411559378864,133.590397769937));
#73735=CARTESIAN_POINT('Ctrl Pts',(78.5873989985902,-10.4921648613059,133.586538367214));
#73736=CARTESIAN_POINT('Ctrl Pts',(78.5356192290186,-10.443146045593,133.582676779267));
#73737=CARTESIAN_POINT('Ctrl Pts',(78.4864402767899,-10.3914727474777,133.57881519132));
#73738=CARTESIAN_POINT('Ctrl Pts',(78.4401299138821,-10.3374613553051,133.574953603373));
#73739=CARTESIAN_POINT('Ctrl Pts',(78.3937385293345,-10.2833554682659,133.57108525944));
#73740=CARTESIAN_POINT('Ctrl Pts',(78.3502260507417,-10.226903705087,133.567216915506));
#73741=CARTESIAN_POINT('Ctrl Pts',(78.3098183000035,-10.1684534152019,133.563348571573));
#73742=CARTESIAN_POINT('Ctrl Pts',(78.2858253404492,-10.1337473151214,133.561051660267));
#73743=CARTESIAN_POINT('Ctrl Pts',(78.2629261494461,-10.0983371353048,133.55875474896));
#73744=CARTESIAN_POINT('Ctrl Pts',(78.2411602539382,-10.0622995388182,133.556457837654));
#73745=CARTESIAN_POINT('Ctrl Pts',(78.2033015192917,-9.99961717400613,133.552462681303));
#73746=CARTESIAN_POINT('Ctrl Pts',(78.1687336620036,-9.9348033260882,133.548467524953));
#73747=CARTESIAN_POINT('Ctrl Pts',(78.1376942678546,-9.86822515657996,133.544472368603));
#73748=CARTESIAN_POINT('Ctrl Pts',(78.1062630365257,-9.80080651312272,133.540426777931));
#73749=CARTESIAN_POINT('Ctrl Pts',(78.0784502909621,-9.73157903424725,133.536381187259));
#73750=CARTESIAN_POINT('Ctrl Pts',(78.0544569760339,-9.66095378385848,133.532335596587));
#73751=CARTESIAN_POINT('Ctrl Pts',(78.0308540830868,-9.59147775566983,133.528355836231));
#73752=CARTESIAN_POINT('Ctrl Pts',(78.0109474205578,-9.52064953469732,133.524376075876));
#73753=CARTESIAN_POINT('Ctrl Pts',(77.9948811787216,-9.44888314187016,133.520396315521));
#73754=CARTESIAN_POINT('Ctrl Pts',(77.97841630266,-9.37533608741029,133.51631780969));
#73755=CARTESIAN_POINT('Ctrl Pts',(77.9659851790174,-9.3008041087637,133.51223930386));
#73756=CARTESIAN_POINT('Ctrl Pts',(77.9576890084772,-9.22575069524891,133.508160798029));
#73757=CARTESIAN_POINT('Ctrl Pts',(77.9493928379371,-9.15069728173412,133.504082292199));
#73758=CARTESIAN_POINT('Ctrl Pts',(77.9452317338588,-9.07512292632964,133.500003786368));
#73759=CARTESIAN_POINT('Ctrl Pts',(77.9452500603398,-8.99950203790955,133.495925280538));
#73760=CARTESIAN_POINT('Ctrl Pts',(77.94525006034,-8.99950203698839,133.495925280488));
#73761=CARTESIAN_POINT('Ctrl Pts',(77.9452690078821,-8.92131859753172,133.491708567086));
#73762=CARTESIAN_POINT('Ctrl Pts',(77.9497549266111,-8.84325445761002,133.487491853684));
#73763=CARTESIAN_POINT('Ctrl Pts',(77.9586394355346,-8.76581074246384,133.483275140282));
#73764=CARTESIAN_POINT('Ctrl Pts',(77.9673566235425,-8.68982551573053,133.479137839749));
#73765=CARTESIAN_POINT('Ctrl Pts',(77.9803079746392,-8.61443788697709,133.475000539216));
#73766=CARTESIAN_POINT('Ctrl Pts',(77.9973777224886,-8.54010699492684,133.470863238684));
#73767=CARTESIAN_POINT('Ctrl Pts',(78.0149389348737,-8.46363600112062,133.466606818847));
#73768=CARTESIAN_POINT('Ctrl Pts',(78.0368591598541,-8.38828393878643,133.46235039901));
#73769=CARTESIAN_POINT('Ctrl Pts',(78.0629590532119,-8.31452940765756,133.458093979173));
#73770=CARTESIAN_POINT('Ctrl Pts',(78.0890589465697,-8.24077487652868,133.453837559336));
#73771=CARTESIAN_POINT('Ctrl Pts',(78.1193382663649,-8.16861823146456,133.449581139499));
#73772=CARTESIAN_POINT('Ctrl Pts',(78.1535669543638,-8.09851091493974,133.445324719662));
#73773=CARTESIAN_POINT('Ctrl Pts',(78.1846808093607,-8.03478341008652,133.441455636815));
#73774=CARTESIAN_POINT('Ctrl Pts',(78.2191586994743,-7.97254376655812,133.437586553968));
#73775=CARTESIAN_POINT('Ctrl Pts',(78.2568351259752,-7.91217014911979,133.433717471121));
#73776=CARTESIAN_POINT('Ctrl Pts',(78.2944554164795,-7.85188648536049,133.429854153015));
#73777=CARTESIAN_POINT('Ctrl Pts',(78.3352645285792,-7.79346373766178,133.425990834909));
#73778=CARTESIAN_POINT('Ctrl Pts',(78.3790502987056,-7.73725710123816,133.422127516802));
#73779=CARTESIAN_POINT('Ctrl Pts',(78.4227847081404,-7.68111639517741,133.418268730366));
#73780=CARTESIAN_POINT('Ctrl Pts',(78.4694885429766,-7.62718701827358,133.41440994393));
#73781=CARTESIAN_POINT('Ctrl Pts',(78.5189063847534,-7.57579521648899,133.410551157495));
#73782=CARTESIAN_POINT('Ctrl Pts',(78.5682930969135,-7.52443578777113,133.406694801811));
#73783=CARTESIAN_POINT('Ctrl Pts',(78.6203900882303,-7.47561111213256,133.402838446128));
#73784=CARTESIAN_POINT('Ctrl Pts',(78.6749026713714,-7.42961322211333,133.398982090445));
#73785=CARTESIAN_POINT('Ctrl Pts',(78.7293991509495,-7.3836289203314,133.395126873968));
#73786=CARTESIAN_POINT('Ctrl Pts',(78.7863094346098,-7.34047005944964,133.39127165749));
#73787=CARTESIAN_POINT('Ctrl Pts',(78.8453043857987,-7.30038957374219,133.387416441013));
#73788=CARTESIAN_POINT('Ctrl Pts',(78.9043016435137,-7.26030752100764,133.383561073809));
#73789=CARTESIAN_POINT('Ctrl Pts',(78.9653833275144,-7.22330435356743,133.379705706604));
#73790=CARTESIAN_POINT('Ctrl Pts',(79.0281912878424,-7.18958971791626,133.375850339399));
#73791=CARTESIAN_POINT('Ctrl Pts',(79.0910649909779,-7.15583979223511,133.371990936677));
#73792=CARTESIAN_POINT('Ctrl Pts',(79.1556681486058,-7.12538549996297,133.368131533954));
#73793=CARTESIAN_POINT('Ctrl Pts',(79.2216187718385,-7.09839009622221,133.364272131231));
#73794=CARTESIAN_POINT('Ctrl Pts',(79.2876067368321,-7.0713794074718,133.360410543284));
#73795=CARTESIAN_POINT('Ctrl Pts',(79.35494322745,-7.04783166635548,133.356548955337));
#73796=CARTESIAN_POINT('Ctrl Pts',(79.4232296777164,-7.02786066470118,133.35268736739));
#73797=CARTESIAN_POINT('Ctrl Pts',(79.4916355975752,-7.00785472306364,133.348819023457));
#73798=CARTESIAN_POINT('Ctrl Pts',(79.5609943224181,-6.99143812635553,133.344950679524));
#73799=CARTESIAN_POINT('Ctrl Pts',(79.6308963387199,-6.97867369043749,133.34108233559));
#73800=CARTESIAN_POINT('Ctrl Pts',(79.672402144395,-6.97109453571783,133.338785424284));
#73801=CARTESIAN_POINT('Ctrl Pts',(79.7140993616812,-6.96480201206941,133.336488512977));
#73802=CARTESIAN_POINT('Ctrl Pts',(79.7559018530522,-6.95980058397306,133.334191601671));
#73803=CARTESIAN_POINT('Ctrl Pts',(79.8262968740992,-6.95137822385623,133.330323623604));
#73804=CARTESIAN_POINT('Ctrl Pts',(79.8972661514778,-6.94658701062118,133.326455645537));
#73805=CARTESIAN_POINT('Ctrl Pts',(79.9684025636867,-6.94549296313728,133.32258766747));
#73806=CARTESIAN_POINT('Ctrl Pts',(80.0394421231407,-6.94440040520718,133.318724955685));
#73807=CARTESIAN_POINT('Ctrl Pts',(80.1106478848647,-6.94699503549171,133.314862243899));
#73808=CARTESIAN_POINT('Ctrl Pts',(80.1816065604025,-6.95329127140211,133.310999532113));
#73809=CARTESIAN_POINT('Ctrl Pts',(80.2524923697579,-6.95958104182157,133.307140786876));
#73810=CARTESIAN_POINT('Ctrl Pts',(80.3231311151167,-6.96956483233156,133.303282041639));
#73811=CARTESIAN_POINT('Ctrl Pts',(80.3931101843536,-6.98320503137837,133.299423296402));
#73812=CARTESIAN_POINT('Ctrl Pts',(80.4630408059895,-6.99683578710266,133.295567222635));
#73813=CARTESIAN_POINT('Ctrl Pts',(80.5323121827187,-7.01411783254821,133.291711148868));
#73814=CARTESIAN_POINT('Ctrl Pts',(80.6005192195216,-7.03496202848769,133.2878550751));
#73815=CARTESIAN_POINT('Ctrl Pts',(80.6687201287411,-7.05580435182643,133.283999347755));
#73816=CARTESIAN_POINT('Ctrl Pts',(80.735856419764,-7.08020806062568,133.280143620409));
#73817=CARTESIAN_POINT('Ctrl Pts',(80.8015369135476,-7.10803379028046,133.276287893064));
#73818=CARTESIAN_POINT('Ctrl Pts',(80.867213554729,-7.1358578877692,133.272432391883));
#73819=CARTESIAN_POINT('Ctrl Pts',(80.9314341240364,-7.16710341035558,133.268576890702));
#73820=CARTESIAN_POINT('Ctrl Pts',(80.9938281893639,-7.20158317052866,133.26472138952));
#73821=CARTESIAN_POINT('Ctrl Pts',(81.0562666112049,-7.23608744267965,133.260863147428));
#73822=CARTESIAN_POINT('Ctrl Pts',(81.1168755162799,-7.27383029855921,133.257004905336));
#73823=CARTESIAN_POINT('Ctrl Pts',(81.1753108603495,-7.31457959427192,133.253146663244));
#73824=CARTESIAN_POINT('Ctrl Pts',(81.2013268074122,-7.3327215516264,133.251428938746));
#73825=CARTESIAN_POINT('Ctrl Pts',(81.2269123279116,-7.35145885228397,133.249711214249));
#73826=CARTESIAN_POINT('Ctrl Pts',(81.2520391107129,-7.3707683934611,133.247993489751));
#73827=CARTESIAN_POINT('',(77.9452500001325,-9.00002333775544,133.554074719471));
#73828=CARTESIAN_POINT('Ctrl Pts',(77.9452500001325,-9.00002333758729,133.554074719462));
#73829=CARTESIAN_POINT('Ctrl Pts',(77.9452491949294,-8.92912950095486,133.550206920375));
#73830=CARTESIAN_POINT('Ctrl Pts',(77.948921710863,-8.85809631169957,133.546339121287));
#73831=CARTESIAN_POINT('Ctrl Pts',(77.9562848605137,-8.78733596652337,133.5424713222));
#73832=CARTESIAN_POINT('Ctrl Pts',(77.9636370380662,-8.71668106392196,133.538609286661));
#73833=CARTESIAN_POINT('Ctrl Pts',(77.97466888319,-8.64629867796401,133.534747251122));
#73834=CARTESIAN_POINT('Ctrl Pts',(77.9893456969755,-8.57660085471362,133.530885215583));
#73835=CARTESIAN_POINT('Ctrl Pts',(78.0040053078095,-8.50698472550769,133.527027706804));
#73836=CARTESIAN_POINT('Ctrl Pts',(78.0223013014783,-8.43805203863106,133.523170198025));
#73837=CARTESIAN_POINT('Ctrl Pts',(78.0441474066621,-8.37020781551908,133.519312689246));
#73838=CARTESIAN_POINT('Ctrl Pts',(78.0659797748482,-8.30240625337239,133.515457606098));
#73839=CARTESIAN_POINT('Ctrl Pts',(78.0913576770541,-8.23569225876866,133.51160252295));
#73840=CARTESIAN_POINT('Ctrl Pts',(78.1201445418238,-8.17045734355309,133.507747439802));
#73841=CARTESIAN_POINT('Ctrl Pts',(78.1489229525421,-8.10524158635715,133.503893488805));
#73842=CARTESIAN_POINT('Ctrl Pts',(78.1811081421473,-8.04150449073841,133.500039537807));
#73843=CARTESIAN_POINT('Ctrl Pts',(78.2165154281123,-7.9796175499654,133.49618558681));
#73844=CARTESIAN_POINT('Ctrl Pts',(78.2519241814885,-7.91772804436478,133.49233147609));
#73845=CARTESIAN_POINT('Ctrl Pts',(78.2905550529745,-7.857689266697,133.488477365371));
#73846=CARTESIAN_POINT('Ctrl Pts',(78.3321782980712,-7.79984653769805,133.484623254651));
#73847=CARTESIAN_POINT('Ctrl Pts',(78.3738451508805,-7.7419432082079,133.480765106069));
#73848=CARTESIAN_POINT('Ctrl Pts',(78.4185103508029,-7.68624091544602,133.476906957487));
#73849=CARTESIAN_POINT('Ctrl Pts',(78.4659023851083,-7.63305374264985,133.473048808904));
#73850=CARTESIAN_POINT('Ctrl Pts',(78.513321406382,-7.57983628289573,133.469188463334));
#73851=CARTESIAN_POINT('Ctrl Pts',(78.5634700109468,-7.52913713982456,133.465328117764));
#73852=CARTESIAN_POINT('Ctrl Pts',(78.6160400988869,-7.48123321256654,133.461467772193));
#73853=CARTESIAN_POINT('Ctrl Pts',(78.6687019134685,-7.43324570039295,133.457600690919));
#73854=CARTESIAN_POINT('Ctrl Pts',(78.7237932705989,-7.3880634493979,133.453733609645));
#73855=CARTESIAN_POINT('Ctrl Pts',(78.7809738927824,-7.34592233785049,133.449866528371));
#73856=CARTESIAN_POINT('Ctrl Pts',(78.8140980817257,-7.32151039394591,133.44762636508));
#73857=CARTESIAN_POINT('Ctrl Pts',(78.8479228431124,-7.29811817395487,133.445386201789));
#73858=CARTESIAN_POINT('Ctrl Pts',(78.8823781830246,-7.27578451557798,133.443146038498));
#73859=CARTESIAN_POINT('Ctrl Pts',(78.9418874898534,-7.23721108886549,133.439276955651));
#73860=CARTESIAN_POINT('Ctrl Pts',(79.0035126729261,-7.20164657081051,133.435407872804));
#73861=CARTESIAN_POINT('Ctrl Pts',(79.0669169949675,-7.16932972159936,133.431538789957));
#73862=CARTESIAN_POINT('Ctrl Pts',(79.1302268477313,-7.13706102288172,133.427675471851));
#73863=CARTESIAN_POINT('Ctrl Pts',(79.1953101483624,-7.10803060679747,133.423812153744));
#73864=CARTESIAN_POINT('Ctrl Pts',(79.2618020099645,-7.08243349789177,133.419948835638));
#73865=CARTESIAN_POINT('Ctrl Pts',(79.3282158766384,-7.05686641438503,133.416090049202));
#73866=CARTESIAN_POINT('Ctrl Pts',(79.3960345712222,-7.03472481221642,133.412231262766));
#73867=CARTESIAN_POINT('Ctrl Pts',(79.4648710613896,-7.01615661365074,133.40837247633));
#73868=CARTESIAN_POINT('Ctrl Pts',(79.5336641896158,-6.99760011168859,133.404516120647));
#73869=CARTESIAN_POINT('Ctrl Pts',(79.60347337351,-6.9826126736317,133.400659764964));
#73870=CARTESIAN_POINT('Ctrl Pts',(79.6738955643609,-6.97129266291155,133.39680340928));
#73871=CARTESIAN_POINT('Ctrl Pts',(79.7442969517914,-6.95997599623592,133.392948192803));
#73872=CARTESIAN_POINT('Ctrl Pts',(79.8153105073031,-6.95232468311315,133.389092976326));
#73873=CARTESIAN_POINT('Ctrl Pts',(79.8865238136966,-6.94838582632064,133.385237759849));
#73874=CARTESIAN_POINT('Ctrl Pts',(79.9577399043173,-6.94444681553062,133.381382392644));
#73875=CARTESIAN_POINT('Ctrl Pts',(80.0291552761617,-6.94422057386752,133.37752702544));
#73876=CARTESIAN_POINT('Ctrl Pts',(80.1003549610624,-6.94770215507345,133.373671658235));
#73877=CARTESIAN_POINT('Ctrl Pts',(80.1716291726179,-6.95118738054552,133.369812255512));
#73878=CARTESIAN_POINT('Ctrl Pts',(80.242686760354,-6.95838815261647,133.365952852789));
#73879=CARTESIAN_POINT('Ctrl Pts',(80.3131162389923,-6.96924748347334,133.362093450067));
#73880=CARTESIAN_POINT('Ctrl Pts',(80.3835855953545,-6.98011296296865,133.35823186212));
#73881=CARTESIAN_POINT('Ctrl Pts',(80.4534256588216,-6.99464102599578,133.354370274173));
#73882=CARTESIAN_POINT('Ctrl Pts',(80.5222362332727,-7.01272375368768,133.350508686226));
#73883=CARTESIAN_POINT('Ctrl Pts',(80.5911671942902,-7.03083811775983,133.346640342292));
#73884=CARTESIAN_POINT('Ctrl Pts',(80.6590646073802,-7.05251941511445,133.342771998359));
#73885=CARTESIAN_POINT('Ctrl Pts',(80.7255451693952,-7.07761040117585,133.338903654425));
#73886=CARTESIAN_POINT('Ctrl Pts',(80.7650194139755,-7.0925087066433,133.336606743119));
#73887=CARTESIAN_POINT('Ctrl Pts',(80.8039945234929,-7.10860822903842,133.334309831813));
#73888=CARTESIAN_POINT('Ctrl Pts',(80.8423943826247,-7.1258683966641,133.332012920506));
#73889=CARTESIAN_POINT('Ctrl Pts',(80.9070806959083,-7.15494393588762,133.328143668699));
#73890=CARTESIAN_POINT('Ctrl Pts',(80.9703866144571,-7.18742936372782,133.324274416891));
#73891=CARTESIAN_POINT('Ctrl Pts',(81.0319288584345,-7.22317125371349,133.320405165084));
#73892=CARTESIAN_POINT('Ctrl Pts',(81.093372977261,-7.25885615555375,133.316542082549));
#73893=CARTESIAN_POINT('Ctrl Pts',(81.1530585893493,-7.2977869662659,133.312679000015));
#73894=CARTESIAN_POINT('Ctrl Pts',(81.210624007114,-7.33976294587214,133.308815917481));
#73895=CARTESIAN_POINT('Ctrl Pts',(81.2245547338712,-7.34992105685204,133.30788105851));
#73896=CARTESIAN_POINT('Ctrl Pts',(81.2383614038783,-7.36025728881951,133.306946199539));
#73897=CARTESIAN_POINT('Ctrl Pts',(81.2520391107129,-7.37076839346111,133.306011340568));
#73898=CARTESIAN_POINT('Ctrl Pts',(81.2520391107129,-7.3707683934611,134.006113615385));
#73899=CARTESIAN_POINT('Ctrl Pts',(81.2874945677546,-7.39801535989994,134.003679619742));
#73900=CARTESIAN_POINT('Ctrl Pts',(81.3220223716194,-7.42639116812375,134.001245624099));
#73901=CARTESIAN_POINT('Ctrl Pts',(81.3555499459166,-7.45582322688577,133.998811628456));
#73902=CARTESIAN_POINT('Ctrl Pts',(81.4088454244803,-7.5026084682794,133.994942545609));
#73903=CARTESIAN_POINT('Ctrl Pts',(81.4598203372147,-7.55224773101518,133.991073462762));
#73904=CARTESIAN_POINT('Ctrl Pts',(81.5081533895656,-7.60448184675306,133.987204379915));
#73905=CARTESIAN_POINT('Ctrl Pts',(81.5564144280789,-7.65663813626349,133.983341061809));
#73906=CARTESIAN_POINT('Ctrl Pts',(81.6020410922966,-7.71138125082055,133.979477743702));
#73907=CARTESIAN_POINT('Ctrl Pts',(81.6447465261169,-7.76841304516227,133.975614425596));
#73908=CARTESIAN_POINT('Ctrl Pts',(81.6874018664798,-7.8253779412312,133.97175563916));
#73909=CARTESIAN_POINT('Ctrl Pts',(81.7271424930792,-7.88462579755637,133.967896852724));
#73910=CARTESIAN_POINT('Ctrl Pts',(81.7637208600582,-7.94582435510224,133.964038066288));
#73911=CARTESIAN_POINT('Ctrl Pts',(81.8002761853482,-8.00698436204436,133.960181710605));
#73912=CARTESIAN_POINT('Ctrl Pts',(81.8336729544594,-8.07009221629728,133.956325354922));
#73913=CARTESIAN_POINT('Ctrl Pts',(81.8637069616787,-8.1347867757076,133.952468999239));
#73914=CARTESIAN_POINT('Ctrl Pts',(81.8937320965514,-8.19946222369726,133.948613782761));
#73915=CARTESIAN_POINT('Ctrl Pts',(81.9203962372521,-8.26572300591116,133.944758566284));
#73916=CARTESIAN_POINT('Ctrl Pts',(81.9435419628082,-8.33318503218383,133.940903349807));
#73917=CARTESIAN_POINT('Ctrl Pts',(81.9666885932929,-8.40064969601996,133.937047982602));
#73918=CARTESIAN_POINT('Ctrl Pts',(81.9863163799621,-8.4693152369516,133.933192615398));
#73919=CARTESIAN_POINT('Ctrl Pts',(82.0023172982288,-8.53878096340919,133.929337248193));
#73920=CARTESIAN_POINT('Ctrl Pts',(82.0183349650936,-8.60831940153999,133.92547784547));
#73921=CARTESIAN_POINT('Ctrl Pts',(82.0307180759414,-8.6786592228294,133.921618442747));
#73922=CARTESIAN_POINT('Ctrl Pts',(82.0394096353205,-8.74938894305702,133.917759040025));
#73923=CARTESIAN_POINT('Ctrl Pts',(82.0481061159287,-8.82015871100782,133.913897452078));
#73924=CARTESIAN_POINT('Ctrl Pts',(82.053106850083,-8.89131833255214,133.910035864131));
#73925=CARTESIAN_POINT('Ctrl Pts',(82.0544069244437,-8.96245334505461,133.906174276184));
#73926=CARTESIAN_POINT('Ctrl Pts',(82.0557092733312,-9.0337128108112,133.90230593225));
#73927=CARTESIAN_POINT('Ctrl Pts',(82.0532980524677,-9.10494709590801,133.898437588317));
#73928=CARTESIAN_POINT('Ctrl Pts',(82.0472204087786,-9.17574458848055,133.894569244383));
#73929=CARTESIAN_POINT('Ctrl Pts',(82.0436116788554,-9.21778210219532,133.892272333077));
#73930=CARTESIAN_POINT('Ctrl Pts',(82.0387112898198,-9.25966575020436,133.889975421771));
#73931=CARTESIAN_POINT('Ctrl Pts',(82.0325375986326,-9.30131125542311,133.887678510464));
#73932=CARTESIAN_POINT('Ctrl Pts',(82.0221381885172,-9.37146194406432,133.883809427617));
#73933=CARTESIAN_POINT('Ctrl Pts',(82.0080823914302,-9.44121101360281,133.87994034477));
#73934=CARTESIAN_POINT('Ctrl Pts',(81.9904136794236,-9.51014796604846,133.876071261923));
#73935=CARTESIAN_POINT('Ctrl Pts',(81.9727712929167,-9.57898220587301,133.872207943817));
#73936=CARTESIAN_POINT('Ctrl Pts',(81.9515267963479,-9.64700626370974,133.868344625711));
#73937=CARTESIAN_POINT('Ctrl Pts',(81.9267750863095,-9.71381743413647,133.864481307604));
#73938=CARTESIAN_POINT('Ctrl Pts',(81.9020524100173,-9.78055023508601,133.860622521168));
#73939=CARTESIAN_POINT('Ctrl Pts',(81.8738308599146,-9.84607252130558,133.856763734733));
#73940=CARTESIAN_POINT('Ctrl Pts',(81.8422553138061,-9.90999611057039,133.852904948297));
#73941=CARTESIAN_POINT('Ctrl Pts',(81.8106996579763,-9.97387943266128,133.849048592614));
#73942=CARTESIAN_POINT('Ctrl Pts',(81.7757944124788,-10.0361656212767,133.84519223693));
#73943=CARTESIAN_POINT('Ctrl Pts',(81.7377322276223,-10.0964872400455,133.841335881247));
#73944=CARTESIAN_POINT('Ctrl Pts',(81.6996812867164,-10.1567910392041,133.83748066477));
#73945=CARTESIAN_POINT('Ctrl Pts',(81.6584755169942,-10.2151310100689,133.833625448293));
#73946=CARTESIAN_POINT('Ctrl Pts',(81.6143522232711,-10.2711665751268,133.829770231815));
#73947=CARTESIAN_POINT('Ctrl Pts',(81.5702272044592,-10.3272043310076,133.825914864611));
#73948=CARTESIAN_POINT('Ctrl Pts',(81.5231847374418,-10.3809371219074,133.822059497406));
#73949=CARTESIAN_POINT('Ctrl Pts',(81.4735028660502,-10.4320568655754,133.818204130202));
#73950=CARTESIAN_POINT('Ctrl Pts',(81.4237689912869,-10.4832301176754,133.814344727479));
#73951=CARTESIAN_POINT('Ctrl Pts',(81.3713905363678,-10.5317845134968,133.810485324756));
#73952=CARTESIAN_POINT('Ctrl Pts',(81.3166822895861,-10.5774489883322,133.806625922033));
#73953=CARTESIAN_POINT('Ctrl Pts',(81.2619430665654,-10.6231393187519,133.802764334086));
#73954=CARTESIAN_POINT('Ctrl Pts',(81.2048718145003,-10.6659361792457,133.798902746139));
#73955=CARTESIAN_POINT('Ctrl Pts',(81.1458140722615,-10.7056106455776,133.795041158192));
#73956=CARTESIAN_POINT('Ctrl Pts',(81.0866530063858,-10.7453545238104,133.791172814259));
#73957=CARTESIAN_POINT('Ctrl Pts',(81.0254989284647,-10.7819648517648,133.787304470326));
#73958=CARTESIAN_POINT('Ctrl Pts',(80.9627232188053,-10.8152579889573,133.783436126392));
#73959=CARTESIAN_POINT('Ctrl Pts',(80.9254488089373,-10.835026495729,133.781139215086));
#73960=CARTESIAN_POINT('Ctrl Pts',(80.8876030962552,-10.8536263832245,133.778842303779));
#73961=CARTESIAN_POINT('Ctrl Pts',(80.8492668411798,-10.8710273635018,133.776545392473));
#73962=CARTESIAN_POINT('Ctrl Pts',(80.7846904918397,-10.900338828042,133.772676309626));
#73963=CARTESIAN_POINT('Ctrl Pts',(80.7184684036561,-10.9263606106449,133.768807226779));
#73964=CARTESIAN_POINT('Ctrl Pts',(80.6509690279542,-10.9489065875881,133.764938143932));
#73965=CARTESIAN_POINT('Ctrl Pts',(80.5835702229558,-10.9714189721501,133.761074825826));
#73966=CARTESIAN_POINT('Ctrl Pts',(80.5148983650355,-10.9904656781335,133.757211507719));
#73967=CARTESIAN_POINT('Ctrl Pts',(80.4453432503833,-11.0059080118086,133.753348189613));
#73968=CARTESIAN_POINT('Ctrl Pts',(80.3758697238538,-11.0213322316323,133.749489403177));
#73969=CARTESIAN_POINT('Ctrl Pts',(80.3055154704923,-11.0331603724661,133.745630616741));
#73970=CARTESIAN_POINT('Ctrl Pts',(80.2346851938962,-11.0413036085467,133.741771830305));
#73971=CARTESIAN_POINT('Ctrl Pts',(80.1638995351806,-11.0494417149858,133.737915474622));
#73972=CARTESIAN_POINT('Ctrl Pts',(80.0926389296107,-11.0538994665824,133.734059118939));
#73973=CARTESIAN_POINT('Ctrl Pts',(80.0213165623721,-11.0546394249767,133.730202763256));
#73974=CARTESIAN_POINT('Ctrl Pts',(79.9500152644751,-11.0553791647799,133.726347546778));
#73975=CARTESIAN_POINT('Ctrl Pts',(79.878652726623,-11.0524032867213,133.722492330301));
#73976=CARTESIAN_POINT('Ctrl Pts',(79.8076437887121,-11.0457264358851,133.718637113824));
#73977=CARTESIAN_POINT('Ctrl Pts',(79.7366320745641,-11.0390493240039,133.714781746619));
#73978=CARTESIAN_POINT('Ctrl Pts',(79.6659744712478,-11.0286709997384,133.710926379415));
#73979=CARTESIAN_POINT('Ctrl Pts',(79.596080614355,-11.0146579591584,133.70707101221));
#73980=CARTESIAN_POINT('Ctrl Pts',(79.5261135976531,-11.000630250746,133.703211609487));
#73981=CARTESIAN_POINT('Ctrl Pts',(79.4569124005049,-10.9829603269613,133.699352206764));
#73982=CARTESIAN_POINT('Ctrl Pts',(79.3888754883127,-10.9617656316989,133.695492804042));
#73983=CARTESIAN_POINT('Ctrl Pts',(79.3208000530864,-10.9405589358335,133.691631216095));
#73984=CARTESIAN_POINT('Ctrl Pts',(79.2538906709944,-10.915823664085,133.687769628148));
#73985=CARTESIAN_POINT('Ctrl Pts',(79.1885270823431,-10.8877259510875,133.683908040201));
#73986=CARTESIAN_POINT('Ctrl Pts',(79.1230491377505,-10.8595790801341,133.680039696267));
#73987=CARTESIAN_POINT('Ctrl Pts',(79.0591228218862,-10.8280582378338,133.676171352334));
#73988=CARTESIAN_POINT('Ctrl Pts',(78.9971038465646,-10.7933758300826,133.6723030084));
#73989=CARTESIAN_POINT('Ctrl Pts',(78.9602787637695,-10.7727824144328,133.670006097094));
#73990=CARTESIAN_POINT('Ctrl Pts',(78.9241256132804,-10.7510751922943,133.667709185788));
#73991=CARTESIAN_POINT('Ctrl Pts',(78.8887136438621,-10.7283055855843,133.665412274481));
#73992=CARTESIAN_POINT('Ctrl Pts',(78.8290631719137,-10.6899508199882,133.661543191634));
#73993=CARTESIAN_POINT('Ctrl Pts',(78.7712838542151,-10.6484291560101,133.657674108787));
#73994=CARTESIAN_POINT('Ctrl Pts',(78.7157319002099,-10.6039491919514,133.65380502594));
#73995=CARTESIAN_POINT('Ctrl Pts',(78.6602627158456,-10.5595355008208,133.649941707834));
#73996=CARTESIAN_POINT('Ctrl Pts',(78.6070146838405,-10.5121725599639,133.646078389728));
#73997=CARTESIAN_POINT('Ctrl Pts',(78.5563157431669,-10.4621126253036,133.642215071621));
#73998=CARTESIAN_POINT('Ctrl Pts',(78.5056762723312,-10.4121114109275,133.638356285185));
#73999=CARTESIAN_POINT('Ctrl Pts',(78.4575802975038,-10.3594198263333,133.63449749875));
#74000=CARTESIAN_POINT('Ctrl Pts',(78.4123219474133,-10.3043296990541,133.630638712314));
#74001=CARTESIAN_POINT('Ctrl Pts',(78.3670921067648,-10.2492742745156,133.626782356631));
#74002=CARTESIAN_POINT('Ctrl Pts',(78.3246966521302,-10.1918236793768,133.622926000947));
#74003=CARTESIAN_POINT('Ctrl Pts',(78.2853911402273,-10.1323047383497,133.619069645264));
#74004=CARTESIAN_POINT('Ctrl Pts',(78.2460972395663,-10.0728033798137,133.615214428787));
#74005=CARTESIAN_POINT('Ctrl Pts',(78.2098917370287,-10.0112352935604,133.61135921231));
#74006=CARTESIAN_POINT('Ctrl Pts',(78.1769873297906,-9.94795694351372,133.607503995832));
#74007=CARTESIAN_POINT('Ctrl Pts',(78.1440816360885,-9.88467611947279,133.603648628628));
#74008=CARTESIAN_POINT('Ctrl Pts',(78.1144775160846,-9.81968533089659,133.599793261423));
#74009=CARTESIAN_POINT('Ctrl Pts',(78.0883412825142,-9.7533647923553,133.595937894219));
#74010=CARTESIAN_POINT('Ctrl Pts',(78.0621776914343,-9.68697483429487,133.592078491496));
#74011=CARTESIAN_POINT('Ctrl Pts',(78.0394894114196,-9.61925280063322,133.588219088773));
#74012=CARTESIAN_POINT('Ctrl Pts',(78.020393893762,-9.55059715459226,133.58435968605));
#74013=CARTESIAN_POINT('Ctrl Pts',(78.0012875640722,-9.48190263518528,133.580498098103));
#74014=CARTESIAN_POINT('Ctrl Pts',(77.9857781519716,-9.41227392546944,133.576636510156));
#74015=CARTESIAN_POINT('Ctrl Pts',(77.9739320459272,-9.34212016599325,133.572774922209));
#74016=CARTESIAN_POINT('Ctrl Pts',(77.9620652146957,-9.27184367000021,133.568906578276));
#74017=CARTESIAN_POINT('Ctrl Pts',(77.9538745412824,-9.20104077296669,133.565038234342));
#74018=CARTESIAN_POINT('Ctrl Pts',(77.949374507556,-9.13012552493194,133.561169890409));
#74019=CARTESIAN_POINT('Ctrl Pts',(77.946702517029,-9.08801809141209,133.558872979102));
#74020=CARTESIAN_POINT('Ctrl Pts',(77.9453307150346,-9.04587106372851,133.556576067796));
#74021=CARTESIAN_POINT('Ctrl Pts',(77.9452534594865,-9.00377051029501,133.55427915649));
#74022=CARTESIAN_POINT('Ctrl Pts',(77.9452511674388,-9.00252145466656,133.55421101083));
#74023=CARTESIAN_POINT('Ctrl Pts',(77.9452500143197,-9.0012723969475,133.55414286517));
#74024=CARTESIAN_POINT('Ctrl Pts',(77.9452500001325,-9.00002333845969,133.55407471951));
#74025=CARTESIAN_POINT('Origin',(80.,-9.,141.545925280538));
#74026=CARTESIAN_POINT('',(81.2520391107129,-7.37076839346111,134.706120114083));
#74027=CARTESIAN_POINT('',(81.2520391107129,-7.37076839346112,134.647862573676));
#74028=CARTESIAN_POINT('',(81.2520391107129,-7.37076839346111,141.545925280538));
#74029=CARTESIAN_POINT('',(77.9452508583196,-9.00187810112593,134.19592528059));
#74030=CARTESIAN_POINT('Ctrl Pts',(81.2520391107129,-7.37076839346111,134.647862573676));
#74031=CARTESIAN_POINT('Ctrl Pts',(81.3084423634553,-7.41411341458736,134.644002866637));
#74032=CARTESIAN_POINT('Ctrl Pts',(81.3626623275803,-7.46044482548973,134.640143159597));
#74033=CARTESIAN_POINT('Ctrl Pts',(81.4143696957603,-7.50951151422936,134.636283452558));
#74034=CARTESIAN_POINT('Ctrl Pts',(81.4660396077081,-7.55854265961508,134.632426541446));
#74035=CARTESIAN_POINT('Ctrl Pts',(81.5152001830901,-7.61030481882812,134.628569630335));
#74036=CARTESIAN_POINT('Ctrl Pts',(81.5615557483562,-7.66450712945533,134.624712719223));
#74037=CARTESIAN_POINT('Ctrl Pts',(81.6078932410243,-7.7186883082816,134.620857311802));
#74038=CARTESIAN_POINT('Ctrl Pts',(81.6514275786264,-7.77530738151462,134.617001904381));
#74039=CARTESIAN_POINT('Ctrl Pts',(81.6919016799579,-7.83403847925596,134.613146496959));
#74040=CARTESIAN_POINT('Ctrl Pts',(81.7323735406718,-7.89276632568549,134.609291302971));
#74041=CARTESIAN_POINT('Ctrl Pts',(81.7697852271571,-7.95360556357426,134.605436108982));
#74042=CARTESIAN_POINT('Ctrl Pts',(81.8039225237931,-8.01620068578403,134.601580914993));
#74043=CARTESIAN_POINT('Ctrl Pts',(81.8380934850055,-8.07885753632238,134.597721919196));
#74044=CARTESIAN_POINT('Ctrl Pts',(81.868983373165,-8.14327330249264,134.593862923398));
#74045=CARTESIAN_POINT('Ctrl Pts',(81.896424007617,-8.20906792590404,134.590003927601));
#74046=CARTESIAN_POINT('Ctrl Pts',(81.923877854851,-8.27489422970581,134.586143073681));
#74047=CARTESIAN_POINT('Ctrl Pts',(81.9478789761604,-8.34210025519686,134.58228221976));
#74048=CARTESIAN_POINT('Ctrl Pts',(81.9683084278477,-8.41028863385224,134.57842136584));
#74049=CARTESIAN_POINT('Ctrl Pts',(81.9887754594446,-8.47860244480755,134.574553409892));
#74050=CARTESIAN_POINT('Ctrl Pts',(82.0056575794369,-8.54790174613055,134.570685453943));
#74051=CARTESIAN_POINT('Ctrl Pts',(82.0188866566306,-8.61777725057383,134.566817497995));
#74052=CARTESIAN_POINT('Ctrl Pts',(82.0304714636668,-8.67896777986658,134.563430298522));
#74053=CARTESIAN_POINT('Ctrl Pts',(82.0392556566401,-8.74059983008632,134.56004309905));
#74054=CARTESIAN_POINT('Ctrl Pts',(82.0452262841889,-8.80239683969454,134.556655899578));
#74055=CARTESIAN_POINT('Ctrl Pts',(82.052046329133,-8.87298546366857,134.552786816731));
#74056=CARTESIAN_POINT('Ctrl Pts',(82.0552210145704,-8.94406583722984,134.548917733884));
#74057=CARTESIAN_POINT('Ctrl Pts',(82.0546935628721,-9.0152290903256,134.545048651037));
#74058=CARTESIAN_POINT('Ctrl Pts',(82.0541668970505,-9.08628631372333,134.541185332931));
#74059=CARTESIAN_POINT('Ctrl Pts',(82.0499490467711,-9.15742568972607,134.537322014825));
#74060=CARTESIAN_POINT('Ctrl Pts',(82.0420350207688,-9.22823351299477,134.533458696718));
#74061=CARTESIAN_POINT('Ctrl Pts',(82.0341302779158,-9.29895827871404,134.529599910282));
#74062=CARTESIAN_POINT('Ctrl Pts',(82.0225380250317,-9.36935178377462,134.525741123847));
#74063=CARTESIAN_POINT('Ctrl Pts',(82.0073052791557,-9.43900236761729,134.521882337411));
#74064=CARTESIAN_POINT('Ctrl Pts',(81.9920821287927,-9.5086090766994,134.518025981728));
#74065=CARTESIAN_POINT('Ctrl Pts',(81.9732231387407,-9.57747331959585,134.514169626044));
#74066=CARTESIAN_POINT('Ctrl Pts',(81.9508266910127,-9.64519205213054,134.510313270361));
#74067=CARTESIAN_POINT('Ctrl Pts',(81.9284368594196,-9.71289077987354,134.506458053884));
#74068=CARTESIAN_POINT('Ctrl Pts',(81.9025117972192,-9.77944420810088,134.502602837407));
#74069=CARTESIAN_POINT('Ctrl Pts',(81.8731996991641,-9.84446459342684,134.498747620929));
#74070=CARTESIAN_POINT('Ctrl Pts',(81.8438864550936,-9.90948752085537,134.494892253725));
#74071=CARTESIAN_POINT('Ctrl Pts',(81.8111861139161,-9.97297684442902,134.49103688652));
#74072=CARTESIAN_POINT('Ctrl Pts',(81.7752942420166,-10.0345665356866,134.487181519316));
#74073=CARTESIAN_POINT('Ctrl Pts',(81.7393648011145,-10.0962206945562,134.483322116593));
#74074=CARTESIAN_POINT('Ctrl Pts',(81.7002374058725,-10.1559708312496,134.47946271387));
#74075=CARTESIAN_POINT('Ctrl Pts',(81.6581522078642,-10.2134779841657,134.475603311147));
#74076=CARTESIAN_POINT('Ctrl Pts',(81.6160431808863,-10.2710176980836,134.4717417232));
#74077=CARTESIAN_POINT('Ctrl Pts',(81.5709733243342,-10.3263115233336,134.467880135253));
#74078=CARTESIAN_POINT('Ctrl Pts',(81.5232227929821,-10.3790539820615,134.464018547306));
#74079=CARTESIAN_POINT('Ctrl Pts',(81.4753887203639,-10.4318887156115,134.460150203373));
#74080=CARTESIAN_POINT('Ctrl Pts',(81.4248649538139,-10.4821628279647,134.45628185944));
#74081=CARTESIAN_POINT('Ctrl Pts',(81.3719676447898,-10.5296085591255,134.452413515506));
#74082=CARTESIAN_POINT('Ctrl Pts',(81.3405587449436,-10.5577804689193,134.4501166042));
#74083=CARTESIAN_POINT('Ctrl Pts',(81.3083136507051,-10.5849559667216,134.447819692893));
#74084=CARTESIAN_POINT('Ctrl Pts',(81.2753034381164,-10.6110861873992,134.445522781587));
#74085=CARTESIAN_POINT('Ctrl Pts',(81.219698658366,-10.6551018132211,134.44165369874));
#74086=CARTESIAN_POINT('Ctrl Pts',(81.1617035722651,-10.6963215672399,134.437784615893));
#74087=CARTESIAN_POINT('Ctrl Pts',(81.1016308900006,-10.7344759856212,134.433915533046));
#74088=CARTESIAN_POINT('Ctrl Pts',(81.0416477130367,-10.7725735558219,134.43005221494));
#74089=CARTESIAN_POINT('Ctrl Pts',(80.9795934911439,-10.8076145978201,134.426188896833));
#74090=CARTESIAN_POINT('Ctrl Pts',(80.9158130846978,-10.8393705326541,134.422325578727));
#74091=CARTESIAN_POINT('Ctrl Pts',(80.8521074926439,-10.8710892177889,134.418466792291));
#74092=CARTESIAN_POINT('Ctrl Pts',(80.7866801707553,-10.8995302345098,134.414608005855));
#74093=CARTESIAN_POINT('Ctrl Pts',(80.7199024698014,-10.9245098068012,134.410749219419));
#74094=CARTESIAN_POINT('Ctrl Pts',(80.6531668339025,-10.9494736437936,134.406892863736));
#74095=CARTESIAN_POINT('Ctrl Pts',(80.5850829605107,-10.9709801925506,134.403036508053));
#74096=CARTESIAN_POINT('Ctrl Pts',(80.5160428208376,-10.9888935038262,134.39918015237));
#74097=CARTESIAN_POINT('Ctrl Pts',(80.4470230763131,-11.0068015233302,134.395324935892));
#74098=CARTESIAN_POINT('Ctrl Pts',(80.3770480962869,-11.0211182907457,134.391469719415));
#74099=CARTESIAN_POINT('Ctrl Pts',(80.3065240147203,-11.0317580050045,134.387614502938));
#74100=CARTESIAN_POINT('Ctrl Pts',(80.235997175873,-11.0423981352443,134.383759135733));
#74101=CARTESIAN_POINT('Ctrl Pts',(80.1649216735389,-11.0493608566172,134.379903768529));
#74102=CARTESIAN_POINT('Ctrl Pts',(80.0937110916941,-11.0526119442782,134.376048401324));
#74103=CARTESIAN_POINT('Ctrl Pts',(80.0224259717883,-11.0558664349414,134.372188998601));
#74104=CARTESIAN_POINT('Ctrl Pts',(79.9510059763948,-11.0554015142251,134.368329595878));
#74105=CARTESIAN_POINT('Ctrl Pts',(79.8798661318538,-11.0512350953082,134.364470193156));
#74106=CARTESIAN_POINT('Ctrl Pts',(79.808686007374,-11.0470663173323,134.360608605209));
#74107=CARTESIAN_POINT('Ctrl Pts',(79.7377868325604,-11.0391919226788,134.356747017262));
#74108=CARTESIAN_POINT('Ctrl Pts',(79.6675771998992,-11.0276815934641,134.352885429315));
#74109=CARTESIAN_POINT('Ctrl Pts',(79.5972447329689,-11.0161511265159,134.349017085381));
#74110=CARTESIAN_POINT('Ctrl Pts',(79.5276046915497,-11.0009721281821,134.345148741448));
#74111=CARTESIAN_POINT('Ctrl Pts',(79.4590535039995,-10.9822649800076,134.341280397514));
#74112=CARTESIAN_POINT('Ctrl Pts',(79.4183497815635,-10.9711572137665,134.338983486208));
#74113=CARTESIAN_POINT('Ctrl Pts',(79.3780296424184,-10.9588064987021,134.336686574902));
#74114=CARTESIAN_POINT('Ctrl Pts',(79.3381726900255,-10.9452460446617,134.334389663595));
#74115=CARTESIAN_POINT('Ctrl Pts',(79.271034768591,-10.9224038391411,134.330520580748));
#74116=CARTESIAN_POINT('Ctrl Pts',(79.2049492964155,-10.8960370323457,134.326651497901));
#74117=CARTESIAN_POINT('Ctrl Pts',(79.1403122668311,-10.8662621905667,134.322782415054));
#74118=CARTESIAN_POINT('Ctrl Pts',(79.075771543197,-10.836531711817,134.318919096948));
#74119=CARTESIAN_POINT('Ctrl Pts',(79.0126754159974,-10.8034034789718,134.315055778841));
#74120=CARTESIAN_POINT('Ctrl Pts',(78.9514029674593,-10.7670432439097,134.311192460735));
#74121=CARTESIAN_POINT('Ctrl Pts',(78.8902023914798,-10.7307256593893,134.307333674299));
#74122=CARTESIAN_POINT('Ctrl Pts',(78.8308216607734,-10.6911838498401,134.303474887863));
#74123=CARTESIAN_POINT('Ctrl Pts',(78.7736165849993,-10.6486301228327,134.299616101428));
#74124=CARTESIAN_POINT('Ctrl Pts',(78.7164475442282,-10.6061032015529,134.295759745744));
#74125=CARTESIAN_POINT('Ctrl Pts',(78.6614518281798,-10.5605684162585,134.291903390061));
#74126=CARTESIAN_POINT('Ctrl Pts',(78.6089562497838,-10.5122813387345,134.288047034378));
#74127=CARTESIAN_POINT('Ctrl Pts',(78.5564761791074,-10.4640085256966,134.284191817901));
#74128=CARTESIAN_POINT('Ctrl Pts',(78.5064951371636,-10.4129853632591,134.280336601423));
#74129=CARTESIAN_POINT('Ctrl Pts',(78.459305487336,-10.3595065211859,134.276481384946));
#74130=CARTESIAN_POINT('Ctrl Pts',(78.4121139925342,-10.30602558825,134.272626017742));
#74131=CARTESIAN_POINT('Ctrl Pts',(78.3677144262841,-10.2500891507715,134.268770650537));
#74132=CARTESIAN_POINT('Ctrl Pts',(78.3263598618196,-10.1920261114469,134.264915283332));
#74133=CARTESIAN_POINT('Ctrl Pts',(78.2849620104029,-10.1339022959532,134.261055880609));
#74134=CARTESIAN_POINT('Ctrl Pts',(78.2466158057055,-10.0736478315659,134.257196477887));
#74135=CARTESIAN_POINT('Ctrl Pts',(78.2115313003927,-10.0116211113973,134.253337075164));
#74136=CARTESIAN_POINT('Ctrl Pts',(78.1764269299573,-9.94955927121262,134.249475487217));
#74137=CARTESIAN_POINT('Ctrl Pts',(78.144588152236,-9.8857236125756,134.24561389927));
#74138=CARTESIAN_POINT('Ctrl Pts',(78.1161780375013,-9.82049520175772,134.241752311323));
#74139=CARTESIAN_POINT('Ctrl Pts',(78.0877182182525,-9.75515267149706,134.23788396739));
#74140=CARTESIAN_POINT('Ctrl Pts',(78.0626992088762,-9.68841297919082,134.234015623456));
#74141=CARTESIAN_POINT('Ctrl Pts',(78.0412348877942,-9.62067446999657,134.230147279523));
#74142=CARTESIAN_POINT('Ctrl Pts',(78.0284899916253,-9.58045329258207,134.227850368216));
#74143=CARTESIAN_POINT('Ctrl Pts',(78.0169973859048,-9.53988022519759,134.22555345691));
#74144=CARTESIAN_POINT('Ctrl Pts',(78.0067723452924,-9.49904015771159,134.223256545603));
#74145=CARTESIAN_POINT('Ctrl Pts',(77.9843222460634,-9.40937170529799,134.218213447125));
#74146=CARTESIAN_POINT('Ctrl Pts',(77.967913679714,-9.31813449884541,134.213170348647));
#74147=CARTESIAN_POINT('Ctrl Pts',(77.9577201042085,-9.22603183347914,134.208127250169));
#74148=CARTESIAN_POINT('Ctrl Pts',(77.9494988556529,-9.15174986007309,134.204059926976));
#74149=CARTESIAN_POINT('Ctrl Pts',(77.9453194352602,-9.07690516324679,134.199992603783));
#74150=CARTESIAN_POINT('Ctrl Pts',(77.9452508583196,-9.00187810112594,134.19592528059));
#74151=CARTESIAN_POINT('Ctrl Pts',(77.9452508583188,-9.00187810017601,134.195925280538));
#74152=CARTESIAN_POINT('Ctrl Pts',(77.9451865584667,-8.93153037992358,134.192111631088));
#74153=CARTESIAN_POINT('Ctrl Pts',(77.9487392155753,-8.86108771113924,134.188297981638));
#74154=CARTESIAN_POINT('Ctrl Pts',(77.9559113871452,-8.79095621201019,134.184484332188));
#74155=CARTESIAN_POINT('Ctrl Pts',(77.9630788626377,-8.72087063243831,134.180673179777));
#74156=CARTESIAN_POINT('Ctrl Pts',(77.9738611037571,-8.65109631311334,134.176862027366));
#74157=CARTESIAN_POINT('Ctrl Pts',(77.9882086454291,-8.58203695357894,134.173050874956));
#74158=CARTESIAN_POINT('Ctrl Pts',(78.0025518660922,-8.51299839245752,134.169240870339));
#74159=CARTESIAN_POINT('Ctrl Pts',(78.0204581554943,-8.44467485161844,134.165430865722));
#74160=CARTESIAN_POINT('Ctrl Pts',(78.0418267999905,-8.37746061870398,134.161620861105));
#74161=CARTESIAN_POINT('Ctrl Pts',(78.0631965645668,-8.31024286262121,134.15781065678));
#74162=CARTESIAN_POINT('Ctrl Pts',(78.0880288903436,-8.24413500386008,134.154000452454));
#74163=CARTESIAN_POINT('Ctrl Pts',(78.1161735511138,-8.17951509887334,134.150190248128));
#74164=CARTESIAN_POINT('Ctrl Pts',(78.1443474516825,-8.11482805955463,134.146376085339));
#74165=CARTESIAN_POINT('Ctrl Pts',(78.1758403520862,-8.05163251518824,134.14256192255));
#74166=CARTESIAN_POINT('Ctrl Pts',(78.210454788899,-7.99028444603172,134.138747759761));
#74167=CARTESIAN_POINT('Ctrl Pts',(78.2450904309211,-7.92889879432974,134.134931260371));
#74168=CARTESIAN_POINT('Ctrl Pts',(78.2828511440636,-7.86936328817681,134.131114760981));
#74169=CARTESIAN_POINT('Ctrl Pts',(78.3234961567948,-7.81200487113028,134.127298261591));
#74170=CARTESIAN_POINT('Ctrl Pts',(78.3642086074958,-7.75455128533028,134.123475429888));
#74171=CARTESIAN_POINT('Ctrl Pts',(78.407814592662,-7.69928238170397,134.119652598184));
#74172=CARTESIAN_POINT('Ctrl Pts',(78.4540338348352,-7.64649116047744,134.115829766481));
#74173=CARTESIAN_POINT('Ctrl Pts',(78.4689707705123,-7.62943032090719,134.114594320191));
#74174=CARTESIAN_POINT('Ctrl Pts',(78.4841803654163,-7.61262795755886,134.113358873901));
#74175=CARTESIAN_POINT('Ctrl Pts',(78.4996524028237,-7.5960930763946,134.112123427611));
#74176=CARTESIAN_POINT('Ctrl Pts',(78.5481066294738,-7.54431031123745,134.108254344765));
#74177=CARTESIAN_POINT('Ctrl Pts',(78.5993397400987,-7.49493758081945,134.104385261918));
#74178=CARTESIAN_POINT('Ctrl Pts',(78.6530824932534,-7.44828778682404,134.100516179071));
#74179=CARTESIAN_POINT('Ctrl Pts',(78.7067451723861,-7.40170749869516,134.096652860964));
#74180=CARTESIAN_POINT('Ctrl Pts',(78.7629097078898,-7.35784240972122,134.092789542858));
#74181=CARTESIAN_POINT('Ctrl Pts',(78.8212689947725,-7.31696976265564,134.088926224751));
#74182=CARTESIAN_POINT('Ctrl Pts',(78.8795598262342,-7.27614505918933,134.085067438316));
#74183=CARTESIAN_POINT('Ctrl Pts',(78.9400398993904,-7.23830610264095,134.08120865188));
#74184=CARTESIAN_POINT('Ctrl Pts',(79.0023692611183,-7.20368976194578,134.077349865444));
#74185=CARTESIAN_POINT('Ctrl Pts',(79.0646593599188,-7.16909522700693,134.073493509761));
#74186=CARTESIAN_POINT('Ctrl Pts',(79.1287960124367,-7.13771951571177,134.069637154078));
#74187=CARTESIAN_POINT('Ctrl Pts',(79.1944117734195,-7.10975526142912,134.065780798394));
#74188=CARTESIAN_POINT('Ctrl Pts',(79.2600081508495,-7.0817992680672,134.061925581917));
#74189=CARTESIAN_POINT('Ctrl Pts',(79.3270823226429,-7.05725292135065,134.05807036544));
#74190=CARTESIAN_POINT('Ctrl Pts',(79.3952453929246,-7.03626136471245,134.054215148963));
#74191=CARTESIAN_POINT('Ctrl Pts',(79.4634111281785,-7.01526898736714,134.050359781758));
#74192=CARTESIAN_POINT('Ctrl Pts',(79.5326653815287,-6.99783181690051,134.046504414553));
#74193=CARTESIAN_POINT('Ctrl Pts',(79.6026042328258,-6.98404509804113,134.042649047349));
#74194=CARTESIAN_POINT('Ctrl Pts',(79.6726162910286,-6.97024394824659,134.038789644626));
#74195=CARTESIAN_POINT('Ctrl Pts',(79.7433139000598,-6.96010097183086,134.034930241903));
#74196=CARTESIAN_POINT('Ctrl Pts',(79.8142839731725,-6.95366006736921,134.03107083918));
#74197=CARTESIAN_POINT('Ctrl Pts',(79.8852942300982,-6.94721551601684,134.027209251233));
#74198=CARTESIAN_POINT('Ctrl Pts',(79.9565767725572,-6.94447722804744,134.023347663287));
#74199=CARTESIAN_POINT('Ctrl Pts',(80.0277171909406,-6.94543695160592,134.01948607534));
#74200=CARTESIAN_POINT('Ctrl Pts',(80.0989820720358,-6.94639835423517,134.015617731406));
#74201=CARTESIAN_POINT('Ctrl Pts',(80.1701038477248,-6.95107065368359,134.011749387473));
#74202=CARTESIAN_POINT('Ctrl Pts',(80.2406726110882,-6.95939365462812,134.007881043539));
#74203=CARTESIAN_POINT('Ctrl Pts',(80.2825743119812,-6.96433561307386,134.005584132233));
#74204=CARTESIAN_POINT('Ctrl Pts',(80.3242812036117,-6.97056369253628,134.003287220926));
#74205=CARTESIAN_POINT('Ctrl Pts',(80.3657096343967,-6.97805686879937,134.00099030962));
#74206=CARTESIAN_POINT('Ctrl Pts',(80.435496785936,-6.99067929782875,133.997121109306));
#74207=CARTESIAN_POINT('Ctrl Pts',(80.5047663681027,-7.00694373601728,133.993251908991));
#74208=CARTESIAN_POINT('Ctrl Pts',(80.5731094334077,-7.02679369050293,133.989382708677));
#74209=CARTESIAN_POINT('Ctrl Pts',(80.6413358826972,-7.04660977435969,133.985520110506));
#74210=CARTESIAN_POINT('Ctrl Pts',(80.7086384934941,-7.0699990848956,133.981657512335));
#74211=CARTESIAN_POINT('Ctrl Pts',(80.7746179998118,-7.09685404740793,133.977794914165));
#74212=CARTESIAN_POINT('Ctrl Pts',(80.8405321010276,-7.12368238875172,133.973936144965));
#74213=CARTESIAN_POINT('Ctrl Pts',(80.9051252521817,-7.15396938460669,133.970077375765));
#74214=CARTESIAN_POINT('Ctrl Pts',(80.9680140702184,-7.18755791199851,133.966218606566));
#74215=CARTESIAN_POINT('Ctrl Pts',(81.030862599658,-7.22112492150066,133.962362309417));
#74216=CARTESIAN_POINT('Ctrl Pts',(81.0920085350432,-7.25798903737295,133.958506012269));
#74217=CARTESIAN_POINT('Ctrl Pts',(81.1510907558965,-7.29794605426575,133.954649715121));
#74218=CARTESIAN_POINT('Ctrl Pts',(81.1854604267632,-7.32119009451308,133.952406406359));
#74219=CARTESIAN_POINT('Ctrl Pts',(81.2191321632765,-7.34547991695526,133.950163097596));
#74220=CARTESIAN_POINT('Ctrl Pts',(81.2520391107129,-7.37076839346111,133.947919788834));
#74221=CARTESIAN_POINT('',(77.9452507619582,-8.99823046142755,134.254074719427));
#74222=CARTESIAN_POINT('Ctrl Pts',(77.9452507619582,-8.99823046142755,134.254074719427));
#74223=CARTESIAN_POINT('Ctrl Pts',(77.9453248874363,-8.91215758797735,134.249416661534));
#74224=CARTESIAN_POINT('Ctrl Pts',(77.9508111829309,-8.82632098520286,134.24475860364));
#74225=CARTESIAN_POINT('Ctrl Pts',(77.9615982093287,-8.74131930437674,134.240100545746));
#74226=CARTESIAN_POINT('Ctrl Pts',(77.9725417920147,-8.65508396126522,134.235374883656));
#74227=CARTESIAN_POINT('Ctrl Pts',(77.9889410126122,-8.56970793661434,134.230649221565));
#74228=CARTESIAN_POINT('Ctrl Pts',(78.0106307458957,-8.48579426945562,134.225923559475));
#74229=CARTESIAN_POINT('Ctrl Pts',(78.0180442984579,-8.45711257134388,134.224308327796));
#74230=CARTESIAN_POINT('Ctrl Pts',(78.0260755171318,-8.42860153023918,134.222693096118));
#74231=CARTESIAN_POINT('Ctrl Pts',(78.0347165430364,-8.40028465395229,134.221077864439));
#74232=CARTESIAN_POINT('Ctrl Pts',(78.0554150258306,-8.33245516436548,134.217208781592));
#74233=CARTESIAN_POINT('Ctrl Pts',(78.0796697562115,-8.26556565706135,134.213339698745));
#74234=CARTESIAN_POINT('Ctrl Pts',(78.1073768028461,-8.20001562759332,134.209470615898));
#74235=CARTESIAN_POINT('Ctrl Pts',(78.135042567363,-8.13456326440015,134.205607297792));
#74236=CARTESIAN_POINT('Ctrl Pts',(78.1661502502832,-8.07044686133226,134.201743979686));
#74237=CARTESIAN_POINT('Ctrl Pts',(78.2005462224255,-8.0080505734299,134.197880661579));
#74238=CARTESIAN_POINT('Ctrl Pts',(78.2349018481057,-7.94572747634918,134.194021875143));
#74239=CARTESIAN_POINT('Ctrl Pts',(78.2725378680003,-7.88512090997112,134.190163088708));
#74240=CARTESIAN_POINT('Ctrl Pts',(78.3132533816179,-7.82659324704664,134.186304302272));
#74241=CARTESIAN_POINT('Ctrl Pts',(78.3539432474475,-7.76810245225814,134.182447946588));
#74242=CARTESIAN_POINT('Ctrl Pts',(78.3977084815971,-7.71168836062039,134.178591590905));
#74243=CARTESIAN_POINT('Ctrl Pts',(78.4443040202919,-7.65768573678892,134.174735235222));
#74244=CARTESIAN_POINT('Ctrl Pts',(78.4908857941979,-7.60369906587329,134.170880018745));
#74245=CARTESIAN_POINT('Ctrl Pts',(78.5402958955815,-7.55212281610491,134.167024802267));
#74246=CARTESIAN_POINT('Ctrl Pts',(78.5922490883443,-7.50325856166388,134.16316958579));
#74247=CARTESIAN_POINT('Ctrl Pts',(78.6442043123216,-7.45439239677664,134.159314218586));
#74248=CARTESIAN_POINT('Ctrl Pts',(78.6987024697097,-7.40823876894237,134.155458851381));
#74249=CARTESIAN_POINT('Ctrl Pts',(78.7554228609497,-7.36506106919762,134.151603484176));
#74250=CARTESIAN_POINT('Ctrl Pts',(78.8122026229723,-7.32183817417522,134.147744081453));
#74251=CARTESIAN_POINT('Ctrl Pts',(78.8712088748859,-7.28159772029608,134.143884678731));
#74252=CARTESIAN_POINT('Ctrl Pts',(78.932090075322,-7.24456103630057,134.140025276008));
#74253=CARTESIAN_POINT('Ctrl Pts',(78.9930057471719,-7.20750338184365,134.136163688061));
#74254=CARTESIAN_POINT('Ctrl Pts',(79.0557980530734,-7.17365333900788,134.132302100114));
#74255=CARTESIAN_POINT('Ctrl Pts',(79.120091297845,-7.14318599790613,134.128440512167));
#74256=CARTESIAN_POINT('Ctrl Pts',(79.1844970259528,-7.11266535309906,134.124572168233));
#74257=CARTESIAN_POINT('Ctrl Pts',(79.2504084863379,-7.08553941073387,134.1207038243));
#74258=CARTESIAN_POINT('Ctrl Pts',(79.3174311513888,-7.06193464263828,134.116835480367));
#74259=CARTESIAN_POINT('Ctrl Pts',(79.3572272811514,-7.04791881062928,134.11453856906));
#74260=CARTESIAN_POINT('Ctrl Pts',(79.3974148942614,-7.03514346187569,134.112241657754));
#74261=CARTESIAN_POINT('Ctrl Pts',(79.4379096287717,-7.02362655930808,134.109944746447));
#74262=CARTESIAN_POINT('Ctrl Pts',(79.5061249302259,-7.00422579054222,134.10607549038));
#74263=CARTESIAN_POINT('Ctrl Pts',(79.5754794623163,-6.98832288444096,134.102206234313));
#74264=CARTESIAN_POINT('Ctrl Pts',(79.645581172235,-6.97604721966502,134.098336978247));
#74265=CARTESIAN_POINT('Ctrl Pts',(79.7155609766724,-6.96379290202634,134.094474450739));
#74266=CARTESIAN_POINT('Ctrl Pts',(79.7862849026504,-6.95515337539077,134.090611923232));
#74267=CARTESIAN_POINT('Ctrl Pts',(79.8573471332508,-6.95020788319687,134.086749395724));
#74268=CARTESIAN_POINT('Ctrl Pts',(79.9283395278624,-6.94526725115633,134.082890664093));
#74269=CARTESIAN_POINT('Ctrl Pts',(79.9996690856365,-6.94401348583595,134.079031932462));
#74270=CARTESIAN_POINT('Ctrl Pts',(80.0709224192402,-6.94647435541965,134.07517320083));
#74271=CARTESIAN_POINT('Ctrl Pts',(80.1421295659897,-6.94893362985238,134.071316970453));
#74272=CARTESIAN_POINT('Ctrl Pts',(80.2132601023311,-6.95510274416918,134.067460740076));
#74273=CARTESIAN_POINT('Ctrl Pts',(80.2838999035947,-6.9649573942448,134.063604509698));
#74274=CARTESIAN_POINT('Ctrl Pts',(80.3545175459512,-6.97480895302809,134.059749488977));
#74275=CARTESIAN_POINT('Ctrl Pts',(80.4246442782307,-6.9883436841954,134.055894468255));
#74276=CARTESIAN_POINT('Ctrl Pts',(80.4938720915139,-7.0054855428642,134.052039447534));
#74277=CARTESIAN_POINT('Ctrl Pts',(80.5631419758923,-7.02263781897557,134.048182084041));
#74278=CARTESIAN_POINT('Ctrl Pts',(80.6315113758258,-7.04340149176895,134.044324720548));
#74279=CARTESIAN_POINT('Ctrl Pts',(80.6985844526089,-7.06764979233238,134.040467357055));
#74280=CARTESIAN_POINT('Ctrl Pts',(80.7656748958074,-7.09190437121314,134.036608994821));
#74281=CARTESIAN_POINT('Ctrl Pts',(80.831467895916,-7.11964519319846,134.032750632588));
#74282=CARTESIAN_POINT('Ctrl Pts',(80.8955871455516,-7.15069709695175,134.028892270355));
#74283=CARTESIAN_POINT('Ctrl Pts',(80.9598054148642,-7.18179695431484,134.025027949634));
#74284=CARTESIAN_POINT('Ctrl Pts',(81.0223443385685,-7.21621788193465,134.021163628913));
#74285=CARTESIAN_POINT('Ctrl Pts',(81.0828523129242,-7.25373872776877,134.017299308192));
#74286=CARTESIAN_POINT('Ctrl Pts',(81.141234597276,-7.28994143846816,134.013570743923));
#74287=CARTESIAN_POINT('Ctrl Pts',(81.1977259690068,-7.32902959010821,134.009842179654));
#74288=CARTESIAN_POINT('Ctrl Pts',(81.2520391107129,-7.3707683934611,134.006113615385));
#74289=CARTESIAN_POINT('Ctrl Pts',(81.2520391107129,-7.37076839346111,134.706120114083));
#74290=CARTESIAN_POINT('Ctrl Pts',(81.308617435007,-7.41424795434766,134.702260546292));
#74291=CARTESIAN_POINT('Ctrl Pts',(81.3628983050282,-7.46065513417077,134.6984009785));
#74292=CARTESIAN_POINT('Ctrl Pts',(81.4145767289439,-7.50970800162167,134.694541410709));
#74293=CARTESIAN_POINT('Ctrl Pts',(81.4662859532541,-7.55879010463279,134.690679542611));
#74294=CARTESIAN_POINT('Ctrl Pts',(81.5153893099384,-7.61052068126371,134.686817674514));
#74295=CARTESIAN_POINT('Ctrl Pts',(81.5616202022989,-7.66458249739198,134.682955806416));
#74296=CARTESIAN_POINT('Ctrl Pts',(81.6079305750915,-7.71873725692424,134.679087298971));
#74297=CARTESIAN_POINT('Ctrl Pts',(81.6513583306771,-7.77523087073858,134.675218791526));
#74298=CARTESIAN_POINT('Ctrl Pts',(81.691678980054,-7.83371539024845,134.671350284081));
#74299=CARTESIAN_POINT('Ctrl Pts',(81.711621074086,-7.86264110958842,134.669436968189));
#74300=CARTESIAN_POINT('Ctrl Pts',(81.7308038121415,-7.8920534289855,134.667523652297));
#74301=CARTESIAN_POINT('Ctrl Pts',(81.7492042338686,-7.9219081158287,134.665610336405));
#74302=CARTESIAN_POINT('Ctrl Pts',(81.7864133305879,-7.98227988049495,134.661741253558));
#74303=CARTESIAN_POINT('Ctrl Pts',(81.8205661439275,-8.04469849530034,134.657872170711));
#74304=CARTESIAN_POINT('Ctrl Pts',(81.8514316391579,-8.10882187637653,134.654003087864));
#74305=CARTESIAN_POINT('Ctrl Pts',(81.8822511463398,-8.17284971681296,134.650139769758));
#74306=CARTESIAN_POINT('Ctrl Pts',(81.9097928487125,-8.2385768475084,134.646276451652));
#74307=CARTESIAN_POINT('Ctrl Pts',(81.9338700765014,-8.30563403761968,134.642413133545));
#74308=CARTESIAN_POINT('Ctrl Pts',(81.9579190617114,-8.37261256967272,134.638554347109));
#74309=CARTESIAN_POINT('Ctrl Pts',(81.9785114811098,-8.44091760715137,134.634695560674));
#74310=CARTESIAN_POINT('Ctrl Pts',(81.995508258998,-8.51015885149286,134.630836774238));
#74311=CARTESIAN_POINT('Ctrl Pts',(82.0124943301625,-8.57935647892769,134.626980418555));
#74312=CARTESIAN_POINT('Ctrl Pts',(82.0258891379882,-8.64948867252513,134.623124062871));
#74313=CARTESIAN_POINT('Ctrl Pts',(82.035603517282,-8.72015024936765,134.619267707188));
#74314=CARTESIAN_POINT('Ctrl Pts',(82.0453150268509,-8.79079095207278,134.615412490711));
#74315=CARTESIAN_POINT('Ctrl Pts',(82.0513482002261,-8.86196024656078,134.611557274234));
#74316=CARTESIAN_POINT('Ctrl Pts',(82.0536653328037,-8.93324475046548,134.607702057756));
#74317=CARTESIAN_POINT('Ctrl Pts',(82.0559825559742,-9.0045320413811,134.603846690552));
#74318=CARTESIAN_POINT('Ctrl Pts',(82.0545834363202,-9.07593406505799,134.599991323347));
#74319=CARTESIAN_POINT('Ctrl Pts',(82.0494823628482,-9.14703607337761,134.596135956143));
#74320=CARTESIAN_POINT('Ctrl Pts',(82.0443759499432,-9.21821250611137,134.59227655342));
#74321=CARTESIAN_POINT('Ctrl Pts',(82.0355598828126,-9.28908781107467,134.588417150697));
#74322=CARTESIAN_POINT('Ctrl Pts',(82.0231004992737,-9.35925190652057,134.584557747974));
#74323=CARTESIAN_POINT('Ctrl Pts',(82.0106340611339,-9.42945572942843,134.580696160027));
#74324=CARTESIAN_POINT('Ctrl Pts',(81.9945203098238,-9.49894706773126,134.57683457208));
#74325=CARTESIAN_POINT('Ctrl Pts',(81.9748762440994,-9.56732828502722,134.572972984133));
#74326=CARTESIAN_POINT('Ctrl Pts',(81.9551978103779,-9.63582913771395,134.5691046402));
#74327=CARTESIAN_POINT('Ctrl Pts',(81.9319768891766,-9.70321553231904,134.565236296267));
#74328=CARTESIAN_POINT('Ctrl Pts',(81.905379407727,-9.76910784361488,134.561367952333));
#74329=CARTESIAN_POINT('Ctrl Pts',(81.8895865886511,-9.80823280184666,134.559071041027));
#74330=CARTESIAN_POINT('Ctrl Pts',(81.8726042233082,-9.84683141646728,134.55677412972));
#74331=CARTESIAN_POINT('Ctrl Pts',(81.8544746051535,-9.88482851521686,134.554477218414));
#74332=CARTESIAN_POINT('Ctrl Pts',(81.82393577049,-9.94883356521285,134.550608135567));
#74333=CARTESIAN_POINT('Ctrl Pts',(81.7900196413615,-10.0113811016805,134.54673905272));
#74334=CARTESIAN_POINT('Ctrl Pts',(81.7528883050505,-10.0720914851435,134.542869969873));
#74335=CARTESIAN_POINT('Ctrl Pts',(81.7158122925787,-10.132711413163,134.539006651767));
#74336=CARTESIAN_POINT('Ctrl Pts',(81.6755308333298,-10.1914992105347,134.53514333366));
#74337=CARTESIAN_POINT('Ctrl Pts',(81.6322528843363,-10.2480977862635,134.531280015554));
#74338=CARTESIAN_POINT('Ctrl Pts',(81.5890257003603,-10.3046299718848,134.527421229118));
#74339=CARTESIAN_POINT('Ctrl Pts',(81.5428093020267,-10.35897765267,134.523562442682));
#74340=CARTESIAN_POINT('Ctrl Pts',(81.4938561601465,-10.4108122962649,134.519703656246));
#74341=CARTESIAN_POINT('Ctrl Pts',(81.4449338551562,-10.4626142878352,134.515847300563));
#74342=CARTESIAN_POINT('Ctrl Pts',(81.3932785596599,-10.5119060305783,134.51199094488));
#74343=CARTESIAN_POINT('Ctrl Pts',(81.3391823197829,-10.5583928506255,134.508134589197));
#74344=CARTESIAN_POINT('Ctrl Pts',(81.2851020604768,-10.6048659380007,134.504279372719));
#74345=CARTESIAN_POINT('Ctrl Pts',(81.2285826565668,-10.6485354312491,134.500424156242));
#74346=CARTESIAN_POINT('Ctrl Pts',(81.1699509540173,-10.6891454430255,134.496568939765));
#74347=CARTESIAN_POINT('Ctrl Pts',(81.1113169591439,-10.7297570425318,134.49271357256));
#74348=CARTESIAN_POINT('Ctrl Pts',(81.0505709022714,-10.767308648295,134.488858205356));
#74349=CARTESIAN_POINT('Ctrl Pts',(80.9880690313273,-10.8015873977778,134.485002838151));
#74350=CARTESIAN_POINT('Ctrl Pts',(80.9255017379676,-10.8359020277641,134.481143435428));
#74351=CARTESIAN_POINT('Ctrl Pts',(80.8611753885617,-10.8669367287521,134.477284032705));
#74352=CARTESIAN_POINT('Ctrl Pts',(80.7954704866765,-10.894524813067,134.473424629983));
#74353=CARTESIAN_POINT('Ctrl Pts',(80.7297283821598,-10.922128517972,134.469563042036));
#74354=CARTESIAN_POINT('Ctrl Pts',(80.6626066286419,-10.9462815568095,134.465701454089));
#74355=CARTESIAN_POINT('Ctrl Pts',(80.5945027514398,-10.9668665539458,134.461839866142));
#74356=CARTESIAN_POINT('Ctrl Pts',(80.5262797240634,-10.9874875652724,134.457971522208));
#74357=CARTESIAN_POINT('Ctrl Pts',(80.4570716142915,-11.0045279555587,134.454103178275));
#74358=CARTESIAN_POINT('Ctrl Pts',(80.3872873535,-11.0179212245078,134.450234834341));
#74359=CARTESIAN_POINT('Ctrl Pts',(80.3458514676581,-11.025873762185,134.447937923035));
#74360=CARTESIAN_POINT('Ctrl Pts',(80.3042125940091,-11.0325414442796,134.445641011729));
#74361=CARTESIAN_POINT('Ctrl Pts',(80.2624568263926,-11.0379190309676,134.443344100422));
#74362=CARTESIAN_POINT('Ctrl Pts',(80.1921204038274,-11.0469774253227,134.439475017575));
#74363=CARTESIAN_POINT('Ctrl Pts',(80.1211767085351,-11.0524079162304,134.435605934728));
#74364=CARTESIAN_POINT('Ctrl Pts',(80.0500326011497,-11.0541407695974,134.431736851881));
#74365=CARTESIAN_POINT('Ctrl Pts',(79.9789944949364,-11.0558710410993,134.427873533775));
#74366=CARTESIAN_POINT('Ctrl Pts',(79.9077570510336,-11.0539145991276,134.424010215668));
#74367=CARTESIAN_POINT('Ctrl Pts',(79.8367336075802,-11.0482533162688,134.420146897562));
#74368=CARTESIAN_POINT('Ctrl Pts',(79.7657934745984,-11.0425986740926,134.416288111126));
#74369=CARTESIAN_POINT('Ctrl Pts',(79.6950673253476,-11.0332478616258,134.41242932469));
#74370=CARTESIAN_POINT('Ctrl Pts',(79.6249681059247,-11.0202347984644,134.408570538255));
#74371=CARTESIAN_POINT('Ctrl Pts',(79.5549130438699,-11.0072299325785,134.404714182571));
#74372=CARTESIAN_POINT('Ctrl Pts',(79.4854846046223,-10.9905674814048,134.400857826888));
#74373=CARTESIAN_POINT('Ctrl Pts',(79.4170887535173,-10.9703329772462,134.397001471205));
#74374=CARTESIAN_POINT('Ctrl Pts',(79.3487131072313,-10.9501044505627,134.393146254728));
#74375=CARTESIAN_POINT('Ctrl Pts',(79.2813699090765,-10.9263061035359,134.38929103825));
#74376=CARTESIAN_POINT('Ctrl Pts',(79.2154514132945,-10.8990737420117,134.385435821773));
#74377=CARTESIAN_POINT('Ctrl Pts',(79.1495303402965,-10.8718403157837,134.381580454569));
#74378=CARTESIAN_POINT('Ctrl Pts',(79.0850345283964,-10.8411727960219,134.377725087364));
#74379=CARTESIAN_POINT('Ctrl Pts',(79.0223360323177,-10.8072550259428,134.373869720159));
#74380=CARTESIAN_POINT('Ctrl Pts',(78.9595719080107,-10.7733017532076,134.370010317437));
#74381=CARTESIAN_POINT('Ctrl Pts',(78.8986092831664,-10.7360916703621,134.366150914714));
#74382=CARTESIAN_POINT('Ctrl Pts',(78.83979457526,-10.6958540429247,134.362291511991));
#74383=CARTESIAN_POINT('Ctrl Pts',(78.7809465660041,-10.6555936326265,134.358429924044));
#74384=CARTESIAN_POINT('Ctrl Pts',(78.7242492809845,-10.6123025602003,134.354568336097));
#74385=CARTESIAN_POINT('Ctrl Pts',(78.6700169412625,-10.5662511375802,134.35070674815));
#74386=CARTESIAN_POINT('Ctrl Pts',(78.6156897201183,-10.5201191463456,134.346838404217));
#74387=CARTESIAN_POINT('Ctrl Pts',(78.5638364078437,-10.4712174964199,134.342970060283));
#74388=CARTESIAN_POINT('Ctrl Pts',(78.5147346698684,-10.4198536761262,134.33910171635));
#74389=CARTESIAN_POINT('Ctrl Pts',(78.4855794708835,-10.3893553177577,134.336804805043));
#74390=CARTESIAN_POINT('Ctrl Pts',(78.4573936249819,-10.3579895422356,134.334507893737));
#74391=CARTESIAN_POINT('Ctrl Pts',(78.4302282299173,-10.3258258378653,134.332210982431));
#74392=CARTESIAN_POINT('Ctrl Pts',(78.3847678948151,-10.2720010075869,134.328367181984));
#74393=CARTESIAN_POINT('Ctrl Pts',(78.3419831696141,-10.2157215771965,134.324523381537));
#74394=CARTESIAN_POINT('Ctrl Pts',(78.3021523840387,-10.1572860646679,134.32067958109));
#74395=CARTESIAN_POINT('Ctrl Pts',(78.2623775799222,-10.0989326822102,134.316841183036));
#74396=CARTESIAN_POINT('Ctrl Pts',(78.2255487573435,-10.0384296294759,134.313002784982));
#74397=CARTESIAN_POINT('Ctrl Pts',(78.1919047913618,-9.97610925566744,134.309164386928));
#74398=CARTESIAN_POINT('Ctrl Pts',(78.1582964950696,-9.91385495458019,134.305330058384));
#74399=CARTESIAN_POINT('Ctrl Pts',(78.1278665893411,-9.8497875856462,134.301495729841));
#74400=CARTESIAN_POINT('Ctrl Pts',(78.1008102845208,-9.78426780318845,134.297661401297));
#74401=CARTESIAN_POINT('Ctrl Pts',(78.0737690938031,-9.71878462117251,134.293829214673));
#74402=CARTESIAN_POINT('Ctrl Pts',(78.0500979587486,-9.65185108679847,134.289997028049));
#74403=CARTESIAN_POINT('Ctrl Pts',(78.029945075938,-9.58385028789842,134.286164841426));
#74404=CARTESIAN_POINT('Ctrl Pts',(78.0097994694122,-9.51587404097869,134.282334038429));
#74405=CARTESIAN_POINT('Ctrl Pts',(77.9931697296341,-9.4468317675747,134.278503235433));
#74406=CARTESIAN_POINT('Ctrl Pts',(77.9801543906818,-9.37712236345498,134.274672432436));
#74407=CARTESIAN_POINT('Ctrl Pts',(77.9671331495257,-9.30738134747254,134.270839892245));
#74408=CARTESIAN_POINT('Ctrl Pts',(77.9577296763164,-9.23697308077803,134.267007352054));
#74409=CARTESIAN_POINT('Ctrl Pts',(77.9519912481155,-9.1663060873945,134.263174811862));
#74410=CARTESIAN_POINT('Ctrl Pts',(77.9474494190888,-9.11037484794392,134.260141447729));
#74411=CARTESIAN_POINT('Ctrl Pts',(77.9452024908778,-9.05428179787052,134.257108083595));
#74412=CARTESIAN_POINT('Ctrl Pts',(77.9452507619577,-8.99823046207066,134.254074719462));
#74413=CARTESIAN_POINT('Origin',(80.,-9.,141.545925280538));
#74414=CARTESIAN_POINT('',(81.2520391107129,-7.37076839346111,135.406026966566));
#74415=CARTESIAN_POINT('',(81.2520391107129,-7.37076839346111,135.347982838348));
#74416=CARTESIAN_POINT('',(81.2520391107129,-7.37076839346111,141.545925280538));
#74417=CARTESIAN_POINT('',(77.9452501039006,-8.99934656332038,134.895925280576));
#74418=CARTESIAN_POINT('Ctrl Pts',(81.2520391107129,-7.37076839346111,135.347982838348));
#74419=CARTESIAN_POINT('Ctrl Pts',(81.3084942669191,-7.41415330159074,135.344113662368));
#74420=CARTESIAN_POINT('Ctrl Pts',(81.3626078704091,-7.46041147904279,135.340244486388));
#74421=CARTESIAN_POINT('Ctrl Pts',(81.4140911496352,-7.50924724282546,135.336375310408));
#74422=CARTESIAN_POINT('Ctrl Pts',(81.4220196881186,-7.51676805809484,135.335779448778));
#74423=CARTESIAN_POINT('Ctrl Pts',(81.4298859208187,-7.52434994013014,135.335183587148));
#74424=CARTESIAN_POINT('Ctrl Pts',(81.4376888783051,-7.53199173990814,135.334587725519));
#74425=CARTESIAN_POINT('Ctrl Pts',(81.4883554885787,-7.5816119117233,135.330718642672));
#74426=CARTESIAN_POINT('Ctrl Pts',(81.5365494452544,-7.63395539912312,135.326849559825));
#74427=CARTESIAN_POINT('Ctrl Pts',(81.5819640552087,-7.68874590924272,135.322980476978));
#74428=CARTESIAN_POINT('Ctrl Pts',(81.6273109996591,-7.74345478423476,135.319117158872));
#74429=CARTESIAN_POINT('Ctrl Pts',(81.6698865098525,-7.80060307389247,135.315253840765));
#74430=CARTESIAN_POINT('Ctrl Pts',(81.7094204040751,-7.85987744315283,135.311390522659));
#74431=CARTESIAN_POINT('Ctrl Pts',(81.748907925055,-7.91908228360087,135.307531736223));
#74432=CARTESIAN_POINT('Ctrl Pts',(81.7853606487122,-7.98040784776143,135.303672949787));
#74433=CARTESIAN_POINT('Ctrl Pts',(81.8185495042662,-8.04350887979387,135.299814163351));
#74434=CARTESIAN_POINT('Ctrl Pts',(81.8517174532748,-8.10657016280314,135.295957807668));
#74435=CARTESIAN_POINT('Ctrl Pts',(81.8816253876486,-8.17140426584292,135.292101451985));
#74436=CARTESIAN_POINT('Ctrl Pts',(81.9080890863941,-8.23763945479594,135.288245096302));
#74437=CARTESIAN_POINT('Ctrl Pts',(81.934544967498,-8.30385507721092,135.284389879824));
#74438=CARTESIAN_POINT('Ctrl Pts',(81.9575584527788,-8.37147051297918,135.280534663347));
#74439=CARTESIAN_POINT('Ctrl Pts',(81.9769932870615,-8.44009366371367,135.27667944687));
#74440=CARTESIAN_POINT('Ctrl Pts',(81.9964288811882,-8.50871949740812,135.272824079665));
#74441=CARTESIAN_POINT('Ctrl Pts',(82.0122854162816,-8.5783526562895,135.268968712461));
#74442=CARTESIAN_POINT('Ctrl Pts',(82.0244768648761,-8.64858715720481,135.265113345256));
#74443=CARTESIAN_POINT('Ctrl Pts',(82.0366810745929,-8.71889517449053,135.261253942533));
#74444=CARTESIAN_POINT('Ctrl Pts',(82.0452124563531,-8.78980531070922,135.25739453981));
#74445=CARTESIAN_POINT('Ctrl Pts',(82.0500365241631,-8.86090358704329,135.253535137088));
#74446=CARTESIAN_POINT('Ctrl Pts',(82.0548633233981,-8.93204211977993,135.249673549141));
#74447=CARTESIAN_POINT('Ctrl Pts',(82.0559786224031,-9.0033685187395,135.245811961194));
#74448=CARTESIAN_POINT('Ctrl Pts',(82.0534001022136,-9.07446866944749,135.241950373247));
#74449=CARTESIAN_POINT('Ctrl Pts',(82.0508170708106,-9.14569321241763,135.238082029313));
#74450=CARTESIAN_POINT('Ctrl Pts',(82.0445273605926,-9.21669023281058,135.23421368538));
#74451=CARTESIAN_POINT('Ctrl Pts',(82.0346004801354,-9.28705129982747,135.230345341446));
#74452=CARTESIAN_POINT('Ctrl Pts',(82.0287061841907,-9.32882967660675,135.22804843014));
#74453=CARTESIAN_POINT('Ctrl Pts',(82.0215305338992,-9.37038402446779,135.225751518834));
#74454=CARTESIAN_POINT('Ctrl Pts',(82.0130964518113,-9.41163119197237,135.223454607527));
#74455=CARTESIAN_POINT('Ctrl Pts',(81.9988894764508,-9.48111089187594,135.21958552468));
#74456=CARTESIAN_POINT('Ctrl Pts',(81.9810534349364,-9.54999030648095,135.215716441833));
#74457=CARTESIAN_POINT('Ctrl Pts',(81.9596541057285,-9.61786191693714,135.211847358986));
#74458=CARTESIAN_POINT('Ctrl Pts',(81.9382866604539,-9.68563240207868,135.20798404088));
#74459=CARTESIAN_POINT('Ctrl Pts',(81.9133666108288,-9.75239760413573,135.204120722774));
#74460=CARTESIAN_POINT('Ctrl Pts',(81.8850106587594,-9.81776058774157,135.200257404667));
#74461=CARTESIAN_POINT('Ctrl Pts',(81.8566879682109,-9.8830469005928,135.196398618231));
#74462=CARTESIAN_POINT('Ctrl Pts',(81.8249375731792,-9.94693381863534,135.192539831796));
#74463=CARTESIAN_POINT('Ctrl Pts',(81.7899252910331,-10.0090416319559,135.18868104536));
#74464=CARTESIAN_POINT('Ctrl Pts',(81.7549350640573,-10.0711103219083,135.184824689677));
#74465=CARTESIAN_POINT('Ctrl Pts',(81.7166872645516,-10.1314017084278,135.180968333993));
#74466=CARTESIAN_POINT('Ctrl Pts',(81.6753942808026,-10.1895594000949,135.17711197831));
#74467=CARTESIAN_POINT('Ctrl Pts',(81.6341134954144,-10.2476999113974,135.173256761833));
#74468=CARTESIAN_POINT('Ctrl Pts',(81.5897895927768,-10.3037075833172,135.169401545356));
#74469=CARTESIAN_POINT('Ctrl Pts',(81.542678085589,-10.357255276926,135.165546328878));
#74470=CARTESIAN_POINT('Ctrl Pts',(81.4955647364821,-10.4108050640894,135.161690961674));
#74471=CARTESIAN_POINT('Ctrl Pts',(81.4456638889813,-10.4618943187293,135.157835594469));
#74472=CARTESIAN_POINT('Ctrl Pts',(81.393269963358,-10.5102305690538,135.153980227265));
#74473=CARTESIAN_POINT('Ctrl Pts',(81.3408211955816,-10.5586174142517,135.150120824542));
#74474=CARTESIAN_POINT('Ctrl Pts',(81.2858744981699,-10.6042451726542,135.146261421819));
#74475=CARTESIAN_POINT('Ctrl Pts',(81.2287589638966,-10.6468603374736,135.142402019096));
#74476=CARTESIAN_POINT('Ctrl Pts',(81.1716110903591,-10.6894996313342,135.138540431149));
#74477=CARTESIAN_POINT('Ctrl Pts',(81.1122923395104,-10.7291226660256,135.134678843202));
#74478=CARTESIAN_POINT('Ctrl Pts',(81.0511602124642,-10.7655196884295,135.130817255255));
#74479=CARTESIAN_POINT('Ctrl Pts',(80.9899211325705,-10.8019803887287,135.126948911322));
#74480=CARTESIAN_POINT('Ctrl Pts',(80.9268627722774,-10.8352035817788,135.123080567389));
#74481=CARTESIAN_POINT('Ctrl Pts',(80.8623659678924,-10.8650261392058,135.119212223455));
#74482=CARTESIAN_POINT('Ctrl Pts',(80.8240696215051,-10.8827339155875,135.116915312149));
#74483=CARTESIAN_POINT('Ctrl Pts',(80.7852665078416,-10.8992436749217,135.114618400842));
#74484=CARTESIAN_POINT('Ctrl Pts',(80.7460389179157,-10.9145295754976,135.112321489536));
#74485=CARTESIAN_POINT('Ctrl Pts',(80.6799611399521,-10.9402782474436,135.108452406689));
#74486=CARTESIAN_POINT('Ctrl Pts',(80.6124193474613,-10.9626524379399,135.104583323842));
#74487=CARTESIAN_POINT('Ctrl Pts',(80.5437915874517,-10.9814863794426,135.100714240995));
#74488=CARTESIAN_POINT('Ctrl Pts',(80.4752660793819,-11.0002922593118,135.096850922889));
#74489=CARTESIAN_POINT('Ctrl Pts',(80.4056582801986,-11.0155682329928,135.092987604782));
#74490=CARTESIAN_POINT('Ctrl Pts',(80.3353649652505,-11.0271970556861,135.089124286676));
#74491=CARTESIAN_POINT('Ctrl Pts',(80.2651541043339,-11.0388122377749,135.08526550024));
#74492=CARTESIAN_POINT('Ctrl Pts',(80.1942598018297,-11.0467886877423,135.081406713804));
#74493=CARTESIAN_POINT('Ctrl Pts',(80.1230910006735,-11.0510597670602,135.077547927368));
#74494=CARTESIAN_POINT('Ctrl Pts',(80.0519670306435,-11.0553281559114,135.073691571685));
#74495=CARTESIAN_POINT('Ctrl Pts',(79.9805693887847,-11.0558957759222,135.069835216002));
#74496=CARTESIAN_POINT('Ctrl Pts',(79.9093126865443,-11.0527477618252,135.065978860319));
#74497=CARTESIAN_POINT('Ctrl Pts',(79.8380770342472,-11.049600677683,135.062123643841));
#74498=CARTESIAN_POINT('Ctrl Pts',(79.7669827239569,-11.0427401599728,135.058268427364));
#74499=CARTESIAN_POINT('Ctrl Pts',(79.6964431809677,-11.0322034396484,135.054413210887));
#74500=CARTESIAN_POINT('Ctrl Pts',(79.6259008800933,-11.0216663073698,135.050557843682));
#74501=CARTESIAN_POINT('Ctrl Pts',(79.5559138697092,-11.0074527610684,135.046702476478));
#74502=CARTESIAN_POINT('Ctrl Pts',(79.4868875528033,-10.9896515220088,135.042847109273));
#74503=CARTESIAN_POINT('Ctrl Pts',(79.4177889841661,-10.971831649906,135.03898770655));
#74504=CARTESIAN_POINT('Ctrl Pts',(79.3496535877346,-10.9504167101113,135.035128303828));
#74505=CARTESIAN_POINT('Ctrl Pts',(79.2828728363905,-10.9255456872568,135.031268901105));
#74506=CARTESIAN_POINT('Ctrl Pts',(79.2160542732604,-10.9006605822338,135.027407313158));
#74507=CARTESIAN_POINT('Ctrl Pts',(79.150592328098,-10.8723156917601,135.023545725211));
#74508=CARTESIAN_POINT('Ctrl Pts',(79.0868571230049,-10.840697598383,135.019684137264));
#74509=CARTESIAN_POINT('Ctrl Pts',(79.0230104108859,-10.8090241880183,135.015815793331));
#74510=CARTESIAN_POINT('Ctrl Pts',(78.9608968938107,-10.7740663797939,135.011947449397));
#74511=CARTESIAN_POINT('Ctrl Pts',(78.9008601794405,-10.7360556492694,135.008079105464));
#74512=CARTESIAN_POINT('Ctrl Pts',(78.8652121061538,-10.7134859713377,135.005782194157));
#74513=CARTESIAN_POINT('Ctrl Pts',(78.8302956660188,-10.6898407605847,135.003485282851));
#74514=CARTESIAN_POINT('Ctrl Pts',(78.7961772025379,-10.6651751363777,135.001188371544));
#74515=CARTESIAN_POINT('Ctrl Pts',(78.7391631807264,-10.6239573823215,134.99735009344));
#74516=CARTESIAN_POINT('Ctrl Pts',(78.6841480871177,-10.5797208791893,134.993511815336));
#74517=CARTESIAN_POINT('Ctrl Pts',(78.6314732100564,-10.5326878311342,134.989673537232));
#74518=CARTESIAN_POINT('Ctrl Pts',(78.5778665128153,-10.4848227670261,134.985767359871));
#74519=CARTESIAN_POINT('Ctrl Pts',(78.5266841028897,-10.4340614803725,134.981861182511));
#74520=CARTESIAN_POINT('Ctrl Pts',(78.4782549032979,-10.3806844038965,134.97795500515));
#74521=CARTESIAN_POINT('Ctrl Pts',(78.4307943615624,-10.3283749503611,134.974126957294));
#74522=CARTESIAN_POINT('Ctrl Pts',(78.3859782647131,-10.2735537602863,134.970298909439));
#74523=CARTESIAN_POINT('Ctrl Pts',(78.3440811368767,-10.2165238514935,134.966470861583));
#74524=CARTESIAN_POINT('Ctrl Pts',(78.3022091390412,-10.159528149381,134.9626451098));
#74525=CARTESIAN_POINT('Ctrl Pts',(78.263252930074,-10.1003267534489,134.958819358016));
#74526=CARTESIAN_POINT('Ctrl Pts',(78.2274466135477,-10.0392555290575,134.954993606233));
#74527=CARTESIAN_POINT('Ctrl Pts',(78.1916493141246,-9.97819968422998,134.951168817889));
#74528=CARTESIAN_POINT('Ctrl Pts',(78.1590005823022,-9.9152753720847,134.947344029545));
#74529=CARTESIAN_POINT('Ctrl Pts',(78.1296900536078,-9.85084561873846,134.9435192412));
#74530=CARTESIAN_POINT('Ctrl Pts',(78.0992961245193,-9.7840343587023,134.939553077815));
#74531=CARTESIAN_POINT('Ctrl Pts',(78.0724922819995,-9.71560468558299,134.93558691443));
#74532=CARTESIAN_POINT('Ctrl Pts',(78.0494357340079,-9.64598498955847,134.931620751044));
#74533=CARTESIAN_POINT('Ctrl Pts',(78.0271754962614,-9.57876976783858,134.927791568118));
#74534=CARTESIAN_POINT('Ctrl Pts',(78.0084080033322,-9.5104458945301,134.923962385192));
#74535=CARTESIAN_POINT('Ctrl Pts',(77.9932234204898,-9.441412870711,134.920133202266));
#74536=CARTESIAN_POINT('Ctrl Pts',(77.9780288922086,-9.37233463236631,134.916301511343));
#74537=CARTESIAN_POINT('Ctrl Pts',(77.9664220204801,-9.30254680699824,134.912469820419));
#74538=CARTESIAN_POINT('Ctrl Pts',(77.9584413426124,-9.23245604088901,134.908638129495));
#74539=CARTESIAN_POINT('Ctrl Pts',(77.9504482845427,-9.16225654493767,134.904800494576));
#74540=CARTESIAN_POINT('Ctrl Pts',(77.9460926623442,-9.09175366297,134.900962859657));
#74541=CARTESIAN_POINT('Ctrl Pts',(77.9453609729324,-9.02135488119547,134.897125224738));
#74542=CARTESIAN_POINT('Ctrl Pts',(77.9452847118622,-9.01401749684174,134.896725243351));
#74543=CARTESIAN_POINT('Ctrl Pts',(77.9452477713803,-9.00668123844234,134.896325261963));
#74544=CARTESIAN_POINT('Ctrl Pts',(77.9452501039006,-8.99934656332038,134.895925280576));
#74545=CARTESIAN_POINT('Ctrl Pts',(77.9452501039008,-8.99934656262625,134.895925280538));
#74546=CARTESIAN_POINT('Ctrl Pts',(77.9452615144079,-8.96346594230785,134.893968604876));
#74547=CARTESIAN_POINT('Ctrl Pts',(77.9462127014812,-8.92760146641289,134.892011929214));
#74548=CARTESIAN_POINT('Ctrl Pts',(77.948101493401,-8.89178687179018,134.890055253553));
#74549=CARTESIAN_POINT('Ctrl Pts',(77.9518363445886,-8.82096796376281,134.886186170706));
#74550=CARTESIAN_POINT('Ctrl Pts',(77.9592491642671,-8.75020393167272,134.882317087859));
#74551=CARTESIAN_POINT('Ctrl Pts',(77.9703354015928,-8.67990754386781,134.878448005012));
#74552=CARTESIAN_POINT('Ctrl Pts',(77.9814051209779,-8.6097158941748,134.874584686905));
#74553=CARTESIAN_POINT('Ctrl Pts',(77.996137318782,-8.53999098164773,134.870721368799));
#74554=CARTESIAN_POINT('Ctrl Pts',(78.0144755138151,-8.47114266833102,134.866858050692));
#74555=CARTESIAN_POINT('Ctrl Pts',(78.0327921981524,-8.4023751140594,134.862999264257));
#74556=CARTESIAN_POINT('Ctrl Pts',(78.0547063534121,-8.33448258368312,134.859140477821));
#74557=CARTESIAN_POINT('Ctrl Pts',(78.080110369965,-8.26786519616665,134.855281691385));
#74558=CARTESIAN_POINT('Ctrl Pts',(78.1054983838503,-8.20128977271945,134.851425335702));
#74559=CARTESIAN_POINT('Ctrl Pts',(78.1343717248418,-8.13598835133011,134.847568980018));
#74560=CARTESIAN_POINT('Ctrl Pts',(78.1665732666696,-8.07234490460657,134.843712624335));
#74561=CARTESIAN_POINT('Ctrl Pts',(78.1987652958395,-8.00872025879446,134.839857407858));
#74562=CARTESIAN_POINT('Ctrl Pts',(78.2342833547564,-7.94675304851614,134.836002191381));
#74563=CARTESIAN_POINT('Ctrl Pts',(78.2729233278852,-7.88680472012461,134.832146974903));
#74564=CARTESIAN_POINT('Ctrl Pts',(78.3115648117214,-7.82685404793276,134.828291607699));
#74565=CARTESIAN_POINT('Ctrl Pts',(78.3533281870658,-7.76892282145853,134.824436240494));
#74566=CARTESIAN_POINT('Ctrl Pts',(78.3979657153935,-7.71334398013873,134.82058087329));
#74567=CARTESIAN_POINT('Ctrl Pts',(78.4426499670412,-7.65770696292771,134.816721470567));
#74568=CARTESIAN_POINT('Ctrl Pts',(78.4902140724076,-7.60442762571345,134.812862067844));
#74569=CARTESIAN_POINT('Ctrl Pts',(78.5403702200733,-7.55380552205067,134.809002665121));
#74570=CARTESIAN_POINT('Ctrl Pts',(78.5905547665438,-7.50315475575514,134.805141077174));
#74571=CARTESIAN_POINT('Ctrl Pts',(78.6433339173323,-7.45516454506113,134.801279489227));
#74572=CARTESIAN_POINT('Ctrl Pts',(78.6983852719671,-7.41009539208548,134.797417901281));
#74573=CARTESIAN_POINT('Ctrl Pts',(78.7535329409201,-7.36494738901126,134.793549557347));
#74574=CARTESIAN_POINT('Ctrl Pts',(78.8109603589956,-7.3227309347253,134.789681213414));
#74575=CARTESIAN_POINT('Ctrl Pts',(78.8703151273709,-7.28366388750543,134.78581286948));
#74576=CARTESIAN_POINT('Ctrl Pts',(78.9055582807505,-7.26046699911813,134.783515958174));
#74577=CARTESIAN_POINT('Ctrl Pts',(78.9414804390346,-7.23837961974738,134.781219046867));
#74578=CARTESIAN_POINT('Ctrl Pts',(78.9780040594418,-7.2174395213675,134.778922135561));
#74579=CARTESIAN_POINT('Ctrl Pts',(79.0395270763861,-7.18216651137894,134.775053052714));
#74580=CARTESIAN_POINT('Ctrl Pts',(79.1029988479682,-7.15001324800689,134.771183969867));
#74581=CARTESIAN_POINT('Ctrl Pts',(79.1680701255574,-7.1211997853657,134.76731488702));
#74582=CARTESIAN_POINT('Ctrl Pts',(79.2330444501883,-7.09242925334685,134.763451568914));
#74583=CARTESIAN_POINT('Ctrl Pts',(79.299613109705,-7.06698883964769,134.759588250807));
#74584=CARTESIAN_POINT('Ctrl Pts',(79.3674011311609,-7.04505339365916,134.755724932701));
#74585=CARTESIAN_POINT('Ctrl Pts',(79.4351096372938,-7.02314367794034,134.751866146265));
#74586=CARTESIAN_POINT('Ctrl Pts',(79.5040342043391,-7.00473091228001,134.74800735983));
#74587=CARTESIAN_POINT('Ctrl Pts',(79.5737803137747,-6.98994170692142,134.744148573394));
#74588=CARTESIAN_POINT('Ctrl Pts',(79.6434824882756,-6.97516181767775,134.74029221771));
#74589=CARTESIAN_POINT('Ctrl Pts',(79.7140047043385,-6.96400106066667,134.736435862027));
#74590=CARTESIAN_POINT('Ctrl Pts',(79.7849391516779,-6.95653568809755,134.732579506344));
#74591=CARTESIAN_POINT('Ctrl Pts',(79.8558526442712,-6.94907252087423,134.728724289867));
#74592=CARTESIAN_POINT('Ctrl Pts',(79.9271776435276,-6.94530262167439,134.72486907339));
#74593=CARTESIAN_POINT('Ctrl Pts',(79.9984997781608,-6.94525054767389,134.721013856912));
#74594=CARTESIAN_POINT('Ctrl Pts',(80.0698247012761,-6.94519847163746,134.717158489708));
#74595=CARTESIAN_POINT('Ctrl Pts',(80.1411462737612,-6.94886450753711,134.713303122503));
#74596=CARTESIAN_POINT('Ctrl Pts',(80.2120504136819,-6.95622110184166,134.709447755299));
#74597=CARTESIAN_POINT('Ctrl Pts',(80.2830287709025,-6.96358539649439,134.705588352576));
#74598=CARTESIAN_POINT('Ctrl Pts',(80.3535883391531,-6.97464791074666,134.701728949853));
#74599=CARTESIAN_POINT('Ctrl Pts',(80.4233213503342,-6.98932931665794,134.69786954713));
#74600=CARTESIAN_POINT('Ctrl Pts',(80.493093844894,-7.00401903529657,134.694007959183));
#74601=CARTESIAN_POINT('Ctrl Pts',(80.5620383810086,-7.02233159984533,134.690146371236));
#74602=CARTESIAN_POINT('Ctrl Pts',(80.6297612385618,-7.04413744222527,134.686284783289));
#74603=CARTESIAN_POINT('Ctrl Pts',(80.6976025796817,-7.06598143470804,134.682416439356));
#74604=CARTESIAN_POINT('Ctrl Pts',(80.7642175207548,-7.09133073420804,134.678548095423));
#74605=CARTESIAN_POINT('Ctrl Pts',(80.8292318976491,-7.12000744086013,134.674679751489));
#74606=CARTESIAN_POINT('Ctrl Pts',(80.8678355636978,-7.13703484402624,134.672382840183));
#74607=CARTESIAN_POINT('Ctrl Pts',(80.9058753734192,-7.15523447752825,134.670085928876));
#74608=CARTESIAN_POINT('Ctrl Pts',(80.9432775356496,-7.17456168188603,134.66778901757));
#74609=CARTESIAN_POINT('Ctrl Pts',(81.00626540739,-7.20711005333276,134.663920857385));
#74610=CARTESIAN_POINT('Ctrl Pts',(81.0676899896171,-7.24298613757157,134.6600526972));
#74611=CARTESIAN_POINT('Ctrl Pts',(81.1271772473667,-7.28201600254284,134.656184537015));
#74612=CARTESIAN_POINT('Ctrl Pts',(81.1698375608372,-7.31000563153863,134.653410549236));
#74613=CARTESIAN_POINT('Ctrl Pts',(81.2115018543262,-7.339616143386,134.650636561456));
#74614=CARTESIAN_POINT('Ctrl Pts',(81.2520391107129,-7.37076839346111,134.647862573676));
#74615=CARTESIAN_POINT('',(77.9452502540764,-9.00102182517148,134.954074719507));
#74616=CARTESIAN_POINT('Ctrl Pts',(77.9452502540759,-9.00102182433968,134.954074719462));
#74617=CARTESIAN_POINT('Ctrl Pts',(77.9452142125462,-8.92854721091016,134.950163294815));
#74618=CARTESIAN_POINT('Ctrl Pts',(77.9490169737962,-8.8560783559993,134.946251870168));
#74619=CARTESIAN_POINT('Ctrl Pts',(77.9566303437358,-8.78404164670334,134.942340445521));
#74620=CARTESIAN_POINT('Ctrl Pts',(77.9642467236715,-8.71197645721814,134.938427474467));
#74621=CARTESIAN_POINT('Ctrl Pts',(77.9756766562268,-8.6403442159496,134.934514503412));
#74622=CARTESIAN_POINT('Ctrl Pts',(77.9908402897156,-8.56956438220089,134.930601532358));
#74623=CARTESIAN_POINT('Ctrl Pts',(78.00602657836,-8.49867880017356,134.926682715147));
#74624=CARTESIAN_POINT('Ctrl Pts',(78.0249576060862,-8.42864862450627,134.922763897937));
#74625=CARTESIAN_POINT('Ctrl Pts',(78.047502858124,-8.35988089118828,134.918845080726));
#74626=CARTESIAN_POINT('Ctrl Pts',(78.0700662114443,-8.291057945173,134.914923117149));
#74627=CARTESIAN_POINT('Ctrl Pts',(78.0962493989041,-8.22349989413301,134.911001153572));
#74628=CARTESIAN_POINT('Ctrl Pts',(78.1258736804293,-8.15759386232501,134.907079189996));
#74629=CARTESIAN_POINT('Ctrl Pts',(78.1555587274254,-8.09155264374307,134.903149181668));
#74630=CARTESIAN_POINT('Ctrl Pts',(78.1886987529193,-8.02717062698403,134.89921917334));
#74631=CARTESIAN_POINT('Ctrl Pts',(78.2250691444905,-7.9648101523583,134.895289165013));
#74632=CARTESIAN_POINT('Ctrl Pts',(78.2479358387258,-7.92560304338773,134.892818300805));
#74633=CARTESIAN_POINT('Ctrl Pts',(78.2720785667058,-7.88719445512439,134.890347436597));
#74634=CARTESIAN_POINT('Ctrl Pts',(78.2974332054889,-7.84966792936633,134.887876572388));
#74635=CARTESIAN_POINT('Ctrl Pts',(78.3371355888423,-7.79090580207634,134.884007489541));
#74636=CARTESIAN_POINT('Ctrl Pts',(78.3799614657705,-7.73408641807268,134.880138406695));
#74637=CARTESIAN_POINT('Ctrl Pts',(78.4256941852279,-7.67956114716557,134.876269323848));
#74638=CARTESIAN_POINT('Ctrl Pts',(78.4713587652141,-7.62511711619277,134.872406005741));
#74639=CARTESIAN_POINT('Ctrl Pts',(78.5199212810797,-7.57296078261917,134.868542687635));
#74640=CARTESIAN_POINT('Ctrl Pts',(78.571122078857,-7.52341425952635,134.864679369528));
#74641=CARTESIAN_POINT('Ctrl Pts',(78.6222628181182,-7.47392585448606,134.860820583093));
#74642=CARTESIAN_POINT('Ctrl Pts',(78.6760353447623,-7.42704151531016,134.856961796657));
#74643=CARTESIAN_POINT('Ctrl Pts',(78.7321412129293,-7.3830486530054,134.853103010221));
#74644=CARTESIAN_POINT('Ctrl Pts',(78.7882117385135,-7.33908350297803,134.849246654538));
#74645=CARTESIAN_POINT('Ctrl Pts',(78.8466123081177,-7.29800651519423,134.845390298854));
#74646=CARTESIAN_POINT('Ctrl Pts',(78.9070103656066,-7.26006574215906,134.841533943171));
#74647=CARTESIAN_POINT('Ctrl Pts',(78.9673905809044,-7.22213617720819,134.837678726694));
#74648=CARTESIAN_POINT('Ctrl Pts',(79.0297667014881,-7.18734124597068,134.833823510217));
#74649=CARTESIAN_POINT('Ctrl Pts',(79.0937775151035,-7.15588547796834,134.82996829374));
#74650=CARTESIAN_POINT('Ctrl Pts',(79.1577908313503,-7.12442848013955,134.826112926535));
#74651=CARTESIAN_POINT('Ctrl Pts',(79.2234385305605,-7.09631111701001,134.82225755933));
#74652=CARTESIAN_POINT('Ctrl Pts',(79.2903367116233,-7.07169100514715,134.818402192126));
#74653=CARTESIAN_POINT('Ctrl Pts',(79.3573049168394,-7.04704512274075,134.814542789403));
#74654=CARTESIAN_POINT('Ctrl Pts',(79.4255257599688,-7.02590396723754,134.81068338668));
#74655=CARTESIAN_POINT('Ctrl Pts',(79.4945982079856,-7.0083758911058,134.806823983957));
#74656=CARTESIAN_POINT('Ctrl Pts',(79.563709765365,-6.99083789043967,134.80296239601));
#74657=CARTESIAN_POINT('Ctrl Pts',(79.6336734108451,-6.97691713645357,134.799100808063));
#74658=CARTESIAN_POINT('Ctrl Pts',(79.7040785989494,-6.96667068901757,134.795239220117));
#74659=CARTESIAN_POINT('Ctrl Pts',(79.774606963454,-6.95640631505451,134.791370876183));
#74660=CARTESIAN_POINT('Ctrl Pts',(79.8455779290268,-6.94982912682779,134.78750253225));
#74661=CARTESIAN_POINT('Ctrl Pts',(79.9165772232856,-6.94694417932068,134.783634188316));
#74662=CARTESIAN_POINT('Ctrl Pts',(79.9587345610346,-6.94523118051251,134.78133727701));
#74663=CARTESIAN_POINT('Ctrl Pts',(80.0009018924247,-6.94481893458073,134.779040365703));
#74664=CARTESIAN_POINT('Ctrl Pts',(80.0429932997395,-6.94569984211715,134.776743454397));
#74665=CARTESIAN_POINT('Ctrl Pts',(80.1138837197782,-6.94718346809346,134.772874992454));
#74666=CARTESIAN_POINT('Ctrl Pts',(80.1848360783876,-6.95234376833629,134.769006530512));
#74667=CARTESIAN_POINT('Ctrl Pts',(80.2554378698441,-6.96118930325802,134.765138068569));
#74668=CARTESIAN_POINT('Ctrl Pts',(80.325940790493,-6.97002245088528,134.761275024024));
#74669=CARTESIAN_POINT('Ctrl Pts',(80.3960936402553,-6.98253053403551,134.757411979479));
#74670=CARTESIAN_POINT('Ctrl Pts',(80.4654850568473,-6.99867013604657,134.753548934934));
#74671=CARTESIAN_POINT('Ctrl Pts',(80.536481586217,-7.01518306782501,134.749596533196));
#74672=CARTESIAN_POINT('Ctrl Pts',(80.6066804960061,-7.03549762531567,134.745644131458));
#74673=CARTESIAN_POINT('Ctrl Pts',(80.675648520014,-7.05951123685221,134.741691729721));
#74674=CARTESIAN_POINT('Ctrl Pts',(80.7429382618448,-7.08294049619321,134.737835506546));
#74675=CARTESIAN_POINT('Ctrl Pts',(80.8090558650348,-7.10989063762988,134.73397928337));
#74676=CARTESIAN_POINT('Ctrl Pts',(80.8736130183895,-7.14021564244656,134.730123060195));
#74677=CARTESIAN_POINT('Ctrl Pts',(80.9405853642445,-7.17167515707978,134.726122569176));
#74678=CARTESIAN_POINT('Ctrl Pts',(81.0058776664664,-7.20676688624266,134.722122078158));
#74679=CARTESIAN_POINT('Ctrl Pts',(81.0690801890059,-7.24527349368194,134.718121587139));
#74680=CARTESIAN_POINT('Ctrl Pts',(81.1322827115453,-7.28378010112123,134.71412109612));
#74681=CARTESIAN_POINT('Ctrl Pts',(81.1933949592345,-7.32570127656327,134.710120605101));
#74682=CARTESIAN_POINT('Ctrl Pts',(81.2520391107129,-7.37076839346111,134.706120114083));
#74683=CARTESIAN_POINT('Ctrl Pts',(81.2520391107129,-7.37076839346111,135.406026966566));
#74684=CARTESIAN_POINT('Ctrl Pts',(81.3085478694585,-7.41419449430732,135.402170997473));
#74685=CARTESIAN_POINT('Ctrl Pts',(81.3628300813749,-7.46059120030964,135.39831502838));
#74686=CARTESIAN_POINT('Ctrl Pts',(81.4145642490411,-7.50969615586794,135.394459059287));
#74687=CARTESIAN_POINT('Ctrl Pts',(81.4662872342288,-7.55879049725901,135.390603923672));
#74688=CARTESIAN_POINT('Ctrl Pts',(81.515462916766,-7.61059159127112,135.386748788057));
#74689=CARTESIAN_POINT('Ctrl Pts',(81.56180511097,-7.66479875754703,135.382893652442));
#74690=CARTESIAN_POINT('Ctrl Pts',(81.6081527898687,-7.71901233935326,135.379038060564));
#74691=CARTESIAN_POINT('Ctrl Pts',(81.6516660009943,-7.77563218785869,135.375182468686));
#74692=CARTESIAN_POINT('Ctrl Pts',(81.6920985972817,-7.83432427340303,135.371326876807));
#74693=CARTESIAN_POINT('Ctrl Pts',(81.7325754841388,-7.89308065127935,135.367467061447));
#74694=CARTESIAN_POINT('Ctrl Pts',(81.7699647470556,-7.95391339462022,135.363607246086));
#74695=CARTESIAN_POINT('Ctrl Pts',(81.8040639134633,-8.016459986254,135.359747430725));
#74696=CARTESIAN_POINT('Ctrl Pts',(81.8381848105413,-8.07904643749463,135.355885155587));
#74697=CARTESIAN_POINT('Ctrl Pts',(81.8690112291951,-8.14334847244807,135.352022880448));
#74698=CARTESIAN_POINT('Ctrl Pts',(81.8963881558205,-8.20898196925509,135.34816060531));
#74699=CARTESIAN_POINT('Ctrl Pts',(81.9238110295093,-8.27472561964063,135.344291848063));
#74700=CARTESIAN_POINT('Ctrl Pts',(81.9477726968834,-8.34180473375835,135.340423090816));
#74701=CARTESIAN_POINT('Ctrl Pts',(81.9681677230269,-8.4098192001299,135.336554333569));
#74702=CARTESIAN_POINT('Ctrl Pts',(81.9754519986149,-8.43411120708983,135.335172570498));
#74703=CARTESIAN_POINT('Ctrl Pts',(81.9822817781762,-8.45852243441226,135.333790807426));
#74704=CARTESIAN_POINT('Ctrl Pts',(81.9886538483545,-8.48303439773548,135.332409044355));
#74705=CARTESIAN_POINT('Ctrl Pts',(82.0064963192771,-8.55167048939985,135.328539961508));
#74706=CARTESIAN_POINT('Ctrl Pts',(82.0208162221759,-8.6213658157439,135.324670878661));
#74707=CARTESIAN_POINT('Ctrl Pts',(82.031493149485,-8.69172553447344,135.320801795814));
#74708=CARTESIAN_POINT('Ctrl Pts',(82.0421541687048,-8.76198042073116,135.316938477708));
#74709=CARTESIAN_POINT('Ctrl Pts',(82.0491829141827,-8.83289725805528,135.313075159601));
#74710=CARTESIAN_POINT('Ctrl Pts',(82.0525093587264,-8.90406828032084,135.309211841495));
#74711=CARTESIAN_POINT('Ctrl Pts',(82.0558319013519,-8.97515581900462,135.305353055059));
#74712=CARTESIAN_POINT('Ctrl Pts',(82.0554607467397,-9.04649646748708,135.301494268623));
#74713=CARTESIAN_POINT('Ctrl Pts',(82.0513775498521,-9.11767629524553,135.297635482187));
#74714=CARTESIAN_POINT('Ctrl Pts',(82.0472969250792,-9.18881128493185,135.293779126504));
#74715=CARTESIAN_POINT('Ctrl Pts',(82.0395089249653,-9.25978517104288,135.289922770821));
#74716=CARTESIAN_POINT('Ctrl Pts',(82.0280472853772,-9.33018444962502,135.286066415137));
#74717=CARTESIAN_POINT('Ctrl Pts',(82.0165890316722,-9.40056293155539,135.28221119866));
#74718=CARTESIAN_POINT('Ctrl Pts',(82.001459370995,-9.47036666373856,135.278355982183));
#74719=CARTESIAN_POINT('Ctrl Pts',(81.982743639037,-9.53918941417479,135.274500765706));
#74720=CARTESIAN_POINT('Ctrl Pts',(81.9640271753499,-9.60801485537473,135.270645398501));
#74721=CARTESIAN_POINT('Ctrl Pts',(81.9417244916246,-9.6758587705007,135.266790031297));
#74722=CARTESIAN_POINT('Ctrl Pts',(81.915971121969,-9.74232891785301,135.262934664092));
#74723=CARTESIAN_POINT('Ctrl Pts',(81.890190795558,-9.80886864132405,135.259075261369));
#74724=CARTESIAN_POINT('Ctrl Pts',(81.8609527488611,-9.87403127262947,135.255215858646));
#74725=CARTESIAN_POINT('Ctrl Pts',(81.8284408048189,-9.93744428409014,135.251356455924));
#74726=CARTESIAN_POINT('Ctrl Pts',(81.7959104522586,-10.000893200496,135.247494867977));
#74727=CARTESIAN_POINT('Ctrl Pts',(81.7601027561565,-10.0625901046345,135.24363328003));
#74728=CARTESIAN_POINT('Ctrl Pts',(81.7212463131005,-10.1221892407869,135.239771692083));
#74729=CARTESIAN_POINT('Ctrl Pts',(81.6823218893047,-10.1818926477641,135.235903348149));
#74730=CARTESIAN_POINT('Ctrl Pts',(81.6403383555224,-10.2394905665673,135.232035004216));
#74731=CARTESIAN_POINT('Ctrl Pts',(81.5955657916373,-10.2946688252433,135.228166660282));
#74732=CARTESIAN_POINT('Ctrl Pts',(81.5689811316447,-10.3274320873529,135.225869748976));
#74733=CARTESIAN_POINT('Ctrl Pts',(81.5414139051124,-10.3593429288424,135.223572837669));
#74734=CARTESIAN_POINT('Ctrl Pts',(81.5129266135238,-10.3903419092409,135.221275926363));
#74735=CARTESIAN_POINT('Ctrl Pts',(81.4649405676835,-10.4425588246247,135.217406843516));
#74736=CARTESIAN_POINT('Ctrl Pts',(81.4141540521792,-10.4923908221379,135.213537760669));
#74737=CARTESIAN_POINT('Ctrl Pts',(81.3608334803885,-10.5395225887118,135.209668677822));
#74738=CARTESIAN_POINT('Ctrl Pts',(81.3075923535905,-10.5865841313039,135.205805359716));
#74739=CARTESIAN_POINT('Ctrl Pts',(81.2518250260106,-10.6309531098095,135.201942041609));
#74740=CARTESIAN_POINT('Ctrl Pts',(81.1938360940875,-10.6723495277465,135.198078723503));
#74741=CARTESIAN_POINT('Ctrl Pts',(81.1359151831591,-10.7136973877013,135.194219937067));
#74742=CARTESIAN_POINT('Ctrl Pts',(81.075778237626,-10.7520793322013,135.190361150631));
#74743=CARTESIAN_POINT('Ctrl Pts',(81.0137630642248,-10.7872554412041,135.186502364195));
#74744=CARTESIAN_POINT('Ctrl Pts',(80.9517869558356,-10.8224093918375,135.182646008512));
#74745=CARTESIAN_POINT('Ctrl Pts',(80.8879353884644,-10.8543612744068,135.178789652829));
#74746=CARTESIAN_POINT('Ctrl Pts',(80.8225740581306,-10.8829151551227,135.174933297146));
#74747=CARTESIAN_POINT('Ctrl Pts',(80.7572320361883,-10.9114606007363,135.171078080668));
#74748=CARTESIAN_POINT('Ctrl Pts',(80.6903815816309,-10.9366098429589,135.167222864191));
#74749=CARTESIAN_POINT('Ctrl Pts',(80.6224102677982,-10.9582142428854,135.163367647714));
#74750=CARTESIAN_POINT('Ctrl Pts',(80.5544362964903,-10.9798194874795,135.159512280509));
#74751=CARTESIAN_POINT('Ctrl Pts',(80.4853418425312,-10.9978794695692,135.155656913305));
#74752=CARTESIAN_POINT('Ctrl Pts',(80.4155299521801,-11.0122953116631,135.1518015461));
#74753=CARTESIAN_POINT('Ctrl Pts',(80.3456449878167,-11.0267262432126,135.147942143377));
#74754=CARTESIAN_POINT('Ctrl Pts',(80.2750415646969,-11.0375053218868,135.144082740654));
#74755=CARTESIAN_POINT('Ctrl Pts',(80.2041323575917,-11.0445849317365,135.140223337932));
#74756=CARTESIAN_POINT('Ctrl Pts',(80.1331830011365,-11.051668550117,135.136361749985));
#74757=CARTESIAN_POINT('Ctrl Pts',(80.0619280015,-11.0550485068064,135.132500162038));
#74758=CARTESIAN_POINT('Ctrl Pts',(79.990781825789,-11.0547293222622,135.128638574091));
#74759=CARTESIAN_POINT('Ctrl Pts',(79.9195111772936,-11.0544095792932,135.124770230157));
#74760=CARTESIAN_POINT('Ctrl Pts',(79.848350218004,-11.0503778014863,135.120901886224));
#74761=CARTESIAN_POINT('Ctrl Pts',(79.7777093801838,-11.0426904912007,135.11703354229));
#74762=CARTESIAN_POINT('Ctrl Pts',(79.7357648835527,-11.0381259875746,135.114736630984));
#74763=CARTESIAN_POINT('Ctrl Pts',(79.6940036089263,-11.0322736611288,135.112439719677));
#74764=CARTESIAN_POINT('Ctrl Pts',(79.6525093937848,-11.0251537820848,135.110142808371));
#74765=CARTESIAN_POINT('Ctrl Pts',(79.5826135490471,-11.013160544991,135.106273725524));
#74766=CARTESIAN_POINT('Ctrl Pts',(79.513202433067,-10.997521008181,135.102404642677));
#74767=CARTESIAN_POINT('Ctrl Pts',(79.4446854481566,-10.9782879747425,135.09853555983));
#74768=CARTESIAN_POINT('Ctrl Pts',(79.3762705501363,-10.9590835975646,135.094672241724));
#74769=CARTESIAN_POINT('Ctrl Pts',(79.3087476026802,-10.9362964817773,135.090808923617));
#74770=CARTESIAN_POINT('Ctrl Pts',(79.2425170472081,-10.9100306643428,135.086945605511));
#74771=CARTESIAN_POINT('Ctrl Pts',(79.1763641801522,-10.883795656702,135.083086819075));
#74772=CARTESIAN_POINT('Ctrl Pts',(79.1115011432172,-10.8540902309144,135.079228032639));
#74773=CARTESIAN_POINT('Ctrl Pts',(79.0483127208927,-10.8210680616839,135.075369246204));
#74774=CARTESIAN_POINT('Ctrl Pts',(78.9851641026408,-10.7880666939987,135.07151289052));
#74775=CARTESIAN_POINT('Ctrl Pts',(78.9236884356437,-10.7517529524849,135.067656534837));
#74776=CARTESIAN_POINT('Ctrl Pts',(78.8642486766826,-10.7123277998335,135.063800179154));
#74777=CARTESIAN_POINT('Ctrl Pts',(78.8048264768216,-10.6729142937671,135.059944962676));
#74778=CARTESIAN_POINT('Ctrl Pts',(78.7474393956033,-10.6303914696825,135.056089746199));
#74779=CARTESIAN_POINT('Ctrl Pts',(78.6924225216405,-10.5850043219458,135.052234529722));
#74780=CARTESIAN_POINT('Ctrl Pts',(78.6374034966826,-10.5396153997074,135.048379162517));
#74781=CARTESIAN_POINT('Ctrl Pts',(78.5847552362845,-10.4913622423186,135.044523795313));
#74782=CARTESIAN_POINT('Ctrl Pts',(78.5347794150567,-10.4405298330678,135.040668428108));
#74783=CARTESIAN_POINT('Ctrl Pts',(78.4847512827717,-10.3896442161458,135.036809025385));
#74784=CARTESIAN_POINT('Ctrl Pts',(78.4374015149919,-10.3361743051257,135.032949622663));
#74785=CARTESIAN_POINT('Ctrl Pts',(78.3929939421255,-10.2804409757793,135.02909021994));
#74786=CARTESIAN_POINT('Ctrl Pts',(78.3485612253426,-10.224676089784,135.025228631993));
#74787=CARTESIAN_POINT('Ctrl Pts',(78.3070743024084,-10.1666456296284,135.021367044046));
#74788=CARTESIAN_POINT('Ctrl Pts',(78.2687541743393,-10.1067002546455,135.017505456099));
#74789=CARTESIAN_POINT('Ctrl Pts',(78.2303670038326,-10.0466500030804,135.013637112166));
#74790=CARTESIAN_POINT('Ctrl Pts',(78.1951579298455,-9.98467857040146,135.009768768232));
#74791=CARTESIAN_POINT('Ctrl Pts',(78.1633020932596,-9.92116142009714,135.005900424299));
#74792=CARTESIAN_POINT('Ctrl Pts',(78.1443870142261,-9.88344676411107,135.003603512992));
#74793=CARTESIAN_POINT('Ctrl Pts',(78.1266532537514,-9.8451875492383,135.001306601686));
#74794=CARTESIAN_POINT('Ctrl Pts',(78.110129253951,-9.80646520428854,134.999009690379));
#74795=CARTESIAN_POINT('Ctrl Pts',(78.0793053040283,-9.73423235291849,134.994725020811));
#74796=CARTESIAN_POINT('Ctrl Pts',(78.052590491782,-9.66014619425519,134.990440351243));
#74797=CARTESIAN_POINT('Ctrl Pts',(78.0301869119698,-9.58466568286928,134.986155681675));
#74798=CARTESIAN_POINT('Ctrl Pts',(78.0078542859392,-9.50942422380289,134.98188458197));
#74799=CARTESIAN_POINT('Ctrl Pts',(77.9898057879736,-9.43279749448197,134.977613482265));
#74800=CARTESIAN_POINT('Ctrl Pts',(77.9761951891263,-9.3552627900365,134.97334238256));
#74801=CARTESIAN_POINT('Ctrl Pts',(77.9626561574425,-9.27813577807579,134.969093741125));
#74802=CARTESIAN_POINT('Ctrl Pts',(77.953508604126,-9.20011059760666,134.964845099689));
#74803=CARTESIAN_POINT('Ctrl Pts',(77.9488557708441,-9.12167544411387,134.960596458253));
#74804=CARTESIAN_POINT('Ctrl Pts',(77.9464750440831,-9.08154233432821,134.958422545337));
#74805=CARTESIAN_POINT('Ctrl Pts',(77.9452702854505,-9.04130216095229,134.956248632422));
#74806=CARTESIAN_POINT('Ctrl Pts',(77.9452502540763,-9.00102182517148,134.954074719507));
#74807=CARTESIAN_POINT('Origin',(80.,-9.,141.545925280538));
#74808=CARTESIAN_POINT('',(81.2520391107129,-7.37076839346112,136.106053391332));
#74809=CARTESIAN_POINT('',(81.2520391107129,-7.37076839346112,136.047954616434));
#74810=CARTESIAN_POINT('',(81.2520391107129,-7.37076839346111,141.545925280538));
#74811=CARTESIAN_POINT('',(77.9452505223076,-8.99853493254343,135.595925280489));
#74812=CARTESIAN_POINT('Ctrl Pts',(81.2520391107129,-7.37076839346111,136.047954616434));
#74813=CARTESIAN_POINT('Ctrl Pts',(81.3089518218122,-7.41450492539866,136.044073934521));
#74814=CARTESIAN_POINT('Ctrl Pts',(81.3635519299052,-7.46121314581298,136.040193252607));
#74815=CARTESIAN_POINT('Ctrl Pts',(81.4155258488792,-7.51060947577379,136.036312570693));
#74816=CARTESIAN_POINT('Ctrl Pts',(81.4672299062672,-7.55974932763548,136.03245203825));
#74817=CARTESIAN_POINT('Ctrl Pts',(81.516334682387,-7.61154904832071,136.028591505807));
#74818=CARTESIAN_POINT('Ctrl Pts',(81.5625698796666,-7.66569383810955,136.024730973364));
#74819=CARTESIAN_POINT('Ctrl Pts',(81.6091670534803,-7.72026252883326,136.020840216715));
#74820=CARTESIAN_POINT('Ctrl Pts',(81.6528492126412,-7.77721277184851,136.016949460066));
#74821=CARTESIAN_POINT('Ctrl Pts',(81.6933836048278,-7.83619179870548,136.013058703416));
#74822=CARTESIAN_POINT('Ctrl Pts',(81.7339179970144,-7.89517082556246,136.009167946767));
#74823=CARTESIAN_POINT('Ctrl Pts',(81.7713044167982,-7.95617817802814,136.005277190118));
#74824=CARTESIAN_POINT('Ctrl Pts',(81.8053578201977,-8.01883706574744,136.001386433468));
#74825=CARTESIAN_POINT('Ctrl Pts',(81.8392215261155,-8.08114690661623,135.997517350621));
#74826=CARTESIAN_POINT('Ctrl Pts',(81.8699219428301,-8.14533399680408,135.993648267774));
#74827=CARTESIAN_POINT('Ctrl Pts',(81.897247021578,-8.21104417004908,135.989779184927));
#74828=CARTESIAN_POINT('Ctrl Pts',(81.9245313873213,-8.27665643841313,135.985915866821));
#74829=CARTESIAN_POINT('Ctrl Pts',(81.9484502126878,-8.34378684040901,135.982052548715));
#74830=CARTESIAN_POINT('Ctrl Pts',(81.9688372273746,-8.41205652091058,135.978189230608));
#74831=CARTESIAN_POINT('Ctrl Pts',(81.989200328101,-8.48024612110317,135.974330444172));
#74832=CARTESIAN_POINT('Ctrl Pts',(82.0060397088494,-8.54957188209905,135.970471657737));
#74833=CARTESIAN_POINT('Ctrl Pts',(82.0192377707971,-8.61963650610701,135.966612871301));
#74834=CARTESIAN_POINT('Ctrl Pts',(82.0324275189334,-8.6896569945394,135.962756515618));
#74835=CARTESIAN_POINT('Ctrl Pts',(82.0419804093478,-8.76041494632014,135.958900159934));
#74836=CARTESIAN_POINT('Ctrl Pts',(82.0478294907081,-8.83150092140787,135.955043804251));
#74837=CARTESIAN_POINT('Ctrl Pts',(82.0536768441911,-8.90256589698681,135.951188587774));
#74838=CARTESIAN_POINT('Ctrl Pts',(82.0558225209815,-8.97395821961339,135.947333371297));
#74839=CARTESIAN_POINT('Ctrl Pts',(82.0542514007093,-9.0452630664432,135.943478154819));
#74840=CARTESIAN_POINT('Ctrl Pts',(82.052680219011,-9.11657070107929,135.939622787615));
#74841=CARTESIAN_POINT('Ctrl Pts',(82.0473919646485,-9.18779036751191,135.93576742041));
#74842=CARTESIAN_POINT('Ctrl Pts',(82.0384236078768,-9.25850871813237,135.931912053206));
#74843=CARTESIAN_POINT('Ctrl Pts',(82.0294458636811,-9.32930109158191,135.928052650483));
#74844=CARTESIAN_POINT('Ctrl Pts',(82.0167803887356,-9.39959061880823,135.92419324776));
#74845=CARTESIAN_POINT('Ctrl Pts',(82.0005157706015,-9.46897144270698,135.920333845037));
#74846=CARTESIAN_POINT('Ctrl Pts',(81.9842419433129,-9.53839155057324,135.91647225709));
#74847=CARTESIAN_POINT('Ctrl Pts',(81.964365051502,-9.60690146410664,135.912610669143));
#74848=CARTESIAN_POINT('Ctrl Pts',(81.9410235901457,-9.67411051393499,135.908749081196));
#74849=CARTESIAN_POINT('Ctrl Pts',(81.9176412920663,-9.74143714840501,135.904880737263));
#74850=CARTESIAN_POINT('Ctrl Pts',(81.8907825058248,-9.80745792514187,135.90101239333));
#74851=CARTESIAN_POINT('Ctrl Pts',(81.8606336006024,-9.87180282564891,135.897144049396));
#74852=CARTESIAN_POINT('Ctrl Pts',(81.8427320482915,-9.91000897588458,135.89484713809));
#74853=CARTESIAN_POINT('Ctrl Pts',(81.8236714017529,-9.94762473769756,135.892550226783));
#74854=CARTESIAN_POINT('Ctrl Pts',(81.8034979882718,-9.98457735541688,135.890253315477));
#74855=CARTESIAN_POINT('Ctrl Pts',(81.7695164375494,-10.0468230063339,135.88638423263));
#74856=CARTESIAN_POINT('Ctrl Pts',(81.7322420417681,-10.1074292564437,135.882515149783));
#74857=CARTESIAN_POINT('Ctrl Pts',(81.6918573366432,-10.1660258637554,135.878646066936));
#74858=CARTESIAN_POINT('Ctrl Pts',(81.6515328027148,-10.2245351650446,135.87478274883));
#74859=CARTESIAN_POINT('Ctrl Pts',(81.6081074316388,-10.2810403703443,135.870919430723));
#74860=CARTESIAN_POINT('Ctrl Pts',(81.561809330398,-10.3351963069084,135.867056112617));
#74861=CARTESIAN_POINT('Ctrl Pts',(81.5155655368123,-10.3892887185796,135.863197326181));
#74862=CARTESIAN_POINT('Ctrl Pts',(81.4664560205841,-10.441036967801,135.859338539745));
#74863=CARTESIAN_POINT('Ctrl Pts',(81.4147507814426,-10.4901267694084,135.855479753309));
#74864=CARTESIAN_POINT('Ctrl Pts',(81.3630781128103,-10.5391856480405,135.851623397626));
#74865=CARTESIAN_POINT('Ctrl Pts',(81.3088133167697,-10.5855890678083,135.847767041943));
#74866=CARTESIAN_POINT('Ctrl Pts',(81.2522640643579,-10.6290587084626,135.84391068626));
#74867=CARTESIAN_POINT('Ctrl Pts',(81.1957315171616,-10.6725155077497,135.840055469782));
#74868=CARTESIAN_POINT('Ctrl Pts',(81.1369162382928,-10.7130399526008,135.836200253305));
#74869=CARTESIAN_POINT('Ctrl Pts',(81.0761585331535,-10.7503943481459,135.832345036828));
#74870=CARTESIAN_POINT('Ctrl Pts',(81.0153984525695,-10.7877502041362,135.828489669623));
#74871=CARTESIAN_POINT('Ctrl Pts',(80.9526962099212,-10.8219355122066,135.824634302419));
#74872=CARTESIAN_POINT('Ctrl Pts',(80.888419124146,-10.852757140683,135.820778935214));
#74873=CARTESIAN_POINT('Ctrl Pts',(80.8240747577897,-10.8836110309996,135.816919532491));
#74874=CARTESIAN_POINT('Ctrl Pts',(80.7581526965937,-10.911094002836,135.813060129768));
#74875=CARTESIAN_POINT('Ctrl Pts',(80.691041962686,-10.9350603526265,135.809200727045));
#74876=CARTESIAN_POINT('Ctrl Pts',(80.6238932301537,-10.9590402723526,135.805339139099));
#74877=CARTESIAN_POINT('Ctrl Pts',(80.5555549506982,-10.9794994668986,135.801477551152));
#74878=CARTESIAN_POINT('Ctrl Pts',(80.4864304555317,-10.9963423990967,135.797615963205));
#74879=CARTESIAN_POINT('Ctrl Pts',(80.4171850245831,-11.0132147986085,135.793747619271));
#74880=CARTESIAN_POINT('Ctrl Pts',(80.3471511091485,-11.0264582138856,135.789879275338));
#74881=CARTESIAN_POINT('Ctrl Pts',(80.2767406569824,-11.0360285290911,135.786010931404));
#74882=CARTESIAN_POINT('Ctrl Pts',(80.234932956723,-11.0417111068504,135.783714020098));
#74883=CARTESIAN_POINT('Ctrl Pts',(80.1929925914078,-11.0460996761472,135.781417108791));
#74884=CARTESIAN_POINT('Ctrl Pts',(80.1510058124904,-11.0491936968218,135.779120197485));
#74885=CARTESIAN_POINT('Ctrl Pts',(80.0802802578498,-11.0544054881029,135.775251114638));
#74886=CARTESIAN_POINT('Ctrl Pts',(80.0091460436975,-11.0559616725954,135.771382031791));
#74887=CARTESIAN_POINT('Ctrl Pts',(79.9380132263567,-11.0538147926221,135.767512948944));
#74888=CARTESIAN_POINT('Ctrl Pts',(79.8669863933663,-11.0516711113929,135.763649630838));
#74889=CARTESIAN_POINT('Ctrl Pts',(79.7959614346627,-11.0458353320829,135.759786312731));
#74890=CARTESIAN_POINT('Ctrl Pts',(79.7253520620256,-11.0363118800092,135.755922994625));
#74891=CARTESIAN_POINT('Ctrl Pts',(79.6548255141554,-11.026799598941,135.752064208189));
#74892=CARTESIAN_POINT('Ctrl Pts',(79.5847140631344,-11.0136083019093,135.748205421753));
#74893=CARTESIAN_POINT('Ctrl Pts',(79.5154281928644,-10.9967943625294,135.744346635318));
#74894=CARTESIAN_POINT('Ctrl Pts',(79.4461859676121,-10.9799910146984,135.740490279634));
#74895=CARTESIAN_POINT('Ctrl Pts',(79.3777687622945,-10.959569666261,135.736633923951));
#74896=CARTESIAN_POINT('Ctrl Pts',(79.3105772776748,-10.9356378464066,135.732777568268));
#74897=CARTESIAN_POINT('Ctrl Pts',(79.2434056420925,-10.9117130962514,135.72892235179));
#74898=CARTESIAN_POINT('Ctrl Pts',(79.177459465732,-10.8842800963727,135.725067135313));
#74899=CARTESIAN_POINT('Ctrl Pts',(79.113123018869,-10.8534958275756,135.721211918836));
#74900=CARTESIAN_POINT('Ctrl Pts',(79.0487840566434,-10.8227103552056,135.717356551631));
#74901=CARTESIAN_POINT('Ctrl Pts',(78.9860553861175,-10.7885735654471,135.713501184427));
#74902=CARTESIAN_POINT('Ctrl Pts',(78.9252984901619,-10.7512893042704,135.709645817222));
#74903=CARTESIAN_POINT('Ctrl Pts',(78.864477998304,-10.7139660166391,135.705786414499));
#74904=CARTESIAN_POINT('Ctrl Pts',(78.8056338159311,-10.6734889355417,135.701927011777));
#74905=CARTESIAN_POINT('Ctrl Pts',(78.7490993513748,-10.6301058645895,135.698067609054));
#74906=CARTESIAN_POINT('Ctrl Pts',(78.6925328765606,-10.5866982298017,135.694206021107));
#74907=CARTESIAN_POINT('Ctrl Pts',(78.6382790925866,-10.5403816452458,135.69034443316));
#74908=CARTESIAN_POINT('Ctrl Pts',(78.5866370222996,-10.4914431453347,135.686482845213));
#74909=CARTESIAN_POINT('Ctrl Pts',(78.5349046023597,-10.4424190257639,135.68261450128));
#74910=CARTESIAN_POINT('Ctrl Pts',(78.4857933536458,-10.390764184664,135.678746157346));
#74911=CARTESIAN_POINT('Ctrl Pts',(78.4395637716867,-10.336800785408,135.674877813413));
#74912=CARTESIAN_POINT('Ctrl Pts',(78.412113976291,-10.3047588718613,135.672580902106));
#74913=CARTESIAN_POINT('Ctrl Pts',(78.3856793652921,-10.2719036572887,135.6702839908));
#74914=CARTESIAN_POINT('Ctrl Pts',(78.360307173587,-10.2383073114174,135.667987079493));
#74915=CARTESIAN_POINT('Ctrl Pts',(78.3174433117301,-10.1815495371952,135.664106670182));
#74916=CARTESIAN_POINT('Ctrl Pts',(78.2774445565979,-10.1224505980396,135.660226260871));
#74917=CARTESIAN_POINT('Ctrl Pts',(78.2405752223932,-10.0613303041199,135.65634585156));
#74918=CARTESIAN_POINT('Ctrl Pts',(78.2037608188311,-10.0003010717042,135.652471223568));
#74919=CARTESIAN_POINT('Ctrl Pts',(78.1700668305629,-9.93725686913624,135.648596595576));
#74920=CARTESIAN_POINT('Ctrl Pts',(78.1397161676285,-9.87254892442625,135.644721967583));
#74921=CARTESIAN_POINT('Ctrl Pts',(78.1078633935518,-9.8046384623624,135.640655576996));
#74922=CARTESIAN_POINT('Ctrl Pts',(78.0796937990201,-9.7348957272421,135.636589186409));
#74923=CARTESIAN_POINT('Ctrl Pts',(78.0554121444881,-9.66375871722748,135.632522795822));
#74924=CARTESIAN_POINT('Ctrl Pts',(78.0323224526799,-9.59611375361004,135.62865602038));
#74925=CARTESIAN_POINT('Ctrl Pts',(78.0127481522004,-9.52720869452225,135.624789244939));
#74926=CARTESIAN_POINT('Ctrl Pts',(77.9968162204212,-9.45744104290337,135.620922469497));
#74927=CARTESIAN_POINT('Ctrl Pts',(77.9808915414106,-9.38770515194222,135.617057454346));
#74928=CARTESIAN_POINT('Ctrl Pts',(77.968606042256,-9.31710791801235,135.613192439195));
#74929=CARTESIAN_POINT('Ctrl Pts',(77.9600362376923,-9.2460597711358,135.609327424043));
#74930=CARTESIAN_POINT('Ctrl Pts',(77.9514663540314,-9.17501096850289,135.605462373219));
#74931=CARTESIAN_POINT('Ctrl Pts',(77.946612293274,-9.10351172242717,135.601597322395));
#74932=CARTESIAN_POINT('Ctrl Pts',(77.945498864882,-9.03197887269597,135.59773227157));
#74933=CARTESIAN_POINT('Ctrl Pts',(77.9453253479641,-9.02083117815062,135.597129941226));
#74934=CARTESIAN_POINT('Ctrl Pts',(77.9452425738058,-9.00968267177878,135.596527610882));
#74935=CARTESIAN_POINT('Ctrl Pts',(77.9452505223069,-8.99853493345712,135.595925280538));
#74936=CARTESIAN_POINT('Ctrl Pts',(77.9452505223076,-8.99853493254344,135.595925280489));
#74937=CARTESIAN_POINT('Ctrl Pts',(77.9453088390013,-8.91674607330211,135.591506096049));
#74938=CARTESIAN_POINT('Ctrl Pts',(77.9502545524831,-8.83515245773087,135.587086911609));
#74939=CARTESIAN_POINT('Ctrl Pts',(77.9599940449637,-8.75429028119236,135.582667727169));
#74940=CARTESIAN_POINT('Ctrl Pts',(77.9698223745246,-8.67269053442832,135.57820823391));
#74941=CARTESIAN_POINT('Ctrl Pts',(77.9845322237854,-8.59183581843483,135.573748740651));
#74942=CARTESIAN_POINT('Ctrl Pts',(78.0039776882017,-8.51225775936117,135.569289247392));
#74943=CARTESIAN_POINT('Ctrl Pts',(78.0220522312958,-8.43829001926129,135.565144152095));
#74944=CARTESIAN_POINT('Ctrl Pts',(78.0442176079845,-8.36542517061296,135.560999056799));
#74945=CARTESIAN_POINT('Ctrl Pts',(78.0703199470975,-8.29407333530297,135.556853961502));
#74946=CARTESIAN_POINT('Ctrl Pts',(78.0946841909334,-8.22747265610305,135.552984878655));
#74947=CARTESIAN_POINT('Ctrl Pts',(78.1225481710407,-8.16200436801017,135.549115795808));
#74948=CARTESIAN_POINT('Ctrl Pts',(78.1537863391279,-8.0980617089239,135.545246712961));
#74949=CARTESIAN_POINT('Ctrl Pts',(78.1849779639025,-8.03421432121068,135.541383394855));
#74950=CARTESIAN_POINT('Ctrl Pts',(78.2195335859642,-7.97188848336657,135.537520076748));
#74951=CARTESIAN_POINT('Ctrl Pts',(78.2572788690438,-7.91145940717916,135.533656758642));
#74952=CARTESIAN_POINT('Ctrl Pts',(78.2949798769208,-7.85110121427484,135.529797972206));
#74953=CARTESIAN_POINT('Ctrl Pts',(78.3358628578839,-7.79263577363492,135.52593918577));
#74954=CARTESIAN_POINT('Ctrl Pts',(78.3797074616774,-7.73641397097142,135.522080399334));
#74955=CARTESIAN_POINT('Ctrl Pts',(78.4235244465856,-7.68022758392105,135.518224043651));
#74956=CARTESIAN_POINT('Ctrl Pts',(78.4702990549624,-7.62628241299098,135.514367687968));
#74957=CARTESIAN_POINT('Ctrl Pts',(78.5197683434641,-7.57489937004817,135.510511332285));
#74958=CARTESIAN_POINT('Ctrl Pts',(78.5692230182428,-7.52353150617074,135.506656115807));
#74959=CARTESIAN_POINT('Ctrl Pts',(78.6213704560568,-7.47472461743221,135.50280089933));
#74960=CARTESIAN_POINT('Ctrl Pts',(78.6759094097281,-7.42876428526668,135.498945682853));
#74961=CARTESIAN_POINT('Ctrl Pts',(78.7304504957095,-7.38280215618959,135.495090315648));
#74962=CARTESIAN_POINT('Ctrl Pts',(78.7873829102919,-7.33968711599724,135.491234948444));
#74963=CARTESIAN_POINT('Ctrl Pts',(78.8463720764142,-7.29966468706224,135.487379581239));
#74964=CARTESIAN_POINT('Ctrl Pts',(78.9054229881079,-7.25960036555775,135.483520178516));
#74965=CARTESIAN_POINT('Ctrl Pts',(78.9665345461123,-7.22263539062787,135.479660775793));
#74966=CARTESIAN_POINT('Ctrl Pts',(79.0293436696696,-7.18897160406316,135.475801373071));
#74967=CARTESIAN_POINT('Ctrl Pts',(79.0921883562461,-7.15528875679807,135.471939785124));
#74968=CARTESIAN_POINT('Ctrl Pts',(79.1567320820357,-7.12491102578324,135.468078197177));
#74969=CARTESIAN_POINT('Ctrl Pts',(79.2225901682402,-7.09799276657967,135.46421660923));
#74970=CARTESIAN_POINT('Ctrl Pts',(79.2885634755271,-7.07102741291679,135.460348265296));
#74971=CARTESIAN_POINT('Ctrl Pts',(79.3558552755072,-7.04753377516652,135.456479921363));
#74972=CARTESIAN_POINT('Ctrl Pts',(79.4240647345015,-7.02761663653966,135.452611577429));
#74973=CARTESIAN_POINT('Ctrl Pts',(79.4645655483546,-7.01579041278846,135.450314666123));
#74974=CARTESIAN_POINT('Ctrl Pts',(79.5053896608541,-7.00522416360188,135.448017754817));
#74975=CARTESIAN_POINT('Ctrl Pts',(79.5464518564912,-6.99593122772204,135.44572084351));
#74976=CARTESIAN_POINT('Ctrl Pts',(79.6192550066374,-6.9794548801799,135.441648426628));
#74977=CARTESIAN_POINT('Ctrl Pts',(79.6931072768256,-6.9669168711275,135.437576009747));
#74978=CARTESIAN_POINT('Ctrl Pts',(79.7675435326616,-6.95844139116886,135.433503592865));
#74979=CARTESIAN_POINT('Ctrl Pts',(79.8381398313005,-6.95040313739657,135.429641260523));
#74980=CARTESIAN_POINT('Ctrl Pts',(79.9092607958587,-6.94601875938677,135.42577892818));
#74981=CARTESIAN_POINT('Ctrl Pts',(79.980496462632,-6.9453425651632,135.421916595838));
#74982=CARTESIAN_POINT('Ctrl Pts',(80.0516622919897,-6.94466703386116,135.418058050016));
#74983=CARTESIAN_POINT('Ctrl Pts',(80.1229421172637,-6.94769247846982,135.414199504194));
#74984=CARTESIAN_POINT('Ctrl Pts',(80.1939215987489,-6.95442135911652,135.410340958372));
#74985=CARTESIAN_POINT('Ctrl Pts',(80.264855239782,-6.96114589407173,135.406484904502));
#74986=CARTESIAN_POINT('Ctrl Pts',(80.3354884395999,-6.97156907186203,135.402628850632));
#74987=CARTESIAN_POINT('Ctrl Pts',(80.4054093394314,-6.98564133531246,135.398772796763));
#74988=CARTESIAN_POINT('Ctrl Pts',(80.4753084723093,-6.99970921795104,135.394917943314));
#74989=CARTESIAN_POINT('Ctrl Pts',(80.5444952700206,-7.01742383308555,135.391063089866));
#74990=CARTESIAN_POINT('Ctrl Pts',(80.6125671730664,-7.03868436477413,135.387208236418));
#74991=CARTESIAN_POINT('Ctrl Pts',(80.6806707825929,-7.05995479917745,135.383351587459));
#74992=CARTESIAN_POINT('Ctrl Pts',(80.7476579949989,-7.08477430739439,135.3794949385));
#74993=CARTESIAN_POINT('Ctrl Pts',(80.8131416938626,-7.11299227659179,135.375638289541));
#74994=CARTESIAN_POINT('Ctrl Pts',(80.8786429816968,-7.14121782515682,135.371780604683));
#74995=CARTESIAN_POINT('Ctrl Pts',(80.9426395127162,-7.17284344390741,135.367922919825));
#74996=CARTESIAN_POINT('Ctrl Pts',(81.004766625319,-7.20767146115866,135.364065234967));
#74997=CARTESIAN_POINT('Ctrl Pts',(81.06696585699,-7.24253990784641,135.36020307199));
#74998=CARTESIAN_POINT('Ctrl Pts',(81.1272909249947,-7.2806179182745,135.356340909013));
#74999=CARTESIAN_POINT('Ctrl Pts',(81.1854050203164,-7.32166377018525,135.352478746035));
#75000=CARTESIAN_POINT('Ctrl Pts',(81.2079550446943,-7.33759080055679,135.35098011014));
#75001=CARTESIAN_POINT('Ctrl Pts',(81.2301725106883,-7.35396425196326,135.349481474244));
#75002=CARTESIAN_POINT('Ctrl Pts',(81.2520391107129,-7.37076839346111,135.347982838348));
#75003=CARTESIAN_POINT('',(77.945250359968,-9.00121625991051,135.654074719411));
#75004=CARTESIAN_POINT('Ctrl Pts',(77.945250359968,-9.00121625991051,135.654074719411));
#75005=CARTESIAN_POINT('Ctrl Pts',(77.9452088811236,-8.93114189521501,135.650257838806));
#75006=CARTESIAN_POINT('Ctrl Pts',(77.9487563144495,-8.86092442684195,135.646440958201));
#75007=CARTESIAN_POINT('Ctrl Pts',(77.9559102037764,-8.79096778364445,135.642624077596));
#75008=CARTESIAN_POINT('Ctrl Pts',(77.9630536357837,-8.72111340076158,135.638812776381));
#75009=CARTESIAN_POINT('Ctrl Pts',(77.9737930081513,-8.65151957937679,135.635001475166));
#75010=CARTESIAN_POINT('Ctrl Pts',(77.9880938466836,-8.5825898986039,135.631190173951));
#75011=CARTESIAN_POINT('Ctrl Pts',(78.0023832068387,-8.51371554331888,135.627381931827));
#75012=CARTESIAN_POINT('Ctrl Pts',(78.0202282665398,-8.44550475924146,135.623573689702));
#75013=CARTESIAN_POINT('Ctrl Pts',(78.0415429670004,-8.37835411012833,135.619765447577));
#75014=CARTESIAN_POINT('Ctrl Pts',(78.0628481279409,-8.31123351468479,135.615958909853));
#75015=CARTESIAN_POINT('Ctrl Pts',(78.0876196992428,-8.24517258878994,135.61215237213));
#75016=CARTESIAN_POINT('Ctrl Pts',(78.1157214210871,-8.18055396788435,135.608345834406));
#75017=CARTESIAN_POINT('Ctrl Pts',(78.1438205431129,-8.11594132514243,135.604539648843));
#75018=CARTESIAN_POINT('Ctrl Pts',(78.1752490033444,-8.05277117987547,135.60073346328));
#75019=CARTESIAN_POINT('Ctrl Pts',(78.209822671994,-7.99140558359992,135.596927277716));
#75020=CARTESIAN_POINT('Ctrl Pts',(78.2444287085066,-7.92998253686311,135.593117528803));
#75021=CARTESIAN_POINT('Ctrl Pts',(78.2821855870687,-7.87036784851871,135.589307779889));
#75022=CARTESIAN_POINT('Ctrl Pts',(78.3228640638333,-7.81289738686239,135.585498030976));
#75023=CARTESIAN_POINT('Ctrl Pts',(78.3635622899698,-7.75539902333731,135.581686432432));
#75024=CARTESIAN_POINT('Ctrl Pts',(78.407184627001,-7.70004735028743,135.577874833887));
#75025=CARTESIAN_POINT('Ctrl Pts',(78.4534612670308,-7.64714542173745,135.574063235343));
#75026=CARTESIAN_POINT('Ctrl Pts',(78.4998192121047,-7.59415054794265,135.570244940069));
#75027=CARTESIAN_POINT('Ctrl Pts',(78.5488404216445,-7.54361436930265,135.566426644794));
#75028=CARTESIAN_POINT('Ctrl Pts',(78.6002185439983,-7.4958027263907,135.56260834952));
#75029=CARTESIAN_POINT('Ctrl Pts',(78.6358004088325,-7.46269082315915,135.559963993126));
#75030=CARTESIAN_POINT('Ctrl Pts',(78.6725119658444,-7.43088485820555,135.557319636732));
#75031=CARTESIAN_POINT('Ctrl Pts',(78.7102431226447,-7.4004610789935,135.554675280338));
#75032=CARTESIAN_POINT('Ctrl Pts',(78.765449361827,-7.35594660940278,135.550806197491));
#75033=CARTESIAN_POINT('Ctrl Pts',(78.823070982614,-7.31420637759796,135.546937114644));
#75034=CARTESIAN_POINT('Ctrl Pts',(78.8827977135628,-7.27551265192246,135.543068031797));
#75035=CARTESIAN_POINT('Ctrl Pts',(78.942435454661,-7.23687657796856,135.539204713691));
#75036=CARTESIAN_POINT('Ctrl Pts',(79.0041716756558,-7.201278262049,135.535341395584));
#75037=CARTESIAN_POINT('Ctrl Pts',(79.067663588119,-7.16894937874977,135.531478077478));
#75038=CARTESIAN_POINT('Ctrl Pts',(79.1310810245934,-7.13665841721817,135.527619291042));
#75039=CARTESIAN_POINT('Ctrl Pts',(79.1962496310247,-7.10762948996541,135.523760504606));
#75040=CARTESIAN_POINT('Ctrl Pts',(79.2627997262892,-7.08204970894948,135.51990171817));
#75041=CARTESIAN_POINT('Ctrl Pts',(79.3293078998736,-7.05648604131993,135.516045362487));
#75042=CARTESIAN_POINT('Ctrl Pts',(79.3971953833863,-7.03436738318268,135.512189006804));
#75043=CARTESIAN_POINT('Ctrl Pts',(79.4660714454971,-7.01583320731686,135.50833265112));
#75044=CARTESIAN_POINT('Ctrl Pts',(79.5349271609297,-6.99730450663215,135.504477434643));
#75045=CARTESIAN_POINT('Ctrl Pts',(79.6047704063476,-6.9823583121868,135.500622218166));
#75046=CARTESIAN_POINT('Ctrl Pts',(79.6751958367452,-6.97108407812636,135.496767001689));
#75047=CARTESIAN_POINT('Ctrl Pts',(79.7456240205664,-6.95980940327711,135.492911634484));
#75048=CARTESIAN_POINT('Ctrl Pts',(79.816633954534,-6.95220704845246,135.48905626728));
#75049=CARTESIAN_POINT('Ctrl Pts',(79.8878123795719,-6.94831496074015,135.485200900075));
#75050=CARTESIAN_POINT('Ctrl Pts',(79.9590653090116,-6.94441879907333,135.481341497352));
#75051=CARTESIAN_POINT('Ctrl Pts',(80.0304865955319,-6.94424068370814,135.477482094629));
#75052=CARTESIAN_POINT('Ctrl Pts',(80.1016610683356,-6.9477664388075,135.473622691907));
#75053=CARTESIAN_POINT('Ctrl Pts',(80.172875840685,-6.95129419021709,135.46976110396));
#75054=CARTESIAN_POINT('Ctrl Pts',(80.2438430376165,-6.95852993759325,135.465899516013));
#75055=CARTESIAN_POINT('Ctrl Pts',(80.3141534558341,-6.96940768033377,135.462037928066));
#75056=CARTESIAN_POINT('Ctrl Pts',(80.3845868846486,-6.98030445407512,135.458169584132));
#75057=CARTESIAN_POINT('Ctrl Pts',(80.4543607649208,-6.9948558454545,135.454301240199));
#75058=CARTESIAN_POINT('Ctrl Pts',(80.5230776005261,-7.01294504697834,135.450432896265));
#75059=CARTESIAN_POINT('Ctrl Pts',(80.5638796800099,-7.02368589428125,135.448135984959));
#75060=CARTESIAN_POINT('Ctrl Pts',(80.6043093824187,-7.03567309355378,135.445839073653));
#75061=CARTESIAN_POINT('Ctrl Pts',(80.6442868085185,-7.04887415299036,135.443542162346));
#75062=CARTESIAN_POINT('Ctrl Pts',(80.7116141902558,-7.07110651897124,135.439673853667));
#75063=CARTESIAN_POINT('Ctrl Pts',(80.7779213073233,-7.09687140314609,135.435805544988));
#75064=CARTESIAN_POINT('Ctrl Pts',(80.8428113700394,-7.1260558820946,135.431937236309));
#75065=CARTESIAN_POINT('Ctrl Pts',(80.907616628674,-7.15520222018102,135.428073983079));
#75066=CARTESIAN_POINT('Ctrl Pts',(80.9710080660985,-7.18775909376035,135.424210729848));
#75067=CARTESIAN_POINT('Ctrl Pts',(81.0326051384994,-7.22356418904463,135.420347476618));
#75068=CARTESIAN_POINT('Ctrl Pts',(81.0941310956293,-7.25932794650305,135.416488683604));
#75069=CARTESIAN_POINT('Ctrl Pts',(81.1538663843257,-7.29833223449443,135.41262989059));
#75070=CARTESIAN_POINT('Ctrl Pts',(81.2114532906711,-7.34036796637863,135.408771097577));
#75071=CARTESIAN_POINT('Ctrl Pts',(81.2251040198816,-7.35033235636819,135.40785638724));
#75072=CARTESIAN_POINT('Ctrl Pts',(81.2386341418168,-7.36046688367673,135.406941676903));
#75073=CARTESIAN_POINT('Ctrl Pts',(81.2520391107129,-7.37076839346111,135.406026966566));
#75074=CARTESIAN_POINT('Ctrl Pts',(81.2520391107129,-7.37076839346111,136.106053391332));
#75075=CARTESIAN_POINT('Ctrl Pts',(81.3083146859017,-7.41401529637627,136.102186604392));
#75076=CARTESIAN_POINT('Ctrl Pts',(81.3624484341154,-7.46025936207125,136.098319817451));
#75077=CARTESIAN_POINT('Ctrl Pts',(81.4141045137042,-7.50925991976423,136.094453030511));
#75078=CARTESIAN_POINT('Ctrl Pts',(81.467120080933,-7.55955007692093,136.090484477253));
#75079=CARTESIAN_POINT('Ctrl Pts',(81.5175252609129,-7.61274362222067,136.086515923994));
#75080=CARTESIAN_POINT('Ctrl Pts',(81.5649910403901,-7.66853441426421,136.082547370735));
#75081=CARTESIAN_POINT('Ctrl Pts',(81.6111305654479,-7.72276634041901,136.078689703917));
#75082=CARTESIAN_POINT('Ctrl Pts',(81.6544924636885,-7.77945187547075,136.074832037098));
#75083=CARTESIAN_POINT('Ctrl Pts',(81.6948115872083,-7.83827230111163,136.070974370279));
#75084=CARTESIAN_POINT('Ctrl Pts',(81.7351106664465,-7.89706348471872,136.067118621264));
#75085=CARTESIAN_POINT('Ctrl Pts',(81.7723696984119,-7.95798705275809,136.063262872248));
#75086=CARTESIAN_POINT('Ctrl Pts',(81.8063653527452,-8.02069321716743,136.059407123233));
#75087=CARTESIAN_POINT('Ctrl Pts',(81.8403554784318,-8.08338918379615,136.055552001271));
#75088=CARTESIAN_POINT('Ctrl Pts',(81.8710830494685,-8.14786674381296,136.051696879308));
#75089=CARTESIAN_POINT('Ctrl Pts',(81.8983702885415,-8.21375079645013,136.047841757346));
#75090=CARTESIAN_POINT('Ctrl Pts',(81.927056966845,-8.28301374453645,136.043788923592));
#75091=CARTESIAN_POINT('Ctrl Pts',(81.9519407108041,-8.3538307905123,136.039736089839));
#75092=CARTESIAN_POINT('Ctrl Pts',(81.9728728500854,-8.4257437158411,136.035683256085));
#75093=CARTESIAN_POINT('Ctrl Pts',(81.9928102665477,-8.49423924427389,136.031823018328));
#75094=CARTESIAN_POINT('Ctrl Pts',(82.0091630513749,-8.56372835764467,136.027962780571));
#75095=CARTESIAN_POINT('Ctrl Pts',(82.0218549347861,-8.63380307868442,136.024102542813));
#75096=CARTESIAN_POINT('Ctrl Pts',(82.0345557101281,-8.703926894058,136.020239600574));
#75097=CARTESIAN_POINT('Ctrl Pts',(82.0435904207257,-8.77463665202572,136.016376658335));
#75098=CARTESIAN_POINT('Ctrl Pts',(82.0489346542456,-8.84551911078864,136.012513716096));
#75099=CARTESIAN_POINT('Ctrl Pts',(82.0542875354261,-8.91651626653303,136.008644523117));
#75100=CARTESIAN_POINT('Ctrl Pts',(82.0559380205708,-8.98768619634296,136.004775330138));
#75101=CARTESIAN_POINT('Ctrl Pts',(82.0539137429452,-9.05861654238137,136.000906137159));
#75102=CARTESIAN_POINT('Ctrl Pts',(82.0536175569377,-9.06899485004974,136.000340008874));
#75103=CARTESIAN_POINT('Ctrl Pts',(82.0532427894454,-9.07936804108318,135.999773880589));
#75104=CARTESIAN_POINT('Ctrl Pts',(82.0527896193309,-9.0897348386495,135.999207752304));
#75105=CARTESIAN_POINT('Ctrl Pts',(82.0496925249742,-9.16058450240403,135.995338669457));
#75106=CARTESIAN_POINT('Ctrl Pts',(82.0429171171316,-9.23141240638119,135.99146958661));
#75107=CARTESIAN_POINT('Ctrl Pts',(82.0324642301758,-9.30180575799021,135.987600503763));
#75108=CARTESIAN_POINT('Ctrl Pts',(82.0220269175002,-9.37209422701601,135.983737185657));
#75109=CARTESIAN_POINT('Ctrl Pts',(82.0079230726634,-9.44194895226674,135.97987386755));
#75110=CARTESIAN_POINT('Ctrl Pts',(81.9902054844461,-9.51095957979161,135.976010549444));
#75111=CARTESIAN_POINT('Ctrl Pts',(81.9725086789529,-9.57988925787698,135.972151763008));
#75112=CARTESIAN_POINT('Ctrl Pts',(81.9512066702234,-9.64797633672259,135.968292976572));
#75113=CARTESIAN_POINT('Ctrl Pts',(81.926403461125,-9.71481974473689,135.964434190136));
#75114=CARTESIAN_POINT('Ctrl Pts',(81.9016158762296,-9.78162104630555,135.960577834453));
#75115=CARTESIAN_POINT('Ctrl Pts',(81.8733316352398,-9.84717977697588,135.95672147877));
#75116=CARTESIAN_POINT('Ctrl Pts',(81.8417044010277,-9.91111056504417,135.952865123087));
#75117=CARTESIAN_POINT('Ctrl Pts',(81.8100865098174,-9.97502246731751,135.949009906609));
#75118=CARTESIAN_POINT('Ctrl Pts',(81.7751278012401,-10.037306946552,135.945154690132));
#75119=CARTESIAN_POINT('Ctrl Pts',(81.73702912834,-10.0976007333262,135.941299473655));
#75120=CARTESIAN_POINT('Ctrl Pts',(81.6989289658958,-10.1578968774073,135.93744410645));
#75121=CARTESIAN_POINT('Ctrl Pts',(81.6576888567552,-10.2162017650157,135.933588739246));
#75122=CARTESIAN_POINT('Ctrl Pts',(81.6135535318411,-10.2721802397393,135.929733372041));
#75123=CARTESIAN_POINT('Ctrl Pts',(81.5693720092769,-10.3282173086614,135.925873969318));
#75124=CARTESIAN_POINT('Ctrl Pts',(81.5222895227638,-10.3819227213963,135.922014566595));
#75125=CARTESIAN_POINT('Ctrl Pts',(81.4725911750785,-10.4329943452717,135.918155163873));
#75126=CARTESIAN_POINT('Ctrl Pts',(81.4228646877985,-10.4840948863017,135.914293575926));
#75127=CARTESIAN_POINT('Ctrl Pts',(81.370519747522,-10.5325583396234,135.910431987979));
#75128=CARTESIAN_POINT('Ctrl Pts',(81.3158763962692,-10.5781213110029,135.906570400032));
#75129=CARTESIAN_POINT('Ctrl Pts',(81.2611374445147,-10.623763996434,135.902702056098));
#75130=CARTESIAN_POINT('Ctrl Pts',(81.204092442359,-10.6664957772108,135.898833712165));
#75131=CARTESIAN_POINT('Ctrl Pts',(81.1450918128935,-10.7060956311251,135.894965368231));
#75132=CARTESIAN_POINT('Ctrl Pts',(81.1100589370072,-10.7296088847949,135.892668456925));
#75133=CARTESIAN_POINT('Ctrl Pts',(81.0743370944697,-10.7520187877172,135.890371545619));
#75134=CARTESIAN_POINT('Ctrl Pts',(81.0380034848463,-10.7732868713062,135.888074634312));
#75135=CARTESIAN_POINT('Ctrl Pts',(80.9768005357524,-10.8091123632051,135.884205551465));
#75136=CARTESIAN_POINT('Ctrl Pts',(80.9136208229209,-10.8418357801991,135.880336468618));
#75137=CARTESIAN_POINT('Ctrl Pts',(80.848811599609,-10.871233932695,135.876467385771));
#75138=CARTESIAN_POINT('Ctrl Pts',(80.7840989388076,-10.9005882834098,135.872604067665));
#75139=CARTESIAN_POINT('Ctrl Pts',(80.7177620256113,-10.9266270050879,135.868740749559));
#75140=CARTESIAN_POINT('Ctrl Pts',(80.6501742435435,-10.9491718794228,135.864877431452));
#75141=CARTESIAN_POINT('Ctrl Pts',(80.5826657419181,-10.9716903086288,135.861018645016));
#75142=CARTESIAN_POINT('Ctrl Pts',(80.5139097444996,-10.9907228780985,135.857159858581));
#75143=CARTESIAN_POINT('Ctrl Pts',(80.4442996139071,-11.006139430743,135.853301072145));
#75144=CARTESIAN_POINT('Ctrl Pts',(80.3747333325926,-11.0215462720898,135.849444716462));
#75145=CARTESIAN_POINT('Ctrl Pts',(80.3043144587391,-11.0333415109886,135.845588360778));
#75146=CARTESIAN_POINT('Ctrl Pts',(80.2334500995799,-11.041445226673,135.841732005095));
#75147=CARTESIAN_POINT('Ctrl Pts',(80.162606674462,-11.0495465484388,135.837876788618));
#75148=CARTESIAN_POINT('Ctrl Pts',(80.0913185076772,-11.053958456799,135.834021572141));
#75149=CARTESIAN_POINT('Ctrl Pts',(80.0199997326211,-11.0546526648548,135.830166355663));
#75150=CARTESIAN_POINT('Ctrl Pts',(79.9486781692142,-11.0553469000522,135.826310988459));
#75151=CARTESIAN_POINT('Ctrl Pts',(79.8773264809416,-11.0523231438444,135.822455621254));
#75152=CARTESIAN_POINT('Ctrl Pts',(79.8063589810277,-11.0456052205329,135.81860025405));
#75153=CARTESIAN_POINT('Ctrl Pts',(79.7353171974932,-11.0388802653875,135.814740851327));
#75154=CARTESIAN_POINT('Ctrl Pts',(79.6646608896919,-11.0284534700421,135.810881448604));
#75155=CARTESIAN_POINT('Ctrl Pts',(79.5947985234111,-11.0144004879542,135.807022045881));
#75156=CARTESIAN_POINT('Ctrl Pts',(79.5248966005098,-11.0003395489575,135.803160457934));
#75157=CARTESIAN_POINT('Ctrl Pts',(79.4557899848465,-10.9826484565105,135.799298869987));
#75158=CARTESIAN_POINT('Ctrl Pts',(79.3878735471228,-10.9614532286516,135.79543728204));
#75159=CARTESIAN_POINT('Ctrl Pts',(79.3198382871569,-10.9402209189819,135.791568938107));
#75160=CARTESIAN_POINT('Ctrl Pts',(79.2529978181222,-10.9154724026927,135.787700594174));
#75161=CARTESIAN_POINT('Ctrl Pts',(79.1877278906751,-10.8873822037184,135.78383225024));
#75162=CARTESIAN_POINT('Ctrl Pts',(79.1489724860621,-10.870703051933,135.781535338934));
#75163=CARTESIAN_POINT('Ctrl Pts',(79.1107703609553,-10.8528466407429,135.779238427627));
#75164=CARTESIAN_POINT('Ctrl Pts',(79.0731957056113,-10.8338569634523,135.776941516321));
#75165=CARTESIAN_POINT('Ctrl Pts',(79.0099022497155,-10.8018693832321,135.773072433474));
#75166=CARTESIAN_POINT('Ctrl Pts',(78.9481427918078,-10.7665385540289,135.769203350627));
#75167=CARTESIAN_POINT('Ctrl Pts',(78.888293184181,-10.7280351611473,135.76533426778));
#75168=CARTESIAN_POINT('Ctrl Pts',(78.8285327494848,-10.689589136401,135.761470949674));
#75169=CARTESIAN_POINT('Ctrl Pts',(78.7706769218817,-10.6479801915525,135.757607631567));
#75170=CARTESIAN_POINT('Ctrl Pts',(78.7150779443411,-10.6034253563485,135.753744313461));
#75171=CARTESIAN_POINT('Ctrl Pts',(78.6595441843798,-10.5589227839491,135.749885527025));
#75172=CARTESIAN_POINT('Ctrl Pts',(78.6062623933193,-10.5114814873496,135.746026740589));
#75173=CARTESIAN_POINT('Ctrl Pts',(78.555555272579,-10.4613613488545,135.742167954153));
#75174=CARTESIAN_POINT('Ctrl Pts',(78.5048800936066,-10.4112727823714,135.73831159847));
#75175=CARTESIAN_POINT('Ctrl Pts',(78.4567767119,-10.3585090626023,135.734455242787));
#75176=CARTESIAN_POINT('Ctrl Pts',(78.4115330784901,-10.3033688663494,135.730598887103));
#75177=CARTESIAN_POINT('Ctrl Pts',(78.3663028105026,-10.2482449590626,135.726743670626));
#75178=CARTESIAN_POINT('Ctrl Pts',(78.3239309216268,-10.1907463443663,135.722888454149));
#75179=CARTESIAN_POINT('Ctrl Pts',(78.2846657944256,-10.1312056071672,135.719033237672));
#75180=CARTESIAN_POINT('Ctrl Pts',(78.2453991320754,-10.0716625421035,135.715177870467));
#75181=CARTESIAN_POINT('Ctrl Pts',(78.2092397381529,-10.0100776027747,135.711322503263));
#75182=CARTESIAN_POINT('Ctrl Pts',(78.176392312414,-9.94681178925757,135.707467136058));
#75183=CARTESIAN_POINT('Ctrl Pts',(78.1435105043773,-9.88347975368548,135.703607733335));
#75184=CARTESIAN_POINT('Ctrl Pts',(78.1139478091927,-9.81846376375441,135.699748330612));
#75185=CARTESIAN_POINT('Ctrl Pts',(78.0878622116925,-9.75214801803009,135.69588892789));
#75186=CARTESIAN_POINT('Ctrl Pts',(78.0617618443221,-9.68579472380968,135.692027339943));
#75187=CARTESIAN_POINT('Ctrl Pts',(78.0391426479369,-9.61814066971615,135.688165751996));
#75188=CARTESIAN_POINT('Ctrl Pts',(78.020112920712,-9.54958594939138,135.684304164049));
#75189=CARTESIAN_POINT('Ctrl Pts',(78.0010499002972,-9.4809112901261,135.680435820115));
#75190=CARTESIAN_POINT('Ctrl Pts',(77.9855889924593,-9.41133329297089,135.676567476182));
#75191=CARTESIAN_POINT('Ctrl Pts',(77.9737873736295,-9.34126229682866,135.672699132248));
#75192=CARTESIAN_POINT('Ctrl Pts',(77.9667799119894,-9.29965615578732,135.670402220942));
#75193=CARTESIAN_POINT('Ctrl Pts',(77.9610615928321,-9.25787632082747,135.668105309635));
#75194=CARTESIAN_POINT('Ctrl Pts',(77.9566356952625,-9.21600898274021,135.665808398329));
#75195=CARTESIAN_POINT('Ctrl Pts',(77.9490991887904,-9.14471644614228,135.66189717204));
#75196=CARTESIAN_POINT('Ctrl Pts',(77.94529286412,-9.07302272422374,135.657985945751));
#75197=CARTESIAN_POINT('Ctrl Pts',(77.9452503599685,-9.00121626084845,135.654074719462));
#75198=CARTESIAN_POINT('Origin',(80.,-9.,141.545925280538));
#75199=CARTESIAN_POINT('',(81.2520391107129,-7.37076839346112,136.806140361831));
#75200=CARTESIAN_POINT('',(81.2520391107129,-7.37076839346111,136.747866921905));
#75201=CARTESIAN_POINT('',(81.2520391107129,-7.37076839346111,141.545925280538));
#75202=CARTESIAN_POINT('',(77.9452505319477,-9.0014785258654,136.295925280587));
#75203=CARTESIAN_POINT('Ctrl Pts',(81.2520391107129,-7.37076839346111,136.747866921905));
#75204=CARTESIAN_POINT('Ctrl Pts',(81.3085184556658,-7.41417189026582,136.74401000071));
#75205=CARTESIAN_POINT('Ctrl Pts',(81.3627855884167,-7.46055213904031,136.740153079514));
#75206=CARTESIAN_POINT('Ctrl Pts',(81.4145162201043,-7.50965056930868,136.736296158318));
#75207=CARTESIAN_POINT('Ctrl Pts',(81.4662266025468,-7.5587297806711,136.732440746861));
#75208=CARTESIAN_POINT('Ctrl Pts',(81.5154021025145,-7.61052472766807,136.728585335404));
#75209=CARTESIAN_POINT('Ctrl Pts',(81.5617531766557,-7.66473801158507,136.724729923947));
#75210=CARTESIAN_POINT('Ctrl Pts',(81.6081016121926,-7.71894820932962,136.720874731965));
#75211=CARTESIAN_POINT('Ctrl Pts',(81.6516256266796,-7.77557610039535,136.717019539983));
#75212=CARTESIAN_POINT('Ctrl Pts',(81.6920752305164,-7.83429035485974,136.713164348002));
#75213=CARTESIAN_POINT('Ctrl Pts',(81.7325646822271,-7.89306245014317,136.709305358178));
#75214=CARTESIAN_POINT('Ctrl Pts',(81.7699733971474,-7.95392461339505,136.705446368354));
#75215=CARTESIAN_POINT('Ctrl Pts',(81.8040946199613,-8.01651631191624,136.70158737853));
#75216=CARTESIAN_POINT('Ctrl Pts',(81.8382322243345,-8.07913806063906,136.69772653601));
#75217=CARTESIAN_POINT('Ctrl Pts',(81.8690789820362,-8.14349056008712,136.693865693489));
#75218=CARTESIAN_POINT('Ctrl Pts',(81.8964753095992,-8.2091909442978,136.690004850969));
#75219=CARTESIAN_POINT('Ctrl Pts',(81.9239220747863,-8.27501228527817,136.686136900498));
#75220=CARTESIAN_POINT('Ctrl Pts',(81.9479055541882,-8.34218601034174,136.682268950028));
#75221=CARTESIAN_POINT('Ctrl Pts',(81.9683154627715,-8.41031211517045,136.678400999558));
#75222=CARTESIAN_POINT('Ctrl Pts',(81.9862840426306,-8.47028932428496,136.674995713511));
#75223=CARTESIAN_POINT('Ctrl Pts',(82.0014835403753,-8.53100427227776,136.671590427464));
#75224=CARTESIAN_POINT('Ctrl Pts',(82.0138717544801,-8.59217881491123,136.668185141417));
#75225=CARTESIAN_POINT('Ctrl Pts',(82.0279472318517,-8.66168527349155,136.66431605857));
#75226=CARTESIAN_POINT('Ctrl Pts',(82.0384476506382,-8.73205742237571,136.660446975723));
#75227=CARTESIAN_POINT('Ctrl Pts',(82.045274300028,-8.80289444415531,136.656577892876));
#75228=CARTESIAN_POINT('Ctrl Pts',(82.0520907780507,-8.87362592230528,136.65271457477));
#75229=CARTESIAN_POINT('Ctrl Pts',(82.0552443056657,-8.94482041888086,136.648851256664));
#75230=CARTESIAN_POINT('Ctrl Pts',(82.0546871818792,-9.01606695744053,136.644987938557));
#75231=CARTESIAN_POINT('Ctrl Pts',(82.0541307115987,-9.08722992383783,136.641129152121));
#75232=CARTESIAN_POINT('Ctrl Pts',(82.0498722394196,-9.15844432755198,136.637270365686));
#75233=CARTESIAN_POINT('Ctrl Pts',(82.0419160056416,-9.22929585343982,136.63341157925));
#75234=CARTESIAN_POINT('Ctrl Pts',(82.0339647837074,-9.30010274806166,136.629555223566));
#75235=CARTESIAN_POINT('Ctrl Pts',(82.022320475588,-9.37054673676131,136.625698867883));
#75236=CARTESIAN_POINT('Ctrl Pts',(82.0070393018439,-9.44021676859681,136.6218425122));
#75237=CARTESIAN_POINT('Ctrl Pts',(81.9917626423116,-9.50986621920728,136.617987295723));
#75238=CARTESIAN_POINT('Ctrl Pts',(81.9728513540896,-9.57874169261185,136.614132079245));
#75239=CARTESIAN_POINT('Ctrl Pts',(81.9504127845803,-9.64644221106426,136.610276862768));
#75240=CARTESIAN_POINT('Ctrl Pts',(81.9279733377901,-9.7141453764044,136.606421495564));
#75241=CARTESIAN_POINT('Ctrl Pts',(81.9020064908407,-9.78067303516738,136.602566128359));
#75242=CARTESIAN_POINT('Ctrl Pts',(81.8726689525193,-9.84564091479191,136.598710761154));
#75243=CARTESIAN_POINT('Ctrl Pts',(81.8433007057953,-9.91067679807057,136.594851358432));
#75244=CARTESIAN_POINT('Ctrl Pts',(81.8105549249676,-9.97414919940608,136.590991955709));
#75245=CARTESIAN_POINT('Ctrl Pts',(81.7746354615352,-10.0356961625697,136.587132552986));
#75246=CARTESIAN_POINT('Ctrl Pts',(81.7386956602205,-10.0972779741073,136.583270965039));
#75247=CARTESIAN_POINT('Ctrl Pts',(81.6995788656065,-10.1569317707976,136.579409377092));
#75248=CARTESIAN_POINT('Ctrl Pts',(81.657532177304,-10.2143247686273,136.575547789145));
#75249=CARTESIAN_POINT('Ctrl Pts',(81.6154119268133,-10.2718181775639,136.571679445212));
#75250=CARTESIAN_POINT('Ctrl Pts',(81.5703518557309,-10.3270425141682,136.567811101278));
#75251=CARTESIAN_POINT('Ctrl Pts',(81.5226387640878,-10.3796987919823,136.563942757345));
#75252=CARTESIAN_POINT('Ctrl Pts',(81.4943081033344,-10.4109645744313,136.561645846039));
#75253=CARTESIAN_POINT('Ctrl Pts',(81.4650427907927,-10.441325655851,136.559348934732));
#75254=CARTESIAN_POINT('Ctrl Pts',(81.4349084744057,-10.4707260902625,136.557052023426));
#75255=CARTESIAN_POINT('Ctrl Pts',(81.3841480613615,-10.520250299647,136.553182940579));
#75256=CARTESIAN_POINT('Ctrl Pts',(81.3307213118379,-10.5672405174436,136.549313857732));
#75257=CARTESIAN_POINT('Ctrl Pts',(81.2749114269963,-10.61139641796,136.545444774885));
#75258=CARTESIAN_POINT('Ctrl Pts',(81.2191846960997,-10.6554865283868,136.541581456779));
#75259=CARTESIAN_POINT('Ctrl Pts',(81.1610822558933,-10.696750405096,136.537718138672));
#75260=CARTESIAN_POINT('Ctrl Pts',(81.1009235091993,-10.734925067371,136.533854820566));
#75261=CARTESIAN_POINT('Ctrl Pts',(81.040835328692,-10.7730549507819,136.52999603413));
#75262=CARTESIAN_POINT('Ctrl Pts',(80.9786960410183,-10.8081025585325,136.526137247694));
#75263=CARTESIAN_POINT('Ctrl Pts',(80.9148560258896,-10.8398467366587,136.522278461258));
#75264=CARTESIAN_POINT('Ctrl Pts',(80.8510562252893,-10.8715709182803,136.518422105575));
#75265=CARTESIAN_POINT('Ctrl Pts',(80.7855582566906,-10.8999955830086,136.514565749892));
#75266=CARTESIAN_POINT('Ctrl Pts',(80.7187379505123,-10.9249450176546,136.510709394209));
#75267=CARTESIAN_POINT('Ctrl Pts',(80.6519373837214,-10.9498870819879,136.506854177731));
#75268=CARTESIAN_POINT('Ctrl Pts',(80.5838157097101,-10.971355784529,136.502998961254));
#75269=CARTESIAN_POINT('Ctrl Pts',(80.5147680262649,-10.9892238289432,136.499143744777));
#75270=CARTESIAN_POINT('Ctrl Pts',(80.445717643262,-11.0070925719444,136.495288377572));
#75271=CARTESIAN_POINT('Ctrl Pts',(80.3757416497898,-11.0213602577598,136.491433010368));
#75272=CARTESIAN_POINT('Ctrl Pts',(80.3052478817002,-11.0319501207504,136.487577643163));
#75273=CARTESIAN_POINT('Ctrl Pts',(80.234680325858,-11.0425510684398,136.48371824044));
#75274=CARTESIAN_POINT('Ctrl Pts',(80.1635943948841,-11.0494664361707,136.479858837718));
#75275=CARTESIAN_POINT('Ctrl Pts',(80.0924047452201,-11.0526711683952,136.475999434995));
#75276=CARTESIAN_POINT('Ctrl Pts',(80.0211747874173,-11.0558777151642,136.472137847048));
#75277=CARTESIAN_POINT('Ctrl Pts',(79.9498414800191,-11.0553694474645,136.468276259101));
#75278=CARTESIAN_POINT('Ctrl Pts',(79.8788184278489,-11.0511734663531,136.464414671154));
#75279=CARTESIAN_POINT('Ctrl Pts',(79.8076711183032,-11.0469701442224,136.46054632722));
#75280=CARTESIAN_POINT('Ctrl Pts',(79.7368356306459,-11.039066281392,136.456677983287));
#75281=CARTESIAN_POINT('Ctrl Pts',(79.6667187079824,-11.0275406636837,136.452809639354));
#75282=CARTESIAN_POINT('Ctrl Pts',(79.6250852970937,-11.0206970835669,136.450512728047));
#75283=CARTESIAN_POINT('Ctrl Pts',(79.5837050187289,-11.0125775795324,136.448215816741));
#75284=CARTESIAN_POINT('Ctrl Pts',(79.542660481108,-11.0032069605908,136.445918905434));
#75285=CARTESIAN_POINT('Ctrl Pts',(79.4735221055763,-10.9874224150972,136.442049822587));
#75286=CARTESIAN_POINT('Ctrl Pts',(79.4050664517629,-10.9680234049621,136.43818073974));
#75287=CARTESIAN_POINT('Ctrl Pts',(79.3376994359524,-10.9450849661036,136.434311656893));
#75288=CARTESIAN_POINT('Ctrl Pts',(79.2704327936357,-10.922180704375,136.430448338787));
#75289=CARTESIAN_POINT('Ctrl Pts',(79.2042520257743,-10.8957476371235,136.426585020681));
#75290=CARTESIAN_POINT('Ctrl Pts',(79.1395513089721,-10.8659114696599,136.422721702574));
#75291=CARTESIAN_POINT('Ctrl Pts',(79.0749264860859,-10.8361103000093,136.418862916138));
#75292=CARTESIAN_POINT('Ctrl Pts',(79.011778704775,-10.8029141617227,136.415004129703));
#75293=CARTESIAN_POINT('Ctrl Pts',(78.9504838028598,-10.7664974708276,136.411145343267));
#75294=CARTESIAN_POINT('Ctrl Pts',(78.8892275122382,-10.7301037197774,136.407288987584));
#75295=CARTESIAN_POINT('Ctrl Pts',(78.8298222019966,-10.6904936885913,136.4034326319));
#75296=CARTESIAN_POINT('Ctrl Pts',(78.7726193376199,-10.6478878214597,136.399576276217));
#75297=CARTESIAN_POINT('Ctrl Pts',(78.715433371542,-10.605294540528,136.39572105974));
#75298=CARTESIAN_POINT('Ctrl Pts',(78.6604489490394,-10.5597074706402,136.391865843263));
#75299=CARTESIAN_POINT('Ctrl Pts',(78.6079873092376,-10.5113895034889,136.388010626785));
#75300=CARTESIAN_POINT('Ctrl Pts',(78.5555236183424,-10.4630696472495,136.384155259581));
#75301=CARTESIAN_POINT('Ctrl Pts',(78.505583261801,-10.4120190124883,136.380299892376));
#75302=CARTESIAN_POINT('Ctrl Pts',(78.458451935106,-10.3585385994228,136.376444525171));
#75303=CARTESIAN_POINT('Ctrl Pts',(78.4112712747642,-10.3050022069484,136.372585122449));
#75304=CARTESIAN_POINT('Ctrl Pts',(78.3669058355862,-10.2490313243411,136.368725719726));
#75305=CARTESIAN_POINT('Ctrl Pts',(78.3256015690602,-10.1909607285575,136.364866317003));
#75306=CARTESIAN_POINT('Ctrl Pts',(78.284273915734,-10.1328572527464,136.361004729056));
#75307=CARTESIAN_POINT('Ctrl Pts',(78.246011146134,-10.0726521072607,136.357143141109));
#75308=CARTESIAN_POINT('Ctrl Pts',(78.211014822882,-10.0107074742734,136.353281553162));
#75309=CARTESIAN_POINT('Ctrl Pts',(78.1759572723082,-9.94865446693053,136.349413209229));
#75310=CARTESIAN_POINT('Ctrl Pts',(78.1441777944373,-9.88485633102083,136.345544865295));
#75311=CARTESIAN_POINT('Ctrl Pts',(78.11583080815,-9.81969751676059,136.341676521362));
#75312=CARTESIAN_POINT('Ctrl Pts',(78.0989991834482,-9.78100808796084,136.339379610055));
#75313=CARTESIAN_POINT('Ctrl Pts',(78.0833767987335,-9.74183928814454,136.337082698749));
#75314=CARTESIAN_POINT('Ctrl Pts',(78.0689876162083,-9.7022739751288,136.334785787443));
#75315=CARTESIAN_POINT('Ctrl Pts',(78.0409616303172,-9.62521213353946,136.330312065342));
#75316=CARTESIAN_POINT('Ctrl Pts',(78.0175257042645,-9.54639696143254,136.325838343242));
#75317=CARTESIAN_POINT('Ctrl Pts',(77.9988702448821,-9.46634457826986,136.321364621142));
#75318=CARTESIAN_POINT('Ctrl Pts',(77.980378474062,-9.38699459858276,136.316930152813));
#75319=CARTESIAN_POINT('Ctrl Pts',(77.9665837380255,-9.30642919168824,136.312495684485));
#75320=CARTESIAN_POINT('Ctrl Pts',(77.9576251286369,-9.22517203939353,136.308061216156));
#75321=CARTESIAN_POINT('Ctrl Pts',(77.9494527016197,-9.15104578631668,136.3040159043));
#75322=CARTESIAN_POINT('Ctrl Pts',(77.9453044026692,-9.07634420048478,136.299970592443));
#75323=CARTESIAN_POINT('Ctrl Pts',(77.9452505319477,-9.0014785258654,136.295925280587));
#75324=CARTESIAN_POINT('Ctrl Pts',(77.945250531947,-9.0014785249549,136.295925280538));
#75325=CARTESIAN_POINT('Ctrl Pts',(77.9451990745752,-8.92996670708856,136.292061191873));
#75326=CARTESIAN_POINT('Ctrl Pts',(77.9488851993071,-8.85842205612611,136.288197103208));
#75327=CARTESIAN_POINT('Ctrl Pts',(77.9562925982608,-8.78726161940889,136.284333014543));
#75328=CARTESIAN_POINT('Ctrl Pts',(77.963699599031,-8.71610500790984,136.280469133592));
#75329=CARTESIAN_POINT('Ctrl Pts',(77.9748274258945,-8.64533304915,136.276605252641));
#75330=CARTESIAN_POINT('Ctrl Pts',(77.9896079183788,-8.57535751430792,136.272741371689));
#75331=CARTESIAN_POINT('Ctrl Pts',(78.004392467588,-8.505362773645,136.268876430239));
#75332=CARTESIAN_POINT('Ctrl Pts',(78.0228315710416,-8.43616536208909,136.265011488788));
#75333=CARTESIAN_POINT('Ctrl Pts',(78.0448063606777,-8.36816505695425,136.261146547337));
#75334=CARTESIAN_POINT('Ctrl Pts',(78.0668090603739,-8.3000783850039,136.257276697046));
#75335=CARTESIAN_POINT('Ctrl Pts',(78.0923562553075,-8.23319231170985,136.253406846754));
#75336=CARTESIAN_POINT('Ctrl Pts',(78.1212800534333,-8.16788887468532,136.249536996462));
#75337=CARTESIAN_POINT('Ctrl Pts',(78.150225897606,-8.10253566264064,136.245664196527));
#75338=CARTESIAN_POINT('Ctrl Pts',(78.1825532470501,-8.03876791594965,136.241791396591));
#75339=CARTESIAN_POINT('Ctrl Pts',(78.218048415587,-7.97694276147033,136.237918596656));
#75340=CARTESIAN_POINT('Ctrl Pts',(78.2536056682715,-7.91500946939994,136.234039022855));
#75341=CARTESIAN_POINT('Ctrl Pts',(78.2923415309161,-7.85502595047044,136.230159449055));
#75342=CARTESIAN_POINT('Ctrl Pts',(78.3339997518957,-7.79731935418567,136.226279875254));
#75343=CARTESIAN_POINT('Ctrl Pts',(78.3434032521695,-7.78429325798648,136.225404139987));
#75344=CARTESIAN_POINT('Ctrl Pts',(78.3529555021339,-7.7713830389363,136.224528404719));
#75345=CARTESIAN_POINT('Ctrl Pts',(78.3626532888616,-7.75859220639458,136.223652669452));
#75346=CARTESIAN_POINT('Ctrl Pts',(78.4054990456459,-7.70208107498526,136.219783586605));
#75347=CARTESIAN_POINT('Ctrl Pts',(78.4513577800799,-7.64768002160084,136.215914503758));
#75348=CARTESIAN_POINT('Ctrl Pts',(78.4999940143903,-7.59572808700198,136.212045420911));
#75349=CARTESIAN_POINT('Ctrl Pts',(78.5485577831372,-7.54385355819469,136.208182102805));
#75350=CARTESIAN_POINT('Ctrl Pts',(78.5998905079846,-7.49442125662193,136.204318784698));
#75351=CARTESIAN_POINT('Ctrl Pts',(78.653715366554,-7.4477386662526,136.200455466592));
#75352=CARTESIAN_POINT('Ctrl Pts',(78.7074770885851,-7.40111083454381,136.196596680156));
#75353=CARTESIAN_POINT('Ctrl Pts',(78.7637247725266,-7.35722662402505,136.19273789372));
#75354=CARTESIAN_POINT('Ctrl Pts',(78.8221447529236,-7.31635675410897,136.188879107284));
#75355=CARTESIAN_POINT('Ctrl Pts',(78.8805279330166,-7.27551262921406,136.185022751601));
#75356=CARTESIAN_POINT('Ctrl Pts',(78.9410802976006,-7.23767935551522,136.181166395918));
#75357=CARTESIAN_POINT('Ctrl Pts',(79.0034562665656,-7.20308649349707,136.177310040234));
#75358=CARTESIAN_POINT('Ctrl Pts',(79.0658138090448,-7.16850385055676,136.173454823757));
#75359=CARTESIAN_POINT('Ctrl Pts',(79.1299934618201,-7.13715995436414,136.16959960728));
#75360=CARTESIAN_POINT('Ctrl Pts',(79.1956234031311,-7.10923934541951,136.165744390803));
#75361=CARTESIAN_POINT('Ctrl Pts',(79.2612559103764,-7.08131764486262,136.161889023598));
#75362=CARTESIAN_POINT('Ctrl Pts',(79.3283383708565,-7.05681968541932,136.158033656394));
#75363=CARTESIAN_POINT('Ctrl Pts',(79.3964788642983,-7.0358819278716,136.154178289189));
#75364=CARTESIAN_POINT('Ctrl Pts',(79.464690682256,-7.01492225420114,136.150318886466));
#75365=CARTESIAN_POINT('Ctrl Pts',(79.5339622786305,-6.99753036445279,136.146459483743));
#75366=CARTESIAN_POINT('Ctrl Pts',(79.6038873114514,-6.98379259487751,136.142600081021));
#75367=CARTESIAN_POINT('Ctrl Pts',(79.6738519363752,-6.97004704686918,136.138738493074));
#75368=CARTESIAN_POINT('Ctrl Pts',(79.7444702531337,-6.95995980648334,136.134876905127));
#75369=CARTESIAN_POINT('Ctrl Pts',(79.8153292167477,-6.95356547519522,136.13101531718));
#75370=CARTESIAN_POINT('Ctrl Pts',(79.8863121506583,-6.94715995679532,136.127146973246));
#75371=CARTESIAN_POINT('Ctrl Pts',(79.9575360864152,-6.94446026522219,136.123278629313));
#75372=CARTESIAN_POINT('Ctrl Pts',(80.0285870917951,-6.94544887124153,136.119410285379));
#75373=CARTESIAN_POINT('Ctrl Pts',(80.0707751341201,-6.94603587704622,136.117113374073));
#75374=CARTESIAN_POINT('Ctrl Pts',(80.1129022677805,-6.94792224733129,136.114816462766));
#75375=CARTESIAN_POINT('Ctrl Pts',(80.1548831168874,-6.95109571170265,136.11251955146));
#75376=CARTESIAN_POINT('Ctrl Pts',(80.2255915701652,-6.9564407859926,136.108650857776));
#75377=CARTESIAN_POINT('Ctrl Pts',(80.2961614847423,-6.96546088698956,136.104782164092));
#75378=CARTESIAN_POINT('Ctrl Pts',(80.3661804272604,-6.97814207789188,136.100913470407));
#75379=CARTESIAN_POINT('Ctrl Pts',(80.436100256216,-6.99080531825163,136.097050252956));
#75380=CARTESIAN_POINT('Ctrl Pts',(80.5054701866994,-7.00711927976587,136.093187035504));
#75381=CARTESIAN_POINT('Ctrl Pts',(80.5738817794945,-7.02701817908419,136.089323818053));
#75382=CARTESIAN_POINT('Ctrl Pts',(80.6422141511602,-7.04689403533025,136.085465074235));
#75383=CARTESIAN_POINT('Ctrl Pts',(80.7095899251629,-7.07034644905535,136.081606330418));
#75384=CARTESIAN_POINT('Ctrl Pts',(80.77561154664,-7.09725874296618,136.077747586601));
#75385=CARTESIAN_POINT('Ctrl Pts',(80.8415882785365,-7.12415273860499,136.07389146643));
#75386=CARTESIAN_POINT('Ctrl Pts',(80.9062122370551,-7.15450176135287,136.070035346259));
#75387=CARTESIAN_POINT('Ctrl Pts',(80.9691031912749,-7.18814002550948,136.066179226088));
#75388=CARTESIAN_POINT('Ctrl Pts',(81.0319836313122,-7.22177266598216,136.062323750588));
#75389=CARTESIAN_POINT('Ctrl Pts',(81.0931312103806,-7.25869323415421,136.058468275088));
#75390=CARTESIAN_POINT('Ctrl Pts',(81.1521891448271,-7.29868940606292,136.054612799588));
#75391=CARTESIAN_POINT('Ctrl Pts',(81.1861856902748,-7.32171309777801,136.052393405203));
#75392=CARTESIAN_POINT('Ctrl Pts',(81.2194902560995,-7.34575510571162,136.050174010819));
#75393=CARTESIAN_POINT('Ctrl Pts',(81.2520391107129,-7.37076839346111,136.047954616434));
#75394=CARTESIAN_POINT('',(77.9452507823625,-8.99820692503895,136.35407471951));
#75395=CARTESIAN_POINT('Ctrl Pts',(77.9452507823632,-8.99820692415778,136.354074719462));
#75396=CARTESIAN_POINT('Ctrl Pts',(77.9453413919223,-8.89437421594169,136.348435142862));
#75397=CARTESIAN_POINT('Ctrl Pts',(77.9533058453998,-8.79087359259561,136.342795566261));
#75398=CARTESIAN_POINT('Ctrl Pts',(77.9689745018475,-8.68865936925234,136.337155989661));
#75399=CARTESIAN_POINT('Ctrl Pts',(77.9731872821077,-8.66117736632162,136.3356396952));
#75400=CARTESIAN_POINT('Ctrl Pts',(77.9779567533565,-8.6337881827006,136.334123400739));
#75401=CARTESIAN_POINT('Ctrl Pts',(77.9832790921583,-8.60651004793739,136.332607106279));
#75402=CARTESIAN_POINT('Ctrl Pts',(77.9968599435675,-8.53690525411839,136.328738023432));
#75403=CARTESIAN_POINT('Ctrl Pts',(78.0140751186039,-8.46786804761569,136.324868940585));
#75404=CARTESIAN_POINT('Ctrl Pts',(78.0348625104967,-8.39980652298718,136.320999857738));
#75405=CARTESIAN_POINT('Ctrl Pts',(78.0556189302123,-8.33184640663594,136.317136539631));
#75406=CARTESIAN_POINT('Ctrl Pts',(78.0799368611765,-8.26485954738233,136.313273221525));
#75407=CARTESIAN_POINT('Ctrl Pts',(78.10770317995,-8.19924391520985,136.309409903418));
#75408=CARTESIAN_POINT('Ctrl Pts',(78.1354369288421,-8.13370525014871,136.305551116983));
#75409=CARTESIAN_POINT('Ctrl Pts',(78.1666108424926,-8.06953506244951,136.301692330547));
#75410=CARTESIAN_POINT('Ctrl Pts',(78.2010625289041,-8.00711453954285,136.297833544111));
#75411=CARTESIAN_POINT('Ctrl Pts',(78.2354925132795,-7.94473333698852,136.293977188428));
#75412=CARTESIAN_POINT('Ctrl Pts',(78.2731959397886,-7.88410003685616,136.290120832745));
#75413=CARTESIAN_POINT('Ctrl Pts',(78.31396363746,-7.82557292832084,136.286264477061));
#75414=CARTESIAN_POINT('Ctrl Pts',(78.3547192919453,-7.76706310927942,136.282409260584));
#75415=CARTESIAN_POINT('Ctrl Pts',(78.3985371429807,-7.71065864500986,136.278554044107));
#75416=CARTESIAN_POINT('Ctrl Pts',(78.4451646335603,-7.65668896164434,136.27469882763));
#75417=CARTESIAN_POINT('Ctrl Pts',(78.4917939471352,-7.60271716822562,136.270843460425));
#75418=CARTESIAN_POINT('Ctrl Pts',(78.5412327990923,-7.55118071085677,136.26698809322));
#75419=CARTESIAN_POINT('Ctrl Pts',(78.5931894143107,-7.50237470023623,136.263132726016));
#75420=CARTESIAN_POINT('Ctrl Pts',(78.6452004139374,-7.45351760303132,136.259273323293));
#75421=CARTESIAN_POINT('Ctrl Pts',(78.6997340829042,-7.40739699112836,136.25541392057));
#75422=CARTESIAN_POINT('Ctrl Pts',(78.7564636241791,-7.36426932396856,136.251554517847));
#75423=CARTESIAN_POINT('Ctrl Pts',(78.8132252861659,-7.32111723758483,136.2476929299));
#75424=CARTESIAN_POINT('Ctrl Pts',(78.8721848938302,-7.28096174301087,136.243831341954));
#75425=CARTESIAN_POINT('Ctrl Pts',(78.9329868490229,-7.24401580356145,136.239969754007));
#75426=CARTESIAN_POINT('Ctrl Pts',(78.9938951794156,-7.20700522586667,136.236101410073));
#75427=CARTESIAN_POINT('Ctrl Pts',(79.0566518647923,-7.17321564463468,136.23223306614));
#75428=CARTESIAN_POINT('Ctrl Pts',(79.1208775529782,-7.14281361041968,136.228364722206));
#75429=CARTESIAN_POINT('Ctrl Pts',(79.1590129183687,-7.12476175739713,136.2260678109));
#75430=CARTESIAN_POINT('Ctrl Pts',(79.1976658166295,-7.10790331027639,136.223770899593));
#75431=CARTESIAN_POINT('Ctrl Pts',(79.2367541927432,-7.09226485061344,136.221473988287));
#75432=CARTESIAN_POINT('Ctrl Pts',(79.3025974689338,-7.06592230274737,136.21760490544));
#75433=CARTESIAN_POINT('Ctrl Pts',(79.3699350818581,-7.042940918566,136.213735822593));
#75434=CARTESIAN_POINT('Ctrl Pts',(79.4383904922889,-7.02348986257381,136.209866739746));
#75435=CARTESIAN_POINT('Ctrl Pts',(79.5067439075722,-7.00406778768498,136.20600342164));
#75436=CARTESIAN_POINT('Ctrl Pts',(79.576211350986,-6.98816573169893,136.202140103533));
#75437=CARTESIAN_POINT('Ctrl Pts',(79.646397118856,-6.97590450695954,136.198276785427));
#75438=CARTESIAN_POINT('Ctrl Pts',(79.7165005588474,-6.96365766463206,136.194417998991));
#75439=CARTESIAN_POINT('Ctrl Pts',(79.787320173404,-6.95504325370055,136.190559212555));
#75440=CARTESIAN_POINT('Ctrl Pts',(79.8584476361331,-6.95013159183725,136.186700426119));
#75441=CARTESIAN_POINT('Ctrl Pts',(79.9295302937763,-6.94522302396076,136.182844070436));
#75442=CARTESIAN_POINT('Ctrl Pts',(80.0009199313708,-6.94401261097418,136.178987714753));
#75443=CARTESIAN_POINT('Ctrl Pts',(80.0722020881108,-6.94651895042286,136.17513135907));
#75444=CARTESIAN_POINT('Ctrl Pts',(80.1434631873879,-6.94902454947377,136.171276142592));
#75445=CARTESIAN_POINT('Ctrl Pts',(80.2146163836262,-6.95524470413217,136.167420926115));
#75446=CARTESIAN_POINT('Ctrl Pts',(80.2852479330856,-6.96514590715442,136.163565709638));
#75447=CARTESIAN_POINT('Ctrl Pts',(80.3558822440273,-6.9750474972841,136.159710342433));
#75448=CARTESIAN_POINT('Ctrl Pts',(80.4259943869255,-6.98863035188814,136.155854975229));
#75449=CARTESIAN_POINT('Ctrl Pts',(80.4951781764373,-7.00580940327154,136.151999608024));
#75450=CARTESIAN_POINT('Ctrl Pts',(80.5644343825113,-7.02300643643724,136.148140205301));
#75451=CARTESIAN_POINT('Ctrl Pts',(80.6327598229708,-7.04380706333403,136.144280802578));
#75452=CARTESIAN_POINT('Ctrl Pts',(80.6997617894774,-7.06807582951935,136.140421399856));
#75453=CARTESIAN_POINT('Ctrl Pts',(80.7668016930238,-7.09235833687073,136.136559811909));
#75454=CARTESIAN_POINT('Ctrl Pts',(80.8325161831507,-7.12011270351405,136.132698223962));
#75455=CARTESIAN_POINT('Ctrl Pts',(80.8965334728951,-7.1511556867928,136.128836636015));
#75456=CARTESIAN_POINT('Ctrl Pts',(80.9606627631826,-7.18225298088349,136.124968292081));
#75457=CARTESIAN_POINT('Ctrl Pts',(81.0230884991664,-7.21665014422836,136.121099948148));
#75458=CARTESIAN_POINT('Ctrl Pts',(81.0834650030631,-7.25411880426027,136.117231604214));
#75459=CARTESIAN_POINT('Ctrl Pts',(81.1193148335923,-7.27636661633304,136.114934692908));
#75460=CARTESIAN_POINT('Ctrl Pts',(81.1544427439922,-7.29969650476408,136.112637781602));
#75461=CARTESIAN_POINT('Ctrl Pts',(81.1887818971918,-7.32405394973193,136.110340870295));
#75462=CARTESIAN_POINT('Ctrl Pts',(81.2101480388384,-7.3392093793463,136.108911710641));
#75463=CARTESIAN_POINT('Ctrl Pts',(81.231239727959,-7.3547843918115,136.107482550986));
#75464=CARTESIAN_POINT('Ctrl Pts',(81.2520391107129,-7.37076839346111,136.106053391332));
#75465=CARTESIAN_POINT('Ctrl Pts',(81.2520391107129,-7.37076839346113,136.806140361831));
#75466=CARTESIAN_POINT('Ctrl Pts',(81.3085695514287,-7.41421115656367,136.802278511048));
#75467=CARTESIAN_POINT('Ctrl Pts',(81.3627835844241,-7.46055901156867,136.798416660265));
#75468=CARTESIAN_POINT('Ctrl Pts',(81.414383045544,-7.50952418235728,136.794554809483));
#75469=CARTESIAN_POINT('Ctrl Pts',(81.4660713106751,-7.55857362347511,136.790686312355));
#75470=CARTESIAN_POINT('Ctrl Pts',(81.5151356879525,-7.61024901931506,136.786817815227));
#75471=CARTESIAN_POINT('Ctrl Pts',(81.5613166927242,-7.66422765879788,136.782949318099));
#75472=CARTESIAN_POINT('Ctrl Pts',(81.584435026541,-7.69124950929039,136.781012738148));
#75473=CARTESIAN_POINT('Ctrl Pts',(81.6068314370808,-7.71884807176579,136.779076158196));
#75474=CARTESIAN_POINT('Ctrl Pts',(81.6284774886262,-7.74698019507359,136.777139578245));
#75475=CARTESIAN_POINT('Ctrl Pts',(81.6717240205759,-7.80318521550851,136.773270495398));
#75476=CARTESIAN_POINT('Ctrl Pts',(81.7121420629601,-7.86174185461321,136.769401412551));
#75477=CARTESIAN_POINT('Ctrl Pts',(81.74946647925,-7.92233372490335,136.765532329704));
#75478=CARTESIAN_POINT('Ctrl Pts',(81.7867352840211,-7.98283531632865,136.761669011597));
#75479=CARTESIAN_POINT('Ctrl Pts',(81.8209193594215,-8.04536570948455,136.757805693491));
#75480=CARTESIAN_POINT('Ctrl Pts',(81.8517948922016,-8.1095769321744,136.753942375384));
#75481=CARTESIAN_POINT('Ctrl Pts',(81.8826342079938,-8.17371283512477,136.750083588949));
#75482=CARTESIAN_POINT('Ctrl Pts',(81.9101724804935,-8.23952521564348,136.746224802513));
#75483=CARTESIAN_POINT('Ctrl Pts',(81.9342310595732,-8.30664022997986,136.742366016077));
#75484=CARTESIAN_POINT('Ctrl Pts',(81.9582744835122,-8.37371296677855,136.738509660393));
#75485=CARTESIAN_POINT('Ctrl Pts',(81.9788423992928,-8.4420862532001,136.73465330471));
#75486=CARTESIAN_POINT('Ctrl Pts',(81.9958042626971,-8.51136628493326,136.730796949027));
#75487=CARTESIAN_POINT('Ctrl Pts',(82.0127611153972,-8.58062585065134,136.726941732549));
#75488=CARTESIAN_POINT('Ctrl Pts',(82.0261139151062,-8.65079115831113,136.723086516072));
#75489=CARTESIAN_POINT('Ctrl Pts',(82.0357824558691,-8.72145493205695,136.719231299595));
#75490=CARTESIAN_POINT('Ctrl Pts',(82.0454513746432,-8.79212146854498,136.71537593239));
#75491=CARTESIAN_POINT('Ctrl Pts',(82.0514356848208,-8.86328602821354,136.711520565186));
#75492=CARTESIAN_POINT('Ctrl Pts',(82.0537068542763,-8.93453459540696,136.707665197981));
#75493=CARTESIAN_POINT('Ctrl Pts',(82.0559804010269,-9.00585774042168,136.703805795258));
#75494=CARTESIAN_POINT('Ctrl Pts',(82.0545330329304,-9.07726458196395,136.699946392535));
#75495=CARTESIAN_POINT('Ctrl Pts',(82.0493883707933,-9.14834037938871,136.696086989812));
#75496=CARTESIAN_POINT('Ctrl Pts',(82.0442407957081,-9.2194564204883,136.692225401865));
#75497=CARTESIAN_POINT('Ctrl Pts',(82.0353918194841,-9.29024056207635,136.688363813918));
#75498=CARTESIAN_POINT('Ctrl Pts',(82.022916738459,-9.36028520891424,136.684502225971));
#75499=CARTESIAN_POINT('Ctrl Pts',(82.0104198318325,-9.43045240137242,136.680633882038));
#75500=CARTESIAN_POINT('Ctrl Pts',(81.9942842644375,-9.49987704270607,136.676765538104));
#75501=CARTESIAN_POINT('Ctrl Pts',(81.9746358599068,-9.56816439810169,136.672897194171));
#75502=CARTESIAN_POINT('Ctrl Pts',(81.9629692027315,-9.60871146458532,136.670600282865));
#75503=CARTESIAN_POINT('Ctrl Pts',(81.9500649911238,-9.64885788541115,136.668303371559));
#75504=CARTESIAN_POINT('Ctrl Pts',(81.9359575268557,-9.68852452150279,136.666006460253));
#75505=CARTESIAN_POINT('Ctrl Pts',(81.9121938979014,-9.75534186046859,136.662137377406));
#75506=CARTESIAN_POINT('Ctrl Pts',(81.8849204792404,-9.82105836347765,136.658268294559));
#75507=CARTESIAN_POINT('Ctrl Pts',(81.8542592736282,-9.8852796782169,136.654399211712));
#75508=CARTESIAN_POINT('Ctrl Pts',(81.8236437516832,-9.94940530640005,136.650535893606));
#75509=CARTESIAN_POINT('Ctrl Pts',(81.7896506697926,-10.0120397335354,136.6466725755));
#75510=CARTESIAN_POINT('Ctrl Pts',(81.7524509790069,-10.0728061934375,136.642809257393));
#75511=CARTESIAN_POINT('Ctrl Pts',(81.7152949234441,-10.1335013743055,136.638950470957));
#75512=CARTESIAN_POINT('Ctrl Pts',(81.6749399827043,-10.1923325279531,136.635091684522));
#75513=CARTESIAN_POINT('Ctrl Pts',(81.631603338975,-10.2489467990054,136.631232898086));
#75514=CARTESIAN_POINT('Ctrl Pts',(81.5882939941534,-10.3055254072183,136.627376542403));
#75515=CARTESIAN_POINT('Ctrl Pts',(81.5420069673467,-10.3598895185864,136.623520186719));
#75516=CARTESIAN_POINT('Ctrl Pts',(81.4930023019683,-10.4117158668859,136.619663831036));
#75517=CARTESIAN_POINT('Ctrl Pts',(81.4440121130588,-10.4635269051631,136.615808614559));
#75518=CARTESIAN_POINT('Ctrl Pts',(81.3923062129689,-10.5128013159132,136.611953398082));
#75519=CARTESIAN_POINT('Ctrl Pts',(81.3381832654853,-10.5592508170513,136.608098181605));
#75520=CARTESIAN_POINT('Ctrl Pts',(81.2840582019563,-10.605702134226,136.6042428144));
#75521=CARTESIAN_POINT('Ctrl Pts',(81.2275162734896,-10.6493280078128,136.600387447195));
#75522=CARTESIAN_POINT('Ctrl Pts',(81.1688898330688,-10.689879913085,136.596532079991));
#75523=CARTESIAN_POINT('Ctrl Pts',(81.1102020267516,-10.7304742651441,136.592672677268));
#75524=CARTESIAN_POINT('Ctrl Pts',(81.0494257532268,-10.7679879489103,136.588813274545));
#75525=CARTESIAN_POINT('Ctrl Pts',(80.9869222612899,-10.8022158618408,136.584953871822));
#75526=CARTESIAN_POINT('Ctrl Pts',(80.9243833793849,-10.8364631548843,136.581092283876));
#75527=CARTESIAN_POINT('Ctrl Pts',(80.8601157701031,-10.8674207626341,136.577230695929));
#75528=CARTESIAN_POINT('Ctrl Pts',(80.7945027069387,-10.894930872398,136.573369107982));
#75529=CARTESIAN_POINT('Ctrl Pts',(80.7287748513685,-10.922489112085,136.569500764048));
#75530=CARTESIAN_POINT('Ctrl Pts',(80.6616972995672,-10.9465876473852,136.565632420115));
#75531=CARTESIAN_POINT('Ctrl Pts',(80.5936699255709,-10.9671180905001,136.561764076181));
#75532=CARTESIAN_POINT('Ctrl Pts',(80.5532772285473,-10.9793084768076,136.559467164875));
#75533=CARTESIAN_POINT('Ctrl Pts',(80.5125499020237,-10.9902418503799,136.557170253568));
#75534=CARTESIAN_POINT('Ctrl Pts',(80.4715730379621,-10.9999041057929,136.554873342262));
#75535=CARTESIAN_POINT('Ctrl Pts',(80.4025486566509,-11.0161799047645,136.551004259415));
#75536=CARTESIAN_POINT('Ctrl Pts',(80.3325454831752,-11.028909941549,136.547135176568));
#75537=CARTESIAN_POINT('Ctrl Pts',(80.261960997851,-11.037982825763,136.543266093721));
#75538=CARTESIAN_POINT('Ctrl Pts',(80.1914816798898,-11.047042191832,136.539402775615));
#75539=CARTESIAN_POINT('Ctrl Pts',(80.1204232472095,-11.052455159967,136.535539457508));
#75540=CARTESIAN_POINT('Ctrl Pts',(80.0491949540307,-11.0541610012358,136.531676139402));
#75541=CARTESIAN_POINT('Ctrl Pts',(79.9780502116125,-11.0558648415534,136.527817352966));
#75542=CARTESIAN_POINT('Ctrl Pts',(79.9067364877533,-11.0538701809413,136.52395856653));
#75543=CARTESIAN_POINT('Ctrl Pts',(79.8356680232695,-11.0481680995279,136.520099780094));
#75544=CARTESIAN_POINT('Ctrl Pts',(79.7646443267072,-11.0424696100077,136.516243424411));
#75545=CARTESIAN_POINT('Ctrl Pts',(79.6938660660862,-11.0330683718492,136.512387068728));
#75546=CARTESIAN_POINT('Ctrl Pts',(79.6237458704838,-11.0200075228875,136.508530713045));
#75547=CARTESIAN_POINT('Ctrl Pts',(79.5536463890894,-11.0069505322314,136.504675496567));
#75548=CARTESIAN_POINT('Ctrl Pts',(79.4842050640868,-10.9902361659327,136.50082028009));
#75549=CARTESIAN_POINT('Ctrl Pts',(79.4158260801514,-10.9699589827884,136.496965063613));
#75550=CARTESIAN_POINT('Ctrl Pts',(79.3474444228022,-10.9496810068669,136.493109696408));
#75551=CARTESIAN_POINT('Ctrl Pts',(79.2801256540917,-10.9258400777689,136.489254329204));
#75552=CARTESIAN_POINT('Ctrl Pts',(79.214258829581,-10.8985806213086,136.485398961999));
#75553=CARTESIAN_POINT('Ctrl Pts',(79.1483230604661,-10.8712926316308,136.481539559276));
#75554=CARTESIAN_POINT('Ctrl Pts',(79.0838427191728,-10.8405791577151,136.477680156553));
#75555=CARTESIAN_POINT('Ctrl Pts',(79.021186053369,-10.8066324530409,136.473820753831));
#75556=CARTESIAN_POINT('Ctrl Pts',(78.9584939108687,-10.7726665274758,136.469959165884));
#75557=CARTESIAN_POINT('Ctrl Pts',(78.8976279140911,-10.7354639802963,136.466097577937));
#75558=CARTESIAN_POINT('Ctrl Pts',(78.838928526699,-10.6952612177439,136.46223598999));
#75559=CARTESIAN_POINT('Ctrl Pts',(78.7801264426247,-10.6549881190175,136.458367646056));
#75560=CARTESIAN_POINT('Ctrl Pts',(78.7234989219708,-10.6117046202694,136.454499302123));
#75561=CARTESIAN_POINT('Ctrl Pts',(78.6693539087199,-10.5656878814952,136.450630958189));
#75562=CARTESIAN_POINT('Ctrl Pts',(78.6372041580082,-10.5383644662566,136.448334046883));
#75563=CARTESIAN_POINT('Ctrl Pts',(78.605928968819,-10.5100781387365,136.446037135576));
#75564=CARTESIAN_POINT('Ctrl Pts',(78.5755863437915,-10.4808927370025,136.44374022427));
#75565=CARTESIAN_POINT('Ctrl Pts',(78.5252398783671,-10.4324664120564,136.439929038996));
#75566=CARTESIAN_POINT('Ctrl Pts',(78.4772533655966,-10.3813612335529,136.436117853722));
#75567=CARTESIAN_POINT('Ctrl Pts',(78.4319314969758,-10.3278398745042,136.432306668448));
#75568=CARTESIAN_POINT('Ctrl Pts',(78.3866698572087,-10.2743896407247,136.428500547911));
#75569=CARTESIAN_POINT('Ctrl Pts',(78.3440661660638,-10.2185299668056,136.424694427373));
#75570=CARTESIAN_POINT('Ctrl Pts',(78.3043895848264,-10.160561451391,136.420888306836));
#75571=CARTESIAN_POINT('Ctrl Pts',(78.2647515349153,-10.1026492312446,136.417085882556));
#75572=CARTESIAN_POINT('Ctrl Pts',(78.2280352419789,-10.0426326403597,136.413283458277));
#75573=CARTESIAN_POINT('Ctrl Pts',(78.1944694698461,-9.98084507807418,136.409481033997));
#75574=CARTESIAN_POINT('Ctrl Pts',(78.1609242933767,-9.91909542809487,136.405680942852));
#75575=CARTESIAN_POINT('Ctrl Pts',(78.1305260421695,-9.85557740152834,136.401880851706));
#75576=CARTESIAN_POINT('Ctrl Pts',(78.1034589744874,-9.79065144093181,136.398080760561));
#75577=CARTESIAN_POINT('Ctrl Pts',(78.0763869021235,-9.72571347557106,136.394279966781));
#75578=CARTESIAN_POINT('Ctrl Pts',(78.0526474523868,-9.65936751256437,136.390479173001));
#75579=CARTESIAN_POINT('Ctrl Pts',(78.0323772815509,-9.59199527054117,136.386678379222));
#75580=CARTESIAN_POINT('Ctrl Pts',(78.0121062978096,-9.52462032665303,136.382877433017));
#75581=CARTESIAN_POINT('Ctrl Pts',(77.9953050033776,-9.45621950575168,136.379076486812));
#75582=CARTESIAN_POINT('Ctrl Pts',(77.982059819869,-9.38718857409885,136.375275540607));
#75583=CARTESIAN_POINT('Ctrl Pts',(77.9687990309019,-9.31807631029025,136.371470116132));
#75584=CARTESIAN_POINT('Ctrl Pts',(77.9591028023245,-9.24833294891454,136.367664691657));
#75585=CARTESIAN_POINT('Ctrl Pts',(77.9530059961545,-9.17836230184846,136.363859267182));
#75586=CARTESIAN_POINT('Ctrl Pts',(77.9477806053111,-9.11839254583255,136.360597751292));
#75587=CARTESIAN_POINT('Ctrl Pts',(77.9451983804903,-9.05825611876819,136.357336235401));
#75588=CARTESIAN_POINT('Ctrl Pts',(77.9452507823624,-8.99820692503894,136.35407471951));
#75589=CARTESIAN_POINT('Origin',(80.,-9.,141.545925280538));
#75590=CARTESIAN_POINT('',(81.2520391107129,-7.37076839346112,137.506056941207));
#75591=CARTESIAN_POINT('',(81.2520391107129,-7.37076839346111,137.447938222965));
#75592=CARTESIAN_POINT('',(81.2520391107129,-7.37076839346111,141.545925280538));
#75593=CARTESIAN_POINT('',(77.9452500969073,-9.00063106298383,136.9959252805));
#75594=CARTESIAN_POINT('Ctrl Pts',(81.2520391107129,-7.37076839346111,137.447938222965));
#75595=CARTESIAN_POINT('Ctrl Pts',(81.2608674563024,-7.37755283952553,137.447331137763));
#75596=CARTESIAN_POINT('Ctrl Pts',(81.2696380423385,-7.38440703668142,137.446724052561));
#75597=CARTESIAN_POINT('Ctrl Pts',(81.278349723312,-7.39132988235372,137.446116967359));
#75598=CARTESIAN_POINT('Ctrl Pts',(81.3338711151901,-7.43545064718095,137.442247884513));
#75599=CARTESIAN_POINT('Ctrl Pts',(81.3872144048877,-7.48253558718294,137.438378801667));
#75600=CARTESIAN_POINT('Ctrl Pts',(81.4380459985655,-7.53234156953681,137.434509718821));
#75601=CARTESIAN_POINT('Ctrl Pts',(81.4888018557037,-7.58207334346069,137.430646400715));
#75602=CARTESIAN_POINT('Ctrl Pts',(81.5370531010313,-7.63451777501446,137.426783082609));
#75603=CARTESIAN_POINT('Ctrl Pts',(81.5824986302664,-7.68939111566231,137.422919764504));
#75604=CARTESIAN_POINT('Ctrl Pts',(81.627890851913,-7.74420008990238,137.419060978069));
#75605=CARTESIAN_POINT('Ctrl Pts',(81.6704835863641,-7.80143194162259,137.415202191634));
#75606=CARTESIAN_POINT('Ctrl Pts',(81.7100133228627,-7.86076692545724,137.411343405199));
#75607=CARTESIAN_POINT('Ctrl Pts',(81.7495181585258,-7.92006453260271,137.407487049517));
#75608=CARTESIAN_POINT('Ctrl Pts',(81.7859635555627,-7.98146224011746,137.403630693834));
#75609=CARTESIAN_POINT('Ctrl Pts',(81.8191278778122,-8.04460933296025,137.399774338152));
#75610=CARTESIAN_POINT('Ctrl Pts',(81.8522824029886,-8.10773777151931,137.395919121676));
#75611=CARTESIAN_POINT('Ctrl Pts',(81.8821575518824,-8.17261413959968,137.392063905199));
#75612=CARTESIAN_POINT('Ctrl Pts',(81.9085772938749,-8.2388625118909,137.388208688723));
#75613=CARTESIAN_POINT('Ctrl Pts',(81.9349980688003,-8.30511347429516,137.384353321519));
#75614=CARTESIAN_POINT('Ctrl Pts',(81.9579629907074,-8.37273609536695,137.380497954316));
#75615=CARTESIAN_POINT('Ctrl Pts',(81.977344553654,-8.44133545070856,137.376642587112));
#75616=CARTESIAN_POINT('Ctrl Pts',(81.9967464038118,-8.51000661086893,137.37278318439));
#75617=CARTESIAN_POINT('Ctrl Pts',(82.0125572752224,-8.57965607774693,137.368923781668));
#75618=CARTESIAN_POINT('Ctrl Pts',(82.0247001017075,-8.64987564973897,137.365064378946));
#75619=CARTESIAN_POINT('Ctrl Pts',(82.0368498035563,-8.72013498060414,137.361202791));
#75620=CARTESIAN_POINT('Ctrl Pts',(82.0453272683024,-8.79096457660569,137.357341203054));
#75621=CARTESIAN_POINT('Ctrl Pts',(82.0501073036935,-8.86195071227024,137.353479615108));
#75622=CARTESIAN_POINT('Ctrl Pts',(82.0548957019278,-8.93306104072356,137.349611271176));
#75623=CARTESIAN_POINT('Ctrl Pts',(82.0559737483448,-9.00432796975142,137.345742927243));
#75624=CARTESIAN_POINT('Ctrl Pts',(82.0533683880917,-9.07533807328007,137.341874583311));
#75625=CARTESIAN_POINT('Ctrl Pts',(82.0518214001433,-9.11750182942235,137.339577671996));
#75626=CARTESIAN_POINT('Ctrl Pts',(82.0489767704361,-9.15957512116204,137.337280760682));
#75627=CARTESIAN_POINT('Ctrl Pts',(82.0448487092084,-9.2014728739772,137.334983849367));
#75628=CARTESIAN_POINT('Ctrl Pts',(82.0378951055636,-9.27204846639731,137.33111476652));
#75629=CARTESIAN_POINT('Ctrl Pts',(82.0272698405453,-9.34240187340793,137.327245683672));
#75630=CARTESIAN_POINT('Ctrl Pts',(82.0129962433475,-9.41212096133174,137.323376600825));
#75631=CARTESIAN_POINT('Ctrl Pts',(81.9987439130975,-9.48173617129175,137.319513282718));
#75632=CARTESIAN_POINT('Ctrl Pts',(81.9808541372859,-9.55071846613516,137.315649964611));
#75633=CARTESIAN_POINT('Ctrl Pts',(81.9594019894067,-9.618660978573,137.311786646504));
#75634=CARTESIAN_POINT('Ctrl Pts',(81.9379750048887,-9.68652379447008,137.307927860067));
#75635=CARTESIAN_POINT('Ctrl Pts',(81.9129940940926,-9.75334878963518,137.304069073631));
#75636=CARTESIAN_POINT('Ctrl Pts',(81.8845849626281,-9.81874115637112,137.300210287195));
#75637=CARTESIAN_POINT('Ctrl Pts',(81.8561937268333,-9.88409233071111,137.296353931511));
#75638=CARTESIAN_POINT('Ctrl Pts',(81.8243787479481,-9.94801222257079,137.292497575827));
#75639=CARTESIAN_POINT('Ctrl Pts',(81.7893144621876,-10.0101244071432,137.288641220143));
#75640=CARTESIAN_POINT('Ctrl Pts',(81.7542605347681,-10.0722182431544,137.284786003665));
#75641=CARTESIAN_POINT('Ctrl Pts',(81.7159594447803,-10.1325050092476,137.280930787188));
#75642=CARTESIAN_POINT('Ctrl Pts',(81.6746315439693,-10.1906329217869,137.27707557071));
#75643=CARTESIAN_POINT('Ctrl Pts',(81.633302027361,-10.2487631069539,137.273220203505));
#75644=CARTESIAN_POINT('Ctrl Pts',(81.5889457482666,-10.3047338763535,137.2693648363));
#75645=CARTESIAN_POINT('Ctrl Pts',(81.5418253390224,-10.3582239088046,137.265509469094));
#75646=CARTESIAN_POINT('Ctrl Pts',(81.4946556075589,-10.4117699307336,137.261650066371));
#75647=CARTESIAN_POINT('Ctrl Pts',(81.4447162920578,-10.4628296669441,137.257790663648));
#75648=CARTESIAN_POINT('Ctrl Pts',(81.3923085370105,-10.5111169710739,137.253931260924));
#75649=CARTESIAN_POINT('Ctrl Pts',(81.3398711082806,-10.5594316158546,137.250069672977));
#75650=CARTESIAN_POINT('Ctrl Pts',(81.2849628318101,-10.6049703933609,137.246208085029));
#75651=CARTESIAN_POINT('Ctrl Pts',(81.2279176282725,-10.6474877421935,137.242346497082));
#75652=CARTESIAN_POINT('Ctrl Pts',(81.1707726221066,-10.6900794766517,137.238478153148));
#75653=CARTESIAN_POINT('Ctrl Pts',(81.1114836288107,-10.7296389588855,137.234609809214));
#75654=CARTESIAN_POINT('Ctrl Pts',(81.0504125958223,-10.7659645922378,137.23074146528));
#75655=CARTESIAN_POINT('Ctrl Pts',(81.0141503739875,-10.7875337079128,137.228444553978));
#75656=CARTESIAN_POINT('Ctrl Pts',(80.9772603389445,-10.8079635657243,137.226147642677));
#75657=CARTESIAN_POINT('Ctrl Pts',(80.9398216719654,-10.8272199614179,137.223850731375));
#75658=CARTESIAN_POINT('Ctrl Pts',(80.8767572845336,-10.859656821396,137.219981648528));
#75659=CARTESIAN_POINT('Ctrl Pts',(80.8118881255425,-10.8888884882119,137.216112565681));
#75660=CARTESIAN_POINT('Ctrl Pts',(80.7455730954224,-10.914711028297,137.212243482835));
#75661=CARTESIAN_POINT('Ctrl Pts',(80.6793568713899,-10.9404950940853,137.208380164728));
#75662=CARTESIAN_POINT('Ctrl Pts',(80.6116995013939,-10.9628799408364,137.204516846622));
#75663=CARTESIAN_POINT('Ctrl Pts',(80.5429835264878,-10.9817079634656,137.200653528516));
#75664=CARTESIAN_POINT('Ctrl Pts',(80.4743481553937,-11.0005139008315,137.19679474208));
#75665=CARTESIAN_POINT('Ctrl Pts',(80.4046571121525,-11.0157711736357,137.192935955644));
#75666=CARTESIAN_POINT('Ctrl Pts',(80.3343102680188,-11.0273712553938,137.189077169208));
#75667=CARTESIAN_POINT('Ctrl Pts',(80.2640077372386,-11.038964029951,137.185220813525));
#75668=CARTESIAN_POINT('Ctrl Pts',(80.1930507033399,-11.0469041052396,137.181364457842));
#75669=CARTESIAN_POINT('Ctrl Pts',(80.1218500240242,-11.0511338654864,137.177508102159));
#75670=CARTESIAN_POINT('Ctrl Pts',(80.0506703781022,-11.0553623762197,137.173652885682));
#75671=CARTESIAN_POINT('Ctrl Pts',(79.9792477143182,-11.055882719111,137.169797669205));
#75672=CARTESIAN_POINT('Ctrl Pts',(79.9079970921908,-11.052689218429,137.165942452728));
#75673=CARTESIAN_POINT('Ctrl Pts',(79.8367436843772,-11.0494955928907,137.162087085523));
#75674=CARTESIAN_POINT('Ctrl Pts',(79.7656628167716,-11.0425878594553,137.158231718318));
#75675=CARTESIAN_POINT('Ctrl Pts',(79.6951668885374,-11.0320123859504,137.154376351114));
#75676=CARTESIAN_POINT('Ctrl Pts',(79.6245971702895,-11.0214258428086,137.150516948391));
#75677=CARTESIAN_POINT('Ctrl Pts',(79.5546140950367,-11.0071639680623,137.146657545668));
#75678=CARTESIAN_POINT('Ctrl Pts',(79.4856213986487,-10.9893245630042,137.142798142946));
#75679=CARTESIAN_POINT('Ctrl Pts',(79.4165896380539,-10.9714750571348,137.138936554999));
#75680=CARTESIAN_POINT('Ctrl Pts',(79.3485498361865,-10.9500441345683,137.135074967052));
#75681=CARTESIAN_POINT('Ctrl Pts',(79.2818894093021,-10.9251791454375,137.131213379105));
#75682=CARTESIAN_POINT('Ctrl Pts',(79.2151123576116,-10.900270654117,137.127345035172));
#75683=CARTESIAN_POINT('Ctrl Pts',(79.149719944888,-10.8719162943588,137.123476691239));
#75684=CARTESIAN_POINT('Ctrl Pts',(79.0860778523182,-10.8403108081182,137.119608347305));
#75685=CARTESIAN_POINT('Ctrl Pts',(79.048289009199,-10.8215443799097,137.117311435998));
#75686=CARTESIAN_POINT('Ctrl Pts',(79.0111167807689,-10.801632594008,137.115014524691));
#75687=CARTESIAN_POINT('Ctrl Pts',(78.9746328495178,-10.780623421505,137.112717613384));
#75688=CARTESIAN_POINT('Ctrl Pts',(78.9131766878655,-10.7452340580989,137.108848530537));
#75689=CARTESIAN_POINT('Ctrl Pts',(78.853434442433,-10.7065900127146,137.10497944769));
#75690=CARTESIAN_POINT('Ctrl Pts',(78.7957721050871,-10.664882199921,137.101110364844));
#75691=CARTESIAN_POINT('Ctrl Pts',(78.7381956817481,-10.6232365296883,137.097247046737));
#75692=CARTESIAN_POINT('Ctrl Pts',(78.6826934055514,-10.5785364355522,137.093383728631));
#75693=CARTESIAN_POINT('Ctrl Pts',(78.629605168481,-10.5310178210086,137.089520410524));
#75694=CARTESIAN_POINT('Ctrl Pts',(78.5765792038922,-10.4835549457817,137.085661624089));
#75695=CARTESIAN_POINT('Ctrl Pts',(78.5259620139863,-10.4332804396436,137.081802837653));
#75696=CARTESIAN_POINT('Ctrl Pts',(78.4780616577515,-10.3804713850326,137.077944051217));
#75697=CARTESIAN_POINT('Ctrl Pts',(78.4301914752288,-10.3276955962538,137.074087695534));
#75698=CARTESIAN_POINT('Ctrl Pts',(78.3850350565736,-10.2723887855567,137.070231339851));
#75699=CARTESIAN_POINT('Ctrl Pts',(78.3428636478343,-10.2148648784252,137.066374984168));
#75700=CARTESIAN_POINT('Ctrl Pts',(78.3007046969516,-10.157357964432,137.062519767691));
#75701=CARTESIAN_POINT('Ctrl Pts',(78.2615292924248,-10.0976356458329,137.058664551214));
#75702=CARTESIAN_POINT('Ctrl Pts',(78.2255673227381,-10.0360435494539,137.054809334737));
#75703=CARTESIAN_POINT('Ctrl Pts',(78.1896039470459,-9.97444904500807,137.050953967532));
#75704=CARTESIAN_POINT('Ctrl Pts',(78.1568544986654,-9.91098503826771,137.047098600327));
#75705=CARTESIAN_POINT('Ctrl Pts',(78.1275036996413,-9.84602314840838,137.043243233123));
#75706=CARTESIAN_POINT('Ctrl Pts',(78.0981221783341,-9.78099326116471,137.0393838304));
#75707=CARTESIAN_POINT('Ctrl Pts',(78.072146608295,-9.7144628045736,137.035524427677));
#75708=CARTESIAN_POINT('Ctrl Pts',(78.0497138018131,-9.64682401599008,137.031665024955));
#75709=CARTESIAN_POINT('Ctrl Pts',(78.0272682936999,-9.57914692979317,137.027803437008));
#75710=CARTESIAN_POINT('Ctrl Pts',(78.0083696711111,-9.5103607309998,137.023941849061));
#75711=CARTESIAN_POINT('Ctrl Pts',(77.993104267279,-9.44087082063364,137.020080261114));
#75712=CARTESIAN_POINT('Ctrl Pts',(77.9778121560757,-9.37125933517854,137.016211917181));
#75713=CARTESIAN_POINT('Ctrl Pts',(77.9661660338547,-9.30094215949368,137.012343573247));
#75714=CARTESIAN_POINT('Ctrl Pts',(77.9582006297367,-9.23033213864404,137.008475229314));
#75715=CARTESIAN_POINT('Ctrl Pts',(77.953471001994,-9.18840594022715,137.006178318007));
#75716=CARTESIAN_POINT('Ctrl Pts',(77.9500380668079,-9.14637656073434,137.003881406699));
#75717=CARTESIAN_POINT('Ctrl Pts',(77.9479004012492,-9.10433024157265,137.001584495392));
#75718=CARTESIAN_POINT('Ctrl Pts',(77.9461447814819,-9.06979848389885,136.999698090441));
#75719=CARTESIAN_POINT('Ctrl Pts',(77.9452607206379,-9.03522204066764,136.997811685489));
#75720=CARTESIAN_POINT('Ctrl Pts',(77.9452500969075,-9.00063106367537,136.995925280538));
#75721=CARTESIAN_POINT('Ctrl Pts',(77.9452500969073,-9.00063106298383,136.9959252805));
#75722=CARTESIAN_POINT('Ctrl Pts',(77.9452284795406,-8.93024461476221,136.992086783991));
#75723=CARTESIAN_POINT('Ctrl Pts',(77.9488278088239,-8.85971198196666,136.988248287481));
#75724=CARTESIAN_POINT('Ctrl Pts',(77.956066989778,-8.78944024072726,136.984409790972));
#75725=CARTESIAN_POINT('Ctrl Pts',(77.9634503271985,-8.71776915252224,136.980494857073));
#75726=CARTESIAN_POINT('Ctrl Pts',(77.9746201460017,-8.6463699740825,136.976579923174));
#75727=CARTESIAN_POINT('Ctrl Pts',(77.9895405666956,-8.57567650367051,136.972664989275));
#75728=CARTESIAN_POINT('Ctrl Pts',(78.0041321582484,-8.50654103712668,136.968836336077));
#75729=CARTESIAN_POINT('Ctrl Pts',(78.0223106191684,-8.43808100216141,136.965007682879));
#75730=CARTESIAN_POINT('Ctrl Pts',(78.0439901438109,-8.37069641269804,136.961179029681));
#75731=CARTESIAN_POINT('Ctrl Pts',(78.0656575011448,-8.30334964182633,136.957352525257));
#75732=CARTESIAN_POINT('Ctrl Pts',(78.0908218742364,-8.23707758891418,136.953526020833));
#75733=CARTESIAN_POINT('Ctrl Pts',(78.1193471946889,-8.17226659583193,136.949699516409));
#75734=CARTESIAN_POINT('Ctrl Pts',(78.1478664215464,-8.1074694477107,136.945873829405));
#75735=CARTESIAN_POINT('Ctrl Pts',(78.1797449711963,-8.04413319186299,136.942048142401));
#75736=CARTESIAN_POINT('Ctrl Pts',(78.2147987712684,-7.98262389676421,136.938222455397));
#75737=CARTESIAN_POINT('Ctrl Pts',(78.2512749609404,-7.91861871872357,136.934241532231));
#75738=CARTESIAN_POINT('Ctrl Pts',(78.2911893552543,-7.85659246133984,136.930260609065));
#75739=CARTESIAN_POINT('Ctrl Pts',(78.3342831480842,-7.79692688013413,136.926279685898));
#75740=CARTESIAN_POINT('Ctrl Pts',(78.3757481853334,-7.73951639512645,136.922449224095));
#75741=CARTESIAN_POINT('Ctrl Pts',(78.4201562185497,-7.68429169388733,136.918618762292));
#75742=CARTESIAN_POINT('Ctrl Pts',(78.4672353624941,-7.63155923456245,136.914788300489));
#75743=CARTESIAN_POINT('Ctrl Pts',(78.51434688584,-7.57879050768187,136.910955204227));
#75744=CARTESIAN_POINT('Ctrl Pts',(78.5641328247559,-7.528517780551,136.907122107966));
#75745=CARTESIAN_POINT('Ctrl Pts',(78.6162853882318,-7.48100973153902,136.903289011704));
#75746=CARTESIAN_POINT('Ctrl Pts',(78.6685215402373,-7.43342553808277,136.899449771873));
#75747=CARTESIAN_POINT('Ctrl Pts',(78.7231314966095,-7.38861516648557,136.895610532042));
#75748=CARTESIAN_POINT('Ctrl Pts',(78.7797764230507,-7.34680552119327,136.891771292211));
#75749=CARTESIAN_POINT('Ctrl Pts',(78.7862678537047,-7.34201419335271,136.891331320608));
#75750=CARTESIAN_POINT('Ctrl Pts',(78.7927859814812,-7.33726222463984,136.890891349004));
#75751=CARTESIAN_POINT('Ctrl Pts',(78.7993302756117,-7.33254991815727,136.8904513774));
#75752=CARTESIAN_POINT('Ctrl Pts',(78.8568803901062,-7.29111018879981,136.886582294554));
#75753=CARTESIAN_POINT('Ctrl Pts',(78.9166911084275,-7.25257220614516,136.882713211707));
#75754=CARTESIAN_POINT('Ctrl Pts',(78.9784377823447,-7.21719092498409,136.87884412886));
#75755=CARTESIAN_POINT('Ctrl Pts',(79.0400924567971,-7.18186236016741,136.874980810753));
#75756=CARTESIAN_POINT('Ctrl Pts',(79.1036769431805,-7.14968140041849,136.871117492647));
#75757=CARTESIAN_POINT('Ctrl Pts',(79.1688363368496,-7.12086069500995,136.867254174541));
#75758=CARTESIAN_POINT('Ctrl Pts',(79.2339192985751,-7.09207379627775,136.863395388105));
#75759=CARTESIAN_POINT('Ctrl Pts',(79.3005730559836,-7.06663951812903,136.859536601669));
#75760=CARTESIAN_POINT('Ctrl Pts',(79.3684182802396,-7.04472454785405,136.855677815233));
#75761=CARTESIAN_POINT('Ctrl Pts',(79.4362207669793,-7.02282338240339,136.85182145955));
#75762=CARTESIAN_POINT('Ctrl Pts',(79.5052127703408,-7.00443727548517,136.847965103867));
#75763=CARTESIAN_POINT('Ctrl Pts',(79.574996538769,-6.98968419882803,136.844108748183));
#75764=CARTESIAN_POINT('Ctrl Pts',(79.6447596923733,-6.97493548037747,136.840253531706));
#75765=CARTESIAN_POINT('Ctrl Pts',(79.715313671678,-6.96381776194594,136.836398315229));
#75766=CARTESIAN_POINT('Ctrl Pts',(79.7862488590475,-6.95639827455506,136.832543098752));
#75767=CARTESIAN_POINT('Ctrl Pts',(79.8571868197706,-6.94897849708443,136.828687731547));
#75768=CARTESIAN_POINT('Ctrl Pts',(79.928505534772,-6.94525728606247,136.824832364343));
#75769=CARTESIAN_POINT('Ctrl Pts',(79.9997902910996,-6.9452500107015,136.820976997138));
#75770=CARTESIAN_POINT('Ctrl Pts',(80.0711496631286,-6.94524272772522,136.817117594415));
#75771=CARTESIAN_POINT('Ctrl Pts',(80.1424745187488,-6.94895714073665,136.813258191692));
#75772=CARTESIAN_POINT('Ctrl Pts',(80.2133510766837,-6.95635646929855,136.80939878897));
#75773=CARTESIAN_POINT('Ctrl Pts',(80.2842677654826,-6.96375998741841,136.805537201023));
#75774=CARTESIAN_POINT('Ctrl Pts',(80.3547351711984,-6.97485249894931,136.801675613076));
#75775=CARTESIAN_POINT('Ctrl Pts',(80.424348295495,-6.98954580091699,136.797814025129));
#75776=CARTESIAN_POINT('Ctrl Pts',(80.4940832104476,-7.00426480934311,136.793945681196));
#75777=CARTESIAN_POINT('Ctrl Pts',(80.5629603903894,-7.02259706077393,136.790077337262));
#75778=CARTESIAN_POINT('Ctrl Pts',(80.6305892955939,-7.04440425885554,136.786208993329));
#75779=CARTESIAN_POINT('Ctrl Pts',(80.6707453933162,-7.05735274552062,136.783912082022));
#75780=CARTESIAN_POINT('Ctrl Pts',(80.7104617445907,-7.07152543845114,136.781615170715));
#75781=CARTESIAN_POINT('Ctrl Pts',(80.7496603396343,-7.08688553983841,136.779318259409));
#75782=CARTESIAN_POINT('Ctrl Pts',(80.8156837929553,-7.11275705221844,136.775449497882));
#75783=CARTESIAN_POINT('Ctrl Pts',(80.8804957013765,-7.14210104542521,136.771580736354));
#75784=CARTESIAN_POINT('Ctrl Pts',(80.9437058827517,-7.17478308977812,136.767711974827));
#75785=CARTESIAN_POINT('Ctrl Pts',(81.0068160594631,-7.20741342795354,136.763849334057));
#75786=CARTESIAN_POINT('Ctrl Pts',(81.0683291135876,-7.24337110879749,136.759986693287));
#75787=CARTESIAN_POINT('Ctrl Pts',(81.1278740897058,-7.28247340624075,136.756124052517));
#75788=CARTESIAN_POINT('Ctrl Pts',(81.1703036669818,-7.31033627661527,136.753371675647));
#75789=CARTESIAN_POINT('Ctrl Pts',(81.2117343093368,-7.33979478144065,136.750619298776));
#75790=CARTESIAN_POINT('Ctrl Pts',(81.2520391107129,-7.37076839346111,136.747866921905));
#75791=CARTESIAN_POINT('',(77.9452500020166,-8.99990896698627,137.054074719424));
#75792=CARTESIAN_POINT('Ctrl Pts',(77.9452500020166,-8.99990896698627,137.054074719424));
#75793=CARTESIAN_POINT('Ctrl Pts',(77.9452533307477,-8.92477457357937,137.050023196181));
#75794=CARTESIAN_POINT('Ctrl Pts',(77.9493820167298,-8.84972529838846,137.045971672937));
#75795=CARTESIAN_POINT('Ctrl Pts',(77.9575824977975,-8.77521497114594,137.041920149694));
#75796=CARTESIAN_POINT('Ctrl Pts',(77.9658071971075,-8.70048459472072,137.037856661204));
#75797=CARTESIAN_POINT('Ctrl Pts',(77.978127678062,-8.62629675433766,137.033793172715));
#75798=CARTESIAN_POINT('Ctrl Pts',(77.9944388833354,-8.55309713603182,137.029729684225));
#75799=CARTESIAN_POINT('Ctrl Pts',(78.0107756928437,-8.47978261387955,137.025659817145));
#75800=CARTESIAN_POINT('Ctrl Pts',(78.0311156065384,-8.40745979942027,137.021589950064));
#75801=CARTESIAN_POINT('Ctrl Pts',(78.0553039258151,-8.33655841135058,137.017520082983));
#75802=CARTESIAN_POINT('Ctrl Pts',(78.0795588774132,-8.26546170900407,137.013439004511));
#75803=CARTESIAN_POINT('Ctrl Pts',(78.1076832711748,-8.19579463867159,137.00935792604));
#75804=CARTESIAN_POINT('Ctrl Pts',(78.1394743984723,-8.12796671591055,137.005276847569));
#75805=CARTESIAN_POINT('Ctrl Pts',(78.1547192877522,-8.09544100007468,137.003319836455));
#75806=CARTESIAN_POINT('Ctrl Pts',(78.1708066784999,-8.06333781496755,137.001362825341));
#75807=CARTESIAN_POINT('Ctrl Pts',(78.1877106415427,-8.03170002389624,136.999405814228));
#75808=CARTESIAN_POINT('Ctrl Pts',(78.2211303973098,-7.96915094898812,136.995536731381));
#75809=CARTESIAN_POINT('Ctrl Pts',(78.2578576247281,-7.90821156189568,136.991667648534));
#75810=CARTESIAN_POINT('Ctrl Pts',(78.2977131288887,-7.84925373303147,136.987798565687));
#75811=CARTESIAN_POINT('Ctrl Pts',(78.3375092503357,-7.79038374839189,136.983935247581));
#75812=CARTESIAN_POINT('Ctrl Pts',(78.3804241267733,-7.733489860678,136.980071929474));
#75813=CARTESIAN_POINT('Ctrl Pts',(78.4262327681652,-7.67891928236645,136.976208611368));
#75814=CARTESIAN_POINT('Ctrl Pts',(78.4719876760385,-7.62441271532224,136.972349824932));
#75815=CARTESIAN_POINT('Ctrl Pts',(78.5206292956542,-7.57222441469258,136.968491038496));
#75816=CARTESIAN_POINT('Ctrl Pts',(78.5718904678376,-7.52267108379792,136.964632252061));
#75817=CARTESIAN_POINT('Ctrl Pts',(78.6231193492412,-7.47314896786815,136.960775896378));
#75818=CARTESIAN_POINT('Ctrl Pts',(78.6769641609443,-7.42625886541624,136.956919540694));
#75819=CARTESIAN_POINT('Ctrl Pts',(78.7331197501868,-7.38228185547259,136.953063185011));
#75820=CARTESIAN_POINT('Ctrl Pts',(78.7892587505059,-7.33831783677804,136.949207968534));
#75821=CARTESIAN_POINT('Ctrl Pts',(78.8477067909087,-7.29726550149995,136.945352752057));
#75822=CARTESIAN_POINT('Ctrl Pts',(78.9081257198297,-7.25936559875358,136.94149753558));
#75823=CARTESIAN_POINT('Ctrl Pts',(78.96854701095,-7.22146421423439,136.937642168375));
#75824=CARTESIAN_POINT('Ctrl Pts',(79.0309389308821,-7.18671576321925,136.933786801171));
#75825=CARTESIAN_POINT('Ctrl Pts',(79.0949359144031,-7.15531667664539,136.929931433966));
#75826=CARTESIAN_POINT('Ctrl Pts',(79.1589998853148,-7.12388472378996,136.926072031243));
#75827=CARTESIAN_POINT('Ctrl Pts',(79.2246718365866,-7.09580934829369,136.922212628521));
#75828=CARTESIAN_POINT('Ctrl Pts',(79.291564073674,-7.07123975030834,136.918353225798));
#75829=CARTESIAN_POINT('Ctrl Pts',(79.3584941856716,-7.04665624082359,136.914491637851));
#75830=CARTESIAN_POINT('Ctrl Pts',(79.4266454946026,-7.02558260394684,136.910630049904));
#75831=CARTESIAN_POINT('Ctrl Pts',(79.4956155457542,-7.00811800429464,136.906768461957));
#75832=CARTESIAN_POINT('Ctrl Pts',(79.5647062624825,-6.99062284969934,136.902900118024));
#75833=CARTESIAN_POINT('Ctrl Pts',(79.6346181046537,-6.97674943327319,136.899031774091));
#75834=CARTESIAN_POINT('Ctrl Pts',(79.704939538399,-6.9665455779635,136.895163430157));
#75835=CARTESIAN_POINT('Ctrl Pts',(79.7466943820948,-6.96048682232018,136.89286651885));
#75836=CARTESIAN_POINT('Ctrl Pts',(79.7885935358446,-6.95572082826681,136.890569607543));
#75837=CARTESIAN_POINT('Ctrl Pts',(79.830550756554,-6.95224891249068,136.888272696236));
#75838=CARTESIAN_POINT('Ctrl Pts',(79.901208363859,-6.94640206998401,136.884404607397));
#75839=CARTESIAN_POINT('Ctrl Pts',(79.9723072994879,-6.94420512848996,136.880536518558));
#75840=CARTESIAN_POINT('Ctrl Pts',(80.0434382677722,-6.94570920281647,136.876668429718));
#75841=CARTESIAN_POINT('Ctrl Pts',(80.1144716684083,-6.94721121406134,136.87280564659));
#75842=CARTESIAN_POINT('Ctrl Pts',(80.1855365333489,-6.95240416047176,136.868942863461));
#75843=CARTESIAN_POINT('Ctrl Pts',(80.256219300306,-6.96128735898099,136.865080080333));
#75844=CARTESIAN_POINT('Ctrl Pts',(80.3268287676249,-6.97016134541117,136.861221302998));
#75845=CARTESIAN_POINT('Ctrl Pts',(80.3970564438626,-6.98271792913604,136.857362525663));
#75846=CARTESIAN_POINT('Ctrl Pts',(80.4664913551475,-6.99890445553626,136.853503748329));
#75847=CARTESIAN_POINT('Ctrl Pts',(80.5375128267714,-7.01546083768106,136.849556799454));
#75848=CARTESIAN_POINT('Ctrl Pts',(80.607704334842,-7.03581507458642,136.845609850579));
#75849=CARTESIAN_POINT('Ctrl Pts',(80.6766354069122,-7.0598551372094,136.841662901704));
#75850=CARTESIAN_POINT('Ctrl Pts',(80.7439678387922,-7.08333766592015,136.837807489939));
#75851=CARTESIAN_POINT('Ctrl Pts',(80.8100972024929,-7.11033669413166,136.833952078174));
#75852=CARTESIAN_POINT('Ctrl Pts',(80.8746382145517,-7.14069756194807,136.830096666409));
#75853=CARTESIAN_POINT('Ctrl Pts',(80.9414777739727,-7.17213969407085,136.826103948979));
#75854=CARTESIAN_POINT('Ctrl Pts',(81.0066131920739,-7.20718744927472,136.822111231549));
#75855=CARTESIAN_POINT('Ctrl Pts',(81.0696421225511,-7.2456159792781,136.81811851412));
#75856=CARTESIAN_POINT('Ctrl Pts',(81.1326710530283,-7.28404450928148,136.81412579669));
#75857=CARTESIAN_POINT('Ctrl Pts',(81.1935930213483,-7.32585348421251,136.81013307926));
#75858=CARTESIAN_POINT('Ctrl Pts',(81.2520391107129,-7.37076839346113,136.806140361831));
#75859=CARTESIAN_POINT('Ctrl Pts',(81.2520391107129,-7.37076839346111,137.506056941207));
#75860=CARTESIAN_POINT('Ctrl Pts',(81.3085836343695,-7.41422197908427,137.50220180446));
#75861=CARTESIAN_POINT('Ctrl Pts',(81.3628760679797,-7.46063245916092,137.498346667712));
#75862=CARTESIAN_POINT('Ctrl Pts',(81.4146004952369,-7.50973056081275,137.494491530965));
#75863=CARTESIAN_POINT('Ctrl Pts',(81.4663309415066,-7.55883437585964,137.490635945607));
#75864=CARTESIAN_POINT('Ctrl Pts',(81.5154924376303,-7.61062609708868,137.486780360249));
#75865=CARTESIAN_POINT('Ctrl Pts',(81.561805417557,-7.66479911616659,137.482924774891));
#75866=CARTESIAN_POINT('Ctrl Pts',(81.6081690741475,-7.71903141253303,137.479064970668));
#75867=CARTESIAN_POINT('Ctrl Pts',(81.6516776792929,-7.77564983589475,137.475205166445));
#75868=CARTESIAN_POINT('Ctrl Pts',(81.6920921389353,-7.8343148985025,137.471345362222));
#75869=CARTESIAN_POINT('Ctrl Pts',(81.7325322819063,-7.89301724266961,137.467483105099));
#75870=CARTESIAN_POINT('Ctrl Pts',(81.769874112489,-7.95376840044712,137.463620847977));
#75871=CARTESIAN_POINT('Ctrl Pts',(81.8039234895922,-8.01620245670292,137.459758590854));
#75872=CARTESIAN_POINT('Ctrl Pts',(81.8380300713486,-8.07874140528959,137.455889844947));
#75873=CARTESIAN_POINT('Ctrl Pts',(81.8688329530289,-8.14296845639921,137.452021099039));
#75874=CARTESIAN_POINT('Ctrl Pts',(81.8961856379346,-8.20849662730306,137.448152353132));
#75875=CARTESIAN_POINT('Ctrl Pts',(81.9061170255109,-8.23228901421703,137.446747664153));
#75876=CARTESIAN_POINT('Ctrl Pts',(81.9155940431147,-8.2562527808878,137.445342975173));
#75877=CARTESIAN_POINT('Ctrl Pts',(81.9246113195382,-8.28036896175498,137.443938286194));
#75878=CARTESIAN_POINT('Ctrl Pts',(81.9494485540355,-8.34679469955542,137.440069203343));
#75879=CARTESIAN_POINT('Ctrl Pts',(81.9708914866249,-8.41463789219201,137.436200120492));
#75880=CARTESIAN_POINT('Ctrl Pts',(81.9887795660641,-8.48351824804187,137.432331037641));
#75881=CARTESIAN_POINT('Ctrl Pts',(82.0066409931575,-8.55229597559809,137.42846771953));
#75882=CARTESIAN_POINT('Ctrl Pts',(82.0209579595018,-8.62210733259121,137.424604401419));
#75883=CARTESIAN_POINT('Ctrl Pts',(82.0316186896447,-8.69255396833502,137.420741083309));
#75884=CARTESIAN_POINT('Ctrl Pts',(82.0422669147554,-8.76291797020327,137.416882296868));
#75885=CARTESIAN_POINT('Ctrl Pts',(82.0492673502678,-8.83391529265563,137.413023510428));
#75886=CARTESIAN_POINT('Ctrl Pts',(82.0525589895964,-8.90513611473707,137.409164723988));
#75887=CARTESIAN_POINT('Ctrl Pts',(82.0558485554335,-8.97631207292382,137.405308368301));
#75888=CARTESIAN_POINT('Ctrl Pts',(82.0554339378344,-9.0477107672997,137.401452012613));
#75889=CARTESIAN_POINT('Ctrl Pts',(82.0513059765539,-9.11891742115505,137.397595656925));
#75890=CARTESIAN_POINT('Ctrl Pts',(82.0471792347145,-9.19010303985237,137.393740440444));
#75891=CARTESIAN_POINT('Ctrl Pts',(82.0393413550608,-9.26109624595062,137.389885223962));
#75892=CARTESIAN_POINT('Ctrl Pts',(82.027835252322,-9.3314841654442,137.38603000748));
#75893=CARTESIAN_POINT('Ctrl Pts',(82.0163286997288,-9.40187483689556,137.382174640271));
#75894=CARTESIAN_POINT('Ctrl Pts',(82.0011537198591,-9.4716596956942,137.378319273062));
#75895=CARTESIAN_POINT('Ctrl Pts',(81.9824046025214,-9.5404345977099,137.374463905853));
#75896=CARTESIAN_POINT('Ctrl Pts',(81.9636358599706,-9.60928148829397,137.370604503126));
#75897=CARTESIAN_POINT('Ctrl Pts',(81.9412856398145,-9.67711584214869,137.366745100399));
#75898=CARTESIAN_POINT('Ctrl Pts',(81.9154982988431,-9.74354813538135,137.362885697672));
#75899=CARTESIAN_POINT('Ctrl Pts',(81.8896963568767,-9.8100180431004,137.35902410972));
#75900=CARTESIAN_POINT('Ctrl Pts',(81.8604536191945,-9.8750838665717,137.355162521769));
#75901=CARTESIAN_POINT('Ctrl Pts',(81.8279617422849,-9.93837808544472,137.351300933817));
#75902=CARTESIAN_POINT('Ctrl Pts',(81.7954130196723,-10.0017830398218,137.347432589879));
#75903=CARTESIAN_POINT('Ctrl Pts',(81.7596040527335,-10.0634097812331,137.343564245942));
#75904=CARTESIAN_POINT('Ctrl Pts',(81.7207710219745,-10.1229179188315,137.339695902004));
#75905=CARTESIAN_POINT('Ctrl Pts',(81.6977130862498,-10.1582521377946,137.337398990737));
#75906=CARTESIAN_POINT('Ctrl Pts',(81.673589784248,-10.1928399972618,137.33510207947));
#75907=CARTESIAN_POINT('Ctrl Pts',(81.6484571427742,-10.2266159182632,137.332805168203));
#75908=CARTESIAN_POINT('Ctrl Pts',(81.6061219104928,-10.2835105133897,137.328936085356));
#75909=CARTESIAN_POINT('Ctrl Pts',(81.5607548249677,-10.3383222428234,137.32506700251));
#75910=CARTESIAN_POINT('Ctrl Pts',(81.5125883019348,-10.3907099594631,137.321197919663));
#75911=CARTESIAN_POINT('Ctrl Pts',(81.4644935446192,-10.4430196210176,137.317334601557));
#75912=CARTESIAN_POINT('Ctrl Pts',(81.4136079552723,-10.4929120841274,137.313471283451));
#75913=CARTESIAN_POINT('Ctrl Pts',(81.3602055766754,-10.5400773849651,137.309607965345));
#75914=CARTESIAN_POINT('Ctrl Pts',(81.3068658390478,-10.5871873609233,137.305749178909));
#75915=CARTESIAN_POINT('Ctrl Pts',(81.2510155385621,-10.6315762088092,137.301890392473));
#75916=CARTESIAN_POINT('Ctrl Pts',(81.192965890586,-10.6729703961512,137.298031606038));
#75917=CARTESIAN_POINT('Ctrl Pts',(81.1349528096313,-10.7143385081907,137.294175250355));
#75918=CARTESIAN_POINT('Ctrl Pts',(81.074743524441,-10.7527154209336,137.290318894672));
#75919=CARTESIAN_POINT('Ctrl Pts',(81.0126815343111,-10.7878684718305,137.286462538989));
#75920=CARTESIAN_POINT('Ctrl Pts',(80.9506378779143,-10.8230111381642,137.282607322512));
#75921=CARTESIAN_POINT('Ctrl Pts',(80.8867430255922,-10.8549315940657,137.278752106035));
#75922=CARTESIAN_POINT('Ctrl Pts',(80.8213671225575,-10.8834419588831,137.274896889558));
#75923=CARTESIAN_POINT('Ctrl Pts',(80.7559886635204,-10.9119534383706,137.271041522354));
#75924=CARTESIAN_POINT('Ctrl Pts',(80.6891294849716,-10.937054369908,137.267186155149));
#75925=CARTESIAN_POINT('Ctrl Pts',(80.6211802626988,-10.9586047696596,137.263330787945));
#75926=CARTESIAN_POINT('Ctrl Pts',(80.5531599161191,-10.9801777268033,137.259471385222));
#75927=CARTESIAN_POINT('Ctrl Pts',(80.4840477121677,-10.9981925861569,137.2556119825));
#75928=CARTESIAN_POINT('Ctrl Pts',(80.4142491990326,-11.012559356541,137.251752579777));
#75929=CARTESIAN_POINT('Ctrl Pts',(80.3444111654309,-11.0269342615035,137.247890991831));
#75930=CARTESIAN_POINT('Ctrl Pts',(80.2738865295666,-11.0376568925161,137.244029403884));
#75931=CARTESIAN_POINT('Ctrl Pts',(80.2030880081496,-11.044688930729,137.240167815937));
#75932=CARTESIAN_POINT('Ctrl Pts',(80.1321656221815,-11.0517332717449,137.236299472004));
#75933=CARTESIAN_POINT('Ctrl Pts',(80.0609688793818,-11.0550741059518,137.232431128071));
#75934=CARTESIAN_POINT('Ctrl Pts',(79.9899118530182,-11.0547252351082,137.228562784137));
#75935=CARTESIAN_POINT('Ctrl Pts',(79.9477202355612,-11.0545180856407,137.226265872829));
#75936=CARTESIAN_POINT('Ctrl Pts',(79.9055778257029,-11.0530110759741,137.22396896152));
#75937=CARTESIAN_POINT('Ctrl Pts',(79.8635701063467,-11.0502157073386,137.221672050211));
#75938=CARTESIAN_POINT('Ctrl Pts',(79.7928092782111,-11.0455069870694,137.217802967365));
#75939=CARTESIAN_POINT('Ctrl Pts',(79.7221539169065,-11.0371214012433,137.213933884519));
#75940=CARTESIAN_POINT('Ctrl Pts',(79.6520166891183,-11.0250691785339,137.210064801673));
#75941=CARTESIAN_POINT('Ctrl Pts',(79.5819839623019,-11.0130349130352,137.206201483567));
#75942=CARTESIAN_POINT('Ctrl Pts',(79.5124683114827,-10.9973449363675,137.202338165462));
#75943=CARTESIAN_POINT('Ctrl Pts',(79.4438787829363,-10.9780613626558,137.198474847356));
#75944=CARTESIAN_POINT('Ctrl Pts',(79.3753697098809,-10.9588004085687,137.194616060921));
#75945=CARTESIAN_POINT('Ctrl Pts',(79.30778506664,-10.9359543612667,137.190757274486));
#75946=CARTESIAN_POINT('Ctrl Pts',(79.2415234539812,-10.9096363244449,137.186898488051));
#75947=CARTESIAN_POINT('Ctrl Pts',(79.1753035812799,-10.8833348660565,137.183042132369));
#75948=CARTESIAN_POINT('Ctrl Pts',(79.1104055360921,-10.853565936213,137.179185776687));
#75949=CARTESIAN_POINT('Ctrl Pts',(79.0472110931796,-10.8204919284468,137.175329421004));
#75950=CARTESIAN_POINT('Ctrl Pts',(78.9840353185384,-10.7874276910737,137.171474204528));
#75951=CARTESIAN_POINT('Ctrl Pts',(78.9225625772248,-10.7510605392452,137.167618988052));
#75952=CARTESIAN_POINT('Ctrl Pts',(78.8631514734681,-10.7115995414297,137.163763771576));
#75953=CARTESIAN_POINT('Ctrl Pts',(78.8037380469151,-10.6721370008073,137.159908404372));
#75954=CARTESIAN_POINT('Ctrl Pts',(78.7463868213841,-10.6295806446556,137.156053037168));
#75955=CARTESIAN_POINT('Ctrl Pts',(78.6914272967846,-10.5841827681488,137.152197669964));
#75956=CARTESIAN_POINT('Ctrl Pts',(78.6364102445497,-10.5387373724448,137.148338267243));
#75957=CARTESIAN_POINT('Ctrl Pts',(78.58379026601,-10.4904448290285,137.144478864521));
#75958=CARTESIAN_POINT('Ctrl Pts',(78.5338629270879,-10.4395970429022,137.140619461799));
#75959=CARTESIAN_POINT('Ctrl Pts',(78.4839073189144,-10.3887204663601,137.136757873853));
#75960=CARTESIAN_POINT('Ctrl Pts',(78.4366477073388,-10.3352861310318,137.132896285907));
#75961=CARTESIAN_POINT('Ctrl Pts',(78.3923401347156,-10.2796199904869,137.129034697961));
#75962=CARTESIAN_POINT('Ctrl Pts',(78.3479550444059,-10.2238564600339,137.125166354028));
#75963=CARTESIAN_POINT('Ctrl Pts',(78.3065325869227,-10.1658537241226,137.121298010096));
#75964=CARTESIAN_POINT('Ctrl Pts',(78.2682857521435,-10.105967145204,137.117429666163));
#75965=CARTESIAN_POINT('Ctrl Pts',(78.2455758822133,-10.0704082178926,137.115132754849));
#75966=CARTESIAN_POINT('Ctrl Pts',(78.2239847570716,-10.034185612918,137.112835843534));
#75967=CARTESIAN_POINT('Ctrl Pts',(78.2035490783993,-9.99737738533625,137.11053893222));
#75968=CARTESIAN_POINT('Ctrl Pts',(78.1674867936405,-9.93242291008696,137.106485635472));
#75969=CARTESIAN_POINT('Ctrl Pts',(78.1348950465757,-9.8654094674081,137.102432338725));
#75970=CARTESIAN_POINT('Ctrl Pts',(78.1060020779535,-9.79672418927981,137.098379041977));
#75971=CARTESIAN_POINT('Ctrl Pts',(78.0771900219366,-9.72823125915408,137.094337096186));
#75972=CARTESIAN_POINT('Ctrl Pts',(78.0520562805304,-9.65807620028567,137.090295150394));
#75973=CARTESIAN_POINT('Ctrl Pts',(78.0307828211536,-9.5866696387545,137.086253204602));
#75974=CARTESIAN_POINT('Ctrl Pts',(78.0095451555341,-9.51538322266288,137.082218059604));
#75975=CARTESIAN_POINT('Ctrl Pts',(77.9921549775743,-9.44284988951571,137.078182914607));
#75976=CARTESIAN_POINT('Ctrl Pts',(77.978745992917,-9.36949939289633,137.074147769609));
#75977=CARTESIAN_POINT('Ctrl Pts',(77.9653646220904,-9.29629995083135,137.070120934399));
#75978=CARTESIAN_POINT('Ctrl Pts',(77.9559481961507,-9.22228710632508,137.066094099189));
#75979=CARTESIAN_POINT('Ctrl Pts',(77.9505800370191,-9.1479032718887,137.062067263979));
#75980=CARTESIAN_POINT('Ctrl Pts',(77.9470284265033,-9.09869042217371,137.059403082473));
#75981=CARTESIAN_POINT('Ctrl Pts',(77.945247813142,-9.04931548698807,137.056738900968));
#75982=CARTESIAN_POINT('Ctrl Pts',(77.9452500020165,-8.99990896768397,137.054074719462));
#75983=CARTESIAN_POINT('Origin',(80.,-9.,141.545925280538));
#75984=CARTESIAN_POINT('',(81.2520391107129,-7.37076839346111,138.206016809128));
#75985=CARTESIAN_POINT('',(81.2520391107129,-7.37076839346111,138.147982307182));
#75986=CARTESIAN_POINT('',(81.2520391107129,-7.37076839346111,141.545925280538));
#75987=CARTESIAN_POINT('',(77.9452508576385,-8.99812264423968,137.695925280507));
#75988=CARTESIAN_POINT('Ctrl Pts',(81.2520391107129,-7.37076839346111,138.147982307182));
#75989=CARTESIAN_POINT('Ctrl Pts',(81.30859831624,-7.41423326187304,138.144121802281));
#75990=CARTESIAN_POINT('Ctrl Pts',(81.3628508305885,-7.46061547005432,138.14026129738));
#75991=CARTESIAN_POINT('Ctrl Pts',(81.4144948396281,-7.50963027702341,138.136400792478));
#75992=CARTESIAN_POINT('Ctrl Pts',(81.4668569716313,-7.55932664723847,138.132486606283));
#75993=CARTESIAN_POINT('Ctrl Pts',(81.5165371353892,-7.61172902392757,138.128572420088));
#75994=CARTESIAN_POINT('Ctrl Pts',(81.5632621184245,-7.66650492629369,138.124658233893));
#75995=CARTESIAN_POINT('Ctrl Pts',(81.6099871014597,-7.72128082865981,138.120744047698));
#75996=CARTESIAN_POINT('Ctrl Pts',(81.6537566440181,-7.77842980912718,138.116829861503));
#75997=CARTESIAN_POINT('Ctrl Pts',(81.6943435741599,-7.83758982488841,138.112915675308));
#75998=CARTESIAN_POINT('Ctrl Pts',(81.7344628184555,-7.89606813592506,138.109046592536));
#75999=CARTESIAN_POINT('Ctrl Pts',(81.7716296199628,-7.9567404259928,138.105177509764));
#76000=CARTESIAN_POINT('Ctrl Pts',(81.8055964784098,-8.01927632859497,138.101308426992));
#76001=CARTESIAN_POINT('Ctrl Pts',(81.8395127279186,-8.08171905579692,138.097445108962));
#76002=CARTESIAN_POINT('Ctrl Pts',(81.8702382682593,-8.14601946047875,138.093581790932));
#76003=CARTESIAN_POINT('Ctrl Pts',(81.897568582308,-8.21181789037196,138.089718472901));
#76004=CARTESIAN_POINT('Ctrl Pts',(81.9248668378963,-8.27753913870203,138.085859686544));
#76005=CARTESIAN_POINT('Ctrl Pts',(81.9487775925488,-8.34475447543659,138.082000900186));
#76006=CARTESIAN_POINT('Ctrl Pts',(81.9691428350753,-8.41308087646445,138.078142113828));
#76007=CARTESIAN_POINT('Ctrl Pts',(81.9894952489868,-8.48136423685131,138.074285758224));
#76008=CARTESIAN_POINT('Ctrl Pts',(82.0063064433988,-8.55075680851853,138.070429402619));
#76009=CARTESIAN_POINT('Ctrl Pts',(82.0194675293368,-8.62085825809528,138.066573047015));
#76010=CARTESIAN_POINT('Ctrl Pts',(82.0326247273551,-8.69093899898543,138.062717830618));
#76011=CARTESIAN_POINT('Ctrl Pts',(82.0421338679957,-8.76172772486692,138.05886261422));
#76012=CARTESIAN_POINT('Ctrl Pts',(82.0479370599022,-8.83281339413957,138.055007397823));
#76013=CARTESIAN_POINT('Ctrl Pts',(82.053740478695,-8.90390184263526,138.051152030699));
#76014=CARTESIAN_POINT('Ctrl Pts',(82.0558376237614,-8.9752867732197,138.047296663575));
#76015=CARTESIAN_POINT('Ctrl Pts',(82.054222568083,-9.04655323058885,138.043441296451));
#76016=CARTESIAN_POINT('Ctrl Pts',(82.052605821882,-9.11789428449572,138.039581893809));
#76017=CARTESIAN_POINT('Ctrl Pts',(82.047269129314,-9.18911613098387,138.035722491168));
#76018=CARTESIAN_POINT('Ctrl Pts',(82.0382586782996,-9.25980593302764,138.031863088526));
#76019=CARTESIAN_POINT('Ctrl Pts',(82.029243125498,-9.33053576018485,138.028001500661));
#76020=CARTESIAN_POINT('Ctrl Pts',(82.0165497598728,-9.40073246494944,138.024139912796));
#76021=CARTESIAN_POINT('Ctrl Pts',(82.0002759786768,-9.46999316125715,138.020278324931));
#76022=CARTESIAN_POINT('Ctrl Pts',(81.9839737259161,-9.5393750316407,138.016409981079));
#76023=CARTESIAN_POINT('Ctrl Pts',(81.9640786868404,-9.60781715746944,138.012541637227));
#76024=CARTESIAN_POINT('Ctrl Pts',(81.9407380100524,-9.67493224759071,138.008673293375));
#76025=CARTESIAN_POINT('Ctrl Pts',(81.9268789832666,-9.71478326991421,138.006376381355));
#76026=CARTESIAN_POINT('Ctrl Pts',(81.9118060744727,-9.75416679838156,138.004079469336));
#76027=CARTESIAN_POINT('Ctrl Pts',(81.8955578473674,-9.79300568080172,138.001782557316));
#76028=CARTESIAN_POINT('Ctrl Pts',(81.868188171565,-9.85842867209067,137.997913474436));
#76029=CARTESIAN_POINT('Ctrl Pts',(81.8373739143581,-9.92256118941954,137.994044391556));
#76030=CARTESIAN_POINT('Ctrl Pts',(81.8032583883211,-9.98501611532485,137.990175308676));
#76031=CARTESIAN_POINT('Ctrl Pts',(81.7691936927123,-10.0473779865129,137.986311990536));
#76032=CARTESIAN_POINT('Ctrl Pts',(81.7318377227877,-10.1080668049176,137.982448672396));
#76033=CARTESIAN_POINT('Ctrl Pts',(81.6913817082797,-10.1667156806167,137.978585354256));
#76034=CARTESIAN_POINT('Ctrl Pts',(81.6509731486556,-10.2252957612152,137.974726567787));
#76035=CARTESIAN_POINT('Ctrl Pts',(81.6074720419677,-10.2818402541869,137.970867781317));
#76036=CARTESIAN_POINT('Ctrl Pts',(81.5611144773083,-10.3360086643576,137.967008994847));
#76037=CARTESIAN_POINT('Ctrl Pts',(81.5147861145119,-10.3901429524059,137.96315263913));
#76038=CARTESIAN_POINT('Ctrl Pts',(81.4656051787558,-10.4419037589918,137.959296283412));
#76039=CARTESIAN_POINT('Ctrl Pts',(81.4138489441355,-10.4909824699395,137.955439927694));
#76040=CARTESIAN_POINT('Ctrl Pts',(81.3621079988221,-10.5400466825475,137.951584711183));
#76041=CARTESIAN_POINT('Ctrl Pts',(81.3077936172875,-10.5864300384086,137.947729494671));
#76042=CARTESIAN_POINT('Ctrl Pts',(81.2512197300677,-10.6298609602016,137.94387427816));
#76043=CARTESIAN_POINT('Ctrl Pts',(81.1946436309757,-10.6732935800156,137.94001891092));
#76044=CARTESIAN_POINT('Ctrl Pts',(81.1358082374835,-10.7137732425222,137.936163543681));
#76045=CARTESIAN_POINT('Ctrl Pts',(81.0750589525922,-10.7510699046444,137.932308176442));
#76046=CARTESIAN_POINT('Ctrl Pts',(81.0142460797654,-10.7884056062014,137.928448773684));
#76047=CARTESIAN_POINT('Ctrl Pts',(80.9515157312946,-10.8225514018019,137.924589370927));
#76048=CARTESIAN_POINT('Ctrl Pts',(80.8872397966611,-10.8533221807664,137.920729968169));
#76049=CARTESIAN_POINT('Ctrl Pts',(80.8229274684877,-10.8841103823881,137.916868380188));
#76050=CARTESIAN_POINT('Ctrl Pts',(80.7570682607569,-10.9115195764983,137.913006792206));
#76051=CARTESIAN_POINT('Ctrl Pts',(80.6900534777516,-10.9354130722776,137.909145204224));
#76052=CARTESIAN_POINT('Ctrl Pts',(80.6229214499872,-10.959348370582,137.905276860257));
#76053=CARTESIAN_POINT('Ctrl Pts',(80.5546302761199,-10.9797555510984,137.901408516289));
#76054=CARTESIAN_POINT('Ctrl Pts',(80.485585142784,-10.996548179135,137.897540172321));
#76055=CARTESIAN_POINT('Ctrl Pts',(80.4445881354143,-11.0065191569884,137.895243261322));
#76056=CARTESIAN_POINT('Ctrl Pts',(80.4033254996451,-11.0152167540812,137.892946350323));
#76057=CARTESIAN_POINT('Ctrl Pts',(80.3618829696563,-11.0226315232322,137.890649439325));
#76058=CARTESIAN_POINT('Ctrl Pts',(80.2920741777511,-11.0351214961376,137.886780356478));
#76059=CARTESIAN_POINT('Ctrl Pts',(80.2214812825332,-11.0440176346564,137.88291127363));
#76060=CARTESIAN_POINT('Ctrl Pts',(80.1505072441012,-11.0492303755247,137.879042190783));
#76061=CARTESIAN_POINT('Ctrl Pts',(80.0796389534447,-11.0544353496693,137.875178872676));
#76062=CARTESIAN_POINT('Ctrl Pts',(80.0083911273402,-11.0559677845549,137.871315554569));
#76063=CARTESIAN_POINT('Ctrl Pts',(79.9371757213841,-11.0537893447275,137.867452236462));
#76064=CARTESIAN_POINT('Ctrl Pts',(79.8660438510692,-11.0516134602092,137.863593450026));
#76065=CARTESIAN_POINT('Ctrl Pts',(79.7949448085641,-11.0457353620015,137.85973466359));
#76066=CARTESIAN_POINT('Ctrl Pts',(79.724292705199,-11.0361687184744,137.855875877153));
#76067=CARTESIAN_POINT('Ctrl Pts',(79.6536851074765,-11.0266081012309,137.852019521469));
#76068=CARTESIAN_POINT('Ctrl Pts',(79.5835243705776,-11.0133636135099,137.848163165785));
#76069=CARTESIAN_POINT('Ctrl Pts',(79.5142201594866,-10.9965008161909,137.844306810101));
#76070=CARTESIAN_POINT('Ctrl Pts',(79.4449364215517,-10.9796430003106,137.840451593623));
#76071=CARTESIAN_POINT('Ctrl Pts',(79.3765091788521,-10.9591691116506,137.836596377145));
#76072=CARTESIAN_POINT('Ctrl Pts',(79.3093368622182,-10.9351955954397,137.832741160667));
#76073=CARTESIAN_POINT('Ctrl Pts',(79.2421619193459,-10.9112211419355,137.828885793462));
#76074=CARTESIAN_POINT('Ctrl Pts',(79.1762424567267,-10.8837469545931,137.825030426256));
#76075=CARTESIAN_POINT('Ctrl Pts',(79.1119590809446,-10.8529384470573,137.821175059051));
#76076=CARTESIAN_POINT('Ctrl Pts',(79.0476084179951,-10.8220976914142,137.817315656327));
#76077=CARTESIAN_POINT('Ctrl Pts',(78.9848976994584,-10.7879158588881,137.813456253603));
#76078=CARTESIAN_POINT('Ctrl Pts',(78.9241841484707,-10.7506049857401,137.809596850879));
#76079=CARTESIAN_POINT('Ctrl Pts',(78.8634362209924,-10.713272986882,137.805735262931));
#76080=CARTESIAN_POINT('Ctrl Pts',(78.8046881124177,-10.6728086962058,137.801873674983));
#76081=CARTESIAN_POINT('Ctrl Pts',(78.7482668969634,-10.6294667229687,137.798012087035));
#76082=CARTESIAN_POINT('Ctrl Pts',(78.6917469705685,-10.5860489213944,137.7941437431));
#76083=CARTESIAN_POINT('Ctrl Pts',(78.6375624345439,-10.5397437012184,137.790275399166));
#76084=CARTESIAN_POINT('Ctrl Pts',(78.5860056707852,-10.4908445926549,137.786407055231));
#76085=CARTESIAN_POINT('Ctrl Pts',(78.5553927482461,-10.4618097092846,137.784110143932));
#76086=CARTESIAN_POINT('Ctrl Pts',(78.5257055636268,-10.4318610058014,137.781813232633));
#76087=CARTESIAN_POINT('Ctrl Pts',(78.4969985543702,-10.401065386388,137.779516321333));
#76088=CARTESIAN_POINT('Ctrl Pts',(78.4492223163319,-10.3498131353968,137.775693638866));
#76089=CARTESIAN_POINT('Ctrl Pts',(78.4039661357283,-10.2960019555863,137.771870956398));
#76090=CARTESIAN_POINT('Ctrl Pts',(78.3615208436963,-10.2399127456633,137.768048273931));
#76091=CARTESIAN_POINT('Ctrl Pts',(78.3191332469998,-10.1838997770766,137.764230787586));
#76092=CARTESIAN_POINT('Ctrl Pts',(78.279549263615,-10.1256153088631,137.760413301241));
#76093=CARTESIAN_POINT('Ctrl Pts',(78.2430220975309,-10.0653760898084,137.756595814896));
#76094=CARTESIAN_POINT('Ctrl Pts',(78.2065316626794,-10.0051974465115,137.752782167365));
#76095=CARTESIAN_POINT('Ctrl Pts',(78.1730922068983,-9.94306837371643,137.748968519833));
#76096=CARTESIAN_POINT('Ctrl Pts',(78.1429147652313,-9.87933610940529,137.745154872302));
#76097=CARTESIAN_POINT('Ctrl Pts',(78.1127570014886,-9.81564540324506,137.741343711551));
#76098=CARTESIAN_POINT('Ctrl Pts',(78.0858572438916,-9.75035402913312,137.7375325508));
#76099=CARTESIAN_POINT('Ctrl Pts',(78.0623806013098,-9.68383377243263,137.733721390049));
#76100=CARTESIAN_POINT('Ctrl Pts',(78.038904093185,-9.61731389671139,137.729910251125));
#76101=CARTESIAN_POINT('Ctrl Pts',(78.0188508409781,-9.54956561720769,137.726099112202));
#76102=CARTESIAN_POINT('Ctrl Pts',(78.0023372240674,-9.48097920553086,137.722287973278));
#76103=CARTESIAN_POINT('Ctrl Pts',(77.985823466128,-9.41239220811633,137.718476801807));
#76104=CARTESIAN_POINT('Ctrl Pts',(77.972849509985,-9.34296755130379,137.714665630336));
#76105=CARTESIAN_POINT('Ctrl Pts',(77.9634808603819,-9.27310685906643,137.710854458865));
#76106=CARTESIAN_POINT('Ctrl Pts',(77.954104932819,-9.20319189611444,137.707040326716));
#76107=CARTESIAN_POINT('Ctrl Pts',(77.9483399514159,-9.13284071762486,137.703226194567));
#76108=CARTESIAN_POINT('Ctrl Pts',(77.9461995397871,-9.06245984413321,137.699412062418));
#76109=CARTESIAN_POINT('Ctrl Pts',(77.9455473032982,-9.0410130470818,137.698249801791));
#76110=CARTESIAN_POINT('Ctrl Pts',(77.9452312678571,-9.01956349172712,137.697087541165));
#76111=CARTESIAN_POINT('Ctrl Pts',(77.945250857638,-8.99812264480472,137.695925280538));
#76112=CARTESIAN_POINT('Ctrl Pts',(77.9452508576385,-8.99812264423968,137.695925280507));
#76113=CARTESIAN_POINT('Ctrl Pts',(77.9453355911812,-8.90538253720821,137.690898045562));
#76114=CARTESIAN_POINT('Ctrl Pts',(77.9517027473503,-8.81292196311298,137.685870810616));
#76115=CARTESIAN_POINT('Ctrl Pts',(77.9642171232013,-8.72145800849217,137.68084357567));
#76116=CARTESIAN_POINT('Ctrl Pts',(77.9745563908271,-8.64589129096623,137.676690118227));
#76117=CARTESIAN_POINT('Ctrl Pts',(77.9890907794789,-8.57100419652186,137.672536660784));
#76118=CARTESIAN_POINT('Ctrl Pts',(78.0077202195897,-8.49718906230229,137.668383203341));
#76119=CARTESIAN_POINT('Ctrl Pts',(78.0250741586275,-8.4284278256959,137.66451412049));
#76120=CARTESIAN_POINT('Ctrl Pts',(78.0460260884595,-8.36043139357307,137.660645037639));
#76121=CARTESIAN_POINT('Ctrl Pts',(78.0704917545785,-8.29360386938326,137.656775954788));
#76122=CARTESIAN_POINT('Ctrl Pts',(78.0949209680755,-8.22687591487056,137.652912636677));
#76123=CARTESIAN_POINT('Ctrl Pts',(78.1228533603049,-8.16131386369155,137.649049318567));
#76124=CARTESIAN_POINT('Ctrl Pts',(78.1541542876671,-8.09730892949901,137.645186000456));
#76125=CARTESIAN_POINT('Ctrl Pts',(78.1854184990542,-8.03337907306842,137.641327214016));
#76126=CARTESIAN_POINT('Ctrl Pts',(78.2200431845955,-7.97100313985777,137.637468427576));
#76127=CARTESIAN_POINT('Ctrl Pts',(78.2578454199538,-7.91055290090612,137.633609641135));
#76128=CARTESIAN_POINT('Ctrl Pts',(78.2956238426761,-7.85014074117173,137.629753285448));
#76129=CARTESIAN_POINT('Ctrl Pts',(78.3365755870682,-7.79165227993754,137.62589692976));
#76130=CARTESIAN_POINT('Ctrl Pts',(78.3804722672276,-7.73543387469017,137.622040574073));
#76131=CARTESIAN_POINT('Ctrl Pts',(78.4243559798685,-7.67923207692214,137.618185357591));
#76132=CARTESIAN_POINT('Ctrl Pts',(78.4711826023524,-7.62529938649872,137.614330141109));
#76133=CARTESIAN_POINT('Ctrl Pts',(78.520682000174,-7.57395097633683,137.610474924628));
#76134=CARTESIAN_POINT('Ctrl Pts',(78.5701833332742,-7.52260055860539,137.606619557419));
#76135=CARTESIAN_POINT('Ctrl Pts',(78.6223573104465,-7.47383496994327,137.60276419021));
#76136=CARTESIAN_POINT('Ctrl Pts',(78.676896507449,-7.42793298154968,137.598908823001));
#76137=CARTESIAN_POINT('Ctrl Pts',(78.7314927921186,-7.38198294629104,137.595049420273));
#76138=CARTESIAN_POINT('Ctrl Pts',(78.7884588663218,-7.33890280824862,137.591190017546));
#76139=CARTESIAN_POINT('Ctrl Pts',(78.8474544423378,-7.29893083620532,137.587330614819));
#76140=CARTESIAN_POINT('Ctrl Pts',(78.9064834221125,-7.25893623171735,137.583469026868));
#76141=CARTESIAN_POINT('Ctrl Pts',(78.9675437752331,-7.22205354786824,137.579607438916));
#76142=CARTESIAN_POINT('Ctrl Pts',(79.030268826082,-7.18847605237149,137.575745850965));
#76143=CARTESIAN_POINT('Ctrl Pts',(79.093103616655,-7.15483981184317,137.571877507027));
#76144=CARTESIAN_POINT('Ctrl Pts',(79.1576084799626,-7.12452051139249,137.568009163089));
#76145=CARTESIAN_POINT('Ctrl Pts',(79.2233955510299,-7.09766378041636,137.564140819151));
#76146=CARTESIAN_POINT('Ctrl Pts',(79.262458019929,-7.08171702672345,137.561843907884));
#76147=CARTESIAN_POINT('Ctrl Pts',(79.3019722152477,-7.06699010951289,137.559546996617));
#76148=CARTESIAN_POINT('Ctrl Pts',(79.3418547552918,-7.05350509906448,137.55725008535));
#76149=CARTESIAN_POINT('Ctrl Pts',(79.4090365153636,-7.03078972698665,137.553380960127));
#76150=CARTESIAN_POINT('Ctrl Pts',(79.4775272460006,-7.01151203626851,137.549511834903));
#76151=CARTESIAN_POINT('Ctrl Pts',(79.5469417357709,-6.99582042428487,137.54564270968));
#76152=CARTESIAN_POINT('Ctrl Pts',(79.6162525807633,-6.98015224189991,137.54177936156));
#76153=CARTESIAN_POINT('Ctrl Pts',(79.6864839770011,-6.96805961584166,137.537916013439));
#76154=CARTESIAN_POINT('Ctrl Pts',(79.7572342153366,-6.95964161572121,137.534052665318));
#76155=CARTESIAN_POINT('Ctrl Pts',(79.8279006001617,-6.95123359265351,137.530193896055));
#76156=CARTESIAN_POINT('Ctrl Pts',(79.8990841254847,-6.94649160115844,137.526335126793));
#76157=CARTESIAN_POINT('Ctrl Pts',(79.9703732449642,-6.94546360025283,137.52247635753));
#76158=CARTESIAN_POINT('Ctrl Pts',(80.0416171339064,-6.94443625157907,137.518620036526));
#76159=CARTESIAN_POINT('Ctrl Pts',(80.1129659995101,-6.94711822512923,137.514763715522));
#76160=CARTESIAN_POINT('Ctrl Pts',(80.1840049945603,-6.95350550343352,137.510907394518));
#76161=CARTESIAN_POINT('Ctrl Pts',(80.2550226814983,-6.95989086587679,137.507052230216));
#76162=CARTESIAN_POINT('Ctrl Pts',(80.3257301988895,-6.96997928287426,137.503197065914));
#76163=CARTESIAN_POINT('Ctrl Pts',(80.3957162605865,-6.9837147514284,137.499341901611));
#76164=CARTESIAN_POINT('Ctrl Pts',(80.4657047407188,-6.99745069462477,137.49548660409));
#76165=CARTESIAN_POINT('Ctrl Pts',(80.5349712394912,-7.01483384359809,137.491631306569));
#76166=CARTESIAN_POINT('Ctrl Pts',(80.6031148326335,-7.03575712775699,137.487776009048));
#76167=CARTESIAN_POINT('Ctrl Pts',(80.67132616268,-7.05670121032744,137.483916879238));
#76168=CARTESIAN_POINT('Ctrl Pts',(80.7384118941889,-7.08119230845913,137.480057749428));
#76169=CARTESIAN_POINT('Ctrl Pts',(80.8039873646176,-7.10907380365194,137.476198619618));
#76170=CARTESIAN_POINT('Ctrl Pts',(80.8695998450386,-7.1369710348192,137.472337311763));
#76171=CARTESIAN_POINT('Ctrl Pts',(80.9336999310067,-7.1682622590305,137.468476003907));
#76172=CARTESIAN_POINT('Ctrl Pts',(80.9959264492284,-7.20274429470169,137.464614696052));
#76173=CARTESIAN_POINT('Ctrl Pts',(81.0582543739519,-7.23728252349944,137.460747095675));
#76174=CARTESIAN_POINT('Ctrl Pts',(81.1187022253211,-7.27502168482671,137.456879495297));
#76175=CARTESIAN_POINT('Ctrl Pts',(81.1769374678791,-7.31571505997286,137.45301189492));
#76176=CARTESIAN_POINT('Ctrl Pts',(81.2024025701055,-7.33350945581485,137.451320670935));
#76177=CARTESIAN_POINT('Ctrl Pts',(81.2274450179012,-7.35186821624316,137.44962944695));
#76178=CARTESIAN_POINT('Ctrl Pts',(81.2520391107129,-7.37076839346111,137.447938222965));
#76179=CARTESIAN_POINT('',(77.9452508246239,-9.00184086701729,137.754074719432));
#76180=CARTESIAN_POINT('Ctrl Pts',(77.9452508246239,-9.00184086701728,137.754074719432));
#76181=CARTESIAN_POINT('Ctrl Pts',(77.9451879957237,-8.93171215608289,137.750267950527));
#76182=CARTESIAN_POINT('Ctrl Pts',(77.9487196432091,-8.86147127332159,137.746461181623));
#76183=CARTESIAN_POINT('Ctrl Pts',(77.9558535710242,-8.79152232876057,137.742654412718));
#76184=CARTESIAN_POINT('Ctrl Pts',(77.9629816800021,-8.72163043853593,137.73885074883));
#76185=CARTESIAN_POINT('Ctrl Pts',(77.9737061958363,-8.65203051067417,137.735047084943));
#76186=CARTESIAN_POINT('Ctrl Pts',(77.9879828890365,-8.58312506948712,137.731243421055));
#76187=CARTESIAN_POINT('Ctrl Pts',(78.0022530301476,-8.5142512514906,137.727441502806));
#76188=CARTESIAN_POINT('Ctrl Pts',(78.0200720145936,-8.44607177785787,137.723639584557));
#76189=CARTESIAN_POINT('Ctrl Pts',(78.0413442350505,-8.37898055028048,137.719837666308));
#76190=CARTESIAN_POINT('Ctrl Pts',(78.0626142800848,-8.3118961838471,137.716036136865));
#76191=CARTESIAN_POINT('Ctrl Pts',(78.0873367072432,-8.24590031936901,137.712234607422));
#76192=CARTESIAN_POINT('Ctrl Pts',(78.1153661610127,-8.18137135681427,137.70843307798));
#76193=CARTESIAN_POINT('Ctrl Pts',(78.1434216019787,-8.1167825669493,137.704628023991));
#76194=CARTESIAN_POINT('Ctrl Pts',(78.1747899917197,-8.05366385490174,137.700822970003));
#76195=CARTESIAN_POINT('Ctrl Pts',(78.2092783941065,-7.99237224498024,137.697017916015));
#76196=CARTESIAN_POINT('Ctrl Pts',(78.2437833388229,-7.93105123659601,137.693211036936));
#76197=CARTESIAN_POINT('Ctrl Pts',(78.2814110055525,-7.87155949732334,137.689404157857));
#76198=CARTESIAN_POINT('Ctrl Pts',(78.3219247244651,-7.81422559812649,137.685597278778));
#76199=CARTESIAN_POINT('Ctrl Pts',(78.3625095297396,-7.75679109946812,137.681783720056));
#76200=CARTESIAN_POINT('Ctrl Pts',(78.4059901860581,-7.70152239258478,137.677970161334));
#76201=CARTESIAN_POINT('Ctrl Pts',(78.4520898455688,-7.64871479090879,137.674156602612));
#76202=CARTESIAN_POINT('Ctrl Pts',(78.4841323747948,-7.61200976666302,137.671505909134));
#76203=CARTESIAN_POINT('Ctrl Pts',(78.5174393844108,-7.576493026584,137.668855215655));
#76204=CARTESIAN_POINT('Ctrl Pts',(78.5519082624525,-7.54225246282259,137.666204522177));
#76205=CARTESIAN_POINT('Ctrl Pts',(78.6022207357351,-7.49227324831671,137.66233543933));
#76206=CARTESIAN_POINT('Ctrl Pts',(78.6552222517713,-7.44480391681055,137.658466356483));
#76207=CARTESIAN_POINT('Ctrl Pts',(78.7106323248068,-7.40014733157491,137.654597273636));
#76208=CARTESIAN_POINT('Ctrl Pts',(78.7659598395983,-7.35555728242294,137.650733955529));
#76209=CARTESIAN_POINT('Ctrl Pts',(78.8236884129031,-7.31377196316542,137.646870637422));
#76210=CARTESIAN_POINT('Ctrl Pts',(78.8835010225438,-7.27505721954632,137.643007319315));
#76211=CARTESIAN_POINT('Ctrl Pts',(78.9432434720188,-7.23638788830505,137.639148532878));
#76212=CARTESIAN_POINT('Ctrl Pts',(79.0050646962477,-7.20078224102097,137.635289746442));
#76213=CARTESIAN_POINT('Ctrl Pts',(79.06861632084,-7.16846457727558,137.631430960006));
#76214=CARTESIAN_POINT('Ctrl Pts',(79.1321279125703,-7.13616727128783,137.627574604322));
#76215=CARTESIAN_POINT('Ctrl Pts',(79.1973673100838,-7.1071540593101,137.623718248638));
#76216=CARTESIAN_POINT('Ctrl Pts',(79.2639602801964,-7.08160403113136,137.619861892954));
#76217=CARTESIAN_POINT('Ctrl Pts',(79.3305335780805,-7.05606155068615,137.616006676476));
#76218=CARTESIAN_POINT('Ctrl Pts',(79.3984592014336,-7.03398039690303,137.612151459998));
#76219=CARTESIAN_POINT('Ctrl Pts',(79.4673432145724,-7.01549141814958,137.60829624352));
#76220=CARTESIAN_POINT('Ctrl Pts',(79.5362299208718,-6.99700171653192,137.604440876314));
#76221=CARTESIAN_POINT('Ctrl Pts',(79.6060746216013,-6.98210459257871,137.600585509109));
#76222=CARTESIAN_POINT('Ctrl Pts',(79.6764701885847,-6.97088048069475,137.596730141903));
#76223=CARTESIAN_POINT('Ctrl Pts',(79.7469394405332,-6.95964462022593,137.592870739179));
#76224=CARTESIAN_POINT('Ctrl Pts',(79.8179602290655,-6.95208952323919,137.589011336456));
#76225=CARTESIAN_POINT('Ctrl Pts',(79.8891181401292,-6.94824397755201,137.585151933732));
#76226=CARTESIAN_POINT('Ctrl Pts',(79.9603163413626,-6.94439625448658,137.581290345784));
#76227=CARTESIAN_POINT('Ctrl Pts',(80.0316513336722,-6.94426226483673,137.577428757836));
#76228=CARTESIAN_POINT('Ctrl Pts',(80.1027092849991,-6.94781863246082,137.573567169888));
#76229=CARTESIAN_POINT('Ctrl Pts',(80.1738915547607,-6.95138122207764,137.569698825953));
#76230=CARTESIAN_POINT('Ctrl Pts',(80.2447953324307,-6.95864700984184,137.565830482018));
#76231=CARTESIAN_POINT('Ctrl Pts',(80.3150131820552,-6.96954087516358,137.561962138084));
#76232=CARTESIAN_POINT('Ctrl Pts',(80.3567065203249,-6.97600933887123,137.559665226784));
#76233=CARTESIAN_POINT('Ctrl Pts',(80.3981582238856,-6.9837559538072,137.557368315485));
#76234=CARTESIAN_POINT('Ctrl Pts',(80.4392854645027,-6.99275665571495,137.555071404186));
#76235=CARTESIAN_POINT('Ctrl Pts',(80.5085688299926,-7.00791932917862,137.551202004181));
#76236=CARTESIAN_POINT('Ctrl Pts',(80.5772019369491,-7.02670306183723,137.547332604176));
#76237=CARTESIAN_POINT('Ctrl Pts',(80.644778110245,-7.04903645573556,137.543463204171));
#76238=CARTESIAN_POINT('Ctrl Pts',(80.7122373862133,-7.0713312159863,137.539600497687));
#76239=CARTESIAN_POINT('Ctrl Pts',(80.7786429038342,-7.09716328564512,137.535737791203));
#76240=CARTESIAN_POINT('Ctrl Pts',(80.8435995584078,-7.1264105712419,137.531875084719));
#76241=CARTESIAN_POINT('Ctrl Pts',(80.9084915578482,-7.15562874531559,137.528016223011));
#76242=CARTESIAN_POINT('Ctrl Pts',(80.9719371146362,-7.18825519303851,137.524157361303));
#76243=CARTESIAN_POINT('Ctrl Pts',(81.0335588124515,-7.22411888244065,137.520298499595));
#76244=CARTESIAN_POINT('Ctrl Pts',(81.0951364101866,-7.25995690569538,137.516442399514));
#76245=CARTESIAN_POINT('Ctrl Pts',(81.1548923224176,-7.29902732574741,137.512586299433));
#76246=CARTESIAN_POINT('Ctrl Pts',(81.2124731810425,-7.34111291892647,137.508730199351));
#76247=CARTESIAN_POINT('Ctrl Pts',(81.2257792412245,-7.35083825906566,137.507839113303));
#76248=CARTESIAN_POINT('Ctrl Pts',(81.2389692666534,-7.36072442189331,137.506948027255));
#76249=CARTESIAN_POINT('Ctrl Pts',(81.2520391107129,-7.37076839346111,137.506056941207));
#76250=CARTESIAN_POINT('Ctrl Pts',(81.2520391107129,-7.37076839346111,138.206016809128));
#76251=CARTESIAN_POINT('Ctrl Pts',(81.3100004179798,-7.41531075521925,138.202046816837));
#76252=CARTESIAN_POINT('Ctrl Pts',(81.3656646502486,-7.46301363829869,138.198076824546));
#76253=CARTESIAN_POINT('Ctrl Pts',(81.4186724490077,-7.51360636272669,138.194106832255));
#76254=CARTESIAN_POINT('Ctrl Pts',(81.470180544976,-7.56276771192698,138.190249159447));
#76255=CARTESIAN_POINT('Ctrl Pts',(81.5191801491463,-7.61465719146405,138.186391486638));
#76256=CARTESIAN_POINT('Ctrl Pts',(81.5653745141076,-7.66898527690999,138.182533813829));
#76257=CARTESIAN_POINT('Ctrl Pts',(81.6115458735347,-7.72328630609853,138.178678062203));
#76258=CARTESIAN_POINT('Ctrl Pts',(81.6549144517787,-7.78002316174998,138.174822310578));
#76259=CARTESIAN_POINT('Ctrl Pts',(81.6952218735085,-7.8388710829204,138.170966558952));
#76260=CARTESIAN_POINT('Ctrl Pts',(81.7355227048577,-7.89770938228475,138.167111437753));
#76261=CARTESIAN_POINT('Ctrl Pts',(81.7727630996661,-7.95865766065981,138.163256316554));
#76262=CARTESIAN_POINT('Ctrl Pts',(81.8067273668012,-8.02136125942632,138.159401195355));
#76263=CARTESIAN_POINT('Ctrl Pts',(81.8424556842878,-8.08732158400432,138.155345845254));
#76264=CARTESIAN_POINT('Ctrl Pts',(81.8745580065639,-8.15522401595865,138.151290495153));
#76265=CARTESIAN_POINT('Ctrl Pts',(81.9028386326526,-8.22462737952329,138.147235145052));
#76266=CARTESIAN_POINT('Ctrl Pts',(81.9297585778696,-8.29069150197893,138.143374912177));
#76267=CARTESIAN_POINT('Ctrl Pts',(81.9532159966933,-8.35811495349229,138.139514679302));
#76268=CARTESIAN_POINT('Ctrl Pts',(81.9730927843165,-8.42649984570362,138.135654446427));
#76269=CARTESIAN_POINT('Ctrl Pts',(81.9929834859348,-8.49493260817794,138.131791511342));
#76270=CARTESIAN_POINT('Ctrl Pts',(82.0092884595855,-8.56432767786134,138.127928576256));
#76271=CARTESIAN_POINT('Ctrl Pts',(82.0219406340872,-8.63427655977905,138.124065641171));
#76272=CARTESIAN_POINT('Ctrl Pts',(82.0346132883302,-8.70433866610792,138.120196453255));
#76273=CARTESIAN_POINT('Ctrl Pts',(82.0436212919721,-8.77495589200382,138.116327265338));
#76274=CARTESIAN_POINT('Ctrl Pts',(82.0489494313871,-8.84571523043957,138.112458077422));
#76275=CARTESIAN_POINT('Ctrl Pts',(82.0497394482973,-8.85620689921254,138.111884382996));
#76276=CARTESIAN_POINT('Ctrl Pts',(82.0504486576644,-8.86670169549341,138.11131068857));
#76277=CARTESIAN_POINT('Ctrl Pts',(82.0510771072001,-8.87719827843336,138.110736994144));
#76278=CARTESIAN_POINT('Ctrl Pts',(82.0553154671481,-8.94798884187682,138.106867911045));
#76279=CARTESIAN_POINT('Ctrl Pts',(82.0558929439494,-9.01913773756604,138.102998827945));
#76280=CARTESIAN_POINT('Ctrl Pts',(82.0527677254119,-9.09023429507291,138.099129744846));
#76281=CARTESIAN_POINT('Ctrl Pts',(82.0496471632914,-9.16122492231617,138.095266426484));
#76282=CARTESIAN_POINT('Ctrl Pts',(82.0428348777429,-9.23216288480688,138.091403108122));
#76283=CARTESIAN_POINT('Ctrl Pts',(82.032340984946,-9.30263457074262,138.087539789761));
#76284=CARTESIAN_POINT('Ctrl Pts',(82.021859401472,-9.37302359348072,138.083681003066));
#76285=CARTESIAN_POINT('Ctrl Pts',(82.0077048599954,-9.44294694792222,138.079822216372));
#76286=CARTESIAN_POINT('Ctrl Pts',(81.9899393756735,-9.51199496447144,138.075963429678));
#76287=CARTESIAN_POINT('Ctrl Pts',(81.9721850822951,-9.58099948586839,138.072107073734));
#76288=CARTESIAN_POINT('Ctrl Pts',(81.9508244796561,-9.64912929399013,138.068250717791));
#76289=CARTESIAN_POINT('Ctrl Pts',(81.9259705990646,-9.71598520518144,138.064394361847));
#76290=CARTESIAN_POINT('Ctrl Pts',(81.9011240605487,-9.78282136649287,138.060539145108));
#76291=CARTESIAN_POINT('Ctrl Pts',(81.8727864619641,-9.84838392288732,138.056683928369));
#76292=CARTESIAN_POINT('Ctrl Pts',(81.8411200555273,-9.91229079992897,138.052828711631));
#76293=CARTESIAN_POINT('Ctrl Pts',(81.8094524110205,-9.97620017555506,138.048973344163));
#76294=CARTESIAN_POINT('Ctrl Pts',(81.7744559179282,-10.0384533090118,138.045117976696));
#76295=CARTESIAN_POINT('Ctrl Pts',(81.7363393757206,-10.0986915558164,138.041262609229));
#76296=CARTESIAN_POINT('Ctrl Pts',(81.6981829358925,-10.1589928556307,138.037403206243));
#76297=CARTESIAN_POINT('Ctrl Pts',(81.6569001878845,-10.2172746473378,138.033543803258));
#76298=CARTESIAN_POINT('Ctrl Pts',(81.6127434984387,-10.2732069630439,138.029684400273));
#76299=CARTESIAN_POINT('Ctrl Pts',(81.5685618071274,-10.329170948068,138.025822812063));
#76300=CARTESIAN_POINT('Ctrl Pts',(81.5215032556432,-10.3827824436303,138.021961223854));
#76301=CARTESIAN_POINT('Ctrl Pts',(81.4718589647921,-10.4337464037482,138.018099635644));
#76302=CARTESIAN_POINT('Ctrl Pts',(81.4221278195125,-10.4847995271025,138.01423129145));
#76303=CARTESIAN_POINT('Ctrl Pts',(81.3698022596313,-10.5331955372286,138.010362947257));
#76304=CARTESIAN_POINT('Ctrl Pts',(81.3152080015881,-10.5786783950694,138.006494603063));
#76305=CARTESIAN_POINT('Ctrl Pts',(81.2827915373983,-10.6056847778885,138.004197694093));
#76306=CARTESIAN_POINT('Ctrl Pts',(81.2495758162233,-10.6316648862377,138.001900785122));
#76307=CARTESIAN_POINT('Ctrl Pts',(81.2156336505187,-10.6565724826359,137.999603876152));
#76308=CARTESIAN_POINT('Ctrl Pts',(81.1584589632516,-10.6985286750322,137.995734793277));
#76309=CARTESIAN_POINT('Ctrl Pts',(81.0989976384083,-10.7376035912017,137.991865710402));
#76310=CARTESIAN_POINT('Ctrl Pts',(81.0375720156334,-10.7735393637792,137.987996627528));
#76311=CARTESIAN_POINT('Ctrl Pts',(80.9762379139521,-10.8094215938601,137.984133309392));
#76312=CARTESIAN_POINT('Ctrl Pts',(80.9129457396517,-10.8421737210908,137.980269991257));
#76313=CARTESIAN_POINT('Ctrl Pts',(80.8480484684536,-10.8715799095025,137.976406673121));
#76314=CARTESIAN_POINT('Ctrl Pts',(80.7832273216993,-10.9009516044803,137.972547886654));
#76315=CARTESIAN_POINT('Ctrl Pts',(80.7168052582111,-10.9269849570654,137.968689100188));
#76316=CARTESIAN_POINT('Ctrl Pts',(80.6491600907199,-10.9495098715104,137.964830313721));
#76317=CARTESIAN_POINT('Ctrl Pts',(80.5815575347049,-10.9720205969173,137.960973958006));
#76318=CARTESIAN_POINT('Ctrl Pts',(80.512733863091,-10.9910271157927,137.957117602291));
#76319=CARTESIAN_POINT('Ctrl Pts',(80.4430857491828,-11.0064078801109,137.953261246575));
#76320=CARTESIAN_POINT('Ctrl Pts',(80.3734582100062,-11.0217841008014,137.949406030065));
#76321=CARTESIAN_POINT('Ctrl Pts',(80.3030071861419,-11.0335365886353,137.945550813555));
#76322=CARTESIAN_POINT('Ctrl Pts',(80.2321416733279,-11.0415944274034,137.941695597045));
#76323=CARTESIAN_POINT('Ctrl Pts',(80.1612733898664,-11.0496525812109,137.937840229806));
#76324=CARTESIAN_POINT('Ctrl Pts',(80.0899910682031,-11.0540157464709,137.933984862568));
#76325=CARTESIAN_POINT('Ctrl Pts',(80.0187092661134,-11.0546648208069,137.930129495329));
#76326=CARTESIAN_POINT('Ctrl Pts',(79.9473528513915,-11.055314574547,137.926270092571));
#76327=CARTESIAN_POINT('Ctrl Pts',(79.875997444087,-11.052242472327,137.922410689813));
#76328=CARTESIAN_POINT('Ctrl Pts',(79.8050571398559,-11.0454815676947,137.918551287055));
#76329=CARTESIAN_POINT('Ctrl Pts',(79.7340766686535,-11.0387168349838,137.914689699072));
#76330=CARTESIAN_POINT('Ctrl Pts',(79.6635122491684,-11.0282592132919,137.910828111089));
#76331=CARTESIAN_POINT('Ctrl Pts',(79.5937696574455,-11.0141932556952,137.906966523106));
#76332=CARTESIAN_POINT('Ctrl Pts',(79.5239050485444,-11.0001026891986,137.903098179136));
#76333=CARTESIAN_POINT('Ctrl Pts',(79.454865608743,-10.9823913036386,137.899229835166));
#76334=CARTESIAN_POINT('Ctrl Pts',(79.3870431070684,-10.9611938736157,137.895361491195));
#76335=CARTESIAN_POINT('Ctrl Pts',(79.3467720628869,-10.948607451412,137.893064580184));
#76336=CARTESIAN_POINT('Ctrl Pts',(79.3069297253047,-10.9347929137085,137.890767669172));
#76337=CARTESIAN_POINT('Ctrl Pts',(79.2675944322142,-10.9197863544614,137.88847075816));
#76338=CARTESIAN_POINT('Ctrl Pts',(79.2013352240665,-10.8945082224174,137.884601675388));
#76339=CARTESIAN_POINT('Ctrl Pts',(79.1362564439906,-10.8657462631716,137.880732592617));
#76340=CARTESIAN_POINT('Ctrl Pts',(79.072749565558,-10.8336314227039,137.876863509845));
#76341=CARTESIAN_POINT('Ctrl Pts',(79.0093373092316,-10.8015644317593,137.873000191815));
#76342=CARTESIAN_POINT('Ctrl Pts',(78.9474927356075,-10.7661546932086,137.869136873785));
#76343=CARTESIAN_POINT('Ctrl Pts',(78.8875886226998,-10.7275816884168,137.865273555755));
#76344=CARTESIAN_POINT('Ctrl Pts',(78.8277547773211,-10.6890539297625,137.861414769397));
#76345=CARTESIAN_POINT('Ctrl Pts',(78.7698572778851,-10.6473705369187,137.85755598304));
#76346=CARTESIAN_POINT('Ctrl Pts',(78.7142439456413,-10.602756666241,137.853697196682));
#76347=CARTESIAN_POINT('Ctrl Pts',(78.658665645734,-10.5581708990425,137.849840841078));
#76348=CARTESIAN_POINT('Ctrl Pts',(78.6053690363735,-10.5106586196787,137.845984485474));
#76349=CARTESIAN_POINT('Ctrl Pts',(78.5546713818689,-10.4604871612278,137.84212812987));
#76350=CARTESIAN_POINT('Ctrl Pts',(78.5039887039709,-10.4103305239398,137.838272913473));
#76351=CARTESIAN_POINT('Ctrl Pts',(78.455903801816,-10.357516608615,137.834417697076));
#76352=CARTESIAN_POINT('Ctrl Pts',(78.4106980856967,-10.3023505625184,137.830562480679));
#76353=CARTESIAN_POINT('Ctrl Pts',(78.3654906021781,-10.2471823596053,137.826707113555));
#76354=CARTESIAN_POINT('Ctrl Pts',(78.3231628343794,-10.1896622204827,137.822851746431));
#76355=CARTESIAN_POINT('Ctrl Pts',(78.2839556788196,-10.1301280680721,137.818996379307));
#76356=CARTESIAN_POINT('Ctrl Pts',(78.2447074840645,-10.0705315996463,137.815136976666));
#76357=CARTESIAN_POINT('Ctrl Pts',(78.2085866898057,-10.0089173161854,137.811277574025));
#76358=CARTESIAN_POINT('Ctrl Pts',(78.175790124002,-9.94565104071822,137.807418171383));
#76359=CARTESIAN_POINT('Ctrl Pts',(78.1429749885287,-9.88234894339576,137.803556583518));
#76360=CARTESIAN_POINT('Ctrl Pts',(78.1134880292955,-9.81739343458066,137.799694995653));
#76361=CARTESIAN_POINT('Ctrl Pts',(78.0874782954112,-9.75117128005319,137.795833407788));
#76362=CARTESIAN_POINT('Ctrl Pts',(78.0614230565633,-9.68483326748785,137.791965063936));
#76363=CARTESIAN_POINT('Ctrl Pts',(78.0388573428529,-9.61722464575904,137.788096720084));
#76364=CARTESIAN_POINT('Ctrl Pts',(78.0198804134945,-9.54874765205621,137.784228376233));
#76365=CARTESIAN_POINT('Ctrl Pts',(78.0086124552047,-9.50808797027721,137.781931464211));
#76366=CARTESIAN_POINT('Ctrl Pts',(77.9986088005102,-9.46712235311462,137.77963455219));
#76367=CARTESIAN_POINT('Ctrl Pts',(77.9898816146324,-9.42593619159094,137.777337640169));
#76368=CARTESIAN_POINT('Ctrl Pts',(77.9692978091794,-9.32879514887455,137.771920179047));
#76369=CARTESIAN_POINT('Ctrl Pts',(77.9557497500277,-9.23011503383561,137.766502717926));
#76370=CARTESIAN_POINT('Ctrl Pts',(77.949413941794,-9.13074547943003,137.761085256805));
#76371=CARTESIAN_POINT('Ctrl Pts',(77.94668096293,-9.08788198326621,137.758748411024));
#76372=CARTESIAN_POINT('Ctrl Pts',(77.9452893931581,-9.04489049479503,137.756411565243));
#76373=CARTESIAN_POINT('Ctrl Pts',(77.9452508246244,-9.00184086757116,137.754074719462));
#76374=CARTESIAN_POINT('Origin',(80.,-9.,141.545925280538));
#76375=CARTESIAN_POINT('',(81.2520391107129,-7.37076839346111,138.906139397208));
#76376=CARTESIAN_POINT('',(81.2520391107129,-7.37076839346111,138.847890491337));
#76377=CARTESIAN_POINT('',(81.2520391107129,-7.37076839346111,141.545925280538));
#76378=CARTESIAN_POINT('',(77.9452500654425,-9.00051859011398,138.39592528059));
#76379=CARTESIAN_POINT('Ctrl Pts',(81.2520391107129,-7.37076839346111,138.847890491337));
#76380=CARTESIAN_POINT('Ctrl Pts',(81.3085681377711,-7.4142100701898,138.844035068992));
#76381=CARTESIAN_POINT('Ctrl Pts',(81.3628582559677,-7.46061620714495,138.840179646647));
#76382=CARTESIAN_POINT('Ctrl Pts',(81.4145905616516,-7.50972113167154,138.836324224303));
#76383=CARTESIAN_POINT('Ctrl Pts',(81.4663198262433,-7.55882316955704,138.832469028599));
#76384=CARTESIAN_POINT('Ctrl Pts',(81.5154912256335,-7.61062334443875,138.828613832896));
#76385=CARTESIAN_POINT('Ctrl Pts',(81.5618216651866,-7.66481812150793,138.824758637193));
#76386=CARTESIAN_POINT('Ctrl Pts',(81.6081976898814,-7.71906622154602,138.820899648311));
#76387=CARTESIAN_POINT('Ctrl Pts',(81.6517268546166,-7.77571326004013,138.817040659429));
#76388=CARTESIAN_POINT('Ctrl Pts',(81.6921660259195,-7.83442215908853,138.813181670547));
#76389=CARTESIAN_POINT('Ctrl Pts',(81.7326245444005,-7.8931591460401,138.809320835421));
#76390=CARTESIAN_POINT('Ctrl Pts',(81.7699898695783,-7.95395954422761,138.805460000296));
#76391=CARTESIAN_POINT('Ctrl Pts',(81.8040634605908,-8.01645915557045,138.801599165171));
#76392=CARTESIAN_POINT('Ctrl Pts',(81.8381998457058,-8.0790739472301,138.797731214926));
#76393=CARTESIAN_POINT('Ctrl Pts',(81.8690321655762,-8.14339376955236,138.793863264681));
#76394=CARTESIAN_POINT('Ctrl Pts',(81.8964091261853,-8.20903224552375,138.789995314436));
#76395=CARTESIAN_POINT('Ctrl Pts',(81.9206649231915,-8.26718747946997,138.786568337376));
#76396=CARTESIAN_POINT('Ctrl Pts',(81.9422089601469,-8.32637733301329,138.783141360317));
#76397=CARTESIAN_POINT('Ctrl Pts',(81.9609690692731,-8.38632429422847,138.779714383257));
#76398=CARTESIAN_POINT('Ctrl Pts',(81.9821493409331,-8.45400476000776,138.775845306345));
#76399=CARTESIAN_POINT('Ctrl Pts',(81.9998631210085,-8.52291559440797,138.771976229432));
#76400=CARTESIAN_POINT('Ctrl Pts',(82.0139708208754,-8.59266832290836,138.76810715252));
#76401=CARTESIAN_POINT('Ctrl Pts',(82.0280575005765,-8.6623171213604,138.764243840448));
#76402=CARTESIAN_POINT('Ctrl Pts',(82.0385486697698,-8.73280485169113,138.760380528376));
#76403=CARTESIAN_POINT('Ctrl Pts',(82.0453544272477,-8.80372766512275,138.756517216304));
#76404=CARTESIAN_POINT('Ctrl Pts',(82.0521522013523,-8.87456728380361,138.752658436021));
#76405=CARTESIAN_POINT('Ctrl Pts',(82.0552731047176,-8.94584049060809,138.748799655739));
#76406=CARTESIAN_POINT('Ctrl Pts',(82.0546785546254,-9.01713475014791,138.744940875457));
#76407=CARTESIAN_POINT('Ctrl Pts',(82.0540843790675,-9.08838409816279,138.741084525997));
#76408=CARTESIAN_POINT('Ctrl Pts',(82.049779397677,-9.15965398798164,138.737228176538));
#76409=CARTESIAN_POINT('Ctrl Pts',(82.0417770670953,-9.23052976116694,138.733371827078));
#76410=CARTESIAN_POINT('Ctrl Pts',(82.0337771006125,-9.30138459578544,138.729516616886));
#76411=CARTESIAN_POINT('Ctrl Pts',(82.0220820079176,-9.37184506246619,138.725661406693));
#76412=CARTESIAN_POINT('Ctrl Pts',(82.0067571395565,-9.44150124047278,138.721806196501));
#76413=CARTESIAN_POINT('Ctrl Pts',(81.9914316722434,-9.51116014089782,138.717950835633));
#76414=CARTESIAN_POINT('Ctrl Pts',(81.9724762541412,-9.58001421627456,138.714095474765));
#76415=CARTESIAN_POINT('Ctrl Pts',(81.9500070587942,-9.64766506247656,138.710240113896));
#76416=CARTESIAN_POINT('Ctrl Pts',(81.9275143444946,-9.71538672016182,138.706380717546));
#76417=CARTESIAN_POINT('Ctrl Pts',(81.9015006643918,-9.78190217257416,138.702521321195));
#76418=CARTESIAN_POINT('Ctrl Pts',(81.8721313878705,-9.84683034254225,138.698661924844));
#76419=CARTESIAN_POINT('Ctrl Pts',(81.8427454824318,-9.91179527491291,138.694800343298));
#76420=CARTESIAN_POINT('Ctrl Pts',(81.8100004214718,-9.97517070397781,138.690938761753));
#76421=CARTESIAN_POINT('Ctrl Pts',(81.7741076046741,-10.0366001010696,138.687077180207));
#76422=CARTESIAN_POINT('Ctrl Pts',(81.7381519917931,-10.0981369716305,138.683208842653));
#76423=CARTESIAN_POINT('Ctrl Pts',(81.6990378945876,-10.1577206064699,138.679340505098));
#76424=CARTESIAN_POINT('Ctrl Pts',(81.6570196921329,-10.2150239925137,138.675472167544));
#76425=CARTESIAN_POINT('Ctrl Pts',(81.6320698419778,-10.249049981529,138.673175200118));
#76426=CARTESIAN_POINT('Ctrl Pts',(81.6060968321676,-10.2822726221546,138.670878232692));
#76427=CARTESIAN_POINT('Ctrl Pts',(81.579160184669,-10.3146294815103,138.668581265266));
#76428=CARTESIAN_POINT('Ctrl Pts',(81.5337872424589,-10.3691324002469,138.664712180582));
#76429=CARTESIAN_POINT('Ctrl Pts',(81.4855004608265,-10.421390317654,138.660843095898));
#76430=CARTESIAN_POINT('Ctrl Pts',(81.4345505021733,-10.4710752595344,138.656974011214));
#76431=CARTESIAN_POINT('Ctrl Pts',(81.3836764561363,-10.5206861736036,138.653110691252));
#76432=CARTESIAN_POINT('Ctrl Pts',(81.330147454379,-10.5677313853259,138.649247371289));
#76433=CARTESIAN_POINT('Ctrl Pts',(81.2742540250556,-10.6119163260324,138.645384051327));
#76434=CARTESIAN_POINT('Ctrl Pts',(81.218426158404,-10.656049438057,138.641525263017));
#76435=CARTESIAN_POINT('Ctrl Pts',(81.1602397524556,-10.6973286435976,138.637666474707));
#76436=CARTESIAN_POINT('Ctrl Pts',(81.100020467273,-10.7354977770313,138.633807686397));
#76437=CARTESIAN_POINT('Ctrl Pts',(81.0398391156441,-10.773642866824,138.629951328829));
#76438=CARTESIAN_POINT('Ctrl Pts',(80.977627834725,-10.8086815118984,138.626094971261));
#76439=CARTESIAN_POINT('Ctrl Pts',(80.9137422932057,-10.8404001152215,138.622238613693));
#76440=CARTESIAN_POINT('Ctrl Pts',(80.8498756239809,-10.8721093486182,138.618383395324));
#76441=CARTESIAN_POINT('Ctrl Pts',(80.7843361109232,-10.900500271449,138.614528176955));
#76442=CARTESIAN_POINT('Ctrl Pts',(80.717503588529,-10.9254054541701,138.610672958585));
#76443=CARTESIAN_POINT('Ctrl Pts',(80.6506684531029,-10.9503116106392,138.606817589484));
#76444=CARTESIAN_POINT('Ctrl Pts',(80.5825406639435,-10.9717315888527,138.602962220382));
#76445=CARTESIAN_POINT('Ctrl Pts',(80.5135179453508,-10.9895469037705,138.599106851281));
#76446=CARTESIAN_POINT('Ctrl Pts',(80.4444229789358,-11.0073808664281,138.595247446667));
#76447=CARTESIAN_POINT('Ctrl Pts',(80.374431684465,-11.0216025121984,138.591388042053));
#76448=CARTESIAN_POINT('Ctrl Pts',(80.3039539120623,-11.0321440849118,138.58752863744));
#76449=CARTESIAN_POINT('Ctrl Pts',(80.2334362346204,-11.0426916263421,138.583667047602));
#76450=CARTESIAN_POINT('Ctrl Pts',(80.1624320146735,-11.0495548999817,138.579805457765));
#76451=CARTESIAN_POINT('Ctrl Pts',(80.0913554442118,-11.0527181358659,138.575943867928));
#76452=CARTESIAN_POINT('Ctrl Pts',(80.020154523198,-11.0558869059244,138.572075522125));
#76453=CARTESIAN_POINT('Ctrl Pts',(79.9488814848721,-11.0553427177614,138.568207176323));
#76454=CARTESIAN_POINT('Ctrl Pts',(79.8779490353346,-11.0511219184934,138.564338830521));
#76455=CARTESIAN_POINT('Ctrl Pts',(79.8358317181288,-11.0486157489929,138.562041936105));
#76456=CARTESIAN_POINT('Ctrl Pts',(79.7938343727432,-11.0448143517772,138.559745041689));
#76457=CARTESIAN_POINT('Ctrl Pts',(79.752041726348,-11.0397338691671,138.557448147274));
#76458=CARTESIAN_POINT('Ctrl Pts',(79.6816426567301,-11.0311758744047,138.553579063983));
#76459=CARTESIAN_POINT('Ctrl Pts',(79.6115492768518,-11.0189522248678,138.549709980692));
#76460=CARTESIAN_POINT('Ctrl Pts',(79.5421730827928,-11.0030956233741,138.5458408974));
#76461=CARTESIAN_POINT('Ctrl Pts',(79.4729002555399,-10.9872626473657,138.541977578836));
#76462=CARTESIAN_POINT('Ctrl Pts',(79.4043429627404,-10.9678075712217,138.538114260271));
#76463=CARTESIAN_POINT('Ctrl Pts',(79.33690625781,-10.9448147088009,138.534250941706));
#76464=CARTESIAN_POINT('Ctrl Pts',(79.2695486557729,-10.9218488168845,138.530392154793));
#76465=CARTESIAN_POINT('Ctrl Pts',(79.2033094882355,-10.8953535376155,138.526533367881));
#76466=CARTESIAN_POINT('Ctrl Pts',(79.1385805998206,-10.8654635293928,138.522674580968));
#76467=CARTESIAN_POINT('Ctrl Pts',(79.0738924856648,-10.8355923495939,138.518818224796));
#76468=CARTESIAN_POINT('Ctrl Pts',(79.0107132031364,-10.8023308866084,138.514961868625));
#76469=CARTESIAN_POINT('Ctrl Pts',(78.9494151096807,-10.7658620984473,138.511105512453));
#76470=CARTESIAN_POINT('Ctrl Pts',(78.8881351241254,-10.7294040834302,138.507250295477));
#76471=CARTESIAN_POINT('Ctrl Pts',(78.8287356416474,-10.6897408724661,138.503395078501));
#76472=CARTESIAN_POINT('Ctrl Pts',(78.7715633399238,-10.6471007664016,138.499539861525));
#76473=CARTESIAN_POINT('Ctrl Pts',(78.714388802788,-10.6044589931275,138.495684493812));
#76474=CARTESIAN_POINT('Ctrl Pts',(78.6594420073859,-10.5588403858577,138.491829126099));
#76475=CARTESIAN_POINT('Ctrl Pts',(78.6070382145787,-10.5105148217928,138.487973758385));
#76476=CARTESIAN_POINT('Ctrl Pts',(78.5545795691395,-10.4621386739011,138.484114355142));
#76477=CARTESIAN_POINT('Ctrl Pts',(78.5046695977665,-10.4110502430044,138.480254951899));
#76478=CARTESIAN_POINT('Ctrl Pts',(78.4575875191282,-10.357557107952,138.476395548656));
#76479=CARTESIAN_POINT('Ctrl Pts',(78.410478782161,-10.3040336845683,138.472533960182));
#76480=CARTESIAN_POINT('Ctrl Pts',(78.3662014270504,-10.248103227629,138.468672371707));
#76481=CARTESIAN_POINT('Ctrl Pts',(78.3249933520731,-10.1901051600177,138.464810783232));
#76482=CARTESIAN_POINT('Ctrl Pts',(78.2837131820377,-10.1320056226324,138.460942438765));
#76483=CARTESIAN_POINT('Ctrl Pts',(78.24551327357,-10.0718316626621,138.457074094298));
#76484=CARTESIAN_POINT('Ctrl Pts',(78.2105869337417,-10.009949721919,138.453205749831));
#76485=CARTESIAN_POINT('Ctrl Pts',(78.1898487213452,-9.97320608267847,138.450908842982));
#76486=CARTESIAN_POINT('Ctrl Pts',(78.1702637553136,-9.93586072306953,138.448611936132));
#76487=CARTESIAN_POINT('Ctrl Pts',(78.1518644288019,-9.89799358181013,138.446315029283));
#76488=CARTESIAN_POINT('Ctrl Pts',(78.1182272557188,-9.82876585307291,138.442115883558));
#76489=CARTESIAN_POINT('Ctrl Pts',(78.0884378127264,-9.75755151755703,138.437916737834));
#76490=CARTESIAN_POINT('Ctrl Pts',(78.0627161720044,-9.68478385807979,138.433717592109));
#76491=CARTESIAN_POINT('Ctrl Pts',(78.0373092445397,-9.61290653632974,138.429569824399));
#76492=CARTESIAN_POINT('Ctrl Pts',(78.015871306733,-9.53951403357927,138.425422056689));
#76493=CARTESIAN_POINT('Ctrl Pts',(77.9985686429311,-9.46504847644219,138.421274288979));
#76494=CARTESIAN_POINT('Ctrl Pts',(77.9809444893882,-9.38919932236631,138.417049454248));
#76495=CARTESIAN_POINT('Ctrl Pts',(77.9676110562636,-9.31223716100421,138.412824619516));
#76496=CARTESIAN_POINT('Ctrl Pts',(77.9586923529769,-9.23465006436166,138.408599784785));
#76497=CARTESIAN_POINT('Ctrl Pts',(77.9497736496901,-9.15706296771911,138.404374950053));
#76498=CARTESIAN_POINT('Ctrl Pts',(77.9452698355286,-9.07885132744909,138.400150115321));
#76499=CARTESIAN_POINT('Ctrl Pts',(77.9452500654424,-9.00051859011397,138.39592528059));
#76500=CARTESIAN_POINT('Ctrl Pts',(77.9452500654422,-9.00051858915731,138.395925280538));
#76501=CARTESIAN_POINT('Ctrl Pts',(77.945231494911,-8.92693857444419,138.391956781386));
#76502=CARTESIAN_POINT('Ctrl Pts',(77.9491695788627,-8.85340118457614,138.387988282233));
#76503=CARTESIAN_POINT('Ctrl Pts',(77.9570245321441,-8.7803439046172,138.384019783081));
#76504=CARTESIAN_POINT('Ctrl Pts',(77.9650800376502,-8.70542133030115,138.379949960432));
#76505=CARTESIAN_POINT('Ctrl Pts',(77.9772551019408,-8.63100421160297,138.375880137783));
#76506=CARTESIAN_POINT('Ctrl Pts',(77.9934509662018,-8.55755391575534,138.371810315134));
#76507=CARTESIAN_POINT('Ctrl Pts',(78.009290174775,-8.48572109862694,138.367830115698));
#76508=CARTESIAN_POINT('Ctrl Pts',(78.0289746941044,-8.41481336367742,138.363849916262));
#76509=CARTESIAN_POINT('Ctrl Pts',(78.0523617931341,-8.34524586472757,138.359869716826));
#76510=CARTESIAN_POINT('Ctrl Pts',(78.076538812492,-8.2733286608601,138.35575508257));
#76511=CARTESIAN_POINT('Ctrl Pts',(78.1046727995094,-8.20284433337413,138.351640448314));
#76512=CARTESIAN_POINT('Ctrl Pts',(78.1365533044576,-8.13422637175051,138.347525814058));
#76513=CARTESIAN_POINT('Ctrl Pts',(78.1684338094059,-8.06560841012688,138.343411179803));
#76514=CARTESIAN_POINT('Ctrl Pts',(78.2040605214212,-7.9988572326398,138.339296545547));
#76515=CARTESIAN_POINT('Ctrl Pts',(78.2431735357102,-7.93437420410772,138.335181911291));
#76516=CARTESIAN_POINT('Ctrl Pts',(78.2799523824106,-7.87373936262925,138.331312828192));
#76517=CARTESIAN_POINT('Ctrl Pts',(78.3199460624041,-7.81489206535987,138.327443745094));
#76518=CARTESIAN_POINT('Ctrl Pts',(78.3629553810999,-7.75819386447393,138.323574661995));
#76519=CARTESIAN_POINT('Ctrl Pts',(78.4059006180928,-7.70158014103087,138.319711343634));
#76520=CARTESIAN_POINT('Ctrl Pts',(78.4518522838164,-7.64710954187769,138.315848025273));
#76521=CARTESIAN_POINT('Ctrl Pts',(78.5005668004012,-7.5951165021822,138.311984706912));
#76522=CARTESIAN_POINT('Ctrl Pts',(78.54922417492,-7.54318445025606,138.308125920218));
#76523=CARTESIAN_POINT('Ctrl Pts',(78.600637632403,-7.49372453791673,138.304267133525));
#76524=CARTESIAN_POINT('Ctrl Pts',(78.6545231511768,-7.44703843840848,138.300408346831));
#76525=CARTESIAN_POINT('Ctrl Pts',(78.7083747260523,-7.4003817476959,138.296551990888));
#76526=CARTESIAN_POINT('Ctrl Pts',(78.7646949064437,-7.35649572054899,138.292695634945));
#76527=CARTESIAN_POINT('Ctrl Pts',(78.8231636749831,-7.31564438831321,138.288839279003));
#76528=CARTESIAN_POINT('Ctrl Pts',(78.8816151712853,-7.27480512395438,138.284984062264));
#76529=CARTESIAN_POINT('Ctrl Pts',(78.9422135976551,-7.23699905282433,138.281128845526));
#76530=CARTESIAN_POINT('Ctrl Pts',(79.0046081848307,-7.20244813794041,138.277273628788));
#76531=CARTESIAN_POINT('Ctrl Pts',(79.0670052114642,-7.16789587221007,138.273418261321));
#76532=CARTESIAN_POINT('Ctrl Pts',(79.1311981122825,-7.13659924880211,138.269562893855));
#76533=CARTESIAN_POINT('Ctrl Pts',(79.1968111603265,-7.10873448444593,138.265707526388));
#76534=CARTESIAN_POINT('Ctrl Pts',(79.2624928873308,-7.08084055328374,138.261848123404));
#76535=CARTESIAN_POINT('Ctrl Pts',(79.329597280913,-7.05638584232824,138.257988720419));
#76536=CARTESIAN_POINT('Ctrl Pts',(79.3977290916283,-7.03549820172414,138.254129317435));
#76537=CARTESIAN_POINT('Ctrl Pts',(79.4658994791117,-7.01459873437332,138.250267729226));
#76538=CARTESIAN_POINT('Ctrl Pts',(79.5350979703206,-6.99727047603946,138.246406141017));
#76539=CARTESIAN_POINT('Ctrl Pts',(79.6049173043764,-6.98359051130015,138.242544552808));
#76540=CARTESIAN_POINT('Ctrl Pts',(79.6748587898068,-6.96988661298257,138.238676208615));
#76541=CARTESIAN_POINT('Ctrl Pts',(79.7454228055971,-6.95984382020474,138.234807864422));
#76542=CARTESIAN_POINT('Ctrl Pts',(79.8161958231854,-6.95348745738378,138.230939520229));
#76543=CARTESIAN_POINT('Ctrl Pts',(79.8582187589169,-6.94971323614222,138.228642611253));
#76544=CARTESIAN_POINT('Ctrl Pts',(79.9003153380999,-6.94723771720572,138.226345702276));
#76545=CARTESIAN_POINT('Ctrl Pts',(79.9423993743177,-6.94605751530842,138.224048793299));
#76546=CARTESIAN_POINT('Ctrl Pts',(80.0132740183771,-6.9440699115302,138.220180518752));
#76547=CARTESIAN_POINT('Ctrl Pts',(80.08439044857,-6.94575118859824,138.216312244204));
#76548=CARTESIAN_POINT('Ctrl Pts',(80.155337132446,-6.95113008275697,138.212443969656));
#76549=CARTESIAN_POINT('Ctrl Pts',(80.2261854267694,-6.95650151741286,138.20858105967));
#76550=CARTESIAN_POINT('Ctrl Pts',(80.2968639617738,-6.96556035954378,138.204718149683));
#76551=CARTESIAN_POINT('Ctrl Pts',(80.3669597863483,-6.97828338343298,138.200855239696));
#76552=CARTESIAN_POINT('Ctrl Pts',(80.4369818596955,-6.99099302080975,138.196996394065));
#76553=CARTESIAN_POINT('Ctrl Pts',(80.5064219639399,-7.00735910187849,138.193137548434));
#76554=CARTESIAN_POINT('Ctrl Pts',(80.5748725845537,-7.0273066447041,138.189278702803));
#76555=CARTESIAN_POINT('Ctrl Pts',(80.6432814451583,-7.04724201803346,138.185422211356));
#76556=CARTESIAN_POINT('Ctrl Pts',(80.7107015541041,-7.07075438381265,138.18156571991));
#76557=CARTESIAN_POINT('Ctrl Pts',(80.7767374728927,-7.09771809115886,138.177709228464));
#76558=CARTESIAN_POINT('Ctrl Pts',(80.8427490507323,-7.12467185963791,138.173854158527));
#76559=CARTESIAN_POINT('Ctrl Pts',(80.9073770035231,-7.15507425641064,138.16999908859));
#76560=CARTESIAN_POINT('Ctrl Pts',(80.9702446392712,-7.18875101036175,138.166144018653));
#76561=CARTESIAN_POINT('Ctrl Pts',(81.0331314679084,-7.22243804550443,138.1622877718));
#76562=CARTESIAN_POINT('Ctrl Pts',(81.0942564769351,-7.25940120604435,138.158431524947));
#76563=CARTESIAN_POINT('Ctrl Pts',(81.1532675878582,-7.29942026552831,138.154575278094));
#76564=CARTESIAN_POINT('Ctrl Pts',(81.1868977428242,-7.32222693957645,138.152377621123));
#76565=CARTESIAN_POINT('Ctrl Pts',(81.2198418371831,-7.34602529029772,138.150179964153));
#76566=CARTESIAN_POINT('Ctrl Pts',(81.2520391107129,-7.37076839346111,138.147982307182));
#76567=CARTESIAN_POINT('',(77.9452502723122,-8.998942140427,138.454074719513));
#76568=CARTESIAN_POINT('Ctrl Pts',(77.9452502723127,-8.99894213949946,138.454074719462));
#76569=CARTESIAN_POINT('Ctrl Pts',(77.9452815714104,-8.93814791146918,138.450761929014));
#76570=CARTESIAN_POINT('Ctrl Pts',(77.9480107215814,-8.87742515330738,138.447449138566));
#76571=CARTESIAN_POINT('Ctrl Pts',(77.9534202484156,-8.8169456831852,138.444136348118));
#76572=CARTESIAN_POINT('Ctrl Pts',(77.95973816009,-8.74631030932362,138.440267263429));
#76573=CARTESIAN_POINT('Ctrl Pts',(77.9697295884145,-8.67586405616008,138.436398178741));
#76574=CARTESIAN_POINT('Ctrl Pts',(77.9833749153706,-8.60601925104963,138.432529094052));
#76575=CARTESIAN_POINT('Ctrl Pts',(77.9969999115456,-8.53627851082886,138.428665774085));
#76576=CARTESIAN_POINT('Ctrl Pts',(78.0142679075652,-8.46713791276437,138.424802454119));
#76577=CARTESIAN_POINT('Ctrl Pts',(78.0351074957963,-8.39900498386093,138.420939134152));
#76578=CARTESIAN_POINT('Ctrl Pts',(78.0559226393103,-8.33095197449105,138.417080345837));
#76579=CARTESIAN_POINT('Ctrl Pts',(78.0803009119579,-8.26390474873362,138.413221557523));
#76580=CARTESIAN_POINT('Ctrl Pts',(78.1081201674743,-8.19825923031046,138.409362769208));
#76581=CARTESIAN_POINT('Ctrl Pts',(78.1359218989831,-8.13265506355303,138.405506411635));
#76582=CARTESIAN_POINT('Ctrl Pts',(78.1671601238633,-8.06845129855351,138.401650054063));
#76583=CARTESIAN_POINT('Ctrl Pts',(78.2016638017234,-8.00602591559542,138.39779369649));
#76584=CARTESIAN_POINT('Ctrl Pts',(78.2361572869241,-7.94361897358904,138.393938478116));
#76585=CARTESIAN_POINT('Ctrl Pts',(78.2739140751586,-7.88298979559202,138.390083259742));
#76586=CARTESIAN_POINT('Ctrl Pts',(78.3147169905254,-7.82449213508538,138.386228041368));
#76587=CARTESIAN_POINT('Ctrl Pts',(78.3555215012133,-7.76599218742458,138.382372672262));
#76588=CARTESIAN_POINT('Ctrl Pts',(78.3993720957678,-7.70962431988504,138.378517303156));
#76589=CARTESIAN_POINT('Ctrl Pts',(78.4460090451571,-7.6557122053792,138.374661934049));
#76590=CARTESIAN_POINT('Ctrl Pts',(78.4926948106186,-7.60174365970214,138.370802529431));
#76591=CARTESIAN_POINT('Ctrl Pts',(78.5421724345315,-7.55023636649636,138.366943124813));
#76592=CARTESIAN_POINT('Ctrl Pts',(78.5941433605884,-7.50147917200917,138.363083720194));
#76593=CARTESIAN_POINT('Ctrl Pts',(78.6461437129704,-7.45269437083563,138.359222130352));
#76594=CARTESIAN_POINT('Ctrl Pts',(78.7006398065214,-7.40666308175431,138.35536054051));
#76595=CARTESIAN_POINT('Ctrl Pts',(78.7572999446834,-7.36363386278741,138.351498950668));
#76596=CARTESIAN_POINT('Ctrl Pts',(78.814059211424,-7.320529362936,138.347630604861));
#76597=CARTESIAN_POINT('Ctrl Pts',(78.8729896799775,-7.28043769271993,138.343762259054));
#76598=CARTESIAN_POINT('Ctrl Pts',(78.9337312323303,-7.24356369953473,138.339893913247));
#76599=CARTESIAN_POINT('Ctrl Pts',(78.9697975347749,-7.22166915553571,138.337597018874));
#76600=CARTESIAN_POINT('Ctrl Pts',(79.0065018723974,-7.20090815423955,138.3353001245));
#76601=CARTESIAN_POINT('Ctrl Pts',(79.0437653768922,-7.18131561064877,138.333003230127));
#76602=CARTESIAN_POINT('Ctrl Pts',(79.1065351778409,-7.14831227191436,138.329134146835));
#76603=CARTESIAN_POINT('Ctrl Pts',(79.171138534669,-7.11849774863183,138.325265063544));
#76604=CARTESIAN_POINT('Ctrl Pts',(79.2372183974205,-7.09207919732861,138.321395980252));
#76605=CARTESIAN_POINT('Ctrl Pts',(79.3031998047232,-7.06570000824887,138.317532661687));
#76606=CARTESIAN_POINT('Ctrl Pts',(79.3706529037847,-7.0427069264209,138.313669343122));
#76607=CARTESIAN_POINT('Ctrl Pts',(79.4391965878916,-7.02326099460056,138.309806024557));
#76608=CARTESIAN_POINT('Ctrl Pts',(79.5076598706248,-7.00383787275389,138.305947237644));
#76609=CARTESIAN_POINT('Ctrl Pts',(79.5772107323073,-6.98795376812263,138.30208845073));
#76610=CARTESIAN_POINT('Ctrl Pts',(79.647450294872,-6.97572080287472,138.298229663817));
#76611=CARTESIAN_POINT('Ctrl Pts',(79.7176456118739,-6.96349554346113,138.294373307645));
#76612=CARTESIAN_POINT('Ctrl Pts',(79.7885282916002,-6.95491694354026,138.290516951473));
#76613=CARTESIAN_POINT('Ctrl Pts',(79.859688011633,-6.9500463155426,138.286660595301));
#76614=CARTESIAN_POINT('Ctrl Pts',(79.9308267105698,-6.94517712636366,138.282805378325));
#76615=CARTESIAN_POINT('Ctrl Pts',(80.0022418029535,-6.94401376766526,138.278950161348));
#76616=CARTESIAN_POINT('Ctrl Pts',(80.0735182971014,-6.94656565176987,138.275094944372));
#76617=CARTESIAN_POINT('Ctrl Pts',(80.1447975781293,-6.94911763565204,138.271239576658));
#76618=CARTESIAN_POINT('Ctrl Pts',(80.2159377647695,-6.95538513115795,138.267384208944));
#76619=CARTESIAN_POINT('Ctrl Pts',(80.286526057035,-6.96532548520901,138.263528841231));
#76620=CARTESIAN_POINT('Ctrl Pts',(80.3571882361979,-6.97527624412885,138.259669437987));
#76621=CARTESIAN_POINT('Ctrl Pts',(80.4272968857762,-6.98890746818216,138.255810034744));
#76622=CARTESIAN_POINT('Ctrl Pts',(80.4964474056642,-7.00612499491335,138.2519506315));
#76623=CARTESIAN_POINT('Ctrl Pts',(80.5656370792465,-7.02335227037497,138.248089043025));
#76624=CARTESIAN_POINT('Ctrl Pts',(80.6338670783263,-7.04416974898001,138.24422745455));
#76625=CARTESIAN_POINT('Ctrl Pts',(80.7007486756555,-7.06843357451339,138.240365866075));
#76626=CARTESIAN_POINT('Ctrl Pts',(80.7677472848243,-7.09273985051112,138.236497521607));
#76627=CARTESIAN_POINT('Ctrl Pts',(80.8333923347223,-7.12050432223672,138.232629177139));
#76628=CARTESIAN_POINT('Ctrl Pts',(80.8973164056134,-7.15153554788925,138.228760832672));
#76629=CARTESIAN_POINT('Ctrl Pts',(80.9352726003762,-7.1699609583517,138.226463925826));
#76630=CARTESIAN_POINT('Ctrl Pts',(80.9726225197316,-7.18953722705832,138.224167018981));
#76631=CARTESIAN_POINT('Ctrl Pts',(81.0092940526334,-7.21021703052608,138.221870112135));
#76632=CARTESIAN_POINT('Ctrl Pts',(81.0710608673403,-7.24504856026857,138.218001372317));
#76633=CARTESIAN_POINT('Ctrl Pts',(81.1311434378208,-7.28314949063208,138.214132632499));
#76634=CARTESIAN_POINT('Ctrl Pts',(81.1891741648745,-7.3243322620236,138.210263892681));
#76635=CARTESIAN_POINT('Ctrl Pts',(81.2104094471644,-7.3394023433474,138.208848198163));
#76636=CARTESIAN_POINT('Ctrl Pts',(81.2313701776481,-7.35488464036548,138.207432503646));
#76637=CARTESIAN_POINT('Ctrl Pts',(81.2520391107129,-7.37076839346111,138.206016809128));
#76638=CARTESIAN_POINT('Ctrl Pts',(81.2520391107129,-7.37076839346111,138.906139397208));
#76639=CARTESIAN_POINT('Ctrl Pts',(81.3085407539465,-7.41418902614719,138.902270840233));
#76640=CARTESIAN_POINT('Ctrl Pts',(81.3627052412802,-7.46049401748224,138.898402283257));
#76641=CARTESIAN_POINT('Ctrl Pts',(81.4142409454556,-7.50938934973049,138.894533726281));
#76642=CARTESIAN_POINT('Ctrl Pts',(81.4402844264973,-7.53409852327941,138.892578757549));
#76643=CARTESIAN_POINT('Ctrl Pts',(81.465657188517,-7.55946864892284,138.890623788816));
#76644=CARTESIAN_POINT('Ctrl Pts',(81.4903255362227,-7.58545860485367,138.888668820084));
#76645=CARTESIAN_POINT('Ctrl Pts',(81.5391460717293,-7.63689470351241,138.884799788338));
#76646=CARTESIAN_POINT('Ctrl Pts',(81.5853962807173,-7.69096197875137,138.880930756591));
#76647=CARTESIAN_POINT('Ctrl Pts',(81.6287797614883,-7.74737313973151,138.877061724845));
#76648=CARTESIAN_POINT('Ctrl Pts',(81.6720985929598,-7.80370023779242,138.873198458661));
#76649=CARTESIAN_POINT('Ctrl Pts',(81.7125588821633,-7.86236390650683,138.869335192478));
#76650=CARTESIAN_POINT('Ctrl Pts',(81.7499020657528,-7.92304116941539,138.865471926294));
#76651=CARTESIAN_POINT('Ctrl Pts',(81.7872014358446,-7.98364724173804,138.86161319275));
#76652=CARTESIAN_POINT('Ctrl Pts',(81.8213907113594,-8.04626180385324,138.857754459207));
#76653=CARTESIAN_POINT('Ctrl Pts',(81.8522535771044,-8.11053147970038,138.853895725663));
#76654=CARTESIAN_POINT('Ctrl Pts',(81.8830969966853,-8.17476066032353,138.850039423442));
#76655=CARTESIAN_POINT('Ctrl Pts',(81.9106179549556,-8.24064244877835,138.84618312122));
#76656=CARTESIAN_POINT('Ctrl Pts',(81.9346459227277,-8.3077986447766,138.842326818998));
#76657=CARTESIAN_POINT('Ctrl Pts',(81.9586667892483,-8.37493499336037,138.838471656473));
#76658=CARTESIAN_POINT('Ctrl Pts',(81.9791965511485,-8.44334454460101,138.834616493947));
#76659=CARTESIAN_POINT('Ctrl Pts',(81.9961133562055,-8.51263049779648,138.830761331421));
#76660=CARTESIAN_POINT('Ctrl Pts',(82.0130308208679,-8.58191915252996,138.826906018578));
#76661=CARTESIAN_POINT('Ctrl Pts',(82.0263349359147,-8.6520838046047,138.823050705735));
#76662=CARTESIAN_POINT('Ctrl Pts',(82.0359545500872,-8.72271561082636,138.819195392892));
#76663=CARTESIAN_POINT('Ctrl Pts',(82.0455842328843,-8.79342134570424,138.815336044783));
#76664=CARTESIAN_POINT('Ctrl Pts',(82.0515216507147,-8.86459472846081,138.811476696675));
#76665=CARTESIAN_POINT('Ctrl Pts',(82.0537474512825,-8.93582080671598,138.807617348566));
#76666=CARTESIAN_POINT('Ctrl Pts',(82.0559745120042,-9.00708721015571,138.803755815458));
#76667=CARTESIAN_POINT('Ctrl Pts',(82.0544857824498,-9.07840588256192,138.79989428235));
#76668=CARTESIAN_POINT('Ctrl Pts',(82.0493140475513,-9.14936364018326,138.796032749242));
#76669=CARTESIAN_POINT('Ctrl Pts',(82.0441332640688,-9.22044554709946,138.792164459909));
#76670=CARTESIAN_POINT('Ctrl Pts',(82.0352566703983,-9.29116479632561,138.788296170576));
#76671=CARTESIAN_POINT('Ctrl Pts',(82.0227686370176,-9.36111577589204,138.784427881242));
#76672=CARTESIAN_POINT('Ctrl Pts',(82.0153519422922,-9.40265995225419,138.782130488192));
#76673=CARTESIAN_POINT('Ctrl Pts',(82.006662387559,-9.44393336415556,138.779833095143));
#76674=CARTESIAN_POINT('Ctrl Pts',(81.9967259333069,-9.48485369933577,138.777535702093));
#76675=CARTESIAN_POINT('Ctrl Pts',(81.979991708908,-9.55376863156547,138.773666606553));
#76676=CARTESIAN_POINT('Ctrl Pts',(81.9596527303735,-9.62195117122628,138.769797511013));
#76677=CARTESIAN_POINT('Ctrl Pts',(81.9357896130199,-9.68899647069068,138.765928415473));
#76678=CARTESIAN_POINT('Ctrl Pts',(81.9119620497925,-9.75594187804965,138.762065084575));
#76679=CARTESIAN_POINT('Ctrl Pts',(81.884620931774,-9.821752954616,138.758201753676));
#76680=CARTESIAN_POINT('Ctrl Pts',(81.8538973773168,-9.88603728864983,138.754338422778));
#76681=CARTESIAN_POINT('Ctrl Pts',(81.82320986079,-9.9502462188316,138.750479623466));
#76682=CARTESIAN_POINT('Ctrl Pts',(81.7891479971028,-10.0129315275076,138.746620824154));
#76683=CARTESIAN_POINT('Ctrl Pts',(81.7518913583523,-10.0737198102999,138.742762024842));
#76684=CARTESIAN_POINT('Ctrl Pts',(81.7146581880431,-10.1344698017623,138.738905656238));
#76685=CARTESIAN_POINT('Ctrl Pts',(81.6742344885484,-10.1933247249269,138.735049287634));
#76686=CARTESIAN_POINT('Ctrl Pts',(81.6308455204021,-10.2499361788045,138.73119291903));
#76687=CARTESIAN_POINT('Ctrl Pts',(81.5874693694662,-10.306530909516,138.727337689607));
#76688=CARTESIAN_POINT('Ctrl Pts',(81.5411299842249,-10.3608831012861,138.723482460184));
#76689=CARTESIAN_POINT('Ctrl Pts',(81.4920946528018,-10.4126751606722,138.719627230761));
#76690=CARTESIAN_POINT('Ctrl Pts',(81.4430574041797,-10.4644692450408,138.715771850605));
#76691=CARTESIAN_POINT('Ctrl Pts',(81.3913243356852,-10.5137026470529,138.711916470449));
#76692=CARTESIAN_POINT('Ctrl Pts',(81.3372003513379,-10.560093837845,138.708061090293));
#76693=CARTESIAN_POINT('Ctrl Pts',(81.2830197152762,-10.6065335864164,138.7042016747));
#76694=CARTESIAN_POINT('Ctrl Pts',(81.226443537245,-10.6501248683155,138.700342259108));
#76695=CARTESIAN_POINT('Ctrl Pts',(81.1678099480159,-10.6906263596121,138.696482843515));
#76696=CARTESIAN_POINT('Ctrl Pts',(81.1091431605051,-10.731150782814,138.692621242726));
#76697=CARTESIAN_POINT('Ctrl Pts',(81.0484170565591,-10.7685816778062,138.688759641936));
#76698=CARTESIAN_POINT('Ctrl Pts',(80.9859965589404,-10.8027224823188,138.684898041146));
#76699=CARTESIAN_POINT('Ctrl Pts',(80.9234668577401,-10.8369230155788,138.681029684552));
#76700=CARTESIAN_POINT('Ctrl Pts',(80.8592372824306,-10.8678217557705,138.677161327959));
#76701=CARTESIAN_POINT('Ctrl Pts',(80.7936943731894,-10.8952695862245,138.673292971365));
#76702=CARTESIAN_POINT('Ctrl Pts',(80.7547789650431,-10.9115664448353,138.670996175611));
#76703=CARTESIAN_POINT('Ctrl Pts',(80.7154009145431,-10.9266477050085,138.668699379856));
#76704=CARTESIAN_POINT('Ctrl Pts',(80.6756433883521,-10.9404905499064,138.666402584101));
#76705=CARTESIAN_POINT('Ctrl Pts',(80.6086694833266,-10.963809641115,138.662533495768));
#76706=CARTESIAN_POINT('Ctrl Pts',(80.5403557402951,-10.9837030370275,138.658664407435));
#76707=CARTESIAN_POINT('Ctrl Pts',(80.4710860079057,-11.0000188838247,138.654795319102));
#76708=CARTESIAN_POINT('Ctrl Pts',(80.401919481237,-11.016310421466,138.650931995365));
#76709=CARTESIAN_POINT('Ctrl Pts',(80.3318002614742,-11.0290348798839,138.647068671628));
#76710=CARTESIAN_POINT('Ctrl Pts',(80.2611291413822,-11.0380895794888,138.643205347892));
#76711=CARTESIAN_POINT('Ctrl Pts',(80.1905409149407,-11.0471336583889,138.639346555638));
#76712=CARTESIAN_POINT('Ctrl Pts',(80.1194025535331,-11.0525164671184,138.635487763385));
#76713=CARTESIAN_POINT('Ctrl Pts',(80.0481251616243,-11.0541863428907,138.631628971132));
#76714=CARTESIAN_POINT('Ctrl Pts',(79.9768926670995,-11.055855166814,138.627772609519));
#76715=CARTESIAN_POINT('Ctrl Pts',(79.905521800321,-11.0538156865004,138.623916247905));
#76716=CARTESIAN_POINT('Ctrl Pts',(79.8344274401024,-11.0480681848779,138.620059886292));
#76717=CARTESIAN_POINT('Ctrl Pts',(79.763354079924,-11.0423223809676,138.616204663781));
#76718=CARTESIAN_POINT('Ctrl Pts',(79.6925575480956,-11.0328707693168,138.61234944127));
#76719=CARTESIAN_POINT('Ctrl Pts',(79.6224496359158,-11.0197656510298,138.608494218759));
#76720=CARTESIAN_POINT('Ctrl Pts',(79.552338981,-11.0066600200492,138.604638845425));
#76721=CARTESIAN_POINT('Ctrl Pts',(79.4829174763242,-10.9899006900868,138.600783472092));
#76722=CARTESIAN_POINT('Ctrl Pts',(79.4145870162218,-10.9695911253161,138.596928098758));
#76723=CARTESIAN_POINT('Ctrl Pts',(79.3461850310351,-10.9492603014564,138.593068689802));
#76724=CARTESIAN_POINT('Ctrl Pts',(79.2788768368191,-10.9253719630721,138.589209280847));
#76725=CARTESIAN_POINT('Ctrl Pts',(79.2130485719069,-10.8980792955834,138.585349871891));
#76726=CARTESIAN_POINT('Ctrl Pts',(79.1471830334149,-10.8707711743162,138.581488277644));
#76727=CARTESIAN_POINT('Ctrl Pts',(79.0827995310201,-10.8400550959288,138.577626683396));
#76728=CARTESIAN_POINT('Ctrl Pts',(79.0202611286595,-10.8061310324792,138.573765089148));
#76729=CARTESIAN_POINT('Ctrl Pts',(78.9576133126571,-10.7721476174122,138.569896738874));
#76730=CARTESIAN_POINT('Ctrl Pts',(78.8968174561364,-10.7349452653864,138.5660283886));
#76731=CARTESIAN_POINT('Ctrl Pts',(78.8382084871952,-10.6947678434744,138.562160038327));
#76732=CARTESIAN_POINT('Ctrl Pts',(78.8034090417435,-10.670912245475,138.559863180921));
#76733=CARTESIAN_POINT('Ctrl Pts',(78.7693799732322,-10.6460085938022,138.557566323515));
#76734=CARTESIAN_POINT('Ctrl Pts',(78.7361855638824,-10.6201143890358,138.55526946611));
#76735=CARTESIAN_POINT('Ctrl Pts',(78.6809217159353,-10.5770043164979,138.551445533679));
#76736=CARTESIAN_POINT('Ctrl Pts',(78.6277456593305,-10.5309690669994,138.547621601249));
#76737=CARTESIAN_POINT('Ctrl Pts',(78.5769890148234,-10.4822406345013,138.543797668819));
#76738=CARTESIAN_POINT('Ctrl Pts',(78.5263187089004,-10.4335950905374,138.539980241013));
#76739=CARTESIAN_POINT('Ctrl Pts',(78.4780599997091,-10.3822658016579,138.536162813207));
#76740=CARTESIAN_POINT('Ctrl Pts',(78.4325126206117,-10.3285258288638,138.532345385401));
#76741=CARTESIAN_POINT('Ctrl Pts',(78.3870085971723,-10.2748370100972,138.52853159133));
#76742=CARTESIAN_POINT('Ctrl Pts',(78.3442111089203,-10.2187424334804,138.524717797259));
#76743=CARTESIAN_POINT('Ctrl Pts',(78.3043830641576,-10.1605519244671,138.520904003188));
#76744=CARTESIAN_POINT('Ctrl Pts',(78.2645788526164,-10.102396236829,138.517092491303));
#76745=CARTESIAN_POINT('Ctrl Pts',(78.2277408418242,-10.0421475141073,138.513280979417));
#76746=CARTESIAN_POINT('Ctrl Pts',(78.1940904592992,-9.98014707738473,138.509469467532));
#76747=CARTESIAN_POINT('Ctrl Pts',(78.1604483206664,-9.91816182993723,138.505658889416));
#76748=CARTESIAN_POINT('Ctrl Pts',(78.1299924973061,-9.85442615832262,138.5018483113));
#76749=CARTESIAN_POINT('Ctrl Pts',(78.1028990537304,-9.78930701388173,138.498037733184));
#76750=CARTESIAN_POINT('Ctrl Pts',(78.0757855811533,-9.72413972969709,138.494224338074));
#76751=CARTESIAN_POINT('Ctrl Pts',(78.0520396486506,-9.6575873893915,138.490410942963));
#76752=CARTESIAN_POINT('Ctrl Pts',(78.0317891516039,-9.59003696388962,138.486597547853));
#76753=CARTESIAN_POINT('Ctrl Pts',(78.0115315638732,-9.52246288569773,138.482782817488));
#76754=CARTESIAN_POINT('Ctrl Pts',(77.994771969706,-9.45389051055339,138.478968087122));
#76755=CARTESIAN_POINT('Ctrl Pts',(77.9815875950891,-9.38471928233684,138.475153356757));
#76756=CARTESIAN_POINT('Ctrl Pts',(77.9683814173209,-9.31543366486841,138.471332317928));
#76757=CARTESIAN_POINT('Ctrl Pts',(77.9587623379457,-9.24554771071851,138.4675112791));
#76758=CARTESIAN_POINT('Ctrl Pts',(77.9527558266144,-9.17546753841907,138.463690240271));
#76759=CARTESIAN_POINT('Ctrl Pts',(77.9477174293809,-9.11668270862904,138.460485066685));
#76760=CARTESIAN_POINT('Ctrl Pts',(77.9452199900004,-9.05776145210071,138.457279893099));
#76761=CARTESIAN_POINT('Ctrl Pts',(77.9452502723122,-8.998942140427,138.454074719513));
#76762=CARTESIAN_POINT('Origin',(80.,-9.,141.545925280538));
#76763=CARTESIAN_POINT('',(81.2520391107129,-7.37076839346112,139.606097362913));
#76764=CARTESIAN_POINT('',(81.2520391107129,-7.37076839346111,139.547882946156));
#76765=CARTESIAN_POINT('',(81.2520391107129,-7.37076839346111,141.545925280538));
#76766=CARTESIAN_POINT('',(77.9455903633547,-9.00215277156236,139.85407487124));
#76767=CARTESIAN_POINT('Ctrl Pts',(77.9452511251707,-9.00215032272264,139.854074719462));
#76768=CARTESIAN_POINT('Ctrl Pts',(77.9451772141952,-8.93152441513387,139.850255486395));
#76769=CARTESIAN_POINT('Ctrl Pts',(77.9487489191035,-8.8608346373683,139.846436253328));
#76770=CARTESIAN_POINT('Ctrl Pts',(77.9559591751019,-8.79048945456173,139.842617020261));
#76771=CARTESIAN_POINT('Ctrl Pts',(77.9631670371951,-8.72016762733346,139.838799055232));
#76772=CARTESIAN_POINT('Ctrl Pts',(77.9740110032964,-8.65019066081581,139.834981090203));
#76773=CARTESIAN_POINT('Ctrl Pts',(77.9884320510566,-8.58096306930816,139.831163125175));
#76774=CARTESIAN_POINT('Ctrl Pts',(78.0028533540946,-8.51173425235067,139.827345092561));
#76775=CARTESIAN_POINT('Ctrl Pts',(78.0208517611104,-8.44325532150668,139.823527059948));
#76776=CARTESIAN_POINT('Ctrl Pts',(78.042317286345,-8.3759199128665,139.819709027335));
#76777=CARTESIAN_POINT('Ctrl Pts',(78.0638059335618,-8.3085119726624,139.815886882058));
#76778=CARTESIAN_POINT('Ctrl Pts',(78.0887690027399,-8.24225048659746,139.812064736781));
#76779=CARTESIAN_POINT('Ctrl Pts',(78.117047128281,-8.17751228253237,139.808242591504));
#76780=CARTESIAN_POINT('Ctrl Pts',(78.1453414305068,-8.11273704455875,139.804418259744));
#76781=CARTESIAN_POINT('Ctrl Pts',(78.1769543394074,-8.04948726524998,139.800593927984));
#76782=CARTESIAN_POINT('Ctrl Pts',(78.211680274969,-7.988115558196,139.796769596225));
#76783=CARTESIAN_POINT('Ctrl Pts',(78.246470364294,-7.92663047115926,139.792938199277));
#76784=CARTESIAN_POINT('Ctrl Pts',(78.2843846938144,-7.86703080006613,139.789106802328));
#76785=CARTESIAN_POINT('Ctrl Pts',(78.3251745145668,-7.80963990496851,139.78527540538));
#76786=CARTESIAN_POINT('Ctrl Pts',(78.3519377903433,-7.77198422705121,139.782761524926));
#76787=CARTESIAN_POINT('Ctrl Pts',(78.3799381149203,-7.73527877551538,139.780247644471));
#76788=CARTESIAN_POINT('Ctrl Pts',(78.4090964455802,-7.69960642764035,139.777733764017));
#76789=CARTESIAN_POINT('Ctrl Pts',(78.4539904848238,-7.64468298898069,139.773863232157));
#76790=CARTESIAN_POINT('Ctrl Pts',(78.5018203572766,-7.59197912134451,139.769992700298));
#76791=CARTESIAN_POINT('Ctrl Pts',(78.5523383786184,-7.54182532168506,139.766122168439));
#76792=CARTESIAN_POINT('Ctrl Pts',(78.6027804379957,-7.49174693632431,139.762257456547));
#76793=CARTESIAN_POINT('Ctrl Pts',(78.6559022811376,-7.44421134674237,139.758392744654));
#76794=CARTESIAN_POINT('Ctrl Pts',(78.7114160407119,-7.39951602870717,139.754528032762));
#76795=CARTESIAN_POINT('Ctrl Pts',(78.766863418076,-7.35487415641255,139.750667942212));
#76796=CARTESIAN_POINT('Ctrl Pts',(78.8246966540222,-7.3130661119175,139.746807851663));
#76797=CARTESIAN_POINT('Ctrl Pts',(78.8845923882131,-7.27435130398223,139.742947761113));
#76798=CARTESIAN_POINT('Ctrl Pts',(78.9444495327706,-7.23566143922973,139.739090157544));
#76799=CARTESIAN_POINT('Ctrl Pts',(79.0063661324868,-7.20006111986884,139.735232553974));
#76800=CARTESIAN_POINT('Ctrl Pts',(79.0699884040452,-7.16776748367202,139.731374950404));
#76801=CARTESIAN_POINT('Ctrl Pts',(79.1335909260111,-7.13548387204895,139.72751854431));
#76802=CARTESIAN_POINT('Ctrl Pts',(79.198897636093,-7.10650512532283,139.723662138215));
#76803=CARTESIAN_POINT('Ctrl Pts',(79.2655301301099,-7.0810024563008,139.719805732121));
#76804=CARTESIAN_POINT('Ctrl Pts',(79.3321641853529,-7.05549918974097,139.715949235669));
#76805=CARTESIAN_POINT('Ctrl Pts',(79.4001236321068,-7.0334723340365,139.712092739217));
#76806=CARTESIAN_POINT('Ctrl Pts',(79.4690116881436,-7.01504433924285,139.708236242766));
#76807=CARTESIAN_POINT('Ctrl Pts',(79.5379700295608,-6.9965975426612,139.704375811593));
#76808=CARTESIAN_POINT('Ctrl Pts',(79.6078584017997,-6.98175706283591,139.700515380419));
#76809=CARTESIAN_POINT('Ctrl Pts',(79.6782673968351,-6.97059474363528,139.696654949246));
#76810=CARTESIAN_POINT('Ctrl Pts',(79.7487152375011,-6.95942626602652,139.692792388219));
#76811=CARTESIAN_POINT('Ctrl Pts',(79.8196837898523,-6.9519400401992,139.688929827192));
#76812=CARTESIAN_POINT('Ctrl Pts',(79.8907587707328,-6.94815597173465,139.685067266165));
#76813=CARTESIAN_POINT('Ctrl Pts',(79.9619562493202,-6.94436538142931,139.681198048015));
#76814=CARTESIAN_POINT('Ctrl Pts',(80.0332600370826,-6.94428968860846,139.677328829865));
#76815=CARTESIAN_POINT('Ctrl Pts',(80.1042568089757,-6.94789666919957,139.673459611715));
#76816=CARTESIAN_POINT('Ctrl Pts',(80.1462088178506,-6.95002803486219,139.671173289818));
#76817=CARTESIAN_POINT('Ctrl Pts',(80.1880537235075,-6.95344426405484,139.668886967922));
#76818=CARTESIAN_POINT('Ctrl Pts',(80.2297077973158,-6.95813029545166,139.666600646025));
#76819=CARTESIAN_POINT('Ctrl Pts',(80.3003043866995,-6.96607232378442,139.662725718236));
#76820=CARTESIAN_POINT('Ctrl Pts',(80.3706220099204,-6.97769490534872,139.658850790447));
#76821=CARTESIAN_POINT('Ctrl Pts',(80.4402478318877,-6.99296751171832,139.654975862658));
#76822=CARTESIAN_POINT('Ctrl Pts',(80.5097766496484,-7.00821883996117,139.651106333502));
#76823=CARTESIAN_POINT('Ctrl Pts',(80.5786151099305,-7.02710999796615,139.647236804346));
#76824=CARTESIAN_POINT('Ctrl Pts',(80.6463564866655,-7.04955880513012,139.643367275191));
#76825=CARTESIAN_POINT('Ctrl Pts',(80.7140192485418,-7.07198156012497,139.63950223668));
#76826=CARTESIAN_POINT('Ctrl Pts',(80.7805869991265,-7.09795360980493,139.63563719817));
#76827=CARTESIAN_POINT('Ctrl Pts',(80.8456659697587,-7.12734236175106,139.631772159659));
#76828=CARTESIAN_POINT('Ctrl Pts',(80.9107019062309,-7.15671168007311,139.627909676947));
#76829=CARTESIAN_POINT('Ctrl Pts',(80.9742505775629,-7.18949301568476,139.624047194234));
#76830=CARTESIAN_POINT('Ctrl Pts',(81.0359374810629,-7.22550539650608,139.620184711521));
#76831=CARTESIAN_POINT('Ctrl Pts',(81.0976087027791,-7.2615086224122,139.616323210713));
#76832=CARTESIAN_POINT('Ctrl Pts',(81.1574186781938,-7.30074101982408,139.612461709904));
#76833=CARTESIAN_POINT('Ctrl Pts',(81.2150182692663,-7.34297611126178,139.608600209095));
#76834=CARTESIAN_POINT('Ctrl Pts',(81.2274627326795,-7.35210105538665,139.607765927035));
#76835=CARTESIAN_POINT('Ctrl Pts',(81.2398041258756,-7.3613659982008,139.606931644974));
#76836=CARTESIAN_POINT('Ctrl Pts',(81.2520391107129,-7.37076839346111,139.606097362913));
#76837=CARTESIAN_POINT('',(79.4698297828115,-10.9851743256717,140.));
#76838=CARTESIAN_POINT('Ctrl Pts',(79.4698297828115,-10.9851743256717,140.));
#76839=CARTESIAN_POINT('Ctrl Pts',(78.809740437582,-10.8088876857538,139.962955627336));
#76840=CARTESIAN_POINT('Ctrl Pts',(78.075115219758,-10.1125316678232,139.914314179016));
#76841=CARTESIAN_POINT('Ctrl Pts',(77.945732886822,-9.21640413993257,139.865672730697));
#76842=CARTESIAN_POINT('Ctrl Pts',(77.947342226875,-9.00216541764168,139.85407565504));
#76843=CARTESIAN_POINT('',(80.5303700197491,-10.9851209546653,139.99999999143));
#76844=CARTESIAN_POINT('Origin',(80.,-9.,140.));
#76845=CARTESIAN_POINT('',(77.9452505498836,-8.99849675473629,139.795925280583));
#76846=CARTESIAN_POINT('Ctrl Pts',(80.5303700197491,-10.9851209546653,139.99999999143));
#76847=CARTESIAN_POINT('Ctrl Pts',(80.4620741507688,-11.0033677427488,139.996143015247));
#76848=CARTESIAN_POINT('Ctrl Pts',(80.3926968367418,-11.0181229590247,139.992286039064));
#76849=CARTESIAN_POINT('Ctrl Pts',(80.322629557872,-11.0292628540648,139.988429062881));
#76850=CARTESIAN_POINT('Ctrl Pts',(80.2526675158343,-11.0403860176536,139.984577879644));
#76851=CARTESIAN_POINT('Ctrl Pts',(80.182018044633,-11.0479045602196,139.980726696407));
#76852=CARTESIAN_POINT('Ctrl Pts',(80.1110860698619,-11.0517449762538,139.976875513169));
#76853=CARTESIAN_POINT('Ctrl Pts',(80.0402379061024,-11.055580854572,139.97302888037));
#76854=CARTESIAN_POINT('Ctrl Pts',(79.9691083877808,-11.055747211313,139.969182247571));
#76855=CARTESIAN_POINT('Ctrl Pts',(79.8981090915934,-11.0522221627504,139.965335614772));
#76856=CARTESIAN_POINT('Ctrl Pts',(79.8271544971697,-11.0486993335886,139.961491403846));
#76857=CARTESIAN_POINT('Ctrl Pts',(79.7563304496936,-11.0414897336107,139.95764719292));
#76858=CARTESIAN_POINT('Ctrl Pts',(79.6860485460449,-11.0306235611406,139.953802981993));
#76859=CARTESIAN_POINT('Ctrl Pts',(79.6157869882531,-11.0197605343108,139.949959883925));
#76860=CARTESIAN_POINT('Ctrl Pts',(79.5460677459476,-11.0052431110503,139.946116785857));
#76861=CARTESIAN_POINT('Ctrl Pts',(79.4772955407152,-10.9871531422474,139.942273687788));
#76862=CARTESIAN_POINT('Ctrl Pts',(79.4085198539763,-10.9690622576626,139.938430395168));
#76863=CARTESIAN_POINT('Ctrl Pts',(79.3406917719253,-10.9473985954838,139.934587102547));
#76864=CARTESIAN_POINT('Ctrl Pts',(79.2742023673069,-10.922294295595,139.930743809927));
#76865=CARTESIAN_POINT('Ctrl Pts',(79.2076443016715,-10.897164071474,139.926896548488));
#76866=CARTESIAN_POINT('Ctrl Pts',(79.1424281306179,-10.8685862925332,139.923049287049));
#76867=CARTESIAN_POINT('Ctrl Pts',(79.0789254608646,-10.8367414776872,139.91920202561));
#76868=CARTESIAN_POINT('Ctrl Pts',(79.0153854805086,-10.8048779526163,139.915352503736));
#76869=CARTESIAN_POINT('Ctrl Pts',(78.953561429991,-10.7697438138146,139.911502981863));
#76870=CARTESIAN_POINT('Ctrl Pts',(78.893798374401,-10.7315644735389,139.907653459989));
#76871=CARTESIAN_POINT('Ctrl Pts',(78.8339351963667,-10.6933211705219,139.903797488921));
#76872=CARTESIAN_POINT('Ctrl Pts',(78.7761403009812,-10.6520227697349,139.899941517853));
#76873=CARTESIAN_POINT('Ctrl Pts',(78.7207272530863,-10.6079361932315,139.896085546786));
#76874=CARTESIAN_POINT('Ctrl Pts',(78.6965845362067,-10.5887282670274,139.894405552248));
#76875=CARTESIAN_POINT('Ctrl Pts',(78.6728934890379,-10.5689915700536,139.89272555771));
#76876=CARTESIAN_POINT('Ctrl Pts',(78.6496778127435,-10.5487503198072,139.891045563173));
#76877=CARTESIAN_POINT('Ctrl Pts',(78.594908743558,-10.5009983430355,139.887082218065));
#76878=CARTESIAN_POINT('Ctrl Pts',(78.5425524721368,-10.4502296884911,139.883118872957));
#76879=CARTESIAN_POINT('Ctrl Pts',(78.4929635830642,-10.3967243108536,139.879155527849));
#76880=CARTESIAN_POINT('Ctrl Pts',(78.4452783531287,-10.3452729417435,139.875344330899));
#76881=CARTESIAN_POINT('Ctrl Pts',(78.400152313208,-10.2912915243667,139.871533133949));
#76882=CARTESIAN_POINT('Ctrl Pts',(78.3578674259957,-10.2350701080886,139.867721936999));
#76883=CARTESIAN_POINT('Ctrl Pts',(78.3156213067393,-10.1789002371624,139.86391423426));
#76884=CARTESIAN_POINT('Ctrl Pts',(78.2762114760096,-10.1204948355065,139.860106531521));
#76885=CARTESIAN_POINT('Ctrl Pts',(78.2398808613688,-10.0601783719376,139.856298828782));
#76886=CARTESIAN_POINT('Ctrl Pts',(78.2035706331938,-9.99989575419088,139.852493262687));
#76887=CARTESIAN_POINT('Ctrl Pts',(78.1703364516158,-9.93770462878445,139.848687696592));
#76888=CARTESIAN_POINT('Ctrl Pts',(78.1403778803837,-9.87395831407092,139.844882130498));
#76889=CARTESIAN_POINT('Ctrl Pts',(78.1104254664197,-9.81022510088838,139.841077346546));
#76890=CARTESIAN_POINT('Ctrl Pts',(78.0837475373579,-9.74493778587895,139.837272562595));
#76891=CARTESIAN_POINT('Ctrl Pts',(78.0604967798146,-9.67847241756049,139.833467778643));
#76892=CARTESIAN_POINT('Ctrl Pts',(78.0372308347851,-9.6119636338024,139.829660509392));
#76893=CARTESIAN_POINT('Ctrl Pts',(78.0173966958587,-9.54427573298083,139.82585324014));
#76894=CARTESIAN_POINT('Ctrl Pts',(78.0010976872857,-9.47580154132315,139.822045970889));
#76895=CARTESIAN_POINT('Ctrl Pts',(77.9847922388687,-9.4073002950685,139.818237197361));
#76896=CARTESIAN_POINT('Ctrl Pts',(77.9720247926029,-9.33801263115874,139.814428423833));
#76897=CARTESIAN_POINT('Ctrl Pts',(77.962847357618,-9.26834059352989,139.810619650305));
#76898=CARTESIAN_POINT('Ctrl Pts',(77.9536577730378,-9.19857632020982,139.806805834512));
#76899=CARTESIAN_POINT('Ctrl Pts',(77.9480677192538,-9.12842715583003,139.802992018719));
#76900=CARTESIAN_POINT('Ctrl Pts',(77.9460771917355,-9.05829802904844,139.799178202926));
#76901=CARTESIAN_POINT('Ctrl Pts',(77.9455112640845,-9.03835958980393,139.798093895478));
#76902=CARTESIAN_POINT('Ctrl Pts',(77.9452359721152,-9.01842275238194,139.79700958803));
#76903=CARTESIAN_POINT('Ctrl Pts',(77.9452505498836,-8.99849675473629,139.795925280583));
#76904=CARTESIAN_POINT('Ctrl Pts',(77.9452505498842,-8.9984967539153,139.795925280538));
#76905=CARTESIAN_POINT('Ctrl Pts',(77.9453223104453,-8.90040903895431,139.790587668752));
#76906=CARTESIAN_POINT('Ctrl Pts',(77.9524183451655,-8.80257549275452,139.785250056967));
#76907=CARTESIAN_POINT('Ctrl Pts',(77.9664267198136,-8.70575983175005,139.779912445181));
#76908=CARTESIAN_POINT('Ctrl Pts',(77.976571754963,-8.63564475354966,139.776046881864));
#76909=CARTESIAN_POINT('Ctrl Pts',(77.9903674947664,-8.56591523418777,139.772181318546));
#76910=CARTESIAN_POINT('Ctrl Pts',(78.0077726664933,-8.49698129843022,139.768315755229));
#76911=CARTESIAN_POINT('Ctrl Pts',(78.0251516536356,-8.4281510678534,139.764456007319));
#76912=CARTESIAN_POINT('Ctrl Pts',(78.0461291766953,-8.36011451330124,139.760596259409));
#76913=CARTESIAN_POINT('Ctrl Pts',(78.0706124987683,-8.29327414608565,139.756736511499));
#76914=CARTESIAN_POINT('Ctrl Pts',(78.0950667072662,-8.22651325999793,139.752881353288));
#76915=CARTESIAN_POINT('Ctrl Pts',(78.1230182678931,-8.16094619082245,139.749026195076));
#76916=CARTESIAN_POINT('Ctrl Pts',(78.1543243910515,-8.09696118077206,139.745171036865));
#76917=CARTESIAN_POINT('Ctrl Pts',(78.1856104997258,-8.0330170773187,139.741318343315));
#76918=CARTESIAN_POINT('Ctrl Pts',(78.2202467029164,-7.9706534626749,139.737465649765));
#76919=CARTESIAN_POINT('Ctrl Pts',(78.2580423382098,-7.91023806864503,139.733612956215));
#76920=CARTESIAN_POINT('Ctrl Pts',(78.295826518032,-7.84984098590428,139.729761430377));
#76921=CARTESIAN_POINT('Ctrl Pts',(78.3367679709835,-7.79139136406186,139.72590990454));
#76922=CARTESIAN_POINT('Ctrl Pts',(78.3806312563075,-7.73523028402328,139.722058378702));
#76923=CARTESIAN_POINT('Ctrl Pts',(78.4244959947189,-7.67906734350036,139.718206725272));
#76924=CARTESIAN_POINT('Ctrl Pts',(78.471282456273,-7.62519347759648,139.714355071842));
#76925=CARTESIAN_POINT('Ctrl Pts',(78.5207143194315,-7.57391745057829,139.710503418413));
#76926=CARTESIAN_POINT('Ctrl Pts',(78.5701978474364,-7.52258783124362,139.706647739339));
#76927=CARTESIAN_POINT('Ctrl Pts',(78.6223319578652,-7.473861822142,139.702792060265));
#76928=CARTESIAN_POINT('Ctrl Pts',(78.6768034311584,-7.42801132233532,139.698936381191));
#76929=CARTESIAN_POINT('Ctrl Pts',(78.7313056172835,-7.38213497048893,139.695078528157));
#76930=CARTESIAN_POINT('Ctrl Pts',(78.7881474011765,-7.33913764908114,139.691220675123));
#76931=CARTESIAN_POINT('Ctrl Pts',(78.8469846502084,-7.29924923470695,139.687362822089));
#76932=CARTESIAN_POINT('Ctrl Pts',(78.9059252833125,-7.25929073162568,139.683498190347));
#76933=CARTESIAN_POINT('Ctrl Pts',(78.9668679650895,-7.222452293824,139.679633558604));
#76934=CARTESIAN_POINT('Ctrl Pts',(79.0294425512897,-7.1889186099866,139.675768926861));
#76935=CARTESIAN_POINT('Ctrl Pts',(79.0671668276065,-7.16870219255865,139.673439060304));
#76936=CARTESIAN_POINT('Ctrl Pts',(79.1054837830116,-7.14968597763149,139.671109193747));
#76937=CARTESIAN_POINT('Ctrl Pts',(79.1443091147733,-7.13190185711778,139.66877932719));
#76938=CARTESIAN_POINT('Ctrl Pts',(79.2087912972159,-7.10236549898486,139.664909820515));
#76939=CARTESIAN_POINT('Ctrl Pts',(79.2749307389754,-7.0761139131,139.66104031384));
#76940=CARTESIAN_POINT('Ctrl Pts',(79.3423595470498,-7.05333449274319,139.657170807165));
#76941=CARTESIAN_POINT('Ctrl Pts',(79.4096878660436,-7.03058902053217,139.653307067212));
#76942=CARTESIAN_POINT('Ctrl Pts',(79.4783012807501,-7.01130559658793,139.649443327259));
#76943=CARTESIAN_POINT('Ctrl Pts',(79.5478103944463,-6.99562425600158,139.645579587305));
#76944=CARTESIAN_POINT('Ctrl Pts',(79.6172378912085,-6.9799613282948,139.641720384118));
#76945=CARTESIAN_POINT('Ctrl Pts',(79.6875585264096,-6.96789218894587,139.637861180932));
#76946=CARTESIAN_POINT('Ctrl Pts',(79.7583678281001,-6.9595070556351,139.634001977745));
#76947=CARTESIAN_POINT('Ctrl Pts',(79.8291324677329,-6.95112721113948,139.630145208701));
#76948=CARTESIAN_POINT('Ctrl Pts',(79.9003846811958,-6.94642681955575,139.626288439657));
#76949=CARTESIAN_POINT('Ctrl Pts',(79.9717113396144,-6.94544474053541,139.622431670613));
#76950=CARTESIAN_POINT('Ctrl Pts',(80.0430168551677,-6.94446295262593,139.618576044804));
#76951=CARTESIAN_POINT('Ctrl Pts',(80.1143962865175,-6.94719729578647,139.614720418995));
#76952=CARTESIAN_POINT('Ctrl Pts',(80.1854346706739,-6.95363455233137,139.610864793186));
#76953=CARTESIAN_POINT('Ctrl Pts',(80.2564757458479,-6.96007205272711,139.607009021322));
#76954=CARTESIAN_POINT('Ctrl Pts',(80.3271752646984,-6.97021269897574,139.603153249457));
#76955=CARTESIAN_POINT('Ctrl Pts',(80.397123288252,-6.9839914046741,139.599297477593));
#76956=CARTESIAN_POINT('Ctrl Pts',(80.4671443389033,-6.99778449560931,139.595437680227));
#76957=CARTESIAN_POINT('Ctrl Pts',(80.536411850583,-7.01522313403648,139.591577882862));
#76958=CARTESIAN_POINT('Ctrl Pts',(80.604526877104,-7.03619124725474,139.587718085497));
#76959=CARTESIAN_POINT('Ctrl Pts',(80.6726803776316,-7.05717120407593,139.583856107968));
#76960=CARTESIAN_POINT('Ctrl Pts',(80.7396796407864,-7.08168443741847,139.57999413044));
#76961=CARTESIAN_POINT('Ctrl Pts',(80.8051442726936,-7.10956611788491,139.576132152911));
#76962=CARTESIAN_POINT('Ctrl Pts',(80.8707232169427,-7.13749648449068,139.572263431716));
#76963=CARTESIAN_POINT('Ctrl Pts',(80.9347617433241,-7.16880682822043,139.56839471052));
#76964=CARTESIAN_POINT('Ctrl Pts',(80.9969033225346,-7.20328596376068,139.564525989324));
#76965=CARTESIAN_POINT('Ctrl Pts',(81.0337389571915,-7.22372414470459,139.562232729282));
#76966=CARTESIAN_POINT('Ctrl Pts',(81.0699085748146,-7.24527491322266,139.55993946924));
#76967=CARTESIAN_POINT('Ctrl Pts',(81.105343077467,-7.2678873467364,139.557646209198));
#76968=CARTESIAN_POINT('Ctrl Pts',(81.1556290406518,-7.29997720024298,139.554391788184));
#76969=CARTESIAN_POINT('Ctrl Pts',(81.2045988689083,-7.33431130662179,139.55113736717));
#76970=CARTESIAN_POINT('Ctrl Pts',(81.2520391107129,-7.37076839346111,139.547882946156));
#76971=CARTESIAN_POINT('Origin',(80.,-9.,134.));
#76972=CARTESIAN_POINT('',(78.4365593938057,-8.4244919888458,129.733376828424));
#76973=CARTESIAN_POINT('',(78.4365593669558,-8.42449206178673,129.539973210016));
#76974=CARTESIAN_POINT('',(78.4365593749993,-8.42449203993574,134.));
#76975=CARTESIAN_POINT('',(79.2300979593296,-10.4774325188554,129.));
#76976=CARTESIAN_POINT('Ctrl Pts',(78.4365593669558,-8.42449206178673,129.539973210016));
#76977=CARTESIAN_POINT('Ctrl Pts',(78.4421051495214,-8.40942623692262,129.538809960763));
#76978=CARTESIAN_POINT('Ctrl Pts',(78.4478692931931,-8.39443896491615,129.537643380814));
#76979=CARTESIAN_POINT('Ctrl Pts',(78.5031573253039,-8.25666554449912,129.526842962418));
#76980=CARTESIAN_POINT('Ctrl Pts',(78.566945264484,-8.14008694623375,129.517194430966));
#76981=CARTESIAN_POINT('Ctrl Pts',(78.6598156206824,-8.00994194088386,129.506139863644));
#76982=CARTESIAN_POINT('Ctrl Pts',(78.676306699791,-7.9879993410312,129.504262795112));
#76983=CARTESIAN_POINT('Ctrl Pts',(78.7011001312814,-7.95665351983249,129.501560125491));
#76984=CARTESIAN_POINT('Ctrl Pts',(78.7089776205111,-7.94692166614924,129.500717927568));
#76985=CARTESIAN_POINT('Ctrl Pts',(78.7231795512279,-7.9297755008893,129.499228174938));
#76986=CARTESIAN_POINT('Ctrl Pts',(78.7294606651604,-7.92232623559256,129.498578906769));
#76987=CARTESIAN_POINT('Ctrl Pts',(78.7427539217707,-7.90683849740872,129.497224481522));
#76988=CARTESIAN_POINT('Ctrl Pts',(78.7497786592342,-7.89881137853938,129.496519885272));
#76989=CARTESIAN_POINT('Ctrl Pts',(78.7685132743193,-7.8778138430891,129.494669362884));
#76990=CARTESIAN_POINT('Ctrl Pts',(78.7803511513633,-7.86495900949914,129.49352885744));
#76991=CARTESIAN_POINT('Ctrl Pts',(78.841554047578,-7.80056171704367,129.487771341444));
#76992=CARTESIAN_POINT('Ctrl Pts',(78.8939951307454,-7.75203994922801,129.483290817009));
#76993=CARTESIAN_POINT('Ctrl Pts',(79.0025415416958,-7.66384038981644,129.474652767779));
#76994=CARTESIAN_POINT('Ctrl Pts',(79.0583029557258,-7.6239721065796,129.470497234));
#76995=CARTESIAN_POINT('Ctrl Pts',(79.1346995757809,-7.57617446652224,129.464983869449));
#76996=CARTESIAN_POINT('Ctrl Pts',(79.1532601749058,-7.56505902057212,129.463657217349));
#76997=CARTESIAN_POINT('Ctrl Pts',(79.2285893136379,-7.52191694293435,129.458304193105));
#76998=CARTESIAN_POINT('Ctrl Pts',(79.2869924491519,-7.49287620261494,129.454224907383));
#76999=CARTESIAN_POINT('Ctrl Pts',(79.3574421351471,-7.46285792580099,129.449214025385));
#77000=CARTESIAN_POINT('Ctrl Pts',(79.3679915115582,-7.45849047400551,129.448461352988));
#77001=CARTESIAN_POINT('Ctrl Pts',(79.3845012182123,-7.45185339398491,129.447278551668));
#77002=CARTESIAN_POINT('Ctrl Pts',(79.3904313386674,-7.44950888173565,129.446852729747));
#77003=CARTESIAN_POINT('Ctrl Pts',(79.4009824191374,-7.44540732738616,129.446093120303));
#77004=CARTESIAN_POINT('Ctrl Pts',(79.4055979580861,-7.44363672301757,129.445760148423));
#77005=CARTESIAN_POINT('Ctrl Pts',(79.4167433589534,-7.43941795366539,129.444954516762));
#77006=CARTESIAN_POINT('Ctrl Pts',(79.4232807587345,-7.4369902287469,129.444480676272));
#77007=CARTESIAN_POINT('Ctrl Pts',(79.4435055772063,-7.42962370903896,129.443011187527));
#77008=CARTESIAN_POINT('Ctrl Pts',(79.4572421835039,-7.42482329415341,129.442008104407));
#77009=CARTESIAN_POINT('Ctrl Pts',(79.5275840643049,-7.40127083481238,129.436852221769));
#77010=CARTESIAN_POINT('Ctrl Pts',(79.5850991855127,-7.38538931416034,129.432574509866));
#77011=CARTESIAN_POINT('Ctrl Pts',(79.746891747963,-7.3499299248934,129.420573036073));
#77012=CARTESIAN_POINT('Ctrl Pts',(79.8523888785454,-7.33716821499544,129.412800023091));
#77013=CARTESIAN_POINT('Ctrl Pts',(80.0157945475274,-7.33308541577284,129.401185023904));
#77014=CARTESIAN_POINT('Ctrl Pts',(80.0732430980142,-7.33462002079192,129.3971774228));
#77015=CARTESIAN_POINT('Ctrl Pts',(80.1476576745716,-7.34046714864326,129.392086436276));
#77016=CARTESIAN_POINT('Ctrl Pts',(80.1647902112465,-7.34208073228306,129.390921102206));
#77017=CARTESIAN_POINT('Ctrl Pts',(80.192516992695,-7.34512617092939,129.38904548791));
#77018=CARTESIAN_POINT('Ctrl Pts',(80.2031274764858,-7.34639502296655,129.388330184557));
#77019=CARTESIAN_POINT('Ctrl Pts',(80.2235279836516,-7.34903393664873,129.386959360675));
#77020=CARTESIAN_POINT('Ctrl Pts',(80.2333194283543,-7.35038921156909,129.386303408469));
#77021=CARTESIAN_POINT('Ctrl Pts',(80.2560618285666,-7.35374362688137,129.384784169683));
#77022=CARTESIAN_POINT('Ctrl Pts',(80.2690025291913,-7.35580859947425,129.383922981935));
#77023=CARTESIAN_POINT('Ctrl Pts',(80.3110274492081,-7.36302404559621,129.381135778116));
#77024=CARTESIAN_POINT('Ctrl Pts',(80.3400003117498,-7.36879544286572,129.379229198639));
#77025=CARTESIAN_POINT('Ctrl Pts',(80.4091469975403,-7.38449202983201,129.374702170212));
#77026=CARTESIAN_POINT('Ctrl Pts',(80.4491348849155,-7.39514939011828,129.372103483886));
#77027=CARTESIAN_POINT('Ctrl Pts',(80.5603451229927,-7.42927161059155,129.3648744392));
#77028=CARTESIAN_POINT('Ctrl Pts',(80.6304397707747,-7.45606979612854,129.36031892819));
#77029=CARTESIAN_POINT('Ctrl Pts',(80.7739311678776,-7.52233584460262,129.350643978906));
#77030=CARTESIAN_POINT('Ctrl Pts',(80.8466493666071,-7.5627657409146,129.345529800997));
#77031=CARTESIAN_POINT('Ctrl Pts',(80.9294110477657,-7.61724644598969,129.339103104612));
#77032=CARTESIAN_POINT('Ctrl Pts',(80.9426546507233,-7.62624075958579,129.338054795383));
#77033=CARTESIAN_POINT('Ctrl Pts',(80.9616544589108,-7.63954846245772,129.336518536545));
#77034=CARTESIAN_POINT('Ctrl Pts',(80.9675160335009,-7.6437107961181,129.336040046828));
#77035=CARTESIAN_POINT('Ctrl Pts',(80.9778647884257,-7.65116072216811,129.335186811843));
#77036=CARTESIAN_POINT('Ctrl Pts',(80.9823627046248,-7.65443303533248,129.334813083378));
#77037=CARTESIAN_POINT('Ctrl Pts',(80.9921302395696,-7.6616141688067,129.333995152748));
#77038=CARTESIAN_POINT('Ctrl Pts',(80.9973931481054,-7.66553158527528,129.333550397849));
#77039=CARTESIAN_POINT('Ctrl Pts',(81.0123582500058,-7.67680875431978,129.332274468473));
#77040=CARTESIAN_POINT('Ctrl Pts',(81.0220028404786,-7.68424376423163,129.331438516697));
#77041=CARTESIAN_POINT('Ctrl Pts',(81.0438463582184,-7.70146797988907,129.329515389397));
#77042=CARTESIAN_POINT('Ctrl Pts',(81.0559905513174,-7.71132449998642,129.32842447879));
#77043=CARTESIAN_POINT('Ctrl Pts',(81.096211033922,-7.74491870195875,129.324742713934));
#77044=CARTESIAN_POINT('Ctrl Pts',(81.1236388480168,-7.7694135093637,129.322117430346));
#77045=CARTESIAN_POINT('Ctrl Pts',(81.2005140827859,-7.84278218217326,129.314467617277));
#77046=CARTESIAN_POINT('Ctrl Pts',(81.2477431818303,-7.89386976861539,129.309398873089));
#77047=CARTESIAN_POINT('Ctrl Pts',(81.3523823720482,-8.02231596145479,129.297428709378));
#77048=CARTESIAN_POINT('Ctrl Pts',(81.4065602181387,-8.10200331115536,129.290600396389));
#77049=CARTESIAN_POINT('Ctrl Pts',(81.4627734102828,-8.20237534866955,129.282738285493));
#77050=CARTESIAN_POINT('Ctrl Pts',(81.471702417144,-8.21897299693459,129.281460096307));
#77051=CARTESIAN_POINT('Ctrl Pts',(81.4854250621002,-8.2455526155487,129.279446908675));
#77052=CARTESIAN_POINT('Ctrl Pts',(81.4904039112463,-8.2554365960657,129.278705532416));
#77053=CARTESIAN_POINT('Ctrl Pts',(81.4996262667756,-8.27420799716288,129.27731090634));
#77054=CARTESIAN_POINT('Ctrl Pts',(81.503890154147,-8.2830848148542,129.276656976824));
#77055=CARTESIAN_POINT('Ctrl Pts',(81.51339256266,-8.30332539064225,129.275178243855));
#77056=CARTESIAN_POINT('Ctrl Pts',(81.5185823110353,-8.31471149230558,129.274355132529));
#77057=CARTESIAN_POINT('Ctrl Pts',(81.5341697356079,-8.34995651944988,129.27183307611));
#77058=CARTESIAN_POINT('Ctrl Pts',(81.5441373349323,-8.37400214563419,129.270148596857));
#77059=CARTESIAN_POINT('Ctrl Pts',(81.5661022838081,-8.43071117584757,129.2662515433));
#77060=CARTESIAN_POINT('Ctrl Pts',(81.5776481178226,-8.46353678720286,129.2640531434));
#77061=CARTESIAN_POINT('Ctrl Pts',(81.6148612060515,-8.5809626793549,129.25635058614));
#77062=CARTESIAN_POINT('Ctrl Pts',(81.6348164241211,-8.66721605467108,129.25099239051));
#77063=CARTESIAN_POINT('Ctrl Pts',(81.66016419167,-8.83745719085409,129.240470953946));
#77064=CARTESIAN_POINT('Ctrl Pts',(81.6662327280654,-8.92106763900409,129.235324432262));
#77065=CARTESIAN_POINT('Ctrl Pts',(81.6659483645958,-9.02042572749627,129.228879170295));
#77066=CARTESIAN_POINT('Ctrl Pts',(81.6656828216231,-9.03608127190637,129.227853784274));
#77067=CARTESIAN_POINT('Ctrl Pts',(81.6649735763235,-9.05891196765729,129.226341071643));
#77068=CARTESIAN_POINT('Ctrl Pts',(81.6647040113192,-9.06609220629656,129.22586281435));
#77069=CARTESIAN_POINT('Ctrl Pts',(81.6641482873134,-9.07871587838213,129.225017213397));
#77070=CARTESIAN_POINT('Ctrl Pts',(81.6638818410816,-9.0841601353511,129.224650966338));
#77071=CARTESIAN_POINT('Ctrl Pts',(81.6632663094816,-9.09558824289128,129.223878707916));
#77072=CARTESIAN_POINT('Ctrl Pts',(81.6629116461076,-9.1015715547018,129.223472360227));
#77073=CARTESIAN_POINT('Ctrl Pts',(81.6618279054598,-9.11832377081192,129.222329174227));
#77074=CARTESIAN_POINT('Ctrl Pts',(81.6610264630458,-9.12908746975198,129.221588322054));
#77075=CARTESIAN_POINT('Ctrl Pts',(81.6550402791469,-9.20015174065917,129.216658629842));
#77076=CARTESIAN_POINT('Ctrl Pts',(81.6466779519982,-9.26013263890496,129.212316204664));
#77077=CARTESIAN_POINT('Ctrl Pts',(81.6120320563035,-9.4374265982666,129.199179546184));
#77078=CARTESIAN_POINT('Ctrl Pts',(81.5763006516239,-9.55251362934102,129.190280518424));
#77079=CARTESIAN_POINT('Ctrl Pts',(81.505826795098,-9.71504511962773,129.177663005555));
#77080=CARTESIAN_POINT('Ctrl Pts',(81.48048531832,-9.76613867419146,129.173682126311));
#77081=CARTESIAN_POINT('Ctrl Pts',(81.4443832378883,-9.83041715376138,129.168654599245));
#77082=CARTESIAN_POINT('Ctrl Pts',(81.435975776323,-9.84487229446125,129.16752250497));
#77083=CARTESIAN_POINT('Ctrl Pts',(81.422061095598,-9.86798818177181,129.165709029961));
#77084=CARTESIAN_POINT('Ctrl Pts',(81.4166891873383,-9.87672857729801,129.165022602217));
#77085=CARTESIAN_POINT('Ctrl Pts',(81.4062436001058,-9.89337741507283,129.163713427037));
#77086=CARTESIAN_POINT('Ctrl Pts',(81.4011831040058,-9.90129361699914,129.163090209504));
#77087=CARTESIAN_POINT('Ctrl Pts',(81.3893422940441,-9.91947557533854,129.161656832144));
#77088=CARTESIAN_POINT('Ctrl Pts',(81.3825146399891,-9.9297099697401,129.160848533992));
#77089=CARTESIAN_POINT('Ctrl Pts',(81.3603535257935,-9.96214458099085,129.158281169335));
#77090=CARTESIAN_POINT('Ctrl Pts',(81.3445934268057,-9.9840490647939,129.156538710523));
#77091=CARTESIAN_POINT('Ctrl Pts',(81.2908335459066,-10.0550637218277,129.150846887588));
#77092=CARTESIAN_POINT('Ctrl Pts',(81.2506197507949,-10.1024345952231,129.146982423801));
#77093=CARTESIAN_POINT('Ctrl Pts',(81.1436257940824,-10.2150603749868,129.137431388163));
#77094=CARTESIAN_POINT('Ctrl Pts',(81.0738399867031,-10.277152343676,129.131825983486));
#77095=CARTESIAN_POINT('Ctrl Pts',(80.9566353766147,-10.3650048822894,129.122733375139));
#77096=CARTESIAN_POINT('Ctrl Pts',(80.9125403291373,-10.3948686158705,129.119372292501));
#77097=CARTESIAN_POINT('Ctrl Pts',(80.8578135471789,-10.428226216401,129.115170830819));
#77098=CARTESIAN_POINT('Ctrl Pts',(80.8484750257994,-10.4337936816692,129.11445287116));
#77099=CARTESIAN_POINT('Ctrl Pts',(80.833755681823,-10.4423749475326,129.113318488733));
#77100=CARTESIAN_POINT('Ctrl Pts',(80.8284112515301,-10.4454510790768,129.112906048126));
#77101=CARTESIAN_POINT('Ctrl Pts',(80.8182622725121,-10.4512178251095,129.112121526084));
#77102=CARTESIAN_POINT('Ctrl Pts',(80.8134612205255,-10.4539144276564,129.11174985938));
#77103=CARTESIAN_POINT('Ctrl Pts',(80.8038690255773,-10.4592396837431,129.111006339217));
#77104=CARTESIAN_POINT('Ctrl Pts',(80.799078134191,-10.4618686665421,129.110634512434));
#77105=CARTESIAN_POINT('Ctrl Pts',(80.7836859065697,-10.4702168200401,129.109438594242));
#77106=CARTESIAN_POINT('Ctrl Pts',(80.7730357413556,-10.4758444428702,129.10860913776));
#77107=CARTESIAN_POINT('Ctrl Pts',(80.7480249590674,-10.4887153316269,129.106658139892));
#77108=CARTESIAN_POINT('Ctrl Pts',(80.7336188013687,-10.4958670024119,129.10553201283));
#77109=CARTESIAN_POINT('Ctrl Pts',(80.6847384433017,-10.5192568402237,129.101708096936));
#77110=CARTESIAN_POINT('Ctrl Pts',(80.6498129233082,-10.5345197474586,129.098971190258));
#77111=CARTESIAN_POINT('Ctrl Pts',(80.507882362411,-10.5908308757962,129.087901487725));
#77112=CARTESIAN_POINT('Ctrl Pts',(80.3972812718764,-10.6219919419258,129.079417142815));
#77113=CARTESIAN_POINT('Ctrl Pts',(80.2098310726684,-10.6544630165915,129.065738018543));
#77114=CARTESIAN_POINT('Ctrl Pts',(80.1345031853498,-10.6622841871778,129.060414502622));
#77115=CARTESIAN_POINT('Ctrl Pts',(80.0392875853344,-10.6656522439802,129.053897824544));
#77116=CARTESIAN_POINT('Ctrl Pts',(80.0196692971777,-10.6659994251104,129.052566049396));
#77117=CARTESIAN_POINT('Ctrl Pts',(79.9881339529254,-10.6660003479618,129.050441511476));
#77118=CARTESIAN_POINT('Ctrl Pts',(79.9762192521891,-10.6658728793751,129.049642532108));
#77119=CARTESIAN_POINT('Ctrl Pts',(79.9534345908827,-10.6653846161134,129.04812127416));
#77120=CARTESIAN_POINT('Ctrl Pts',(79.9425648355876,-10.6650451848089,129.047398428518));
#77121=CARTESIAN_POINT('Ctrl Pts',(79.9174608320011,-10.6640151297221,129.045735185369));
#77122=CARTESIAN_POINT('Ctrl Pts',(79.9032304499663,-10.6632482493494,129.044796968387));
#77123=CARTESIAN_POINT('Ctrl Pts',(79.8572148200931,-10.6601758694142,129.04177623738));
#77124=CARTESIAN_POINT('Ctrl Pts',(79.8254844654185,-10.6571409217714,129.039713673389));
#77125=CARTESIAN_POINT('Ctrl Pts',(79.7061279291857,-10.6422580968799,129.032003191899));
#77126=CARTESIAN_POINT('Ctrl Pts',(79.6194042500843,-10.6243523978704,129.026506258357));
#77127=CARTESIAN_POINT('Ctrl Pts',(79.4530587979164,-10.5759463542871,129.015705200889));
#77128=CARTESIAN_POINT('Ctrl Pts',(79.3735468198919,-10.5460612398616,129.010415206558));
#77129=CARTESIAN_POINT('Ctrl Pts',(79.2839673137288,-10.5043434987173,129.003983026668));
#77130=CARTESIAN_POINT('Ctrl Pts',(79.2713460464801,-10.4982708572166,129.003065253333));
#77131=CARTESIAN_POINT('Ctrl Pts',(79.253473921207,-10.489392568874,129.001747290998));
#77132=CARTESIAN_POINT('Ctrl Pts',(79.2481589036594,-10.4867166422333,129.001352998794));
#77133=CARTESIAN_POINT('Ctrl Pts',(79.2385954444432,-10.481837375072,129.000639121319));
#77134=CARTESIAN_POINT('Ctrl Pts',(79.234341920028,-10.4796440811167,129.0003200235));
#77135=CARTESIAN_POINT('Ctrl Pts',(79.2300979593296,-10.4774325188555,129.));
#77136=CARTESIAN_POINT('',(78.6641544596132,-8.00193394365392,128.999128947666));
#77137=CARTESIAN_POINT('Origin',(80.,-9.,129.));
#77138=CARTESIAN_POINT('',(78.4365593804234,-8.42449202520043,129.032769696));
#77139=CARTESIAN_POINT('Ctrl Pts',(78.6653336475789,-8.00289332179799,128.998257895331));
#77140=CARTESIAN_POINT('Ctrl Pts',(78.6630695895503,-8.00592385216835,128.998515381112));
#77141=CARTESIAN_POINT('Ctrl Pts',(78.6608158838452,-8.00896205294451,128.998773542407));
#77142=CARTESIAN_POINT('Ctrl Pts',(78.6540156321242,-8.01819496474882,128.99955808582));
#77143=CARTESIAN_POINT('Ctrl Pts',(78.6495016584439,-8.02441337142469,129.000086487955));
#77144=CARTESIAN_POINT('Ctrl Pts',(78.6275129566489,-8.05514984269038,129.002697449622));
#77145=CARTESIAN_POINT('Ctrl Pts',(78.6106631800488,-8.08010574189685,129.004814697559));
#77146=CARTESIAN_POINT('Ctrl Pts',(78.5348728686095,-8.19919303571354,129.014858057607));
#77147=CARTESIAN_POINT('Ctrl Pts',(78.484764080392,-8.29860885504514,129.023048835688));
#77148=CARTESIAN_POINT('Ctrl Pts',(78.4420795996736,-8.40965885144952,129.031630802593));
#77149=CARTESIAN_POINT('Ctrl Pts',(78.4392928985672,-8.41706607545248,129.032200782898));
#77150=CARTESIAN_POINT('Ctrl Pts',(78.4365593804234,-8.42449202520042,129.032769696));
#77151=CARTESIAN_POINT('',(78.4365593749993,-8.42449203993574,128.));
#77152=CARTESIAN_POINT('',(78.4365593749993,-8.42449203993574,134.));
#77153=CARTESIAN_POINT('Origin',(80.,-9.,128.));
#77154=CARTESIAN_POINT('Ctrl Pts',(78.4365593804234,-8.42449202520042,129.032769696));
#77155=CARTESIAN_POINT('Ctrl Pts',(78.4096421356088,-8.49761614467909,129.038371844014));
#77156=CARTESIAN_POINT('Ctrl Pts',(78.3878815483186,-8.57255645732196,129.043863517686));
#77157=CARTESIAN_POINT('Ctrl Pts',(78.3675657998122,-8.66675351310855,129.050446145633));
#77158=CARTESIAN_POINT('Ctrl Pts',(78.3639843431817,-8.68480568466688,129.051693840243));
#77159=CARTESIAN_POINT('Ctrl Pts',(78.3587462013066,-8.71370935642439,129.053670362302));
#77160=CARTESIAN_POINT('Ctrl Pts',(78.3568964522487,-8.72452385664356,129.054405193902));
#77161=CARTESIAN_POINT('Ctrl Pts',(78.3535870427762,-8.74509289096038,129.055794215036));
#77162=CARTESIAN_POINT('Ctrl Pts',(78.3521069179843,-8.75484360653624,129.056449017273));
#77163=CARTESIAN_POINT('Ctrl Pts',(78.3489233111293,-8.77714962911568,129.057938911605));
#77164=CARTESIAN_POINT('Ctrl Pts',(78.3472762808697,-8.78971247513152,129.058772216853));
#77165=CARTESIAN_POINT('Ctrl Pts',(78.3433203235853,-8.82281225660801,129.060953369334));
#77166=CARTESIAN_POINT('Ctrl Pts',(78.3412498728459,-8.84337585894582,129.062293887701));
#77167=CARTESIAN_POINT('Ctrl Pts',(78.3276469462407,-9.00942286243062,129.073015574458));
#77168=CARTESIAN_POINT('Ctrl Pts',(78.3348930193932,-9.15580098927435,129.081762368785));
#77169=CARTESIAN_POINT('Ctrl Pts',(78.3720834551145,-9.35939909493017,129.094552020351));
#77170=CARTESIAN_POINT('Ctrl Pts',(78.3863380897752,-9.41877639812151,129.09837109746));
#77171=CARTESIAN_POINT('Ctrl Pts',(78.4080452696062,-9.49137990511416,129.103299314955));
#77172=CARTESIAN_POINT('Ctrl Pts',(78.4124631859569,-9.50547097133187,129.104268228217));
#77173=CARTESIAN_POINT('Ctrl Pts',(78.4188413398983,-9.52490536890206,129.1056242622));
#77174=CARTESIAN_POINT('Ctrl Pts',(78.4206426747747,-9.53030066157981,129.106002839049));
#77175=CARTESIAN_POINT('Ctrl Pts',(78.4225463402344,-9.53590671330397,129.106398519546));
#77176=CARTESIAN_POINT('Ctrl Pts',(78.4226211554302,-9.53612688309365,129.106414063065));
#77177=CARTESIAN_POINT('Ctrl Pts',(78.422770798915,-9.53656695873192,129.106445138926));
#77178=CARTESIAN_POINT('Ctrl Pts',(78.4228456270988,-9.53678686459003,129.106460671261));
#77179=CARTESIAN_POINT('Ctrl Pts',(78.4229967420417,-9.5372306584089,129.106492024724));
#77180=CARTESIAN_POINT('Ctrl Pts',(78.4230730304888,-9.53745454577447,129.106507845947));
#77181=CARTESIAN_POINT('Ctrl Pts',(78.4232288600846,-9.53791154756071,129.106540148343));
#77182=CARTESIAN_POINT('Ctrl Pts',(78.4233084052583,-9.53814466060712,129.106556629747));
#77183=CARTESIAN_POINT('Ctrl Pts',(78.4234731817409,-9.53862720019305,129.106590754658));
#77184=CARTESIAN_POINT('Ctrl Pts',(78.4235584205148,-9.5388766240504,129.106608398588));
#77185=CARTESIAN_POINT('Ctrl Pts',(78.4237382273484,-9.5394023631487,129.1066455989));
#77186=CARTESIAN_POINT('Ctrl Pts',(78.423832808883,-9.53967867378591,129.106665156056));
#77187=CARTESIAN_POINT('Ctrl Pts',(78.4240374452184,-9.54027598602979,129.10670744644));
#77188=CARTESIAN_POINT('Ctrl Pts',(78.424147525423,-9.54059697883303,129.106730181126));
#77189=CARTESIAN_POINT('Ctrl Pts',(78.4243953955544,-9.54131904667906,129.106781340535));
#77190=CARTESIAN_POINT('Ctrl Pts',(78.4245332404916,-9.54172010257193,129.106809768427));
#77191=CARTESIAN_POINT('Ctrl Pts',(78.4248089410281,-9.54252125010253,129.106866581082));
#77192=CARTESIAN_POINT('Ctrl Pts',(78.4249467959659,-9.54292134194454,129.106894965805));
#77193=CARTESIAN_POINT('Ctrl Pts',(78.4268295298595,-9.54837878633416,129.107282319114));
#77194=CARTESIAN_POINT('Ctrl Pts',(78.428598525952,-9.55342752580425,129.107642699987));
#77195=CARTESIAN_POINT('Ctrl Pts',(78.4327683479179,-9.56514707022418,129.108483982786));
#77196=CARTESIAN_POINT('Ctrl Pts',(78.4351874402871,-9.57181107953126,129.1089659129));
#77197=CARTESIAN_POINT('Ctrl Pts',(78.4431430177107,-9.59329816599076,129.110530889108));
#77198=CARTESIAN_POINT('Ctrl Pts',(78.4488479811817,-9.6080573545679,129.111622943353));
#77199=CARTESIAN_POINT('Ctrl Pts',(78.4845977626891,-9.69676628128776,129.118281279102));
#77200=CARTESIAN_POINT('Ctrl Pts',(78.5197126889738,-9.76855332466226,129.124065225017));
#77201=CARTESIAN_POINT('Ctrl Pts',(78.5940700406345,-9.89641236903334,129.134820673432));
#77202=CARTESIAN_POINT('Ctrl Pts',(78.6318872286945,-9.95313300038912,129.139777824227));
#77203=CARTESIAN_POINT('Ctrl Pts',(78.7017399623389,-10.0451433854631,129.148049068867));
#77204=CARTESIAN_POINT('Ctrl Pts',(78.7320089393397,-10.081666844528,129.151401916215));
#77205=CARTESIAN_POINT('Ctrl Pts',(78.7856439840373,-10.1410335191105,129.156963574378));
#77206=CARTESIAN_POINT('Ctrl Pts',(78.8081968196041,-10.164570075073,129.159201282403));
#77207=CARTESIAN_POINT('Ctrl Pts',(78.8411224095579,-10.1969727520342,129.162331499006));
#77208=CARTESIAN_POINT('Ctrl Pts',(78.8509345237074,-10.2063952871565,129.163248053969));
#77209=CARTESIAN_POINT('Ctrl Pts',(78.8681298696912,-10.2225077629295,129.164826817197));
#77210=CARTESIAN_POINT('Ctrl Pts',(78.8754596089702,-10.2292534883524,129.165491384624));
#77211=CARTESIAN_POINT('Ctrl Pts',(78.8906336128491,-10.242969153047,129.16685030353));
#77212=CARTESIAN_POINT('Ctrl Pts',(78.8984841204855,-10.2499315469333,129.167544321678));
#77213=CARTESIAN_POINT('Ctrl Pts',(78.9187041954616,-10.2675256996774,129.169309383794));
#77214=CARTESIAN_POINT('Ctrl Pts',(78.9311652512517,-10.278050987555,129.170376048325));
#77215=CARTESIAN_POINT('Ctrl Pts',(78.9823649599522,-10.3200243931331,129.174677221132));
#77216=CARTESIAN_POINT('Ctrl Pts',(79.0223546163069,-10.3499095162561,129.177850029573));
#77217=CARTESIAN_POINT('Ctrl Pts',(79.1633883788147,-10.4457470422045,129.188528116886));
#77218=CARTESIAN_POINT('Ctrl Pts',(79.2702099834336,-10.5025010153419,129.195744032815));
#77219=CARTESIAN_POINT('Ctrl Pts',(79.4330600782967,-10.5675240858282,129.206598739541));
#77220=CARTESIAN_POINT('Ctrl Pts',(79.4848635012946,-10.58530306482,129.210037212744));
#77221=CARTESIAN_POINT('Ctrl Pts',(79.5512169646293,-10.604479785553,129.214531661322));
#77222=CARTESIAN_POINT('Ctrl Pts',(79.5650420669351,-10.6082826734889,129.215472970861));
#77223=CARTESIAN_POINT('Ctrl Pts',(79.5856206905315,-10.6136585257693,129.216883661276));
#77224=CARTESIAN_POINT('Ctrl Pts',(79.5923381451511,-10.6153686445306,129.217345651641));
#77225=CARTESIAN_POINT('Ctrl Pts',(79.6038586880922,-10.6182250905566,129.218140845998));
#77226=CARTESIAN_POINT('Ctrl Pts',(79.6086565176863,-10.6193920651842,129.218472869485));
#77227=CARTESIAN_POINT('Ctrl Pts',(79.6196893173018,-10.6220236750174,129.219238427623));
#77228=CARTESIAN_POINT('Ctrl Pts',(79.625927440841,-10.6234736630792,129.219672763043));
#77229=CARTESIAN_POINT('Ctrl Pts',(79.6434351589962,-10.6274368912019,129.220895590287));
#77230=CARTESIAN_POINT('Ctrl Pts',(79.6547224906052,-10.6298689344806,129.221688395545));
#77231=CARTESIAN_POINT('Ctrl Pts',(79.7354173412039,-10.6463801635573,129.22738353793));
#77232=CARTESIAN_POINT('Ctrl Pts',(79.8056280414769,-10.6561367382867,129.232479283037));
#77233=CARTESIAN_POINT('Ctrl Pts',(79.8909017485095,-10.6624890395765,129.23868862336));
#77234=CARTESIAN_POINT('Ctrl Pts',(79.9055797847451,-10.6633872227276,129.239758284618));
#77235=CARTESIAN_POINT('Ctrl Pts',(79.9872832888677,-10.6673019181041,129.245712372193));
#77236=CARTESIAN_POINT('Ctrl Pts',(80.0544349201842,-10.6664618395219,129.250602377746));
#77237=CARTESIAN_POINT('Ctrl Pts',(80.1947253237735,-10.6562155437339,129.260692005127));
#77238=CARTESIAN_POINT('Ctrl Pts',(80.2676679650444,-10.6460025706391,129.265864060174));
#77239=CARTESIAN_POINT('Ctrl Pts',(80.3569385338475,-10.6274092066713,129.272087197347));
#77240=CARTESIAN_POINT('Ctrl Pts',(80.3741136599144,-10.6235469977397,129.273279810671));
#77241=CARTESIAN_POINT('Ctrl Pts',(80.401618131403,-10.6169023468378,129.275182799228));
#77242=CARTESIAN_POINT('Ctrl Pts',(80.411987114148,-10.6142914698798,129.275898631705));
#77243=CARTESIAN_POINT('Ctrl Pts',(80.4317456122551,-10.6091135631706,129.277259908056));
#77244=CARTESIAN_POINT('Ctrl Pts',(80.441139131806,-10.6065637261465,129.277905877371));
#77245=CARTESIAN_POINT('Ctrl Pts',(80.462505068764,-10.6005624935669,129.279372687967));
#77246=CARTESIAN_POINT('Ctrl Pts',(80.4744622886533,-10.5970587920311,129.280191790036));
#77247=CARTESIAN_POINT('Ctrl Pts',(80.5062136229817,-10.5873669456274,129.282362892754));
#77248=CARTESIAN_POINT('Ctrl Pts',(80.5259337868642,-10.5809426824809,129.283707181825));
#77249=CARTESIAN_POINT('Ctrl Pts',(80.6640028537375,-10.5330942043162,129.293102046469));
#77250=CARTESIAN_POINT('Ctrl Pts',(80.7774638600435,-10.478793938927,129.300693851854));
#77251=CARTESIAN_POINT('Ctrl Pts',(80.9619418148984,-10.3633518960431,129.313985497023));
#77252=CARTESIAN_POINT('Ctrl Pts',(81.0359088301449,-10.308032274021,129.319644951935));
#77253=CARTESIAN_POINT('Ctrl Pts',(81.1137263748375,-10.2390756053764,129.326443735746));
#77254=CARTESIAN_POINT('Ctrl Pts',(81.1224602857129,-10.2311692334273,129.327219994112));
#77255=CARTESIAN_POINT('Ctrl Pts',(81.1357899796162,-10.2188427978369,129.328426612819));
#77256=CARTESIAN_POINT('Ctrl Pts',(81.1404456733377,-10.2144876723935,129.328852252722));
#77257=CARTESIAN_POINT('Ctrl Pts',(81.1490514031147,-10.2063444057755,129.329647130337));
#77258=CARTESIAN_POINT('Ctrl Pts',(81.1530079164191,-10.2025633844024,129.330015834876));
#77259=CARTESIAN_POINT('Ctrl Pts',(81.1620623576548,-10.1938247958838,129.330867054166));
#77260=CARTESIAN_POINT('Ctrl Pts',(81.1671472619829,-10.1888539988368,129.331350567942));
#77261=CARTESIAN_POINT('Ctrl Pts',(81.1830096500442,-10.1731477201653,129.332875735517));
#77262=CARTESIAN_POINT('Ctrl Pts',(81.1936716612685,-10.1622974360859,129.333925595327));
#77263=CARTESIAN_POINT('Ctrl Pts',(81.2719261072152,-10.0804487223339,129.341807328732));
#77264=CARTESIAN_POINT('Ctrl Pts',(81.3332772576937,-10.0037598843842,129.348971688738));
#77265=CARTESIAN_POINT('Ctrl Pts',(81.4322556200153,-9.85482767619449,129.361983145366));
#77266=CARTESIAN_POINT('Ctrl Pts',(81.4720327621261,-9.78435230836564,129.367825855314));
#77267=CARTESIAN_POINT('Ctrl Pts',(81.5197616983309,-9.68325652546844,129.375696198326));
#77268=CARTESIAN_POINT('Ctrl Pts',(81.5322005865692,-9.65488676243698,129.377853500018));
#77269=CARTESIAN_POINT('Ctrl Pts',(81.5527754565263,-9.60415998945305,129.381621185544));
#77270=CARTESIAN_POINT('Ctrl Pts',(81.5612369029593,-9.58194531104749,129.383241664363));
#77271=CARTESIAN_POINT('Ctrl Pts',(81.5732563253708,-9.54823801654378,129.385657666451));
#77272=CARTESIAN_POINT('Ctrl Pts',(81.5771696907278,-9.53687630591745,129.386464827723));
#77273=CARTESIAN_POINT('Ctrl Pts',(81.5840276294898,-9.516243226196,129.387917987705));
#77274=CARTESIAN_POINT('Ctrl Pts',(81.5870145492163,-9.50698661424842,129.388565352295));
#77275=CARTESIAN_POINT('Ctrl Pts',(81.5932726818051,-9.48699495679227,129.389953920819));
#77276=CARTESIAN_POINT('Ctrl Pts',(81.5965168544273,-9.47625189804618,129.390694215873));
#77277=CARTESIAN_POINT('Ctrl Pts',(81.6052025035908,-9.44640288524095,129.392735409332));
#77278=CARTESIAN_POINT('Ctrl Pts',(81.6104113000333,-9.42723074879825,129.394028776547));
#77279=CARTESIAN_POINT('Ctrl Pts',(81.6415714534823,-9.30385811828331,129.40224810757));
#77280=CARTESIAN_POINT('Ctrl Pts',(81.6577413694293,-9.19744403187217,129.408846045515));
#77281=CARTESIAN_POINT('Ctrl Pts',(81.6694756847925,-8.98103396986609,129.422090064455));
#77282=CARTESIAN_POINT('Ctrl Pts',(81.6646339036772,-8.87156324183172,129.428709153294));
#77283=CARTESIAN_POINT('Ctrl Pts',(81.6470201250653,-8.7488084117633,129.436771650201));
#77284=CARTESIAN_POINT('Ctrl Pts',(81.6447374542312,-8.73427236363221,129.437736932729));
#77285=CARTESIAN_POINT('Ctrl Pts',(81.6410853627971,-8.71286968180983,129.439176362717));
#77286=CARTESIAN_POINT('Ctrl Pts',(81.6398646308326,-8.70597793321021,129.439642656321));
#77287=CARTESIAN_POINT('Ctrl Pts',(81.6376114368216,-8.69370802893159,129.44047814703));
#77288=CARTESIAN_POINT('Ctrl Pts',(81.6365958330058,-8.68832698657475,129.440846399267));
#77289=CARTESIAN_POINT('Ctrl Pts',(81.6342945821157,-8.67645557646187,129.441662960924));
#77290=CARTESIAN_POINT('Ctrl Pts',(81.6329968127525,-8.66996790930031,129.442111915263));
#77291=CARTESIAN_POINT('Ctrl Pts',(81.6290744137912,-8.65094918562685,129.443435648521));
#77292=CARTESIAN_POINT('Ctrl Pts',(81.6263440055483,-8.63844078303207,129.444315979006));
#77293=CARTESIAN_POINT('Ctrl Pts',(81.6197100478641,-8.60964656151575,129.446363090263));
#77294=CARTESIAN_POINT('Ctrl Pts',(81.6157045896166,-8.59338583630867,129.447534446949));
#77295=CARTESIAN_POINT('Ctrl Pts',(81.6010465372756,-8.53751976987163,129.451605685435));
#77296=CARTESIAN_POINT('Ctrl Pts',(81.5891775745634,-8.49825087460818,129.454548939693));
#77297=CARTESIAN_POINT('Ctrl Pts',(81.5358427326902,-8.34275946089723,129.466440042762));
#77298=CARTESIAN_POINT('Ctrl Pts',(81.4829659982357,-8.23084681331225,129.475503008274));
#77299=CARTESIAN_POINT('Ctrl Pts',(81.3937203127852,-8.0860644898412,129.487488889464));
#77300=CARTESIAN_POINT('Ctrl Pts',(81.3675685043992,-8.04737649300279,129.490725641308));
#77301=CARTESIAN_POINT('Ctrl Pts',(81.3303695542058,-7.9970414275945,129.494985033702));
#77302=CARTESIAN_POINT('Ctrl Pts',(81.3207321185703,-7.98438405380397,129.496060508078));
#77303=CARTESIAN_POINT('Ctrl Pts',(81.3045140640033,-7.96370533916564,129.497825438851));
#77304=CARTESIAN_POINT('Ctrl Pts',(81.298037363818,-7.95560420443892,129.498518929313));
#77305=CARTESIAN_POINT('Ctrl Pts',(81.2852030999192,-7.9398547793325,129.499871453844));
#77306=CARTESIAN_POINT('Ctrl Pts',(81.278851880996,-7.93220190545565,129.500530702896));
#77307=CARTESIAN_POINT('Ctrl Pts',(81.2635644684063,-7.91411346252924,129.502094122966));
#77308=CARTESIAN_POINT('Ctrl Pts',(81.2545668775261,-7.90373055019752,129.502995741496));
#77309=CARTESIAN_POINT('Ctrl Pts',(81.2230440369481,-7.86825071776,129.506092836269));
#77310=CARTESIAN_POINT('Ctrl Pts',(81.1998850866693,-7.8437261650007,129.50826188435));
#77311=CARTESIAN_POINT('Ctrl Pts',(81.1407295831974,-7.78477536566424,129.513568249281));
#77312=CARTESIAN_POINT('Ctrl Pts',(81.1039034746794,-7.7512275759412,129.516671347967));
#77313=CARTESIAN_POINT('Ctrl Pts',(81.0147299416358,-7.67702475430291,129.523826243238));
#77314=CARTESIAN_POINT('Ctrl Pts',(80.9613524648524,-7.63774380970178,129.527845788089));
#77315=CARTESIAN_POINT('Ctrl Pts',(80.8995878948306,-7.59773325471521,129.532351577536));
#77316=CARTESIAN_POINT('Ctrl Pts',(80.8933707509953,-7.59376420688563,129.532803598771));
#77317=CARTESIAN_POINT('Ctrl Pts',(80.8215182851377,-7.54856214254918,129.538012374849));
#77318=CARTESIAN_POINT('Ctrl Pts',(80.7531168654114,-7.51192205848376,129.542822035831));
#77319=CARTESIAN_POINT('Ctrl Pts',(80.6718314202186,-7.47542354097248,129.548650215978));
#77320=CARTESIAN_POINT('Ctrl Pts',(80.6611892936752,-7.47077812728171,129.549415434918));
#77321=CARTESIAN_POINT('Ctrl Pts',(80.6445756303972,-7.46373190289868,129.550614723483));
#77322=CARTESIAN_POINT('Ctrl Pts',(80.6386370294827,-7.46125370818591,129.551044334992));
#77323=CARTESIAN_POINT('Ctrl Pts',(80.6276137023138,-7.45672844739292,129.551843758788));
#77324=CARTESIAN_POINT('Ctrl Pts',(80.6225330520719,-7.45467199587074,129.552213006875));
#77325=CARTESIAN_POINT('Ctrl Pts',(80.6107467266368,-7.44996890161242,129.553071395728));
#77326=CARTESIAN_POINT('Ctrl Pts',(80.6040339591825,-7.44734068727761,129.553561593192));
#77327=CARTESIAN_POINT('Ctrl Pts',(80.5824443388883,-7.43904901152836,129.555141884271));
#77328=CARTESIAN_POINT('Ctrl Pts',(80.5675038080964,-7.43355537033496,129.556241114139));
#77329=CARTESIAN_POINT('Ctrl Pts',(80.4837467766038,-7.40411334087662,129.562425890288));
#77330=CARTESIAN_POINT('Ctrl Pts',(80.4135013021998,-7.38448776983677,129.567693500649));
#77331=CARTESIAN_POINT('Ctrl Pts',(80.2093058802686,-7.34163116108932,129.582866015755));
#77332=CARTESIAN_POINT('Ctrl Pts',(80.0734667500323,-7.3300860907803,129.592743571448));
#77333=CARTESIAN_POINT('Ctrl Pts',(79.9140801323266,-7.33604890318619,129.603724393727));
#77334=CARTESIAN_POINT('Ctrl Pts',(79.8904639400111,-7.3374364891958,129.605337553233));
#77335=CARTESIAN_POINT('Ctrl Pts',(79.8547895173569,-7.34029606937242,129.607754563777));
#77336=CARTESIAN_POINT('Ctrl Pts',(79.8427055028622,-7.34139767385291,129.608569839626));
#77337=CARTESIAN_POINT('Ctrl Pts',(79.8209688406627,-7.34361893242463,129.610030476796));
#77338=CARTESIAN_POINT('Ctrl Pts',(79.8113120165988,-7.34469119230794,129.61067729217));
#77339=CARTESIAN_POINT('Ctrl Pts',(79.7906497720514,-7.34716862309817,129.61205700983));
#77340=CARTESIAN_POINT('Ctrl Pts',(79.7796478468959,-7.34859937717827,129.612789075835));
#77341=CARTESIAN_POINT('Ctrl Pts',(79.7495184947372,-7.35282403856453,129.614787336265));
#77342=CARTESIAN_POINT('Ctrl Pts',(79.7304237325863,-7.35584115154222,129.616046485166));
#77343=CARTESIAN_POINT('Ctrl Pts',(79.594608376844,-7.37973077332341,129.624959911134));
#77344=CARTESIAN_POINT('Ctrl Pts',(79.4803543478131,-7.41267907807416,129.632201026817));
#77345=CARTESIAN_POINT('Ctrl Pts',(79.2790812601726,-7.49481130831862,129.645474050551));
#77346=CARTESIAN_POINT('Ctrl Pts',(79.1911208241831,-7.54019656438399,129.651491358508));
#77347=CARTESIAN_POINT('Ctrl Pts',(79.0947278034089,-7.60133112420974,129.658902404308));
#77348=CARTESIAN_POINT('Ctrl Pts',(79.0818595543526,-7.60974446418748,129.659910003334));
#77349=CARTESIAN_POINT('Ctrl Pts',(79.0632768808135,-7.62226444085727,129.661394741468));
#77350=CARTESIAN_POINT('Ctrl Pts',(79.057468692785,-7.62623138651246,129.661863114736));
#77351=CARTESIAN_POINT('Ctrl Pts',(79.04734102478,-7.63324296103815,129.662687713331));
#77352=CARTESIAN_POINT('Ctrl Pts',(79.0430106498823,-7.63627154124793,129.663042863947));
#77353=CARTESIAN_POINT('Ctrl Pts',(79.038631193083,-7.6393655806482,129.663404695187));
#77354=CARTESIAN_POINT('Ctrl Pts',(79.0385677336052,-7.63941042074669,129.663409938779));
#77355=CARTESIAN_POINT('Ctrl Pts',(79.0384037054441,-7.6395263392985,129.663423493717));
#77356=CARTESIAN_POINT('Ctrl Pts',(79.0383031414642,-7.63959742449208,129.663431805524));
#77357=CARTESIAN_POINT('Ctrl Pts',(79.0381073036602,-7.63973588801838,129.66344799465));
#77358=CARTESIAN_POINT('Ctrl Pts',(79.0380120290431,-7.6398032652035,129.66345587189));
#77359=CARTESIAN_POINT('Ctrl Pts',(79.0378262514459,-7.63993467440556,129.663471234329));
#77360=CARTESIAN_POINT('Ctrl Pts',(79.0377357477108,-7.6399987054943,129.663478719467));
#77361=CARTESIAN_POINT('Ctrl Pts',(79.0375590601058,-7.64012373784807,129.663493334703));
#77362=CARTESIAN_POINT('Ctrl Pts',(79.0374728757355,-7.64018473820744,129.663500464735));
#77363=CARTESIAN_POINT('Ctrl Pts',(79.0373044317979,-7.6403039850307,129.66351440213));
#77364=CARTESIAN_POINT('Ctrl Pts',(79.0372221716709,-7.64036223079924,129.663521209448));
#77365=CARTESIAN_POINT('Ctrl Pts',(79.0370612283736,-7.64047621153728,129.663534529926));
#77366=CARTESIAN_POINT('Ctrl Pts',(79.0369825447501,-7.64053194587682,129.663541043045));
#77367=CARTESIAN_POINT('Ctrl Pts',(79.0368284467748,-7.6406411189091,129.663553800361));
#77368=CARTESIAN_POINT('Ctrl Pts',(79.036753032093,-7.6406945570031,129.663560044514));
#77369=CARTESIAN_POINT('Ctrl Pts',(79.0366051991417,-7.6407993284438,129.663572286284));
#77370=CARTESIAN_POINT('Ctrl Pts',(79.036532780421,-7.64085066137814,129.663578283876));
#77371=CARTESIAN_POINT('Ctrl Pts',(79.0363906955298,-7.64095139320473,129.663590052536));
#77372=CARTESIAN_POINT('Ctrl Pts',(79.036321029128,-7.64100079161436,129.663595823569));
#77373=CARTESIAN_POINT('Ctrl Pts',(79.0361842307604,-7.64109780714756,129.66360715702));
#77374=CARTESIAN_POINT('Ctrl Pts',(79.0361170985661,-7.64114542385967,129.663612719407));
#77375=CARTESIAN_POINT('Ctrl Pts',(79.0359851727473,-7.64123901323716,129.663623651653));
#77376=CARTESIAN_POINT('Ctrl Pts',(79.0359203788248,-7.64128498560353,129.663629021493));
#77377=CARTESIAN_POINT('Ctrl Pts',(79.0357929526966,-7.64137541026624,129.663639583173));
#77378=CARTESIAN_POINT('Ctrl Pts',(79.0357303202857,-7.64141986225229,129.663644774991));
#77379=CARTESIAN_POINT('Ctrl Pts',(79.035607057197,-7.64150735835607,129.663654993776));
#77380=CARTESIAN_POINT('Ctrl Pts',(79.0355464263586,-7.64155040217933,129.663660020722));
#77381=CARTESIAN_POINT('Ctrl Pts',(79.0354270213497,-7.6416351837396,129.663669921687));
#77382=CARTESIAN_POINT('Ctrl Pts',(79.0353682469778,-7.64167692125265,129.663674795693));
#77383=CARTESIAN_POINT('Ctrl Pts',(79.0352524227304,-7.6417591829689,129.663684401647));
#77384=CARTESIAN_POINT('Ctrl Pts',(79.0351953726902,-7.6417997069583,129.663689133582));
#77385=CARTESIAN_POINT('Ctrl Pts',(79.0350828765919,-7.64187962625542,129.663698465307));
#77386=CARTESIAN_POINT('Ctrl Pts',(79.0350274303308,-7.64191902140844,129.66370306509));
#77387=CARTESIAN_POINT('Ctrl Pts',(79.0349180313275,-7.64199676063556,129.663712141603));
#77388=CARTESIAN_POINT('Ctrl Pts',(79.0348640784739,-7.6420351045181,129.663716618319));
#77389=CARTESIAN_POINT('Ctrl Pts',(79.0347575647386,-7.64211081257364,129.663725457055));
#77390=CARTESIAN_POINT('Ctrl Pts',(79.0347050038745,-7.64214817648842,129.663729819053));
#77391=CARTESIAN_POINT('Ctrl Pts',(79.0346011812592,-7.64222198989296,129.663738435999));
#77392=CARTESIAN_POINT('Ctrl Pts',(79.0345499192983,-7.64225843930835,129.663742690946));
#77393=CARTESIAN_POINT('Ctrl Pts',(79.0344486084306,-7.64233048424501,129.663751100877));
#77394=CARTESIAN_POINT('Ctrl Pts',(79.034398559412,-7.64236607964214,129.663755255853));
#77395=CARTESIAN_POINT('Ctrl Pts',(79.034299594889,-7.64243647250967,129.663763472395));
#77396=CARTESIAN_POINT('Ctrl Pts',(79.0342506793253,-7.64247126983627,129.66376753395));
#77397=CARTESIAN_POINT('Ctrl Pts',(79.0341539082047,-7.64254011830429,129.663775569707));
#77398=CARTESIAN_POINT('Ctrl Pts',(79.0341060525173,-7.64257416936841,129.663779543906));
#77399=CARTESIAN_POINT('Ctrl Pts',(79.034011332843,-7.64264157341076,129.66378741058));
#77400=CARTESIAN_POINT('Ctrl Pts',(79.0339644687292,-7.64267492632344,129.663791303053));
#77401=CARTESIAN_POINT('Ctrl Pts',(79.0338716684268,-7.64274097899074,129.663799011534));
#77402=CARTESIAN_POINT('Ctrl Pts',(79.0338257322336,-7.64277367860572,129.663802827531));
#77403=CARTESIAN_POINT('Ctrl Pts',(79.0337347285458,-7.64283846641518,129.663810387944));
#77404=CARTESIAN_POINT('Ctrl Pts',(79.0336896609904,-7.64287055452182,129.663814132354));
#77405=CARTESIAN_POINT('Ctrl Pts',(79.0336003391557,-7.64293415838738,129.663821554167));
#77406=CARTESIAN_POINT('Ctrl Pts',(79.0335560848077,-7.64296567407474,129.663825231565));
#77407=CARTESIAN_POINT('Ctrl Pts',(79.0334683376524,-7.64302816958831,129.663832523621));
#77408=CARTESIAN_POINT('Ctrl Pts',(79.0334248447051,-7.64305914940331,129.663836138282));
#77409=CARTESIAN_POINT('Ctrl Pts',(79.0333385715155,-7.64312060762961,129.663843308896));
#77410=CARTESIAN_POINT('Ctrl Pts',(79.0332957912819,-7.64315108593262,129.66384686484));
#77411=CARTESIAN_POINT('Ctrl Pts',(79.0332108974944,-7.64321157362305,129.663853921819));
#77412=CARTESIAN_POINT('Ctrl Pts',(79.0331687840547,-7.6432415828351,129.663857422837));
#77413=CARTESIAN_POINT('Ctrl Pts',(79.0330851814234,-7.64330116230142,129.66386437347));
#77414=CARTESIAN_POINT('Ctrl Pts',(79.0330436919574,-7.64333073266457,129.6638678231));
#77415=CARTESIAN_POINT('Ctrl Pts',(79.0329612958847,-7.64338946367549,129.663874674375));
#77416=CARTESIAN_POINT('Ctrl Pts',(79.0329203894405,-7.64341862412765,129.663878076001));
#77417=CARTESIAN_POINT('Ctrl Pts',(79.0328391216176,-7.64347656202198,129.663884834391));
#77418=CARTESIAN_POINT('Ctrl Pts',(79.0327987599985,-7.64350533956201,129.663888191169));
#77419=CARTESIAN_POINT('Ctrl Pts',(79.0327185448268,-7.64356253779469,129.663894862922));
#77420=CARTESIAN_POINT('Ctrl Pts',(79.0326786914107,-7.64359095832226,129.663898177881));
#77421=CARTESIAN_POINT('Ctrl Pts',(79.0325994583428,-7.64364746679155,129.663904768832));
#77422=CARTESIAN_POINT('Ctrl Pts',(79.0325600786426,-7.64367555470543,129.663908044823));
#77423=CARTESIAN_POINT('Ctrl Pts',(79.0324817599268,-7.64373142135731,129.663914560576));
#77424=CARTESIAN_POINT('Ctrl Pts',(79.0324428209724,-7.64375919999428,129.663917800328));
#77425=CARTESIAN_POINT('Ctrl Pts',(79.0265053569533,-7.6479953096944,129.664411834297));
#77426=CARTESIAN_POINT('Ctrl Pts',(79.0206344838947,-7.65224197882215,129.664905186614));
#77427=CARTESIAN_POINT('Ctrl Pts',(79.0078784053937,-7.66159638528165,129.665987455159));
#77428=CARTESIAN_POINT('Ctrl Pts',(79.0010045819552,-7.66671921875005,129.666577306224));
#77429=CARTESIAN_POINT('Ctrl Pts',(78.9186701944317,-7.7290744669457,129.673720143616));
#77430=CARTESIAN_POINT('Ctrl Pts',(78.8481909104483,-7.79258213981179,129.680615370289));
#77431=CARTESIAN_POINT('Ctrl Pts',(78.7005474443368,-7.95037244048865,129.696345603662));
#77432=CARTESIAN_POINT('Ctrl Pts',(78.6275229733317,-8.04783825080116,129.705113144021));
#77433=CARTESIAN_POINT('Ctrl Pts',(78.555065254074,-8.17044627079254,129.714909670994));
#77434=CARTESIAN_POINT('Ctrl Pts',(78.5447370037935,-8.18870135529724,129.716340242617));
#77435=CARTESIAN_POINT('Ctrl Pts',(78.5287781334731,-8.2181944043214,129.71860800874));
#77436=CARTESIAN_POINT('Ctrl Pts',(78.5229254807155,-8.22930897925426,129.719452982495));
#77437=CARTESIAN_POINT('Ctrl Pts',(78.5127348142947,-8.24920431973421,129.720948788938));
#77438=CARTESIAN_POINT('Ctrl Pts',(78.5083475285705,-8.25795903237727,129.721601327405));
#77439=CARTESIAN_POINT('Ctrl Pts',(78.4993114788223,-8.27639425773511,129.722963808336));
#77440=CARTESIAN_POINT('Ctrl Pts',(78.4946785956039,-8.28608208706773,129.723673175715));
#77441=CARTESIAN_POINT('Ctrl Pts',(78.4826844209806,-8.31179906385109,129.72553929064));
#77442=CARTESIAN_POINT('Ctrl Pts',(78.4754833271746,-8.32790175732582,129.726690524951));
#77443=CARTESIAN_POINT('Ctrl Pts',(78.4571826872773,-8.37063298275656,129.72970300732));
#77444=CARTESIAN_POINT('Ctrl Pts',(78.4465195527456,-8.39743395206965,129.731549510502));
#77445=CARTESIAN_POINT('Ctrl Pts',(78.4365593938057,-8.42449198884581,129.733376828424));
#77446=CARTESIAN_POINT('Origin',(80.,-9.,134.));
#77447=CARTESIAN_POINT('',(78.4345148344113,-8.42372400280583,130.432124665727));
#77448=CARTESIAN_POINT('',(78.4365593712355,-8.42449205016053,130.240113128671));
#77449=CARTESIAN_POINT('',(78.4365593749993,-8.42449203993574,134.));
#77450=CARTESIAN_POINT('Ctrl Pts',(78.4365593712355,-8.42449205016054,130.240113128671));
#77451=CARTESIAN_POINT('Ctrl Pts',(78.4562489674097,-8.37100275495381,130.236594916316));
#77452=CARTESIAN_POINT('Ctrl Pts',(78.4786723687427,-8.3185543893542,130.233028078192));
#77453=CARTESIAN_POINT('Ctrl Pts',(78.5107180139043,-8.25310858487162,130.2283009661));
#77454=CARTESIAN_POINT('Ctrl Pts',(78.5178965700835,-8.23896320842644,130.227262057371));
#77455=CARTESIAN_POINT('Ctrl Pts',(78.5286264146443,-8.21854773312112,130.225734315427));
#77456=CARTESIAN_POINT('Ctrl Pts',(78.5320183854576,-8.21219428303662,130.22525482372));
#77457=CARTESIAN_POINT('Ctrl Pts',(78.5380414429338,-8.20108654908569,130.22440904851));
#77458=CARTESIAN_POINT('Ctrl Pts',(78.5406547529564,-8.19632284260615,130.224043878242));
#77459=CARTESIAN_POINT('Ctrl Pts',(78.54640817077,-8.18595574479711,130.223243721417));
#77460=CARTESIAN_POINT('Ctrl Pts',(78.5495573437357,-8.18035778973985,130.222808190793));
#77461=CARTESIAN_POINT('Ctrl Pts',(78.5584637423665,-8.16473788328814,130.221583495256));
#77462=CARTESIAN_POINT('Ctrl Pts',(78.5642928754636,-8.15475765626252,130.220790030511));
#77463=CARTESIAN_POINT('Ctrl Pts',(78.6059234670989,-8.08515393390818,130.215183224136));
#77464=CARTESIAN_POINT('Ctrl Pts',(78.6453202268297,-8.02776893801363,130.210184040967));
#77465=CARTESIAN_POINT('Ctrl Pts',(78.6998429395048,-7.95812404811907,130.203765394012));
#77466=CARTESIAN_POINT('Ctrl Pts',(78.7117572784247,-7.94342791983462,130.202389324106));
#77467=CARTESIAN_POINT('Ctrl Pts',(78.7712000470168,-7.87260683263331,130.195659711576));
#77468=CARTESIAN_POINT('Ctrl Pts',(78.8221620006092,-7.81946468673388,130.190306651402));
#77469=CARTESIAN_POINT('Ctrl Pts',(78.9246253009635,-7.7258813575024,130.180402885944));
#77470=CARTESIAN_POINT('Ctrl Pts',(78.9753245989724,-7.68476188212218,130.175837625116));
#77471=CARTESIAN_POINT('Ctrl Pts',(79.0422169721025,-7.63673159185644,130.170222167182));
#77472=CARTESIAN_POINT('Ctrl Pts',(79.0562766590351,-7.62696126242622,130.169062960979));
#77473=CARTESIAN_POINT('Ctrl Pts',(79.0780706460221,-7.61230917767639,130.167297435918));
#77474=CARTESIAN_POINT('Ctrl Pts',(79.0856983464037,-7.60727172640133,130.166685282373));
#77475=CARTESIAN_POINT('Ctrl Pts',(79.101525269002,-7.5970054476837,130.165426768109));
#77476=CARTESIAN_POINT('Ctrl Pts',(79.109729602413,-7.59178510798048,130.164780740794));
#77477=CARTESIAN_POINT('Ctrl Pts',(79.1282824555546,-7.58020705066821,130.163333799139));
#77478=CARTESIAN_POINT('Ctrl Pts',(79.1386558078989,-7.57389001404572,130.162534402935));
#77479=CARTESIAN_POINT('Ctrl Pts',(79.1694559694582,-7.55559238631713,130.160188241922));
#77480=CARTESIAN_POINT('Ctrl Pts',(79.1900707086901,-7.54393290856342,130.158653033531));
#77481=CARTESIAN_POINT('Ctrl Pts',(79.302175072845,-7.48364570286396,130.150476769271));
#77482=CARTESIAN_POINT('Ctrl Pts',(79.3978041221713,-7.44319125698328,130.144126799862));
#77483=CARTESIAN_POINT('Ctrl Pts',(79.5714126844545,-7.38815902626617,130.133004543948));
#77484=CARTESIAN_POINT('Ctrl Pts',(79.6478218321723,-7.36975853676477,130.128231134946));
#77485=CARTESIAN_POINT('Ctrl Pts',(79.7495424799942,-7.35274947236639,130.121726987987));
#77486=CARTESIAN_POINT('Ctrl Pts',(79.773933799732,-7.34922526822217,130.120155954105));
#77487=CARTESIAN_POINT('Ctrl Pts',(79.8154182317847,-7.34416796195394,130.117451122044));
#77488=CARTESIAN_POINT('Ctrl Pts',(79.8324737224539,-7.34235556960559,130.116329723554));
#77489=CARTESIAN_POINT('Ctrl Pts',(79.8569518546057,-7.34013602473691,130.114702977381));
#77490=CARTESIAN_POINT('Ctrl Pts',(79.8643546127382,-7.33951467577272,130.114208748101));
#77491=CARTESIAN_POINT('Ctrl Pts',(79.8772524414581,-7.33851892234612,130.113343325437));
#77492=CARTESIAN_POINT('Ctrl Pts',(79.8827456069124,-7.33812222446614,130.112973368173));
#77493=CARTESIAN_POINT('Ctrl Pts',(79.8945297572386,-7.33732993115931,130.112176652894));
#77494=CARTESIAN_POINT('Ctrl Pts',(79.9008209460103,-7.33694280258446,130.111749468479));
#77495=CARTESIAN_POINT('Ctrl Pts',(79.9181195111698,-7.33597683807036,130.110570073436));
#77496=CARTESIAN_POINT('Ctrl Pts',(79.9291304381353,-7.33547154219307,130.109814037617));
#77497=CARTESIAN_POINT('Ctrl Pts',(79.9922258798403,-7.33320323179177,130.105454305496));
#77498=CARTESIAN_POINT('Ctrl Pts',(80.0443606165131,-7.33377584956241,130.10174559877));
#77499=CARTESIAN_POINT('Ctrl Pts',(80.1986023738523,-7.3427135963045,130.090608413702));
#77500=CARTESIAN_POINT('Ctrl Pts',(80.3000714787427,-7.35804993281389,130.083081385085));
#77501=CARTESIAN_POINT('Ctrl Pts',(80.4701068503262,-7.40004793807312,130.070526767085));
#77502=CARTESIAN_POINT('Ctrl Pts',(80.5395138421777,-7.42209807379113,130.065415467588));
#77503=CARTESIAN_POINT('Ctrl Pts',(80.6236694280322,-7.45503956353026,130.059248047805));
#77504=CARTESIAN_POINT('Ctrl Pts',(80.6399706537873,-7.46172047098607,130.058054549339));
#77505=CARTESIAN_POINT('Ctrl Pts',(80.6660298674103,-7.4728865674394,130.056147801498));
#77506=CARTESIAN_POINT('Ctrl Pts',(80.675855429789,-7.47720957858888,130.055429137591));
#77507=CARTESIAN_POINT('Ctrl Pts',(80.6945653749809,-7.48565827062489,130.054060908962));
#77508=CARTESIAN_POINT('Ctrl Pts',(80.7034564604505,-7.48976791562052,130.053410830928));
#77509=CARTESIAN_POINT('Ctrl Pts',(80.7236761314824,-7.49933117622764,130.051932427284));
#77510=CARTESIAN_POINT('Ctrl Pts',(80.7349803515376,-7.50483513979877,130.051105877068));
#77511=CARTESIAN_POINT('Ctrl Pts',(80.7650064928709,-7.51987753605714,130.048909509002));
#77512=CARTESIAN_POINT('Ctrl Pts',(80.7836124663331,-7.5296432377673,130.047547591853));
#77513=CARTESIAN_POINT('Ctrl Pts',(80.9078369461697,-7.59787284045522,130.038436056632));
#77514=CARTESIAN_POINT('Ctrl Pts',(81.0070169636583,-7.66731505112715,130.031103578709));
#77515=CARTESIAN_POINT('Ctrl Pts',(81.1477032665413,-7.79056635603684,130.019674552662));
#77516=CARTESIAN_POINT('Ctrl Pts',(81.1949209082573,-7.83719507999336,130.015611970953));
#77517=CARTESIAN_POINT('Ctrl Pts',(81.2542447687083,-7.90321804288564,130.009994306451));
#77518=CARTESIAN_POINT('Ctrl Pts',(81.2689181879826,-7.92022820337079,130.00855770085));
#77519=CARTESIAN_POINT('Ctrl Pts',(81.2934513075985,-7.94985907261235,130.006062863773));
#77520=CARTESIAN_POINT('Ctrl Pts',(81.3034814413055,-7.96233515116671,130.005014641894));
#77521=CARTESIAN_POINT('Ctrl Pts',(81.3177775368196,-7.98065186508941,130.003475666234));
#77522=CARTESIAN_POINT('Ctrl Pts',(81.3221880394496,-7.98637924241827,130.002994445667));
#77523=CARTESIAN_POINT('Ctrl Pts',(81.3298504479927,-7.99646457391867,130.002146696995));
#77524=CARTESIAN_POINT('Ctrl Pts',(81.3331185044392,-8.00081001940362,130.001781298783));
#77525=CARTESIAN_POINT('Ctrl Pts',(81.3401922272381,-8.01031223782528,130.000981901113));
#77526=CARTESIAN_POINT('Ctrl Pts',(81.3439893690652,-8.01547491401748,130.00054736898));
#77527=CARTESIAN_POINT('Ctrl Pts',(81.3545090794997,-8.02995200871444,129.999328574087));
#77528=CARTESIAN_POINT('Ctrl Pts',(81.3611650884005,-8.03931402857036,129.998540078512));
#77529=CARTESIAN_POINT('Ctrl Pts',(81.4054685847778,-8.1030139381261,129.993176928803));
#77530=CARTESIAN_POINT('Ctrl Pts',(81.439946061721,-8.15947675384267,129.988434194037));
#77531=CARTESIAN_POINT('Ctrl Pts',(81.4813324729098,-8.23730949777258,129.982043702622));
#77532=CARTESIAN_POINT('Ctrl Pts',(81.4913019513496,-8.25699181158267,129.980439347805));
#77533=CARTESIAN_POINT('Ctrl Pts',(81.5315342487989,-8.34049467232167,129.973693641993));
#77534=CARTESIAN_POINT('Ctrl Pts',(81.5581154647473,-8.40601201963876,129.968551867066));
#77535=CARTESIAN_POINT('Ctrl Pts',(81.6019915139492,-8.53760052806315,129.958635381771));
#77536=CARTESIAN_POINT('Ctrl Pts',(81.6195482075004,-8.60344501003612,129.953863125404));
#77537=CARTESIAN_POINT('Ctrl Pts',(81.6364567550507,-8.68716568887623,129.948037086216));
#77538=CARTESIAN_POINT('Ctrl Pts',(81.6396208598089,-8.70419686821001,129.946863960421));
#77539=CARTESIAN_POINT('Ctrl Pts',(81.6443043490202,-8.73179653056876,129.944981636755));
#77540=CARTESIAN_POINT('Ctrl Pts',(81.6459887029334,-8.74233531052925,129.944267274214));
#77541=CARTESIAN_POINT('Ctrl Pts',(81.6490275276901,-8.76259623442835,129.942902065167));
#77542=CARTESIAN_POINT('Ctrl Pts',(81.6503975686912,-8.77231555328744,129.942250753972));
#77543=CARTESIAN_POINT('Ctrl Pts',(81.6533440220763,-8.79464419258868,129.940762403013));
#77544=CARTESIAN_POINT('Ctrl Pts',(81.6548622395854,-8.80726067908265,129.939927222597));
#77545=CARTESIAN_POINT('Ctrl Pts',(81.6592931853532,-8.84800710326969,129.937247506579));
#77546=CARTESIAN_POINT('Ctrl Pts',(81.6616342006517,-8.8761951142858,129.935420781766));
#77547=CARTESIAN_POINT('Ctrl Pts',(81.6707675273531,-9.03514811038791,129.92524571895));
#77548=CARTESIAN_POINT('Ctrl Pts',(81.6628435021933,-9.16629323540851,129.917373557133));
#77549=CARTESIAN_POINT('Ctrl Pts',(81.6270065293568,-9.36536842599655,129.904962964013));
#77550=CARTESIAN_POINT('Ctrl Pts',(81.6098741333425,-9.43468066079452,129.900540853335));
#77551=CARTESIAN_POINT('Ctrl Pts',(81.5835972696578,-9.51771079301962,129.8948904473));
#77552=CARTESIAN_POINT('Ctrl Pts',(81.5786251621711,-9.5326793883301,129.893857296503));
#77553=CARTESIAN_POINT('Ctrl Pts',(81.5710795984695,-9.55436137685456,129.892336480976));
#77554=CARTESIAN_POINT('Ctrl Pts',(81.5686738463451,-9.56113278278878,129.891858038952));
#77555=CARTESIAN_POINT('Ctrl Pts',(81.5643731923813,-9.57299390013294,129.891013494545));
#77556=CARTESIAN_POINT('Ctrl Pts',(81.5624970978877,-9.57809022867613,129.890648495646));
#77557=CARTESIAN_POINT('Ctrl Pts',(81.558345404965,-9.58920025362453,129.889848050222));
#77558=CARTESIAN_POINT('Ctrl Pts',(81.556059938379,-9.59520988291922,129.889412053678));
#77559=CARTESIAN_POINT('Ctrl Pts',(81.5495543095432,-9.61202284606181,129.888184092584));
#77560=CARTESIAN_POINT('Ctrl Pts',(81.5452561288073,-9.62279531141073,129.887387787092));
#77561=CARTESIAN_POINT('Ctrl Pts',(81.5123599439697,-9.70280513425765,129.881406707882));
#77562=CARTESIAN_POINT('Ctrl Pts',(81.4792364637049,-9.77008090094177,129.87600647646));
#77563=CARTESIAN_POINT('Ctrl Pts',(81.4365724877883,-9.84375373036876,129.869820280643));
#77564=CARTESIAN_POINT('Ctrl Pts',(81.4313589715068,-9.85256809889896,129.869075423762));
#77565=CARTESIAN_POINT('Ctrl Pts',(81.3984151400417,-9.90711144748691,129.864438456259));
#77566=CARTESIAN_POINT('Ctrl Pts',(81.3685767550498,-9.95153247332523,129.860540925779));
#77567=CARTESIAN_POINT('Ctrl Pts',(81.285101803817,-10.0637330909048,129.850450789761));
#77568=CARTESIAN_POINT('Ctrl Pts',(81.2282345042584,-10.1289193882629,129.844341959158));
#77569=CARTESIAN_POINT('Ctrl Pts',(81.1535026628115,-10.2022154777481,129.837190979985));
#77570=CARTESIAN_POINT('Ctrl Pts',(81.140235942271,-10.2148055360057,129.835950952778));
#77571=CARTESIAN_POINT('Ctrl Pts',(81.1187545223984,-10.2345292857427,129.833988588503));
#77572=CARTESIAN_POINT('Ctrl Pts',(81.1106729435498,-10.2418050816921,129.833260246867));
#77573=CARTESIAN_POINT('Ctrl Pts',(81.0952084443737,-10.2554559296427,129.831884923769));
#77574=CARTESIAN_POINT('Ctrl Pts',(81.0878396792485,-10.2618462533395,129.831237321222));
#77575=CARTESIAN_POINT('Ctrl Pts',(81.0709033206699,-10.2762751343051,129.82976609731));
#77576=CARTESIAN_POINT('Ctrl Pts',(81.0613004804071,-10.2842715620653,129.828944221658));
#77577=CARTESIAN_POINT('Ctrl Pts',(81.0358744784454,-10.3049642077827,129.826799254864));
#77578=CARTESIAN_POINT('Ctrl Pts',(81.0199075182236,-10.3174810169984,129.825483298234));
#77579=CARTESIAN_POINT('Ctrl Pts',(80.8821314384003,-10.4214801146542,129.814374562119));
#77580=CARTESIAN_POINT('Ctrl Pts',(80.7485423448441,-10.4961441767399,129.805297172332));
#77581=CARTESIAN_POINT('Ctrl Pts',(80.550173775588,-10.5737038009776,129.792162596528));
#77582=CARTESIAN_POINT('Ctrl Pts',(80.4925264962668,-10.5926866937094,129.788370789343));
#77583=CARTESIAN_POINT('Ctrl Pts',(80.4198457033443,-10.6122964668454,129.783476238388));
#77584=CARTESIAN_POINT('Ctrl Pts',(80.4056626676359,-10.615923288962,129.782515797768));
#77585=CARTESIAN_POINT('Ctrl Pts',(80.3846560582215,-10.6210010319848,129.78108295452));
#77586=CARTESIAN_POINT('Ctrl Pts',(80.3778677649744,-10.6225968620248,129.780618348246));
#77587=CARTESIAN_POINT('Ctrl Pts',(80.3662539665188,-10.6252502683978,129.779820459057));
#77588=CARTESIAN_POINT('Ctrl Pts',(80.3614334607402,-10.6263290735062,129.779488387));
#77589=CARTESIAN_POINT('Ctrl Pts',(80.3503725239455,-10.6287528493538,129.778724314905));
#77590=CARTESIAN_POINT('Ctrl Pts',(80.3441292484284,-10.6300833741772,129.778291529286));
#77591=CARTESIAN_POINT('Ctrl Pts',(80.3267383617414,-10.6336852425491,129.777082082871));
#77592=CARTESIAN_POINT('Ctrl Pts',(80.3155751473921,-10.635878277052,129.776301286539));
#77593=CARTESIAN_POINT('Ctrl Pts',(80.2469302582341,-10.6486349439905,129.771476303066));
#77594=CARTESIAN_POINT('Ctrl Pts',(80.1889535691919,-10.6562810178661,129.767300688954));
#77595=CARTESIAN_POINT('Ctrl Pts',(79.9813673613194,-10.6726170396098,129.752245137594));
#77596=CARTESIAN_POINT('Ctrl Pts',(79.8310928637872,-10.6641759328561,129.741233574809));
#77597=CARTESIAN_POINT('Ctrl Pts',(79.6555558801329,-10.6302611308564,129.728852681626));
#77598=CARTESIAN_POINT('Ctrl Pts',(79.6272948034205,-10.6240332890535,129.726871439424));
#77599=CARTESIAN_POINT('Ctrl Pts',(79.58662838514,-10.6139541177168,129.724036402142));
#77600=CARTESIAN_POINT('Ctrl Pts',(79.5740846003788,-10.6106893166929,129.723164111496));
#77601=CARTESIAN_POINT('Ctrl Pts',(79.5521038005499,-10.60469357567,129.721639071754));
#77602=CARTESIAN_POINT('Ctrl Pts',(79.5426505969199,-10.6020249710547,129.720984348335));
#77603=CARTESIAN_POINT('Ctrl Pts',(79.5229870827171,-10.5962857952125,129.719624616609));
#77604=CARTESIAN_POINT('Ctrl Pts',(79.5127815089568,-10.5932004940225,129.718920120408));
#77605=CARTESIAN_POINT('Ctrl Pts',(79.4861318556273,-10.5848638704819,129.717083220198));
#77606=CARTESIAN_POINT('Ctrl Pts',(79.4697382693343,-10.5794544916105,129.715956007674));
#77607=CARTESIAN_POINT('Ctrl Pts',(79.3965460899949,-10.5540352598911,129.710931718787));
#77608=CARTESIAN_POINT('Ctrl Pts',(79.3407701251768,-10.5312084679691,129.707127905271));
#77609=CARTESIAN_POINT('Ctrl Pts',(79.1920039237619,-10.4606845608547,129.696895632408));
#77610=CARTESIAN_POINT('Ctrl Pts',(79.1020761755456,-10.4071920085322,129.690622684558));
#77611=CARTESIAN_POINT('Ctrl Pts',(78.9832026449799,-10.3204197492197,129.681531252842));
#77612=CARTESIAN_POINT('Ctrl Pts',(78.949644131555,-10.2938845495352,129.678860827546));
#77613=CARTESIAN_POINT('Ctrl Pts',(78.904070107656,-10.2549062598838,129.67502759815));
#77614=CARTESIAN_POINT('Ctrl Pts',(78.89116877281,-10.2435213347824,129.673917796747));
#77615=CARTESIAN_POINT('Ctrl Pts',(78.868779355724,-10.2231380823707,129.671942991095));
#77616=CARTESIAN_POINT('Ctrl Pts',(78.8592163837481,-10.2142238794662,129.67108326768));
#77617=CARTESIAN_POINT('Ctrl Pts',(78.8449328651977,-10.200591701573,129.669772532845));
#77618=CARTESIAN_POINT('Ctrl Pts',(78.840133879012,-10.1959561435628,129.669327506683));
#77619=CARTESIAN_POINT('Ctrl Pts',(78.8314480425868,-10.1874646512513,129.668513242234));
#77620=CARTESIAN_POINT('Ctrl Pts',(78.8275521905069,-10.1836182266586,129.66814472639));
#77621=CARTESIAN_POINT('Ctrl Pts',(78.8187624937985,-10.174854070225,129.667305794942));
#77622=CARTESIAN_POINT('Ctrl Pts',(78.8138803874055,-10.1699249517288,129.666834512977));
#77623=CARTESIAN_POINT('Ctrl Pts',(78.7989692463701,-10.1546809549692,129.665379091345));
#77624=CARTESIAN_POINT('Ctrl Pts',(78.7890432290859,-10.1442668584192,129.66438770624));
#77625=CARTESIAN_POINT('Ctrl Pts',(78.7025441790252,-10.051128486279,129.655556852204));
#77626=CARTESIAN_POINT('Ctrl Pts',(78.634421708776,-9.96096568098782,129.647274342617));
#77627=CARTESIAN_POINT('Ctrl Pts',(78.5208163862279,-9.77385308810089,129.631386140596));
#77628=CARTESIAN_POINT('Ctrl Pts',(78.4745008520548,-9.67800633567131,129.62380605576));
#77629=CARTESIAN_POINT('Ctrl Pts',(78.4310551098949,-9.56064758164267,129.615249424404));
#77630=CARTESIAN_POINT('Ctrl Pts',(78.4247907092429,-9.54279786328208,129.613966020551));
#77631=CARTESIAN_POINT('Ctrl Pts',(78.4153590588307,-9.51438368671037,129.611950596357));
#77632=CARTESIAN_POINT('Ctrl Pts',(78.4119905242534,-9.50388828584718,129.61121202972));
#77633=CARTESIAN_POINT('Ctrl Pts',(78.4061271503014,-9.48497667464124,129.609891471137));
#77634=CARTESIAN_POINT('Ctrl Pts',(78.4035942225085,-9.47657280092303,129.609308256));
#77635=CARTESIAN_POINT('Ctrl Pts',(78.3978012868829,-9.45678815845285,129.607943486356));
#77636=CARTESIAN_POINT('Ctrl Pts',(78.394595904774,-9.44539178386632,129.607163727866));
#77637=CARTESIAN_POINT('Ctrl Pts',(78.3855587994676,-9.41189559073053,129.604889752691));
#77638=CARTESIAN_POINT('Ctrl Pts',(78.3800598963578,-9.38970823716448,129.603406229091));
#77639=CARTESIAN_POINT('Ctrl Pts',(78.3567710078587,-9.28670722237465,129.596613029166));
#77640=CARTESIAN_POINT('Ctrl Pts',(78.3445596094683,-9.20474858965247,129.591479866595));
#77641=CARTESIAN_POINT('Ctrl Pts',(78.3342832475888,-9.06504004771183,129.582891624144));
#77642=CARTESIAN_POINT('Ctrl Pts',(78.3330316961664,-9.00768799540359,129.579409293732));
#77643=CARTESIAN_POINT('Ctrl Pts',(78.3370332642402,-8.87337796289595,129.571163206144));
#77644=CARTESIAN_POINT('Ctrl Pts',(78.3446663050754,-8.79663152608362,129.566381266975));
#77645=CARTESIAN_POINT('Ctrl Pts',(78.3595251353606,-8.70925440496168,129.560584047531));
#77646=CARTESIAN_POINT('Ctrl Pts',(78.3615909663109,-8.69783017632925,129.559818991777));
#77647=CARTESIAN_POINT('Ctrl Pts',(78.3649870959763,-8.68010906475886,129.558619886321));
#77648=CARTESIAN_POINT('Ctrl Pts',(78.3662348218431,-8.67379646547043,129.558190293493));
#77649=CARTESIAN_POINT('Ctrl Pts',(78.3686091834629,-8.66213932360055,129.557392187906));
#77650=CARTESIAN_POINT('Ctrl Pts',(78.3697255679078,-8.65679291054558,129.557024251764));
#77651=CARTESIAN_POINT('Ctrl Pts',(78.3723670093262,-8.64444667106826,129.556170222869));
#77652=CARTESIAN_POINT('Ctrl Pts',(78.3739109302899,-8.63745116931079,129.555683093661));
#77653=CARTESIAN_POINT('Ctrl Pts',(78.379004616887,-8.61505892765786,129.554113930225));
#77654=CARTESIAN_POINT('Ctrl Pts',(78.3827282008986,-8.5997031808566,129.553022833416));
#77655=CARTESIAN_POINT('Ctrl Pts',(78.4006109934767,-8.53028283862264,129.548028822059));
#77656=CARTESIAN_POINT('Ctrl Pts',(78.4172634050794,-8.47691200050206,129.544020612337));
#77657=CARTESIAN_POINT('Ctrl Pts',(78.4365593669558,-8.42449206178673,129.539973210016));
#77658=CARTESIAN_POINT('',(78.3314565003769,-9.00039636157243,129.771406545978));
#77659=CARTESIAN_POINT('Ctrl Pts',(78.4365593938057,-8.42449198884581,129.733376828424));
#77660=CARTESIAN_POINT('Ctrl Pts',(78.4212621561002,-8.4660488779381,129.736183301371));
#77661=CARTESIAN_POINT('Ctrl Pts',(78.4076230942358,-8.5082121619528,129.738944145127));
#77662=CARTESIAN_POINT('Ctrl Pts',(78.3774921208378,-8.61584510834271,129.745843697833));
#77663=CARTESIAN_POINT('Ctrl Pts',(78.3632688753793,-8.68185193517039,129.749938839626));
#77664=CARTESIAN_POINT('Ctrl Pts',(78.3435271826576,-8.81114823422785,129.757946195357));
#77665=CARTESIAN_POINT('Ctrl Pts',(78.3375464657446,-8.87424579974563,129.761848452997));
#77666=CARTESIAN_POINT('Ctrl Pts',(78.3343844978591,-8.95850538309094,129.767222862207));
#77667=CARTESIAN_POINT('Ctrl Pts',(78.3339938900017,-8.97949774424152,129.768575424904));
#77668=CARTESIAN_POINT('Ctrl Pts',(78.3340000722425,-9.00049062409868,129.769946575773));
#77669=CARTESIAN_POINT('Ctrl Pts',(78.331327895087,-9.000391595574,129.77148036339));
#77670=CARTESIAN_POINT('Ctrl Pts',(78.3312607934084,-9.02159739328517,129.772904623852));
#77671=CARTESIAN_POINT('Ctrl Pts',(78.3316301189342,-9.0428007934763,129.774328884314));
#77672=CARTESIAN_POINT('Ctrl Pts',(78.3535891091806,-9.6150351256133,129.81279751744));
#77673=CARTESIAN_POINT('Ctrl Pts',(78.9961810223348,-10.6940907034897,129.886886262768));
#77674=CARTESIAN_POINT('Ctrl Pts',(80.8788147299153,-10.762182300724,129.99801938076));
#77675=CARTESIAN_POINT('Ctrl Pts',(81.9571171311415,-9.21745201145648,130.10915249875));
#77676=CARTESIAN_POINT('Ctrl Pts',(81.2441915797765,-7.47370268910709,130.220285616743));
#77677=CARTESIAN_POINT('Ctrl Pts',(79.4504429588567,-7.13772696278846,130.327943005734));
#77678=CARTESIAN_POINT('Ctrl Pts',(78.6106062169705,-7.95554246370299,130.398556022063));
#77679=CARTESIAN_POINT('Ctrl Pts',(78.4345148344113,-8.42372400280583,130.432124665727));
#77680=CARTESIAN_POINT('Origin',(80.,-9.,134.));
#77681=CARTESIAN_POINT('',(78.4365594227781,-8.42449191013859,131.131996270822));
#77682=CARTESIAN_POINT('',(78.4365593749572,-8.42449204005001,130.937771468334));
#77683=CARTESIAN_POINT('',(78.4365593749993,-8.42449203993574,134.));
#77684=CARTESIAN_POINT('',(78.3340004597058,-9.00014280943258,130.276978848223));
#77685=CARTESIAN_POINT('Ctrl Pts',(78.4365593749572,-8.42449204005001,130.937771468334));
#77686=CARTESIAN_POINT('Ctrl Pts',(78.4379751786435,-8.42064582912985,130.937505217487));
#77687=CARTESIAN_POINT('Ctrl Pts',(78.4394051976635,-8.41680478221285,130.937239411317));
#77688=CARTESIAN_POINT('Ctrl Pts',(78.4707357895122,-8.3335909330545,130.931482490514));
#77689=CARTESIAN_POINT('Ctrl Pts',(78.5066420832507,-8.25660581212541,130.926197191765));
#77690=CARTESIAN_POINT('Ctrl Pts',(78.5811686898538,-8.12422985648461,130.916866704775));
#77691=CARTESIAN_POINT('Ctrl Pts',(78.6175766910789,-8.0678190663728,130.912799700205));
#77692=CARTESIAN_POINT('Ctrl Pts',(78.700583954414,-7.95480933705074,130.904182065975));
#77693=CARTESIAN_POINT('Ctrl Pts',(78.7477116502163,-7.89878397792025,130.899629813918));
#77694=CARTESIAN_POINT('Ctrl Pts',(78.8063923604581,-7.83767849066319,130.894088350327));
#77695=CARTESIAN_POINT('Ctrl Pts',(78.8145118151106,-7.82939834561506,130.893324114215));
#77696=CARTESIAN_POINT('Ctrl Pts',(78.8272678033789,-7.81665872811047,130.892126023023));
#77697=CARTESIAN_POINT('Ctrl Pts',(78.8318450286061,-7.81214002084199,130.891696612699));
#77698=CARTESIAN_POINT('Ctrl Pts',(78.8403363115843,-7.80385383711295,130.890900657176));
#77699=CARTESIAN_POINT('Ctrl Pts',(78.8442427715019,-7.80007886138395,130.890534701351));
#77700=CARTESIAN_POINT('Ctrl Pts',(78.8533621386253,-7.79135228168231,130.88968097387));
#77701=CARTESIAN_POINT('Ctrl Pts',(78.8585886828827,-7.78641527181206,130.889192132031));
#77702=CARTESIAN_POINT('Ctrl Pts',(78.8753978949519,-7.77074187647731,130.887621865087));
#77703=CARTESIAN_POINT('Ctrl Pts',(78.8871009469279,-7.76013666828329,130.886531468779));
#77704=CARTESIAN_POINT('Ctrl Pts',(78.952643580292,-7.70241807934173,130.880448871238));
#77705=CARTESIAN_POINT('Ctrl Pts',(79.0093195000568,-7.65864827724601,130.875280748648));
#77706=CARTESIAN_POINT('Ctrl Pts',(79.1777138439869,-7.54510769288029,130.86051577728));
#77707=CARTESIAN_POINT('Ctrl Pts',(79.295152273063,-7.48472191251716,130.850933429242));
#77708=CARTESIAN_POINT('Ctrl Pts',(79.4444116480076,-7.42912671411549,130.839919206391));
#77709=CARTESIAN_POINT('Ctrl Pts',(79.4705734664749,-7.42011740900082,130.838026779079));
#77710=CARTESIAN_POINT('Ctrl Pts',(79.5089588858195,-7.40795938078234,130.835303590602));
#77711=CARTESIAN_POINT('Ctrl Pts',(79.5210118700461,-7.40429166338219,130.834456045037));
#77712=CARTESIAN_POINT('Ctrl Pts',(79.5425107821774,-7.39801510220942,130.832957278427));
#77713=CARTESIAN_POINT('Ctrl Pts',(79.5519401807672,-7.39535224967844,130.832304328109));
#77714=CARTESIAN_POINT('Ctrl Pts',(79.5717351409171,-7.38995026702352,130.830942566229));
#77715=CARTESIAN_POINT('Ctrl Pts',(79.5821047842792,-7.38722768813281,130.830234316185));
#77716=CARTESIAN_POINT('Ctrl Pts',(79.6095211552821,-7.38031162845498,130.828374743925));
#77717=CARTESIAN_POINT('Ctrl Pts',(79.6266094179509,-7.37628707571677,130.827228864698));
#77718=CARTESIAN_POINT('Ctrl Pts',(79.7138357034984,-7.35719383769863,130.821441595589));
#77719=CARTESIAN_POINT('Ctrl Pts',(79.7848351438677,-7.34639544267265,130.816937575108));
#77720=CARTESIAN_POINT('Ctrl Pts',(79.9242063943786,-7.33433051378958,130.808296276992));
#77721=CARTESIAN_POINT('Ctrl Pts',(79.9923925808898,-7.33262426702841,130.804159512606));
#77722=CARTESIAN_POINT('Ctrl Pts',(80.0813617029876,-7.33585686431539,130.798710670584));
#77723=CARTESIAN_POINT('Ctrl Pts',(80.1022146132505,-7.33700744116704,130.797429602586));
#77724=CARTESIAN_POINT('Ctrl Pts',(80.18861058098,-7.34340556530168,130.792087469822));
#77725=CARTESIAN_POINT('Ctrl Pts',(80.2538284915496,-7.35213833318391,130.787973315768));
#77726=CARTESIAN_POINT('Ctrl Pts',(80.3296165436456,-7.36689233412866,130.782921575209));
#77727=CARTESIAN_POINT('Ctrl Pts',(80.3408583982308,-7.36920165299669,130.782165102061));
#77728=CARTESIAN_POINT('Ctrl Pts',(80.3583356545238,-7.37298045944227,130.78097662716));
#77729=CARTESIAN_POINT('Ctrl Pts',(80.364588208444,-7.37437013391965,130.780548957687));
#77730=CARTESIAN_POINT('Ctrl Pts',(80.3761326966877,-7.37700592996078,130.779754454781));
#77731=CARTESIAN_POINT('Ctrl Pts',(80.3814267353306,-7.37824194180872,130.779388191247));
#77732=CARTESIAN_POINT('Ctrl Pts',(80.3937470006999,-7.38118204522755,130.778531391237));
#77733=CARTESIAN_POINT('Ctrl Pts',(80.4007682535684,-7.38290597882792,130.778039757918));
#77734=CARTESIAN_POINT('Ctrl Pts',(80.4233066214429,-7.38859563955571,130.776451311067));
#77735=CARTESIAN_POINT('Ctrl Pts',(80.4387773078315,-7.3927393068761,130.775345243089));
#77736=CARTESIAN_POINT('Ctrl Pts',(80.475812514774,-7.40323334535298,130.772663327211));
#77737=CARTESIAN_POINT('Ctrl Pts',(80.4973125926134,-7.40979832050611,130.771078338583));
#77738=CARTESIAN_POINT('Ctrl Pts',(80.5817605968819,-7.4374642587155,130.764757789034));
#77739=CARTESIAN_POINT('Ctrl Pts',(80.6435539932315,-7.46188404670908,130.759924299184));
#77740=CARTESIAN_POINT('Ctrl Pts',(80.8130252587442,-7.54086063983661,130.746314159855));
#77741=CARTESIAN_POINT('Ctrl Pts',(80.9164942383467,-7.60352368730289,130.73760809624));
#77742=CARTESIAN_POINT('Ctrl Pts',(81.0289942761497,-7.68959224325825,130.727863888625));
#77743=CARTESIAN_POINT('Ctrl Pts',(81.0454438793713,-7.70267780631879,130.726430157856));
#77744=CARTESIAN_POINT('Ctrl Pts',(81.071332361068,-7.72408422160583,130.724158368675));
#77745=CARTESIAN_POINT('Ctrl Pts',(81.0809317845535,-7.7322064073299,130.72331248652));
#77746=CARTESIAN_POINT('Ctrl Pts',(81.0978435890471,-7.74684742117823,130.721815613545));
#77747=CARTESIAN_POINT('Ctrl Pts',(81.1051920659364,-7.75332344360976,130.721162908601));
#77748=CARTESIAN_POINT('Ctrl Pts',(81.1204722978016,-7.76703081163949,130.719800618051));
#77749=CARTESIAN_POINT('Ctrl Pts',(81.1283921664166,-7.77427477897728,130.719091603048));
#77750=CARTESIAN_POINT('Ctrl Pts',(81.1491205100005,-7.7936053016993,130.71722764733));
#77751=CARTESIAN_POINT('Ctrl Pts',(81.1618085235067,-7.80581948273725,130.716078197239));
#77752=CARTESIAN_POINT('Ctrl Pts',(81.2258416721733,-7.86944808258024,130.710227964373));
#77753=CARTESIAN_POINT('Ctrl Pts',(81.2739803943592,-7.92398359149619,130.705668406939));
#77754=CARTESIAN_POINT('Ctrl Pts',(81.3809287815911,-8.06242335177976,130.694867304089));
#77755=CARTESIAN_POINT('Ctrl Pts',(81.4358613894735,-8.14893308402113,130.68872635182));
#77756=CARTESIAN_POINT('Ctrl Pts',(81.5063768868028,-8.28647324729803,130.679116775095));
#77757=CARTESIAN_POINT('Ctrl Pts',(81.528031873874,-8.33411023384711,130.675810695852));
#77758=CARTESIAN_POINT('Ctrl Pts',(81.5514980860824,-8.39293205122977,130.671662912455));
#77759=CARTESIAN_POINT('Ctrl Pts',(81.5554854683014,-8.40322303379583,130.670934873472));
#77760=CARTESIAN_POINT('Ctrl Pts',(81.5615900748789,-8.41945524887713,130.669781652355));
#77761=CARTESIAN_POINT('Ctrl Pts',(81.5637763884082,-8.42537040296432,130.669360401225));
#77762=CARTESIAN_POINT('Ctrl Pts',(81.5678090009686,-8.43647425306369,130.668567494961));
#77763=CARTESIAN_POINT('Ctrl Pts',(81.5696632186497,-8.4416598639921,130.668196307275));
#77764=CARTESIAN_POINT('Ctrl Pts',(81.5739565745366,-8.45385732919949,130.667321194772));
#77765=CARTESIAN_POINT('Ctrl Pts',(81.5763745887056,-8.46087639059137,130.666816071392));
#77766=CARTESIAN_POINT('Ctrl Pts',(81.5842136674819,-8.48413549877322,130.665137709382));
#77767=CARTESIAN_POINT('Ctrl Pts',(81.5894310989104,-8.50044234283363,130.663953750486));
#77768=CARTESIAN_POINT('Ctrl Pts',(81.6015258094516,-8.54035292144257,130.661043178718));
#77769=CARTESIAN_POINT('Ctrl Pts',(81.6081335736433,-8.5640336758851,130.659305390575));
#77770=CARTESIAN_POINT('Ctrl Pts',(81.6335455273103,-8.66356154161786,130.651979361482));
#77771=CARTESIAN_POINT('Ctrl Pts',(81.6475251687453,-8.74053560742116,130.646265062631));
#77772=CARTESIAN_POINT('Ctrl Pts',(81.6674238403131,-8.92179965718661,130.633009243394));
#77773=CARTESIAN_POINT('Ctrl Pts',(81.6690521899081,-9.026249960386,130.625534035596));
#77774=CARTESIAN_POINT('Ctrl Pts',(81.6590634112011,-9.15368997235432,130.61673426691));
#77775=CARTESIAN_POINT('Ctrl Pts',(81.656721920953,-9.17715695103335,130.615126224066));
#77776=CARTESIAN_POINT('Ctrl Pts',(81.6524232451519,-9.21260392185124,130.612714844952));
#77777=CARTESIAN_POINT('Ctrl Pts',(81.6508321809667,-9.22462442536748,130.611900181043));
#77778=CARTESIAN_POINT('Ctrl Pts',(81.6477289998494,-9.24625125571113,130.610439675983));
#77779=CARTESIAN_POINT('Ctrl Pts',(81.646263752607,-9.25586363870974,130.609792391712));
#77780=CARTESIAN_POINT('Ctrl Pts',(81.6429428379427,-9.27643885969083,130.608410630332));
#77781=CARTESIAN_POINT('Ctrl Pts',(81.6410614019871,-9.28739710659669,130.607677000098));
#77782=CARTESIAN_POINT('Ctrl Pts',(81.6355939044603,-9.31743577248257,130.605671708726));
#77783=CARTESIAN_POINT('Ctrl Pts',(81.6317837427775,-9.3364740077268,130.604407164274));
#77784=CARTESIAN_POINT('Ctrl Pts',(81.6037188544358,-9.46498887986672,130.595905374797));
#77785=CARTESIAN_POINT('Ctrl Pts',(81.5687976423735,-9.57184534855465,130.589031974806));
#77786=CARTESIAN_POINT('Ctrl Pts',(81.4806404119436,-9.77098524382982,130.575732493722));
#77787=CARTESIAN_POINT('Ctrl Pts',(81.4287966779467,-9.86327755070613,130.569324840339));
#77788=CARTESIAN_POINT('Ctrl Pts',(81.3601531717696,-9.96216296114336,130.561502913589));
#77789=CARTESIAN_POINT('Ctrl Pts',(81.3515687945304,-9.97418477274017,130.560534312451));
#77790=CARTESIAN_POINT('Ctrl Pts',(81.3386226105081,-9.99181446921927,130.559084894736));
#77791=CARTESIAN_POINT('Ctrl Pts',(81.3343826924601,-9.99751153386184,130.558611943584));
#77792=CARTESIAN_POINT('Ctrl Pts',(81.3268100611465,-10.0075519999819,130.557769943426));
#77793=CARTESIAN_POINT('Ctrl Pts',(81.323492177072,-10.0119063329974,130.557401913929));
#77794=CARTESIAN_POINT('Ctrl Pts',(81.3161780712314,-10.0214077266664,130.556592461005));
#77795=CARTESIAN_POINT('Ctrl Pts',(81.3121731502927,-10.0265476507736,130.556150456456));
#77796=CARTESIAN_POINT('Ctrl Pts',(81.3005032256842,-10.041344985319,130.554866324836));
#77797=CARTESIAN_POINT('Ctrl Pts',(81.2927612267938,-10.0509407245668,130.554019113226));
#77798=CARTESIAN_POINT('Ctrl Pts',(81.2236904824365,-10.1346316171562,130.546507932999));
#77799=CARTESIAN_POINT('Ctrl Pts',(81.1561643678984,-10.2033650622613,130.539498089612));
#77800=CARTESIAN_POINT('Ctrl Pts',(80.9927268640371,-10.3432029953362,130.523841081859));
#77801=CARTESIAN_POINT('Ctrl Pts',(80.8943225059096,-10.4106373831664,130.515260103051));
#77802=CARTESIAN_POINT('Ctrl Pts',(80.7709777360487,-10.4770222091074,130.505622964162));
#77803=CARTESIAN_POINT('Ctrl Pts',(80.7522074186084,-10.4866692119515,130.504183328547));
#77804=CARTESIAN_POINT('Ctrl Pts',(80.7219462400565,-10.5015020239545,130.501904073351));
#77805=CARTESIAN_POINT('Ctrl Pts',(80.7105715758021,-10.50691829648,130.501056548512));
#77806=CARTESIAN_POINT('Ctrl Pts',(80.6902430406924,-10.516316767711,130.499557809267));
#77807=CARTESIAN_POINT('Ctrl Pts',(80.681313531692,-10.5203499182258,130.498904865735));
#77808=CARTESIAN_POINT('Ctrl Pts',(80.6625399329366,-10.5286306846625,130.497543108927));
#77809=CARTESIAN_POINT('Ctrl Pts',(80.6526893485531,-10.5328625366215,130.496834857243));
#77810=CARTESIAN_POINT('Ctrl Pts',(80.6266031420297,-10.5437722189913,130.494975260309));
#77811=CARTESIAN_POINT('Ctrl Pts',(80.6103013627048,-10.550289149343,130.493829358415));
#77812=CARTESIAN_POINT('Ctrl Pts',(80.5268691621918,-10.5821226218604,130.488041613524));
#77813=CARTESIAN_POINT('Ctrl Pts',(80.458252622996,-10.6033432241656,130.483537170095));
#77814=CARTESIAN_POINT('Ctrl Pts',(80.3222154669893,-10.6359632846762,130.474895848719));
#77815=CARTESIAN_POINT('Ctrl Pts',(80.255044083031,-10.6477716441688,130.470759456356));
#77816=CARTESIAN_POINT('Ctrl Pts',(80.1665936209609,-10.6577811642385,130.465311399429));
#77817=CARTESIAN_POINT('Ctrl Pts',(80.1458076476477,-10.6597385119645,130.464030743268));
#77818=CARTESIAN_POINT('Ctrl Pts',(80.0594209790125,-10.6662379399585,130.458688733597));
#77819=CARTESIAN_POINT('Ctrl Pts',(79.9936243433958,-10.6672843127791,130.454574285287));
#77820=CARTESIAN_POINT('Ctrl Pts',(79.9164807371749,-10.663944785375,130.449522215874));
#77821=CARTESIAN_POINT('Ctrl Pts',(79.9050205399134,-10.6633299733551,130.448765737469));
#77822=CARTESIAN_POINT('Ctrl Pts',(79.887175888407,-10.6621876387491,130.447577257663));
#77823=CARTESIAN_POINT('Ctrl Pts',(79.8807863206327,-10.6617415929644,130.447149588667));
#77824=CARTESIAN_POINT('Ctrl Pts',(79.8689784955862,-10.660848855838,130.446355088328));
#77825=CARTESIAN_POINT('Ctrl Pts',(79.8635596581383,-10.6604124748095,130.445988826901));
#77826=CARTESIAN_POINT('Ctrl Pts',(79.8509395571915,-10.6593339791497,130.445132034986));
#77827=CARTESIAN_POINT('Ctrl Pts',(79.8437402666757,-10.6586715048006,130.444640407693));
#77828=CARTESIAN_POINT('Ctrl Pts',(79.8206074879546,-10.6563909024663,130.443051995644));
#77829=CARTESIAN_POINT('Ctrl Pts',(79.8046934963907,-10.6545899243362,130.44194595692));
#77830=CARTESIAN_POINT('Ctrl Pts',(79.7665119627536,-10.6497104593924,130.439264125732));
#77831=CARTESIAN_POINT('Ctrl Pts',(79.7442762870278,-10.6464101990776,130.437679193191));
#77832=CARTESIAN_POINT('Ctrl Pts',(79.6566617277263,-10.6315886771896,130.431358999439));
#77833=CARTESIAN_POINT('Ctrl Pts',(79.5919317840731,-10.6166144268172,130.426525817943));
#77834=CARTESIAN_POINT('Ctrl Pts',(79.4126685246305,-10.5636900643682,130.412919849561));
#77835=CARTESIAN_POINT('Ctrl Pts',(79.3010903760441,-10.5171091710704,130.40421751504));
#77836=CARTESIAN_POINT('Ctrl Pts',(79.177069215543,-10.4487180775746,130.394474164678));
#77837=CARTESIAN_POINT('Ctrl Pts',(79.1588289082504,-10.4382038829372,130.393038054886));
#77838=CARTESIAN_POINT('Ctrl Pts',(79.1300111278939,-10.4208566804488,130.390763254938));
#77839=CARTESIAN_POINT('Ctrl Pts',(79.1193038486856,-10.4142449038642,130.389916708291));
#77840=CARTESIAN_POINT('Ctrl Pts',(79.1003962927541,-10.4022714174054,130.388419077895));
#77841=CARTESIAN_POINT('Ctrl Pts',(79.0921665732345,-10.3969575635843,130.387766273986));
#77842=CARTESIAN_POINT('Ctrl Pts',(79.0763844252012,-10.3865688044735,130.386512336961));
#77843=CARTESIAN_POINT('Ctrl Pts',(79.0688257856487,-10.3815040237468,130.385910857295));
#77844=CARTESIAN_POINT('Ctrl Pts',(79.0481156161052,-10.3673796630799,130.384259983483));
#77845=CARTESIAN_POINT('Ctrl Pts',(79.0350520407655,-10.3581923605481,130.383215437355));
#77846=CARTESIAN_POINT('Ctrl Pts',(78.9802666599839,-10.3184735901038,130.378818164374));
#77847=CARTESIAN_POINT('Ctrl Pts',(78.9398435683865,-10.2861951013431,130.37553308263));
#77848=CARTESIAN_POINT('Ctrl Pts',(78.8350349486768,-10.1941995420655,130.36681005697));
#77849=CARTESIAN_POINT('Ctrl Pts',(78.7737617404019,-10.1311926192413,130.361487607277));
#77850=CARTESIAN_POINT('Ctrl Pts',(78.664474129254,-9.99944280630085,130.351018855969));
#77851=CARTESIAN_POINT('Ctrl Pts',(78.6161177349635,-9.9313333045399,130.345888803918));
#77852=CARTESIAN_POINT('Ctrl Pts',(78.5649535755764,-9.84643077202604,130.339459110195));
#77853=CARTESIAN_POINT('Ctrl Pts',(78.5570283715056,-9.83284820206149,130.338429382553));
#77854=CARTESIAN_POINT('Ctrl Pts',(78.5457517353161,-9.81287758797118,130.336910672011));
#77855=CARTESIAN_POINT('Ctrl Pts',(78.5422473808255,-9.80657627343514,130.336430803434));
#77856=CARTESIAN_POINT('Ctrl Pts',(78.5361437305159,-9.79543135338164,130.335580539162));
#77857=CARTESIAN_POINT('Ctrl Pts',(78.5335273354806,-9.79059733034208,130.335211227187));
#77858=CARTESIAN_POINT('Ctrl Pts',(78.5279358262035,-9.78014325702492,130.334411331313));
#77859=CARTESIAN_POINT('Ctrl Pts',(78.5249689973576,-9.77451918705533,130.333980280205));
#77860=CARTESIAN_POINT('Ctrl Pts',(78.516690140713,-9.75860527313978,130.332758829244));
#77861=CARTESIAN_POINT('Ctrl Pts',(78.5114532225692,-9.74827706884176,130.331964057096));
#77862=CARTESIAN_POINT('Ctrl Pts',(78.4733556629172,-9.67115857451692,130.326019101976));
#77863=CARTESIAN_POINT('Ctrl Pts',(78.4449001050395,-9.60229440920325,130.320655598117));
#77864=CARTESIAN_POINT('Ctrl Pts',(78.3797244376846,-9.40878356916902,130.305821591508));
#77865=CARTESIAN_POINT('Ctrl Pts',(78.3528067216336,-9.28135729323273,130.29634947586));
#77866=CARTESIAN_POINT('Ctrl Pts',(78.3381320600553,-9.12127693737839,130.285186056999));
#77867=CARTESIAN_POINT('Ctrl Pts',(78.336166388487,-9.09039402050533,130.283062852791));
#77868=CARTESIAN_POINT('Ctrl Pts',(78.3346320841121,-9.04744096532827,130.280150357049));
#77869=CARTESIAN_POINT('Ctrl Pts',(78.334332733261,-9.03540494588075,130.279338626029));
#77870=CARTESIAN_POINT('Ctrl Pts',(78.3340552946905,-9.0156258602895,130.278011637488));
#77871=CARTESIAN_POINT('Ctrl Pts',(78.3340006704557,-9.00788450869137,130.277494013668));
#77872=CARTESIAN_POINT('Ctrl Pts',(78.334000006134,-9.00014296370202,130.276978071365));
#77873=CARTESIAN_POINT('Ctrl Pts',(78.3340000061253,-9.00014286169838,130.276978064567));
#77874=CARTESIAN_POINT('Ctrl Pts',(78.3339997367268,-8.99700123680821,130.276768688126));
#77875=CARTESIAN_POINT('Ctrl Pts',(78.3340083537072,-8.99385959459696,130.276559589479));
#77876=CARTESIAN_POINT('Ctrl Pts',(78.3340569686603,-8.98513399509389,130.275979602651));
#77877=CARTESIAN_POINT('Ctrl Pts',(78.3341161544701,-8.97955015239747,130.275609316099));
#77878=CARTESIAN_POINT('Ctrl Pts',(78.334372662962,-8.9631369346624,130.274523376322));
#77879=CARTESIAN_POINT('Ctrl Pts',(78.3346475204383,-8.95230891536532,130.273810149919));
#77880=CARTESIAN_POINT('Ctrl Pts',(78.3357842883398,-8.91996407050541,130.271688564743));
#77881=CARTESIAN_POINT('Ctrl Pts',(78.3369577962785,-8.89845994695566,130.270289889103));
#77882=CARTESIAN_POINT('Ctrl Pts',(78.3488699338953,-8.73757508373254,130.259900036097));
#77883=CARTESIAN_POINT('Ctrl Pts',(78.3766951673673,-8.60002230815777,130.251496490578));
#77884=CARTESIAN_POINT('Ctrl Pts',(78.4262408798902,-8.45312708993837,130.241988178509));
#77885=CARTESIAN_POINT('Ctrl Pts',(78.4313026982203,-8.43877247177136,130.241052411112));
#77886=CARTESIAN_POINT('Ctrl Pts',(78.4365593712355,-8.42449205016054,130.240113128671));
#77887=CARTESIAN_POINT('',(78.3344014643664,-8.99848374960743,130.471480117348));
#77888=CARTESIAN_POINT('Ctrl Pts',(78.4345148344113,-8.42372400280583,130.432124665727));
#77889=CARTESIAN_POINT('Ctrl Pts',(78.4162821667148,-8.47219996057315,130.435600394726));
#77890=CARTESIAN_POINT('Ctrl Pts',(78.3564961095336,-8.65837616141247,130.4487188786));
#77891=CARTESIAN_POINT('Ctrl Pts',(78.3331165493187,-8.85422408541304,130.461837362474));
#77892=CARTESIAN_POINT('Ctrl Pts',(78.3344014643664,-8.99848374960743,130.471480117348));
#77893=CARTESIAN_POINT('Ctrl Pts',(78.3340007022079,-8.99847037383078,130.471710616873));
#77894=CARTESIAN_POINT('Ctrl Pts',(78.3339349962914,-9.07003427155384,130.476898790049));
#77895=CARTESIAN_POINT('Ctrl Pts',(78.3384804025895,-9.14153633045385,130.482027598063));
#77896=CARTESIAN_POINT('Ctrl Pts',(78.3517548529112,-9.24474170582688,130.489298976558));
#77897=CARTESIAN_POINT('Ctrl Pts',(78.3568386683126,-9.27682423362049,130.491541426185));
#77898=CARTESIAN_POINT('Ctrl Pts',(78.3651641916091,-9.32097168702806,130.494603337894));
#77899=CARTESIAN_POINT('Ctrl Pts',(78.3676080353816,-9.33317777945166,130.495447392491));
#77900=CARTESIAN_POINT('Ctrl Pts',(78.3721676567293,-9.35469566604922,130.496931158938));
#77901=CARTESIAN_POINT('Ctrl Pts',(78.3742270887476,-9.36401868212237,130.49757262701));
#77902=CARTESIAN_POINT('Ctrl Pts',(78.3785607079475,-9.38286615914597,130.498866758121));
#77903=CARTESIAN_POINT('Ctrl Pts',(78.3808389486926,-9.39238930999188,130.499519262949));
#77904=CARTESIAN_POINT('Ctrl Pts',(78.3857896109931,-9.41230566956377,130.500881216119));
#77905=CARTESIAN_POINT('Ctrl Pts',(78.3884787640826,-9.42269428717302,130.501590093497));
#77906=CARTESIAN_POINT('Ctrl Pts',(78.395845467767,-9.45006035456796,130.50345385919));
#77907=CARTESIAN_POINT('Ctrl Pts',(78.4006922195962,-9.46699116488763,130.504603256466));
#77908=CARTESIAN_POINT('Ctrl Pts',(78.4246464313182,-9.54591694311443,130.509948632133));
#77909=CARTESIAN_POINT('Ctrl Pts',(78.4470968889685,-9.60684226960879,130.514034925297));
#77910=CARTESIAN_POINT('Ctrl Pts',(78.5114041204336,-9.75421267713005,130.523999465394));
#77911=CARTESIAN_POINT('Ctrl Pts',(78.5572802094065,-9.83863802790201,130.529775232375));
#77912=CARTESIAN_POINT('Ctrl Pts',(78.6438709655651,-9.96964258787924,130.539459137901));
#77913=CARTESIAN_POINT('Ctrl Pts',(78.6803554417283,-10.0187390846018,130.543280858618));
#77914=CARTESIAN_POINT('Ctrl Pts',(78.7284371630885,-10.0765135101543,130.548170346282));
#77915=CARTESIAN_POINT('Ctrl Pts',(78.7375602322723,-10.0871978600399,130.549092228681));
#77916=CARTESIAN_POINT('Ctrl Pts',(78.751459540794,-10.1030649862324,130.55049035203));
#77917=CARTESIAN_POINT('Ctrl Pts',(78.7561355921269,-10.1083352256711,130.550959657423));
#77918=CARTESIAN_POINT('Ctrl Pts',(78.7641519328284,-10.1172555816057,130.551762745771));
#77919=CARTESIAN_POINT('Ctrl Pts',(78.7674752795892,-10.1209207342306,130.552095272333));
#77920=CARTESIAN_POINT('Ctrl Pts',(78.7750891478601,-10.1292428872085,130.552856242805));
#77921=CARTESIAN_POINT('Ctrl Pts',(78.7793898269372,-10.1338901604976,130.553285435664));
#77922=CARTESIAN_POINT('Ctrl Pts',(78.7913398032136,-10.1466564258724,130.554475964399));
#77923=CARTESIAN_POINT('Ctrl Pts',(78.7990441471252,-10.1547231066074,130.555241240959));
#77924=CARTESIAN_POINT('Ctrl Pts',(78.8446863825659,-10.2015610418966,130.559758495396));
#77925=CARTESIAN_POINT('Ctrl Pts',(78.8844151630289,-10.2385345094071,130.563624042726));
#77926=CARTESIAN_POINT('Ctrl Pts',(79.0023348661794,-10.3379933616657,130.574756164542));
#77927=CARTESIAN_POINT('Ctrl Pts',(79.0844569030679,-10.3954728708792,130.582104453583));
#77928=CARTESIAN_POINT('Ctrl Pts',(79.234327251112,-10.4814149119788,130.594488158848));
#77929=CARTESIAN_POINT('Ctrl Pts',(79.2997232162067,-10.5134265584611,130.59959835429));
#77930=CARTESIAN_POINT('Ctrl Pts',(79.3833014121684,-10.5477561184446,130.605764416584));
#77931=CARTESIAN_POINT('Ctrl Pts',(79.3996974180764,-10.5541888565728,130.606957609198));
#77932=CARTESIAN_POINT('Ctrl Pts',(79.4262434251179,-10.5641210139541,130.608863843208));
#77933=CARTESIAN_POINT('Ctrl Pts',(79.4363302411152,-10.5677842854651,130.609582296842));
#77934=CARTESIAN_POINT('Ctrl Pts',(79.4556870709455,-10.5746032219618,130.610950104293));
#77935=CARTESIAN_POINT('Ctrl Pts',(79.4649508511102,-10.5777751064724,130.611599971338));
#77936=CARTESIAN_POINT('Ctrl Pts',(79.4861676535505,-10.584831305075,130.613077860562));
#77937=CARTESIAN_POINT('Ctrl Pts',(79.4981378380038,-10.5886624344247,130.613904108824));
#77938=CARTESIAN_POINT('Ctrl Pts',(79.5302234525753,-10.5985327799545,130.61609957673));
#77939=CARTESIAN_POINT('Ctrl Pts',(79.5504120410543,-10.604327829163,130.617460902834));
#77940=CARTESIAN_POINT('Ctrl Pts',(79.6878855308817,-10.6409900307895,130.626607855615));
#77941=CARTESIAN_POINT('Ctrl Pts',(79.8081290242379,-10.6593532170167,130.633971881391));
#77942=CARTESIAN_POINT('Ctrl Pts',(79.9951672340737,-10.6672964652315,130.645411826756));
#77943=CARTESIAN_POINT('Ctrl Pts',(80.0611267486218,-10.6661822004068,130.649451503037));
#77944=CARTESIAN_POINT('Ctrl Pts',(80.1491626392878,-10.6594600465141,130.655040270119));
#77945=CARTESIAN_POINT('Ctrl Pts',(80.1714460790178,-10.6573060312199,130.656472101945));
#77946=CARTESIAN_POINT('Ctrl Pts',(80.2095354739301,-10.6528477797081,130.658959373959));
#77947=CARTESIAN_POINT('Ctrl Pts',(80.2253645281284,-10.6507639690004,130.660004881676));
#77948=CARTESIAN_POINT('Ctrl Pts',(80.2483040931285,-10.6474080250113,130.661540487815));
#77949=CARTESIAN_POINT('Ctrl Pts',(80.2554406826258,-10.6463165480506,130.6620211072));
#77950=CARTESIAN_POINT('Ctrl Pts',(80.2679360840632,-10.6443222876067,130.662868041826));
#77951=CARTESIAN_POINT('Ctrl Pts',(80.2732979144741,-10.6434396184187,130.663233231789));
#77952=CARTESIAN_POINT('Ctrl Pts',(80.2849738446537,-10.6414587959512,130.664032418627));
#77953=CARTESIAN_POINT('Ctrl Pts',(80.2912858560192,-10.6403504557155,130.66446695004));
#77954=CARTESIAN_POINT('Ctrl Pts',(80.3089030958394,-10.637152116998,130.665686426224));
#77955=CARTESIAN_POINT('Ctrl Pts',(80.3201930617965,-10.6349815172269,130.666475615621));
#77956=CARTESIAN_POINT('Ctrl Pts',(80.3967805439833,-10.6194332116624,130.67187752762));
#77957=CARTESIAN_POINT('Ctrl Pts',(80.4612401564026,-10.6022653519447,130.676661174944));
#77958=CARTESIAN_POINT('Ctrl Pts',(80.5449875676661,-10.5744875039766,130.683058938858));
#77959=CARTESIAN_POINT('Ctrl Pts',(80.5653502840295,-10.567291098561,130.684629520004));
#77960=CARTESIAN_POINT('Ctrl Pts',(80.6530219722544,-10.5343760330184,130.691445250736));
#77961=CARTESIAN_POINT('Ctrl Pts',(80.7187668878932,-10.5047002537558,130.696690519489));
#77962=CARTESIAN_POINT('Ctrl Pts',(80.8413634571602,-10.4394880833444,130.706610484027));
#77963=CARTESIAN_POINT('Ctrl Pts',(80.8984060004816,-10.4045950053442,130.711290522432));
#77964=CARTESIAN_POINT('Ctrl Pts',(80.9673362819525,-10.3565077860403,130.717022665434));
#77965=CARTESIAN_POINT('Ctrl Pts',(80.9813136869283,-10.3464309646386,130.718189470369));
#77966=CARTESIAN_POINT('Ctrl Pts',(81.0036733627508,-10.3297778704295,130.720063965301));
#77967=CARTESIAN_POINT('Ctrl Pts',(81.0121529828278,-10.3233350869063,130.720776746996));
#77968=CARTESIAN_POINT('Ctrl Pts',(81.0283289145614,-10.3107982281401,130.722140409185));
#77969=CARTESIAN_POINT('Ctrl Pts',(81.0360342555722,-10.3047165898122,130.722791740303));
#77970=CARTESIAN_POINT('Ctrl Pts',(81.0536148448369,-10.2905867024288,130.724282179668));
#77971=CARTESIAN_POINT('Ctrl Pts',(81.0634525138686,-10.2824925120503,130.725119405891));
#77972=CARTESIAN_POINT('Ctrl Pts',(81.0949848363604,-10.255936166672,130.727814502186));
#77973=CARTESIAN_POINT('Ctrl Pts',(81.1162998049607,-10.2370296464228,130.729654255701));
#77974=CARTESIAN_POINT('Ctrl Pts',(81.2326405640691,-10.1283772925202,130.739825103638));
#77975=CARTESIAN_POINT('Ctrl Pts',(81.3173305023669,-10.0282416172791,130.747682960545));
#77976=CARTESIAN_POINT('Ctrl Pts',(81.4287681531836,-9.85979973806537,130.760075036412));
#77977=CARTESIAN_POINT('Ctrl Pts',(81.464228715595,-9.79791350891299,130.764492911404));
#77978=CARTESIAN_POINT('Ctrl Pts',(81.5025598138242,-9.719804482804,130.770138126559));
#77979=CARTESIAN_POINT('Ctrl Pts',(81.5093029094214,-9.70555593044175,130.771170688264));
#77980=CARTESIAN_POINT('Ctrl Pts',(81.5188227689612,-9.68467875259524,130.772690706941));
#77981=CARTESIAN_POINT('Ctrl Pts',(81.5217606540628,-9.67812395974106,130.773168951957));
#77982=CARTESIAN_POINT('Ctrl Pts',(81.5268450210865,-9.66658065754449,130.77401327899));
#77983=CARTESIAN_POINT('Ctrl Pts',(81.5290096381502,-9.66160034506998,130.774378259752));
#77984=CARTESIAN_POINT('Ctrl Pts',(81.5336853733046,-9.65069698105437,130.775178924295));
#77985=CARTESIAN_POINT('Ctrl Pts',(81.5361865080277,-9.64477003225855,130.775615160342));
#77986=CARTESIAN_POINT('Ctrl Pts',(81.5431038140211,-9.62810933413548,130.77684393083));
#77987=CARTESIAN_POINT('Ctrl Pts',(81.5474421305327,-9.61734394814327,130.7776408096));
#77988=CARTESIAN_POINT('Ctrl Pts',(81.5797035290483,-9.53481119429368,130.783767442007));
#77989=CARTESIAN_POINT('Ctrl Pts',(81.6027298466803,-9.4612381194497,130.789324547852));
#77990=CARTESIAN_POINT('Ctrl Pts',(81.6338713713232,-9.33061058580814,130.799085601361));
#77991=CARTESIAN_POINT('Ctrl Pts',(81.6442748597005,-9.27422521883321,130.803266799623));
#77992=CARTESIAN_POINT('Ctrl Pts',(81.6625427760792,-9.13543976952625,130.813381921777));
#77993=CARTESIAN_POINT('Ctrl Pts',(81.6672167964606,-9.05276509734269,130.819253342362));
#77994=CARTESIAN_POINT('Ctrl Pts',(81.6653211370544,-8.94724904151348,130.826508511372));
#77995=CARTESIAN_POINT('Ctrl Pts',(81.664441948953,-8.92443386100817,130.828063657201));
#77996=CARTESIAN_POINT('Ctrl Pts',(81.662396235259,-8.88984341716917,130.830401903338));
#77997=CARTESIAN_POINT('Ctrl Pts',(81.6615728292183,-8.8780513983945,130.831195577415));
#77998=CARTESIAN_POINT('Ctrl Pts',(81.6599206693514,-8.85753548451438,130.83257071638));
#77999=CARTESIAN_POINT('Ctrl Pts',(81.6591484689769,-8.8488076402864,130.833153924702));
#78000=CARTESIAN_POINT('Ctrl Pts',(81.657251608415,-8.82913718673916,130.834464461788));
#78001=CARTESIAN_POINT('Ctrl Pts',(81.6560873480727,-8.81819873523137,130.835190522481));
#78002=CARTESIAN_POINT('Ctrl Pts',(81.6526323147927,-8.78853282324315,130.837152825602));
#78003=CARTESIAN_POINT('Ctrl Pts',(81.6501315873015,-8.76983109164512,130.838382462097));
#78004=CARTESIAN_POINT('Ctrl Pts',(81.6325665270246,-8.65354377805336,130.845989601109));
#78005=CARTESIAN_POINT('Ctrl Pts',(81.6091687584517,-8.5574111158663,130.852091928085));
#78006=CARTESIAN_POINT('Ctrl Pts',(81.5546416263406,-8.39697167087249,130.862457980312));
#78007=CARTESIAN_POINT('Ctrl Pts',(81.5276565773295,-8.33155519145757,130.866745363976));
#78008=CARTESIAN_POINT('Ctrl Pts',(81.4800461213261,-8.23420691757921,130.873469238923));
#78009=CARTESIAN_POINT('Ctrl Pts',(81.4623505494835,-8.20093425361032,130.875833686416));
#78010=CARTESIAN_POINT('Ctrl Pts',(81.4319356984658,-8.14814507655618,130.879739252365));
#78011=CARTESIAN_POINT('Ctrl Pts',(81.4199079247614,-8.12824429516696,130.881248666677));
#78012=CARTESIAN_POINT('Ctrl Pts',(81.4029979605197,-8.10154436312205,130.883334011098));
#78013=CARTESIAN_POINT('Ctrl Pts',(81.3984745951529,-8.09451968100571,130.883888458908));
#78014=CARTESIAN_POINT('Ctrl Pts',(81.3907978027002,-8.08279253905306,130.884824371434));
#78015=CARTESIAN_POINT('Ctrl Pts',(81.3876728141512,-8.07807147025708,130.885203984046));
#78016=CARTESIAN_POINT('Ctrl Pts',(81.3812325122673,-8.06844873248295,130.88598374448));
#78017=CARTESIAN_POINT('Ctrl Pts',(81.377915063145,-8.06354867027114,130.886384020439));
#78018=CARTESIAN_POINT('Ctrl Pts',(81.3691722055018,-8.05078201105671,130.887435104111));
#78019=CARTESIAN_POINT('Ctrl Pts',(81.3637051862832,-8.04294437312531,130.888088589271));
#78020=CARTESIAN_POINT('Ctrl Pts',(81.3403033530246,-8.01000262850932,130.890868655212));
#78021=CARTESIAN_POINT('Ctrl Pts',(81.3217415758271,-7.98535385856593,130.893031748975));
#78022=CARTESIAN_POINT('Ctrl Pts',(81.285084696454,-7.93938971865251,130.897205550448));
#78023=CARTESIAN_POINT('Ctrl Pts',(81.2671154623649,-7.91798562025579,130.899210828371));
#78024=CARTESIAN_POINT('Ctrl Pts',(81.1837249630317,-7.8235821568325,130.908305867638));
#78025=CARTESIAN_POINT('Ctrl Pts',(81.112471366274,-7.75598519805464,130.915503351778));
#78026=CARTESIAN_POINT('Ctrl Pts',(80.9782578558318,-7.64946555261912,130.927789459145));
#78027=CARTESIAN_POINT('Ctrl Pts',(80.9178753618898,-7.60772156917584,130.932942943766));
#78028=CARTESIAN_POINT('Ctrl Pts',(80.8397846694581,-7.5610319318352,130.939152342283));
#78029=CARTESIAN_POINT('Ctrl Pts',(80.8244956027776,-7.55221740760362,130.940347971198));
#78030=CARTESIAN_POINT('Ctrl Pts',(80.7996816476042,-7.53843215060789,130.942257135475));
#78031=CARTESIAN_POINT('Ctrl Pts',(80.7902440582646,-7.53330792133854,130.942976113034));
#78032=CARTESIAN_POINT('Ctrl Pts',(80.7721096005433,-7.52368750058408,130.944344317003));
#78033=CARTESIAN_POINT('Ctrl Pts',(80.7634213915043,-7.51917603437965,130.944994062325));
#78034=CARTESIAN_POINT('Ctrl Pts',(80.7435029479819,-7.50905501954871,130.946470856878));
#78035=CARTESIAN_POINT('Ctrl Pts',(80.732247980091,-7.50349524611999,130.947296141659));
#78036=CARTESIAN_POINT('Ctrl Pts',(80.7020458272479,-7.48899818728424,130.949487225157));
#78037=CARTESIAN_POINT('Ctrl Pts',(80.682990739516,-7.48028998357588,130.950845181426));
#78038=CARTESIAN_POINT('Ctrl Pts',(80.5520955391911,-7.42343014636041,130.960020689904));
#78039=CARTESIAN_POINT('Ctrl Pts',(80.4354321426459,-7.3873051455299,130.967412568938));
#78040=CARTESIAN_POINT('Ctrl Pts',(80.2514272741726,-7.3517745597988,130.978865153797));
#78041=CARTESIAN_POINT('Ctrl Pts',(80.1863171475013,-7.34315134885402,130.982887875269));
#78042=CARTESIAN_POINT('Ctrl Pts',(80.0986023530793,-7.3367705492934,130.988455299123));
#78043=CARTESIAN_POINT('Ctrl Pts',(80.0763019554807,-7.33559844323361,130.989883661545));
#78044=CARTESIAN_POINT('Ctrl Pts',(80.038058757277,-7.33435854068887,130.992365482683));
#78045=CARTESIAN_POINT('Ctrl Pts',(80.0221257547304,-7.33407072618035,130.993409066881));
#78046=CARTESIAN_POINT('Ctrl Pts',(79.9989775909897,-7.33398469388084,130.994942358131));
#78047=CARTESIAN_POINT('Ctrl Pts',(79.9917634494024,-7.33400474191033,130.995422626066));
#78048=CARTESIAN_POINT('Ctrl Pts',(79.979067267385,-7.33412248895304,130.996272462684));
#78049=CARTESIAN_POINT('Ctrl Pts',(79.973585239474,-7.33420039613402,130.996640936562));
#78050=CARTESIAN_POINT('Ctrl Pts',(79.9616716768041,-7.33442852931824,130.997445117796));
#78051=CARTESIAN_POINT('Ctrl Pts',(79.9552406947495,-7.33458894401272,130.99788134771));
#78052=CARTESIAN_POINT('Ctrl Pts',(79.9372100727314,-7.33514320966316,130.99911008477));
#78053=CARTESIAN_POINT('Ctrl Pts',(79.92561364928,-7.33562102893979,130.999906935883));
#78054=CARTESIAN_POINT('Ctrl Pts',(79.8372212372407,-7.34018873811724,131.006026392456));
#78055=CARTESIAN_POINT('Ctrl Pts',(79.760794240132,-7.34947030524099,131.011575748592));
#78056=CARTESIAN_POINT('Ctrl Pts',(79.6291675076378,-7.37479057317232,131.021318573695));
#78057=CARTESIAN_POINT('Ctrl Pts',(79.5736352839467,-7.38846786895871,131.025489219892));
#78058=CARTESIAN_POINT('Ctrl Pts',(79.4395576803271,-7.42890772652891,131.035609628235));
#78059=CARTESIAN_POINT('Ctrl Pts',(79.3620876943569,-7.45873492602896,131.041496341761));
#78060=CARTESIAN_POINT('Ctrl Pts',(79.2664930760454,-7.50398999017591,131.048767739415));
#78061=CARTESIAN_POINT('Ctrl Pts',(79.246038392162,-7.51419370682019,131.050324718605));
#78062=CARTESIAN_POINT('Ctrl Pts',(79.2153282633118,-7.53031088130757,131.052665130445));
#78063=CARTESIAN_POINT('Ctrl Pts',(79.2049158712771,-7.53591766600507,131.053459166687));
#78064=CARTESIAN_POINT('Ctrl Pts',(79.1868936858972,-7.54587108630127,131.054834704235));
#78065=CARTESIAN_POINT('Ctrl Pts',(79.1792569649429,-7.55016771620758,131.055417952201));
#78066=CARTESIAN_POINT('Ctrl Pts',(79.162113886921,-7.55999174534771,131.056728286416));
#78067=CARTESIAN_POINT('Ctrl Pts',(79.1526275785951,-7.56555345127182,131.057454107168));
#78068=CARTESIAN_POINT('Ctrl Pts',(79.1270319199945,-7.58090239872992,131.059415030927));
#78069=CARTESIAN_POINT('Ctrl Pts',(79.1110321679757,-7.59086994525747,131.060643544204));
#78070=CARTESIAN_POINT('Ctrl Pts',(79.0091997788899,-7.65673452824745,131.068488277696));
#78071=CARTESIAN_POINT('Ctrl Pts',(78.9285035260769,-7.72017720525288,131.074805814438));
#78072=CARTESIAN_POINT('Ctrl Pts',(78.7941286541876,-7.84749654549597,131.08612265459));
#78073=CARTESIAN_POINT('Ctrl Pts',(78.7384386361225,-7.90873871294369,131.091130846483));
#78074=CARTESIAN_POINT('Ctrl Pts',(78.6702836766794,-7.99591122926426,131.098074883096));
#78075=CARTESIAN_POINT('Ctrl Pts',(78.653599824774,-8.01839613359637,131.099851652771));
#78076=CARTESIAN_POINT('Ctrl Pts',(78.6266524900329,-8.05669337869112,131.10287387624));
#78077=CARTESIAN_POINT('Ctrl Pts',(78.6160762103203,-8.07227933281521,131.104102775823));
#78078=CARTESIAN_POINT('Ctrl Pts',(78.6015482732039,-8.09449010836787,131.105857639076));
#78079=CARTESIAN_POINT('Ctrl Pts',(78.5973744748722,-8.10096884008838,131.106369946345));
#78080=CARTESIAN_POINT('Ctrl Pts',(78.590274796018,-8.11215901988406,131.107255969064));
#78081=CARTESIAN_POINT('Ctrl Pts',(78.5873272327987,-8.11685651863825,131.10762826374));
#78082=CARTESIAN_POINT('Ctrl Pts',(78.5811559200268,-8.12680162410432,131.108417344547));
#78083=CARTESIAN_POINT('Ctrl Pts',(78.5779378438558,-8.13205233572931,131.108834448185));
#78084=CARTESIAN_POINT('Ctrl Pts',(78.5692311393943,-8.14643686832164,131.109978205508));
#78085=CARTESIAN_POINT('Ctrl Pts',(78.5638010279701,-8.15560551268972,131.110708417531));
#78086=CARTESIAN_POINT('Ctrl Pts',(78.5367500253487,-8.2022964846864,131.114430542781));
#78087=CARTESIAN_POINT('Ctrl Pts',(78.5165118726414,-8.24059651117372,131.117494917529));
#78088=CARTESIAN_POINT('Ctrl Pts',(78.4751020078549,-8.32695065359558,131.12436273958));
#78089=CARTESIAN_POINT('Ctrl Pts',(78.4546708836615,-8.37528983399627,131.128179703618));
#78090=CARTESIAN_POINT('Ctrl Pts',(78.4365594227781,-8.42449191013859,131.131996270822));
#78091=CARTESIAN_POINT('Origin',(80.,-9.,134.));
#78092=CARTESIAN_POINT('',(78.4365593750065,-8.42449203991615,131.833731407018));
#78093=CARTESIAN_POINT('',(78.4365593409241,-8.42449213250519,131.638964580993));
#78094=CARTESIAN_POINT('',(78.4365593749993,-8.42449203993574,134.));
#78095=CARTESIAN_POINT('Ctrl Pts',(78.4365593409241,-8.42449213250519,131.638964580993));
#78096=CARTESIAN_POINT('Ctrl Pts',(78.4458655786914,-8.39921054848143,131.637009426607));
#78097=CARTESIAN_POINT('Ctrl Pts',(78.45578681441,-8.37414987847205,131.635060102878));
#78098=CARTESIAN_POINT('Ctrl Pts',(78.4868519260182,-8.30092644683857,131.629339976712));
#78099=CARTESIAN_POINT('Ctrl Pts',(78.5096700688799,-8.25351589953718,131.625605512207));
#78100=CARTESIAN_POINT('Ctrl Pts',(78.5460367147342,-8.18629555394418,131.620279049753));
#78101=CARTESIAN_POINT('Ctrl Pts',(78.5578278365022,-8.16557582110753,131.618632423778));
#78102=CARTESIAN_POINT('Ctrl Pts',(78.5800172557813,-8.12846024571771,131.615673421396));
#78103=CARTESIAN_POINT('Ctrl Pts',(78.5902650070094,-8.1119798189514,131.614356053443));
#78104=CARTESIAN_POINT('Ctrl Pts',(78.6068326692018,-8.08634560308722,131.612300613037));
#78105=CARTESIAN_POINT('Ctrl Pts',(78.6129600127437,-8.07707007160663,131.611555520689));
#78106=CARTESIAN_POINT('Ctrl Pts',(78.6246201136149,-8.05979751678223,131.610165217369));
#78107=CARTESIAN_POINT('Ctrl Pts',(78.6301309035784,-8.0517863073952,131.609519219788));
#78108=CARTESIAN_POINT('Ctrl Pts',(78.6426719589249,-8.03389252008994,131.608073432858));
#78109=CARTESIAN_POINT('Ctrl Pts',(78.6497406821475,-8.02403746928345,131.607275150101));
#78110=CARTESIAN_POINT('Ctrl Pts',(78.6708760989417,-7.99524018386758,131.604935709937));
#78111=CARTESIAN_POINT('Ctrl Pts',(78.6852386309918,-7.97651806824382,131.603406005969));
#78112=CARTESIAN_POINT('Ctrl Pts',(78.7642767000292,-7.8778996173458,131.595286882628));
#78113=CARTESIAN_POINT('Ctrl Pts',(78.8358459349932,-7.80381022204583,131.58898361292));
#78114=CARTESIAN_POINT('Ctrl Pts',(78.9738804213262,-7.68511820104678,131.577865215615));
#78115=CARTESIAN_POINT('Ctrl Pts',(79.0375709331692,-7.63780908912981,131.573048674426));
#78116=CARTESIAN_POINT('Ctrl Pts',(79.1252629771434,-7.58190110541228,131.566491204802));
#78117=CARTESIAN_POINT('Ctrl Pts',(79.1464387070191,-7.56905544365617,131.564912614831));
#78118=CARTESIAN_POINT('Ctrl Pts',(79.1828054296177,-7.54808905865068,131.562196030298));
#78119=CARTESIAN_POINT('Ctrl Pts',(79.1978508139614,-7.53972298034343,131.561070575995));
#78120=CARTESIAN_POINT('Ctrl Pts',(79.2195800071615,-7.52807745154977,131.559438959644));
#78121=CARTESIAN_POINT('Ctrl Pts',(79.2261609327953,-7.52460701957523,131.558944006111));
#78122=CARTESIAN_POINT('Ctrl Pts',(79.2376550203745,-7.51864370112384,131.558077754094));
#78123=CARTESIAN_POINT('Ctrl Pts',(79.2425576551244,-7.51613092040974,131.557707698912));
#78124=CARTESIAN_POINT('Ctrl Pts',(79.2530910098671,-7.51079799368046,131.556911295267));
#78125=CARTESIAN_POINT('Ctrl Pts',(79.2587251890072,-7.5079854871808,131.556484524989));
#78126=CARTESIAN_POINT('Ctrl Pts',(79.2742412935967,-7.50034963484902,131.555307364634));
#78127=CARTESIAN_POINT('Ctrl Pts',(79.2841550317748,-7.49559218196858,131.554553172224));
#78128=CARTESIAN_POINT('Ctrl Pts',(79.3407539751862,-7.46911730288394,131.550238673728));
#78129=CARTESIAN_POINT('Ctrl Pts',(79.3883748931019,-7.44947725096099,131.546575858626));
#78130=CARTESIAN_POINT('Ctrl Pts',(79.527155106851,-7.39962932382511,131.535949581446));
#78131=CARTESIAN_POINT('Ctrl Pts',(79.6201227032875,-7.37504987889197,131.528899677945));
#78132=CARTESIAN_POINT('Ctrl Pts',(79.7665216443112,-7.34960268970617,131.518213422867));
#78133=CARTESIAN_POINT('Ctrl Pts',(79.818752213746,-7.34305294148303,131.514477205166));
#78134=CARTESIAN_POINT('Ctrl Pts',(79.8949812530474,-7.33714235290396,131.509148545286));
#78135=CARTESIAN_POINT('Ctrl Pts',(79.9187907712315,-7.3358096106454,131.507501424643));
#78136=CARTESIAN_POINT('Ctrl Pts',(79.9620192377495,-7.33431990755659,131.504541625467));
#78137=CARTESIAN_POINT('Ctrl Pts',(79.9814275835736,-7.33399044742003,131.503223951292));
#78138=CARTESIAN_POINT('Ctrl Pts',(80.0119550658292,-7.33400580258322,131.50116814413));
#78139=CARTESIAN_POINT('Ctrl Pts',(80.0230720345102,-7.33412266927534,131.500422987071));
#78140=CARTESIAN_POINT('Ctrl Pts',(80.0439083220803,-7.33455033143151,131.499032625192));
#78141=CARTESIAN_POINT('Ctrl Pts',(80.0536276446551,-7.33483495656921,131.498386633122));
#78142=CARTESIAN_POINT('Ctrl Pts',(80.0754613864867,-7.33566571254057,131.496940938652));
#78143=CARTESIAN_POINT('Ctrl Pts',(80.0875735394324,-7.33625905579204,131.496142741986));
#78144=CARTESIAN_POINT('Ctrl Pts',(80.1232226992481,-7.33839580778805,131.493803808395));
#78145=CARTESIAN_POINT('Ctrl Pts',(80.1467352532577,-7.34030690181749,131.492274517283));
#78146=CARTESIAN_POINT('Ctrl Pts',(80.2732026987212,-7.35329490145321,131.484107156664));
#78147=CARTESIAN_POINT('Ctrl Pts',(80.3749988433689,-7.37345254427141,131.477760068691));
#78148=CARTESIAN_POINT('Ctrl Pts',(80.5496839388112,-7.42532807027902,131.466631331814));
#78149=CARTESIAN_POINT('Ctrl Pts',(80.6234075954246,-7.45303349692442,131.461848397888));
#78150=CARTESIAN_POINT('Ctrl Pts',(80.717314455519,-7.49613012789184,131.455332470186));
#78151=CARTESIAN_POINT('Ctrl Pts',(80.7395037349128,-7.50691637277533,131.453759748105));
#78152=CARTESIAN_POINT('Ctrl Pts',(80.7767119634748,-7.52603623361309,131.451052281686));
#78153=CARTESIAN_POINT('Ctrl Pts',(80.7918568923749,-7.53411689940639,131.449929967366));
#78154=CARTESIAN_POINT('Ctrl Pts',(80.8133753906402,-7.54602898834544,131.448302108394));
#78155=CARTESIAN_POINT('Ctrl Pts',(80.8198529382876,-7.54967162918538,131.447807701658));
#78156=CARTESIAN_POINT('Ctrl Pts',(80.8310887136411,-7.55608937584467,131.446942066126));
#78157=CARTESIAN_POINT('Ctrl Pts',(80.8358578947802,-7.55884493575117,131.446572075076));
#78158=CARTESIAN_POINT('Ctrl Pts',(80.846054397116,-7.56480396040778,131.445775408652));
#78159=CARTESIAN_POINT('Ctrl Pts',(80.8514771436474,-7.56801453028059,131.445348307929));
#78160=CARTESIAN_POINT('Ctrl Pts',(80.8663297020705,-7.57692226954918,131.444169368613));
#78161=CARTESIAN_POINT('Ctrl Pts',(80.8757212192001,-7.58268221290394,131.443413709574));
#78162=CARTESIAN_POINT('Ctrl Pts',(80.9291293800028,-7.61617162121528,131.439060719835));
#78163=CARTESIAN_POINT('Ctrl Pts',(80.9718811358459,-7.64585512972602,131.435358744385));
#78164=CARTESIAN_POINT('Ctrl Pts',(81.0944626015655,-7.739764039765,131.424228053455));
#78165=CARTESIAN_POINT('Ctrl Pts',(81.1698458319262,-7.80940957006429,131.416700270466));
#78166=CARTESIAN_POINT('Ctrl Pts',(81.2870595185933,-7.93965356445614,131.404139782459));
#78167=CARTESIAN_POINT('Ctrl Pts',(81.3321685239625,-7.99691155836971,131.399023632875));
#78168=CARTESIAN_POINT('Ctrl Pts',(81.3833648212215,-8.07146987214609,131.39285139671));
#78169=CARTESIAN_POINT('Ctrl Pts',(81.3931074652497,-8.08615205937241,131.39165766225));
#78170=CARTESIAN_POINT('Ctrl Pts',(81.4084083175703,-8.11002402194833,131.389750649041));
#78171=CARTESIAN_POINT('Ctrl Pts',(81.4141135680451,-8.11911745589448,131.389031952547));
#78172=CARTESIAN_POINT('Ctrl Pts',(81.4248553339725,-8.13661179135328,131.387663731977));
#78173=CARTESIAN_POINT('Ctrl Pts',(81.4299064148513,-8.14500317349381,131.387013693947));
#78174=CARTESIAN_POINT('Ctrl Pts',(81.4412706341251,-8.16426501511268,131.385535477412));
#78175=CARTESIAN_POINT('Ctrl Pts',(81.4475353806834,-8.17516344538691,131.384709073121));
#78176=CARTESIAN_POINT('Ctrl Pts',(81.4639368455201,-8.20445863922648,131.382513311268));
#78177=CARTESIAN_POINT('Ctrl Pts',(81.4738502258437,-8.22297830189355,131.381151848116));
#78178=CARTESIAN_POINT('Ctrl Pts',(81.5384207042964,-8.34929003323565,131.372031869747));
#78179=CARTESIAN_POINT('Ctrl Pts',(81.5815596006821,-8.46256646799858,131.36469163028));
#78180=CARTESIAN_POINT('Ctrl Pts',(81.6360938151624,-8.67164530780132,131.351488360123));
#78181=CARTESIAN_POINT('Ctrl Pts',(81.6521779437584,-8.76564435143321,131.345654650789));
#78182=CARTESIAN_POINT('Ctrl Pts',(81.6611437627277,-8.87233346178025,131.338653936978));
#78183=CARTESIAN_POINT('Ctrl Pts',(81.662012479237,-8.88419048222527,131.337870598005));
#78184=CARTESIAN_POINT('Ctrl Pts',(81.6631549948394,-8.90246677499294,131.33665359572));
#78185=CARTESIAN_POINT('Ctrl Pts',(81.6635187004372,-8.90888031674602,131.336224710363));
#78186=CARTESIAN_POINT('Ctrl Pts',(81.6641242216537,-8.92077455626452,131.335425693152));
#78187=CARTESIAN_POINT('Ctrl Pts',(81.6643760691832,-8.92625453822107,131.3350561157));
#78188=CARTESIAN_POINT('Ctrl Pts',(81.6648922226903,-8.93884074479375,131.334204006438));
#78189=CARTESIAN_POINT('Ctrl Pts',(81.665138099408,-8.94594749838666,131.333720489071));
#78190=CARTESIAN_POINT('Ctrl Pts',(81.6657831315884,-8.96882974464267,131.332156478196));
#78191=CARTESIAN_POINT('Ctrl Pts',(81.6660036296677,-8.98460886358292,131.331066979627));
#78192=CARTESIAN_POINT('Ctrl Pts',(81.6659801411667,-9.08546423598645,131.324042817735));
#78193=CARTESIAN_POINT('Ctrl Pts',(81.6594435855025,-9.17040600857637,131.317858820687));
#78194=CARTESIAN_POINT('Ctrl Pts',(81.6351141222184,-9.32782176743634,131.306264204932));
#78195=CARTESIAN_POINT('Ctrl Pts',(81.618886649581,-9.40034081569565,131.300867342512));
#78196=CARTESIAN_POINT('Ctrl Pts',(81.5862231349415,-9.51102550919333,131.292648286159));
#78197=CARTESIAN_POINT('Ctrl Pts',(81.5731103827957,-9.5500682614269,131.28975159488));
#78198=CARTESIAN_POINT('Ctrl Pts',(81.5481723112403,-9.61610355189692,131.284860823126));
#78199=CARTESIAN_POINT('Ctrl Pts',(81.5370537016945,-9.6433406563753,131.282846009276));
#78200=CARTESIAN_POINT('Ctrl Pts',(81.5199730613387,-9.68220811855459,131.279972728956));
#78201=CARTESIAN_POINT('Ctrl Pts',(81.5145869422515,-9.69408388207942,131.279095046393));
#78202=CARTESIAN_POINT('Ctrl Pts',(81.5048969265439,-9.71479917633505,131.277564116494));
#78203=CARTESIAN_POINT('Ctrl Pts',(81.5006532446356,-9.72366599235934,131.276908841072));
#78204=CARTESIAN_POINT('Ctrl Pts',(81.4916623041498,-9.7420325712057,131.275551298613));
#78205=CARTESIAN_POINT('Ctrl Pts',(81.4869021803769,-9.75152556919881,131.274849514543));
#78206=CARTESIAN_POINT('Ctrl Pts',(81.4742495990483,-9.77616742562916,131.273027057211));
#78207=CARTESIAN_POINT('Ctrl Pts',(81.4662142349603,-9.79124181218071,131.271911429947));
#78208=CARTESIAN_POINT('Ctrl Pts',(81.4305063555684,-9.85581742277738,131.267125201772));
#78209=CARTESIAN_POINT('Ctrl Pts',(81.4005467730613,-9.90401418610575,131.263536343956));
#78210=CARTESIAN_POINT('Ctrl Pts',(81.3075764453768,-10.0378259725601,131.253388422396));
#78211=CARTESIAN_POINT('Ctrl Pts',(81.2387666897964,-10.1190601862772,131.247007538993));
#78212=CARTESIAN_POINT('Ctrl Pts',(81.1198762639925,-10.234911750383,131.236765125093));
#78213=CARTESIAN_POINT('Ctrl Pts',(81.0748501724917,-10.2742941017695,131.233025046109));
#78214=CARTESIAN_POINT('Ctrl Pts',(81.0163647980167,-10.3201401884637,131.228192440881));
#78215=CARTESIAN_POINT('Ctrl Pts',(81.0048021391684,-10.3289620557987,131.227238143958));
#78216=CARTESIAN_POINT('Ctrl Pts',(80.9875399316191,-10.3417784048487,131.225812614709));
#78217=CARTESIAN_POINT('Ctrl Pts',(80.9819281036176,-10.3458906342102,131.225349056806));
#78218=CARTESIAN_POINT('Ctrl Pts',(80.9722885688292,-10.3528619051586,131.224552264536));
#78219=CARTESIAN_POINT('Ctrl Pts',(80.9682736457543,-10.3557383749834,131.224220229837));
#78220=CARTESIAN_POINT('Ctrl Pts',(80.9590293973587,-10.3622993556297,131.223455284448));
#78221=CARTESIAN_POINT('Ctrl Pts',(80.9537917167311,-10.3659715505825,131.223021579553));
#78222=CARTESIAN_POINT('Ctrl Pts',(80.9391290419711,-10.3761262647808,131.221806911243));
#78223=CARTESIAN_POINT('Ctrl Pts',(80.9296584465635,-10.3825418651067,131.221021755724));
#78224=CARTESIAN_POINT('Ctrl Pts',(80.8664827686277,-10.4243959175322,131.215784141136));
#78225=CARTESIAN_POINT('Ctrl Pts',(80.8108346402948,-10.4567914972086,131.211172226164));
#78226=CARTESIAN_POINT('Ctrl Pts',(80.7325963960003,-10.4964644114896,131.204816264652));
#78227=CARTESIAN_POINT('Ctrl Pts',(80.711512535999,-10.5066031662938,131.203115255327));
#78228=CARTESIAN_POINT('Ctrl Pts',(80.6268215987685,-10.5451547711884,131.196343033857));
#78229=CARTESIAN_POINT('Ctrl Pts',(80.5616695724448,-10.570011748226,131.191270542404));
#78230=CARTESIAN_POINT('Ctrl Pts',(80.4510957057507,-10.6044305789594,131.18298462564));
#78231=CARTESIAN_POINT('Ctrl Pts',(80.406487887433,-10.6163084627075,131.17972436833));
#78232=CARTESIAN_POINT('Ctrl Pts',(80.3302571408869,-10.6332503440041,131.174299005777));
#78233=CARTESIAN_POINT('Ctrl Pts',(80.2988786767481,-10.6392828445552,131.172106551839));
#78234=CARTESIAN_POINT('Ctrl Pts',(80.2540607244863,-10.6465692401506,131.169030759013));
#78235=CARTESIAN_POINT('Ctrl Pts',(80.2407512512279,-10.6485678535705,131.168124238321));
#78236=CARTESIAN_POINT('Ctrl Pts',(80.217616082208,-10.6517557798064,131.166560018261));
#78237=CARTESIAN_POINT('Ctrl Pts',(80.2078014727354,-10.6530191984851,131.165900017342));
#78238=CARTESIAN_POINT('Ctrl Pts',(80.1875911714186,-10.655437990949,131.164548068667));
#78239=CARTESIAN_POINT('Ctrl Pts',(80.1771946705243,-10.6565830636122,131.163856472428));
#78240=CARTESIAN_POINT('Ctrl Pts',(80.1505403861338,-10.6592649714502,131.162092850528));
#78241=CARTESIAN_POINT('Ctrl Pts',(80.1342692930381,-10.660660844725,131.161025264474));
#78242=CARTESIAN_POINT('Ctrl Pts',(80.0675438935439,-10.6653979784359,131.156681027819));
#78243=CARTESIAN_POINT('Ctrl Pts',(80.0169679475903,-10.6666809673076,131.15346824237));
#78244=CARTESIAN_POINT('Ctrl Pts',(79.8572490463909,-10.6634598483811,131.143473349963));
#78245=CARTESIAN_POINT('Ctrl Pts',(79.7485734331196,-10.6505336684615,131.136911382521));
#78246=CARTESIAN_POINT('Ctrl Pts',(79.5796315275146,-10.6133558432963,131.126261859302));
#78247=CARTESIAN_POINT('Ctrl Pts',(79.5181659521544,-10.5960767188038,131.122283197339));
#78248=CARTESIAN_POINT('Ctrl Pts',(79.4436751154021,-10.5704404921533,131.117164532706));
#78249=CARTESIAN_POINT('Ctrl Pts',(79.4295675978083,-10.565371378551,131.116181545578));
#78250=CARTESIAN_POINT('Ctrl Pts',(79.4089367853213,-10.5576424053649,131.114721284565));
#78251=CARTESIAN_POINT('Ctrl Pts',(79.4023584382069,-10.5551302665283,131.114252232981));
#78252=CARTESIAN_POINT('Ctrl Pts',(79.3911848610749,-10.5507819360683,131.113449349733));
#78253=CARTESIAN_POINT('Ctrl Pts',(79.3865815679417,-10.548966853394,131.113116771407));
#78254=CARTESIAN_POINT('Ctrl Pts',(79.3761006664735,-10.5447801753478,131.112355345465));
#78255=CARTESIAN_POINT('Ctrl Pts',(79.3702285937258,-10.5423955851238,131.111925745568));
#78256=CARTESIAN_POINT('Ctrl Pts',(79.354039481854,-10.5357134886961,131.1107333257));
#78257=CARTESIAN_POINT('Ctrl Pts',(79.3437520859572,-10.531345672533,131.10996654682));
#78258=CARTESIAN_POINT('Ctrl Pts',(79.2833788371888,-10.5049923790786,131.105416241671));
#78259=CARTESIAN_POINT('Ctrl Pts',(79.2343610308612,-10.4806564974867,131.101517260273));
#78260=CARTESIAN_POINT('Ctrl Pts',(79.1002965325023,-10.4056587834121,131.090429413026));
#78261=CARTESIAN_POINT('Ctrl Pts',(79.0184266620057,-10.349762345456,131.08316342681));
#78262=CARTESIAN_POINT('Ctrl Pts',(78.8854050424377,-10.2404039613561,131.070816219604));
#78263=CARTESIAN_POINT('Ctrl Pts',(78.8319340291888,-10.1901884186516,131.065666602184));
#78264=CARTESIAN_POINT('Ctrl Pts',(78.7698978622216,-10.123706419606,131.059460863011));
#78265=CARTESIAN_POINT('Ctrl Pts',(78.7580643443188,-10.1106139093169,131.058265245751));
#78266=CARTESIAN_POINT('Ctrl Pts',(78.7393663531112,-10.0892539484748,131.056355968303));
#78267=CARTESIAN_POINT('Ctrl Pts',(78.7323702141229,-10.0811041074925,131.055636867204));
#78268=CARTESIAN_POINT('Ctrl Pts',(78.7191470513043,-10.0653955200778,131.054268340989));
#78269=CARTESIAN_POINT('Ctrl Pts',(78.7129069295663,-10.0578484416075,131.053618397522));
#78270=CARTESIAN_POINT('Ctrl Pts',(78.6988167754124,-10.0404979239043,131.052141028486));
#78271=CARTESIAN_POINT('Ctrl Pts',(78.6910102619647,-10.0306597856117,131.051315369808));
#78272=CARTESIAN_POINT('Ctrl Pts',(78.6665038325572,-9.99904799294626,131.048699381254));
#78273=CARTESIAN_POINT('Ctrl Pts',(78.6502297194569,-9.97694894903163,131.04692566924));
#78274=CARTESIAN_POINT('Ctrl Pts',(78.558979137228,-9.84640148887605,131.036736927588));
#78275=CARTESIAN_POINT('Ctrl Pts',(78.4965433845736,-9.72976528600962,131.028809827571));
#78276=CARTESIAN_POINT('Ctrl Pts',(78.4224131503897,-9.54028274575061,131.016327503265));
#78277=CARTESIAN_POINT('Ctrl Pts',(78.4006499410546,-9.47197748760387,131.011888444127));
#78278=CARTESIAN_POINT('Ctrl Pts',(78.379533148169,-9.3871599883793,131.006217717961));
#78279=CARTESIAN_POINT('Ctrl Pts',(78.3759342246032,-9.37177410770109,131.005182747008));
#78280=CARTESIAN_POINT('Ctrl Pts',(78.3710167274966,-9.3493153451493,131.003659749694));
#78281=CARTESIAN_POINT('Ctrl Pts',(78.3695241519386,-9.34228090303748,131.003180983918));
#78282=CARTESIAN_POINT('Ctrl Pts',(78.3669840164233,-9.32991561272275,131.002335996631));
#78283=CARTESIAN_POINT('Ctrl Pts',(78.3659169202432,-9.3245889728867,131.001970880914));
#78284=CARTESIAN_POINT('Ctrl Pts',(78.3636434814905,-9.31294520742212,131.001170226983));
#78285=CARTESIAN_POINT('Ctrl Pts',(78.3624476755718,-9.30662638468164,131.000734139032));
#78286=CARTESIAN_POINT('Ctrl Pts',(78.3591989068843,-9.28889818600297,130.999506490884));
#78287=CARTESIAN_POINT('Ctrl Pts',(78.3572284503758,-9.27747433401644,130.998710599833));
#78288=CARTESIAN_POINT('Ctrl Pts',(78.3438152459265,-9.19455302981011,130.992903208467));
#78289=CARTESIAN_POINT('Ctrl Pts',(78.3369264852316,-9.12240479457994,130.987690481246));
#78290=CARTESIAN_POINT('Ctrl Pts',(78.3342650542894,-9.03384832452713,130.981256601982));
#78291=CARTESIAN_POINT('Ctrl Pts',(78.3340146152127,-9.01764398355277,130.980077686109));
#78292=CARTESIAN_POINT('Ctrl Pts',(78.333889406962,-8.87265096241319,130.969524597057));
#78293=CARTESIAN_POINT('Ctrl Pts',(78.3487122814742,-8.74425940938005,130.960198804359));
#78294=CARTESIAN_POINT('Ctrl Pts',(78.3828536587066,-8.59898927122409,130.949942217047));
#78295=CARTESIAN_POINT('Ctrl Pts',(78.3878837061593,-8.57922332198349,130.948551940134));
#78296=CARTESIAN_POINT('Ctrl Pts',(78.3965884154774,-8.54746899448516,130.946326160262));
#78297=CARTESIAN_POINT('Ctrl Pts',(78.4000375342468,-8.53542154225168,130.945483516037));
#78298=CARTESIAN_POINT('Ctrl Pts',(78.4064150735652,-8.51405927323683,130.943992239616));
#78299=CARTESIAN_POINT('Ctrl Pts',(78.4092900336537,-8.50472924816484,130.943341905896));
#78300=CARTESIAN_POINT('Ctrl Pts',(78.4155376869815,-8.48506967678336,130.941973412031));
#78301=CARTESIAN_POINT('Ctrl Pts',(78.4189297690752,-8.47474673399138,130.941255920823));
#78302=CARTESIAN_POINT('Ctrl Pts',(78.4269651601825,-8.45107643519932,130.939612795179));
#78303=CARTESIAN_POINT('Ctrl Pts',(78.4316777696174,-8.43775354229633,130.938689485125));
#78304=CARTESIAN_POINT('Ctrl Pts',(78.4365593749572,-8.42449204005001,130.937771468334));
#78305=CARTESIAN_POINT('Ctrl Pts',(78.4365594227781,-8.42449191013859,131.131996270822));
#78306=CARTESIAN_POINT('Ctrl Pts',(78.4235761673907,-8.45976256689324,131.134732188538));
#78307=CARTESIAN_POINT('Ctrl Pts',(78.4117849555462,-8.49547663369563,131.13746816417));
#78308=CARTESIAN_POINT('Ctrl Pts',(78.3772965578482,-8.61318938570139,131.146340231324));
#78309=CARTESIAN_POINT('Ctrl Pts',(78.3596657873488,-8.69652602544283,131.152387296996));
#78310=CARTESIAN_POINT('Ctrl Pts',(78.3454336264977,-8.80378322644139,131.159828485104));
#78311=CARTESIAN_POINT('Ctrl Pts',(78.342869015249,-8.82677211793479,131.161404455124));
#78312=CARTESIAN_POINT('Ctrl Pts',(78.3397128484832,-8.86163924033204,131.163767284688));
#78313=CARTESIAN_POINT('Ctrl Pts',(78.3387684394046,-8.87348185874766,131.164565058941));
#78314=CARTESIAN_POINT('Ctrl Pts',(78.33734731046,-8.89408066677514,131.16594472061));
#78315=CARTESIAN_POINT('Ctrl Pts',(78.3368129066966,-8.9028322641114,131.166528387983));
#78316=CARTESIAN_POINT('Ctrl Pts',(78.3357660830759,-8.92253034850817,131.167836685924));
#78317=CARTESIAN_POINT('Ctrl Pts',(78.3352925225985,-8.93347856370225,131.168560077128));
#78318=CARTESIAN_POINT('Ctrl Pts',(78.3343042584106,-8.96309090897862,131.170507039486));
#78319=CARTESIAN_POINT('Ctrl Pts',(78.333995210254,-8.98176069142106,131.171724185505));
#78320=CARTESIAN_POINT('Ctrl Pts',(78.334025399594,-9.09808660637892,131.17925069829));
#78321=CARTESIAN_POINT('Ctrl Pts',(78.3426363912761,-9.19555512328972,131.185291057286));
#78322=CARTESIAN_POINT('Ctrl Pts',(78.3768931288007,-9.38817213921979,131.197262568064));
#78323=CARTESIAN_POINT('Ctrl Pts',(78.4025200085894,-9.48291617632865,131.203173327976));
#78324=CARTESIAN_POINT('Ctrl Pts',(78.4474708800055,-9.60518932489194,131.211423092386));
#78325=CARTESIAN_POINT('Ctrl Pts',(78.4595036544767,-9.63519404434482,131.213500940887));
#78326=CARTESIAN_POINT('Ctrl Pts',(78.4762762779447,-9.67373314656306,131.216263628589));
#78327=CARTESIAN_POINT('Ctrl Pts',(78.4802298261564,-9.68260452784972,131.21690617709));
#78328=CARTESIAN_POINT('Ctrl Pts',(78.4867307953796,-9.69685560833873,131.217949862233));
#78329=CARTESIAN_POINT('Ctrl Pts',(78.4892299457115,-9.70225726396787,131.218348141172));
#78330=CARTESIAN_POINT('Ctrl Pts',(78.4941536457533,-9.71275140764668,131.219127370169));
#78331=CARTESIAN_POINT('Ctrl Pts',(78.4965751935204,-9.71784514993842,131.219508141732));
#78332=CARTESIAN_POINT('Ctrl Pts',(78.5025999086656,-9.73035397842765,131.220449321646));
#78333=CARTESIAN_POINT('Ctrl Pts',(78.5062323140834,-9.73775474295358,131.221011476393));
#78334=CARTESIAN_POINT('Ctrl Pts',(78.51995583963,-9.76519856179563,131.223115091475));
#78335=CARTESIAN_POINT('Ctrl Pts',(78.5303961715476,-9.7850630686603,131.224675703936));
#78336=CARTESIAN_POINT('Ctrl Pts',(78.6115818772415,-9.93223539752564,131.236492773686));
#78337=CARTESIAN_POINT('Ctrl Pts',(78.6983472001639,-10.0499863844994,131.247328008473));
#78338=CARTESIAN_POINT('Ctrl Pts',(78.8443874629582,-10.2018074825112,131.262368685855));
#78339=CARTESIAN_POINT('Ctrl Pts',(78.8921595598234,-10.2459827527107,131.266922037966));
#78340=CARTESIAN_POINT('Ctrl Pts',(78.9560088661246,-10.298440930226,131.27256140148));
#78341=CARTESIAN_POINT('Ctrl Pts',(78.9697973586504,-10.3094078417488,131.273754960245));
#78342=CARTESIAN_POINT('Ctrl Pts',(78.992261899242,-10.3267008322504,131.275661634988));
#78343=CARTESIAN_POINT('Ctrl Pts',(79.0008293452605,-10.3331651023197,131.276380167694));
#78344=CARTESIAN_POINT('Ctrl Pts',(79.0173313533483,-10.3453676807137,131.277748035452));
#78345=CARTESIAN_POINT('Ctrl Pts',(79.0252551776222,-10.3511196851692,131.278397884586));
#78346=CARTESIAN_POINT('Ctrl Pts',(79.0436370499541,-10.3642174392655,131.279889757032));
#78347=CARTESIAN_POINT('Ctrl Pts',(79.0541299186394,-10.3715134407402,131.280729854853));
#78348=CARTESIAN_POINT('Ctrl Pts',(79.0878176531082,-10.3943670044879,131.283391730513));
#78349=CARTESIAN_POINT('Ctrl Pts',(79.1113209476974,-10.4094628994058,131.285196291933));
#78350=CARTESIAN_POINT('Ctrl Pts',(79.1999437245756,-10.46328565117,131.291825258049));
#78351=CARTESIAN_POINT('Ctrl Pts',(79.2673038185802,-10.4981498450688,131.296516757853));
#78352=CARTESIAN_POINT('Ctrl Pts',(79.416482708141,-10.5628841241907,131.306483853868));
#78353=CARTESIAN_POINT('Ctrl Pts',(79.4987338297728,-10.5911725396823,131.311728429494));
#78354=CARTESIAN_POINT('Ctrl Pts',(79.6291678118446,-10.6249099219855,131.320132968678));
#78355=CARTESIAN_POINT('Ctrl Pts',(79.6760158950084,-10.6348951472366,131.323170146666));
#78356=CARTESIAN_POINT('Ctrl Pts',(79.7340106057263,-10.6446657105387,131.327024088314));
#78357=CARTESIAN_POINT('Ctrl Pts',(79.7448146754482,-10.6463766554863,131.327746036344));
#78358=CARTESIAN_POINT('Ctrl Pts',(79.7617870313953,-10.6488933465009,131.328887510982));
#78359=CARTESIAN_POINT('Ctrl Pts',(79.7679445454255,-10.6497711809184,131.329303147153));
#78360=CARTESIAN_POINT('Ctrl Pts',(79.7795826196477,-10.6513638986268,131.330091826584));
#78361=CARTESIAN_POINT('Ctrl Pts',(79.7850620002083,-10.6520860146524,131.330464467462));
#78362=CARTESIAN_POINT('Ctrl Pts',(79.7980641877281,-10.6537337686017,131.331351745269));
#78363=CARTESIAN_POINT('Ctrl Pts',(79.8055898381186,-10.6546353474618,131.331867684759));
#78364=CARTESIAN_POINT('Ctrl Pts',(79.8310594385515,-10.6575104728943,131.333621283196));
#78365=CARTESIAN_POINT('Ctrl Pts',(79.8490285195014,-10.6592436310399,131.334870975461));
#78366=CARTESIAN_POINT('Ctrl Pts',(79.8933524806792,-10.6627928567919,131.337978705836));
#78367=CARTESIAN_POINT('Ctrl Pts',(79.9197286972502,-10.6642746593209,131.339849842052));
#78368=CARTESIAN_POINT('Ctrl Pts',(80.0360758048018,-10.6680388818661,131.348170062387));
#78369=CARTESIAN_POINT('Ctrl Pts',(80.1261097839662,-10.6636559212747,131.354774159003));
#78370=CARTESIAN_POINT('Ctrl Pts',(80.3122473496333,-10.639392174998,131.368373760117));
#78371=CARTESIAN_POINT('Ctrl Pts',(80.4078616449494,-10.6182583080106,131.375324199531));
#78372=CARTESIAN_POINT('Ctrl Pts',(80.5188754329337,-10.583247373121,131.383283266209));
#78373=CARTESIAN_POINT('Ctrl Pts',(80.5365704813197,-10.5773383045695,131.384549040968));
#78374=CARTESIAN_POINT('Ctrl Pts',(80.5645920115753,-10.567454672806,131.386549670926));
#78375=CARTESIAN_POINT('Ctrl Pts',(80.574984154071,-10.5636724476731,131.387290786442));
#78376=CARTESIAN_POINT('Ctrl Pts',(80.5935342361823,-10.556711195946,131.388612428773));
#78377=CARTESIAN_POINT('Ctrl Pts',(80.6017061452099,-10.5535708406523,131.389194214383));
#78378=CARTESIAN_POINT('Ctrl Pts',(80.6207784810072,-10.5460685340735,131.390551208275));
#78379=CARTESIAN_POINT('Ctrl Pts',(80.6316583985691,-10.5416554458963,131.39132467192));
#78380=CARTESIAN_POINT('Ctrl Pts',(80.6631859808786,-10.5284774979807,131.393564847808));
#78381=CARTESIAN_POINT('Ctrl Pts',(80.6837049159427,-10.5194100080589,131.395021327691));
#78382=CARTESIAN_POINT('Ctrl Pts',(80.7761932494394,-10.4762854738253,131.401589414786));
#78383=CARTESIAN_POINT('Ctrl Pts',(80.8458510199626,-10.4375092917663,131.406538348014));
#78384=CARTESIAN_POINT('Ctrl Pts',(80.9505202713853,-10.3689904747214,131.414216655985));
#78385=CARTESIAN_POINT('Ctrl Pts',(80.9875301199682,-10.3425379004362,131.416985736688));
#78386=CARTESIAN_POINT('Ctrl Pts',(81.0913849026212,-10.2616875882799,131.425031432797));
#78387=CARTESIAN_POINT('Ctrl Pts',(81.1551434834546,-10.2035848077741,131.430320106844));
#78388=CARTESIAN_POINT('Ctrl Pts',(81.2249261328506,-10.1293188931778,131.436931767804));
#78389=CARTESIAN_POINT('Ctrl Pts',(81.2355712479461,-10.1176622210156,131.437965763383));
#78390=CARTESIAN_POINT('Ctrl Pts',(81.2507687089481,-10.100538141771,131.439482453151));
#78391=CARTESIAN_POINT('Ctrl Pts',(81.2554545663262,-10.0951896603187,131.439955855419));
#78392=CARTESIAN_POINT('Ctrl Pts',(81.2636936620114,-10.0856631195614,131.440798854115));
#78393=CARTESIAN_POINT('Ctrl Pts',(81.2672607192338,-10.081497271752,131.441167430399));
#78394=CARTESIAN_POINT('Ctrl Pts',(81.2749591810721,-10.0724161097713,131.441970865179));
#78395=CARTESIAN_POINT('Ctrl Pts',(81.2790826974783,-10.0674945786423,131.44240623731));
#78396=CARTESIAN_POINT('Ctrl Pts',(81.2907536941616,-10.0534002121502,131.443652622143));
#78397=CARTESIAN_POINT('Ctrl Pts',(81.2982314766246,-10.0441705410988,131.444468286287));
#78398=CARTESIAN_POINT('Ctrl Pts',(81.364718549674,-9.96028866936057,131.451870606439));
#78399=CARTESIAN_POINT('Ctrl Pts',(81.417323390191,-9.88079602607164,131.458799941915));
#78400=CARTESIAN_POINT('Ctrl Pts',(81.5207126166027,-9.69109221364698,131.474526837408));
#78401=CARTESIAN_POINT('Ctrl Pts',(81.5668546688677,-9.57892302507623,131.483257135814));
#78402=CARTESIAN_POINT('Ctrl Pts',(81.6062809044694,-9.44255906873708,131.493021805051));
#78403=CARTESIAN_POINT('Ctrl Pts',(81.6117311683976,-9.42227903554291,131.494454147757));
#78404=CARTESIAN_POINT('Ctrl Pts',(81.6198283065318,-9.38970523881117,131.496724060969));
#78405=CARTESIAN_POINT('Ctrl Pts',(81.622721789246,-9.37747572839121,131.497569437401));
#78406=CARTESIAN_POINT('Ctrl Pts',(81.6276230902474,-9.35566127757586,131.499065587766));
#78407=CARTESIAN_POINT('Ctrl Pts',(81.6296852686911,-9.34608929529792,131.499718072435));
#78408=CARTESIAN_POINT('Ctrl Pts',(81.6338305478312,-9.32598912190236,131.501080070041));
#78409=CARTESIAN_POINT('Ctrl Pts',(81.6358965527004,-9.31545783328286,131.50178901126));
#78410=CARTESIAN_POINT('Ctrl Pts',(81.6410843510511,-9.2875906866489,131.503653142698));
#78411=CARTESIAN_POINT('Ctrl Pts',(81.6440332810671,-9.27022372137051,131.504802837899));
#78412=CARTESIAN_POINT('Ctrl Pts',(81.6577496825342,-9.18088135407764,131.510660690822));
#78413=CARTESIAN_POINT('Ctrl Pts',(81.6640689195304,-9.10829878055827,131.51522713665));
#78414=CARTESIAN_POINT('Ctrl Pts',(81.6678057759094,-8.9331077850239,131.526045686722));
#78415=CARTESIAN_POINT('Ctrl Pts',(81.6605390429065,-8.83070946241532,131.532196929265));
#78416=CARTESIAN_POINT('Ctrl Pts',(81.6354696537977,-8.67828090631664,131.541803043561));
#78417=CARTESIAN_POINT('Ctrl Pts',(81.6246237696407,-8.62735992939889,131.545093133628));
#78418=CARTESIAN_POINT('Ctrl Pts',(81.6086178020925,-8.56638020405897,131.549222479066));
#78419=CARTESIAN_POINT('Ctrl Pts',(81.6057154340369,-8.55575312092573,131.549949213593));
#78420=CARTESIAN_POINT('Ctrl Pts',(81.6009877848167,-8.53909457336029,131.551100746918));
#78421=CARTESIAN_POINT('Ctrl Pts',(81.5992332453044,-8.53304312482268,131.551521632101));
#78422=CARTESIAN_POINT('Ctrl Pts',(81.5958810622113,-8.52172188209529,131.552314124717));
#78423=CARTESIAN_POINT('Ctrl Pts',(81.5942915669891,-8.516449879853,131.552685267818));
#78424=CARTESIAN_POINT('Ctrl Pts',(81.5904964731112,-8.50408453429794,131.553560636681));
#78425=CARTESIAN_POINT('Ctrl Pts',(81.5882695383499,-8.49699796383648,131.554066064633));
#78426=CARTESIAN_POINT('Ctrl Pts',(81.5807435135289,-8.47359693470009,131.555746979429));
#78427=CARTESIAN_POINT('Ctrl Pts',(81.5752400472542,-8.45735003999213,131.556933232162));
#78428=CARTESIAN_POINT('Ctrl Pts',(81.5612194476903,-8.41797132363961,131.559850737597));
#78429=CARTESIAN_POINT('Ctrl Pts',(81.5524380276693,-8.39493836296873,131.561593232655));
#78430=CARTESIAN_POINT('Ctrl Pts',(81.5135494387733,-8.29936286523725,131.568952897489));
#78431=CARTESIAN_POINT('Ctrl Pts',(81.478843571217,-8.22880279889845,131.574697108613));
#78432=CARTESIAN_POINT('Ctrl Pts',(81.3870631378972,-8.07136297374987,131.587943537972));
#78433=CARTESIAN_POINT('Ctrl Pts',(81.3265750604024,-7.9868286864708,131.595380353435));
#78434=CARTESIAN_POINT('Ctrl Pts',(81.2431564103606,-7.89064240074824,131.604145006203));
#78435=CARTESIAN_POINT('Ctrl Pts',(81.2273281456317,-7.8731557936916,131.605753245688));
#78436=CARTESIAN_POINT('Ctrl Pts',(81.2028085054054,-7.84719703572044,131.60816472492));
#78437=CARTESIAN_POINT('Ctrl Pts',(81.1943876600075,-7.83847466397561,131.608979297008));
#78438=CARTESIAN_POINT('Ctrl Pts',(81.1790447382035,-7.8229256636898,131.61043954062));
#78439=CARTESIAN_POINT('Ctrl Pts',(81.1721567735728,-7.81606630552004,131.61108665575));
#78440=CARTESIAN_POINT('Ctrl Pts',(81.1572659430072,-7.80149466126838,131.612467948047));
#78441=CARTESIAN_POINT('Ctrl Pts',(81.1492451103219,-7.79380134460412,131.613201279828));
#78442=CARTESIAN_POINT('Ctrl Pts',(81.1270125253147,-7.7728996904679,131.615205459814));
#78443=CARTESIAN_POINT('Ctrl Pts',(81.1126458151924,-7.75985817632879,131.616469202088));
#78444=CARTESIAN_POINT('Ctrl Pts',(81.0801308284989,-7.73136239645004,131.619263548815));
#78445=CARTESIAN_POINT('Ctrl Pts',(81.0618719698616,-7.7160405067067,131.620788851588));
#78446=CARTESIAN_POINT('Ctrl Pts',(81.0022999140359,-7.66819105936158,131.625637333851));
#78447=CARTESIAN_POINT('Ctrl Pts',(80.9597724559267,-7.63722429268645,131.628906612746));
#78448=CARTESIAN_POINT('Ctrl Pts',(80.8356512413603,-7.55554158194246,131.638053474279));
#78449=CARTESIAN_POINT('Ctrl Pts',(80.7510454521757,-7.5097978437155,131.643830285086));
#78450=CARTESIAN_POINT('Ctrl Pts',(80.6156941667761,-7.45108656384421,131.653008226286));
#78451=CARTESIAN_POINT('Ctrl Pts',(80.5674915627972,-7.4327845247519,131.656267849422));
#78452=CARTESIAN_POINT('Ctrl Pts',(80.5080786521613,-7.41332647039939,131.660362902791));
#78453=CARTESIAN_POINT('Ctrl Pts',(80.4976001181492,-7.41000914692264,131.661088009249));
#78454=CARTESIAN_POINT('Ctrl Pts',(80.4810698832316,-7.40495536264248,131.662237522514));
#78455=CARTESIAN_POINT('Ctrl Pts',(80.475039631697,-7.40314904491215,131.662658038131));
#78456=CARTESIAN_POINT('Ctrl Pts',(80.4637142778653,-7.39982644524963,131.663450251357));
#78457=CARTESIAN_POINT('Ctrl Pts',(80.4584217175928,-7.39830219388272,131.663821488933));
#78458=CARTESIAN_POINT('Ctrl Pts',(80.4459637650599,-7.39478112073818,131.664697646789));
#78459=CARTESIAN_POINT('Ctrl Pts',(80.4387924570966,-7.39280601531959,131.665203775957));
#78460=CARTESIAN_POINT('Ctrl Pts',(80.4149835504506,-7.3864198436843,131.666889468489));
#78461=CARTESIAN_POINT('Ctrl Pts',(80.398291452127,-7.38221876341182,131.668079878854));
#78462=CARTESIAN_POINT('Ctrl Pts',(80.3574334262281,-7.37260621180815,131.671009743737));
#78463=CARTESIAN_POINT('Ctrl Pts',(80.3332065603375,-7.36747359805217,131.672760556846));
#78464=CARTESIAN_POINT('Ctrl Pts',(80.2310169164863,-7.34819342649752,131.680178911411));
#78465=CARTESIAN_POINT('Ctrl Pts',(80.1522124578486,-7.33907727904711,131.685975182024));
#78466=CARTESIAN_POINT('Ctrl Pts',(79.9703617869121,-7.33109461967067,131.69920415078));
#78467=CARTESIAN_POINT('Ctrl Pts',(79.8674501388419,-7.33610078564603,131.706573173012));
#78468=CARTESIAN_POINT('Ctrl Pts',(79.7422862257752,-7.35388453218234,131.715276002977));
#78469=CARTESIAN_POINT('Ctrl Pts',(79.7190022121216,-7.3576989116387,131.716884802495));
#78470=CARTESIAN_POINT('Ctrl Pts',(79.6838848389204,-7.36422060771146,131.719296946586));
#78471=CARTESIAN_POINT('Ctrl Pts',(79.671987941799,-7.36656462678864,131.720111632849));
#78472=CARTESIAN_POINT('Ctrl Pts',(79.6506012380265,-7.37102148708713,131.721571999992));
#78473=CARTESIAN_POINT('Ctrl Pts',(79.6411024292714,-7.37308788467288,131.722219125531));
#78474=CARTESIAN_POINT('Ctrl Pts',(79.6207847896032,-7.37769444667959,131.723600353556));
#78475=CARTESIAN_POINT('Ctrl Pts',(79.6099721449218,-7.38025996948403,131.724333611448));
#78476=CARTESIAN_POINT('Ctrl Pts',(79.5803598111892,-7.38759983181462,131.726337364952));
#78477=CARTESIAN_POINT('Ctrl Pts',(79.5616161868808,-7.3925946765683,131.727600759806));
#78478=CARTESIAN_POINT('Ctrl Pts',(79.4326016501931,-7.42939946325379,131.736271980696));
#78479=CARTESIAN_POINT('Ctrl Pts',(79.3257842115861,-7.47220274965911,131.743296386014));
#78480=CARTESIAN_POINT('Ctrl Pts',(79.1332954069401,-7.57348958976585,131.756578319682));
#78481=CARTESIAN_POINT('Ctrl Pts',(79.0470175050946,-7.62962508976139,131.762820577318));
#78482=CARTESIAN_POINT('Ctrl Pts',(78.9545835844362,-7.70273742655758,131.770475763271));
#78483=CARTESIAN_POINT('Ctrl Pts',(78.9428268756396,-7.71230026327776,131.771469287838));
#78484=CARTESIAN_POINT('Ctrl Pts',(78.9257784149653,-7.72655821118568,131.772942210409));
#78485=CARTESIAN_POINT('Ctrl Pts',(78.9203831267429,-7.7311290823351,131.773413179627));
#78486=CARTESIAN_POINT('Ctrl Pts',(78.9108654703834,-7.73929705782073,131.774252966508));
#78487=CARTESIAN_POINT('Ctrl Pts',(78.906731489144,-7.7428803184892,131.774620784136));
#78488=CARTESIAN_POINT('Ctrl Pts',(78.8977049489005,-7.75078256160792,131.775430719388));
#78489=CARTESIAN_POINT('Ctrl Pts',(78.8928201569517,-7.75510989257313,131.775873426714));
#78490=CARTESIAN_POINT('Ctrl Pts',(78.8793626175268,-7.76717349180127,131.777105029212));
#78491=CARTESIAN_POINT('Ctrl Pts',(78.8708448783743,-7.77497019009992,131.777898133249));
#78492=CARTESIAN_POINT('Ctrl Pts',(78.8512754153641,-7.79326056051038,131.779750676825));
#78493=CARTESIAN_POINT('Ctrl Pts',(78.8402853948725,-7.80381847351903,131.780814087352));
#78494=CARTESIAN_POINT('Ctrl Pts',(78.8041695486948,-7.83947986989369,131.784381958025));
#78495=CARTESIAN_POINT('Ctrl Pts',(78.7797028735409,-7.86523480392826,131.78691993339));
#78496=CARTESIAN_POINT('Ctrl Pts',(78.6924711721465,-7.96314530765645,131.796372403422));
#78497=CARTESIAN_POINT('Ctrl Pts',(78.6351267542301,-8.03988469725625,131.803394937501));
#78498=CARTESIAN_POINT('Ctrl Pts',(78.543502771379,-8.18743333640404,131.815883981024));
#78499=CARTESIAN_POINT('Ctrl Pts',(78.5070315460716,-8.25656396350369,131.821386784816));
#78500=CARTESIAN_POINT('Ctrl Pts',(78.4681182441537,-8.34484144003548,131.827978433095));
#78501=CARTESIAN_POINT('Ctrl Pts',(78.4609767564664,-8.36179787248843,131.82922601524));
#78502=CARTESIAN_POINT('Ctrl Pts',(78.4500537133038,-8.38898338197496,131.831197621849));
#78503=CARTESIAN_POINT('Ctrl Pts',(78.4460893481639,-8.39913687496472,131.831927742689));
#78504=CARTESIAN_POINT('Ctrl Pts',(78.440311810998,-8.41437395314495,131.833014313653));
#78505=CARTESIAN_POINT('Ctrl Pts',(78.4384233036404,-8.41942844053872,131.833373268318));
#78506=CARTESIAN_POINT('Ctrl Pts',(78.4365593750065,-8.42449203991602,131.833731407018));
#78507=CARTESIAN_POINT('Origin',(80.,-9.,134.));
#78508=CARTESIAN_POINT('',(78.4365593757978,-8.42449203776636,132.531716974833));
#78509=CARTESIAN_POINT('',(78.4365593746692,-8.42449204083249,132.34076576841));
#78510=CARTESIAN_POINT('',(78.4365593749993,-8.42449203993574,134.));
#78511=CARTESIAN_POINT('',(78.3340003204321,-8.99896671418601,131.679718342728));
#78512=CARTESIAN_POINT('Ctrl Pts',(78.4365593746692,-8.42449204083248,132.34076576841));
#78513=CARTESIAN_POINT('Ctrl Pts',(78.4390138554722,-8.4178241313095,132.340304576558));
#78514=CARTESIAN_POINT('Ctrl Pts',(78.4415110902992,-8.4111716600942,132.339841349361));
#78515=CARTESIAN_POINT('Ctrl Pts',(78.4479889080622,-8.39424513180157,132.338654284345));
#78516=CARTESIAN_POINT('Ctrl Pts',(78.4520287265719,-8.38399487785357,132.337927463635));
#78517=CARTESIAN_POINT('Ctrl Pts',(78.4585385975825,-8.36794584003524,132.336775754262));
#78518=CARTESIAN_POINT('Ctrl Pts',(78.4609404868607,-8.36211950334775,132.336354779793));
#78519=CARTESIAN_POINT('Ctrl Pts',(78.4655035579377,-8.3512265338598,132.335562085204));
#78520=CARTESIAN_POINT('Ctrl Pts',(78.4676568805521,-8.34615682169059,132.335190829334));
#78521=CARTESIAN_POINT('Ctrl Pts',(78.4727743967095,-8.3342724410677,132.334315135706));
#78522=CARTESIAN_POINT('Ctrl Pts',(78.4757590874159,-8.32746683263963,132.333809494426));
#78523=CARTESIAN_POINT('Ctrl Pts',(78.4857880525261,-8.30500877715541,132.332127600537));
#78524=CARTESIAN_POINT('Ctrl Pts',(78.4930284281871,-8.28944581755006,132.330940567757));
#78525=CARTESIAN_POINT('Ctrl Pts',(78.5112573464877,-8.25179559762374,132.328020864471));
#78526=CARTESIAN_POINT('Ctrl Pts',(78.5224983485425,-8.22983556547231,132.326276933038));
#78527=CARTESIAN_POINT('Ctrl Pts',(78.5716047804195,-8.13893740803797,132.318907781584));
#78528=CARTESIAN_POINT('Ctrl Pts',(78.6138390492161,-8.07247714628997,132.313155264429));
#78529=CARTESIAN_POINT('Ctrl Pts',(78.7221884903929,-7.92599964484594,132.299912284184));
#78530=CARTESIAN_POINT('Ctrl Pts',(78.7914062011884,-7.84865876223397,132.292486942134));
#78531=CARTESIAN_POINT('Ctrl Pts',(78.8846666075101,-7.76220206015346,132.283732579222));
#78532=CARTESIAN_POINT('Ctrl Pts',(78.9023029834943,-7.74653533156957,132.282124083819));
#78533=CARTESIAN_POINT('Ctrl Pts',(78.929501560374,-7.72338880965422,132.279712169194));
#78534=CARTESIAN_POINT('Ctrl Pts',(78.9388219412196,-7.71563082347502,132.278897414716));
#78535=CARTESIAN_POINT('Ctrl Pts',(78.9557669434384,-7.70183673491072,132.27743681384));
#78536=CARTESIAN_POINT('Ctrl Pts',(78.9633612010551,-7.6957643822364,132.276789523463));
#78537=CARTESIAN_POINT('Ctrl Pts',(78.9797514704731,-7.68289236283971,132.275407820087));
#78538=CARTESIAN_POINT('Ctrl Pts',(78.9885632981431,-7.67611352522975,132.274674253307));
#78539=CARTESIAN_POINT('Ctrl Pts',(79.0129438815596,-7.65774334339052,132.272669320105));
#78540=CARTESIAN_POINT('Ctrl Pts',(79.0286486825662,-7.64633483373563,132.271405066081));
#78541=CARTESIAN_POINT('Ctrl Pts',(79.0640823888214,-7.62152884380707,132.268609517381));
#78542=CARTESIAN_POINT('Ctrl Pts',(79.0839069487887,-7.60827513136339,132.267083530185));
#78543=CARTESIAN_POINT('Ctrl Pts',(79.1483619602897,-7.56715798283446,132.26223236815));
#78544=CARTESIAN_POINT('Ctrl Pts',(79.1940312582562,-7.54098025767199,132.258961158955));
#78545=CARTESIAN_POINT('Ctrl Pts',(79.3262962095248,-7.47327474193002,132.249814520825));
#78546=CARTESIAN_POINT('Ctrl Pts',(79.4153416452689,-7.43700926514236,132.244039619524));
#78547=CARTESIAN_POINT('Ctrl Pts',(79.5562148879313,-7.39336865188749,132.234865153142));
#78548=CARTESIAN_POINT('Ctrl Pts',(79.6060956539418,-7.38041741116058,132.231607085556));
#78549=CARTESIAN_POINT('Ctrl Pts',(79.6672460728669,-7.36753203877562,132.227513661619));
#78550=CARTESIAN_POINT('Ctrl Pts',(79.6780235330704,-7.36537222606435,132.226788513093));
#78551=CARTESIAN_POINT('Ctrl Pts',(79.6950066493537,-7.3621432606454,132.225638878526));
#78552=CARTESIAN_POINT('Ctrl Pts',(79.7011985697911,-7.36100233538198,132.225218283648));
#78553=CARTESIAN_POINT('Ctrl Pts',(79.7128206219749,-7.3589288984493,132.224425875865));
#78554=CARTESIAN_POINT('Ctrl Pts',(79.7182490928005,-7.35798819180292,132.224054522793));
#78555=CARTESIAN_POINT('Ctrl Pts',(79.7310207746876,-7.35584016693622,132.223178018032));
#78556=CARTESIAN_POINT('Ctrl Pts',(79.7383675124889,-7.35465510712965,132.222671655933));
#78557=CARTESIAN_POINT('Ctrl Pts',(79.762745097692,-7.35089029563906,132.220984849409));
#78558=CARTESIAN_POINT('Ctrl Pts',(79.7798073643738,-7.34852555239971,132.219793541349));
#78559=CARTESIAN_POINT('Ctrl Pts',(79.8215032819806,-7.34340431717928,132.216861126487));
#78560=CARTESIAN_POINT('Ctrl Pts',(79.846167281314,-7.34093228049031,132.215108639107));
#78561=CARTESIAN_POINT('Ctrl Pts',(79.9500010431229,-7.33286031298507,132.207679043735));
#78562=CARTESIAN_POINT('Ctrl Pts',(80.0294615613863,-7.33237120551508,132.201872899958));
#78563=CARTESIAN_POINT('Ctrl Pts',(80.2110508572643,-7.34423914152668,132.188647894957));
#78564=CARTESIAN_POINT('Ctrl Pts',(80.3126280641072,-7.36037912427822,132.181292348828));
#78565=CARTESIAN_POINT('Ctrl Pts',(80.4349492723316,-7.39160582032479,132.172601645145));
#78566=CARTESIAN_POINT('Ctrl Pts',(80.4576851139909,-7.39792723573308,132.170992573184));
#78567=CARTESIAN_POINT('Ctrl Pts',(80.4918928991399,-7.40822600294466,132.168579974081));
#78568=CARTESIAN_POINT('Ctrl Pts',(80.5034674870425,-7.41184900437356,132.167765102057));
#78569=CARTESIAN_POINT('Ctrl Pts',(80.5242487834139,-7.41860385895263,132.166304374011));
#78570=CARTESIAN_POINT('Ctrl Pts',(80.5334694885374,-7.42169050769239,132.165657072925));
#78571=CARTESIAN_POINT('Ctrl Pts',(80.5531724983306,-7.42847852369167,132.164275435761));
#78572=CARTESIAN_POINT('Ctrl Pts',(80.5636458906848,-7.43220445102253,132.163541945084));
#78573=CARTESIAN_POINT('Ctrl Pts',(80.5922965347342,-7.44272118417166,132.16153745116));
#78574=CARTESIAN_POINT('Ctrl Pts',(80.610394031465,-7.44972529122425,132.160273554981));
#78575=CARTESIAN_POINT('Ctrl Pts',(80.6504398305175,-7.46603386303442,132.157478916854));
#78576=CARTESIAN_POINT('Ctrl Pts',(80.6723193056744,-7.47549650092215,132.155953476952));
#78577=CARTESIAN_POINT('Ctrl Pts',(80.7417879430125,-7.5073275406437,132.151104722753));
#78578=CARTESIAN_POINT('Ctrl Pts',(80.7885254753155,-7.53148080649983,132.14783531081));
#78579=CARTESIAN_POINT('Ctrl Pts',(80.9171322188888,-7.60585624908078,132.13868987609));
#78580=CARTESIAN_POINT('Ctrl Pts',(80.9959074435753,-7.66099466397898,132.132914529277));
#78581=CARTESIAN_POINT('Ctrl Pts',(81.1090204556218,-7.75569816072375,132.123737466394));
#78582=CARTESIAN_POINT('Ctrl Pts',(81.1469850335465,-7.79060442767444,132.120477087942));
#78583=CARTESIAN_POINT('Ctrl Pts',(81.1910055738852,-7.83501820474529,132.116381069937));
#78584=CARTESIAN_POINT('Ctrl Pts',(81.1986668831073,-7.84290253316042,132.115655804238));
#78585=CARTESIAN_POINT('Ctrl Pts',(81.2105925175451,-7.85542086153305,132.114506024282));
#78586=CARTESIAN_POINT('Ctrl Pts',(81.2149097137643,-7.86000437199037,132.114085402798));
#78587=CARTESIAN_POINT('Ctrl Pts',(81.2229554815718,-7.86864406812863,132.113292974968));
#78588=CARTESIAN_POINT('Ctrl Pts',(81.2266900412187,-7.87269440978877,132.112921628763));
#78589=CARTESIAN_POINT('Ctrl Pts',(81.2354212421437,-7.88225865071046,132.112045181097));
#78590=CARTESIAN_POINT('Ctrl Pts',(81.2404011027583,-7.88778757944596,132.111538869711));
#78591=CARTESIAN_POINT('Ctrl Pts',(81.2567827100098,-7.9062222444754,132.109852409155));
#78592=CARTESIAN_POINT('Ctrl Pts',(81.2680209550141,-7.91927091344793,132.108661402239));
#78593=CARTESIAN_POINT('Ctrl Pts',(81.2949308263346,-7.95151343423113,132.105729883274));
#78594=CARTESIAN_POINT('Ctrl Pts',(81.3103801199245,-7.97088691895358,132.103977999103));
#78595=CARTESIAN_POINT('Ctrl Pts',(81.3734455078844,-8.05369453133679,132.096552680094));
#78596=CARTESIAN_POINT('Ctrl Pts',(81.4169311826397,-8.1201410488441,132.090750332607));
#78597=CARTESIAN_POINT('Ctrl Pts',(81.5054771231403,-8.27914031728263,132.077524054422));
#78598=CARTESIAN_POINT('Ctrl Pts',(81.5470431553519,-8.37329115606433,132.070163571888));
#78599=CARTESIAN_POINT('Ctrl Pts',(81.587173788204,-8.4930561728192,132.061468365871));
#78600=CARTESIAN_POINT('Ctrl Pts',(81.5941942214222,-8.51558534176302,132.059859336487));
#78601=CARTESIAN_POINT('Ctrl Pts',(81.6040952881193,-8.54990958074568,132.05744678793));
#78602=CARTESIAN_POINT('Ctrl Pts',(81.6073292732164,-8.56159870001947,132.056631924586));
#78603=CARTESIAN_POINT('Ctrl Pts',(81.6129256181999,-8.58272132597783,132.055171205931));
#78604=CARTESIAN_POINT('Ctrl Pts',(81.6153335448347,-8.59214207443145,132.054523905637));
#78605=CARTESIAN_POINT('Ctrl Pts',(81.620317242589,-8.6123769889062,132.053142263587));
#78606=CARTESIAN_POINT('Ctrl Pts',(81.6228675442374,-8.62319698874166,132.052408767294));
#78607=CARTESIAN_POINT('Ctrl Pts',(81.6295717268579,-8.65297190547595,132.05040424095));
#78608=CARTESIAN_POINT('Ctrl Pts',(81.633503136431,-8.67197551056528,132.049140318361));
#78609=CARTESIAN_POINT('Ctrl Pts',(81.6415219596932,-8.71446581748976,132.046345613033));
#78610=CARTESIAN_POINT('Ctrl Pts',(81.6454391430599,-8.73798048730697,132.04482013274));
#78611=CARTESIAN_POINT('Ctrl Pts',(81.6563754769981,-8.81361079262504,132.039971200864));
#78612=CARTESIAN_POINT('Ctrl Pts',(81.6614330148538,-8.86597903814657,132.036701656302));
#78613=CARTESIAN_POINT('Ctrl Pts',(81.6687006217978,-9.01436722626628,132.027556136803));
#78614=CARTESIAN_POINT('Ctrl Pts',(81.6651025996308,-9.11045422485917,132.021780826678));
#78615=CARTESIAN_POINT('Ctrl Pts',(81.6468889631369,-9.25684605866391,132.012603956121));
#78616=CARTESIAN_POINT('Ctrl Pts',(81.6381546126156,-9.30767108964271,132.009343744548));
#78617=CARTESIAN_POINT('Ctrl Pts',(81.6247175969581,-9.36874054232483,132.005247913885));
#78618=CARTESIAN_POINT('Ctrl Pts',(81.6222490813424,-9.37945323773523,132.004522656656));
#78619=CARTESIAN_POINT('Ctrl Pts',(81.618200283463,-9.39626189569163,132.00337288721));
#78620=CARTESIAN_POINT('Ctrl Pts',(81.616691093091,-9.40237489189451,132.00295226765));
#78621=CARTESIAN_POINT('Ctrl Pts',(81.6137964687685,-9.41382038609896,132.002159841269));
#78622=CARTESIAN_POINT('Ctrl Pts',(81.6124191919873,-9.41915474508975,132.001788494566));
#78623=CARTESIAN_POINT('Ctrl Pts',(81.609119571383,-9.43167762882553,132.000912042774));
#78624=CARTESIAN_POINT('Ctrl Pts',(81.6071754986794,-9.43886020711391,132.000405727722));
#78625=CARTESIAN_POINT('Ctrl Pts',(81.60057288572,-9.46262188316392,131.998719242162));
#78626=CARTESIAN_POINT('Ctrl Pts',(81.5957055744258,-9.47914113916711,131.997528213483));
#78627=CARTESIAN_POINT('Ctrl Pts',(81.583212648774,-9.51923757766001,131.994596629776));
#78628=CARTESIAN_POINT('Ctrl Pts',(81.5753155137285,-9.54272539481332,131.992844702014));
#78629=CARTESIAN_POINT('Ctrl Pts',(81.5399498954958,-9.64062586768529,131.985419074057));
#78630=CARTESIAN_POINT('Ctrl Pts',(81.5077098880013,-9.71320209183247,131.979616452315));
#78631=CARTESIAN_POINT('Ctrl Pts',(81.4221540866066,-9.87382882997936,131.966390266095));
#78632=CARTESIAN_POINT('Ctrl Pts',(81.3656017331419,-9.95981114022294,131.959030140193));
#78633=CARTESIAN_POINT('Ctrl Pts',(81.2867522134217,-10.0584807136639,131.950335259466));
#78634=CARTESIAN_POINT('Ctrl Pts',(81.2716324317419,-10.0765982246591,131.948726227032));
#78635=CARTESIAN_POINT('Ctrl Pts',(81.2481656135652,-10.1035332709996,131.946313674854));
#78636=CARTESIAN_POINT('Ctrl Pts',(81.2400992420526,-10.1125902041824,131.945498810888));
#78637=CARTESIAN_POINT('Ctrl Pts',(81.2253887666518,-10.1287483830406,131.944038091559));
#78638=CARTESIAN_POINT('Ctrl Pts',(81.2187800960244,-10.1358809911544,131.943390791208));
#78639=CARTESIAN_POINT('Ctrl Pts',(81.2044831389323,-10.1510429762822,131.942009149506));
#78640=CARTESIAN_POINT('Ctrl Pts',(81.1967761372451,-10.1590541197949,131.941275653614));
#78641=CARTESIAN_POINT('Ctrl Pts',(81.1753974876219,-10.1808358295315,131.939271129589));
#78642=CARTESIAN_POINT('Ctrl Pts',(81.161564271656,-10.1944458983397,131.938007208889));
#78643=CARTESIAN_POINT('Ctrl Pts',(81.1302160694115,-10.2242286337766,131.935212508369));
#78644=CARTESIAN_POINT('Ctrl Pts',(81.112585257366,-10.2402734542893,131.933687030967));
#78645=CARTESIAN_POINT('Ctrl Pts',(81.0549775527976,-10.2904816944714,131.928838111805));
#78646=CARTESIAN_POINT('Ctrl Pts',(81.0137245022189,-10.3231341193944,131.925568576734));
#78647=CARTESIAN_POINT('Ctrl Pts',(80.8930006170416,-10.4097226993484,131.916423063324));
#78648=CARTESIAN_POINT('Ctrl Pts',(80.8103232364147,-10.4588156375441,131.910647750595));
#78649=CARTESIAN_POINT('Ctrl Pts',(80.6774557027464,-10.5229139653606,131.901470866278));
#78650=CARTESIAN_POINT('Ctrl Pts',(80.6300183958495,-10.5431425324435,131.898210642741));
#78651=CARTESIAN_POINT('Ctrl Pts',(80.5714237629889,-10.5649765943034,131.894114798647));
#78652=CARTESIAN_POINT('Ctrl Pts',(80.561084790177,-10.568713071273,131.893389540811));
#78653=CARTESIAN_POINT('Ctrl Pts',(80.5447672815434,-10.5744282315696,131.892239770611));
#78654=CARTESIAN_POINT('Ctrl Pts',(80.5388129940871,-10.576475880417,131.891819150913));
#78655=CARTESIAN_POINT('Ctrl Pts',(80.5276272670334,-10.5802518222227,131.891026724428));
#78656=CARTESIAN_POINT('Ctrl Pts',(80.5223986882551,-10.5819879776801,131.890655377762));
#78657=CARTESIAN_POINT('Ctrl Pts',(80.510088154221,-10.5860080217651,131.889778926266));
#78658=CARTESIAN_POINT('Ctrl Pts',(80.5029994094838,-10.5882704300421,131.889272611477));
#78659=CARTESIAN_POINT('Ctrl Pts',(80.4794553369939,-10.5956112146605,131.887586127711));
#78660=CARTESIAN_POINT('Ctrl Pts',(80.4629370511585,-10.6004817391643,131.886395100593));
#78661=CARTESIAN_POINT('Ctrl Pts',(80.422474853255,-10.6117335231138,131.883463521531));
#78662=CARTESIAN_POINT('Ctrl Pts',(80.3984587527755,-10.6178382002461,131.881711596896));
#78663=CARTESIAN_POINT('Ctrl Pts',(80.2970280123449,-10.6412256095007,131.874285991096));
#78664=CARTESIAN_POINT('Ctrl Pts',(80.2185682447507,-10.6535036168591,131.868483389024));
#78665=CARTESIAN_POINT('Ctrl Pts',(80.0372165552375,-10.6687462564714,131.855257196203));
#78666=CARTESIAN_POINT('Ctrl Pts',(79.9343067437774,-10.6678698944816,131.84789704472));
#78667=CARTESIAN_POINT('Ctrl Pts',(79.8086444060226,-10.6551422042981,131.839202140661));
#78668=CARTESIAN_POINT('Ctrl Pts',(79.7852226168708,-10.652266157235,131.837593108446));
#78669=CARTESIAN_POINT('Ctrl Pts',(79.7498656569269,-10.6471599465411,131.83518055653));
#78670=CARTESIAN_POINT('Ctrl Pts',(79.7378815872724,-10.6452954234043,131.83436569261));
#78671=CARTESIAN_POINT('Ctrl Pts',(79.7163278951061,-10.641700544727,131.832904973331));
#78672=CARTESIAN_POINT('Ctrl Pts',(79.7067511422757,-10.6400169681968,131.832257672985));
#78673=CARTESIAN_POINT('Ctrl Pts',(79.6862586685287,-10.6362291838728,131.830876031261));
#78674=CARTESIAN_POINT('Ctrl Pts',(79.6753481154141,-10.6340993632999,131.830142535341));
#78675=CARTESIAN_POINT('Ctrl Pts',(79.6454532193076,-10.6279524227061,131.828138011154));
#78676=CARTESIAN_POINT('Ctrl Pts',(79.626516084198,-10.6237125133367,131.826874090322));
#78677=CARTESIAN_POINT('Ctrl Pts',(79.5844919699034,-10.6135294197492,131.824079389465));
#78678=CARTESIAN_POINT('Ctrl Pts',(79.5614495768711,-10.6074195851901,131.822553911859));
#78679=CARTESIAN_POINT('Ctrl Pts',(79.4880226746003,-10.5862534035045,131.817704991802));
#78680=CARTESIAN_POINT('Ctrl Pts',(79.4382154393115,-10.5693053790952,131.814435456063));
#78681=CARTESIAN_POINT('Ctrl Pts',(79.3010763505116,-10.5152727150492,131.805361737594));
#78682=CARTESIAN_POINT('Ctrl Pts',(79.2159945627614,-10.4730512116047,131.799654630386));
#78683=CARTESIAN_POINT('Ctrl Pts',(79.0900529554257,-10.3965365960898,131.790494728809));
#78684=CARTESIAN_POINT('Ctrl Pts',(79.046458083827,-10.3671410771866,131.787173617382));
#78685=CARTESIAN_POINT('Ctrl Pts',(78.9954457596652,-10.3291160827815,131.783006928775));
#78686=CARTESIAN_POINT('Ctrl Pts',(78.9866281896581,-10.3224055130902,131.782276032691));
#78687=CARTESIAN_POINT('Ctrl Pts',(78.9728906280675,-10.311732531444,131.781119267297));
#78688=CARTESIAN_POINT('Ctrl Pts',(78.9679249309892,-10.3078290960931,131.780697368555));
#78689=CARTESIAN_POINT('Ctrl Pts',(78.9588177635487,-10.3005859661669,131.779916381778));
#78690=CARTESIAN_POINT('Ctrl Pts',(78.9546699401155,-10.2972545500703,131.779557871074));
#78691=CARTESIAN_POINT('Ctrl Pts',(78.9504874760473,-10.2938622284968,131.779193535027));
#78692=CARTESIAN_POINT('Ctrl Pts',(78.9504367611324,-10.2938210895955,131.77918911681));
#78693=CARTESIAN_POINT('Ctrl Pts',(78.9503356688527,-10.2937390757512,131.779180308942));
#78694=CARTESIAN_POINT('Ctrl Pts',(78.9502852914157,-10.2936982008144,131.779175919291));
#78695=CARTESIAN_POINT('Ctrl Pts',(78.9501848574102,-10.2936167015562,131.779167167118));
#78696=CARTESIAN_POINT('Ctrl Pts',(78.9501348008209,-10.293576077279,131.779162804599));
#78697=CARTESIAN_POINT('Ctrl Pts',(78.9500349921428,-10.2934950662379,131.779154105282));
#78698=CARTESIAN_POINT('Ctrl Pts',(78.9499852401427,-10.2934546796035,131.779149768495));
#78699=CARTESIAN_POINT('Ctrl Pts',(78.9498860248407,-10.2933741311912,131.779141119278));
#78700=CARTESIAN_POINT('Ctrl Pts',(78.9498365615822,-10.2933339695029,131.779136806856));
#78701=CARTESIAN_POINT('Ctrl Pts',(78.9497379087235,-10.2932538589322,131.77912820507));
#78702=CARTESIAN_POINT('Ctrl Pts',(78.9496887189448,-10.293213909956,131.779123915696));
#78703=CARTESIAN_POINT('Ctrl Pts',(78.9495905977843,-10.2931342125669,131.779115358688));
#78704=CARTESIAN_POINT('Ctrl Pts',(78.9495416663926,-10.2930944641939,131.779111091058));
#78705=CARTESIAN_POINT('Ctrl Pts',(78.9494440474455,-10.2930151563256,131.779102576282));
#78706=CARTESIAN_POINT('Ctrl Pts',(78.9493953598266,-10.2929755968237,131.779098329134));
#78707=CARTESIAN_POINT('Ctrl Pts',(78.9492982139278,-10.2928966550517,131.779089854068));
#78708=CARTESIAN_POINT('Ctrl Pts',(78.9492497556804,-10.2928572728501,131.779085626157));
#78709=CARTESIAN_POINT('Ctrl Pts',(78.9491530546733,-10.2927786745468,131.779077188368));
#78710=CARTESIAN_POINT('Ctrl Pts',(78.9491048118317,-10.2927394584177,131.779072978486));
#78711=CARTESIAN_POINT('Ctrl Pts',(78.9435936679568,-10.2882589916685,131.778592008303));
#78712=CARTESIAN_POINT('Ctrl Pts',(78.9381590949362,-10.2837832589096,131.778112828331));
#78713=CARTESIAN_POINT('Ctrl Pts',(78.9263376294428,-10.2739210806555,131.777060051966));
#78714=CARTESIAN_POINT('Ctrl Pts',(78.9199625924164,-10.2685207909121,131.77648554986));
#78715=CARTESIAN_POINT('Ctrl Pts',(78.902520287083,-10.253518631209,131.774895580284));
#78716=CARTESIAN_POINT('Ctrl Pts',(78.8915389116066,-10.2438185807195,131.773874203754));
#78717=CARTESIAN_POINT('Ctrl Pts',(78.8558975721785,-10.2114890830967,131.770495515559));
#78718=CARTESIAN_POINT('Ctrl Pts',(78.8317925055993,-10.1882622355015,131.768108144967));
#78719=CARTESIAN_POINT('Ctrl Pts',(78.7191904794858,-10.0730230819379,131.756512862521));
#78720=CARTESIAN_POINT('Ctrl Pts',(78.6407531864533,-9.97175393740744,131.747097908635));
#78721=CARTESIAN_POINT('Ctrl Pts',(78.54727896112,-9.81728396794897,131.734312245805));
#78722=CARTESIAN_POINT('Ctrl Pts',(78.5220724739797,-9.77076765711,131.730632540249));
#78723=CARTESIAN_POINT('Ctrl Pts',(78.4919262977753,-9.70819792594375,131.725900734967));
#78724=CARTESIAN_POINT('Ctrl Pts',(78.4849566348642,-9.69316248446617,131.72477945326));
#78725=CARTESIAN_POINT('Ctrl Pts',(78.4739348051216,-9.66842462994766,131.722959589786));
#78726=CARTESIAN_POINT('Ctrl Pts',(78.4697482366556,-9.6587837387716,131.722256453152));
#78727=CARTESIAN_POINT('Ctrl Pts',(78.4618068342,-9.64001190520926,131.720898908933));
#78728=CARTESIAN_POINT('Ctrl Pts',(78.4580413866192,-9.63088596108174,131.720244164257));
#78729=CARTESIAN_POINT('Ctrl Pts',(78.449388458603,-9.60937436899457,131.718712730757));
#78730=CARTESIAN_POINT('Ctrl Pts',(78.4445678521679,-9.5969624145978,131.717838314566));
#78731=CARTESIAN_POINT('Ctrl Pts',(78.4289998366686,-9.55540898736597,131.714940153122));
#78732=CARTESIAN_POINT('Ctrl Pts',(78.4189181815305,-9.52602389371686,131.712938367513));
#78733=CARTESIAN_POINT('Ctrl Pts',(78.3964437244496,-9.45401759116544,131.708132387151));
#78734=CARTESIAN_POINT('Ctrl Pts',(78.3849206709727,-9.41114947304623,131.705354187579));
#78735=CARTESIAN_POINT('Ctrl Pts',(78.3477129961438,-9.24680354893202,131.69491768606));
#78736=CARTESIAN_POINT('Ctrl Pts',(78.3339233495109,-9.12306938570736,131.687524146382));
#78737=CARTESIAN_POINT('Ctrl Pts',(78.3340003204321,-8.99896671418601,131.679718342728));
#78738=CARTESIAN_POINT('Ctrl Pts',(78.3340003219591,-8.998964255121,131.679718188058));
#78739=CARTESIAN_POINT('Ctrl Pts',(78.3340235477069,-8.96160554903245,131.677368400364));
#78740=CARTESIAN_POINT('Ctrl Pts',(78.3353033767596,-8.92426065044466,131.674981768813));
#78741=CARTESIAN_POINT('Ctrl Pts',(78.3383818272231,-8.87898127153856,131.672008370228));
#78742=CARTESIAN_POINT('Ctrl Pts',(78.3389844347566,-8.87097375979838,131.671479493273));
#78743=CARTESIAN_POINT('Ctrl Pts',(78.3401157678519,-8.85726559464761,131.670568408757));
#78744=CARTESIAN_POINT('Ctrl Pts',(78.3406160404092,-8.85156264999074,131.670187684067));
#78745=CARTESIAN_POINT('Ctrl Pts',(78.3416182463319,-8.84077673723529,131.669464231128));
#78746=CARTESIAN_POINT('Ctrl Pts',(78.3421141841099,-8.83569324959901,131.669121833836));
#78747=CARTESIAN_POINT('Ctrl Pts',(78.3431534777294,-8.82552433291402,131.668433904773));
#78748=CARTESIAN_POINT('Ctrl Pts',(78.3436968895286,-8.82043897635919,131.668088376536));
#78749=CARTESIAN_POINT('Ctrl Pts',(78.3450460614502,-8.80834068753394,131.667262899008));
#78750=CARTESIAN_POINT('Ctrl Pts',(78.345872988445,-8.8013302842618,131.666781809456));
#78751=CARTESIAN_POINT('Ctrl Pts',(78.3489767353076,-8.77638170300056,131.665060362435));
#78752=CARTESIAN_POINT('Ctrl Pts',(78.351500922452,-8.75847631837876,131.663807664797));
#78753=CARTESIAN_POINT('Ctrl Pts',(78.3619153581104,-8.69240090991068,131.659129490043));
#78754=CARTESIAN_POINT('Ctrl Pts',(78.3716295171211,-8.64454636678423,131.655632552103));
#78755=CARTESIAN_POINT('Ctrl Pts',(78.3980065525462,-8.53868875348034,131.647741443782));
#78756=CARTESIAN_POINT('Ctrl Pts',(78.4157446379831,-8.48103793269769,131.643337557353));
#78757=CARTESIAN_POINT('Ctrl Pts',(78.4365593409241,-8.42449213250519,131.638964580993));
#78758=CARTESIAN_POINT('',(78.3340002424327,-9.00128863288225,131.870599662366));
#78759=CARTESIAN_POINT('Ctrl Pts',(78.4365593750065,-8.42449203991602,131.833731407018));
#78760=CARTESIAN_POINT('Ctrl Pts',(78.435054346559,-8.42858064125575,131.834020585971));
#78761=CARTESIAN_POINT('Ctrl Pts',(78.4335653428238,-8.43267518337795,131.834309232973));
#78762=CARTESIAN_POINT('Ctrl Pts',(78.4278795475944,-8.4485033348739,131.835421421153));
#78763=CARTESIAN_POINT('Ctrl Pts',(78.4237983197513,-8.46027825154674,131.836241125397));
#78764=CARTESIAN_POINT('Ctrl Pts',(78.4115574972136,-8.49691828400013,131.838769040101));
#78765=CARTESIAN_POINT('Ctrl Pts',(78.4038510981433,-8.52193138397899,131.840462454949));
#78766=CARTESIAN_POINT('Ctrl Pts',(78.3871741035046,-8.58097003216267,131.844392686761));
#78767=CARTESIAN_POINT('Ctrl Pts',(78.3786855856983,-8.61511911372465,131.846614795668));
#78768=CARTESIAN_POINT('Ctrl Pts',(78.346405873371,-8.76512322839677,131.856205052507));
#78769=CARTESIAN_POINT('Ctrl Pts',(78.333909190809,-8.88304341633613,131.863279796691));
#78770=CARTESIAN_POINT('Ctrl Pts',(78.3340004966965,-9.00128646516507,131.870599084676));
#78771=CARTESIAN_POINT('Ctrl Pts',(78.3340004983928,-9.0012886600276,131.870599220539));
#78772=CARTESIAN_POINT('Ctrl Pts',(78.3340321196368,-9.04216909052046,131.873129735217));
#78773=CARTESIAN_POINT('Ctrl Pts',(78.3355684237451,-9.08303249464215,131.87568896695));
#78774=CARTESIAN_POINT('Ctrl Pts',(78.3400975380125,-9.14381523758201,131.879593155217));
#78775=CARTESIAN_POINT('Ctrl Pts',(78.3419509048717,-9.16380513354296,131.880892980567));
#78776=CARTESIAN_POINT('Ctrl Pts',(78.3449992886001,-9.19127433863501,131.882706986491));
#78777=CARTESIAN_POINT('Ctrl Pts',(78.3458848578507,-9.19878711905922,131.883205992588));
#78778=CARTESIAN_POINT('Ctrl Pts',(78.3475086460371,-9.21179970775164,131.884075702536));
#78779=CARTESIAN_POINT('Ctrl Pts',(78.3482232444392,-9.21730241307577,131.884445159621));
#78780=CARTESIAN_POINT('Ctrl Pts',(78.3497070429375,-9.22829787079051,131.885186948462));
#78781=CARTESIAN_POINT('Ctrl Pts',(78.3504761918229,-9.2337904346705,131.885559272398));
#78782=CARTESIAN_POINT('Ctrl Pts',(78.3521570865827,-9.24537245666064,131.886348286418));
#78783=CARTESIAN_POINT('Ctrl Pts',(78.353075152663,-9.25146064089973,131.886765292928));
#78784=CARTESIAN_POINT('Ctrl Pts',(78.3556732395593,-9.26806514286679,131.887908511837));
#78785=CARTESIAN_POINT('Ctrl Pts',(78.3574203499857,-9.27857044804912,131.888638277172));
#78786=CARTESIAN_POINT('Ctrl Pts',(78.3667644898343,-9.33160905197933,131.892353057818));
#78787=CARTESIAN_POINT('Ctrl Pts',(78.3759127776337,-9.37384861842069,131.895410201041));
#78788=CARTESIAN_POINT('Ctrl Pts',(78.4088204323466,-9.50156735091101,131.904867664855));
#78789=CARTESIAN_POINT('Ctrl Pts',(78.4377723653983,-9.5855483814739,131.911376125597));
#78790=CARTESIAN_POINT('Ctrl Pts',(78.5110634565282,-9.75335190586252,131.924626964921));
#78791=CARTESIAN_POINT('Ctrl Pts',(78.5561479364638,-9.83652123578932,131.931330721001));
#78792=CARTESIAN_POINT('Ctrl Pts',(78.6182535411965,-9.93095533943586,131.93905542961));
#78793=CARTESIAN_POINT('Ctrl Pts',(78.6287207077375,-9.94630559099729,131.940315497481));
#78794=CARTESIAN_POINT('Ctrl Pts',(78.6457553790043,-9.97041081411814,131.942302096822));
#78795=CARTESIAN_POINT('Ctrl Pts',(78.6521558848247,-9.97928131439143,131.943034886225));
#78796=CARTESIAN_POINT('Ctrl Pts',(78.6644233302848,-9.99593470284866,131.944414198127));
#78797=CARTESIAN_POINT('Ctrl Pts',(78.6702720760128,-10.003730356265,131.945061385013));
#78798=CARTESIAN_POINT('Ctrl Pts',(78.6837146170901,-10.0213238653724,131.946525720378));
#78799=CARTESIAN_POINT('Ctrl Pts',(78.6913500901491,-10.0310892660324,131.94734118974));
#78800=CARTESIAN_POINT('Ctrl Pts',(78.7152193585032,-10.0609245907382,131.949841873932));
#78801=CARTESIAN_POINT('Ctrl Pts',(78.7318116063492,-10.0807037514705,131.951512761807));
#78802=CARTESIAN_POINT('Ctrl Pts',(78.8371123049505,-10.2004631756827,131.96173330062));
#78803=CARTESIAN_POINT('Ctrl Pts',(78.937122555842,-10.2898503742027,131.969771336136));
#78804=CARTESIAN_POINT('Ctrl Pts',(79.1059551663074,-10.4076406214928,131.98239783046));
#78805=CARTESIAN_POINT('Ctrl Pts',(79.1677812414,-10.4450528791687,131.986870517345));
#78806=CARTESIAN_POINT('Ctrl Pts',(79.2459000760047,-10.485644883087,131.992581476702));
#78807=CARTESIAN_POINT('Ctrl Pts',(79.26007304626,-10.4927543241237,131.993619969719));
#78808=CARTESIAN_POINT('Ctrl Pts',(79.280825733421,-10.5027961315938,131.995147131803));
#78809=CARTESIAN_POINT('Ctrl Pts',(79.2873268972639,-10.5058900632867,131.995626467001));
#78810=CARTESIAN_POINT('Ctrl Pts',(79.2988124666569,-10.5112650626089,131.996475284383));
#78811=CARTESIAN_POINT('Ctrl Pts',(79.3037883786177,-10.5135638154085,131.99684368125));
#78812=CARTESIAN_POINT('Ctrl Pts',(79.3146377432341,-10.5185111413832,131.997648455186));
#78813=CARTESIAN_POINT('Ctrl Pts',(79.3205151546212,-10.5211501736821,131.998085361834));
#78814=CARTESIAN_POINT('Ctrl Pts',(79.3370629895589,-10.5284653233663,131.999317795776));
#78815=CARTESIAN_POINT('Ctrl Pts',(79.3477671251166,-10.5330635937391,132.000117706979));
#78816=CARTESIAN_POINT('Ctrl Pts',(79.4295022931189,-10.5671643727818,132.00624139629));
#78817=CARTESIAN_POINT('Ctrl Pts',(79.5024443227339,-10.5918252023334,132.011791715511));
#78818=CARTESIAN_POINT('Ctrl Pts',(79.6322218136303,-10.6259078611341,132.021544744789));
#78819=CARTESIAN_POINT('Ctrl Pts',(79.6883394136397,-10.6375912532945,132.025724771962));
#78820=CARTESIAN_POINT('Ctrl Pts',(79.8266839939385,-10.6590234117932,132.035840904689));
#78821=CARTESIAN_POINT('Ctrl Pts',(79.9092591257557,-10.6655830223465,132.04171443686));
#78822=CARTESIAN_POINT('Ctrl Pts',(80.0148230932484,-10.6660905123571,132.048971847056));
#78823=CARTESIAN_POINT('Ctrl Pts',(80.0376560194855,-10.665730900642,132.050527246296));
#78824=CARTESIAN_POINT('Ctrl Pts',(80.0722884332743,-10.6644729241821,132.052865791811));
#78825=CARTESIAN_POINT('Ctrl Pts',(80.0840968650154,-10.6639181057682,132.053659515976));
#78826=CARTESIAN_POINT('Ctrl Pts',(80.104645865219,-10.6627332951643,132.05503471007));
#78827=CARTESIAN_POINT('Ctrl Pts',(80.1133890952879,-10.6621599459911,132.05561792388));
#78828=CARTESIAN_POINT('Ctrl Pts',(80.1330971801894,-10.6607113306497,132.056928432906));
#78829=CARTESIAN_POINT('Ctrl Pts',(80.1440587804744,-10.6597963913257,132.057654460407));
#78830=CARTESIAN_POINT('Ctrl Pts',(80.173792706204,-10.6570177844738,132.059616572637));
#78831=CARTESIAN_POINT('Ctrl Pts',(80.1925440956127,-10.6549437032903,132.060846053678));
#78832=CARTESIAN_POINT('Ctrl Pts',(80.3094567004957,-10.6399979732241,132.068469883845));
#78833=CARTESIAN_POINT('Ctrl Pts',(80.4063476699741,-10.6187161656053,132.074587432156));
#78834=CARTESIAN_POINT('Ctrl Pts',(80.568823531528,-10.5675090846156,132.085008159284));
#78835=CARTESIAN_POINT('Ctrl Pts',(80.6354111525916,-10.5417188122892,132.089334227471));
#78836=CARTESIAN_POINT('Ctrl Pts',(80.7338037839405,-10.4961498845915,132.096065986805));
#78837=CARTESIAN_POINT('Ctrl Pts',(80.7669370175872,-10.4794389900358,132.098395687312));
#78838=CARTESIAN_POINT('Ctrl Pts',(80.8132427379196,-10.4541108070232,132.101780367295));
#78839=CARTESIAN_POINT('Ctrl Pts',(80.8268953831342,-10.4463906721799,132.102794787423));
#78840=CARTESIAN_POINT('Ctrl Pts',(80.8509431208304,-10.4323406986326,132.104614791611));
#78841=CARTESIAN_POINT('Ctrl Pts',(80.8613818395354,-10.4260874367043,132.105416175597));
#78842=CARTESIAN_POINT('Ctrl Pts',(80.8772741086849,-10.4163291100904,132.106655237239));
#78843=CARTESIAN_POINT('Ctrl Pts',(80.8827775151652,-10.4129054692478,132.10708786011));
#78844=CARTESIAN_POINT('Ctrl Pts',(80.8928939731447,-10.4065298952878,132.10788994706));
#78845=CARTESIAN_POINT('Ctrl Pts',(80.8975126161732,-10.4035872236395,132.108258814229));
#78846=CARTESIAN_POINT('Ctrl Pts',(80.9080233227687,-10.3968174567629,132.109104342529));
#78847=CARTESIAN_POINT('Ctrl Pts',(80.913905741243,-10.3929758267279,132.10958193402));
#78848=CARTESIAN_POINT('Ctrl Pts',(80.932533132624,-10.3806420636811,132.111107838917));
#78849=CARTESIAN_POINT('Ctrl Pts',(80.9451849632606,-10.37201162356,132.11216457811));
#78850=CARTESIAN_POINT('Ctrl Pts',(81.0407800692325,-10.3048517451646,132.120294978693));
#78851=CARTESIAN_POINT('Ctrl Pts',(81.1183298665335,-10.2390303195043,132.127724832671));
#78852=CARTESIAN_POINT('Ctrl Pts',(81.2703564375848,-10.0840282279089,132.143516198847));
#78853=CARTESIAN_POINT('Ctrl Pts',(81.342514178779,-9.9932712513982,132.15180978059));
#78854=CARTESIAN_POINT('Ctrl Pts',(81.4151572946302,-9.8793544402138,132.161055526028));
#78855=CARTESIAN_POINT('Ctrl Pts',(81.4253286015919,-9.86277044061573,132.162376217263));
#78856=CARTESIAN_POINT('Ctrl Pts',(81.4408565887629,-9.83642814570942,132.164435509861));
#78857=CARTESIAN_POINT('Ctrl Pts',(81.4464096585687,-9.82678828142979,132.165181177672));
#78858=CARTESIAN_POINT('Ctrl Pts',(81.456632720532,-9.80862326335147,132.166571804607));
#78859=CARTESIAN_POINT('Ctrl Pts',(81.4613254390525,-9.80011151259059,132.167217557667));
#78860=CARTESIAN_POINT('Ctrl Pts',(81.4716962007195,-9.78090517417354,132.168661827098));
#78861=CARTESIAN_POINT('Ctrl Pts',(81.4773327242669,-9.77018869960252,132.169458848109));
#78862=CARTESIAN_POINT('Ctrl Pts',(81.4935673849794,-9.73848836294817,132.171791495594));
#78863=CARTESIAN_POINT('Ctrl Pts',(81.5038390874986,-9.71734000532881,132.173315767468));
#78864=CARTESIAN_POINT('Ctrl Pts',(81.5589385377694,-9.59750640443749,132.181789878686));
#78865=CARTESIAN_POINT('Ctrl Pts',(81.5945013405354,-9.49484573089368,132.188416594995));
#78866=CARTESIAN_POINT('Ctrl Pts',(81.637382106173,-9.31649057665,132.199617765142));
#78867=CARTESIAN_POINT('Ctrl Pts',(81.6499725231119,-9.24243664599759,132.204189811422));
#78868=CARTESIAN_POINT('Ctrl Pts',(81.6611299141817,-9.13221894674011,132.21118281793));
#78869=CARTESIAN_POINT('Ctrl Pts',(81.6635845998015,-9.09654166499363,132.213475795502));
#78870=CARTESIAN_POINT('Ctrl Pts',(81.6652439304393,-9.05111621041222,132.216463657714));
#78871=CARTESIAN_POINT('Ctrl Pts',(81.665513469019,-9.0414136231496,132.217105808627));
#78872=CARTESIAN_POINT('Ctrl Pts',(81.6658114616797,-9.02576009777273,132.218149004307));
#78873=CARTESIAN_POINT('Ctrl Pts',(81.6658928419021,-9.01981022479718,132.218547196219));
#78874=CARTESIAN_POINT('Ctrl Pts',(81.6659887283855,-9.00828500870662,132.219321981245));
#78875=CARTESIAN_POINT('Ctrl Pts',(81.6660071241545,-9.00270983260339,132.21969835942));
#78876=CARTESIAN_POINT('Ctrl Pts',(81.6659856911072,-8.99024732520934,132.220543100376));
#78877=CARTESIAN_POINT('Ctrl Pts',(81.6659311354573,-8.98336012657935,132.221012251989));
#78878=CARTESIAN_POINT('Ctrl Pts',(81.6656405062171,-8.96278152621034,132.222420594565));
#78879=CARTESIAN_POINT('Ctrl Pts',(81.6652783387284,-8.94909287055782,132.223366060494));
#78880=CARTESIAN_POINT('Ctrl Pts',(81.6607646042034,-8.83275412547422,132.231466563769));
#78881=CARTESIAN_POINT('Ctrl Pts',(81.6472952179804,-8.73069485031223,132.238988976958));
#78882=CARTESIAN_POINT('Ctrl Pts',(81.599076449266,-8.518679487388,132.254801368189));
#78883=CARTESIAN_POINT('Ctrl Pts',(81.5621480966043,-8.40973101139748,132.263026382946));
#78884=CARTESIAN_POINT('Ctrl Pts',(81.5062203657711,-8.28779750578302,132.272205704492));
#78885=CARTESIAN_POINT('Ctrl Pts',(81.4978266768859,-8.27031000815241,132.273522440321));
#78886=CARTESIAN_POINT('Ctrl Pts',(81.4841464916188,-8.2430398459942,132.275576995798));
#78887=CARTESIAN_POINT('Ctrl Pts',(81.4790644264461,-8.2331571763924,132.27632182792));
#78888=CARTESIAN_POINT('Ctrl Pts',(81.4693520872585,-8.21472620434297,132.277711697275));
#78889=CARTESIAN_POINT('Ctrl Pts',(81.4647451636199,-8.20616619939979,132.278357520174));
#78890=CARTESIAN_POINT('Ctrl Pts',(81.4542240252029,-8.18702060229962,132.279802977315));
#78891=CARTESIAN_POINT('Ctrl Pts',(81.4482685953857,-8.1764581946507,132.28060110517));
#78892=CARTESIAN_POINT('Ctrl Pts',(81.4303880270165,-8.14553956842806,132.282940261883));
#78893=CARTESIAN_POINT('Ctrl Pts',(81.4181449225842,-8.12537001819633,132.284469838377));
#78894=CARTESIAN_POINT('Ctrl Pts',(81.3503006574022,-8.01877417389043,132.292587183117));
#78895=CARTESIAN_POINT('Ctrl Pts',(81.2872197795695,-7.93736904122788,132.298888959422));
#78896=CARTESIAN_POINT('Ctrl Pts',(81.1628989994817,-7.8043806226364,132.310007421919));
#78897=CARTESIAN_POINT('Ctrl Pts',(81.104705132187,-7.75041422878135,132.314825524784));
#78898=CARTESIAN_POINT('Ctrl Pts',(81.0235808504587,-7.68529405402791,132.321384851457));
#78899=CARTESIAN_POINT('Ctrl Pts',(81.0039231563842,-7.670222707349,132.32296362833));
#78900=CARTESIAN_POINT('Ctrl Pts',(80.9700456731267,-7.64542856887439,132.325680447472));
#78901=CARTESIAN_POINT('Ctrl Pts',(80.9559973453454,-7.63547759674423,132.326805944588));
#78902=CARTESIAN_POINT('Ctrl Pts',(80.9356617934914,-7.62154131515328,132.328437532949));
#78903=CARTESIAN_POINT('Ctrl Pts',(80.9294976051768,-7.61737729862326,132.328932413844));
#78904=CARTESIAN_POINT('Ctrl Pts',(80.9187212386999,-7.61020230887844,132.329798497944));
#78905=CARTESIAN_POINT('Ctrl Pts',(80.9141216855576,-7.60717270285408,132.330168457883));
#78906=CARTESIAN_POINT('Ctrl Pts',(80.9042330860898,-7.60072942211105,132.330964597894));
#78907=CARTESIAN_POINT('Ctrl Pts',(80.89893977881,-7.59732295416597,132.331391199042));
#78908=CARTESIAN_POINT('Ctrl Pts',(80.884352235185,-7.58805173509775,132.33256775388));
#78909=CARTESIAN_POINT('Ctrl Pts',(80.8750192689168,-7.58224894937167,132.333321505046));
#78910=CARTESIAN_POINT('Ctrl Pts',(80.8216179210651,-7.54977471444806,132.337637007748));
#78911=CARTESIAN_POINT('Ctrl Pts',(80.7763926333708,-7.52506855153028,132.341301377097));
#78912=CARTESIAN_POINT('Ctrl Pts',(80.6437991547922,-7.46042309691272,132.351931447797));
#78913=CARTESIAN_POINT('Ctrl Pts',(80.5540209569969,-7.42588557037395,132.358983590216));
#78914=CARTESIAN_POINT('Ctrl Pts',(80.4112410286266,-7.38469758446319,132.369670221335));
#78915=CARTESIAN_POINT('Ctrl Pts',(80.3600518318519,-7.37252199859724,132.373404780799));
#78916=CARTESIAN_POINT('Ctrl Pts',(80.28494499347,-7.35837566484272,132.378731250655));
#78917=CARTESIAN_POINT('Ctrl Pts',(80.2614289099509,-7.35446691580834,132.380377795236));
#78918=CARTESIAN_POINT('Ctrl Pts',(80.2186318496623,-7.34829403776919,132.383336598715));
#78919=CARTESIAN_POINT('Ctrl Pts',(80.1993801203271,-7.34585971145186,132.384653849583));
#78920=CARTESIAN_POINT('Ctrl Pts',(80.169040771893,-7.34256078971381,132.386709021938));
#78921=CARTESIAN_POINT('Ctrl Pts',(80.1579800440934,-7.34146997784515,132.387453962916));
#78922=CARTESIAN_POINT('Ctrl Pts',(80.137226413665,-7.33963275193658,132.388843930783));
#78923=CARTESIAN_POINT('Ctrl Pts',(80.127536347605,-7.338860338823,132.389489744417));
#78924=CARTESIAN_POINT('Ctrl Pts',(80.1057474812901,-7.33731529387086,132.390935046019));
#78925=CARTESIAN_POINT('Ctrl Pts',(80.0936458076379,-7.33658981682944,132.391733029045));
#78926=CARTESIAN_POINT('Ctrl Pts',(80.0579852011558,-7.33484242892865,132.394071333496));
#78927=CARTESIAN_POINT('Ctrl Pts',(80.0344106487367,-7.33418848102524,132.395600215382));
#78928=CARTESIAN_POINT('Ctrl Pts',(79.9068353987634,-7.33335921114161,132.403796257104));
#78929=CARTESIAN_POINT('Ctrl Pts',(79.8030026469127,-7.3424214689515,132.410169518184));
#78930=CARTESIAN_POINT('Ctrl Pts',(79.6236308787605,-7.37518083371644,132.421304936487));
#78931=CARTESIAN_POINT('Ctrl Pts',(79.5476725925114,-7.39466849524455,132.426068245187));
#78932=CARTESIAN_POINT('Ctrl Pts',(79.4500218901552,-7.42720444123743,132.432559826914));
#78933=CARTESIAN_POINT('Ctrl Pts',(79.4268475844415,-7.43550072809721,132.434129018617));
#78934=CARTESIAN_POINT('Ctrl Pts',(79.3878662013054,-7.45043818271576,132.436830941777));
#78935=CARTESIAN_POINT('Ctrl Pts',(79.3719618913626,-7.45681572997584,132.437951307948));
#78936=CARTESIAN_POINT('Ctrl Pts',(79.3493112457265,-7.46630665437703,132.43957675623));
#78937=CARTESIAN_POINT('Ctrl Pts',(79.342482371947,-7.46922186554151,132.44007074325));
#78938=CARTESIAN_POINT('Ctrl Pts',(79.3306239265987,-7.47437816285633,132.440935819748));
#78939=CARTESIAN_POINT('Ctrl Pts',(79.3255856150809,-7.47659868911413,132.441305675039));
#78940=CARTESIAN_POINT('Ctrl Pts',(79.314803683406,-7.48141456293347,132.44210224547));
#78941=CARTESIAN_POINT('Ctrl Pts',(79.3090638500406,-7.48401749504684,132.442529387471));
#78942=CARTESIAN_POINT('Ctrl Pts',(79.2933248968458,-7.49126283487397,132.443708854159));
#78943=CARTESIAN_POINT('Ctrl Pts',(79.283357085113,-7.49597192474842,132.444465005974));
#78944=CARTESIAN_POINT('Ctrl Pts',(79.226491354791,-7.52353059882319,132.448828578866));
#78945=CARTESIAN_POINT('Ctrl Pts',(79.1806447868976,-7.54847203637923,132.452541224214));
#78946=CARTESIAN_POINT('Ctrl Pts',(79.0487712547293,-7.62845371138045,132.463659344451));
#78947=CARTESIAN_POINT('Ctrl Pts',(78.9665372630134,-7.68930099715414,132.47116230885));
#78948=CARTESIAN_POINT('Ctrl Pts',(78.8359641567243,-7.80588925293691,132.483711487921));
#78949=CARTESIAN_POINT('Ctrl Pts',(78.7847831076796,-7.8580146797057,132.488839183625));
#78950=CARTESIAN_POINT('Ctrl Pts',(78.725682703302,-7.92669571786026,132.495022772812));
#78951=CARTESIAN_POINT('Ctrl Pts',(78.7143987392386,-7.94023771793119,132.496216955377));
#78952=CARTESIAN_POINT('Ctrl Pts',(78.6965917590267,-7.96231113674697,132.498124380316));
#78953=CARTESIAN_POINT('Ctrl Pts',(78.6899328687333,-7.97073067642218,132.498843047088));
#78954=CARTESIAN_POINT('Ctrl Pts',(78.6773568413267,-7.98695166459002,132.50021101604));
#78955=CARTESIAN_POINT('Ctrl Pts',(78.6714262193241,-7.99474203741312,132.500860833758));
#78956=CARTESIAN_POINT('Ctrl Pts',(78.6580440528446,-8.01264594587972,132.502338278073));
#78957=CARTESIAN_POINT('Ctrl Pts',(78.6506374691082,-8.0227924647801,132.503164134606));
#78958=CARTESIAN_POINT('Ctrl Pts',(78.6311692136781,-8.05010609921862,132.505357818712));
#78959=CARTESIAN_POINT('Ctrl Pts',(78.6193156260609,-8.06741924378956,132.506717773559));
#78960=CARTESIAN_POINT('Ctrl Pts',(78.5412032923739,-8.1862640141107,132.515861061319));
#78961=CARTESIAN_POINT('Ctrl Pts',(78.4858706108274,-8.29454260679863,132.523223016254));
#78962=CARTESIAN_POINT('Ctrl Pts',(78.4406740918851,-8.41340500872868,132.530993826561));
#78963=CARTESIAN_POINT('Ctrl Pts',(78.4386018914004,-8.41894328418144,132.531355307084));
#78964=CARTESIAN_POINT('Ctrl Pts',(78.4365593757978,-8.42449203776637,132.531716974833));
#78965=CARTESIAN_POINT('Origin',(80.,-9.,134.));
#78966=CARTESIAN_POINT('',(78.4365594153165,-8.4244919304089,133.231049000392));
#78967=CARTESIAN_POINT('',(78.4365593697901,-8.4244920540871,133.038342736257));
#78968=CARTESIAN_POINT('',(78.4365593749993,-8.42449203993574,134.));
#78969=CARTESIAN_POINT('Ctrl Pts',(78.4365593697901,-8.4244920540871,133.038342736257));
#78970=CARTESIAN_POINT('Ctrl Pts',(78.4628061193141,-8.35318941629014,133.03360761879));
#78971=CARTESIAN_POINT('Ctrl Pts',(78.4939041984131,-8.28375384386915,133.02898652258));
#78972=CARTESIAN_POINT('Ctrl Pts',(78.561214954218,-8.1574070897627,133.020239035207));
#78973=CARTESIAN_POINT('Ctrl Pts',(78.5963402310007,-8.10010937121719,133.016124919609));
#78974=CARTESIAN_POINT('Ctrl Pts',(78.6535462851658,-8.01832521231255,133.009803734371));
#78975=CARTESIAN_POINT('Ctrl Pts',(78.6730506737764,-7.99211699782551,133.007703247721));
#78976=CARTESIAN_POINT('Ctrl Pts',(78.6991841628878,-7.95907551198317,133.004932413371));
#78977=CARTESIAN_POINT('Ctrl Pts',(78.7051202654679,-7.95170037940832,133.004305759935));
#78978=CARTESIAN_POINT('Ctrl Pts',(78.7148565738052,-7.93981267045829,133.003281565034));
#78979=CARTESIAN_POINT('Ctrl Pts',(78.7186185588224,-7.93526886065503,133.002886689248));
#78980=CARTESIAN_POINT('Ctrl Pts',(78.7260049108909,-7.92644330276556,133.002112831928));
#78981=CARTESIAN_POINT('Ctrl Pts',(78.7296269035633,-7.92215972345916,133.001734017121));
#78982=CARTESIAN_POINT('Ctrl Pts',(78.7387075861672,-7.91152973305655,133.000786086764));
#78983=CARTESIAN_POINT('Ctrl Pts',(78.7441925567266,-7.90520607728211,133.000215108605));
#78984=CARTESIAN_POINT('Ctrl Pts',(78.7640094902605,-7.88270388410603,132.99815869683));
#78985=CARTESIAN_POINT('Ctrl Pts',(78.7786076633492,-7.86676401301595,132.996655858209));
#78986=CARTESIAN_POINT('Ctrl Pts',(78.8874916271528,-7.7524208418627,132.985560771926));
#78987=CARTESIAN_POINT('Ctrl Pts',(78.9932244310413,-7.66563394739609,132.975447055159));
#78988=CARTESIAN_POINT('Ctrl Pts',(79.1502573126506,-7.56613988581271,132.962107931343));
#78989=CARTESIAN_POINT('Ctrl Pts',(79.1933347581965,-7.54147011898524,132.958592383899));
#78990=CARTESIAN_POINT('Ctrl Pts',(79.2673572284867,-7.50336315150526,132.95279812802));
#78991=CARTESIAN_POINT('Ctrl Pts',(79.2977228468922,-7.48887645458893,132.950486878261));
#78992=CARTESIAN_POINT('Ctrl Pts',(79.3410671274373,-7.46978701217852,132.947276870002));
#78993=CARTESIAN_POINT('Ctrl Pts',(79.3536941822265,-7.46441114613154,132.946352084262));
#78994=CARTESIAN_POINT('Ctrl Pts',(79.3755799234528,-7.4554112591725,132.944766555005));
#78995=CARTESIAN_POINT('Ctrl Pts',(79.3848071100372,-7.45171303506075,132.944103333911));
#78996=CARTESIAN_POINT('Ctrl Pts',(79.4037294557153,-7.44432489458287,132.942753704367));
#78997=CARTESIAN_POINT('Ctrl Pts',(79.413427095572,-7.44064249396593,132.942067571759));
#78998=CARTESIAN_POINT('Ctrl Pts',(79.438095306397,-7.43153813951464,132.940335843413));
#78999=CARTESIAN_POINT('Ctrl Pts',(79.4531105909201,-7.42623969568196,132.939294369759));
#79000=CARTESIAN_POINT('Ctrl Pts',(79.5125729198906,-7.40621105941954,132.935216709227));
#79001=CARTESIAN_POINT('Ctrl Pts',(79.5575589068905,-7.39314131368899,132.932234517607));
#79002=CARTESIAN_POINT('Ctrl Pts',(79.7122185630681,-7.35519744060681,132.922242261325));
#79003=CARTESIAN_POINT('Ctrl Pts',(79.8238262386276,-7.33953113110188,132.91548705435));
#79004=CARTESIAN_POINT('Ctrl Pts',(80.0010847397146,-7.33273401068903,132.90457282982));
#79005=CARTESIAN_POINT('Ctrl Pts',(80.0660898201429,-7.33404462124014,132.900525133508));
#79006=CARTESIAN_POINT('Ctrl Pts',(80.1459140896061,-7.34033329199974,132.895323701359));
#79007=CARTESIAN_POINT('Ctrl Pts',(80.1609662175044,-7.34172549294908,132.894332642906));
#79008=CARTESIAN_POINT('Ctrl Pts',(80.183022414331,-7.34406862638646,132.892862624704));
#79009=CARTESIAN_POINT('Ctrl Pts',(80.1900431875613,-7.34485967344103,132.892392044608));
#79010=CARTESIAN_POINT('Ctrl Pts',(80.2019749655849,-7.34628097086639,132.891587452357));
#79011=CARTESIAN_POINT('Ctrl Pts',(80.2068885363969,-7.34688849539379,132.891254708467));
#79012=CARTESIAN_POINT('Ctrl Pts',(80.2180703928207,-7.34832167942787,132.890494193003));
#79013=CARTESIAN_POINT('Ctrl Pts',(80.2243365903599,-7.3491611036296,132.890065680317));
#79014=CARTESIAN_POINT('Ctrl Pts',(80.241597854255,-7.35157352510601,132.888879130739));
#79015=CARTESIAN_POINT('Ctrl Pts',(80.2525819664453,-7.35322081020548,132.888117195497));
#79016=CARTESIAN_POINT('Ctrl Pts',(80.3158419436076,-7.36335566787966,132.883692413098));
#79017=CARTESIAN_POINT('Ctrl Pts',(80.3677010739732,-7.37422155243195,132.879921299376));
#79018=CARTESIAN_POINT('Ctrl Pts',(80.5173538371733,-7.41310421819481,132.868770245084));
#79019=CARTESIAN_POINT('Ctrl Pts',(80.6132187608485,-7.44762834092024,132.861298328387));
#79020=CARTESIAN_POINT('Ctrl Pts',(80.7709996605853,-7.52136256312843,132.848816183098));
#79021=CARTESIAN_POINT('Ctrl Pts',(80.8345968220762,-7.55630339480565,132.843723893006));
#79022=CARTESIAN_POINT('Ctrl Pts',(80.910562799522,-7.60474334819562,132.837575563113));
#79023=CARTESIAN_POINT('Ctrl Pts',(80.9252516028103,-7.61444045633709,132.836383185083));
#79024=CARTESIAN_POINT('Ctrl Pts',(80.9486446301411,-7.63042177810377,132.834477803156));
#79025=CARTESIAN_POINT('Ctrl Pts',(80.9574462568691,-7.6365603003019,132.833759398177));
#79026=CARTESIAN_POINT('Ctrl Pts',(80.974167790149,-7.64846418437229,132.832391397068));
#79027=CARTESIAN_POINT('Ctrl Pts',(80.9820973253557,-7.65421517514561,132.831741290156));
#79028=CARTESIAN_POINT('Ctrl Pts',(81.0000926800359,-7.66751028188434,132.830262459357));
#79029=CARTESIAN_POINT('Ctrl Pts',(81.010124784145,-7.67509919147521,132.829435514994));
#79030=CARTESIAN_POINT('Ctrl Pts',(81.0366998609108,-7.6956795651641,132.827237294747));
#79031=CARTESIAN_POINT('Ctrl Pts',(81.0530846964875,-7.70887216597268,132.825873941988));
#79032=CARTESIAN_POINT('Ctrl Pts',(81.1614825713486,-7.79958772097864,132.816787169467));
#79033=CARTESIAN_POINT('Ctrl Pts',(81.2451155205109,-7.8865716972318,132.809477672488));
#79034=CARTESIAN_POINT('Ctrl Pts',(81.3593481732068,-8.03451473641377,132.79805701234));
#79035=CARTESIAN_POINT('Ctrl Pts',(81.396841794092,-8.08960394667465,132.79397828883));
#79036=CARTESIAN_POINT('Ctrl Pts',(81.4424673892459,-8.16612302913608,132.788340328566));
#79037=CARTESIAN_POINT('Ctrl Pts',(81.4536048178128,-8.18569299163068,132.78690046957));
#79038=CARTESIAN_POINT('Ctrl Pts',(81.4719891491043,-8.21957633963112,132.784400539124));
#79039=CARTESIAN_POINT('Ctrl Pts',(81.4794323780598,-8.23378009873849,132.783350533682));
#79040=CARTESIAN_POINT('Ctrl Pts',(81.4899337485244,-8.25454326224539,132.781809438179));
#79041=CARTESIAN_POINT('Ctrl Pts',(81.4931562564454,-8.26101913972246,132.781327919972));
#79042=CARTESIAN_POINT('Ctrl Pts',(81.4987268566032,-8.27239889389514,132.780479905602));
#79043=CARTESIAN_POINT('Ctrl Pts',(81.5010932703707,-8.27729359159184,132.780114543085));
#79044=CARTESIAN_POINT('Ctrl Pts',(81.5061944370699,-8.28797800974474,132.77931558338));
#79045=CARTESIAN_POINT('Ctrl Pts',(81.5089197422572,-8.29377184646675,132.778881456882));
#79046=CARTESIAN_POINT('Ctrl Pts',(81.5164321597137,-8.30998479734562,132.777664495741));
#79047=CARTESIAN_POINT('Ctrl Pts',(81.5211450968081,-8.32043760316743,132.776877444629));
#79048=CARTESIAN_POINT('Ctrl Pts',(81.5519978182549,-8.39079508451345,132.771567455939));
#79049=CARTESIAN_POINT('Ctrl Pts',(81.5746980614344,-8.45213873188183,132.766880069889));
#79050=CARTESIAN_POINT('Ctrl Pts',(81.5999803136546,-8.53515745502293,132.760590050769));
#79051=CARTESIAN_POINT('Ctrl Pts',(81.6058293379807,-8.55578415835092,132.759031289682));
#79052=CARTESIAN_POINT('Ctrl Pts',(81.62874740918,-8.64298355937333,132.752469936565));
#79053=CARTESIAN_POINT('Ctrl Pts',(81.6420877587951,-8.71047005477192,132.747464313843));
#79054=CARTESIAN_POINT('Ctrl Pts',(81.6606685882657,-8.84904153065469,132.737451629434));
#79055=CARTESIAN_POINT('Ctrl Pts',(81.665597880524,-8.92003264419149,132.732460942705));
#79056=CARTESIAN_POINT('Ctrl Pts',(81.6660696298094,-9.00864433451294,132.726414619291));
#79057=CARTESIAN_POINT('Ctrl Pts',(81.6658866973958,-9.02615889899833,132.725228151296));
#79058=CARTESIAN_POINT('Ctrl Pts',(81.6651468317012,-9.05437624418066,132.723329877337));
#79059=CARTESIAN_POINT('Ctrl Pts',(81.6647627797226,-9.06508182215686,132.72261274267));
#79060=CARTESIAN_POINT('Ctrl Pts',(81.6638296949817,-9.08557331172566,132.721245690273));
#79061=CARTESIAN_POINT('Ctrl Pts',(81.6632975133836,-9.09535950165407,132.720595275641));
#79062=CARTESIAN_POINT('Ctrl Pts',(81.661882833037,-9.11773106072618,132.719113731521));
#79063=CARTESIAN_POINT('Ctrl Pts',(81.660943665876,-9.13031234301575,132.718284404982));
#79064=CARTESIAN_POINT('Ctrl Pts',(81.6575690410271,-9.16951538422329,132.715711295771));
#79065=CARTESIAN_POINT('Ctrl Pts',(81.654635644927,-9.19609080034345,132.71398301054));
#79066=CARTESIAN_POINT('Ctrl Pts',(81.6333961878039,-9.35363799821407,132.70380948757));
#79067=CARTESIAN_POINT('Ctrl Pts',(81.6001896077223,-9.48211904785678,132.695857850917));
#79068=CARTESIAN_POINT('Ctrl Pts',(81.526068531088,-9.67217472149256,132.683343587908));
#79069=CARTESIAN_POINT('Ctrl Pts',(81.4957106024904,-9.73725941700626,132.67889705109));
#79070=CARTESIAN_POINT('Ctrl Pts',(81.4536619545557,-9.81404729330117,132.673217355844));
#79071=CARTESIAN_POINT('Ctrl Pts',(81.4458698862522,-9.8278081307099,132.672181575324));
#79072=CARTESIAN_POINT('Ctrl Pts',(81.4342502574912,-9.84766381558653,132.67065760297));
#79073=CARTESIAN_POINT('Ctrl Pts',(81.4305769479412,-9.85384854431348,132.670178688358));
#79074=CARTESIAN_POINT('Ctrl Pts',(81.4240592521183,-9.8646622247977,132.669333537986));
#79075=CARTESIAN_POINT('Ctrl Pts',(81.421232103019,-9.86930134281507,132.668968409527));
#79076=CARTESIAN_POINT('Ctrl Pts',(81.4150095455925,-9.87940054833436,132.668167849903));
#79077=CARTESIAN_POINT('Ctrl Pts',(81.4116052587202,-9.88485474999599,132.66773187012));
#79078=CARTESIAN_POINT('Ctrl Pts',(81.4019783332577,-9.90008165213583,132.666504811552));
#79079=CARTESIAN_POINT('Ctrl Pts',(81.3956853393783,-9.90980912402503,132.66570940825));
#79080=CARTESIAN_POINT('Ctrl Pts',(81.3497800994107,-9.97917057965944,132.659958986398));
#79081=CARTESIAN_POINT('Ctrl Pts',(81.306465701874,-10.0362559502864,132.654807202752));
#79082=CARTESIAN_POINT('Ctrl Pts',(81.2505036866459,-10.1009044360093,132.64859897745));
#79083=CARTESIAN_POINT('Ctrl Pts',(81.2412549610045,-10.1113218097621,132.647585963284));
#79084=CARTESIAN_POINT('Ctrl Pts',(81.1872493633575,-10.1706361286461,132.641748751946));
#79085=CARTESIAN_POINT('Ctrl Pts',(81.1397343722851,-10.2169454933137,132.636918942927));
#79086=CARTESIAN_POINT('Ctrl Pts',(81.0522763581015,-10.2925566698174,132.628625216851));
#79087=CARTESIAN_POINT('Ctrl Pts',(81.0135515415972,-10.3231410746955,132.625131381835));
#79088=CARTESIAN_POINT('Ctrl Pts',(80.9463433485087,-10.3715363970818,132.619368298839));
#79089=CARTESIAN_POINT('Ctrl Pts',(80.9185775920956,-10.390285333292,132.617066968719));
#79090=CARTESIAN_POINT('Ctrl Pts',(80.8786826620773,-10.4155071540131,132.613868131652));
#79091=CARTESIAN_POINT('Ctrl Pts',(80.8670115371286,-10.4226857480351,132.612944840979));
#79092=CARTESIAN_POINT('Ctrl Pts',(80.8467255689278,-10.4348207365521,132.611361061483));
#79093=CARTESIAN_POINT('Ctrl Pts',(80.8381526449522,-10.439845438317,132.61069810958));
#79094=CARTESIAN_POINT('Ctrl Pts',(80.820533788081,-10.4499613913401,132.609348321176));
#79095=CARTESIAN_POINT('Ctrl Pts',(80.8114841907148,-10.4550454117424,132.608661766522));
#79096=CARTESIAN_POINT('Ctrl Pts',(80.788406512914,-10.4677280652419,132.60692756251));
#79097=CARTESIAN_POINT('Ctrl Pts',(80.774315510965,-10.4752105007322,132.605884059613));
#79098=CARTESIAN_POINT('Ctrl Pts',(80.7181887881325,-10.5039884274052,132.601785206916));
#79099=CARTESIAN_POINT('Ctrl Pts',(80.6753630391188,-10.5237000079728,132.598784609546));
#79100=CARTESIAN_POINT('Ctrl Pts',(80.5279728255844,-10.5841024462646,132.58879214491));
#79101=CARTESIAN_POINT('Ctrl Pts',(80.4201624656764,-10.6160444892451,132.58205231361));
#79102=CARTESIAN_POINT('Ctrl Pts',(80.2462147002532,-10.6489825153716,132.57115911966));
#79103=CARTESIAN_POINT('Ctrl Pts',(80.1818266400267,-10.6573177808013,132.567116903301));
#79104=CARTESIAN_POINT('Ctrl Pts',(80.1020555385948,-10.6629398275944,132.561922041275));
#79105=CARTESIAN_POINT('Ctrl Pts',(80.0869734191753,-10.6637967989842,132.560931619842));
#79106=CARTESIAN_POINT('Ctrl Pts',(80.0648255313732,-10.6647532978196,132.559462371492));
#79107=CARTESIAN_POINT('Ctrl Pts',(80.0577669669406,-10.665013172659,132.558991911758));
#79108=CARTESIAN_POINT('Ctrl Pts',(80.0457584732086,-10.6653788379769,132.558187454295));
#79109=CARTESIAN_POINT('Ctrl Pts',(80.0408093794307,-10.6655074618602,132.557854723654));
#79110=CARTESIAN_POINT('Ctrl Pts',(80.02953766703,-10.6657501350732,132.557094137516));
#79111=CARTESIAN_POINT('Ctrl Pts',(80.0232150695413,-10.6658502464163,132.556665540036));
#79112=CARTESIAN_POINT('Ctrl Pts',(80.0057803210671,-10.6660270328463,132.555478532953));
#79113=CARTESIAN_POINT('Ctrl Pts',(79.9946679747136,-10.6660285229165,132.554716220296));
#79114=CARTESIAN_POINT('Ctrl Pts',(79.9304589107186,-10.6653947580465,132.550281336751));
#79115=CARTESIAN_POINT('Ctrl Pts',(79.8774216670898,-10.6623324111577,132.546499926768));
#79116=CARTESIAN_POINT('Ctrl Pts',(79.7243947393697,-10.6461339093797,132.535401447877));
#79117=CARTESIAN_POINT('Ctrl Pts',(79.6253248774927,-10.6264486999272,132.527995105171));
#79118=CARTESIAN_POINT('Ctrl Pts',(79.4584982207439,-10.5772381492018,132.515524753495));
#79119=CARTESIAN_POINT('Ctrl Pts',(79.3897847196958,-10.551948559544,132.510384861366));
#79120=CARTESIAN_POINT('Ctrl Pts',(79.3068310585781,-10.5150524504498,132.504188854034));
#79121=CARTESIAN_POINT('Ctrl Pts',(79.2908293375031,-10.5076286419254,132.5029937815));
#79122=CARTESIAN_POINT('Ctrl Pts',(79.2652795958838,-10.4952783177129,132.501085159112));
#79123=CARTESIAN_POINT('Ctrl Pts',(79.2556564327779,-10.4905113159321,132.500366175053));
#79124=CARTESIAN_POINT('Ctrl Pts',(79.2373471100845,-10.4812199258996,132.49899773735));
#79125=CARTESIAN_POINT('Ctrl Pts',(79.2286534721638,-10.4767113598669,132.498347766625));
#79126=CARTESIAN_POINT('Ctrl Pts',(79.2088999899896,-10.4662450586745,132.496870152935));
#79127=CARTESIAN_POINT('Ctrl Pts',(79.1978666759877,-10.4602383171276,132.496044278973));
#79128=CARTESIAN_POINT('Ctrl Pts',(79.1685955698161,-10.4438706967361,132.49385093017));
#79129=CARTESIAN_POINT('Ctrl Pts',(79.1504833642781,-10.4332890371368,132.492491321604));
#79130=CARTESIAN_POINT('Ctrl Pts',(79.028962818056,-10.3591802558185,132.483340344464));
#79131=CARTESIAN_POINT('Ctrl Pts',(78.9325628869623,-10.2848603187997,132.475971354361));
#79132=CARTESIAN_POINT('Ctrl Pts',(78.7768704876421,-10.1351072236162,132.462770402837));
#79133=CARTESIAN_POINT('Ctrl Pts',(78.714380758827,-10.0638102341602,132.456968930806));
#79134=CARTESIAN_POINT('Ctrl Pts',(78.6512058662437,-9.97798424046067,132.450001529669));
#79135=CARTESIAN_POINT('Ctrl Pts',(78.6442261913598,-9.96828515917442,132.44921427928));
#79136=CARTESIAN_POINT('Ctrl Pts',(78.6336484352558,-9.95324751895324,132.447992477885));
#79137=CARTESIAN_POINT('Ctrl Pts',(78.6299757906708,-9.94796154628915,132.447562764113));
#79138=CARTESIAN_POINT('Ctrl Pts',(78.6232309069204,-9.93813268800382,132.4467630501));
#79139=CARTESIAN_POINT('Ctrl Pts',(78.6201503564435,-9.93359575510221,132.446393613512));
#79140=CARTESIAN_POINT('Ctrl Pts',(78.6131370243566,-9.92315621304728,132.445542909355));
#79141=CARTESIAN_POINT('Ctrl Pts',(78.6092194934486,-9.917243634422,132.44506066826));
#79142=CARTESIAN_POINT('Ctrl Pts',(78.5967638951246,-9.89818163016667,132.443505008774));
#79143=CARTESIAN_POINT('Ctrl Pts',(78.5883739415129,-9.88493707881446,132.44242271436));
#79144=CARTESIAN_POINT('Ctrl Pts',(78.5325282458581,-9.79396258240091,132.434989404229));
#79145=CARTESIAN_POINT('Ctrl Pts',(78.4913326360921,-9.71257960117055,132.428352487438));
#79146=CARTESIAN_POINT('Ctrl Pts',(78.4247981823295,-9.54916801018671,132.415509565079));
#79147=CARTESIAN_POINT('Ctrl Pts',(78.3987241090773,-9.46772274949642,132.409321320066));
#79148=CARTESIAN_POINT('Ctrl Pts',(78.3680020106449,-9.33824711606812,132.399941795619));
#79149=CARTESIAN_POINT('Ctrl Pts',(78.3589911515499,-9.29140914651757,132.396636443554));
#79150=CARTESIAN_POINT('Ctrl Pts',(78.3497214859849,-9.22886371949396,132.392336222087));
#79151=CARTESIAN_POINT('Ctrl Pts',(78.3476572751646,-9.21345098753675,132.39128549454));
#79152=CARTESIAN_POINT('Ctrl Pts',(78.344585459482,-9.18778894981642,132.389550366783));
#79153=CARTESIAN_POINT('Ctrl Pts',(78.3434565908137,-9.17755543451907,132.388862199855));
#79154=CARTESIAN_POINT('Ctrl Pts',(78.3414309101958,-9.15748679548525,132.387519785941));
#79155=CARTESIAN_POINT('Ctrl Pts',(78.3405265443351,-9.14765288175546,132.386865328795));
#79156=CARTESIAN_POINT('Ctrl Pts',(78.3385587769912,-9.12394608464232,132.385295347423));
#79157=CARTESIAN_POINT('Ctrl Pts',(78.3375816037598,-9.11006663726376,132.384382550121));
#79158=CARTESIAN_POINT('Ctrl Pts',(78.3349117758727,-9.06389602089076,132.381365763054));
#79159=CARTESIAN_POINT('Ctrl Pts',(78.3339852172248,-9.0315667646501,132.379285475395));
#79160=CARTESIAN_POINT('Ctrl Pts',(78.3340225505802,-8.95087241551319,132.374154817107));
#79161=CARTESIAN_POINT('Ctrl Pts',(78.3361502746032,-8.90253721712625,132.371137437581));
#79162=CARTESIAN_POINT('Ctrl Pts',(78.3493322717099,-8.75232329209449,132.361827850156));
#79163=CARTESIAN_POINT('Ctrl Pts',(78.3676768928935,-8.65133468893829,132.355677451397));
#79164=CARTESIAN_POINT('Ctrl Pts',(78.4072397004561,-8.50939955348026,132.346514706518));
#79165=CARTESIAN_POINT('Ctrl Pts',(78.4210455134462,-8.46663741954607,132.343680790756));
#79166=CARTESIAN_POINT('Ctrl Pts',(78.4365593746692,-8.42449204083248,132.34076576841));
#79167=CARTESIAN_POINT('Ctrl Pts',(78.4365593757978,-8.42449203776637,132.531716974833));
#79168=CARTESIAN_POINT('Ctrl Pts',(78.4158152968604,-8.48084596829506,132.535390123933));
#79169=CARTESIAN_POINT('Ctrl Pts',(78.3981331141248,-8.53828076475871,132.539081327909));
#79170=CARTESIAN_POINT('Ctrl Pts',(78.3781664810635,-8.61827538701239,132.544300119671));
#79171=CARTESIAN_POINT('Ctrl Pts',(78.3731815364889,-8.64011219783514,132.545732647857));
#79172=CARTESIAN_POINT('Ctrl Pts',(78.3653986161774,-8.67768120417352,132.548221013902));
#79173=CARTESIAN_POINT('Ctrl Pts',(78.3623839019968,-8.69336575563498,132.549266907653));
#79174=CARTESIAN_POINT('Ctrl Pts',(78.3583344181542,-8.71620032307511,132.550802978582));
#79175=CARTESIAN_POINT('Ctrl Pts',(78.3571198281678,-8.72331809703613,132.551283668714));
#79176=CARTESIAN_POINT('Ctrl Pts',(78.3550723073871,-8.7358060977931,132.552130681393));
#79177=CARTESIAN_POINT('Ctrl Pts',(78.3542193237079,-8.74117284490548,132.552495877947));
#79178=CARTESIAN_POINT('Ctrl Pts',(78.3524177218992,-8.75287715876222,132.553295022104));
#79179=CARTESIAN_POINT('Ctrl Pts',(78.3514794203367,-8.75921595413856,132.553729503724));
#79180=CARTESIAN_POINT('Ctrl Pts',(78.3489603439765,-8.77693911718939,132.554948709072));
#79181=CARTESIAN_POINT('Ctrl Pts',(78.3474608138544,-8.78833440724614,132.55573767454));
#79182=CARTESIAN_POINT('Ctrl Pts',(78.3380833665429,-8.8657830019875,132.561130179634));
#79183=CARTESIAN_POINT('Ctrl Pts',(78.3340507255463,-8.9322346958779,132.56590397706));
#79184=CARTESIAN_POINT('Ctrl Pts',(78.3338866236568,-9.14942545685867,132.58165164396));
#79185=CARTESIAN_POINT('Ctrl Pts',(78.3542177057676,-9.2994673582841,132.592678401743));
#79186=CARTESIAN_POINT('Ctrl Pts',(78.3999680512033,-9.46462843896716,132.604461614973));
#79187=CARTESIAN_POINT('Ctrl Pts',(78.40584594122,-9.48441173241258,132.605868756683));
#79188=CARTESIAN_POINT('Ctrl Pts',(78.4158613430934,-9.51596130427402,132.608106753117));
#79189=CARTESIAN_POINT('Ctrl Pts',(78.4197658645175,-9.52779867707683,132.608945070794));
#79190=CARTESIAN_POINT('Ctrl Pts',(78.426969745976,-9.54884188980903,132.610433213838));
#79191=CARTESIAN_POINT('Ctrl Pts',(78.4302179651041,-9.55806448552675,132.611084685801));
#79192=CARTESIAN_POINT('Ctrl Pts',(78.4372192182297,-9.57739806893125,132.612449075184));
#79193=CARTESIAN_POINT('Ctrl Pts',(78.4409896286756,-9.58750231761332,132.613161381381));
#79194=CARTESIAN_POINT('Ctrl Pts',(78.451264013806,-9.61424084701655,132.615044795323));
#79195=CARTESIAN_POINT('Ctrl Pts',(78.4579379224952,-9.63080865745263,132.616210196466));
#79196=CARTESIAN_POINT('Ctrl Pts',(78.4948473974399,-9.71834691112663,132.62236458341));
#79197=CARTESIAN_POINT('Ctrl Pts',(78.5297201404637,-9.78726487106699,132.627192788968));
#79198=CARTESIAN_POINT('Ctrl Pts',(78.6205084632086,-9.93945208313728,132.638110963633));
#79199=CARTESIAN_POINT('Ctrl Pts',(78.679402675396,-10.0205822827333,132.644123620688));
#79200=CARTESIAN_POINT('Ctrl Pts',(78.7779661704362,-10.1334319031237,132.653456651628));
#79201=CARTESIAN_POINT('Ctrl Pts',(78.8123770773947,-10.1694380403403,132.656609753309));
#79202=CARTESIAN_POINT('Ctrl Pts',(78.8562259004477,-10.2113858928923,132.660585351344));
#79203=CARTESIAN_POINT('Ctrl Pts',(78.8641811817914,-10.2188480499981,132.661305043859));
#79204=CARTESIAN_POINT('Ctrl Pts',(78.8768283138518,-10.2304798872114,132.662447838725));
#79205=CARTESIAN_POINT('Ctrl Pts',(78.8814716054946,-10.2347022381293,132.662867124056));
#79206=CARTESIAN_POINT('Ctrl Pts',(78.8902376889261,-10.24258359811,132.663658418623));
#79207=CARTESIAN_POINT('Ctrl Pts',(78.8943549179573,-10.2462485042515,132.664029982204));
#79208=CARTESIAN_POINT('Ctrl Pts',(78.9040963971883,-10.2548335080476,132.664908818345));
#79209=CARTESIAN_POINT('Ctrl Pts',(78.9097356442377,-10.2597362695311,132.665417322477));
#79210=CARTESIAN_POINT('Ctrl Pts',(78.9286252058328,-10.2759370151046,132.667119270985));
#79211=CARTESIAN_POINT('Ctrl Pts',(78.9420191451869,-10.2870647486891,132.668323840663));
#79212=CARTESIAN_POINT('Ctrl Pts',(78.9751817009875,-10.3137488990789,132.671295909271));
#79213=CARTESIAN_POINT('Ctrl Pts',(78.9951326397183,-10.3290711672589,132.673075168257));
#79214=CARTESIAN_POINT('Ctrl Pts',(79.081288061803,-10.3921893680708,132.680697551053));
#79215=CARTESIAN_POINT('Ctrl Pts',(79.150610370743,-10.4355345063037,132.686675298426));
#79216=CARTESIAN_POINT('Ctrl Pts',(79.3108758938014,-10.5200567631612,132.699835811052));
#79217=CARTESIAN_POINT('Ctrl Pts',(79.4029201945575,-10.558514106641,132.706962339044));
#79218=CARTESIAN_POINT('Ctrl Pts',(79.5204474213307,-10.595664884564,132.715448553096));
#79219=CARTESIAN_POINT('Ctrl Pts',(79.5431840538902,-10.6023221869954,132.717064097743));
#79220=CARTESIAN_POINT('Ctrl Pts',(79.5777816762202,-10.6116560383882,132.719484247576));
#79221=CARTESIAN_POINT('Ctrl Pts',(79.5895418734781,-10.6146911899588,132.720300307338));
#79222=CARTESIAN_POINT('Ctrl Pts',(79.6107742212711,-10.6199240149705,132.721762162006));
#79223=CARTESIAN_POINT('Ctrl Pts',(79.6202343090276,-10.6221678544288,132.722409414242));
#79224=CARTESIAN_POINT('Ctrl Pts',(79.6405345976397,-10.6267955624123,132.723789876356));
#79225=CARTESIAN_POINT('Ctrl Pts',(79.6513801166758,-10.6291541867961,132.724522251137));
#79226=CARTESIAN_POINT('Ctrl Pts',(79.6811777265671,-10.6353232178694,132.726520909046));
#79227=CARTESIAN_POINT('Ctrl Pts',(79.7001742110378,-10.6389125100781,132.727780153089));
#79228=CARTESIAN_POINT('Ctrl Pts',(79.7426115828233,-10.6461682494264,132.730563058112));
#79229=CARTESIAN_POINT('Ctrl Pts',(79.7660771718582,-10.6496662987064,132.732081485437));
#79230=CARTESIAN_POINT('Ctrl Pts',(79.8413897075775,-10.659253845929,132.736899769277));
#79231=CARTESIAN_POINT('Ctrl Pts',(79.893452634329,-10.6634087961407,132.740146515545));
#79232=CARTESIAN_POINT('Ctrl Pts',(80.0433753531649,-10.6683043262529,132.749382744675));
#79233=CARTESIAN_POINT('Ctrl Pts',(80.1412090102354,-10.6628828131774,132.75526419388));
#79234=CARTESIAN_POINT('Ctrl Pts',(80.2879360713108,-10.6417047856632,132.764493801283));
#79235=CARTESIAN_POINT('Ctrl Pts',(80.3375160720623,-10.6322327119384,132.767687695366));
#79236=CARTESIAN_POINT('Ctrl Pts',(80.3972256713105,-10.6179887037877,132.771709025876));
#79237=CARTESIAN_POINT('Ctrl Pts',(80.4078412782409,-10.6153455220601,132.772430811117));
#79238=CARTESIAN_POINT('Ctrl Pts',(80.4245117554956,-10.6110199411952,132.773576203108));
#79239=CARTESIAN_POINT('Ctrl Pts',(80.4305846738193,-10.6094074427887,132.773995964239));
#79240=CARTESIAN_POINT('Ctrl Pts',(80.4419661222363,-10.6063163801216,132.774787611976));
#79241=CARTESIAN_POINT('Ctrl Pts',(80.4472766148384,-10.6048457846498,132.775159047355));
#79242=CARTESIAN_POINT('Ctrl Pts',(80.4597583884856,-10.601322536176,132.77603683814));
#79243=CARTESIAN_POINT('Ctrl Pts',(80.4669232826222,-10.5992480368798,132.776544416275));
#79244=CARTESIAN_POINT('Ctrl Pts',(80.4906918612159,-10.5921928237475,132.778240012906));
#79245=CARTESIAN_POINT('Ctrl Pts',(80.5072310923569,-10.5870012762234,132.779439047536));
#79246=CARTESIAN_POINT('Ctrl Pts',(80.5474189323835,-10.5736942357623,132.782394597509));
#79247=CARTESIAN_POINT('Ctrl Pts',(80.5709712463872,-10.5653027619819,132.784162714937));
#79248=CARTESIAN_POINT('Ctrl Pts',(80.6697101985818,-10.5275980949115,132.791704560633));
#79249=CARTESIAN_POINT('Ctrl Pts',(80.7429019767104,-10.4933732013583,132.797610581001));
#79250=CARTESIAN_POINT('Ctrl Pts',(80.9013573331191,-10.4047369775956,132.810801329379));
#79251=CARTESIAN_POINT('Ctrl Pts',(80.9847498232759,-10.3475922769379,132.818026556118));
#79252=CARTESIAN_POINT('Ctrl Pts',(81.0806643418262,-10.2681792279019,132.826599076604));
#79253=CARTESIAN_POINT('Ctrl Pts',(81.0985371963692,-10.2527290613549,132.828210017449));
#79254=CARTESIAN_POINT('Ctrl Pts',(81.1250830171934,-10.2287763723764,132.830624703444));
#79255=CARTESIAN_POINT('Ctrl Pts',(81.1340009452007,-10.2205511208777,132.831439826067));
#79256=CARTESIAN_POINT('Ctrl Pts',(81.1499018020704,-10.2055605939398,132.832900665503));
#79257=CARTESIAN_POINT('Ctrl Pts',(81.1569167861001,-10.1988302869793,132.833547830998));
#79258=CARTESIAN_POINT('Ctrl Pts',(81.1718204224324,-10.1842788032407,132.834928814232));
#79259=CARTESIAN_POINT('Ctrl Pts',(81.1796906051357,-10.1764393194891,132.835661790403));
#79260=CARTESIAN_POINT('Ctrl Pts',(81.2010713519051,-10.1547116490995,132.837663918047));
#79261=CARTESIAN_POINT('Ctrl Pts',(81.2144192453219,-10.1406653025051,132.838925988465));
#79262=CARTESIAN_POINT('Ctrl Pts',(81.3034428476702,-10.0436488817863,132.84743652416));
#79263=CARTESIAN_POINT('Ctrl Pts',(81.3708096935066,-9.95344185250607,132.854319798004));
#79264=CARTESIAN_POINT('Ctrl Pts',(81.4828880313821,-9.76663934118246,132.867623192274));
#79265=CARTESIAN_POINT('Ctrl Pts',(81.5284536881442,-9.67120483582628,132.874025086864));
#79266=CARTESIAN_POINT('Ctrl Pts',(81.5697578165006,-9.55824251204767,132.881840561365));
#79267=CARTESIAN_POINT('Ctrl Pts',(81.5746466927612,-9.54429960590879,132.882809358926));
#79268=CARTESIAN_POINT('Ctrl Pts',(81.5815856872882,-9.5236335346917,132.884253958279));
#79269=CARTESIAN_POINT('Ctrl Pts',(81.5837798873492,-9.51695902049629,132.884721840826));
#79270=CARTESIAN_POINT('Ctrl Pts',(81.5876091580003,-9.50505757560984,132.88555881122));
#79271=CARTESIAN_POINT('Ctrl Pts',(81.5892607675465,-9.49983617773504,132.885926934036));
#79272=CARTESIAN_POINT('Ctrl Pts',(81.5928108435998,-9.48841746952314,132.886734090532));
#79273=CARTESIAN_POINT('Ctrl Pts',(81.5946988731554,-9.48221728340004,132.887173681521));
#79274=CARTESIAN_POINT('Ctrl Pts',(81.6000271977416,-9.46434579991353,132.888444232073));
#79275=CARTESIAN_POINT('Ctrl Pts',(81.6033757833033,-9.45264791101363,132.889280119208));
#79276=CARTESIAN_POINT('Ctrl Pts',(81.6310851294426,-9.35168120120261,132.89652509023));
#79277=CARTESIAN_POINT('Ctrl Pts',(81.6480949869689,-9.26057178358526,132.903256408156));
#79278=CARTESIAN_POINT('Ctrl Pts',(81.6699287213006,-9.04584574233947,132.918967736365));
#79279=CARTESIAN_POINT('Ctrl Pts',(81.668745261142,-8.92213018775728,132.927880056535));
#79280=CARTESIAN_POINT('Ctrl Pts',(81.6514041694624,-8.77896884929953,132.937797963883));
#79281=CARTESIAN_POINT('Ctrl Pts',(81.6485093423848,-8.75832352879022,132.939219687155));
#79282=CARTESIAN_POINT('Ctrl Pts',(81.6432562627092,-8.72536990308967,132.941476158024));
#79283=CARTESIAN_POINT('Ctrl Pts',(81.6411453937733,-8.71302500731883,132.942318566198));
#79284=CARTESIAN_POINT('Ctrl Pts',(81.6371375406534,-8.69107860761379,132.943811343712));
#79285=CARTESIAN_POINT('Ctrl Pts',(81.6352947993765,-8.68146792964494,132.944463396795));
#79286=CARTESIAN_POINT('Ctrl Pts',(81.6312495242113,-8.66133109774449,132.945826371088));
#79287=CARTESIAN_POINT('Ctrl Pts',(81.6290295289294,-8.65080887952893,132.946536704153));
#79288=CARTESIAN_POINT('Ctrl Pts',(81.6228829379358,-8.62301085719126,132.948408812287));
#79289=CARTESIAN_POINT('Ctrl Pts',(81.6187823319621,-8.60577462670225,132.949565005195));
#79290=CARTESIAN_POINT('Ctrl Pts',(81.596005957803,-8.51639462779842,132.955541616139));
#79291=CARTESIAN_POINT('Ctrl Pts',(81.5727790716396,-8.44549373641885,132.960212859109));
#79292=CARTESIAN_POINT('Ctrl Pts',(81.5202038506543,-8.31525051526367,132.968876971414));
#79293=CARTESIAN_POINT('Ctrl Pts',(81.4919216806215,-8.25564024213442,132.972879261933));
#79294=CARTESIAN_POINT('Ctrl Pts',(81.453052511677,-8.18488427490483,132.977821225375));
#79295=CARTESIAN_POINT('Ctrl Pts',(81.4457506773648,-8.17200228397415,132.978729230212));
#79296=CARTESIAN_POINT('Ctrl Pts',(81.4025542259513,-8.09810843123554,132.983994794105));
#79297=CARTESIAN_POINT('Ctrl Pts',(81.3629760745773,-8.03934373853891,132.988407911037));
#79298=CARTESIAN_POINT('Ctrl Pts',(81.3127238305807,-7.9741120342173,132.993794268414));
#79299=CARTESIAN_POINT('Ctrl Pts',(81.3055649526431,-7.9650168553237,132.994557070523));
#79300=CARTESIAN_POINT('Ctrl Pts',(81.2942852564308,-7.95098952877681,132.99575331608));
#79301=CARTESIAN_POINT('Ctrl Pts',(81.2902295199812,-7.94600518214882,132.996182335017));
#79302=CARTESIAN_POINT('Ctrl Pts',(81.2826926133445,-7.93685129790907,132.996977838491));
#79303=CARTESIAN_POINT('Ctrl Pts',(81.2792197636935,-7.93267516839633,132.997343737002));
#79304=CARTESIAN_POINT('Ctrl Pts',(81.2710999887562,-7.92300762888036,132.998197679754));
#79305=CARTESIAN_POINT('Ctrl Pts',(81.2664378755928,-7.91752928384904,132.998686797546));
#79306=CARTESIAN_POINT('Ctrl Pts',(81.2514089112804,-7.9000990697772,133.000259286629));
#79307=CARTESIAN_POINT('Ctrl Pts',(81.2409075799827,-7.88826502619166,133.001351665555));
#79308=CARTESIAN_POINT('Ctrl Pts',(81.1817937264921,-7.82353019701535,133.007457531567));
#79309=CARTESIAN_POINT('Ctrl Pts',(81.1299711988407,-7.77367187492198,133.012648321675));
#79310=CARTESIAN_POINT('Ctrl Pts',(80.9738691934974,-7.64180453156737,133.027504891379));
#79311=CARTESIAN_POINT('Ctrl Pts',(80.8627775051936,-7.56865679934544,133.037153419174));
#79312=CARTESIAN_POINT('Ctrl Pts',(80.7225627058335,-7.49865302733902,133.047980017715));
#79313=CARTESIAN_POINT('Ctrl Pts',(80.700715915299,-7.48833306982371,133.049633197859));
#79314=CARTESIAN_POINT('Ctrl Pts',(80.6674859339321,-7.47351121929718,133.052098572088));
#79315=CARTESIAN_POINT('Ctrl Pts',(80.6562657614842,-7.46865394709259,133.052922742239));
#79316=CARTESIAN_POINT('Ctrl Pts',(80.6366176807033,-7.46040380629872,133.054351926406));
#79317=CARTESIAN_POINT('Ctrl Pts',(80.6282137286017,-7.45695559756736,133.054958794181));
#79318=CARTESIAN_POINT('Ctrl Pts',(80.610512616879,-7.44986127581422,133.056227947113));
#79319=CARTESIAN_POINT('Ctrl Pts',(80.6012100040343,-7.44622966368224,133.056889723907));
#79320=CARTESIAN_POINT('Ctrl Pts',(80.5787978814287,-7.43771170102919,133.058471955769));
#79321=CARTESIAN_POINT('Ctrl Pts',(80.5656582357957,-7.43290635358832,133.059389684776));
#79322=CARTESIAN_POINT('Ctrl Pts',(80.5190371530316,-7.41651918778691,133.062612715534));
#79323=CARTESIAN_POINT('Ctrl Pts',(80.4852471041173,-7.40583985045085,133.06488849212));
#79324=CARTESIAN_POINT('Ctrl Pts',(80.399684714473,-7.38177093524388,133.07052624976));
#79325=CARTESIAN_POINT('Ctrl Pts',(80.3475600776867,-7.36978043965928,133.073847758025));
#79326=CARTESIAN_POINT('Ctrl Pts',(80.1997407208815,-7.3431907309335,133.08308835023));
#79327=CARTESIAN_POINT('Ctrl Pts',(80.1032298667384,-7.33439039792309,133.088908042074));
#79328=CARTESIAN_POINT('Ctrl Pts',(79.996351570097,-7.33397305178477,133.09556666818));
#79329=CARTESIAN_POINT('Ctrl Pts',(79.9861976747816,-7.33402623287396,133.096201508343));
#79330=CARTESIAN_POINT('Ctrl Pts',(79.9356214334154,-7.33475352949348,133.099377492607));
#79331=CARTESIAN_POINT('Ctrl Pts',(79.8952359291423,-7.33680599233644,133.101957553004));
#79332=CARTESIAN_POINT('Ctrl Pts',(79.8445503188952,-7.34123516684255,133.10529549855));
#79333=CARTESIAN_POINT('Ctrl Pts',(79.8341409004791,-7.34224364867037,133.105986353036));
#79334=CARTESIAN_POINT('Ctrl Pts',(79.8176609755389,-7.34399701764252,133.107089538914));
#79335=CARTESIAN_POINT('Ctrl Pts',(79.8115836845716,-7.34467746753537,133.107498399673));
#79336=CARTESIAN_POINT('Ctrl Pts',(79.7999869807061,-7.34604059245775,133.108282722863));
#79337=CARTESIAN_POINT('Ctrl Pts',(79.7944670607851,-7.34671746613816,133.108657866207));
#79338=CARTESIAN_POINT('Ctrl Pts',(79.7812096785281,-7.34841055437289,133.10956309663));
#79339=CARTESIAN_POINT('Ctrl Pts',(79.7734758308322,-7.34945351583315,133.110094635323));
#79340=CARTESIAN_POINT('Ctrl Pts',(79.7464936842369,-7.35328544547661,133.111960526385));
#79341=CARTESIAN_POINT('Ctrl Pts',(79.7272879575286,-7.35635699230105,133.113309011756));
#79342=CARTESIAN_POINT('Ctrl Pts',(79.6793318054228,-7.36489016132777,133.116720128808));
#79343=CARTESIAN_POINT('Ctrl Pts',(79.6506638199184,-7.37077432188388,133.118799111772));
#79344=CARTESIAN_POINT('Ctrl Pts',(79.512140613932,-7.40303051728754,133.128995819326));
#79345=CARTESIAN_POINT('Ctrl Pts',(79.4050039016121,-7.43977567209337,133.137323087963));
#79346=CARTESIAN_POINT('Ctrl Pts',(79.2374776266775,-7.51702070433264,133.150543957348));
#79347=CARTESIAN_POINT('Ctrl Pts',(79.1745369284178,-7.55111036764585,133.155568501978));
#79348=CARTESIAN_POINT('Ctrl Pts',(79.0986876842548,-7.59874415685813,133.161684964036));
#79349=CARTESIAN_POINT('Ctrl Pts',(79.0835579239352,-7.60859215390399,133.162908572599));
#79350=CARTESIAN_POINT('Ctrl Pts',(79.0596151996061,-7.62473652923424,133.164851375605));
#79351=CARTESIAN_POINT('Ctrl Pts',(79.0506987498941,-7.63087607100305,133.16557636095));
#79352=CARTESIAN_POINT('Ctrl Pts',(79.0340463431707,-7.64258320490658,133.166933392714));
#79353=CARTESIAN_POINT('Ctrl Pts',(79.026297134487,-7.648131086651,133.167566152538));
#79354=CARTESIAN_POINT('Ctrl Pts',(79.0181373382699,-7.65407948399196,133.168233908238));
#79355=CARTESIAN_POINT('Ctrl Pts',(79.0176790286989,-7.65441394505793,133.168271418884));
#79356=CARTESIAN_POINT('Ctrl Pts',(79.0168042104152,-7.65505304728113,133.168343028467));
#79357=CARTESIAN_POINT('Ctrl Pts',(79.0163876722894,-7.65535764789969,133.16837712895));
#79358=CARTESIAN_POINT('Ctrl Pts',(79.0155836537838,-7.65594617367591,133.168442959062));
#79359=CARTESIAN_POINT('Ctrl Pts',(79.0151961546095,-7.65623007294442,133.168474689675));
#79360=CARTESIAN_POINT('Ctrl Pts',(79.0144410161087,-7.65678382333709,133.1685365317));
#79361=CARTESIAN_POINT('Ctrl Pts',(79.0140733647186,-7.65705365787708,133.168566643743));
#79362=CARTESIAN_POINT('Ctrl Pts',(79.0133508791919,-7.65758437644078,133.16862582447));
#79363=CARTESIAN_POINT('Ctrl Pts',(79.0129960376394,-7.65784525025894,133.168654893542));
#79364=CARTESIAN_POINT('Ctrl Pts',(79.0122934669367,-7.65836219826909,133.168712455094));
#79365=CARTESIAN_POINT('Ctrl Pts',(79.0119457338286,-7.65861826701337,133.16874094778));
#79366=CARTESIAN_POINT('Ctrl Pts',(79.0112524962273,-7.65912917918932,133.168797756442));
#79367=CARTESIAN_POINT('Ctrl Pts',(79.0109069905987,-7.65938402102904,133.168826072476));
#79368=CARTESIAN_POINT('Ctrl Pts',(79.010213794509,-7.65989573006845,133.168882889498));
#79369=CARTESIAN_POINT('Ctrl Pts',(79.0098661054437,-7.66015259909183,133.168911390412));
#79370=CARTESIAN_POINT('Ctrl Pts',(79.0091643422305,-7.66067147670592,133.16896892168));
#79371=CARTESIAN_POINT('Ctrl Pts',(79.0088102719173,-7.66093349046409,133.168997951835));
#79372=CARTESIAN_POINT('Ctrl Pts',(79.0001405132159,-7.66735447687778,133.169708860074));
#79373=CARTESIAN_POINT('Ctrl Pts',(78.9918821330406,-7.67359076529657,133.170387756767));
#79374=CARTESIAN_POINT('Ctrl Pts',(78.9720939428277,-7.68882532764748,133.17201910786));
#79375=CARTESIAN_POINT('Ctrl Pts',(78.960623345634,-7.69789936038672,133.172968600568));
#79376=CARTESIAN_POINT('Ctrl Pts',(78.8635035999248,-7.77682901625709,133.181046251922));
#79377=CARTESIAN_POINT('Ctrl Pts',(78.7848792030455,-7.85489874582346,133.187820102659));
#79378=CARTESIAN_POINT('Ctrl Pts',(78.6473993478902,-8.02164764340797,133.201017862272));
#79379=CARTESIAN_POINT('Ctrl Pts',(78.5881436278529,-8.10929395911782,133.207422190819));
#79380=CARTESIAN_POINT('Ctrl Pts',(78.5305081129846,-8.21490902219319,133.215240360801));
#79381=CARTESIAN_POINT('Ctrl Pts',(78.5236044191713,-8.2279700124642,133.216209038305));
#79382=CARTESIAN_POINT('Ctrl Pts',(78.5136753631901,-8.24737497135535,133.217653491449));
#79383=CARTESIAN_POINT('Ctrl Pts',(78.510514778311,-8.25364945926426,133.218121350122));
#79384=CARTESIAN_POINT('Ctrl Pts',(78.5049612861768,-8.26485019412939,133.218958294643));
#79385=CARTESIAN_POINT('Ctrl Pts',(78.5025528484962,-8.26976851619361,133.219326415699));
#79386=CARTESIAN_POINT('Ctrl Pts',(78.4973468395443,-8.28053388479694,133.220133589179));
#79387=CARTESIAN_POINT('Ctrl Pts',(78.4945591657769,-8.28638532621985,133.220573199109));
#79388=CARTESIAN_POINT('Ctrl Pts',(78.486636108547,-8.30326919173247,133.221843858602));
#79389=CARTESIAN_POINT('Ctrl Pts',(78.4815874937763,-8.31434153801031,133.222679837));
#79390=CARTESIAN_POINT('Ctrl Pts',(78.4622319575474,-8.3580533818118,133.22598786149));
#79391=CARTESIAN_POINT('Ctrl Pts',(78.4488589367769,-8.3910787220815,133.228503759881));
#79392=CARTESIAN_POINT('Ctrl Pts',(78.4365594153165,-8.4244919304089,133.231049000392));
#79393=CARTESIAN_POINT('Origin',(80.,-9.,134.));
#79394=CARTESIAN_POINT('',(78.4365594263723,-8.42449190037431,133.93353979929));
#79395=CARTESIAN_POINT('',(78.4365593580908,-8.42449208586977,133.738116396704));
#79396=CARTESIAN_POINT('',(78.4365593749993,-8.42449203993574,134.));
#79397=CARTESIAN_POINT('',(78.3340006446021,-9.00146554209231,133.077925694822));
#79398=CARTESIAN_POINT('Ctrl Pts',(78.4365593580908,-8.42449208586977,133.738116396704));
#79399=CARTESIAN_POINT('Ctrl Pts',(78.4533138667674,-8.37897632638644,133.734685142075));
#79400=CARTESIAN_POINT('Ctrl Pts',(78.4720530811991,-8.3342000924349,133.731307647191));
#79401=CARTESIAN_POINT('Ctrl Pts',(78.5003899433233,-8.27401843136631,133.726765495222));
#79402=CARTESIAN_POINT('Ctrl Pts',(78.508315955554,-8.25786907107223,133.725546243208));
#79403=CARTESIAN_POINT('Ctrl Pts',(78.5214232395522,-8.23222158195401,133.723608549351));
#79404=CARTESIAN_POINT('Ctrl Pts',(78.526437971788,-8.22264043435211,133.722884372604));
#79405=CARTESIAN_POINT('Ctrl Pts',(78.5361622085575,-8.20449358869406,133.721511911016));
#79406=CARTESIAN_POINT('Ctrl Pts',(78.5408544821735,-8.19591922368459,133.720863053366));
#79407=CARTESIAN_POINT('Ctrl Pts',(78.5517809892182,-8.17636346813049,133.719382049155));
#79408=CARTESIAN_POINT('Ctrl Pts',(78.5580652056686,-8.16541057799479,133.718551728765));
#79409=CARTESIAN_POINT('Ctrl Pts',(78.5782078064762,-8.13121038717511,133.715955433786));
#79410=CARTESIAN_POINT('Ctrl Pts',(78.5925088871898,-8.1082279812748,133.714205462608));
#79411=CARTESIAN_POINT('Ctrl Pts',(78.6587528887146,-8.00733769276167,133.706481469928));
#79412=CARTESIAN_POINT('Ctrl Pts',(78.716649758199,-7.9335399405343,133.700729428705));
#79413=CARTESIAN_POINT('Ctrl Pts',(78.8570283046628,-7.78270480563669,133.688140393348));
#79414=CARTESIAN_POINT('Ctrl Pts',(78.94173087951,-7.70839205729023,133.681349333308));
#79415=CARTESIAN_POINT('Ctrl Pts',(79.0450251742556,-7.63479377606791,133.673099955543));
#79416=CARTESIAN_POINT('Ctrl Pts',(79.0569058825938,-7.62655964717383,133.672151347801));
#79417=CARTESIAN_POINT('Ctrl Pts',(79.0746469987598,-7.6146025869256,133.670732714913));
#79418=CARTESIAN_POINT('Ctrl Pts',(79.0804263238281,-7.61075976920946,133.670270257671));
#79419=CARTESIAN_POINT('Ctrl Pts',(79.090799158767,-7.60395569599645,133.669439327743));
#79420=CARTESIAN_POINT('Ctrl Pts',(79.0953834588731,-7.60098077921779,133.669071766976));
#79421=CARTESIAN_POINT('Ctrl Pts',(79.1055745161043,-7.59443847044575,133.668253887085));
#79422=CARTESIAN_POINT('Ctrl Pts',(79.111187948624,-7.59088208687161,133.667802895745));
#79423=CARTESIAN_POINT('Ctrl Pts',(79.1278103623157,-7.58048981561205,133.666466342105));
#79424=CARTESIAN_POINT('Ctrl Pts',(79.138877701091,-7.57374886917976,133.665575062322));
#79425=CARTESIAN_POINT('Ctrl Pts',(79.1646552465304,-7.55845755486214,133.663497914242));
#79426=CARTESIAN_POINT('Ctrl Pts',(79.1794198870932,-7.55000216985275,133.662307284708));
#79427=CARTESIAN_POINT('Ctrl Pts',(79.2311098041938,-7.52144278988786,133.658142329133));
#79428=CARTESIAN_POINT('Ctrl Pts',(79.2686630154529,-7.50251233089856,133.655122636084));
#79429=CARTESIAN_POINT('Ctrl Pts',(79.4010492882962,-7.44194482434151,133.644584745545));
#79430=CARTESIAN_POINT('Ctrl Pts',(79.4990293222452,-7.40773457687879,133.636987697878));
#79431=CARTESIAN_POINT('Ctrl Pts',(79.659642412605,-7.3679630070081,133.62519617809));
#79432=CARTESIAN_POINT('Ctrl Pts',(79.7205192921871,-7.35644281495842,133.620866630459));
#79433=CARTESIAN_POINT('Ctrl Pts',(79.7991860460248,-7.34605512179524,133.615453062732));
#79434=CARTESIAN_POINT('Ctrl Pts',(79.8165041720785,-7.34404431656801,133.614272198444));
#79435=CARTESIAN_POINT('Ctrl Pts',(79.8444925623591,-7.34123907335018,133.612380664533));
#79436=CARTESIAN_POINT('Ctrl Pts',(79.8551440994919,-7.34027497691531,133.611664734488));
#79437=CARTESIAN_POINT('Ctrl Pts',(79.8755779075552,-7.33862367653564,133.610298569988));
#79438=CARTESIAN_POINT('Ctrl Pts',(79.8853583706529,-7.33792014358867,133.609647851876));
#79439=CARTESIAN_POINT('Ctrl Pts',(79.9079878620645,-7.33649305068916,133.608149323691));
#79440=CARTESIAN_POINT('Ctrl Pts',(79.9208403101122,-7.33583193070292,133.60730349556));
#79441=CARTESIAN_POINT('Ctrl Pts',(79.9621010771884,-7.33418860475422,133.60460388092));
#79442=CARTESIAN_POINT('Ctrl Pts',(79.9905282571934,-7.33378441608296,133.602768023737));
#79443=CARTESIAN_POINT('Ctrl Pts',(80.108613025317,-7.33512789595377,133.595222295321));
#79444=CARTESIAN_POINT('Ctrl Pts',(80.1980481373214,-7.34338441258375,133.589709336541));
#79445=CARTESIAN_POINT('Ctrl Pts',(80.3994318352907,-7.37852618049508,133.577216721648));
#79446=CARTESIAN_POINT('Ctrl Pts',(80.5101149494159,-7.40987479005604,133.570293704643));
#79447=CARTESIAN_POINT('Ctrl Pts',(80.6298696552314,-7.457592218266,133.561904880392));
#79448=CARTESIAN_POINT('Ctrl Pts',(80.6429897545246,-7.46301539031032,133.560972878244));
#79449=CARTESIAN_POINT('Ctrl Pts',(80.6623723378939,-7.4713187489628,133.559574391791));
#79450=CARTESIAN_POINT('Ctrl Pts',(80.6686892332579,-7.47407136916926,133.559115168488));
#79451=CARTESIAN_POINT('Ctrl Pts',(80.6799837145581,-7.47907659704441,133.558287568766));
#79452=CARTESIAN_POINT('Ctrl Pts',(80.6849675398563,-7.48131460891143,133.557920070878));
#79453=CARTESIAN_POINT('Ctrl Pts',(80.6960289018128,-7.4863472947156,133.55709923453));
#79454=CARTESIAN_POINT('Ctrl Pts',(80.7021005901423,-7.48915404432202,133.55664519331));
#79455=CARTESIAN_POINT('Ctrl Pts',(80.7200811974411,-7.49759770140704,133.555290607492));
#79456=CARTESIAN_POINT('Ctrl Pts',(80.7319400008513,-7.50333924825636,133.554384119599));
#79457=CARTESIAN_POINT('Ctrl Pts',(80.8135332625971,-7.54404498544958,133.548062214842));
#79458=CARTESIAN_POINT('Ctrl Pts',(80.880798166495,-7.58372553925565,133.542422279533));
#79459=CARTESIAN_POINT('Ctrl Pts',(81.0596299720167,-7.70690117389728,133.526630021248));
#79460=CARTESIAN_POINT('Ctrl Pts',(81.1639156222914,-7.79990173560627,133.516518126028));
#79461=CARTESIAN_POINT('Ctrl Pts',(81.268077763225,-7.91930347475049,133.505646075288));
#79462=CARTESIAN_POINT('Ctrl Pts',(81.2804743458944,-7.93402078045473,133.504336079165));
#79463=CARTESIAN_POINT('Ctrl Pts',(81.3003063633836,-7.95841080825115,133.502212788022));
#79464=CARTESIAN_POINT('Ctrl Pts',(81.3078951421285,-7.96795591473291,133.5013933793));
#79465=CARTESIAN_POINT('Ctrl Pts',(81.3213490360387,-7.98526487630589,133.499927728057));
#79466=CARTESIAN_POINT('Ctrl Pts',(81.3272521618083,-7.99299833556981,133.499279998614));
#79467=CARTESIAN_POINT('Ctrl Pts',(81.3397273052546,-8.00964182630015,133.497900842285));
#79468=CARTESIAN_POINT('Ctrl Pts',(81.3462789592926,-8.01856658994189,133.497170229755));
#79469=CARTESIAN_POINT('Ctrl Pts',(81.3639433363302,-8.04313904535226,133.495182333228));
#79470=CARTESIAN_POINT('Ctrl Pts',(81.3748756347908,-8.05891480218871,133.493931956197));
#79471=CARTESIAN_POINT('Ctrl Pts',(81.4490298851866,-8.16997368240963,133.485298333208));
#79472=CARTESIAN_POINT('Ctrl Pts',(81.5025702479063,-8.27135852524312,133.478296078032));
#79473=CARTESIAN_POINT('Ctrl Pts',(81.584030613147,-8.4735580082545,133.464984553828));
#79474=CARTESIAN_POINT('Ctrl Pts',(81.6136963320868,-8.57306628377615,133.458691042137));
#79475=CARTESIAN_POINT('Ctrl Pts',(81.6368714642679,-8.68945972023276,133.450981231153));
#79476=CARTESIAN_POINT('Ctrl Pts',(81.6396154513551,-8.70428968812911,133.449992398164));
#79477=CARTESIAN_POINT('Ctrl Pts',(81.6433475588429,-8.72611201604772,133.448525069648));
#79478=CARTESIAN_POINT('Ctrl Pts',(81.6444932392356,-8.73307714878011,133.448054910248));
#79479=CARTESIAN_POINT('Ctrl Pts',(81.646448341435,-8.74545374286702,133.447215891084));
#79480=CARTESIAN_POINT('Ctrl Pts',(81.6472754164775,-8.75086220936775,133.44684802229));
#79481=CARTESIAN_POINT('Ctrl Pts',(81.6490338786682,-8.76275297262645,133.446036486262));
#79482=CARTESIAN_POINT('Ctrl Pts',(81.6499536813191,-8.769236634588,133.445592214764));
#79483=CARTESIAN_POINT('Ctrl Pts',(81.6525161717919,-8.78809855523841,133.444294962084));
#79484=CARTESIAN_POINT('Ctrl Pts',(81.6540579064927,-8.80048975198712,133.443436741255));
#79485=CARTESIAN_POINT('Ctrl Pts',(81.6652741972421,-8.89972967002329,133.436521535527));
#79486=CARTESIAN_POINT('Ctrl Pts',(81.6682400733814,-8.98719112720432,133.430178651183));
#79487=CARTESIAN_POINT('Ctrl Pts',(81.6585796053075,-9.2030909417412,133.414448977104));
#79488=CARTESIAN_POINT('Ctrl Pts',(81.6379329755294,-9.33063558207947,133.405126136297));
#79489=CARTESIAN_POINT('Ctrl Pts',(81.5972277975585,-9.47416812168722,133.394871923007));
#79490=CARTESIAN_POINT('Ctrl Pts',(81.5913026016324,-9.49368830132768,133.393481387875));
#79491=CARTESIAN_POINT('Ctrl Pts',(81.5811606216304,-9.52501822420807,133.391255279489));
#79492=CARTESIAN_POINT('Ctrl Pts',(81.5771665661634,-9.53689727566338,133.390412561551));
#79493=CARTESIAN_POINT('Ctrl Pts',(81.5698232211865,-9.55794835265927,133.388921203123));
#79494=CARTESIAN_POINT('Ctrl Pts',(81.5665266656359,-9.56713801039342,133.388270860424));
#79495=CARTESIAN_POINT('Ctrl Pts',(81.5593911015059,-9.58649248814824,133.386902396314));
#79496=CARTESIAN_POINT('Ctrl Pts',(81.5555330375977,-9.59664983405357,133.38618494341));
#79497=CARTESIAN_POINT('Ctrl Pts',(81.5449375126894,-9.62374377315015,133.384272635885));
#79498=CARTESIAN_POINT('Ctrl Pts',(81.5380208976747,-9.64060906451234,133.383083808359));
#79499=CARTESIAN_POINT('Ctrl Pts',(81.4973875955961,-9.73523425063597,133.376416282509));
#79500=CARTESIAN_POINT('Ctrl Pts',(81.4580507379254,-9.81045035137135,133.371134848421));
#79501=CARTESIAN_POINT('Ctrl Pts',(81.3774428705731,-9.93954983153217,133.361786631262));
#79502=CARTESIAN_POINT('Ctrl Pts',(81.3382915470587,-9.99452417956614,133.357698706954));
#79503=CARTESIAN_POINT('Ctrl Pts',(81.2501271176305,-10.1036517789193,133.349075651628));
#79504=CARTESIAN_POINT('Ctrl Pts',(81.2006738992874,-10.1572573309112,133.344539786208));
#79505=CARTESIAN_POINT('Ctrl Pts',(81.1394751862315,-10.2154368580119,133.339016543279));
#79506=CARTESIAN_POINT('Ctrl Pts',(81.1309883502346,-10.223337970069,133.338252397329));
#79507=CARTESIAN_POINT('Ctrl Pts',(81.1176670964474,-10.235482751097,133.337054417855));
#79508=CARTESIAN_POINT('Ctrl Pts',(81.1128892127569,-10.2397882736169,133.336625027775));
#79509=CARTESIAN_POINT('Ctrl Pts',(81.1040298489659,-10.2476792882462,133.335829089156));
#79510=CARTESIAN_POINT('Ctrl Pts',(81.0999556148451,-10.2512726145808,133.335463129761));
#79511=CARTESIAN_POINT('Ctrl Pts',(81.0904481941125,-10.2595754978366,133.334609366828));
#79512=CARTESIAN_POINT('Ctrl Pts',(81.0850020450138,-10.2642698510644,133.334120492799));
#79513=CARTESIAN_POINT('Ctrl Pts',(81.0674947060846,-10.2791640088564,133.332550018255));
#79514=CARTESIAN_POINT('Ctrl Pts',(81.0553191839195,-10.2892272429027,133.331459443341));
#79515=CARTESIAN_POINT('Ctrl Pts',(80.9871956723876,-10.3439206347133,133.325374864325));
#79516=CARTESIAN_POINT('Ctrl Pts',(80.9285645041819,-10.3850790283139,133.320204823061));
#79517=CARTESIAN_POINT('Ctrl Pts',(80.7550820010143,-10.490885120868,133.305432089289));
#79518=CARTESIAN_POINT('Ctrl Pts',(80.6349367190937,-10.5458830875849,133.295844128403));
#79519=CARTESIAN_POINT('Ctrl Pts',(80.4832858219372,-10.5946009090372,133.284830343213));
#79520=CARTESIAN_POINT('Ctrl Pts',(80.4568105127833,-10.6023862073558,133.28294304469));
#79521=CARTESIAN_POINT('Ctrl Pts',(80.4179942487842,-10.6127601162185,133.280225770502));
#79522=CARTESIAN_POINT('Ctrl Pts',(80.4057991744592,-10.6158717243573,133.279379113084));
#79523=CARTESIAN_POINT('Ctrl Pts',(80.3840509535066,-10.6211590999533,133.27788135762));
#79524=CARTESIAN_POINT('Ctrl Pts',(80.3745117956259,-10.6233893199827,133.277228538393));
#79525=CARTESIAN_POINT('Ctrl Pts',(80.3544868502458,-10.627885174799,133.275866495089));
#79526=CARTESIAN_POINT('Ctrl Pts',(80.3439977050833,-10.6301339384558,133.275157837372));
#79527=CARTESIAN_POINT('Ctrl Pts',(80.3162592978414,-10.6358011040009,133.273295929878));
#79528=CARTESIAN_POINT('Ctrl Pts',(80.2989760801053,-10.6390480582314,133.272148148442));
#79529=CARTESIAN_POINT('Ctrl Pts',(80.2104583092256,-10.6542308808987,133.266327520544));
#79530=CARTESIAN_POINT('Ctrl Pts',(80.1385489362517,-10.6617998031448,133.261794078396));
#79531=CARTESIAN_POINT('Ctrl Pts',(79.9661868862269,-10.6686715815886,133.251141285174));
#79532=CARTESIAN_POINT('Ctrl Pts',(79.8658543605867,-10.6636141132819,133.245116553544));
#79533=CARTESIAN_POINT('Ctrl Pts',(79.7125740712422,-10.6419251886125,133.235507371677));
#79534=CARTESIAN_POINT('Ctrl Pts',(79.6589731910374,-10.6316345816674,133.232065388663));
#79535=CARTESIAN_POINT('Ctrl Pts',(79.5951269918162,-10.6160936262512,133.227763037117));
#79536=CARTESIAN_POINT('Ctrl Pts',(79.5843014074159,-10.6133429347415,133.22702639555));
#79537=CARTESIAN_POINT('Ctrl Pts',(79.5673794441732,-10.608861586405,133.225862503675));
#79538=CARTESIAN_POINT('Ctrl Pts',(79.5612636566299,-10.6072045816297,133.225439304001));
#79539=CARTESIAN_POINT('Ctrl Pts',(79.5503885638563,-10.6041913994828,133.224681965123));
#79540=CARTESIAN_POINT('Ctrl Pts',(79.5456256389454,-10.6028488473074,133.224348610791));
#79541=CARTESIAN_POINT('Ctrl Pts',(79.5340975556181,-10.5995438507754,133.223537766283));
#79542=CARTESIAN_POINT('Ctrl Pts',(79.5273388434327,-10.5975597155602,133.22305905178));
#79543=CARTESIAN_POINT('Ctrl Pts',(79.5062251447896,-10.591215719854,133.221553579368));
#79544=CARTESIAN_POINT('Ctrl Pts',(79.491916801865,-10.5867049188131,133.220518824025));
#79545=CARTESIAN_POINT('Ctrl Pts',(79.4169826766383,-10.5619639881928,133.215029935782));
#79546=CARTESIAN_POINT('Ctrl Pts',(79.357502492438,-10.5384524778238,133.210433125733));
#79547=CARTESIAN_POINT('Ctrl Pts',(79.2002897335136,-10.4655995671432,133.197859911223));
#79548=CARTESIAN_POINT('Ctrl Pts',(79.1058112361221,-10.4099467186223,133.189853435972));
#79549=CARTESIAN_POINT('Ctrl Pts',(78.9768541114127,-10.3157725403069,133.178567637458));
#79550=CARTESIAN_POINT('Ctrl Pts',(78.9376028078378,-10.2842889098674,133.175072915361));
#79551=CARTESIAN_POINT('Ctrl Pts',(78.8875912623926,-10.2403098502144,133.170537671087));
#79552=CARTESIAN_POINT('Ctrl Pts',(78.8755083612627,-10.2293658166959,133.169435029025));
#79553=CARTESIAN_POINT('Ctrl Pts',(78.8559440647082,-10.211115717106,133.16763757602));
#79554=CARTESIAN_POINT('Ctrl Pts',(78.8483676071161,-10.2039136611744,133.16693842334));
#79555=CARTESIAN_POINT('Ctrl Pts',(78.8337497379333,-10.1897538817642,133.16558320609));
#79556=CARTESIAN_POINT('Ctrl Pts',(78.8267015804713,-10.1828037871409,133.164926852764));
#79557=CARTESIAN_POINT('Ctrl Pts',(78.8194395798959,-10.1755140354318,133.164247384722));
#79558=CARTESIAN_POINT('Ctrl Pts',(78.819163606737,-10.1752368124594,133.164221558479));
#79559=CARTESIAN_POINT('Ctrl Pts',(78.8186190150012,-10.1746893689219,133.164170584649));
#79560=CARTESIAN_POINT('Ctrl Pts',(78.8183503914444,-10.1744191533587,133.164145436845));
#79561=CARTESIAN_POINT('Ctrl Pts',(78.809839362714,-10.165851807505,133.163348510929));
#79562=CARTESIAN_POINT('Ctrl Pts',(78.8016842923687,-10.1574680367095,133.162580557559));
#79563=CARTESIAN_POINT('Ctrl Pts',(78.7735959120466,-10.1279768717481,133.159919264611));
#79564=CARTESIAN_POINT('Ctrl Pts',(78.7541258342425,-10.1064341533194,133.158045584328));
#79565=CARTESIAN_POINT('Ctrl Pts',(78.7086527321511,-10.0533969751689,133.153585636621));
#79566=CARTESIAN_POINT('Ctrl Pts',(78.683224887093,-10.0214336026417,133.151020900114));
#79567=CARTESIAN_POINT('Ctrl Pts',(78.607652409245,-9.91891847405607,133.143107382217));
#79568=CARTESIAN_POINT('Ctrl Pts',(78.5618131373326,-9.84537676647108,133.137873794813));
#79569=CARTESIAN_POINT('Ctrl Pts',(78.4850924529382,-9.69783518671517,133.127677489305));
#79570=CARTESIAN_POINT('Ctrl Pts',(78.4534269397785,-9.62452156485839,133.122735946446));
#79571=CARTESIAN_POINT('Ctrl Pts',(78.4233032485605,-9.5382551271212,133.11675956546));
#79572=CARTESIAN_POINT('Ctrl Pts',(78.4195847571195,-9.52723701436853,133.115993273416));
#79573=CARTESIAN_POINT('Ctrl Pts',(78.4139869965921,-9.51005903082281,133.11479263629));
#79574=CARTESIAN_POINT('Ctrl Pts',(78.4120275077825,-9.50392541350993,133.114362765966));
#79575=CARTESIAN_POINT('Ctrl Pts',(78.4084651663653,-9.4925474044237,133.113562919594));
#79576=CARTESIAN_POINT('Ctrl Pts',(78.4068525911845,-9.48730627214856,133.113193508944));
#79577=CARTESIAN_POINT('Ctrl Pts',(78.4031796413574,-9.4751554799136,133.112334885332));
#79578=CARTESIAN_POINT('Ctrl Pts',(78.4011382270982,-9.46824033805653,133.111844616063));
#79579=CARTESIAN_POINT('Ctrl Pts',(78.3947372325598,-9.44602743814125,133.11026507179));
#79580=CARTESIAN_POINT('Ctrl Pts',(78.3905519857202,-9.43068093903555,133.109166681608));
#79581=CARTESIAN_POINT('Ctrl Pts',(78.3517886860116,-9.28007998761419,133.098333863763));
#79582=CARTESIAN_POINT('Ctrl Pts',(78.3341234393601,-9.14105620196211,133.087965797041));
#79583=CARTESIAN_POINT('Ctrl Pts',(78.3340006446021,-9.00146554209231,133.077925694822));
#79584=CARTESIAN_POINT('Ctrl Pts',(78.3340006433067,-9.00146406876337,133.077925588852));
#79585=CARTESIAN_POINT('Ctrl Pts',(78.3339557795667,-8.95041253084761,133.074253691684));
#79586=CARTESIAN_POINT('Ctrl Pts',(78.3362574875391,-8.89938133463348,133.070625660202));
#79587=CARTESIAN_POINT('Ctrl Pts',(78.3434724212921,-8.82035306990941,133.06508751588));
#79588=CARTESIAN_POINT('Ctrl Pts',(78.3467625632695,-8.79224345465086,133.063133300972));
#79589=CARTESIAN_POINT('Ctrl Pts',(78.3526326291935,-8.75118184671486,133.060300908169));
#79590=CARTESIAN_POINT('Ctrl Pts',(78.3546527512714,-8.73815619881368,133.059405695518));
#79591=CARTESIAN_POINT('Ctrl Pts',(78.358444577942,-8.71548655266099,133.057853137201));
#79592=CARTESIAN_POINT('Ctrl Pts',(78.3601472018672,-8.70583182872112,133.057193654487));
#79593=CARTESIAN_POINT('Ctrl Pts',(78.363744613137,-8.68643535616325,133.055872052782));
#79594=CARTESIAN_POINT('Ctrl Pts',(78.3656414214097,-8.67669438478769,133.055210027292));
#79595=CARTESIAN_POINT('Ctrl Pts',(78.369704743846,-8.65677761962082,133.053859646418));
#79596=CARTESIAN_POINT('Ctrl Pts',(78.3718797665199,-8.64660399228132,133.053171593961));
#79597=CARTESIAN_POINT('Ctrl Pts',(78.3776557214902,-8.62077297136029,133.051428621622));
#79598=CARTESIAN_POINT('Ctrl Pts',(78.3813881513399,-8.60514583689018,133.050377934898));
#79599=CARTESIAN_POINT('Ctrl Pts',(78.39721509255,-8.54288108328702,133.046203830266));
#79600=CARTESIAN_POINT('Ctrl Pts',(78.4111046198013,-8.49672145218842,133.043137896813));
#79601=CARTESIAN_POINT('Ctrl Pts',(78.4300953670899,-8.44228584116502,133.039524165461));
#79602=CARTESIAN_POINT('Ctrl Pts',(78.4332897259278,-8.4333744580521,133.038932605405));
#79603=CARTESIAN_POINT('Ctrl Pts',(78.4365593697901,-8.4244920540871,133.038342736257));
#79604=CARTESIAN_POINT('',(78.3340000765193,-8.99949506206163,133.272970329525));
#79605=CARTESIAN_POINT('Ctrl Pts',(78.4365594153165,-8.4244919304089,133.231049000392));
#79606=CARTESIAN_POINT('Ctrl Pts',(78.4169016046737,-8.47789486355425,133.235116951829));
#79607=CARTESIAN_POINT('Ctrl Pts',(78.3999859734769,-8.53228865755636,133.239258820952));
#79608=CARTESIAN_POINT('Ctrl Pts',(78.3591291913327,-8.69214623975658,133.251269527389));
#79609=CARTESIAN_POINT('Ctrl Pts',(78.3426173016183,-8.79920153575082,133.259095417802));
#79610=CARTESIAN_POINT('Ctrl Pts',(78.3348735958138,-8.93787647209043,133.268758890274));
#79611=CARTESIAN_POINT('Ctrl Pts',(78.3340094155008,-8.96868188443447,133.270877725158));
#79612=CARTESIAN_POINT('Ctrl Pts',(78.3340000765193,-8.99949506206163,133.272970329525));
#79613=CARTESIAN_POINT('Ctrl Pts',(78.3340000762188,-8.99949605454145,133.272970396927));
#79614=CARTESIAN_POINT('Ctrl Pts',(78.3339976905965,-9.00738271465986,133.273506000723));
#79615=CARTESIAN_POINT('Ctrl Pts',(78.3340513068087,-9.01526943507976,133.274039866371));
#79616=CARTESIAN_POINT('Ctrl Pts',(78.3342826459358,-9.03191220643399,133.275162849773));
#79617=CARTESIAN_POINT('Ctrl Pts',(78.3344734091424,-9.04066783470319,133.275751542062));
#79618=CARTESIAN_POINT('Ctrl Pts',(78.3350069259462,-9.05864471200285,133.276956055915));
#79619=CARTESIAN_POINT('Ctrl Pts',(78.3353572678232,-9.06786544777664,133.277571619044));
#79620=CARTESIAN_POINT('Ctrl Pts',(78.3362616311666,-9.08739059026412,133.278870503318));
#79621=CARTESIAN_POINT('Ctrl Pts',(78.3368348206864,-9.0976937542916,133.279553198778));
#79622=CARTESIAN_POINT('Ctrl Pts',(78.3385195573599,-9.12362985231068,133.281265311306));
#79623=CARTESIAN_POINT('Ctrl Pts',(78.3397560464906,-9.13925388296953,133.28229079552));
#79624=CARTESIAN_POINT('Ctrl Pts',(78.3453906920561,-9.19961009437805,133.286231987792));
#79625=CARTESIAN_POINT('Ctrl Pts',(78.3513780395266,-9.24417684578525,133.289098295909));
#79626=CARTESIAN_POINT('Ctrl Pts',(78.3744558474355,-9.37545417849947,133.297475027547));
#79627=CARTESIAN_POINT('Ctrl Pts',(78.3966464648053,-9.46110554478804,133.302846601555));
#79628=CARTESIAN_POINT('Ctrl Pts',(78.4567536615628,-9.63488025455061,133.314080558537));
#79629=CARTESIAN_POINT('Ctrl Pts',(78.4956850759552,-9.72229745089437,133.319928689779));
#79630=CARTESIAN_POINT('Ctrl Pts',(78.5479448248526,-9.81685300266526,133.326983012949));
#79631=CARTESIAN_POINT('Ctrl Pts',(78.5541303718902,-9.82775241168547,133.3278078664));
#79632=CARTESIAN_POINT('Ctrl Pts',(78.563738514104,-9.84424637288987,133.329075671561));
#79633=CARTESIAN_POINT('Ctrl Pts',(78.567072318361,-9.84989249292746,133.3295131989));
#79634=CARTESIAN_POINT('Ctrl Pts',(78.5732478247967,-9.86021168489491,133.330319645113));
#79635=CARTESIAN_POINT('Ctrl Pts',(78.5760793146266,-9.86489062383157,133.330687913518));
#79636=CARTESIAN_POINT('Ctrl Pts',(78.5826101205488,-9.87556355643477,133.331533920798));
#79637=CARTESIAN_POINT('Ctrl Pts',(78.5863244316876,-9.8815480671857,133.332012605091));
#79638=CARTESIAN_POINT('Ctrl Pts',(78.5980705246104,-9.90020827004241,133.333518296356));
#79639=CARTESIAN_POINT('Ctrl Pts',(78.6062354311041,-9.91279870220469,133.334553305873));
#79640=CARTESIAN_POINT('Ctrl Pts',(78.6726614972274,-10.012259489797,133.342872497762));
#79641=CARTESIAN_POINT('Ctrl Pts',(78.7388115647394,-10.0935707540443,133.350536788483));
#79642=CARTESIAN_POINT('Ctrl Pts',(78.8914760175719,-10.2488127460606,133.366367480931));
#79643=CARTESIAN_POINT('Ctrl Pts',(78.9788374196915,-10.321209509879,133.374474519769));
#79644=CARTESIAN_POINT('Ctrl Pts',(79.0889731347742,-10.394977141385,133.383544677698));
#79645=CARTESIAN_POINT('Ctrl Pts',(79.10525355026,-10.4054750157039,133.384859609808));
#79646=CARTESIAN_POINT('Ctrl Pts',(79.1311519693164,-10.421542282271,133.386912004808));
#79647=CARTESIAN_POINT('Ctrl Pts',(79.1406484940575,-10.4273031774243,133.387656455614));
#79648=CARTESIAN_POINT('Ctrl Pts',(79.1585636120169,-10.4379274347415,133.389045980287));
#79649=CARTESIAN_POINT('Ctrl Pts',(79.166968489529,-10.4428128818439,133.389691836043));
#79650=CARTESIAN_POINT('Ctrl Pts',(79.1859584148176,-10.4536297694642,133.391137839997));
#79651=CARTESIAN_POINT('Ctrl Pts',(79.1965665390288,-10.4595197483663,133.391936476739));
#79652=CARTESIAN_POINT('Ctrl Pts',(79.2280211556656,-10.4765375105128,133.394278629311));
#79653=CARTESIAN_POINT('Ctrl Pts',(79.2490416603501,-10.4873385687717,133.395810647642));
#79654=CARTESIAN_POINT('Ctrl Pts',(79.3673976897871,-10.5450047946258,133.40426820204));
#79655=CARTESIAN_POINT('Ctrl Pts',(79.4688845300493,-10.5827651065281,133.410873462124));
#79656=CARTESIAN_POINT('Ctrl Pts',(79.6459756401576,-10.6296845394323,133.422060215578));
#79657=CARTESIAN_POINT('Ctrl Pts',(79.719842632773,-10.6439936733598,133.426639428557));
#79658=CARTESIAN_POINT('Ctrl Pts',(79.8299308669531,-10.6576830873738,133.433641988216));
#79659=CARTESIAN_POINT('Ctrl Pts',(79.8655747645331,-10.6609533874633,133.435936949813));
#79660=CARTESIAN_POINT('Ctrl Pts',(79.9109853092113,-10.663648596655,133.438927071686));
#79661=CARTESIAN_POINT('Ctrl Pts',(79.9206819974643,-10.6641390902288,133.439569401219));
#79662=CARTESIAN_POINT('Ctrl Pts',(79.9363280405427,-10.6647934698571,133.440612816794));
#79663=CARTESIAN_POINT('Ctrl Pts',(79.9422751239601,-10.6650102857316,133.441011047805));
#79664=CARTESIAN_POINT('Ctrl Pts',(79.9537954300195,-10.6653684932562,133.44178584785));
#79665=CARTESIAN_POINT('Ctrl Pts',(79.9593683966915,-10.6655137795521,133.442162201405));
#79666=CARTESIAN_POINT('Ctrl Pts',(79.9718264543493,-10.6657759964044,133.443006823653));
#79667=CARTESIAN_POINT('Ctrl Pts',(79.9787117477343,-10.6658782143431,133.443475880464));
#79668=CARTESIAN_POINT('Ctrl Pts',(79.9992847199339,-10.6660560756403,133.444883743139));
#79669=CARTESIAN_POINT('Ctrl Pts',(80.0129725238945,-10.6660057151717,133.445828818276));
#79670=CARTESIAN_POINT('Ctrl Pts',(80.1294326774497,-10.6641420020371,133.4539326332));
#79671=CARTESIAN_POINT('Ctrl Pts',(80.2318260645922,-10.6529896068574,133.461459174235));
#79672=CARTESIAN_POINT('Ctrl Pts',(80.4448897550273,-10.6095893145318,133.477272165677));
#79673=CARTESIAN_POINT('Ctrl Pts',(80.554605962369,-10.5751590714603,133.485493804684));
#79674=CARTESIAN_POINT('Ctrl Pts',(80.6777394093593,-10.5220385902219,133.49467004799));
#79675=CARTESIAN_POINT('Ctrl Pts',(80.695413263213,-10.5140451200776,133.495986773261));
#79676=CARTESIAN_POINT('Ctrl Pts',(80.7229875321801,-10.5009891774864,133.498041316093));
#79677=CARTESIAN_POINT('Ctrl Pts',(80.7329832720138,-10.4961333549944,133.498786145984));
#79678=CARTESIAN_POINT('Ctrl Pts',(80.7516304808649,-10.4868430013897,133.500176013319));
#79679=CARTESIAN_POINT('Ctrl Pts',(80.7602931176226,-10.4824320802956,133.500821836409));
#79680=CARTESIAN_POINT('Ctrl Pts',(80.7796732432428,-10.4723493646066,133.502267296741));
#79681=CARTESIAN_POINT('Ctrl Pts',(80.7903684911444,-10.4666358371689,133.503065427567));
#79682=CARTESIAN_POINT('Ctrl Pts',(80.8216862765814,-10.4494634215597,133.505404601765));
#79683=CARTESIAN_POINT('Ctrl Pts',(80.8421294262872,-10.4376823941721,133.50693419251));
#79684=CARTESIAN_POINT('Ctrl Pts',(80.950219864591,-10.3722947635359,133.515049899328));
#79685=CARTESIAN_POINT('Ctrl Pts',(81.033020121515,-10.311100097151,133.521350186711));
#79686=CARTESIAN_POINT('Ctrl Pts',(81.1688044771587,-10.1898483065746,133.532468300325));
#79687=CARTESIAN_POINT('Ctrl Pts',(81.2240966347742,-10.1328850677276,133.537287545242));
#79688=CARTESIAN_POINT('Ctrl Pts',(81.2910617499602,-10.0532469793383,133.54384828301));
#79689=CARTESIAN_POINT('Ctrl Pts',(81.3065787328773,-10.0339349721425,133.545427258493));
#79690=CARTESIAN_POINT('Ctrl Pts',(81.332140567466,-10.0006267714197,133.548144386176));
#79691=CARTESIAN_POINT('Ctrl Pts',(81.3424097099089,-9.98680724623321,133.549269989483));
#79692=CARTESIAN_POINT('Ctrl Pts',(81.3568063492455,-9.96679256953123,133.550901704897));
#79693=CARTESIAN_POINT('Ctrl Pts',(81.3611097452609,-9.96072451721202,133.551396604261));
#79694=CARTESIAN_POINT('Ctrl Pts',(81.368528321773,-9.95011397715609,133.552262709199));
#79695=CARTESIAN_POINT('Ctrl Pts',(81.3716618457523,-9.94558453719693,133.552632671317));
#79696=CARTESIAN_POINT('Ctrl Pts',(81.378328444134,-9.93584524479607,133.553428802512));
#79697=CARTESIAN_POINT('Ctrl Pts',(81.3818544123961,-9.9306309697025,133.553855392544));
#79698=CARTESIAN_POINT('Ctrl Pts',(81.3914547540172,-9.91625893209888,133.555031887564));
#79699=CARTESIAN_POINT('Ctrl Pts',(81.3974680696614,-9.90706104607363,133.555785589418));
#79700=CARTESIAN_POINT('Ctrl Pts',(81.4311409713177,-9.85442575994328,133.560100012507));
#79701=CARTESIAN_POINT('Ctrl Pts',(81.456863273399,-9.80978773403668,133.563763292817));
#79702=CARTESIAN_POINT('Ctrl Pts',(81.5245050487877,-9.67871798065568,133.57439196795));
#79703=CARTESIAN_POINT('Ctrl Pts',(81.5610783934606,-9.5897533848694,133.581443869823));
#79704=CARTESIAN_POINT('Ctrl Pts',(81.605512699765,-9.44794118776061,133.592131209116));
#79705=CARTESIAN_POINT('Ctrl Pts',(81.6188543971261,-9.39703106633235,133.595866652682));
#79706=CARTESIAN_POINT('Ctrl Pts',(81.6347106047286,-9.32225069886422,133.601194230665));
#79707=CARTESIAN_POINT('Ctrl Pts',(81.6391544272509,-9.29882626531135,133.602841024702));
#79708=CARTESIAN_POINT('Ctrl Pts',(81.6463009563173,-9.2561751725945,133.605800229999));
#79709=CARTESIAN_POINT('Ctrl Pts',(81.6491732215023,-9.23698164179548,133.607117635293));
#79710=CARTESIAN_POINT('Ctrl Pts',(81.6531622152748,-9.20672256491316,133.609172992605));
#79711=CARTESIAN_POINT('Ctrl Pts',(81.6545045573501,-9.19568906185629,133.609917966219));
#79712=CARTESIAN_POINT('Ctrl Pts',(81.6568137231118,-9.17498220747502,133.611307963631));
#79713=CARTESIAN_POINT('Ctrl Pts',(81.6578064848816,-9.16531228495021,133.611953774496));
#79714=CARTESIAN_POINT('Ctrl Pts',(81.6598469955976,-9.14356495602038,133.613399029516));
#79715=CARTESIAN_POINT('Ctrl Pts',(81.6608476811531,-9.13148360493405,133.614196969158));
#79716=CARTESIAN_POINT('Ctrl Pts',(81.663406043482,-9.0958759604373,133.616535018348));
#79717=CARTESIAN_POINT('Ctrl Pts',(81.6645963324937,-9.07232568382532,133.618063692197));
#79718=CARTESIAN_POINT('Ctrl Pts',(81.6683393113823,-8.94448516801164,133.626280156226));
#79719=CARTESIAN_POINT('Ctrl Pts',(81.6615926852596,-8.84015289178326,133.63267197218));
#79720=CARTESIAN_POINT('Ctrl Pts',(81.6328099509266,-8.66002277642012,133.643811887084));
#79721=CARTESIAN_POINT('Ctrl Pts',(81.6150850942583,-8.58388549538828,133.648561015107));
#79722=CARTESIAN_POINT('Ctrl Pts',(81.5848512902794,-8.48579558324173,133.655035050917));
#79723=CARTESIAN_POINT('Ctrl Pts',(81.5770952560203,-8.46247770207241,133.65660174401));
#79724=CARTESIAN_POINT('Ctrl Pts',(81.5630673980937,-8.42322516993826,133.659299782432));
#79725=CARTESIAN_POINT('Ctrl Pts',(81.55706024496,-8.40719966818956,133.660418809146));
#79726=CARTESIAN_POINT('Ctrl Pts',(81.5480958593724,-8.38436188376008,133.66204265416));
#79727=CARTESIAN_POINT('Ctrl Pts',(81.5453380614535,-8.37747180739011,133.662536407364));
#79728=CARTESIAN_POINT('Ctrl Pts',(81.5404543857011,-8.36550287767333,133.663401220569));
#79729=CARTESIAN_POINT('Ctrl Pts',(81.5383492209843,-8.36041577103342,133.663771048759));
#79730=CARTESIAN_POINT('Ctrl Pts',(81.5337792555254,-8.34952560154517,133.664567732996));
#79731=CARTESIAN_POINT('Ctrl Pts',(81.5313067605332,-8.34372616266693,133.664995017425));
#79732=CARTESIAN_POINT('Ctrl Pts',(81.5244168750763,-8.32781630079384,133.666175251278));
#79733=CARTESIAN_POINT('Ctrl Pts',(81.5199319644061,-8.31773572438035,133.666932035656));
#79734=CARTESIAN_POINT('Ctrl Pts',(81.4936202128274,-8.26014293276102,133.671304452874));
#79735=CARTESIAN_POINT('Ctrl Pts',(81.4696683382951,-8.21363897157253,133.67502577066));
#79736=CARTESIAN_POINT('Ctrl Pts',(81.3925143860814,-8.07971673871163,133.686167987996));
#79737=CARTESIAN_POINT('Ctrl Pts',(81.3333986547187,-7.99597439332068,133.693686184765));
#79738=CARTESIAN_POINT('Ctrl Pts',(81.2197946781932,-7.86292640181156,133.706226215633));
#79739=CARTESIAN_POINT('Ctrl Pts',(81.1690437497628,-7.81080920323398,133.711331666761));
#79740=CARTESIAN_POINT('Ctrl Pts',(81.1019623501586,-7.75038206141623,133.717492976774));
#79741=CARTESIAN_POINT('Ctrl Pts',(81.0886938358631,-7.7388054128458,133.718685900679));
#79742=CARTESIAN_POINT('Ctrl Pts',(81.0670477209241,-7.72051561282908,133.720591811923));
#79743=CARTESIAN_POINT('Ctrl Pts',(81.0587847309792,-7.71366954537114,133.721310208189));
#79744=CARTESIAN_POINT('Ctrl Pts',(81.042856053203,-7.70072977086798,133.722677973116));
#79745=CARTESIAN_POINT('Ctrl Pts',(81.0352016849585,-7.69462290718215,133.723327854375));
#79746=CARTESIAN_POINT('Ctrl Pts',(81.0175996463144,-7.68083172114363,133.724805866862));
#79747=CARTESIAN_POINT('Ctrl Pts',(81.0076178823878,-7.67319172236144,133.725632223117));
#79748=CARTESIAN_POINT('Ctrl Pts',(80.9807252600766,-7.65308676336552,133.727828181275));
#79749=CARTESIAN_POINT('Ctrl Pts',(80.9636631693813,-7.6408272140896,133.729189883931));
#79750=CARTESIAN_POINT('Ctrl Pts',(80.8469932920619,-7.56029866769342,133.738303631306));
#79751=CARTESIAN_POINT('Ctrl Pts',(80.7404491586042,-7.50271029738933,133.745638199615));
#79752=CARTESIAN_POINT('Ctrl Pts',(80.567211869434,-7.43212832413474,133.757068679495));
#79753=CARTESIAN_POINT('Ctrl Pts',(80.5043839556051,-7.41080320475072,133.761130515969));
#79754=CARTESIAN_POINT('Ctrl Pts',(80.4187979439278,-7.38734110932624,133.766747165373));
#79755=CARTESIAN_POINT('Ctrl Pts',(80.3970210918388,-7.3818422303494,133.768183514117));
#79756=CARTESIAN_POINT('Ctrl Pts',(80.3595473180854,-7.37318167199245,133.770677880824));
#79757=CARTESIAN_POINT('Ctrl Pts',(80.3439033485443,-7.36980289934193,133.771725890636));
#79758=CARTESIAN_POINT('Ctrl Pts',(80.3211287868474,-7.36522645993465,133.773264507926));
#79759=CARTESIAN_POINT('Ctrl Pts',(80.3140347007547,-7.36384889850058,133.773745584339));
#79760=CARTESIAN_POINT('Ctrl Pts',(80.3015901391559,-7.36151627213661,133.774593022745));
#79761=CARTESIAN_POINT('Ctrl Pts',(80.2962436119711,-7.36054116865741,133.774958254838));
#79762=CARTESIAN_POINT('Ctrl Pts',(80.2845866141595,-7.35847404201647,133.775757165277));
#79763=CARTESIAN_POINT('Ctrl Pts',(80.2782746894911,-7.35739225454501,133.7761913748));
#79764=CARTESIAN_POINT('Ctrl Pts',(80.2606346489957,-7.35447355514359,133.777409099069));
#79765=CARTESIAN_POINT('Ctrl Pts',(80.2492938120254,-7.35271730475782,133.778196839765));
#79766=CARTESIAN_POINT('Ctrl Pts',(80.1727929469362,-7.34167838063601,133.783539309828));
#79767=CARTESIAN_POINT('Ctrl Pts',(80.1071568807101,-7.33614800363321,133.788260773178));
#79768=CARTESIAN_POINT('Ctrl Pts',(80.0205526783311,-7.33399658439232,133.794540674751));
#79769=CARTESIAN_POINT('Ctrl Pts',(79.9997237292618,-7.33386984308063,133.796055051637));
#79770=CARTESIAN_POINT('Ctrl Pts',(79.9107261756953,-7.33499719451583,133.802532202975));
#79771=CARTESIAN_POINT('Ctrl Pts',(79.8426680396476,-7.34004466542439,133.807498326553));
#79772=CARTESIAN_POINT('Ctrl Pts',(79.704070582836,-7.35892664007696,133.81751912812));
#79773=CARTESIAN_POINT('Ctrl Pts',(79.6337241988074,-7.37318084949938,133.822554296935));
#79774=CARTESIAN_POINT('Ctrl Pts',(79.547567710075,-7.39651349216286,133.828645111702));
#79775=CARTESIAN_POINT('Ctrl Pts',(79.5307021467986,-7.40136823387309,133.829833990993));
#79776=CARTESIAN_POINT('Ctrl Pts',(79.503664606551,-7.40961575591624,133.83173503789));
#79777=CARTESIAN_POINT('Ctrl Pts',(79.4934435631474,-7.41284170537806,133.832452564826));
#79778=CARTESIAN_POINT('Ctrl Pts',(79.4739421152303,-7.41920429961048,133.833819677867));
#79779=CARTESIAN_POINT('Ctrl Pts',(79.4646568886899,-7.42232458830664,133.834469767091));
#79780=CARTESIAN_POINT('Ctrl Pts',(79.4434968735197,-7.42964370472721,133.835949623724));
#79781=CARTESIAN_POINT('Ctrl Pts',(79.4316410038073,-7.43389569638078,133.836777600236));
#79782=CARTESIAN_POINT('Ctrl Pts',(79.4000579845595,-7.44562853488086,133.838980937765));
#79783=CARTESIAN_POINT('Ctrl Pts',(79.3804224162109,-7.45335047437402,133.840348313163));
#79784=CARTESIAN_POINT('Ctrl Pts',(79.2510204840719,-7.50709945962742,133.84935534867));
#79785=CARTESIAN_POINT('Ctrl Pts',(79.1463095077185,-7.56440301348871,133.856591346483));
#79786=CARTESIAN_POINT('Ctrl Pts',(78.9699650840164,-7.68708038064582,133.869715375268));
#79787=CARTESIAN_POINT('Ctrl Pts',(78.8962134430123,-7.74844901882281,133.875577743605));
#79788=CARTESIAN_POINT('Ctrl Pts',(78.8192432211413,-7.82461644085024,133.882648370344));
#79789=CARTESIAN_POINT('Ctrl Pts',(78.8104346410356,-7.83353211977652,133.883473281171));
#79790=CARTESIAN_POINT('Ctrl Pts',(78.7971722212994,-7.84726224526244,133.884741156544));
#79791=CARTESIAN_POINT('Ctrl Pts',(78.7926446096592,-7.8520052464573,133.885178695802));
#79792=CARTESIAN_POINT('Ctrl Pts',(78.7843921961703,-7.86075306479148,133.885985152824));
#79793=CARTESIAN_POINT('Ctrl Pts',(78.7806589708722,-7.86474964701672,133.886353419989));
#79794=CARTESIAN_POINT('Ctrl Pts',(78.7721629845168,-7.87393522751475,133.887199409881));
#79795=CARTESIAN_POINT('Ctrl Pts',(78.7674134228655,-7.87913607705212,133.887678077869));
#79796=CARTESIAN_POINT('Ctrl Pts',(78.7526491198931,-7.89551055790167,133.889183666216));
#79797=CARTESIAN_POINT('Ctrl Pts',(78.7427525878823,-7.90678910937542,133.890218587618));
#79798=CARTESIAN_POINT('Ctrl Pts',(78.6650772264852,-7.9977614030156,133.898539084728));
#79799=CARTESIAN_POINT('Ctrl Pts',(78.6047953550745,-8.08353859734886,133.906204921304));
#79800=CARTESIAN_POINT('Ctrl Pts',(78.5073001242087,-8.25441841247182,133.920509154064));
#79801=CARTESIAN_POINT('Ctrl Pts',(78.4683707136649,-8.33807251325376,133.927135512778));
#79802=CARTESIAN_POINT('Ctrl Pts',(78.4365594263723,-8.4244919003743,133.93353979929));
#79803=CARTESIAN_POINT('Origin',(80.,-9.,134.));
#79804=CARTESIAN_POINT('',(78.4365594680555,-8.42449178713676,134.632696249083));
#79805=CARTESIAN_POINT('',(78.4365593695135,-8.4244920548384,134.440654933552));
#79806=CARTESIAN_POINT('',(78.4365593749993,-8.42449203993574,134.));
#79807=CARTESIAN_POINT('Ctrl Pts',(78.4365593695135,-8.4244920548384,134.440654933552));
#79808=CARTESIAN_POINT('Ctrl Pts',(78.4604281544172,-8.35964946068749,134.435817450756));
#79809=CARTESIAN_POINT('Ctrl Pts',(78.4883094068626,-8.2963502231991,134.430817626444));
#79810=CARTESIAN_POINT('Ctrl Pts',(78.5600797186349,-8.15751128644456,134.419450966649));
#79811=CARTESIAN_POINT('Ctrl Pts',(78.6061381558519,-8.0833162960484,134.413091474615));
#79812=CARTESIAN_POINT('Ctrl Pts',(78.6815254624746,-7.98079172361757,134.404038301892));
#79813=CARTESIAN_POINT('Ctrl Pts',(78.7064132363256,-7.94938383223044,134.40122264318));
#79814=CARTESIAN_POINT('Ctrl Pts',(78.7509808543772,-7.89712825121749,134.396467114652));
#79815=CARTESIAN_POINT('Ctrl Pts',(78.7701096548337,-7.87583593969998,134.39450753354));
#79816=CARTESIAN_POINT('Ctrl Pts',(78.7977805476383,-7.84658768869443,134.391782711849));
#79817=CARTESIAN_POINT('Ctrl Pts',(78.8058711457575,-7.83821350372441,134.390998558487));
#79818=CARTESIAN_POINT('Ctrl Pts',(78.8143192790629,-7.82965074612878,134.390192421115));
#79819=CARTESIAN_POINT('Ctrl Pts',(78.8145895998778,-7.82937694738164,134.390166639819));
#79820=CARTESIAN_POINT('Ctrl Pts',(78.815138042624,-7.82882183317268,134.390114360048));
#79821=CARTESIAN_POINT('Ctrl Pts',(78.8154161699469,-7.82854052307942,134.390087861815));
#79822=CARTESIAN_POINT('Ctrl Pts',(78.8159816583395,-7.82796897079121,134.390034014012));
#79823=CARTESIAN_POINT('Ctrl Pts',(78.8162690260306,-7.82767873512303,134.390006664733));
#79824=CARTESIAN_POINT('Ctrl Pts',(78.8168546160354,-7.82708773567737,134.389950963421));
#79825=CARTESIAN_POINT('Ctrl Pts',(78.8171528463984,-7.82678697986582,134.389922611745));
#79826=CARTESIAN_POINT('Ctrl Pts',(78.8177620141437,-7.82617312200096,134.389864733003));
#79827=CARTESIAN_POINT('Ctrl Pts',(78.8180729612844,-7.82586002969489,134.389835206373));
#79828=CARTESIAN_POINT('Ctrl Pts',(78.8185020571743,-7.82542831673484,134.389794484572));
#79829=CARTESIAN_POINT('Ctrl Pts',(78.8186200992656,-7.82530959050026,134.389783284704));
#79830=CARTESIAN_POINT('Ctrl Pts',(78.818890796289,-7.82503740665418,134.389757606603));
#79831=CARTESIAN_POINT('Ctrl Pts',(78.8190434632945,-7.82488396093598,134.389743128897));
#79832=CARTESIAN_POINT('Ctrl Pts',(78.8193957159969,-7.8245300494634,134.389709733695));
#79833=CARTESIAN_POINT('Ctrl Pts',(78.8195953228865,-7.82432960474896,134.389690817135));
#79834=CARTESIAN_POINT('Ctrl Pts',(78.8200596899689,-7.82386352602137,134.389646826012));
#79835=CARTESIAN_POINT('Ctrl Pts',(78.8203244889154,-7.82359793046469,134.389621753158));
#79836=CARTESIAN_POINT('Ctrl Pts',(78.8209475382402,-7.82297342868785,134.3895627882));
#79837=CARTESIAN_POINT('Ctrl Pts',(78.8213058630013,-7.82261459642031,134.389528899379));
#79838=CARTESIAN_POINT('Ctrl Pts',(78.8278609207265,-7.81605624611889,134.388909366331));
#79839=CARTESIAN_POINT('Ctrl Pts',(78.8341064206742,-7.80990546583899,134.388325889288));
#79840=CARTESIAN_POINT('Ctrl Pts',(78.8482931346758,-7.79615277661807,134.387015531196));
#79841=CARTESIAN_POINT('Ctrl Pts',(78.8562616819097,-7.78857954847971,134.386289912049));
#79842=CARTESIAN_POINT('Ctrl Pts',(78.8780776085952,-7.76825306473355,134.384330746181));
#79843=CARTESIAN_POINT('Ctrl Pts',(78.8920673884735,-7.75565449334599,134.383103765968));
#79844=CARTESIAN_POINT('Ctrl Pts',(78.9752609182827,-7.68324972529538,134.375969508528));
#79845=CARTESIAN_POINT('Ctrl Pts',(79.0490852196478,-7.62898370000524,134.370294372178));
#79846=CARTESIAN_POINT('Ctrl Pts',(79.2080289381381,-7.53119477209854,134.358859043487));
#79847=CARTESIAN_POINT('Ctrl Pts',(79.2931735232444,-7.48837803039206,134.353123925114));
#79848=CARTESIAN_POINT('Ctrl Pts',(79.4066903535852,-7.44299143420336,134.345442532917));
#79849=CARTESIAN_POINT('Ctrl Pts',(79.4321218958737,-7.43353700798298,134.343718797002));
#79850=CARTESIAN_POINT('Ctrl Pts',(79.4751783966695,-7.41871660149663,134.340777900067));
#79851=CARTESIAN_POINT('Ctrl Pts',(79.4926825959062,-7.41301421406123,134.339576162977));
#79852=CARTESIAN_POINT('Ctrl Pts',(79.5175786461641,-7.40535772122652,134.337853517496));
#79853=CARTESIAN_POINT('Ctrl Pts',(79.5248956886389,-7.4031624229224,134.337345599253));
#79854=CARTESIAN_POINT('Ctrl Pts',(79.5375414843708,-7.39946297209523,134.336464564497));
#79855=CARTESIAN_POINT('Ctrl Pts',(79.5428630738136,-7.3979349307168,134.336092823265));
#79856=CARTESIAN_POINT('Ctrl Pts',(79.5541534482153,-7.39475384810932,134.335301903068));
#79857=CARTESIAN_POINT('Ctrl Pts',(79.5601237688585,-7.39310757857471,134.334882380969));
#79858=CARTESIAN_POINT('Ctrl Pts',(79.5765409583558,-7.38867901434732,134.333725517092));
#79859=CARTESIAN_POINT('Ctrl Pts',(79.5870057298549,-7.38596511928022,134.33298448573));
#79860=CARTESIAN_POINT('Ctrl Pts',(79.6419335895716,-7.37228946970346,134.329078673721));
#79861=CARTESIAN_POINT('Ctrl Pts',(79.686804531605,-7.363063559037,134.325832839242));
#79862=CARTESIAN_POINT('Ctrl Pts',(79.8191738558044,-7.34148856145347,134.316199696814));
#79863=CARTESIAN_POINT('Ctrl Pts',(79.9073450160713,-7.33423489150616,134.309717824102));
#79864=CARTESIAN_POINT('Ctrl Pts',(80.0798740565613,-7.33378705899995,134.297242989146));
#79865=CARTESIAN_POINT('Ctrl Pts',(80.1639779990175,-7.33995168353664,134.291258941342));
#79866=CARTESIAN_POINT('Ctrl Pts',(80.2700353051403,-7.3558689111397,134.283884221775));
#79867=CARTESIAN_POINT('Ctrl Pts',(80.2927319233199,-7.35975787872547,134.282315493636));
#79868=CARTESIAN_POINT('Ctrl Pts',(80.3269881800399,-7.36636129700816,134.27996107715));
#79869=CARTESIAN_POINT('Ctrl Pts',(80.338610651751,-7.36873070250928,134.279164594538));
#79870=CARTESIAN_POINT('Ctrl Pts',(80.3587789966513,-7.37306714767717,134.277786222555));
#79871=CARTESIAN_POINT('Ctrl Pts',(80.3673363535131,-7.37497788235475,134.277202565745));
#79872=CARTESIAN_POINT('Ctrl Pts',(80.38657166401,-7.379432559903,134.275893090737));
#79873=CARTESIAN_POINT('Ctrl Pts',(80.3972404324327,-7.38201467007062,134.275168523132));
#79874=CARTESIAN_POINT('Ctrl Pts',(80.4260600425129,-7.38929198554653,134.273215398645));
#79875=CARTESIAN_POINT('Ctrl Pts',(80.4441587602555,-7.39418851992955,134.271993337626));
#79876=CARTESIAN_POINT('Ctrl Pts',(80.548757120659,-7.42439099280467,134.264949947773));
#79877=CARTESIAN_POINT('Ctrl Pts',(80.6331766852885,-7.45637813520837,134.259353444285));
#79878=CARTESIAN_POINT('Ctrl Pts',(80.8016359315266,-7.53636808914985,134.247921545156));
#79879=CARTESIAN_POINT('Ctrl Pts',(80.8849137526741,-7.58516296545013,134.242116811753));
#79880=CARTESIAN_POINT('Ctrl Pts',(80.9857665153195,-7.65665895948425,134.23435110281));
#79881=CARTESIAN_POINT('Ctrl Pts',(81.007637769759,-7.6729857829191,134.232617502212));
#79882=CARTESIAN_POINT('Ctrl Pts',(81.0436369081636,-7.70126220900221,134.229661443933));
#79883=CARTESIAN_POINT('Ctrl Pts',(81.0579850350533,-7.71292368440036,134.228454617076));
#79884=CARTESIAN_POINT('Ctrl Pts',(81.0779925931422,-7.72974548715713,134.226725914759));
#79885=CARTESIAN_POINT('Ctrl Pts',(81.0838156553143,-7.73471023955476,134.226217152874));
#79886=CARTESIAN_POINT('Ctrl Pts',(81.0937940908496,-7.74333729081661,134.225335146039));
#79887=CARTESIAN_POINT('Ctrl Pts',(81.097965752787,-7.74698049389898,134.224963284983));
#79888=CARTESIAN_POINT('Ctrl Pts',(81.1067589691621,-7.75473743221446,134.2241726757));
#79889=CARTESIAN_POINT('Ctrl Pts',(81.1113757270145,-7.75885606442307,134.223753589144));
#79890=CARTESIAN_POINT('Ctrl Pts',(81.1239751415644,-7.7702227281193,134.222599145985));
#79891=CARTESIAN_POINT('Ctrl Pts',(81.1319103766087,-7.77752253954141,134.221860124429));
#79892=CARTESIAN_POINT('Ctrl Pts',(81.1727162984845,-7.81579879091319,134.217999861508));
#79893=CARTESIAN_POINT('Ctrl Pts',(81.2043854110169,-7.84802299561058,134.214799800512));
#79894=CARTESIAN_POINT('Ctrl Pts',(81.3060463051857,-7.96024468216313,134.203927798364));
#79895=CARTESIAN_POINT('Ctrl Pts',(81.3696915784666,-8.0456444655024,134.196105403601));
#79896=CARTESIAN_POINT('Ctrl Pts',(81.4642161464865,-8.20161456954474,134.183009233408));
#79897=CARTESIAN_POINT('Ctrl Pts',(81.4991597275764,-8.26933502185664,134.177652493886));
#79898=CARTESIAN_POINT('Ctrl Pts',(81.5364164067653,-8.35556402601269,134.171240195187));
#79899=CARTESIAN_POINT('Ctrl Pts',(81.5432169680661,-8.37202346241667,134.170033431159));
#79900=CARTESIAN_POINT('Ctrl Pts',(81.5537069007831,-8.39861246578579,134.168110750083));
#79901=CARTESIAN_POINT('Ctrl Pts',(81.5575639864799,-8.40867391626479,134.167389254215));
#79902=CARTESIAN_POINT('Ctrl Pts',(81.564736436126,-8.42794091311735,134.166018893941));
#79903=CARTESIAN_POINT('Ctrl Pts',(81.5680688371174,-8.43713958883738,134.165369485333));
#79904=CARTESIAN_POINT('Ctrl Pts',(81.575471012176,-8.45814843702911,134.163897012699));
#79905=CARTESIAN_POINT('Ctrl Pts',(81.5794894106835,-8.46997618715963,134.163075673167));
#79906=CARTESIAN_POINT('Ctrl Pts',(81.59179053065,-8.50756610365097,134.160488502339));
#79907=CARTESIAN_POINT('Ctrl Pts',(81.5995790915591,-8.53348622888576,134.158738761298));
#79908=CARTESIAN_POINT('Ctrl Pts',(81.6416951053189,-8.68713521954408,134.148543042906));
#79909=CARTESIAN_POINT('Ctrl Pts',(81.6613452972767,-8.81839159700811,134.140590427004));
#79910=CARTESIAN_POINT('Ctrl Pts',(81.6673951326799,-9.02232081244227,134.128074890246));
#79911=CARTESIAN_POINT('Ctrl Pts',(81.6648867296921,-9.09409867496912,134.12362805577));
#79912=CARTESIAN_POINT('Ctrl Pts',(81.656190220502,-9.18121822000287,134.117948003497));
#79913=CARTESIAN_POINT('Ctrl Pts',(81.6543955005055,-9.19693037611636,134.116912190772));
#79914=CARTESIAN_POINT('Ctrl Pts',(81.6514594466223,-9.21974859007526,134.115388179631));
#79915=CARTESIAN_POINT('Ctrl Pts',(81.6504952355611,-9.22687710176757,134.114909259099));
#79916=CARTESIAN_POINT('Ctrl Pts',(81.6487218285582,-9.23937804550147,134.114064102235));
#79917=CARTESIAN_POINT('Ctrl Pts',(81.6479324730694,-9.24475309920712,134.113698973264));
#79918=CARTESIAN_POINT('Ctrl Pts',(81.6461515386529,-9.25648089505401,134.112898417369));
#79919=CARTESIAN_POINT('Ctrl Pts',(81.6451494878438,-9.26283168928598,134.112462441872));
#79920=CARTESIAN_POINT('Ctrl Pts',(81.6422388684703,-9.28060955064329,134.111235406685));
#79921=CARTESIAN_POINT('Ctrl Pts',(81.6402478692286,-9.29202248166598,134.110440022732));
#79922=CARTESIAN_POINT('Ctrl Pts',(81.6251048208468,-9.3737802784709,134.104691538413));
#79923=CARTESIAN_POINT('Ctrl Pts',(81.6075525216211,-9.44322674926886,134.09954182347));
#79924=CARTESIAN_POINT('Ctrl Pts',(81.5813084429264,-9.52460893271757,134.093333368532));
#79925=CARTESIAN_POINT('Ctrl Pts',(81.5768565989234,-9.53784215703743,134.092318070302));
#79926=CARTESIAN_POINT('Ctrl Pts',(81.5503241928956,-9.61354803164934,134.086480605595));
#79927=CARTESIAN_POINT('Ctrl Pts',(81.5246975025853,-9.67471815677951,134.08165283596));
#79928=CARTESIAN_POINT('Ctrl Pts',(81.4627725835815,-9.80085300514316,134.071572383585));
#79929=CARTESIAN_POINT('Ctrl Pts',(81.4256277807417,-9.86524989328049,134.06635102227));
#79930=CARTESIAN_POINT('Ctrl Pts',(81.37445416223,-9.94167147444477,134.060073582733));
#79931=CARTESIAN_POINT('Ctrl Pts',(81.3643698508529,-9.95622401242201,134.058874006735));
#79932=CARTESIAN_POINT('Ctrl Pts',(81.3477906294414,-9.97935286749778,134.05695996871));
#79933=CARTESIAN_POINT('Ctrl Pts',(81.3414415277462,-9.98803150602629,134.056240016948));
#79934=CARTESIAN_POINT('Ctrl Pts',(81.3291526136429,-10.0044924866336,134.054870844027));
#79935=CARTESIAN_POINT('Ctrl Pts',(81.3232273836548,-10.0122851002471,134.054221095302));
#79936=CARTESIAN_POINT('Ctrl Pts',(81.3095595133667,-10.0299354286428,134.052745488531));
#79937=CARTESIAN_POINT('Ctrl Pts',(81.3017735584805,-10.039758973486,134.05192138213));
#79938=CARTESIAN_POINT('Ctrl Pts',(81.2807260566603,-10.0657075604624,134.049736068617));
#79939=CARTESIAN_POINT('Ctrl Pts',(81.2672707744724,-10.0816730942799,134.048382634449));
#79940=CARTESIAN_POINT('Ctrl Pts',(81.1725655472882,-10.1898530541529,134.039137657389));
#79941=CARTESIAN_POINT('Ctrl Pts',(81.0816286729673,-10.2730842594732,134.031681170422));
#79942=CARTESIAN_POINT('Ctrl Pts',(80.9299564152572,-10.383815781604,134.020203215644));
#79943=CARTESIAN_POINT('Ctrl Pts',(80.8753715402846,-10.4189744542783,134.0162243749));
#79944=CARTESIAN_POINT('Ctrl Pts',(80.7901965573352,-10.467048148943,134.010031333431));
#79945=CARTESIAN_POINT('Ctrl Pts',(80.7610410287725,-10.4823822315928,134.00791366116));
#79946=CARTESIAN_POINT('Ctrl Pts',(80.7229594434782,-10.5009913400821,134.005125747321));
#79947=CARTESIAN_POINT('Ctrl Pts',(80.7144313054781,-10.5050691875502,134.004500025969));
#79948=CARTESIAN_POINT('Ctrl Pts',(80.7005285650467,-10.5115721921344,134.003476977466));
#79949=CARTESIAN_POINT('Ctrl Pts',(80.6951748352517,-10.5140418449269,134.003082304922));
#79950=CARTESIAN_POINT('Ctrl Pts',(80.6847000029934,-10.518806570568,134.002308504491));
#79951=CARTESIAN_POINT('Ctrl Pts',(80.6795802263952,-10.5211042717181,134.001929540396));
#79952=CARTESIAN_POINT('Ctrl Pts',(80.6667847319004,-10.5267692614012,134.00098071632));
#79953=CARTESIAN_POINT('Ctrl Pts',(80.6590950970591,-10.5301045395165,134.000408986378));
#79954=CARTESIAN_POINT('Ctrl Pts',(80.6314237885211,-10.5418593175358,133.998347009341));
#79955=CARTESIAN_POINT('Ctrl Pts',(80.6113042784857,-10.5499461685438,133.996839238729));
#79956=CARTESIAN_POINT('Ctrl Pts',(80.4914623485628,-10.5954192898092,133.987831306368));
#79957=CARTESIAN_POINT('Ctrl Pts',(80.3885033330421,-10.6235642845263,133.980001452305));
#79958=CARTESIAN_POINT('Ctrl Pts',(80.1989852292527,-10.6562996949848,133.966051091097));
#79959=CARTESIAN_POINT('Ctrl Pts',(80.113389406705,-10.6643528356489,133.959910700826));
#79960=CARTESIAN_POINT('Ctrl Pts',(79.9985607754945,-10.6662515301852,133.951957237713));
#79961=CARTESIAN_POINT('Ctrl Pts',(79.9695689329967,-10.665974299154,133.949972239948));
#79962=CARTESIAN_POINT('Ctrl Pts',(79.9276393308621,-10.6644783147152,133.947133171567));
#79963=CARTESIAN_POINT('Ctrl Pts',(79.9146867435558,-10.6638647154661,133.946260516424));
#79964=CARTESIAN_POINT('Ctrl Pts',(79.8919403380547,-10.6625208340308,133.944735336558));
#79965=CARTESIAN_POINT('Ctrl Pts',(79.8821434964361,-10.6618550676255,133.944080830936));
#79966=CARTESIAN_POINT('Ctrl Pts',(79.861733610264,-10.6602866744464,133.942722029031));
#79967=CARTESIAN_POINT('Ctrl Pts',(79.8511221576218,-10.6593688055455,133.94201824041));
#79968=CARTESIAN_POINT('Ctrl Pts',(79.8233714391934,-10.6567000770141,133.940184265758));
#79969=CARTESIAN_POINT('Ctrl Pts',(79.8062489674001,-10.6547849912203,133.93905924769));
#79970=CARTESIAN_POINT('Ctrl Pts',(79.7298492782139,-10.6450378282656,133.93406480769));
#79971=CARTESIAN_POINT('Ctrl Pts',(79.670986197031,-10.6342833155264,133.930287268569));
#79972=CARTESIAN_POINT('Ctrl Pts',(79.5110290925058,-10.5960630171867,133.920063922536));
#79973=CARTESIAN_POINT('Ctrl Pts',(79.4117563054396,-10.5622031178988,133.913776654347));
#79974=CARTESIAN_POINT('Ctrl Pts',(79.2771215662817,-10.5016158568823,133.904658725152));
#79975=CARTESIAN_POINT('Ctrl Pts',(79.238625823429,-10.4824683035283,133.901975711185));
#79976=CARTESIAN_POINT('Ctrl Pts',(79.1857736944808,-10.4535781135716,133.898126151816));
#79977=CARTESIAN_POINT('Ctrl Pts',(79.1707613264984,-10.4450664279501,133.897013179087));
#79978=CARTESIAN_POINT('Ctrl Pts',(79.1445896861132,-10.4296855702496,133.895033381867));
#79979=CARTESIAN_POINT('Ctrl Pts',(79.1333739678954,-10.4229149409468,133.894171885651));
#79980=CARTESIAN_POINT('Ctrl Pts',(79.1165670873087,-10.4124966661632,133.892859225489));
#79981=CARTESIAN_POINT('Ctrl Pts',(79.1109157840619,-10.4089463425788,133.892414085797));
#79982=CARTESIAN_POINT('Ctrl Pts',(79.1006768882704,-10.402427822106,133.891600437776));
#79983=CARTESIAN_POINT('Ctrl Pts',(79.0960823736167,-10.3994708920489,133.891232660568));
#79984=CARTESIAN_POINT('Ctrl Pts',(79.085712406993,-10.3927246355635,133.890396513062));
#79985=CARTESIAN_POINT('Ctrl Pts',(79.0799459634399,-10.3889219844041,133.889927290139));
#79986=CARTESIAN_POINT('Ctrl Pts',(79.0623281501129,-10.3771461538933,133.88848097378));
#79987=CARTESIAN_POINT('Ctrl Pts',(79.0505558967655,-10.3690565686035,133.887496723574));
#79988=CARTESIAN_POINT('Ctrl Pts',(78.9457893431323,-10.295062618417,133.878586293032));
#79989=CARTESIAN_POINT('Ctrl Pts',(78.8596901102479,-10.2199331985886,133.870204812937));
#79990=CARTESIAN_POINT('Ctrl Pts',(78.7209604058106,-10.0712622015278,133.855442551632));
#79991=CARTESIAN_POINT('Ctrl Pts',(78.6653314691638,-10.0011039158258,133.8490392964));
#79992=CARTESIAN_POINT('Ctrl Pts',(78.5994405667938,-9.90268073790606,133.84083614186));
#79993=CARTESIAN_POINT('Ctrl Pts',(78.5839189624327,-9.87813092338495,133.838847514511));
#79994=CARTESIAN_POINT('Ctrl Pts',(78.5624013300585,-9.84204181744154,133.836004277962));
#79995=CARTESIAN_POINT('Ctrl Pts',(78.555886733001,-9.83081962347559,133.835131007876));
#79996=CARTESIAN_POINT('Ctrl Pts',(78.5446730156189,-9.81097213748313,133.833605125644));
#79997=CARTESIAN_POINT('Ctrl Pts',(78.5399178933261,-9.80237939163076,133.832950526835));
#79998=CARTESIAN_POINT('Ctrl Pts',(78.5301664438174,-9.78438426147971,133.831591884029));
#79999=CARTESIAN_POINT('Ctrl Pts',(78.5251836994121,-9.77497499375271,133.830888344641));
#80000=CARTESIAN_POINT('Ctrl Pts',(78.5123837464134,-9.75023332837819,133.829055801276));
#80001=CARTESIAN_POINT('Ctrl Pts',(78.5047131786277,-9.73482618543004,133.827931950045));
#80002=CARTESIAN_POINT('Ctrl Pts',(78.4715817838219,-9.66561034177503,133.82295566711));
#80003=CARTESIAN_POINT('Ctrl Pts',(78.4487754234425,-9.61057582615569,133.819194234605));
#80004=CARTESIAN_POINT('Ctrl Pts',(78.3874605002678,-9.43683440399255,133.807739203704));
#80005=CARTESIAN_POINT('Ctrl Pts',(78.35929672025,-9.31495645834477,133.800310403973));
#80006=CARTESIAN_POINT('Ctrl Pts',(78.3415069515466,-9.16087713967949,133.790608129399));
#80007=CARTESIAN_POINT('Ctrl Pts',(78.3388471370996,-9.13058174901709,133.788684097398));
#80008=CARTESIAN_POINT('Ctrl Pts',(78.3358148742834,-9.08027269593718,133.785437350806));
#80009=CARTESIAN_POINT('Ctrl Pts',(78.3349713554805,-9.06029398819754,133.784134531648));
#80010=CARTESIAN_POINT('Ctrl Pts',(78.3342967627965,-9.03241870018604,133.782291971479));
#80011=CARTESIAN_POINT('Ctrl Pts',(78.3341619212222,-9.02453030077042,133.781767778837));
#80012=CARTESIAN_POINT('Ctrl Pts',(78.3340274107809,-9.0110649252554,133.780867810309));
#80013=CARTESIAN_POINT('Ctrl Pts',(78.3339997062126,-9.00548824500956,133.780493567682));
#80014=CARTESIAN_POINT('Ctrl Pts',(78.3340003253352,-8.99382919224086,133.779707801327));
#80015=CARTESIAN_POINT('Ctrl Pts',(78.3340339570069,-8.98774702239071,133.779296012302));
#80016=CARTESIAN_POINT('Ctrl Pts',(78.3342142738354,-8.97136335691666,133.77818195045));
#80017=CARTESIAN_POINT('Ctrl Pts',(78.3344232108852,-8.96106301293832,133.777476413428));
#80018=CARTESIAN_POINT('Ctrl Pts',(78.3360154175545,-8.90720924942272,133.773763050365));
#80019=CARTESIAN_POINT('Ctrl Pts',(78.3390114428183,-8.86372415998546,133.770680907367));
#80020=CARTESIAN_POINT('Ctrl Pts',(78.3559301161319,-8.7076886804988,133.759428309044));
#80021=CARTESIAN_POINT('Ctrl Pts',(78.379627376782,-8.59650734151485,133.751070154554));
#80022=CARTESIAN_POINT('Ctrl Pts',(78.4213756147411,-8.46707201417176,133.741325715804));
#80023=CARTESIAN_POINT('Ctrl Pts',(78.4287520063035,-8.44570175265309,133.739715310315));
#80024=CARTESIAN_POINT('Ctrl Pts',(78.4365593580908,-8.42449208586977,133.738116396704));
#80025=CARTESIAN_POINT('Ctrl Pts',(78.4365594263723,-8.4244919003743,133.93353979929));
#80026=CARTESIAN_POINT('Ctrl Pts',(78.4292827658715,-8.44425986936527,133.93500474531));
#80027=CARTESIAN_POINT('Ctrl Pts',(78.4223785765527,-8.4641724876544,133.936458744668));
#80028=CARTESIAN_POINT('Ctrl Pts',(78.4098685482923,-8.50259529746954,133.939223460302));
#80029=CARTESIAN_POINT('Ctrl Pts',(78.4042055318288,-8.52107459690236,133.940535343517));
#80030=CARTESIAN_POINT('Ctrl Pts',(78.3957986584612,-8.55031432170058,133.94258408617));
#80031=CARTESIAN_POINT('Ctrl Pts',(78.3928387767658,-8.5610102890579,133.943327892097));
#80032=CARTESIAN_POINT('Ctrl Pts',(78.3874866911236,-8.58113086501106,133.944716835285));
#80033=CARTESIAN_POINT('Ctrl Pts',(78.3850697037473,-8.59054833173501,133.945362748037));
#80034=CARTESIAN_POINT('Ctrl Pts',(78.3798188296641,-8.61177775394053,133.946809683789));
#80035=CARTESIAN_POINT('Ctrl Pts',(78.377031384831,-8.62360071165609,133.947609186707));
#80036=CARTESIAN_POINT('Ctrl Pts',(78.3691885509082,-8.6585743417681,133.949956443125));
#80037=CARTESIAN_POINT('Ctrl Pts',(78.3644973337424,-8.68180417670322,133.951492622017));
#80038=CARTESIAN_POINT('Ctrl Pts',(78.3427139812442,-8.80293468151543,133.959398129095));
#80039=CARTESIAN_POINT('Ctrl Pts',(78.333910218843,-8.90212409965979,133.965502759633));
#80040=CARTESIAN_POINT('Ctrl Pts',(78.3341019469804,-9.11275783268123,133.97837042487));
#80041=CARTESIAN_POINT('Ctrl Pts',(78.3453445221357,-9.22369359293837,133.985095487123));
#80042=CARTESIAN_POINT('Ctrl Pts',(78.3704604199684,-9.34694251898306,133.993274707298));
#80043=CARTESIAN_POINT('Ctrl Pts',(78.3735573037419,-9.36118205208093,133.994230845626));
#80044=CARTESIAN_POINT('Ctrl Pts',(78.3784090198239,-9.38216116708226,133.995658531687));
#80045=CARTESIAN_POINT('Ctrl Pts',(78.3800200633337,-9.3889337540938,133.996122369623));
#80046=CARTESIAN_POINT('Ctrl Pts',(78.3829713981018,-9.40100419364035,133.996954635746));
#80047=CARTESIAN_POINT('Ctrl Pts',(78.3842953736583,-9.40630582238773,133.997322136986));
#80048=CARTESIAN_POINT('Ctrl Pts',(78.3872818210453,-9.41801907315317,133.998138457141));
#80049=CARTESIAN_POINT('Ctrl Pts',(78.3889564343288,-9.42442725638386,133.998587933964));
#80050=CARTESIAN_POINT('Ctrl Pts',(78.3939939217679,-9.44324459776028,133.99991593539));
#80051=CARTESIAN_POINT('Ctrl Pts',(78.3974621934096,-9.45562468102995,134.000800073401));
#80052=CARTESIAN_POINT('Ctrl Pts',(78.4058039213543,-9.48412653831921,134.002857816002));
#80053=CARTESIAN_POINT('Ctrl Pts',(78.4107792144989,-9.50021684235532,134.004036066356));
#80054=CARTESIAN_POINT('Ctrl Pts',(78.4288217049656,-9.55557869467189,134.008141422183));
#80055=CARTESIAN_POINT('Ctrl Pts',(78.4431071607122,-9.59443516849589,134.011112654195));
#80056=CARTESIAN_POINT('Ctrl Pts',(78.5067068162444,-9.74935171683419,134.023229981363));
#80057=CARTESIAN_POINT('Ctrl Pts',(78.5676840530407,-9.86019250148546,134.032491050464));
#80058=CARTESIAN_POINT('Ctrl Pts',(78.6660828270149,-9.99908257765676,134.044461387281));
#80059=CARTESIAN_POINT('Ctrl Pts',(78.6929986494428,-10.034045024901,134.047515221621));
#80060=CARTESIAN_POINT('Ctrl Pts',(78.7312815510882,-10.079885786275,134.051577565385));
#80061=CARTESIAN_POINT('Ctrl Pts',(78.7414587074118,-10.0917296632852,134.052632808588));
#80062=CARTESIAN_POINT('Ctrl Pts',(78.7586276065021,-10.1111511197035,134.054373220408));
#80063=CARTESIAN_POINT('Ctrl Pts',(78.7655256728305,-10.1188098024058,134.055062205806));
#80064=CARTESIAN_POINT('Ctrl Pts',(78.7792395513224,-10.1337545818071,134.056412201371));
#80065=CARTESIAN_POINT('Ctrl Pts',(78.786050606249,-10.1410444345415,134.057073371456));
#80066=CARTESIAN_POINT('Ctrl Pts',(78.8025322309468,-10.1583700442849,134.058651517908));
#80067=CARTESIAN_POINT('Ctrl Pts',(78.8122641521326,-10.1683466063583,134.059565804759));
#80068=CARTESIAN_POINT('Ctrl Pts',(78.8469169595075,-10.2029899873905,134.062761953608));
#80069=CARTESIAN_POINT('Ctrl Pts',(78.8724912286758,-10.2269921173564,134.065014962686));
#80070=CARTESIAN_POINT('Ctrl Pts',(78.9383222979008,-10.2849784499329,134.070581416209));
#80071=CARTESIAN_POINT('Ctrl Pts',(78.9794690594892,-10.3178946790545,134.073855782634));
#80072=CARTESIAN_POINT('Ctrl Pts',(79.099820970463,-10.4051502913865,134.083006287883));
#80073=CARTESIAN_POINT('Ctrl Pts',(79.1822534347788,-10.4546679320136,134.088782062847));
#80074=CARTESIAN_POINT('Ctrl Pts',(79.314690556998,-10.5193918674606,134.097952697684));
#80075=CARTESIAN_POINT('Ctrl Pts',(79.3619104914205,-10.5398186077943,134.101205564474));
#80076=CARTESIAN_POINT('Ctrl Pts',(79.4202677956596,-10.5619178151596,134.105293034575));
#80077=CARTESIAN_POINT('Ctrl Pts',(79.4305796015699,-10.5657065766197,134.106017799103));
#80078=CARTESIAN_POINT('Ctrl Pts',(79.4468566749004,-10.5715050348482,134.107166888096));
#80079=CARTESIAN_POINT('Ctrl Pts',(79.4527973675493,-10.5735834545484,134.107587326072));
#80080=CARTESIAN_POINT('Ctrl Pts',(79.4639589397967,-10.5774176116596,134.108379480801));
#80081=CARTESIAN_POINT('Ctrl Pts',(79.4691769227751,-10.5791811792647,134.108750738425));
#80082=CARTESIAN_POINT('Ctrl Pts',(79.4814640451072,-10.5832661890077,134.109627062937));
#80083=CARTESIAN_POINT('Ctrl Pts',(79.488540090438,-10.5855661819649,134.110133340128));
#80084=CARTESIAN_POINT('Ctrl Pts',(79.5120477068619,-10.5930333507688,134.111820042482));
#80085=CARTESIAN_POINT('Ctrl Pts',(79.5285433797077,-10.5979928956034,134.113011331831));
#80086=CARTESIAN_POINT('Ctrl Pts',(79.5689573023215,-10.6094634473464,134.115943811591));
#80087=CARTESIAN_POINT('Ctrl Pts',(79.5929492856933,-10.6156979854235,134.117696385264));
#80088=CARTESIAN_POINT('Ctrl Pts',(79.6943247637283,-10.6396401545466,134.125127217116));
#80089=CARTESIAN_POINT('Ctrl Pts',(79.7727816911643,-10.6523402115628,134.130934563748));
#80090=CARTESIAN_POINT('Ctrl Pts',(79.9540413246789,-10.6685238374717,134.144159819736));
#80091=CARTESIAN_POINT('Ctrl Pts',(80.0568800574186,-10.6681891652364,134.151514439752));
#80092=CARTESIAN_POINT('Ctrl Pts',(80.1825333909696,-10.6561383297429,134.160204133224));
#80093=CARTESIAN_POINT('Ctrl Pts',(80.2059686214435,-10.6533873205866,134.161813055674));
#80094=CARTESIAN_POINT('Ctrl Pts',(80.2413485049412,-10.6484701766428,134.164225345702));
#80095=CARTESIAN_POINT('Ctrl Pts',(80.2533401055619,-10.6466699209363,134.165040057024));
#80096=CARTESIAN_POINT('Ctrl Pts',(80.2749078565126,-10.6431908475222,134.166500451282));
#80097=CARTESIAN_POINT('Ctrl Pts',(80.2844908872714,-10.6415588423463,134.167147579108));
#80098=CARTESIAN_POINT('Ctrl Pts',(80.3049968852284,-10.6378816741444,134.168528793037));
#80099=CARTESIAN_POINT('Ctrl Pts',(80.3159148275612,-10.6358109029731,134.16926203472));
#80100=CARTESIAN_POINT('Ctrl Pts',(80.3458290767552,-10.6298264919091,134.171265694674));
#80101=CARTESIAN_POINT('Ctrl Pts',(80.3647794188693,-10.6256900598178,134.172529013322));
#80102=CARTESIAN_POINT('Ctrl Pts',(80.4949920291305,-10.594875942142,134.181177454284));
#80103=CARTESIAN_POINT('Ctrl Pts',(80.6033241737846,-10.557129006175,134.188181788303));
#80104=CARTESIAN_POINT('Ctrl Pts',(80.8003169804827,-10.4648146621754,134.201466215994));
#80105=CARTESIAN_POINT('Ctrl Pts',(80.8894139033819,-10.4124894138518,134.207730747794));
#80106=CARTESIAN_POINT('Ctrl Pts',(80.9853716031139,-10.3434387685317,134.215410068768));
#80107=CARTESIAN_POINT('Ctrl Pts',(80.9975311048848,-10.3344349277599,134.216402014125));
#80108=CARTESIAN_POINT('Ctrl Pts',(81.0151871878791,-10.3209848265773,134.217873028519));
#80109=CARTESIAN_POINT('Ctrl Pts',(81.0207811777829,-10.3166668982845,134.218343699755));
#80110=CARTESIAN_POINT('Ctrl Pts',(81.0306566903959,-10.3089433582546,134.219183168925));
#80111=CARTESIAN_POINT('Ctrl Pts',(81.0349491502649,-10.3055520607704,134.219550969869));
#80112=CARTESIAN_POINT('Ctrl Pts',(81.0443358284447,-10.2980606444942,134.220361778326));
#80113=CARTESIAN_POINT('Ctrl Pts',(81.0494225692489,-10.2939517096269,134.220805384279));
#80114=CARTESIAN_POINT('Ctrl Pts',(81.0641201940356,-10.2819356865279,134.222099122877));
#80115=CARTESIAN_POINT('Ctrl Pts',(81.073666583166,-10.2739509162153,134.222954454908));
#80116=CARTESIAN_POINT('Ctrl Pts',(81.1510007894549,-10.2077805783689,134.230001198648));
#80117=CARTESIAN_POINT('Ctrl Pts',(81.2140906708677,-10.1443413753495,134.236491412577));
#80118=CARTESIAN_POINT('Ctrl Pts',(81.3534985039486,-9.97959189862281,134.252200637322));
#80119=CARTESIAN_POINT('Ctrl Pts',(81.4239632906421,-9.87401288515521,134.261353426494));
#80120=CARTESIAN_POINT('Ctrl Pts',(81.4912166869833,-9.74313731362072,134.271469742676));
#80121=CARTESIAN_POINT('Ctrl Pts',(81.5002908954914,-9.7246430632648,134.272874266104));
#80122=CARTESIAN_POINT('Ctrl Pts',(81.5143544762918,-9.69458259381862,134.275118052451));
#80123=CARTESIAN_POINT('Ctrl Pts',(81.5195595239156,-9.68312028799751,134.275964647412));
#80124=CARTESIAN_POINT('Ctrl Pts',(81.5285715573802,-9.66266159373057,134.277460189477));
#80125=CARTESIAN_POINT('Ctrl Pts',(81.5324302254004,-9.65368876776061,134.278110875941));
#80126=CARTESIAN_POINT('Ctrl Pts',(81.5404004165549,-9.63469664577142,134.279477387173));
#80127=CARTESIAN_POINT('Ctrl Pts',(81.5444936163413,-9.62467011605464,134.28019256751));
#80128=CARTESIAN_POINT('Ctrl Pts',(81.5551549834062,-9.59780891275826,134.28209244906));
#80129=CARTESIAN_POINT('Ctrl Pts',(81.5615476367147,-9.58090579129727,134.283271260448));
#80130=CARTESIAN_POINT('Ctrl Pts',(81.5951923770168,-9.48737232862071,134.289708546599));
#80131=CARTESIAN_POINT('Ctrl Pts',(81.617081706908,-9.40892510205804,134.294786678539));
#80132=CARTESIAN_POINT('Ctrl Pts',(81.6427292892478,-9.28168176460839,134.30276976461));
#80133=CARTESIAN_POINT('Ctrl Pts',(81.6502270476375,-9.23378391083949,134.305721165263));
#80134=CARTESIAN_POINT('Ctrl Pts',(81.6561283783128,-9.18114937776188,134.308957527548));
#80135=CARTESIAN_POINT('Ctrl Pts',(81.6566122533579,-9.17666959113448,134.309232930461));
#80136=CARTESIAN_POINT('Ctrl Pts',(81.665819090058,-9.08806611875033,134.314679870135));
#80137=CARTESIAN_POINT('Ctrl Pts',(81.6681407894447,-9.0034108967471,134.319877501067));
#80138=CARTESIAN_POINT('Ctrl Pts',(81.6632588291239,-8.90317093516773,134.326388483428));
#80139=CARTESIAN_POINT('Ctrl Pts',(81.662265418857,-8.88739701077373,134.327423710482));
#80140=CARTESIAN_POINT('Ctrl Pts',(81.6604996645589,-8.86454713856628,134.328941880589));
#80141=CARTESIAN_POINT('Ctrl Pts',(81.6599061125614,-8.85745770260244,134.329415506386));
#80142=CARTESIAN_POINT('Ctrl Pts',(81.658774571574,-8.84490968721675,134.330258751075));
#80143=CARTESIAN_POINT('Ctrl Pts',(81.6582550064039,-8.83944964373234,134.330627347597));
#80144=CARTESIAN_POINT('Ctrl Pts',(81.657068918047,-8.8276056949357,134.331430639946));
#80145=CARTESIAN_POINT('Ctrl Pts',(81.6563924739572,-8.82122314378105,134.331865847696));
#80146=CARTESIAN_POINT('Ctrl Pts',(81.6543602448719,-8.80305071695764,134.333111294929));
#80147=CARTESIAN_POINT('Ctrl Pts',(81.6529153717143,-8.79127148312748,134.333926175283));
#80148=CARTESIAN_POINT('Ctrl Pts',(81.6387310570383,-8.68503944927931,134.341337928602));
#80149=CARTESIAN_POINT('Ctrl Pts',(81.6180353018436,-8.59183635437831,134.348278623742));
#80150=CARTESIAN_POINT('Ctrl Pts',(81.5533134672623,-8.38570580150564,134.364005803122));
#80151=CARTESIAN_POINT('Ctrl Pts',(81.5047095036511,-8.2747417854604,134.372725095181));
#80152=CARTESIAN_POINT('Ctrl Pts',(81.4340586983671,-8.15178253447627,134.382480412671));
#80153=CARTESIAN_POINT('Ctrl Pts',(81.4232499552787,-8.13376859112513,134.383913329452));
#80154=CARTESIAN_POINT('Ctrl Pts',(81.4054335571921,-8.10530983544477,134.38618396905));
#80155=CARTESIAN_POINT('Ctrl Pts',(81.39864363339,-8.09473209708972,134.387029505684));
#80156=CARTESIAN_POINT('Ctrl Pts',(81.3863522606568,-8.07605233703291,134.38852583832));
#80157=CARTESIAN_POINT('Ctrl Pts',(81.380897929932,-8.06792018116672,134.389178346512));
#80158=CARTESIAN_POINT('Ctrl Pts',(81.3693166942414,-8.05097790725196,134.390540292577));
#80159=CARTESIAN_POINT('Ctrl Pts',(81.3631757100119,-8.04217792133702,134.391249159608));
#80160=CARTESIAN_POINT('Ctrl Pts',(81.3467340951886,-8.01909565391363,134.39311286582));
#80161=CARTESIAN_POINT('Ctrl Pts',(81.3362911425038,-8.00491604360166,134.394262214612));
#80162=CARTESIAN_POINT('Ctrl Pts',(81.2816007757981,-7.93307061648487,134.400113877658));
#80163=CARTESIAN_POINT('Ctrl Pts',(81.2338361142941,-7.87817594252731,134.404674862731));
#80164=CARTESIAN_POINT('Ctrl Pts',(81.1105600652069,-7.7539328981265,134.41548111725));
#80165=CARTESIAN_POINT('Ctrl Pts',(81.0319516515263,-7.68809252785914,134.42162563817));
#80166=CARTESIAN_POINT('Ctrl Pts',(80.9048458900799,-7.60016488358483,134.431235225722));
#80167=CARTESIAN_POINT('Ctrl Pts',(80.8605188925679,-7.57248799874148,134.434537085882));
#80168=CARTESIAN_POINT('Ctrl Pts',(80.8053511394162,-7.5415463042026,134.438679869126));
#80169=CARTESIAN_POINT('Ctrl Pts',(80.7956787335038,-7.53624695471797,134.439407424297));
#80170=CARTESIAN_POINT('Ctrl Pts',(80.7803966829641,-7.52807039814425,134.440559975802));
#80171=CARTESIAN_POINT('Ctrl Pts',(80.7748218995872,-7.52512822379691,134.440981047197));
#80172=CARTESIAN_POINT('Ctrl Pts',(80.7643467318049,-7.51967557967916,134.441773681179));
#80173=CARTESIAN_POINT('Ctrl Pts',(80.7594504365315,-7.51715767974026,134.442144777272));
#80174=CARTESIAN_POINT('Ctrl Pts',(80.7479235359005,-7.51130208252279,134.44301975126));
#80175=CARTESIAN_POINT('Ctrl Pts',(80.7412830120814,-7.50798438486794,134.443524827989));
#80176=CARTESIAN_POINT('Ctrl Pts',(80.7192513201532,-7.49716043065008,134.445203353457));
#80177=CARTESIAN_POINT('Ctrl Pts',(80.7037671705056,-7.48984737672318,134.446387527633));
#80178=CARTESIAN_POINT('Ctrl Pts',(80.6657785498853,-7.47261672975433,134.449298859705));
#80179=CARTESIAN_POINT('Ctrl Pts',(80.6431622682002,-7.46295644185148,134.451037202124));
#80180=CARTESIAN_POINT('Ctrl Pts',(80.547770340733,-7.42468479288244,134.458367726801));
#80181=CARTESIAN_POINT('Ctrl Pts',(80.4732420488356,-7.40071533541414,134.46408611378));
#80182=CARTESIAN_POINT('Ctrl Pts',(80.2961574665958,-7.35722933801795,134.477341278724));
#80183=CARTESIAN_POINT('Ctrl Pts',(80.1928842189041,-7.3419266974643,134.484811850572));
#80184=CARTESIAN_POINT('Ctrl Pts',(80.065298487664,-7.33511320407712,134.493607237537));
#80185=CARTESIAN_POINT('Ctrl Pts',(80.0417287266177,-7.33435575594236,134.495215169867));
#80186=CARTESIAN_POINT('Ctrl Pts',(80.0060280428315,-7.33396680231363,134.497626284443));
#80187=CARTESIAN_POINT('Ctrl Pts',(79.993904991723,-7.33396704191,134.498440793903));
#80188=CARTESIAN_POINT('Ctrl Pts',(79.972062903696,-7.33420589352749,134.499900969763));
#80189=CARTESIAN_POINT('Ctrl Pts',(79.9623440119483,-7.3343972502591,134.500548079191));
#80190=CARTESIAN_POINT('Ctrl Pts',(79.9415175349273,-7.33498969216655,134.501929406787));
#80191=CARTESIAN_POINT('Ctrl Pts',(79.9304111187463,-7.33541689255676,134.502662779132));
#80192=CARTESIAN_POINT('Ctrl Pts',(79.8999282801208,-7.33689502169682,134.504667193256));
#80193=CARTESIAN_POINT('Ctrl Pts',(79.8805642575413,-7.33817339278846,134.505931126263));
#80194=CARTESIAN_POINT('Ctrl Pts',(79.8374722021615,-7.34177537256366,134.508725958328));
#80195=CARTESIAN_POINT('Ctrl Pts',(79.8137626135259,-7.34427057735474,134.51025155281));
#80196=CARTESIAN_POINT('Ctrl Pts',(79.7379413646647,-7.35389941536268,134.515101318387));
#80197=CARTESIAN_POINT('Ctrl Pts',(79.6861094692054,-7.3629919909374,134.51837155516));
#80198=CARTESIAN_POINT('Ctrl Pts',(79.5411252078008,-7.39556671760973,134.527519029308));
#80199=CARTESIAN_POINT('Ctrl Pts',(79.4494578137711,-7.42466697126672,134.533295575406));
#80200=CARTESIAN_POINT('Ctrl Pts',(79.3132519982137,-7.48125533530951,134.542470969164));
#80201=CARTESIAN_POINT('Ctrl Pts',(79.2666405046927,-7.5032064579193,134.545728190481));
#80202=CARTESIAN_POINT('Ctrl Pts',(79.2114010581597,-7.53242079546742,134.54982124773));
#80203=CARTESIAN_POINT('Ctrl Pts',(79.2017281898612,-7.5376597133766,134.550546960634));
#80204=CARTESIAN_POINT('Ctrl Pts',(79.1866010131659,-7.54604754457162,134.551697226376));
#80205=CARTESIAN_POINT('Ctrl Pts',(79.1811112670207,-7.54913236504575,134.552117879677));
#80206=CARTESIAN_POINT('Ctrl Pts',(79.1708533227672,-7.55497331540321,134.552910196809));
#80207=CARTESIAN_POINT('Ctrl Pts',(79.1660811426601,-7.5577220561197,134.553281399005));
#80208=CARTESIAN_POINT('Ctrl Pts',(79.1548988444578,-7.56423702828533,134.554157262092));
#80209=CARTESIAN_POINT('Ctrl Pts',(79.148500218352,-7.56802255931892,134.554663129371));
#80210=CARTESIAN_POINT('Ctrl Pts',(79.127391119667,-7.58070254978715,134.556347036359));
#80211=CARTESIAN_POINT('Ctrl Pts',(79.1127935337693,-7.58978152791956,134.55753589272));
#80212=CARTESIAN_POINT('Ctrl Pts',(79.0775530574905,-7.61246307526759,134.560461136249));
#80213=CARTESIAN_POINT('Ctrl Pts',(79.0570677708726,-7.6263021584186,134.562208838476));
#80214=CARTESIAN_POINT('Ctrl Pts',(78.9724600075178,-7.68624424950195,134.569605193289));
#80215=CARTESIAN_POINT('Ctrl Pts',(78.9113510744778,-7.73641966397281,134.575381941928));
#80216=CARTESIAN_POINT('Ctrl Pts',(78.7791702891653,-7.86168177330922,134.588617446902));
#80217=CARTESIAN_POINT('Ctrl Pts',(78.7110461167117,-7.93943506442631,134.596011862628));
#80218=CARTESIAN_POINT('Ctrl Pts',(78.6367110615838,-8.0421087470549,134.604737857928));
#80219=CARTESIAN_POINT('Ctrl Pts',(78.6232851714385,-8.06150718613825,134.606346449602));
#80220=CARTESIAN_POINT('Ctrl Pts',(78.6035884391703,-8.09129886476789,134.608758346948));
#80221=CARTESIAN_POINT('Ctrl Pts',(78.5970121880381,-8.10148555194778,134.60957299084));
#80222=CARTESIAN_POINT('Ctrl Pts',(78.585364884483,-8.11996705776851,134.611033312138));
#80223=CARTESIAN_POINT('Ctrl Pts',(78.5802541766147,-8.1282361023082,134.611680433811));
#80224=CARTESIAN_POINT('Ctrl Pts',(78.5694565408014,-8.14605333597346,134.613061685677));
#80225=CARTESIAN_POINT('Ctrl Pts',(78.5637921615218,-8.15561469197104,134.613794970981));
#80226=CARTESIAN_POINT('Ctrl Pts',(78.548504349547,-8.18201916551864,134.615798882702));
#80227=CARTESIAN_POINT('Ctrl Pts',(78.5390785519315,-8.1989751299592,134.617062406442));
#80228=CARTESIAN_POINT('Ctrl Pts',(78.4940698695076,-8.28337919127685,134.623244806254));
#80229=CARTESIAN_POINT('Ctrl Pts',(78.4628720992874,-8.35301021093932,134.62800685597));
#80230=CARTESIAN_POINT('Ctrl Pts',(78.4365594680555,-8.42449178713676,134.632696249083));
#80231=CARTESIAN_POINT('Origin',(80.,-9.,134.));
#80232=CARTESIAN_POINT('',(78.4365593749993,-8.42449203993567,135.330578627164));
#80233=CARTESIAN_POINT('',(78.4365593350865,-8.42449214836376,135.139259965645));
#80234=CARTESIAN_POINT('',(78.4365593749993,-8.42449203993574,134.));
#80235=CARTESIAN_POINT('',(78.3340005883416,-8.9985998736709,134.47795669959));
#80236=CARTESIAN_POINT('Ctrl Pts',(78.4365593350865,-8.42449214836376,135.139259965645));
#80237=CARTESIAN_POINT('Ctrl Pts',(78.4595770340976,-8.36196162589672,135.135189971337));
#80238=CARTESIAN_POINT('Ctrl Pts',(78.4863351525883,-8.30084183598527,135.13113531974));
#80239=CARTESIAN_POINT('Ctrl Pts',(78.5389131195365,-8.19802641900077,135.123936636303));
#80240=CARTESIAN_POINT('Ctrl Pts',(78.5630228224522,-8.15558770865141,135.120844126155));
#80241=CARTESIAN_POINT('Ctrl Pts',(78.5947307026104,-8.10507422314614,135.116936330962));
#80242=CARTESIAN_POINT('Ctrl Pts',(78.6005941427007,-8.09593298064479,135.116219691288));
#80243=CARTESIAN_POINT('Ctrl Pts',(78.6099810250474,-8.08160873406148,135.115080616419));
#80244=CARTESIAN_POINT('Ctrl Pts',(78.6134451839667,-8.07638698201634,135.114661956085));
#80245=CARTESIAN_POINT('Ctrl Pts',(78.6200142423709,-8.06660525923144,135.113870983743));
#80246=CARTESIAN_POINT('Ctrl Pts',(78.6231124327411,-8.06204101535449,135.113499108902));
#80247=CARTESIAN_POINT('Ctrl Pts',(78.6304738953643,-8.05131120036578,135.11261835153));
#80248=CARTESIAN_POINT('Ctrl Pts',(78.6347561744854,-8.04515892352745,135.112108222604));
#80249=CARTESIAN_POINT('Ctrl Pts',(78.6491994291896,-8.02470434223818,135.110395571658));
#80250=CARTESIAN_POINT('Ctrl Pts',(78.6595443985481,-8.01053422404222,135.109181741546));
#80251=CARTESIAN_POINT('Ctrl Pts',(78.6854151106593,-7.97624798498357,135.106182101068));
#80252=CARTESIAN_POINT('Ctrl Pts',(78.7011807578211,-7.95631898755379,135.104384266743));
#80253=CARTESIAN_POINT('Ctrl Pts',(78.7705317998867,-7.87265966126243,135.096626423372));
#80254=CARTESIAN_POINT('Ctrl Pts',(78.8283971268501,-7.81263558804286,135.090527875419));
#80255=CARTESIAN_POINT('Ctrl Pts',(78.9696097783315,-7.68657062137669,135.076784213937));
#80256=CARTESIAN_POINT('Ctrl Pts',(79.0552887227416,-7.62365381658308,135.069213978658));
#80257=CARTESIAN_POINT('Ctrl Pts',(79.1624696559496,-7.55970495399906,135.060679224766));
#80258=CARTESIAN_POINT('Ctrl Pts',(79.1787174599824,-7.55037869224015,135.059408006955));
#80259=CARTESIAN_POINT('Ctrl Pts',(79.2048190648998,-7.53597609231756,135.057400662815));
#80260=CARTESIAN_POINT('Ctrl Pts',(79.2145717717768,-7.5307208466782,135.056658206746));
#80261=CARTESIAN_POINT('Ctrl Pts',(79.2329036191681,-7.52107742659557,135.055276452319));
#80262=CARTESIAN_POINT('Ctrl Pts',(79.2414697617659,-7.51666567491935,135.054636342653));
#80263=CARTESIAN_POINT('Ctrl Pts',(79.2609113985985,-7.50686526475417,135.053195796726));
#80264=CARTESIAN_POINT('Ctrl Pts',(79.2718085506382,-7.50152059593467,135.052396920712));
#80265=CARTESIAN_POINT('Ctrl Pts',(79.3048175879237,-7.4857759544867,135.050001821179));
#80266=CARTESIAN_POINT('Ctrl Pts',(79.3271014070675,-7.47574259752548,135.048418177598));
#80267=CARTESIAN_POINT('Ctrl Pts',(79.3791768156469,-7.45366021107353,135.04478686273));
#80268=CARTESIAN_POINT('Ctrl Pts',(79.4091126373617,-7.44197545474172,135.042750884785));
#80269=CARTESIAN_POINT('Ctrl Pts',(79.5207988426877,-7.40206388665551,135.035311150927));
#80270=CARTESIAN_POINT('Ctrl Pts',(79.6043718861882,-7.37934794847096,135.030054782485));
#80271=CARTESIAN_POINT('Ctrl Pts',(79.7073523961798,-7.35980192515111,135.023650091205));
#80272=CARTESIAN_POINT('Ctrl Pts',(79.7254255209208,-7.35667982746918,135.022528339556));
#80273=CARTESIAN_POINT('Ctrl Pts',(79.8200902975363,-7.34193194448609,135.016649596042));
#80274=CARTESIAN_POINT('Ctrl Pts',(79.8973630934295,-7.3353619991716,135.011842704575));
#80275=CARTESIAN_POINT('Ctrl Pts',(79.9864107022758,-7.33401496225293,135.006017625944));
#80276=CARTESIAN_POINT('Ctrl Pts',(79.9980214807866,-7.33396072017218,135.005252480809));
#80277=CARTESIAN_POINT('Ctrl Pts',(80.0160665085711,-7.33406504378312,135.004053263937));
#80278=CARTESIAN_POINT('Ctrl Pts',(80.0225011376284,-7.33413952974075,135.003623650212));
#80279=CARTESIAN_POINT('Ctrl Pts',(80.034366383432,-7.33434563606311,135.002827523103));
#80280=CARTESIAN_POINT('Ctrl Pts',(80.0397969859595,-7.33446654034419,135.002461601358));
#80281=CARTESIAN_POINT('Ctrl Pts',(80.0524093383324,-7.33480905382207,135.001608224779));
#80282=CARTESIAN_POINT('Ctrl Pts',(80.0595903096703,-7.33505056647917,135.001119702819));
#80283=CARTESIAN_POINT('Ctrl Pts',(80.0825245838325,-7.3359704568226,134.999551511326));
#80284=CARTESIAN_POINT('Ctrl Pts',(80.0982693737121,-7.33682601251735,134.998462902655));
#80285=CARTESIAN_POINT('Ctrl Pts',(80.1851183459718,-7.34278276466411,134.992400142951));
#80286=CARTESIAN_POINT('Ctrl Pts',(80.2558446351054,-7.35221989060694,134.987251230197));
#80287=CARTESIAN_POINT('Ctrl Pts',(80.4539862530033,-7.39172361223971,134.97256368386));
#80288=CARTESIAN_POINT('Ctrl Pts',(80.5787995948267,-7.43230774268162,134.963037279015));
#80289=CARTESIAN_POINT('Ctrl Pts',(80.7233827361843,-7.49897369665789,134.952018346345));
#80290=CARTESIAN_POINT('Ctrl Pts',(80.7488659444659,-7.51152342479597,134.950074444951));
#80291=CARTESIAN_POINT('Ctrl Pts',(80.7852864668139,-7.53063172832563,134.947292001966));
#80292=CARTESIAN_POINT('Ctrl Pts',(80.7964878339778,-7.53667327684771,134.946435629892));
#80293=CARTESIAN_POINT('Ctrl Pts',(80.8162048154638,-7.54760127492435,134.944926772722));
#80294=CARTESIAN_POINT('Ctrl Pts',(80.8247484102004,-7.55243569249882,134.944272477817));
#80295=CARTESIAN_POINT('Ctrl Pts',(80.842479489308,-7.56267681544452,134.94291330907));
#80296=CARTESIAN_POINT('Ctrl Pts',(80.8516588370472,-7.56809676969414,134.94220894986));
#80297=CARTESIAN_POINT('Ctrl Pts',(80.8755715024308,-7.58252732676567,134.940371699113));
#80298=CARTESIAN_POINT('Ctrl Pts',(80.8902180870378,-7.59167971358375,134.939244010435));
#80299=CARTESIAN_POINT('Ctrl Pts',(80.9612666525135,-7.63762807468132,134.93375756812));
#80300=CARTESIAN_POINT('Ctrl Pts',(81.015547792024,-7.67759495096403,134.929518629652));
#80301=CARTESIAN_POINT('Ctrl Pts',(81.122311087216,-7.76666597919458,134.920909803424));
#80302=CARTESIAN_POINT('Ctrl Pts',(81.1743361769062,-7.81609551483648,134.916558264143));
#80303=CARTESIAN_POINT('Ctrl Pts',(81.2383180250598,-7.88526581017985,134.910793193035));
#80304=CARTESIAN_POINT('Ctrl Pts',(81.2532829691558,-7.90211766856884,134.909411218824));
#80305=CARTESIAN_POINT('Ctrl Pts',(81.3103994202164,-7.96912594926011,134.903981163259));
#80306=CARTESIAN_POINT('Ctrl Pts',(81.3499147443503,-8.02144184902819,134.899881128447));
#80307=CARTESIAN_POINT('Ctrl Pts',(81.392605451346,-8.08548502962895,134.894845224273));
#80308=CARTESIAN_POINT('Ctrl Pts',(81.3988687358981,-8.09509458175673,134.894089145168));
#80309=CARTESIAN_POINT('Ctrl Pts',(81.4084732152304,-8.11016843659735,134.892901158263));
#80310=CARTESIAN_POINT('Ctrl Pts',(81.4118831098485,-8.11558884564656,134.892473577062));
#80311=CARTESIAN_POINT('Ctrl Pts',(81.4181300451258,-8.12564724829787,134.891679146676));
#80312=CARTESIAN_POINT('Ctrl Pts',(81.4209757364171,-8.13027963537631,134.891312866394));
#80313=CARTESIAN_POINT('Ctrl Pts',(81.4275538993163,-8.1411064291571,134.890455905735));
#80314=CARTESIAN_POINT('Ctrl Pts',(81.4312687480956,-8.14731127172097,134.88996412713));
#80315=CARTESIAN_POINT('Ctrl Pts',(81.4430862385932,-8.16734461569995,134.888374731461));
#80316=CARTESIAN_POINT('Ctrl Pts',(81.4510294824002,-8.18126544286772,134.887267845065));
#80317=CARTESIAN_POINT('Ctrl Pts',(81.4696384076648,-8.21499985460932,134.884583553367));
#80318=CARTESIAN_POINT('Ctrl Pts',(81.4801057423278,-8.23491884976268,134.882996987279));
#80319=CARTESIAN_POINT('Ctrl Pts',(81.519902073269,-8.31452493314344,134.876666651372));
#80320=CARTESIAN_POINT('Ctrl Pts',(81.5460485064376,-8.37573123773124,134.87182468724));
#80321=CARTESIAN_POINT('Ctrl Pts',(81.6090637709776,-8.5517024548868,134.858218677217));
#80322=CARTESIAN_POINT('Ctrl Pts',(81.6372573948194,-8.66915996472706,134.849525409811));
#80323=CARTESIAN_POINT('Ctrl Pts',(81.6552067644714,-8.80950415929666,134.839792101912));
#80324=CARTESIAN_POINT('Ctrl Pts',(81.6574792126088,-8.83040982282763,134.838357725663));
#80325=CARTESIAN_POINT('Ctrl Pts',(81.660477499567,-8.86388005071383,134.836085119794));
#80326=CARTESIAN_POINT('Ctrl Pts',(81.6614577644362,-8.87641893667384,134.835239057551));
#80327=CARTESIAN_POINT('Ctrl Pts',(81.6629487579776,-8.89874108815865,134.833741979593));
#80328=CARTESIAN_POINT('Ctrl Pts',(81.6635153548643,-8.90851989254091,134.833089248116));
#80329=CARTESIAN_POINT('Ctrl Pts',(81.6645219276044,-8.9290217347799,134.831727015136));
#80330=CARTESIAN_POINT('Ctrl Pts',(81.6649446026819,-8.93974520184122,134.831018083247));
#80331=CARTESIAN_POINT('Ctrl Pts',(81.6657869838347,-8.9680684317809,134.829154604133));
#80332=CARTESIAN_POINT('Ctrl Pts',(81.6660314095419,-8.98567235349846,134.828005542342));
#80333=CARTESIAN_POINT('Ctrl Pts',(81.6658540375682,-9.07583549934513,134.822162228331));
#80334=CARTESIAN_POINT('Ctrl Pts',(81.6609714707634,-9.14831175867685,134.817608774634));
#80335=CARTESIAN_POINT('Ctrl Pts',(81.6378978560055,-9.32131475564214,134.806832053501));
#80336=CARTESIAN_POINT('Ctrl Pts',(81.6151690677491,-9.42092759131997,134.800708601513));
#80337=CARTESIAN_POINT('Ctrl Pts',(81.5763225683016,-9.53971583289705,134.792940495281));
#80338=CARTESIAN_POINT('Ctrl Pts',(81.5687141664789,-9.56144617366989,134.791498863826));
#80339=CARTESIAN_POINT('Ctrl Pts',(81.5493296563802,-9.61333643402813,134.787991250943));
#80340=CARTESIAN_POINT('Ctrl Pts',(81.5371204641159,-9.64332287388392,134.78591034512));
#80341=CARTESIAN_POINT('Ctrl Pts',(81.5201208374032,-9.68182336657085,134.783144035793));
#80342=CARTESIAN_POINT('Ctrl Pts',(81.5161174225967,-9.69067967481296,134.782501054123));
#80343=CARTESIAN_POINT('Ctrl Pts',(81.5095368241562,-9.70490427073001,134.781456765782));
#80344=CARTESIAN_POINT('Ctrl Pts',(81.5070078751695,-9.71029480904442,134.781058321519));
#80345=CARTESIAN_POINT('Ctrl Pts',(81.5020267713931,-9.72076584433124,134.780278852064));
#80346=CARTESIAN_POINT('Ctrl Pts',(81.4995776259497,-9.72584761789911,134.779898006205));
#80347=CARTESIAN_POINT('Ctrl Pts',(81.493485822658,-9.73832517572923,134.77895675164));
#80348=CARTESIAN_POINT('Ctrl Pts',(81.48981401351,-9.74570648760143,134.778394597122));
#80349=CARTESIAN_POINT('Ctrl Pts',(81.4759487384856,-9.77306820235624,134.776291644873));
#80350=CARTESIAN_POINT('Ctrl Pts',(81.4654073624579,-9.79286837816158,134.774731713571));
#80351=CARTESIAN_POINT('Ctrl Pts',(81.3834394928083,-9.9396097685221,134.76291457146));
#80352=CARTESIAN_POINT('Ctrl Pts',(81.2960409403727,-10.0569072463972,134.752078366232));
#80353=CARTESIAN_POINT('Ctrl Pts',(81.1491877331454,-10.2079521638097,134.737037184466));
#80354=CARTESIAN_POINT('Ctrl Pts',(81.10118473183,-10.2518685882026,134.732484196918));
#80355=CARTESIAN_POINT('Ctrl Pts',(81.0370589315132,-10.3039843576651,134.726844988755));
#80356=CARTESIAN_POINT('Ctrl Pts',(81.0232100676481,-10.3148793219644,134.725651243418));
#80357=CARTESIAN_POINT('Ctrl Pts',(81.0006495310242,-10.3320554595426,134.723744217125));
#80358=CARTESIAN_POINT('Ctrl Pts',(80.9920457458399,-10.3384754307517,134.723025518288));
#80359=CARTESIAN_POINT('Ctrl Pts',(80.9754745608034,-10.3505929448306,134.721657295945));
#80360=CARTESIAN_POINT('Ctrl Pts',(80.9675178243394,-10.3563042387219,134.721007258458));
#80361=CARTESIAN_POINT('Ctrl Pts',(80.9490601134014,-10.3693079764402,134.719514893307));
#80362=CARTESIAN_POINT('Ctrl Pts',(80.938524552036,-10.3765504398901,134.718674492941));
#80363=CARTESIAN_POINT('Ctrl Pts',(80.9046989976945,-10.3992342621798,134.716011371556));
#80364=CARTESIAN_POINT('Ctrl Pts',(80.8811027039194,-10.4142117832447,134.714205886392));
#80365=CARTESIAN_POINT('Ctrl Pts',(80.7918224145945,-10.4677790839561,134.707549490834));
#80366=CARTESIAN_POINT('Ctrl Pts',(80.7238909448072,-10.5024452759759,134.702833216025));
#80367=CARTESIAN_POINT('Ctrl Pts',(80.5732190554284,-10.566733879394,134.692794054025));
#80368=CARTESIAN_POINT('Ctrl Pts',(80.490035263764,-10.5947097196123,134.687502989554));
#80369=CARTESIAN_POINT('Ctrl Pts',(80.359676118395,-10.6273833155937,134.679111837194));
#80370=CARTESIAN_POINT('Ctrl Pts',(80.3138558079837,-10.6368375086744,134.67614267141));
#80371=CARTESIAN_POINT('Ctrl Pts',(80.2569633293007,-10.6460997097192,134.672364915299));
#80372=CARTESIAN_POINT('Ctrl Pts',(80.2462067104766,-10.6477428947505,134.671646672907));
#80373=CARTESIAN_POINT('Ctrl Pts',(80.2292889368182,-10.6501579102668,134.670509689661));
#80374=CARTESIAN_POINT('Ctrl Pts',(80.2231380210954,-10.6510008981709,134.670094787554));
#80375=CARTESIAN_POINT('Ctrl Pts',(80.2114974742476,-10.652530007249,134.669306469576));
#80376=CARTESIAN_POINT('Ctrl Pts',(80.2060089587909,-10.6532231887014,134.668933446066));
#80377=CARTESIAN_POINT('Ctrl Pts',(80.1929643506541,-10.6548047145764,134.668043817711));
#80378=CARTESIAN_POINT('Ctrl Pts',(80.1854055028075,-10.6556686497899,134.667525892015));
#80379=CARTESIAN_POINT('Ctrl Pts',(80.1597269056849,-10.658425525904,134.665758804767));
#80380=CARTESIAN_POINT('Ctrl Pts',(80.1415828476452,-10.6600729318058,134.664497369311));
#80381=CARTESIAN_POINT('Ctrl Pts',(80.096744043622,-10.6634037180127,134.661354170434));
#80382=CARTESIAN_POINT('Ctrl Pts',(80.0700293014619,-10.6647423454954,134.659458949532));
#80383=CARTESIAN_POINT('Ctrl Pts',(79.9510027949963,-10.6678366140256,134.650945512812));
#80384=CARTESIAN_POINT('Ctrl Pts',(79.8586724262388,-10.662560037362,134.644166627032));
#80385=CARTESIAN_POINT('Ctrl Pts',(79.6731949992742,-10.6363917693144,134.630607560278));
#80386=CARTESIAN_POINT('Ctrl Pts',(79.5804286110354,-10.6150990359347,134.623859740041));
#80387=CARTESIAN_POINT('Ctrl Pts',(79.4720877813883,-10.5802586871293,134.61607940845));
#80388=CARTESIAN_POINT('Ctrl Pts',(79.4543038474139,-10.5742060182796,134.614805053408));
#80389=CARTESIAN_POINT('Ctrl Pts',(79.4262884620084,-10.5641392906645,134.612801178886));
#80390=CARTESIAN_POINT('Ctrl Pts',(79.4159882727425,-10.5603227108047,134.612065215707));
#80391=CARTESIAN_POINT('Ctrl Pts',(79.3975363748909,-10.5532773208182,134.610747960638));
#80392=CARTESIAN_POINT('Ctrl Pts',(79.3893710645594,-10.5500855341478,134.610165462149));
#80393=CARTESIAN_POINT('Ctrl Pts',(79.370228935208,-10.5424282239076,134.608800660836));
#80394=CARTESIAN_POINT('Ctrl Pts',(79.3592737166715,-10.5379097053935,134.608020169134));
#80395=CARTESIAN_POINT('Ctrl Pts',(79.3272287948392,-10.5242908037662,134.605738173161));
#80396=CARTESIAN_POINT('Ctrl Pts',(79.3062774531805,-10.5148705093417,134.604247508801));
#80397=CARTESIAN_POINT('Ctrl Pts',(79.2098572990438,-10.4690972710692,134.597382672941));
#80398=CARTESIAN_POINT('Ctrl Pts',(79.137000274639,-10.4275174697447,134.592189834619));
#80399=CARTESIAN_POINT('Ctrl Pts',(78.9951464206837,-10.3317145130248,134.581699221926));
#80400=CARTESIAN_POINT('Ctrl Pts',(78.9266847645311,-10.2771793958034,134.576422095966));
#80401=CARTESIAN_POINT('Ctrl Pts',(78.828397737918,-10.1853787209171,134.568027029418));
#80402=CARTESIAN_POINT('Ctrl Pts',(78.7953576185797,-10.1517857530904,134.565037550925));
#80403=CARTESIAN_POINT('Ctrl Pts',(78.7564814841443,-10.1087544805613,134.561237001151));
#80404=CARTESIAN_POINT('Ctrl Pts',(78.7492545818048,-10.1005956027413,134.560517599131));
#80405=CARTESIAN_POINT('Ctrl Pts',(78.738035145519,-10.0876761005289,134.559379188394));
#80406=CARTESIAN_POINT('Ctrl Pts',(78.7339881522555,-10.0829628764776,134.558964034378));
#80407=CARTESIAN_POINT('Ctrl Pts',(78.7263879463462,-10.0740106753153,134.558175544376));
#80408=CARTESIAN_POINT('Ctrl Pts',(78.7228293658957,-10.0697765007617,134.557802603789));
#80409=CARTESIAN_POINT('Ctrl Pts',(78.7144310524679,-10.0596821439433,134.556913596875));
#80410=CARTESIAN_POINT('Ctrl Pts',(78.7096102584103,-10.0538064690579,134.55639621489));
#80411=CARTESIAN_POINT('Ctrl Pts',(78.6934007142733,-10.033771968731,134.554632965941));
#80412=CARTESIAN_POINT('Ctrl Pts',(78.6822039181712,-10.0194604437154,134.553374894496));
#80413=CARTESIAN_POINT('Ctrl Pts',(78.6141843361677,-9.92952593831224,134.545492669597));
#80414=CARTESIAN_POINT('Ctrl Pts',(78.5636581467632,-9.84936612425774,134.538579423431));
#80415=CARTESIAN_POINT('Ctrl Pts',(78.483742814344,-9.69485337883322,134.525923075884));
#80416=CARTESIAN_POINT('Ctrl Pts',(78.4523584077222,-9.62182386272021,134.520184681434));
#80417=CARTESIAN_POINT('Ctrl Pts',(78.4112168365699,-9.50342376969325,134.511356299255));
#80418=CARTESIAN_POINT('Ctrl Pts',(78.3979356800917,-9.45941054467738,134.508171022092));
#80419=CARTESIAN_POINT('Ctrl Pts',(78.3825486164873,-9.39957168790171,134.503966904184));
#80420=CARTESIAN_POINT('Ctrl Pts',(78.378825451367,-9.38418696580942,134.502896957911));
#80421=CARTESIAN_POINT('Ctrl Pts',(78.3730304226634,-9.3586546838525,134.501138778493));
#80422=CARTESIAN_POINT('Ctrl Pts',(78.3708329841123,-9.34853698588228,134.500446568906));
#80423=CARTESIAN_POINT('Ctrl Pts',(78.3667085381386,-9.32865489412879,134.499094892106));
#80424=CARTESIAN_POINT('Ctrl Pts',(78.364774431335,-9.31889243597133,134.498435224417));
#80425=CARTESIAN_POINT('Ctrl Pts',(78.3610995940139,-9.29943038570299,134.497127873068));
#80426=CARTESIAN_POINT('Ctrl Pts',(78.359357214964,-9.28973152308358,134.496480161984));
#80427=CARTESIAN_POINT('Ctrl Pts',(78.3554622532095,-9.2668876302688,134.494963169856));
#80428=CARTESIAN_POINT('Ctrl Pts',(78.3533810378689,-9.25373099502853,134.494096130788));
#80429=CARTESIAN_POINT('Ctrl Pts',(78.3397677171448,-9.16043609987433,134.487991767609));
#80430=CARTESIAN_POINT('Ctrl Pts',(78.3339325374407,-9.07957311045808,134.482936828984));
#80431=CARTESIAN_POINT('Ctrl Pts',(78.3340005883416,-8.9985998736709,134.47795669959));
#80432=CARTESIAN_POINT('Ctrl Pts',(78.3340005871935,-8.99860124042719,134.47795678365));
#80433=CARTESIAN_POINT('Ctrl Pts',(78.3341161231815,-8.86099153826944,134.469493317637));
#80434=CARTESIAN_POINT('Ctrl Pts',(78.3512803163155,-8.72394302691231,134.46132014703));
#80435=CARTESIAN_POINT('Ctrl Pts',(78.3889956810779,-8.57517810429444,134.451364961208));
#80436=CARTESIAN_POINT('Ctrl Pts',(78.3931211871174,-8.55983072105692,134.45032415857));
#80437=CARTESIAN_POINT('Ctrl Pts',(78.3994358404868,-8.53761236960593,134.448794138787));
#80438=CARTESIAN_POINT('Ctrl Pts',(78.4014511939541,-8.5306923617065,134.448314302381));
#80439=CARTESIAN_POINT('Ctrl Pts',(78.4050787622014,-8.51853108705294,134.447464846563));
#80440=CARTESIAN_POINT('Ctrl Pts',(78.4066720452708,-8.51328437842448,134.447096316818));
#80441=CARTESIAN_POINT('Ctrl Pts',(78.4101931791924,-8.50189182130291,134.446291541461));
#80442=CARTESIAN_POINT('Ctrl Pts',(78.4121307473039,-8.49574935002067,134.445854768662));
#80443=CARTESIAN_POINT('Ctrl Pts',(78.4176688187356,-8.47854103727911,134.444623380188));
#80444=CARTESIAN_POINT('Ctrl Pts',(78.4213496353584,-8.46750171431008,134.443824393295));
#80445=CARTESIAN_POINT('Ctrl Pts',(78.4288419455592,-8.44579178596344,134.442236434915));
#80446=CARTESIAN_POINT('Ctrl Pts',(78.4326467504955,-8.43512118271736,134.441447903419));
#80447=CARTESIAN_POINT('Ctrl Pts',(78.4365593695135,-8.4244920548384,134.440654933552));
#80448=CARTESIAN_POINT('',(78.3339996279362,-8.9995716607509,134.670001230007));
#80449=CARTESIAN_POINT('Ctrl Pts',(78.4365594680555,-8.42449178713676,134.632696249083));
#80450=CARTESIAN_POINT('Ctrl Pts',(78.4230664091285,-8.46114738084474,134.635100959469));
#80451=CARTESIAN_POINT('Ctrl Pts',(78.4108580173571,-8.49828954855501,134.637487701189));
#80452=CARTESIAN_POINT('Ctrl Pts',(78.3785500153332,-8.60966343661029,134.644568869371));
#80453=CARTESIAN_POINT('Ctrl Pts',(78.3622729774936,-8.68486328966597,134.649250240163));
#80454=CARTESIAN_POINT('Ctrl Pts',(78.3463552023685,-8.79463231339255,134.656260430122));
#80455=CARTESIAN_POINT('Ctrl Pts',(78.3425013367062,-8.8284925305262,134.658447268492));
#80456=CARTESIAN_POINT('Ctrl Pts',(78.338872193042,-8.87229665142323,134.661335079901));
#80457=CARTESIAN_POINT('Ctrl Pts',(78.3381436651677,-8.88215583637794,134.661988880378));
#80458=CARTESIAN_POINT('Ctrl Pts',(78.3371147149533,-8.89799799750504,134.663046420861));
#80459=CARTESIAN_POINT('Ctrl Pts',(78.3367587310208,-8.90397730446751,134.663447164606));
#80460=CARTESIAN_POINT('Ctrl Pts',(78.3361542698538,-8.91514502163804,134.664198842126));
#80461=CARTESIAN_POINT('Ctrl Pts',(78.3358978011997,-8.92033287994357,134.664549328504));
#80462=CARTESIAN_POINT('Ctrl Pts',(78.3354160274224,-8.9310988746163,134.665279266662));
#80463=CARTESIAN_POINT('Ctrl Pts',(78.3351944918527,-8.93667713966902,134.665658918725));
#80464=CARTESIAN_POINT('Ctrl Pts',(78.3346997108799,-8.95094380408305,134.666633408942));
#80465=CARTESIAN_POINT('Ctrl Pts',(78.3344664264399,-8.95963329653432,134.667230278338));
#80466=CARTESIAN_POINT('Ctrl Pts',(78.3341030873741,-8.97873966103855,134.668549418527));
#80467=CARTESIAN_POINT('Ctrl Pts',(78.3340027210467,-8.98915664129192,134.669273035995));
#80468=CARTESIAN_POINT('Ctrl Pts',(78.3340000545808,-8.99957354585502,134.670000621529));
#80469=CARTESIAN_POINT('Ctrl Pts',(78.3340000550511,-8.99957171231383,134.670000493463));
#80470=CARTESIAN_POINT('Ctrl Pts',(78.3339655640915,-9.13373839219119,134.679371576049));
#80471=CARTESIAN_POINT('Ctrl Pts',(78.3501375019262,-9.26742048515377,134.689320602716));
#80472=CARTESIAN_POINT('Ctrl Pts',(78.3979871940484,-9.46206173214905,134.703754922728));
#80473=CARTESIAN_POINT('Ctrl Pts',(78.4176304081814,-9.52540878035722,134.70845310578));
#80474=CARTESIAN_POINT('Ctrl Pts',(78.4507577760545,-9.61332763812592,134.714950196648));
#80475=CARTESIAN_POINT('Ctrl Pts',(78.4611626667193,-9.63898519600179,134.716843838627));
#80476=CARTESIAN_POINT('Ctrl Pts',(78.4772814709453,-9.67605212743428,134.719577533887));
#80477=CARTESIAN_POINT('Ctrl Pts',(78.4824941231686,-9.68767297980347,134.720434299254));
#80478=CARTESIAN_POINT('Ctrl Pts',(78.4919466410799,-9.70811497651373,134.721941282511));
#80479=CARTESIAN_POINT('Ctrl Pts',(78.4961318790929,-9.71696055348584,134.722593334171));
#80480=CARTESIAN_POINT('Ctrl Pts',(78.505079483049,-9.73544835656566,134.723956311786));
#80481=CARTESIAN_POINT('Ctrl Pts',(78.5098577750967,-9.74508240878569,134.72466664954));
#80482=CARTESIAN_POINT('Ctrl Pts',(78.52275414945,-9.77046385587785,134.726538784549));
#80483=CARTESIAN_POINT('Ctrl Pts',(78.5310308467589,-9.78612945638457,134.727694999347));
#80484=CARTESIAN_POINT('Ctrl Pts',(78.5717446085006,-9.86030070461446,134.733177494711));
#80485=CARTESIAN_POINT('Ctrl Pts',(78.6074377863159,-9.91695299704115,134.737386473143));
#80486=CARTESIAN_POINT('Ctrl Pts',(78.7306340209266,-10.0886312118089,134.750467129965));
#80487=CARTESIAN_POINT('Ctrl Pts',(78.8297057845599,-10.1944910101378,134.758995725453));
#80488=CARTESIAN_POINT('Ctrl Pts',(78.952679850075,-10.2957233498186,134.769227916008));
#80489=CARTESIAN_POINT('Ctrl Pts',(78.9643224077977,-10.3050480401016,134.77019409343));
#80490=CARTESIAN_POINT('Ctrl Pts',(78.982758472502,-10.3194116778307,134.771722891968));
#80491=CARTESIAN_POINT('Ctrl Pts',(78.98946810218,-10.3245575779515,134.772279050622));
#80492=CARTESIAN_POINT('Ctrl Pts',(79.0019141405984,-10.3339533658567,134.773310876572));
#80493=CARTESIAN_POINT('Ctrl Pts',(79.0076392937887,-10.3382179154274,134.773785583136));
#80494=CARTESIAN_POINT('Ctrl Pts',(79.0134457632717,-10.3424852857742,134.774267300784));
#80495=CARTESIAN_POINT('Ctrl Pts',(79.0134999811191,-10.3425251272416,134.774271798841));
#80496=CARTESIAN_POINT('Ctrl Pts',(79.0136085108232,-10.3426048691337,134.774280802802));
#80497=CARTESIAN_POINT('Ctrl Pts',(79.0136628224429,-10.3426447693677,134.774285308686));
#80498=CARTESIAN_POINT('Ctrl Pts',(79.0137715557547,-10.3427246405428,134.774294329634));
#80499=CARTESIAN_POINT('Ctrl Pts',(79.013825977572,-10.3427646115562,134.774298844709));
#80500=CARTESIAN_POINT('Ctrl Pts',(79.0139349477684,-10.3428446363401,134.774307885406));
#80501=CARTESIAN_POINT('Ctrl Pts',(79.0139894959941,-10.3428846899752,134.774312411017));
#80502=CARTESIAN_POINT('Ctrl Pts',(79.0140987356719,-10.3429648921693,134.774321474169));
#80503=CARTESIAN_POINT('Ctrl Pts',(79.0141534271985,-10.3430050407569,134.774326011718));
#80504=CARTESIAN_POINT('Ctrl Pts',(79.0142372954618,-10.3430665998569,134.774332969988));
#80505=CARTESIAN_POINT('Ctrl Pts',(79.0142664706427,-10.3430880129055,134.774335390562));
#80506=CARTESIAN_POINT('Ctrl Pts',(79.0143255429488,-10.3431313659103,134.774340291623));
#80507=CARTESIAN_POINT('Ctrl Pts',(79.0143554400502,-10.3431533057758,134.774342772107));
#80508=CARTESIAN_POINT('Ctrl Pts',(79.0144159922831,-10.3431977386738,134.774347795983));
#80509=CARTESIAN_POINT('Ctrl Pts',(79.0144466474883,-10.3432202316816,134.774350339381));
#80510=CARTESIAN_POINT('Ctrl Pts',(79.0145087542789,-10.3432657987639,134.774355492267));
#80511=CARTESIAN_POINT('Ctrl Pts',(79.0145402060875,-10.3432888729174,134.774358101774));
#80512=CARTESIAN_POINT('Ctrl Pts',(79.0146039474237,-10.3433356323609,134.774363390308));
#80513=CARTESIAN_POINT('Ctrl Pts',(79.0146362367528,-10.343359317414,134.77436606932));
#80514=CARTESIAN_POINT('Ctrl Pts',(79.0147016970534,-10.3434073305974,134.774371500511));
#80515=CARTESIAN_POINT('Ctrl Pts',(79.0147348681049,-10.3434316586875,134.774374252696));
#80516=CARTESIAN_POINT('Ctrl Pts',(79.0148021388393,-10.3434809921068,134.774379834135));
#80517=CARTESIAN_POINT('Ctrl Pts',(79.0148362386128,-10.3435059973954,134.774382663395));
#80518=CARTESIAN_POINT('Ctrl Pts',(79.0149054174014,-10.3435567219983,134.774388403185));
#80519=CARTESIAN_POINT('Ctrl Pts',(79.0149404963375,-10.3435824411387,134.774391313707));
#80520=CARTESIAN_POINT('Ctrl Pts',(79.0192893398945,-10.3467706601818,134.774752141436));
#80521=CARTESIAN_POINT('Ctrl Pts',(79.0236181220911,-10.3499122332568,134.775111473011));
#80522=CARTESIAN_POINT('Ctrl Pts',(79.0330801786284,-10.3567099077547,134.775897391517));
#80523=CARTESIAN_POINT('Ctrl Pts',(79.0382190017326,-10.3603576819476,134.776324493823));
#80524=CARTESIAN_POINT('Ctrl Pts',(79.0524019511165,-10.3703048627952,134.777503746734));
#80525=CARTESIAN_POINT('Ctrl Pts',(79.061487896114,-10.3765436767027,134.778259722285));
#80526=CARTESIAN_POINT('Ctrl Pts',(79.1133507500622,-10.4114028825208,134.782574772295));
#80527=CARTESIAN_POINT('Ctrl Pts',(79.1573701053193,-10.4381163947461,134.786236186844));
#80528=CARTESIAN_POINT('Ctrl Pts',(79.2868519069303,-10.5087063475569,134.79686350198));
#80529=CARTESIAN_POINT('Ctrl Pts',(79.374969743379,-10.5472922451104,134.803915886907));
#80530=CARTESIAN_POINT('Ctrl Pts',(79.5157217824108,-10.5949277474463,134.814601881482));
#80531=CARTESIAN_POINT('Ctrl Pts',(79.5662935521673,-10.6094158933086,134.818335622565));
#80532=CARTESIAN_POINT('Ctrl Pts',(79.6406651286282,-10.6269610943946,134.823661066639));
#80533=CARTESIAN_POINT('Ctrl Pts',(79.6639758579436,-10.6319349948502,134.825307380278));
#80534=CARTESIAN_POINT('Ctrl Pts',(79.7064425288364,-10.6400476829755,134.828265811755));
#80535=CARTESIAN_POINT('Ctrl Pts',(79.725561523881,-10.6433550953282,134.829582919654));
#80536=CARTESIAN_POINT('Ctrl Pts',(79.7557168691385,-10.6480307219866,134.831637920771));
#80537=CARTESIAN_POINT('Ctrl Pts',(79.7667160729204,-10.649623632337,134.832382831533));
#80538=CARTESIAN_POINT('Ctrl Pts',(79.7873642226649,-10.6524032541108,134.83377277205));
#80539=CARTESIAN_POINT('Ctrl Pts',(79.7970091532958,-10.6536157990899,134.83441858825));
#80540=CARTESIAN_POINT('Ctrl Pts',(79.8187058179514,-10.6561507771167,134.835863933002));
#80541=CARTESIAN_POINT('Ctrl Pts',(79.8307625695265,-10.6574262222151,134.83666195621));
#80542=CARTESIAN_POINT('Ctrl Pts',(79.866310382155,-10.6607947644141,134.839000497099));
#80543=CARTESIAN_POINT('Ctrl Pts',(79.8898337995487,-10.6625208754126,134.840529571684));
#80544=CARTESIAN_POINT('Ctrl Pts',(80.0169213852895,-10.6691369336915,134.848705135352));
#80545=CARTESIAN_POINT('Ctrl Pts',(80.1207370622526,-10.6648514547836,134.855059796419));
#80546=CARTESIAN_POINT('Ctrl Pts',(80.3013522301192,-10.6404012746056,134.866190751969));
#80547=CARTESIAN_POINT('Ctrl Pts',(80.3783651080232,-10.6243668395529,134.870968298552));
#80548=CARTESIAN_POINT('Ctrl Pts',(80.4776737703714,-10.5962429520857,134.877477491342));
#80549=CARTESIAN_POINT('Ctrl Pts',(80.501241105463,-10.589000005949,134.879049184282));
#80550=CARTESIAN_POINT('Ctrl Pts',(80.5409210087273,-10.5758346341372,134.881754995544));
#80551=CARTESIAN_POINT('Ctrl Pts',(80.5571190456132,-10.5701810865987,134.882876701772));
#80552=CARTESIAN_POINT('Ctrl Pts',(80.5802013040859,-10.56172264934,134.884503753885));
#80553=CARTESIAN_POINT('Ctrl Pts',(80.5871591613581,-10.5591200405168,134.884997974632));
#80554=CARTESIAN_POINT('Ctrl Pts',(80.5992437850293,-10.5545073845682,134.885863314436));
#80555=CARTESIAN_POINT('Ctrl Pts',(80.6043783622986,-10.5525183144636,134.886233196932));
#80556=CARTESIAN_POINT('Ctrl Pts',(80.6153668345606,-10.5481987453737,134.887029654107));
#80557=CARTESIAN_POINT('Ctrl Pts',(80.6212173019891,-10.5458605230313,134.88745665413));
#80558=CARTESIAN_POINT('Ctrl Pts',(80.6372594904589,-10.5393432618707,134.888635356231));
#80559=CARTESIAN_POINT('Ctrl Pts',(80.6474230308605,-10.5350963288823,134.889390877641));
#80560=CARTESIAN_POINT('Ctrl Pts',(80.7053400824852,-10.5102176771152,134.893743500901));
#80561=CARTESIAN_POINT('Ctrl Pts',(80.7521442491115,-10.4874609164817,134.897445240398));
#80562=CARTESIAN_POINT('Ctrl Pts',(80.8876327028721,-10.4135539652158,134.908569889407));
#80563=CARTESIAN_POINT('Ctrl Pts',(80.9727640360823,-10.3563769860894,134.916091705519));
#80564=CARTESIAN_POINT('Ctrl Pts',(81.108624851904,-10.2457205151263,134.928652816149));
#80565=CARTESIAN_POINT('Ctrl Pts',(81.1620638983282,-10.1960262534107,134.933774892698));
#80566=CARTESIAN_POINT('Ctrl Pts',(81.2241712531038,-10.1301642519014,134.939952855472));
#80567=CARTESIAN_POINT('Ctrl Pts',(81.2360565134369,-10.1171530021458,134.941146721057));
#80568=CARTESIAN_POINT('Ctrl Pts',(81.2548456494016,-10.0959167827094,134.943053764791));
#80569=CARTESIAN_POINT('Ctrl Pts',(81.2618800743664,-10.0878096734668,134.943772363441));
#80570=CARTESIAN_POINT('Ctrl Pts',(81.2751806568171,-10.0721782280951,134.94514028096));
#80571=CARTESIAN_POINT('Ctrl Pts',(81.2814597632777,-10.0646655542489,134.945790114628));
#80572=CARTESIAN_POINT('Ctrl Pts',(81.2956440900474,-10.047387336875,134.947267701777));
#80573=CARTESIAN_POINT('Ctrl Pts',(81.3035058661933,-10.0375867735755,134.94809368396));
#80574=CARTESIAN_POINT('Ctrl Pts',(81.3242020903954,-10.0111801319241,134.950287939771));
#80575=CARTESIAN_POINT('Ctrl Pts',(81.3368351410188,-9.99441857593888,134.951648334009));
#80576=CARTESIAN_POINT('Ctrl Pts',(81.4202062247464,-9.87934038134007,134.960784321498));
#80577=CARTESIAN_POINT('Ctrl Pts',(81.4803582617905,-9.77380132754669,134.968139504169));
#80578=CARTESIAN_POINT('Ctrl Pts',(81.5548125319775,-9.60206059398917,134.979577859045));
#80579=CARTESIAN_POINT('Ctrl Pts',(81.5774562682301,-9.53995317480335,134.98362557116));
#80580=CARTESIAN_POINT('Ctrl Pts',(81.60276500431,-9.45519519827983,134.989224450874));
#80581=CARTESIAN_POINT('Ctrl Pts',(81.6087433117181,-9.43359333996628,134.990657923125));
#80582=CARTESIAN_POINT('Ctrl Pts',(81.6182343533038,-9.39639491518517,134.993147772109));
#80583=CARTESIAN_POINT('Ctrl Pts',(81.6219618000273,-9.38085591015712,134.994194188927));
#80584=CARTESIAN_POINT('Ctrl Pts',(81.6270484498644,-9.35821990766349,134.995730889327));
#80585=CARTESIAN_POINT('Ctrl Pts',(81.6285860298727,-9.35116335079337,134.99621167499));
#80586=CARTESIAN_POINT('Ctrl Pts',(81.6312000864178,-9.33877988663787,134.99705879292));
#80587=CARTESIAN_POINT('Ctrl Pts',(81.6322964539683,-9.33345737158956,134.997423998227));
#80588=CARTESIAN_POINT('Ctrl Pts',(81.6346286825067,-9.32184797605086,134.998223084424));
#80589=CARTESIAN_POINT('Ctrl Pts',(81.6358543059121,-9.31555940127625,134.998657498626));
#80590=CARTESIAN_POINT('Ctrl Pts',(81.6391763853969,-9.29797446371018,134.999876336945));
#80591=CARTESIAN_POINT('Ctrl Pts',(81.6411922554431,-9.28666350632705,135.000664998887));
#80592=CARTESIAN_POINT('Ctrl Pts',(81.6540552666921,-9.20990156134054,135.006044873079));
#80593=CARTESIAN_POINT('Ctrl Pts',(81.661100209379,-9.14388056898265,135.010805449705));
#80594=CARTESIAN_POINT('Ctrl Pts',(81.6652096704722,-9.05577697596238,135.017200097133));
#80595=CARTESIAN_POINT('Ctrl Pts',(81.665798379235,-9.03391251562046,135.018790675824));
#80596=CARTESIAN_POINT('Ctrl Pts',(81.6664767850191,-8.94006623175308,135.025621083104));
#80597=CARTESIAN_POINT('Ctrl Pts',(81.6623319886287,-8.86812706646643,135.030861097291));
#80598=CARTESIAN_POINT('Ctrl Pts',(81.645381018262,-8.73027056741288,135.040784064559));
#80599=CARTESIAN_POINT('Ctrl Pts',(81.6332216477549,-8.66440831011032,135.045471825213));
#80600=CARTESIAN_POINT('Ctrl Pts',(81.612987228798,-8.58271675104982,135.051211811907));
#80601=CARTESIAN_POINT('Ctrl Pts',(81.6085834722453,-8.56605027743998,135.052379126672));
#80602=CARTESIAN_POINT('Ctrl Pts',(81.6010413784179,-8.5392007574084,135.05425423469));
#80603=CARTESIAN_POINT('Ctrl Pts',(81.5980627336176,-8.52897458039818,135.054967125767));
#80604=CARTESIAN_POINT('Ctrl Pts',(81.5921510087143,-8.50938048682056,135.056330864971));
#80605=CARTESIAN_POINT('Ctrl Pts',(81.5892328122197,-8.50000858321588,135.05698216495));
#80606=CARTESIAN_POINT('Ctrl Pts',(81.5823383932591,-8.47853725094815,135.058472348632));
#80607=CARTESIAN_POINT('Ctrl Pts',(81.5783058845753,-8.46645643185838,135.059309352503));
#80608=CARTESIAN_POINT('Ctrl Pts',(81.5648132508347,-8.4275266024776,135.062002928243));
#80609=CARTESIAN_POINT('Ctrl Pts',(81.5548031451842,-8.40087260591408,135.063841412918));
#80610=CARTESIAN_POINT('Ctrl Pts',(81.4950344855907,-8.25333029494713,135.074012595117));
#80611=CARTESIAN_POINT('Ctrl Pts',(81.4318675300645,-8.13837273581656,135.081871775029));
#80612=CARTESIAN_POINT('Ctrl Pts',(81.3144980280403,-7.97397370461078,135.094265581886));
#80613=CARTESIAN_POINT('Ctrl Pts',(81.2694138161518,-7.91869464926673,135.09868386757));
#80614=CARTESIAN_POINT('Ctrl Pts',(81.210209995916,-7.85492520975466,135.104329575303));
#80615=CARTESIAN_POINT('Ctrl Pts',(81.1993213180594,-7.84352568498104,135.105362181486));
#80616=CARTESIAN_POINT('Ctrl Pts',(81.1832381788494,-7.82715942615533,135.106882253578));
#80617=CARTESIAN_POINT('Ctrl Pts',(81.1781703721315,-7.8220686908685,135.107360506613));
#80618=CARTESIAN_POINT('Ctrl Pts',(81.1692137656287,-7.81318718333462,135.108204842296));
#80619=CARTESIAN_POINT('Ctrl Pts',(81.165339115256,-7.80938241373852,135.108569823608));
#80620=CARTESIAN_POINT('Ctrl Pts',(81.156833788951,-7.80111177791663,135.109370482636));
#80621=CARTESIAN_POINT('Ctrl Pts',(81.1521958994567,-7.79665383613564,135.109806712555));
#80622=CARTESIAN_POINT('Ctrl Pts',(81.1391183129126,-7.7842285673267,135.111035449682));
#80623=CARTESIAN_POINT('Ctrl Pts',(81.1306211984808,-7.7763225939623,135.111832300858));
#80624=CARTESIAN_POINT('Ctrl Pts',(81.0651948429934,-7.71671112250744,135.117951778171));
#80625=CARTESIAN_POINT('Ctrl Pts',(81.0048351857145,-7.66892000078039,135.123501156732));
#80626=CARTESIAN_POINT('Ctrl Pts',(80.8942454603738,-7.59317821923879,135.133244034475));
#80627=CARTESIAN_POINT('Ctrl Pts',(80.8454598586471,-7.56333011596693,135.137414711098));
#80628=CARTESIAN_POINT('Ctrl Pts',(80.7224006028771,-7.49648285817966,135.147535104135));
#80629=CARTESIAN_POINT('Ctrl Pts',(80.6467053257672,-7.46240373932795,135.153421773494));
#80630=CARTESIAN_POINT('Ctrl Pts',(80.5472951060551,-7.42629531983579,135.160693124238));
#80631=CARTESIAN_POINT('Ctrl Pts',(80.5256540900555,-7.41893509903838,135.162250098101));
#80632=CARTESIAN_POINT('Ctrl Pts',(80.4925959369778,-7.40844570232025,135.16459050362));
#80633=CARTESIAN_POINT('Ctrl Pts',(80.4812863608128,-7.40498925051011,135.165384538784));
#80634=CARTESIAN_POINT('Ctrl Pts',(80.4615343282968,-7.39918182186175,135.166760075115));
#80635=CARTESIAN_POINT('Ctrl Pts',(80.4531084708974,-7.3967765301468,135.167343322934));
#80636=CARTESIAN_POINT('Ctrl Pts',(80.434066786017,-7.39150289479416,135.168653657651));
#80637=CARTESIAN_POINT('Ctrl Pts',(80.4234406784741,-7.38867293396076,135.169379479044));
#80638=CARTESIAN_POINT('Ctrl Pts',(80.3945261688822,-7.38127816640636,135.171340406612));
#80639=CARTESIAN_POINT('Ctrl Pts',(80.3761867126155,-7.37691809305534,135.172568923011));
#80640=CARTESIAN_POINT('Ctrl Pts',(80.2578261671444,-7.35089273968766,135.180407935869));
#80641=CARTESIAN_POINT('Ctrl Pts',(80.1560581931952,-7.33817004567148,135.186720324653));
#80642=CARTESIAN_POINT('Ctrl Pts',(79.9711519344295,-7.33220082725675,135.198030572033));
#80643=CARTESIAN_POINT('Ctrl Pts',(79.8884705956017,-7.33568457134481,135.203037332583));
#80644=CARTESIAN_POINT('Ctrl Pts',(79.7785236846193,-7.34854861557631,135.209983476996));
#80645=CARTESIAN_POINT('Ctrl Pts',(79.7507409538766,-7.35251307057591,135.211764255161));
#80646=CARTESIAN_POINT('Ctrl Pts',(79.7044684385107,-7.36031311830765,135.214792617982));
#80647=CARTESIAN_POINT('Ctrl Pts',(79.6859192166138,-7.36376494292112,135.216023561489));
#80648=CARTESIAN_POINT('Ctrl Pts',(79.6598767919797,-7.36907030241892,135.21778085283));
#80649=CARTESIAN_POINT('Ctrl Pts',(79.6523309637325,-7.37066218649873,135.21829349354));
#80650=CARTESIAN_POINT('Ctrl Pts',(79.6393775081506,-7.37348895364017,135.219179902661));
#80651=CARTESIAN_POINT('Ctrl Pts',(79.6339645289813,-7.37469855144849,135.219552246888));
#80652=CARTESIAN_POINT('Ctrl Pts',(79.6225563755177,-7.37730772840862,135.22034121488));
#80653=CARTESIAN_POINT('Ctrl Pts',(79.6165629772903,-7.37871349093621,135.220758154326));
#80654=CARTESIAN_POINT('Ctrl Pts',(79.6002272580043,-7.38264070886757,135.221901001507));
#80655=CARTESIAN_POINT('Ctrl Pts',(79.5899013053382,-7.38522807562341,135.222630458448));
#80656=CARTESIAN_POINT('Ctrl Pts',(79.5378591172056,-7.3987996067678,135.226340184451));
#80657=CARTESIAN_POINT('Ctrl Pts',(79.4965593227174,-7.41130126126427,135.229392352303));
#80658=CARTESIAN_POINT('Ctrl Pts',(79.3705388583657,-7.4548554930012,135.238952966392));
#80659=CARTESIAN_POINT('Ctrl Pts',(79.2878176306945,-7.49119614370717,135.245574474084));
#80660=CARTESIAN_POINT('Ctrl Pts',(79.1265572284294,-7.5782706138291,135.258830483274));
#80661=CARTESIAN_POINT('Ctrl Pts',(79.0485070069298,-7.62927645808574,135.265433725204));
#80662=CARTESIAN_POINT('Ctrl Pts',(78.9605025230795,-7.69794603449026,135.273062234116));
#80663=CARTESIAN_POINT('Ctrl Pts',(78.9460808071472,-7.70959156980129,135.274319341418));
#80664=CARTESIAN_POINT('Ctrl Pts',(78.9234688097721,-7.72848278100851,135.276302386316));
#80665=CARTESIAN_POINT('Ctrl Pts',(78.9151506902299,-7.73557229282677,135.277034543382));
#80666=CARTESIAN_POINT('Ctrl Pts',(78.8995471097111,-7.74913852053893,135.278413321286));
#80667=CARTESIAN_POINT('Ctrl Pts',(78.8922475930745,-7.75559828978252,135.279060600017));
#80668=CARTESIAN_POINT('Ctrl Pts',(78.8757834713942,-7.77042803108348,135.280526026533));
#80669=CARTESIAN_POINT('Ctrl Pts',(78.8666547908596,-7.77883716043145,135.281342485338));
#80670=CARTESIAN_POINT('Ctrl Pts',(78.8430726209364,-7.80105274723584,135.283462824265));
#80671=CARTESIAN_POINT('Ctrl Pts',(78.8287718542016,-7.81501891972989,135.284759847613));
#80672=CARTESIAN_POINT('Ctrl Pts',(78.7067132739332,-7.93859068784639,135.295942575706));
#80673=CARTESIAN_POINT('Ctrl Pts',(78.6143578809276,-8.06235533176093,135.305096383721));
#80674=CARTESIAN_POINT('Ctrl Pts',(78.5113756955332,-8.24956745276767,135.318278434067));
#80675=CARTESIAN_POINT('Ctrl Pts',(78.4853363497141,-8.30362092487862,135.322029180513));
#80676=CARTESIAN_POINT('Ctrl Pts',(78.4566659949515,-8.37239485799929,135.326874476996));
#80677=CARTESIAN_POINT('Ctrl Pts',(78.4512393321645,-8.38590845647614,135.327829978261));
#80678=CARTESIAN_POINT('Ctrl Pts',(78.4434820897048,-8.4059828005563,135.329256892356));
#80679=CARTESIAN_POINT('Ctrl Pts',(78.4410142065181,-8.4124902301322,135.329720607381));
#80680=CARTESIAN_POINT('Ctrl Pts',(78.4379080626342,-8.42083804333813,135.330317178921));
#80681=CARTESIAN_POINT('Ctrl Pts',(78.4372321141303,-8.42266445845914,135.330447807108));
#80682=CARTESIAN_POINT('Ctrl Pts',(78.4365593749993,-8.42449203993567,135.330578627164));
#80683=CARTESIAN_POINT('Origin',(80.,-9.,134.));
#80684=CARTESIAN_POINT('',(78.4365593762033,-8.4244920366647,136.032852185112));
#80685=CARTESIAN_POINT('',(78.4365593748807,-8.42449204025778,135.837694108205));
#80686=CARTESIAN_POINT('',(78.4365593749993,-8.42449203993574,134.));
#80687=CARTESIAN_POINT('Ctrl Pts',(78.4365593748807,-8.42449204025778,135.837694108205));
#80688=CARTESIAN_POINT('Ctrl Pts',(78.4383939076403,-8.41950829851134,135.837334131949));
#80689=CARTESIAN_POINT('Ctrl Pts',(78.4402523135159,-8.41453321100119,135.836974938851));
#80690=CARTESIAN_POINT('Ctrl Pts',(78.4463332781694,-8.39848850480445,135.835817009369));
#80691=CARTESIAN_POINT('Ctrl Pts',(78.4506501675972,-8.3874549234687,135.835021458479));
#80692=CARTESIAN_POINT('Ctrl Pts',(78.4583654957885,-8.36833877271354,135.83364411433));
#80693=CARTESIAN_POINT('Ctrl Pts',(78.4617106704672,-8.3602353602156,135.833060561932));
#80694=CARTESIAN_POINT('Ctrl Pts',(78.4693916474057,-8.34203741850409,135.831750578648));
#80695=CARTESIAN_POINT('Ctrl Pts',(78.4737636770115,-8.33195854634371,135.831025404877));
#80696=CARTESIAN_POINT('Ctrl Pts',(78.4858836455377,-8.30475845833332,135.829068798149));
#80697=CARTESIAN_POINT('Ctrl Pts',(78.4938222333095,-8.28772356648408,135.827843901735));
#80698=CARTESIAN_POINT('Ctrl Pts',(78.5459111333964,-8.1807165988968,135.820145019594));
#80699=CARTESIAN_POINT('Ctrl Pts',(78.5978179491005,-8.09474370543545,135.813955697692));
#80700=CARTESIAN_POINT('Ctrl Pts',(78.7020167114911,-7.9528404496892,135.80318867182));
#80701=CARTESIAN_POINT('Ctrl Pts',(78.7510052880733,-7.89486881111581,135.798593382761));
#80702=CARTESIAN_POINT('Ctrl Pts',(78.8271405395223,-7.81632593121283,135.791776868014));
#80703=CARTESIAN_POINT('Ctrl Pts',(78.8512349740222,-7.79292823306179,135.789660066913));
#80704=CARTESIAN_POINT('Ctrl Pts',(78.8868571773618,-7.76036913385192,135.786558188611));
#80705=CARTESIAN_POINT('Ctrl Pts',(78.8978261777244,-7.75060636264791,135.78560660933));
#80706=CARTESIAN_POINT('Ctrl Pts',(78.9152457023473,-7.73551032921353,135.784098287101));
#80707=CARTESIAN_POINT('Ctrl Pts',(78.9216100735742,-7.73007828054375,135.783547791416));
#80708=CARTESIAN_POINT('Ctrl Pts',(78.9334104480814,-7.72015922539667,135.782527580717));
#80709=CARTESIAN_POINT('Ctrl Pts',(78.9388345663148,-7.71565830150089,135.782058818015));
#80710=CARTESIAN_POINT('Ctrl Pts',(78.9443349429914,-7.71115272772209,135.781583457167));
#80711=CARTESIAN_POINT('Ctrl Pts',(78.9443829285015,-7.71111342539069,135.781579310099));
#80712=CARTESIAN_POINT('Ctrl Pts',(78.9444791139154,-7.71103465410426,135.781570997433));
#80713=CARTESIAN_POINT('Ctrl Pts',(78.9445273138624,-7.71099518515308,135.781566831832));
#80714=CARTESIAN_POINT('Ctrl Pts',(78.9446239420666,-7.71091606935077,135.781558480895));
#80715=CARTESIAN_POINT('Ctrl Pts',(78.9446723703386,-7.71087642252949,135.781554295559));
#80716=CARTESIAN_POINT('Ctrl Pts',(78.9447694693343,-7.71079693953716,135.781545903931));
#80717=CARTESIAN_POINT('Ctrl Pts',(78.9448181401431,-7.71075710334139,135.781541697632));
#80718=CARTESIAN_POINT('Ctrl Pts',(78.9449157387769,-7.7106772298155,135.781533262819));
#80719=CARTESIAN_POINT('Ctrl Pts',(78.9449646665673,-7.71063719256158,135.781529034309));
#80720=CARTESIAN_POINT('Ctrl Pts',(78.945062793984,-7.71055690493771,135.781520553792));
#80721=CARTESIAN_POINT('Ctrl Pts',(78.9451119936912,-7.71051665455248,135.781516301779));
#80722=CARTESIAN_POINT('Ctrl Pts',(78.9452106802047,-7.71043592833354,135.781507772938));
#80723=CARTESIAN_POINT('Ctrl Pts',(78.945260166977,-7.71039545258179,135.781503496112));
#80724=CARTESIAN_POINT('Ctrl Pts',(78.9453594432432,-7.71031426301585,135.781494916296));
#80725=CARTESIAN_POINT('Ctrl Pts',(78.945409232749,-7.71027354924947,135.781490613305));
#80726=CARTESIAN_POINT('Ctrl Pts',(78.9455091304601,-7.710191870763,135.781481979774));
#80727=CARTESIAN_POINT('Ctrl Pts',(78.9455592387293,-7.71015090605151,135.78147764923));
#80728=CARTESIAN_POINT('Ctrl Pts',(78.9456597904758,-7.71006871236304,135.781468959168));
#80729=CARTESIAN_POINT('Ctrl Pts',(78.9457102339212,-7.71002748347658,135.781464599653));
#80730=CARTESIAN_POINT('Ctrl Pts',(78.9498796479072,-7.70662010879387,135.781104262798));
#80731=CARTESIAN_POINT('Ctrl Pts',(78.9540145362725,-7.7032738509777,135.780746886022));
#80732=CARTESIAN_POINT('Ctrl Pts',(78.9630893941307,-7.69600145301667,135.779962392012));
#80733=CARTESIAN_POINT('Ctrl Pts',(78.968035577044,-7.6920836259374,135.779534738161));
#80734=CARTESIAN_POINT('Ctrl Pts',(78.9817064309062,-7.6813808879947,135.77835281934));
#80735=CARTESIAN_POINT('Ctrl Pts',(78.9904763642322,-7.67465469863019,135.777594703506));
#80736=CARTESIAN_POINT('Ctrl Pts',(79.0408342507606,-7.63682200865986,135.773245076621));
#80737=CARTESIAN_POINT('Ctrl Pts',(79.0837880996224,-7.60758920742123,135.769549402611));
#80738=CARTESIAN_POINT('Ctrl Pts',(79.2150509514012,-7.52696222425652,135.758445590601));
#80739=CARTESIAN_POINT('Ctrl Pts',(79.3068069189079,-7.48162244657397,135.750938797174));
#80740=CARTESIAN_POINT('Ctrl Pts',(79.470350793193,-7.41874456707789,135.738376910084));
#80741=CARTESIAN_POINT('Ctrl Pts',(79.5402243519671,-7.39703211563662,135.733240668417));
#80742=CARTESIAN_POINT('Ctrl Pts',(79.6284561167797,-7.37586264519249,135.727048314786));
#80743=CARTESIAN_POINT('Ctrl Pts',(79.6456695425891,-7.37202058584756,135.725853447226));
#80744=CARTESIAN_POINT('Ctrl Pts',(79.6734573218843,-7.366279955023,135.723945071337));
#80745=CARTESIAN_POINT('Ctrl Pts',(79.683994289227,-7.36420914965044,135.723226131327));
#80746=CARTESIAN_POINT('Ctrl Pts',(79.7041777537373,-7.36044484649549,135.721857726924));
#80747=CARTESIAN_POINT('Ctrl Pts',(79.7138205634914,-7.35873425677817,135.721207745928));
#80748=CARTESIAN_POINT('Ctrl Pts',(79.7358668438709,-7.35502355471972,135.719730040084));
#80749=CARTESIAN_POINT('Ctrl Pts',(79.7482790759779,-7.35307850202868,135.718904085037));
#80750=CARTESIAN_POINT('Ctrl Pts',(79.7814735289224,-7.3482608303342,135.716710367351));
#80751=CARTESIAN_POINT('Ctrl Pts',(79.8022904084353,-7.34563997765474,135.715350475287));
#80752=CARTESIAN_POINT('Ctrl Pts',(79.9437506440844,-7.33053847234002,135.706204142184));
#80753=CARTESIAN_POINT('Ctrl Pts',(80.0653963566273,-7.33087060094516,135.698839462544));
#80754=CARTESIAN_POINT('Ctrl Pts',(80.2514621884996,-7.35176752148609,135.68739780262));
#80755=CARTESIAN_POINT('Ctrl Pts',(80.3164868468536,-7.36300935972011,135.683356945727));
#80756=CARTESIAN_POINT('Ctrl Pts',(80.4024681817477,-7.38318933156897,135.677766619055));
#80757=CARTESIAN_POINT('Ctrl Pts',(80.4241607993943,-7.38874431226376,135.676334464093));
#80758=CARTESIAN_POINT('Ctrl Pts',(80.4611207594921,-7.39900697722901,135.673846632523));
#80759=CARTESIAN_POINT('Ctrl Pts',(80.4764448366359,-7.40350030204292,135.672800892618));
#80760=CARTESIAN_POINT('Ctrl Pts',(80.4986010621413,-7.4103443358034,135.671264929807));
#80761=CARTESIAN_POINT('Ctrl Pts',(80.5054867739309,-7.4125204673926,135.670784189941));
#80762=CARTESIAN_POINT('Ctrl Pts',(80.5175302329767,-7.41641293106894,135.669937033602));
#80763=CARTESIAN_POINT('Ctrl Pts',(80.5226940575881,-7.41810984329749,135.669571742901));
#80764=CARTESIAN_POINT('Ctrl Pts',(80.5339300780641,-7.4218631968693,135.668772313184));
#80765=CARTESIAN_POINT('Ctrl Pts',(80.539998641126,-7.42392939188108,135.668337639144));
#80766=CARTESIAN_POINT('Ctrl Pts',(80.5569211369628,-7.42980028934295,135.667117697882));
#80767=CARTESIAN_POINT('Ctrl Pts',(80.5677475731315,-7.433682356924,135.666328182428));
#80768=CARTESIAN_POINT('Ctrl Pts',(80.6411436826058,-7.46086112485284,135.660918140859));
#80769=CARTESIAN_POINT('Ctrl Pts',(80.7022977614075,-7.48778653667888,135.656126132143));
#80770=CARTESIAN_POINT('Ctrl Pts',(80.7807771079322,-7.52812876505948,135.649727624631));
#80771=CARTESIAN_POINT('Ctrl Pts',(80.7996977670178,-7.53832244032269,135.648164671113));
#80772=CARTESIAN_POINT('Ctrl Pts',(80.8801006239151,-7.58366874245671,135.641446320003));
#80773=CARTESIAN_POINT('Ctrl Pts',(80.9395080190151,-7.62235812846393,135.636290611703));
#80774=CARTESIAN_POINT('Ctrl Pts',(81.0324153518665,-7.69167750951371,135.628004396148));
#80775=CARTESIAN_POINT('Ctrl Pts',(81.067448260924,-7.7201000033821,135.624820979092));
#80776=CARTESIAN_POINT('Ctrl Pts',(81.1248650608886,-7.77068232619236,135.619507681416));
#80777=CARTESIAN_POINT('Ctrl Pts',(81.1478516576813,-7.79211749273543,135.617351926669));
#80778=CARTESIAN_POINT('Ctrl Pts',(81.1797385270572,-7.82358516594212,135.614317790017));
#80779=CARTESIAN_POINT('Ctrl Pts',(81.1891442511561,-7.83309348186384,135.61341707404));
#80780=CARTESIAN_POINT('Ctrl Pts',(81.2052988242849,-7.84982245432557,135.611859592708));
#80781=CARTESIAN_POINT('Ctrl Pts',(81.212099691251,-7.85699169377217,135.611200581259));
#80782=CARTESIAN_POINT('Ctrl Pts',(81.225987020049,-7.87189458022222,135.609847710728));
#80783=CARTESIAN_POINT('Ctrl Pts',(81.2330650526035,-7.87963550751747,135.609154228349));
#80784=CARTESIAN_POINT('Ctrl Pts',(81.2510679210011,-7.89970172342409,135.607379663128));
#80785=CARTESIAN_POINT('Ctrl Pts',(81.2618841183515,-7.91212328642472,135.606303130617));
#80786=CARTESIAN_POINT('Ctrl Pts',(81.3060213017579,-7.96435559340015,135.601863161036));
#80787=CARTESIAN_POINT('Ctrl Pts',(81.3376584174224,-8.00555455425008,135.598567361822));
#80788=CARTESIAN_POINT('Ctrl Pts',(81.4290417440531,-8.13682809789294,135.588570167249));
#80789=CARTESIAN_POINT('Ctrl Pts',(81.4819902394504,-8.23127956995287,135.582076927784));
#80790=CARTESIAN_POINT('Ctrl Pts',(81.5509065263991,-8.38822986804488,135.571521770207));
#80791=CARTESIAN_POINT('Ctrl Pts',(81.573054799165,-8.44766804635366,135.567567768311));
#80792=CARTESIAN_POINT('Ctrl Pts',(81.5961730984153,-8.52249523526723,135.5624786694));
#80793=CARTESIAN_POINT('Ctrl Pts',(81.6003922334336,-8.53683262034233,135.561498590011));
#80794=CARTESIAN_POINT('Ctrl Pts',(81.6063123207462,-8.55799751651901,135.560041845528));
#80795=CARTESIAN_POINT('Ctrl Pts',(81.6081639473392,-8.56478260467207,135.559573346392));
#80796=CARTESIAN_POINT('Ctrl Pts',(81.6112447696592,-8.57636009491999,135.558771079305));
#80797=CARTESIAN_POINT('Ctrl Pts',(81.6124956694893,-8.58114657470802,135.558438559297));
#80798=CARTESIAN_POINT('Ctrl Pts',(81.6153018703657,-8.59208320856258,135.557676796998));
#80799=CARTESIAN_POINT('Ctrl Pts',(81.6168433421262,-8.59823658105232,135.557246798334));
#80800=CARTESIAN_POINT('Ctrl Pts',(81.6210095297212,-8.61527986235172,135.556052223295));
#80801=CARTESIAN_POINT('Ctrl Pts',(81.6235595546928,-8.62618743317122,135.555283665678));
#80802=CARTESIAN_POINT('Ctrl Pts',(81.6380311793001,-8.69103206495627,135.550694045268));
#80803=CARTESIAN_POINT('Ctrl Pts',(81.6473730459765,-8.74550424502651,135.546755266948));
#80804=CARTESIAN_POINT('Ctrl Pts',(81.6657735937353,-8.89793009896356,135.535670640689));
#80805=CARTESIAN_POINT('Ctrl Pts',(81.6688943965567,-8.99638484146893,135.528451610779));
#80806=CARTESIAN_POINT('Ctrl Pts',(81.6591558999855,-9.16772160325569,135.516146491686));
#80807=CARTESIAN_POINT('Ctrl Pts',(81.6501708767704,-9.24055684332047,135.510994424597));
#80808=CARTESIAN_POINT('Ctrl Pts',(81.6331039422934,-9.32990751788484,135.504786234551));
#80809=CARTESIAN_POINT('Ctrl Pts',(81.6295174824161,-9.34718910235691,135.503590480379));
#80810=CARTESIAN_POINT('Ctrl Pts',(81.6233075931183,-9.37489174863058,135.501681038262));
#80811=CARTESIAN_POINT('Ctrl Pts',(81.6208568648414,-9.38534970884734,135.50096190772));
#80812=CARTESIAN_POINT('Ctrl Pts',(81.6159788225714,-9.40529536531078,135.499593359175));
#80813=CARTESIAN_POINT('Ctrl Pts',(81.6135686677059,-9.41478675210875,135.498943422501));
#80814=CARTESIAN_POINT('Ctrl Pts',(81.6078770675369,-9.43640007808269,135.497466114757));
#80815=CARTESIAN_POINT('Ctrl Pts',(81.6045419437463,-9.44850736624858,135.496640510046));
#80816=CARTESIAN_POINT('Ctrl Pts',(81.5952758385749,-9.48071851561596,135.494448385969));
#80817=CARTESIAN_POINT('Ctrl Pts',(81.5891017239668,-9.50075050282238,135.493089718617));
#80818=CARTESIAN_POINT('Ctrl Pts',(81.5445459236425,-9.63617791969349,135.483923553231));
#80819=CARTESIAN_POINT('Ctrl Pts',(81.4940074647466,-9.74718806594842,135.476540457815));
#80820=CARTESIAN_POINT('Ctrl Pts',(81.3837790771595,-9.93249414058302,135.463364246062));
#80821=CARTESIAN_POINT('Ctrl Pts',(81.3289859381131,-10.0090496467401,135.457602280899));
#80822=CARTESIAN_POINT('Ctrl Pts',(81.2601244677779,-10.0898584100671,135.450664997258));
#80823=CARTESIAN_POINT('Ctrl Pts',(81.2521049461546,-10.0990624234618,135.449861081478));
#80824=CARTESIAN_POINT('Ctrl Pts',(81.2396678243958,-10.1130237261968,135.448618845724));
#80825=CARTESIAN_POINT('Ctrl Pts',(81.2353221572715,-10.1178449329456,135.44818561919));
#80826=CARTESIAN_POINT('Ctrl Pts',(81.227257594154,-10.1266875338113,135.447382885672));
#80827=CARTESIAN_POINT('Ctrl Pts',(81.2235469049681,-10.1307161312871,135.447013981236));
#80828=CARTESIAN_POINT('Ctrl Pts',(81.2150363999968,-10.1398648162468,135.446168953998));
#80829=CARTESIAN_POINT('Ctrl Pts',(81.2102240540331,-10.1449729198564,135.445691906759));
#80830=CARTESIAN_POINT('Ctrl Pts',(81.1952123087992,-10.1607068855986,135.444206627641));
#80831=CARTESIAN_POINT('Ctrl Pts',(81.1849044847329,-10.1712276731728,135.443190763733));
#80832=CARTESIAN_POINT('Ctrl Pts',(81.0988458232378,-10.256765517001,135.434752255089));
#80833=CARTESIAN_POINT('Ctrl Pts',(81.0161997778977,-10.3244833604926,135.426934312391));
#80834=CARTESIAN_POINT('Ctrl Pts',(80.8353061284195,-10.4457460442801,135.411104789846));
#80835=CARTESIAN_POINT('Ctrl Pts',(80.7369720946791,-10.4982651805633,135.403144920433));
#80836=CARTESIAN_POINT('Ctrl Pts',(80.6161605284524,-10.547992071442,135.394204925114));
#80837=CARTESIAN_POINT('Ctrl Pts',(80.598071040794,-10.5550705243262,135.392886284624));
#80838=CARTESIAN_POINT('Ctrl Pts',(80.5694364803041,-10.5657016797744,135.390829320125));
#80839=CARTESIAN_POINT('Ctrl Pts',(80.5589730388702,-10.5694676827981,135.390083958867));
#80840=CARTESIAN_POINT('Ctrl Pts',(80.5392916467636,-10.5763296142076,135.388693412042));
#80841=CARTESIAN_POINT('Ctrl Pts',(80.5300828352837,-10.5794501345361,135.388047437203));
#80842=CARTESIAN_POINT('Ctrl Pts',(80.5093328547878,-10.586279603908,135.386602033777));
#80843=CARTESIAN_POINT('Ctrl Pts',(80.4977773822075,-10.5899435931722,135.385804108222));
#80844=CARTESIAN_POINT('Ctrl Pts',(80.463642447802,-10.600358409488,135.383466769636));
#80845=CARTESIAN_POINT('Ctrl Pts',(80.4409579774769,-10.6067568296459,135.381938778431));
#80846=CARTESIAN_POINT('Ctrl Pts',(80.3161426684702,-10.6391197809079,135.373654915505));
#80847=CARTESIAN_POINT('Ctrl Pts',(80.2118579831632,-10.6558319590356,135.367201924982));
#80848=CARTESIAN_POINT('Ctrl Pts',(80.0295678783465,-10.667529009758,135.35604724617));
#80849=CARTESIAN_POINT('Ctrl Pts',(79.9522071013403,-10.667105701846,135.351345090981));
#80850=CARTESIAN_POINT('Ctrl Pts',(79.8507915989673,-10.6594848858688,135.344929142454));
#80851=CARTESIAN_POINT('Ctrl Pts',(79.8264664511588,-10.6571177433717,135.343370694582));
#80852=CARTESIAN_POINT('Ctrl Pts',(79.7852781773838,-10.6521928158553,135.340685425391));
#80853=CARTESIAN_POINT('Ctrl Pts',(79.768385721024,-10.649909492222,135.339570767969));
#80854=CARTESIAN_POINT('Ctrl Pts',(79.7442039282953,-10.6462622188573,135.337952074943));
#80855=CARTESIAN_POINT('Ctrl Pts',(79.7368834012025,-10.6451080735904,135.337459006005));
#80856=CARTESIAN_POINT('Ctrl Pts',(79.7241383466785,-10.6430114608672,135.336594876149));
#80857=CARTESIAN_POINT('Ctrl Pts',(79.7187104050076,-10.6420908851305,135.336225039383));
#80858=CARTESIAN_POINT('Ctrl Pts',(79.7070674607948,-10.6400568253947,135.335427718297));
#80859=CARTESIAN_POINT('Ctrl Pts',(79.7008542976147,-10.6389349311296,135.334999799894));
#80860=CARTESIAN_POINT('Ctrl Pts',(79.6837660876834,-10.6357489539311,135.333816455222));
#80861=CARTESIAN_POINT('Ctrl Pts',(79.6729052346935,-10.6336118038436,135.333057163494));
#80862=CARTESIAN_POINT('Ctrl Pts',(79.6106132183702,-10.6207081829048,135.328663973521));
#80863=CARTESIAN_POINT('Ctrl Pts',(79.5596977218537,-10.6076224190586,135.324923422212));
#80864=CARTESIAN_POINT('Ctrl Pts',(79.4119688331959,-10.5621103152775,135.313777811983));
#80865=CARTESIAN_POINT('Ctrl Pts',(79.3174060645967,-10.5231666383592,135.30627757059));
#80866=CARTESIAN_POINT('Ctrl Pts',(79.1627104076536,-10.4421405968979,135.29376097206));
#80867=CARTESIAN_POINT('Ctrl Pts',(79.1006810571642,-10.4042974786623,135.288661548636));
#80868=CARTESIAN_POINT('Ctrl Pts',(79.0269119784182,-10.3523925634111,135.282506069526));
#80869=CARTESIAN_POINT('Ctrl Pts',(79.0126747455877,-10.3420338395948,135.281313284718));
#80870=CARTESIAN_POINT('Ctrl Pts',(78.9900273057665,-10.3250004996883,135.279407413584));
#80871=CARTESIAN_POINT('Ctrl Pts',(78.9815130725154,-10.3184671232668,135.278688921181));
#80872=CARTESIAN_POINT('Ctrl Pts',(78.9653497333927,-10.3058142146827,135.277320854322));
#80873=CARTESIAN_POINT('Ctrl Pts',(78.9576903362711,-10.2997086247869,135.276670768132));
#80874=CARTESIAN_POINT('Ctrl Pts',(78.9403207371306,-10.2856103662315,135.275192121867));
#80875=CARTESIAN_POINT('Ctrl Pts',(78.9306462211732,-10.2775745238718,135.274365339721));
#80876=CARTESIAN_POINT('Ctrl Pts',(78.9050436637096,-10.2558139364783,135.272167857993));
#80877=CARTESIAN_POINT('Ctrl Pts',(78.889282561388,-10.2418956704791,135.270805072906));
#80878=CARTESIAN_POINT('Ctrl Pts',(78.7850070921004,-10.14623881434,135.261708140156));
#80879=CARTESIAN_POINT('Ctrl Pts',(78.7053199332686,-10.0554044504728,135.254389242633));
#80880=CARTESIAN_POINT('Ctrl Pts',(78.5979474577496,-9.90234316385511,135.242965047997));
#80881=CARTESIAN_POINT('Ctrl Pts',(78.5630672644076,-9.84569353518899,135.238892805906));
#80882=CARTESIAN_POINT('Ctrl Pts',(78.5210386775775,-9.76729096251886,135.233262995623));
#80883=CARTESIAN_POINT('Ctrl Pts',(78.5108139771359,-9.74725290405196,135.231824451065));
#80884=CARTESIAN_POINT('Ctrl Pts',(78.4940058356331,-9.71259691109633,135.229326584376));
#80885=CARTESIAN_POINT('Ctrl Pts',(78.4872217572517,-9.69807930979763,135.228277306131));
#80886=CARTESIAN_POINT('Ctrl Pts',(78.4776817946995,-9.67687190456469,135.226737085544));
#80887=CARTESIAN_POINT('Ctrl Pts',(78.4747581868851,-9.67025793547792,135.226255699886));
#80888=CARTESIAN_POINT('Ctrl Pts',(78.4697121609575,-9.65863851063518,135.225407831745));
#80889=CARTESIAN_POINT('Ctrl Pts',(78.4675710450408,-9.65364138088882,135.225042481567));
#80890=CARTESIAN_POINT('Ctrl Pts',(78.4629609835975,-9.64273484113436,135.224243442312));
#80891=CARTESIAN_POINT('Ctrl Pts',(78.4605016793919,-9.63682174220386,135.223809222955));
#80892=CARTESIAN_POINT('Ctrl Pts',(78.4537321835503,-9.62027691535868,135.222591756587));
#80893=CARTESIAN_POINT('Ctrl Pts',(78.4494977238917,-9.60961486653051,135.22180428773));
#80894=CARTESIAN_POINT('Ctrl Pts',(78.4217951171761,-9.5377056080225,135.216477923464));
#80895=CARTESIAN_POINT('Ctrl Pts',(78.4018538674087,-9.47516838486711,135.211773439132));
#80896=CARTESIAN_POINT('Ctrl Pts',(78.3800892955835,-9.38981046480314,135.205388297193));
#80897=CARTESIAN_POINT('Ctrl Pts',(78.3749694674895,-9.36788399828525,135.203750981773));
#80898=CARTESIAN_POINT('Ctrl Pts',(78.3556833956392,-9.27700755545551,135.19698965436));
#80899=CARTESIAN_POINT('Ctrl Pts',(78.3454484878604,-9.20729362310927,135.191865040038));
#80900=CARTESIAN_POINT('Ctrl Pts',(78.3359116043374,-9.09182965559912,135.183580428998));
#80901=CARTESIAN_POINT('Ctrl Pts',(78.3340252030434,-9.04638382201416,135.180369756322));
#80902=CARTESIAN_POINT('Ctrl Pts',(78.3339832799272,-8.96998909899421,135.175064092908));
#80903=CARTESIAN_POINT('Ctrl Pts',(78.3348273798544,-8.93906781637886,135.172941563736));
#80904=CARTESIAN_POINT('Ctrl Pts',(78.3372103811871,-8.89589301781814,135.170011160881));
#80905=CARTESIAN_POINT('Ctrl Pts',(78.3380251523454,-8.88360756007382,135.169181059222));
#80906=CARTESIAN_POINT('Ctrl Pts',(78.3396793289291,-8.86225317288682,135.167744421283));
#80907=CARTESIAN_POINT('Ctrl Pts',(78.3404570346014,-8.85318014152402,135.167135983822));
#80908=CARTESIAN_POINT('Ctrl Pts',(78.3422420209813,-8.8341871814754,135.165866241765));
#80909=CARTESIAN_POINT('Ctrl Pts',(78.3432640458672,-8.82426897422111,135.165205425325));
#80910=CARTESIAN_POINT('Ctrl Pts',(78.3459230567602,-8.80055461789486,135.163630478538));
#80911=CARTESIAN_POINT('Ctrl Pts',(78.3476437063625,-8.78676845266505,135.162719006752));
#80912=CARTESIAN_POINT('Ctrl Pts',(78.3542717192831,-8.73857666057836,135.159545682791));
#80913=CARTESIAN_POINT('Ctrl Pts',(78.3600831270989,-8.70430309960197,135.157312114117));
#80914=CARTESIAN_POINT('Ctrl Pts',(78.3772529875,-8.61927597781728,135.151806430982));
#80915=CARTESIAN_POINT('Ctrl Pts',(78.3899232382344,-8.56882477145895,135.148572223972));
#80916=CARTESIAN_POINT('Ctrl Pts',(78.4145339022593,-8.48720443493499,135.143322354091));
#80917=CARTESIAN_POINT('Ctrl Pts',(78.4250815971791,-8.45567289096299,135.141289461639));
#80918=CARTESIAN_POINT('Ctrl Pts',(78.4365593350865,-8.42449214836376,135.139259965645));
#80919=CARTESIAN_POINT('Ctrl Pts',(78.4365593749993,-8.42449203993567,135.330578627164));
#80920=CARTESIAN_POINT('Ctrl Pts',(78.4355262731809,-8.42729859251999,135.330779522923));
#80921=CARTESIAN_POINT('Ctrl Pts',(78.4345007399363,-8.43010789542315,135.330980874855));
#80922=CARTESIAN_POINT('Ctrl Pts',(78.4313071291383,-8.4389300126237,135.331613988554));
#80923=CARTESIAN_POINT('Ctrl Pts',(78.4291661459327,-8.44495238644834,135.332047339247));
#80924=CARTESIAN_POINT('Ctrl Pts',(78.4232962774157,-8.46176974445812,135.333260392863));
#80925=CARTESIAN_POINT('Ctrl Pts',(78.4196437473155,-8.47259073441824,135.33404427212));
#80926=CARTESIAN_POINT('Ctrl Pts',(78.3963375081978,-8.54405437768576,135.339239248275));
#80927=CARTESIAN_POINT('Ctrl Pts',(78.380069099068,-8.60573882491424,135.343806912988));
#80928=CARTESIAN_POINT('Ctrl Pts',(78.3452668310428,-8.77698147651284,135.356465494113));
#80929=CARTESIAN_POINT('Ctrl Pts',(78.3340839882609,-8.88771739067351,135.364607438158));
#80930=CARTESIAN_POINT('Ctrl Pts',(78.333960105889,-9.05240943781643,135.376277053692));
#80931=CARTESIAN_POINT('Ctrl Pts',(78.3365124688393,-9.10604720710605,135.380013448242));
#80932=CARTESIAN_POINT('Ctrl Pts',(78.3432447666648,-9.17605568673706,135.38480577823));
#80933=CARTESIAN_POINT('Ctrl Pts',(78.3450880338692,-9.19261341434206,135.385933121138));
#80934=CARTESIAN_POINT('Ctrl Pts',(78.3485009066,-9.21958497765593,135.387760146348));
#80935=CARTESIAN_POINT('Ctrl Pts',(78.3499213966887,-9.23001615073439,135.38846445472));
#80936=CARTESIAN_POINT('Ctrl Pts',(78.3528637800764,-9.25019094399288,135.389822463916));
#80937=CARTESIAN_POINT('Ctrl Pts',(78.3543734966964,-9.25993586552764,135.390476517913));
#80938=CARTESIAN_POINT('Ctrl Pts',(78.3581156895823,-9.2827502210897,135.392003607387));
#80939=CARTESIAN_POINT('Ctrl Pts',(78.3604178536093,-9.29580767130029,135.392874406126));
#80940=CARTESIAN_POINT('Ctrl Pts',(78.3685721444306,-9.33903308249695,135.395747686064));
#80941=CARTESIAN_POINT('Ctrl Pts',(78.3751032126185,-9.36906760960462,135.397728732291));
#80942=CARTESIAN_POINT('Ctrl Pts',(78.3929306864518,-9.44135689561609,135.402474141945));
#80943=CARTESIAN_POINT('Ctrl Pts',(78.4050672096251,-9.48338131303913,135.405213412114));
#80944=CARTESIAN_POINT('Ctrl Pts',(78.4417659737733,-9.59393279114656,135.412431973884));
#80945=CARTESIAN_POINT('Ctrl Pts',(78.469187338651,-9.66140939121931,135.416848648503));
#80946=CARTESIAN_POINT('Ctrl Pts',(78.5082912027581,-9.74205483343944,135.422331578807));
#80947=CARTESIAN_POINT('Ctrl Pts',(78.515880497758,-9.75711941162343,135.423365183253));
#80948=CARTESIAN_POINT('Ctrl Pts',(78.5569116448512,-9.83557695259039,135.428809900326));
#80949=CARTESIAN_POINT('Ctrl Pts',(78.5941858934046,-9.8968706349051,135.433275373302));
#80950=CARTESIAN_POINT('Ctrl Pts',(78.6419287095258,-9.96505573471517,135.438720124378));
#80951=CARTESIAN_POINT('Ctrl Pts',(78.6486718028772,-9.97447539032831,135.439483560455));
#80952=CARTESIAN_POINT('Ctrl Pts',(78.6593083965521,-9.98901129735335,135.440680591179));
#80953=CARTESIAN_POINT('Ctrl Pts',(78.663134361529,-9.99417683691514,135.441109752094));
#80954=CARTESIAN_POINT('Ctrl Pts',(78.6702479461729,-10.0036657685702,135.441905374871));
#80955=CARTESIAN_POINT('Ctrl Pts',(78.6735269311231,-10.007995383969,135.442271249124));
#80956=CARTESIAN_POINT('Ctrl Pts',(78.681196117597,-10.0180196570363,135.443124945014));
#80957=CARTESIAN_POINT('Ctrl Pts',(78.6856020548501,-10.0237019777944,135.443613838057));
#80958=CARTESIAN_POINT('Ctrl Pts',(78.6998089743626,-10.0417816718146,135.445184867954));
#80959=CARTESIAN_POINT('Ctrl Pts',(78.7097492965875,-10.0540677548791,135.446275989853));
#80960=CARTESIAN_POINT('Ctrl Pts',(78.765725932875,-10.1212757113765,135.452367858337));
#80961=CARTESIAN_POINT('Ctrl Pts',(78.8150903471115,-10.1733195593721,135.457545086692));
#80962=CARTESIAN_POINT('Ctrl Pts',(78.9644272114544,-10.3116989777376,135.472346540187));
#80963=CARTESIAN_POINT('Ctrl Pts',(79.071539327848,-10.3895819502659,135.48195518204));
#80964=CARTESIAN_POINT('Ctrl Pts',(79.2105803728829,-10.4673510817889,135.492967535828));
#80965=CARTESIAN_POINT('Ctrl Pts',(79.2347523357253,-10.4801009121257,135.49483611561));
#80966=CARTESIAN_POINT('Ctrl Pts',(79.2704566879891,-10.4978249903886,135.497531647256));
#80967=CARTESIAN_POINT('Ctrl Pts',(79.2817479146326,-10.5032721319534,135.498374910287));
#80968=CARTESIAN_POINT('Ctrl Pts',(79.3019621659085,-10.5127441847858,135.499868658346));
#80969=CARTESIAN_POINT('Ctrl Pts',(79.3108610900638,-10.5168188277655,135.500520834889));
#80970=CARTESIAN_POINT('Ctrl Pts',(79.3296060676239,-10.5252027651225,135.501883523649));
#80971=CARTESIAN_POINT('Ctrl Pts',(79.3394589820578,-10.5294956920664,135.502593452478));
#80972=CARTESIAN_POINT('Ctrl Pts',(79.3656344908504,-10.5406002723171,135.504463244113));
#80973=CARTESIAN_POINT('Ctrl Pts',(79.3820254762902,-10.5472479844239,135.505617550118));
#80974=CARTESIAN_POINT('Ctrl Pts',(79.4675328256897,-10.5803516593296,135.511559140819));
#80975=CARTESIAN_POINT('Ctrl Pts',(79.5382541497404,-10.6024435799612,135.516199475138));
#80976=CARTESIAN_POINT('Ctrl Pts',(79.6749347772821,-10.6353346536221,135.524873631087));
#80977=CARTESIAN_POINT('Ctrl Pts',(79.740527048473,-10.6470157161123,135.528914623565));
#80978=CARTESIAN_POINT('Ctrl Pts',(79.8206909608897,-10.6563829005471,135.533855450762));
#80979=CARTESIAN_POINT('Ctrl Pts',(79.8347593096595,-10.6578454547886,135.534722736919));
#80980=CARTESIAN_POINT('Ctrl Pts',(79.9199176347961,-10.6656038366701,135.539981924922));
#80981=CARTESIAN_POINT('Ctrl Pts',(79.9913248241879,-10.6675045693128,135.544429406272));
#80982=CARTESIAN_POINT('Ctrl Pts',(80.0741971314396,-10.6643872492668,135.549854100756));
#80983=CARTESIAN_POINT('Ctrl Pts',(80.0857651395046,-10.6638312571511,135.550617338171));
#80984=CARTESIAN_POINT('Ctrl Pts',(80.1037425554612,-10.6627792382724,135.551814122857));
#80985=CARTESIAN_POINT('Ctrl Pts',(80.1101567392705,-10.6623666269425,135.552243239286));
#80986=CARTESIAN_POINT('Ctrl Pts',(80.121986385737,-10.6615368856644,135.553038824661));
#80987=CARTESIAN_POINT('Ctrl Pts',(80.1274023929413,-10.6611303765512,135.553404706496));
#80988=CARTESIAN_POINT('Ctrl Pts',(80.1399848362193,-10.6601240804651,135.554258479652));
#80989=CARTESIAN_POINT('Ctrl Pts',(80.1471494414926,-10.6595043699788,135.55474744305));
#80990=CARTESIAN_POINT('Ctrl Pts',(80.1700509051904,-10.6573740136638,135.556318929629));
#80991=CARTESIAN_POINT('Ctrl Pts',(80.1857698246274,-10.6556857970013,135.557410444924));
#80992=CARTESIAN_POINT('Ctrl Pts',(80.2726555271094,-10.645101442159,135.563506691196));
#80993=CARTESIAN_POINT('Ctrl Pts',(80.343208373796,-10.6318412242077,135.568688160618));
#80994=CARTESIAN_POINT('Ctrl Pts',(80.5406842505535,-10.5813515668489,135.583506823124));
#80995=CARTESIAN_POINT('Ctrl Pts',(80.6643665785313,-10.533506233294,135.593127914921));
#80996=CARTESIAN_POINT('Ctrl Pts',(80.8027279036113,-10.4600626944706,135.603953904724));
#80997=CARTESIAN_POINT('Ctrl Pts',(80.8240938879187,-10.4481106769402,135.605629490446));
#80998=CARTESIAN_POINT('Ctrl Pts',(80.8557920351668,-10.4294500195427,135.608122229329));
#80999=CARTESIAN_POINT('Ctrl Pts',(80.8663251096201,-10.4230910667889,135.608951732539));
#81000=CARTESIAN_POINT('Ctrl Pts',(80.8845267145437,-10.4118255350073,135.610387517227));
#81001=CARTESIAN_POINT('Ctrl Pts',(80.8922271441489,-10.4069717761769,135.610995695854));
#81002=CARTESIAN_POINT('Ctrl Pts',(80.9082769064928,-10.3966704823726,135.612265067652));
#81003=CARTESIAN_POINT('Ctrl Pts',(80.9166179243367,-10.3912106107022,135.612925771662));
#81004=CARTESIAN_POINT('Ctrl Pts',(80.9364662765708,-10.3779622539267,135.614500758185));
#81005=CARTESIAN_POINT('Ctrl Pts',(80.9479262877194,-10.3701039496195,135.615412379409));
#81006=CARTESIAN_POINT('Ctrl Pts',(80.9877255006586,-10.3420745969456,135.618587853349));
#81007=CARTESIAN_POINT('Ctrl Pts',(81.0155312863061,-10.3211594779654,135.620823364375));
#81008=CARTESIAN_POINT('Ctrl Pts',(81.0832652078284,-10.2668079721503,135.626335306234));
#81009=CARTESIAN_POINT('Ctrl Pts',(81.122319498465,-10.2323414716649,135.629573705253));
#81010=CARTESIAN_POINT('Ctrl Pts',(81.2309895076531,-10.1269787610188,135.638894482858));
#81011=CARTESIAN_POINT('Ctrl Pts',(81.2959547269485,-10.0516254042706,135.644863331075));
#81012=CARTESIAN_POINT('Ctrl Pts',(81.382547020713,-9.93088625497374,135.654121892469));
#81013=CARTESIAN_POINT('Ctrl Pts',(81.409478425099,-9.88958139409313,135.657244839241));
#81014=CARTESIAN_POINT('Ctrl Pts',(81.4400707768826,-9.83777717851968,135.661186634006));
#81015=CARTESIAN_POINT('Ctrl Pts',(81.4455126450187,-9.8283523531352,135.661904756946));
#81016=CARTESIAN_POINT('Ctrl Pts',(81.4539437423657,-9.81341435590741,135.663045603797));
#81017=CARTESIAN_POINT('Ctrl Pts',(81.4569949572909,-9.80793626701459,135.663464532077));
#81018=CARTESIAN_POINT('Ctrl Pts',(81.4626707874389,-9.79760928253296,135.664255563397));
#81019=CARTESIAN_POINT('Ctrl Pts',(81.4653023458829,-9.79276442375454,135.664627224973));
#81020=CARTESIAN_POINT('Ctrl Pts',(81.4714485719595,-9.78131369534124,135.665506853635));
#81021=CARTESIAN_POINT('Ctrl Pts',(81.4749428358345,-9.77469711248493,135.666016058988));
#81022=CARTESIAN_POINT('Ctrl Pts',(81.4864475524603,-9.75255230236352,135.667722829231));
#81023=CARTESIAN_POINT('Ctrl Pts',(81.4942579700291,-9.73692221625749,135.668931602659));
#81024=CARTESIAN_POINT('Ctrl Pts',(81.5127597045187,-9.69839291856715,135.671916234599));
#81025=CARTESIAN_POINT('Ctrl Pts',(81.5231783781498,-9.67536810898402,135.673703974035));
#81026=CARTESIAN_POINT('Ctrl Pts',(81.5653168624551,-9.57630423285464,135.681388211939));
#81027=CARTESIAN_POINT('Ctrl Pts',(81.5918958839658,-9.49820694710658,135.687421128465));
#81028=CARTESIAN_POINT('Ctrl Pts',(81.6373188618132,-9.3231666259707,135.700553726765));
#81029=CARTESIAN_POINT('Ctrl Pts',(81.6535561297683,-9.22584859002855,135.707600033417));
#81030=CARTESIAN_POINT('Ctrl Pts',(81.6629242930125,-9.10394338421816,135.716018745893));
#81031=CARTESIAN_POINT('Ctrl Pts',(81.6642385471,-9.08019720024782,135.717640650187));
#81032=CARTESIAN_POINT('Ctrl Pts',(81.6654560444901,-9.0442732278568,135.720068345016));
#81033=CARTESIAN_POINT('Ctrl Pts',(81.6657349069284,-9.03211212056762,135.720885697022));
#81034=CARTESIAN_POINT('Ctrl Pts',(81.665996994287,-9.01022574073723,135.722348953673));
#81035=CARTESIAN_POINT('Ctrl Pts',(81.6660283028545,-9.00050171167892,135.722996327569));
#81036=CARTESIAN_POINT('Ctrl Pts',(81.6659131095358,-8.97969226939058,135.72437608127));
#81037=CARTESIAN_POINT('Ctrl Pts',(81.6657410988884,-8.9686074226696,135.725107634832));
#81038=CARTESIAN_POINT('Ctrl Pts',(81.6649671608321,-8.93826114098241,135.727101556844));
#81039=CARTESIAN_POINT('Ctrl Pts',(81.664141663783,-8.9190067518587,135.728356943319));
#81040=CARTESIAN_POINT('Ctrl Pts',(81.6615608590606,-8.87618676336635,135.731130043053));
#81041=CARTESIAN_POINT('Ctrl Pts',(81.6596378892046,-8.85263526330765,135.732642580561));
#81042=CARTESIAN_POINT('Ctrl Pts',(81.6518941871683,-8.7775307674222,135.73743506905));
#81043=CARTESIAN_POINT('Ctrl Pts',(81.644166459128,-8.72620404349717,135.740662579849));
#81044=CARTESIAN_POINT('Ctrl Pts',(81.6143429736189,-8.5761085532356,135.750087170798));
#81045=CARTESIAN_POINT('Ctrl Pts',(81.5856374198292,-8.4789056373043,135.756163698559));
#81046=CARTESIAN_POINT('Ctrl Pts',(81.5306223575826,-8.34042224827635,135.765459430542));
#81047=CARTESIAN_POINT('Ctrl Pts',(81.5110408417259,-8.29672035167029,135.768495872958));
#81048=CARTESIAN_POINT('Ctrl Pts',(81.484709148366,-8.24414658279281,135.772348989523));
#81049=CARTESIAN_POINT('Ctrl Pts',(81.4797147453269,-8.23441532126142,135.773070896926));
#81050=CARTESIAN_POINT('Ctrl Pts',(81.4717307334529,-8.21922901368865,135.77421232156));
#81051=CARTESIAN_POINT('Ctrl Pts',(81.4688056690406,-8.21374012674534,135.774627948916));
#81052=CARTESIAN_POINT('Ctrl Pts',(81.4632234080043,-8.20340486698522,135.775416622239));
#81053=CARTESIAN_POINT('Ctrl Pts',(81.4605727448325,-8.19855517904087,135.775789265932));
#81054=CARTESIAN_POINT('Ctrl Pts',(81.4542296989428,-8.18708583695093,135.776676565089));
#81055=CARTESIAN_POINT('Ctrl Pts',(81.4505162124318,-8.18047808713489,135.777192523295));
#81056=CARTESIAN_POINT('Ctrl Pts',(81.4378056838691,-8.15821810702523,135.778946253225));
#81057=CARTESIAN_POINT('Ctrl Pts',(81.4285997029371,-8.14268747666244,135.780196060627));
#81058=CARTESIAN_POINT('Ctrl Pts',(81.4053049045252,-8.10480612435782,135.783304139457));
#81059=CARTESIAN_POINT('Ctrl Pts',(81.3909335584144,-8.08263549696637,135.785175512523));
#81060=CARTESIAN_POINT('Ctrl Pts',(81.3252956707159,-7.98646626025524,135.793497616316));
#81061=CARTESIAN_POINT('Ctrl Pts',(81.26860812812,-7.91635236270762,135.800103414872));
#81062=CARTESIAN_POINT('Ctrl Pts',(81.1391697945811,-7.78041330523172,135.813702478902));
#81063=CARTESIAN_POINT('Ctrl Pts',(81.0657024735681,-7.71571665043239,135.820650802584));
#81064=CARTESIAN_POINT('Ctrl Pts',(80.9717693841213,-7.64664250173487,135.828623028917));
#81065=CARTESIAN_POINT('Ctrl Pts',(80.9563739679159,-7.63571955288704,135.829903684356));
#81066=CARTESIAN_POINT('Ctrl Pts',(80.9317161631004,-7.61884757330649,135.831914990394));
#81067=CARTESIAN_POINT('Ctrl Pts',(80.9225751423151,-7.61272491870699,135.832652169005));
#81068=CARTESIAN_POINT('Ctrl Pts',(80.9060466132159,-7.60188974071801,135.83397030598));
#81069=CARTESIAN_POINT('Ctrl Pts',(80.8986813826161,-7.59714414853699,135.834552484362));
#81070=CARTESIAN_POINT('Ctrl Pts',(80.8812946553441,-7.5861345938802,135.835914874432));
#81071=CARTESIAN_POINT('Ctrl Pts',(80.8712431798858,-7.57991866792703,135.836693293865));
#81072=CARTESIAN_POINT('Ctrl Pts',(80.8415942605421,-7.56201680171253,135.838963380257));
#81073=CARTESIAN_POINT('Ctrl Pts',(80.8218214048979,-7.55062557014839,135.84044437985));
#81074=CARTESIAN_POINT('Ctrl Pts',(80.7294265454685,-7.49989545581792,135.84722515247));
#81075=CARTESIAN_POINT('Ctrl Pts',(80.654173556158,-7.46558284756121,135.852348990203));
#81076=CARTESIAN_POINT('Ctrl Pts',(80.5228555594444,-7.41713257439729,135.860930630532));
#81077=CARTESIAN_POINT('Ctrl Pts',(80.4680435725637,-7.40006801321869,135.864415508163));
#81078=CARTESIAN_POINT('Ctrl Pts',(80.3378013276486,-7.36678712508914,135.87266519345));
#81079=CARTESIAN_POINT('Ctrl Pts',(80.261917391431,-7.3529146397612,135.877448117471));
#81080=CARTESIAN_POINT('Ctrl Pts',(80.1738222333491,-7.34305203519499,135.883246277199));
#81081=CARTESIAN_POINT('Ctrl Pts',(80.1622743212221,-7.34188126087881,135.88401117691));
#81082=CARTESIAN_POINT('Ctrl Pts',(80.1443086467896,-7.34024929546995,135.885210020238));
#81083=CARTESIAN_POINT('Ctrl Pts',(80.1378985913507,-7.33970443542221,135.885639508796));
#81084=CARTESIAN_POINT('Ctrl Pts',(80.1260719757006,-7.33876812311061,135.886435407561));
#81085=CARTESIAN_POINT('Ctrl Pts',(80.1206564601087,-7.33836601280564,135.886801226508));
#81086=CARTESIAN_POINT('Ctrl Pts',(80.1080733090859,-7.33749353220929,135.88765435572));
#81087=CARTESIAN_POINT('Ctrl Pts',(80.10090453398,-7.33704303548779,135.888142732459));
#81088=CARTESIAN_POINT('Ctrl Pts',(80.0779955381416,-7.33575207444401,135.889710413694));
#81089=CARTESIAN_POINT('Ctrl Pts',(80.0622467464349,-7.33508866325179,135.890798651506));
#81090=CARTESIAN_POINT('Ctrl Pts',(79.9752685816344,-7.33266049192449,135.896858503602));
#81091=CARTESIAN_POINT('Ctrl Pts',(79.903998064701,-7.33524346902666,135.902004727388));
#81092=CARTESIAN_POINT('Ctrl Pts',(79.7031389500549,-7.35546489389957,135.916680042758));
#81093=CARTESIAN_POINT('Ctrl Pts',(79.5751233401283,-7.38379657932082,135.926197246953));
#81094=CARTESIAN_POINT('Ctrl Pts',(79.4247905605017,-7.43618944298602,135.937216846116));
#81095=CARTESIAN_POINT('Ctrl Pts',(79.3981039063056,-7.4462655878706,135.939169120612));
#81096=CARTESIAN_POINT('Ctrl Pts',(79.3598841193415,-7.46182898078638,135.941961042852));
#81097=CARTESIAN_POINT('Ctrl Pts',(79.3481358788281,-7.46677085593219,135.942818695584));
#81098=CARTESIAN_POINT('Ctrl Pts',(79.3274407337455,-7.47575710545454,135.944328877299));
#81099=CARTESIAN_POINT('Ctrl Pts',(79.318470826052,-7.47974661311075,135.944983228999));
#81100=CARTESIAN_POINT('Ctrl Pts',(79.2998474467593,-7.48822761314794,135.946341605517));
#81101=CARTESIAN_POINT('Ctrl Pts',(79.29020068965,-7.49273283875478,135.947045123891));
#81102=CARTESIAN_POINT('Ctrl Pts',(79.2650683210252,-7.50476494852482,135.948878148297));
#81103=CARTESIAN_POINT('Ctrl Pts',(79.2496547838107,-7.51244007699564,135.950002494021));
#81104=CARTESIAN_POINT('Ctrl Pts',(79.1751894718625,-7.55097185824301,135.955439589461));
#81105=CARTESIAN_POINT('Ctrl Pts',(79.1179023373438,-7.58511476559386,135.959635254769));
#81106=CARTESIAN_POINT('Ctrl Pts',(79.003133893035,-7.66320395638896,135.968233678969));
#81107=CARTESIAN_POINT('Ctrl Pts',(78.9461595717073,-7.70764309423015,135.972615160241));
#81108=CARTESIAN_POINT('Ctrl Pts',(78.8767632322408,-7.7694209105575,135.978299452942));
#81109=CARTESIAN_POINT('Ctrl Pts',(78.861538488781,-7.78349225383452,135.979570351591));
#81110=CARTESIAN_POINT('Ctrl Pts',(78.7978289407144,-7.84461894982535,135.985009900097));
#81111=CARTESIAN_POINT('Ctrl Pts',(78.7519736357233,-7.89431081429408,135.989231822588));
#81112=CARTESIAN_POINT('Ctrl Pts',(78.7019843304581,-7.95556523047784,135.994404286884));
#81113=CARTESIAN_POINT('Ctrl Pts',(78.6947948037225,-7.96456383893094,135.995163433037));
#81114=CARTESIAN_POINT('Ctrl Pts',(78.6837483313387,-7.97868776737917,135.996355150152));
#81115=CARTESIAN_POINT('Ctrl Pts',(78.679826545077,-7.98376224374992,135.996783349626));
#81116=CARTESIAN_POINT('Ctrl Pts',(78.6726364699279,-7.99317748214126,135.997578167998));
#81117=CARTESIAN_POINT('Ctrl Pts',(78.6693599973233,-7.99751174392324,135.997944210028));
#81118=CARTESIAN_POINT('Ctrl Pts',(78.6617836346137,-8.00763666952269,135.998799593189));
#81119=CARTESIAN_POINT('Ctrl Pts',(78.6575001050023,-8.01343928349378,135.999290020375));
#81120=CARTESIAN_POINT('Ctrl Pts',(78.6438794019379,-8.03214331960909,136.00087102896));
#81121=CARTESIAN_POINT('Ctrl Pts',(78.6346898176738,-8.04515043595365,136.001970750449));
#81122=CARTESIAN_POINT('Ctrl Pts',(78.6130766642929,-8.07669209918186,136.004634366466));
#81123=CARTESIAN_POINT('Ctrl Pts',(78.6008364311504,-8.09534811887406,136.006207249543));
#81124=CARTESIAN_POINT('Ctrl Pts',(78.5275463265607,-8.21210045116397,136.016009681774));
#81125=CARTESIAN_POINT('Ctrl Pts',(78.4764681494425,-8.31607477521382,136.024536811395));
#81126=CARTESIAN_POINT('Ctrl Pts',(78.4365593762033,-8.4244920366647,136.032852185112));
#81127=CARTESIAN_POINT('Origin',(80.,-9.,134.));
#81128=CARTESIAN_POINT('',(78.4365593881204,-8.4244920042904,136.733447186333));
#81129=CARTESIAN_POINT('',(78.4365593622862,-8.42449207447235,136.539851301691));
#81130=CARTESIAN_POINT('',(78.4365593749993,-8.42449203993574,134.));
#81131=CARTESIAN_POINT('',(78.3340002443612,-9.00090233676016,135.879690672883));
#81132=CARTESIAN_POINT('Ctrl Pts',(78.4365593622862,-8.42449207447235,136.539851301691));
#81133=CARTESIAN_POINT('Ctrl Pts',(78.4458979984507,-8.39912247896779,136.537889787967));
#81134=CARTESIAN_POINT('Ctrl Pts',(78.455854587738,-8.37397895835581,136.535921247526));
#81135=CARTESIAN_POINT('Ctrl Pts',(78.5134129738292,-8.23836951363643,136.52519748894));
#81136=CARTESIAN_POINT('Ctrl Pts',(78.5722644369613,-8.13304953404382,136.516515178362));
#81137=CARTESIAN_POINT('Ctrl Pts',(78.6541410729474,-8.01782782744679,136.506791211876));
#81138=CARTESIAN_POINT('Ctrl Pts',(78.6666490233352,-8.00091358175776,136.505356289194));
#81139=CARTESIAN_POINT('Ctrl Pts',(78.6871436587462,-7.97426979666754,136.503082992003));
#81140=CARTESIAN_POINT('Ctrl Pts',(78.6949257154184,-7.96438648638276,136.502236777347));
#81141=CARTESIAN_POINT('Ctrl Pts',(78.7089655621025,-7.94696532582124,136.500739525924));
#81142=CARTESIAN_POINT('Ctrl Pts',(78.7151792254797,-7.93939284875827,136.500086772006));
#81143=CARTESIAN_POINT('Ctrl Pts',(78.7283389164118,-7.92364075401344,136.498724587753));
#81144=CARTESIAN_POINT('Ctrl Pts',(78.7352979317373,-7.91547253351798,136.498015726198));
#81145=CARTESIAN_POINT('Ctrl Pts',(78.7538775336075,-7.89408656833953,136.496152650241));
#81146=CARTESIAN_POINT('Ctrl Pts',(78.7656296767321,-7.88098451170213,136.495003916887));
#81147=CARTESIAN_POINT('Ctrl Pts',(78.826827592354,-7.81489461363774,136.48916643996));
#81148=CARTESIAN_POINT('Ctrl Pts',(78.8794882176982,-7.76498440405701,136.484618135389));
#81149=CARTESIAN_POINT('Ctrl Pts',(79.0133917116924,-7.65371407264057,136.473867730857));
#81150=CARTESIAN_POINT('Ctrl Pts',(79.0973195120229,-7.59605972736649,136.467764440725));
#81151=CARTESIAN_POINT('Ctrl Pts',(79.2322430241922,-7.52050092347646,136.458155543224));
#81152=CARTESIAN_POINT('Ctrl Pts',(79.2797187045284,-7.49681606523634,136.454805666835));
#81153=CARTESIAN_POINT('Ctrl Pts',(79.3384037686755,-7.47095786415576,136.450606239352));
#81154=CARTESIAN_POINT('Ctrl Pts',(79.3486145561412,-7.46658015740575,136.449873470062));
#81155=CARTESIAN_POINT('Ctrl Pts',(79.3647039354683,-7.45987179462465,136.448714381012));
#81156=CARTESIAN_POINT('Ctrl Pts',(79.3705535350147,-7.45747184044791,136.448292057849));
#81157=CARTESIAN_POINT('Ctrl Pts',(79.3810077314937,-7.45325209391485,136.447535425562));
#81158=CARTESIAN_POINT('Ctrl Pts',(79.3856069792557,-7.45141944765787,136.447201891594));
#81159=CARTESIAN_POINT('Ctrl Pts',(79.3967884356634,-7.44702166345237,136.446389466975));
#81160=CARTESIAN_POINT('Ctrl Pts',(79.40337881163,-7.4444778824587,136.44590933898));
#81161=CARTESIAN_POINT('Ctrl Pts',(79.4241169634453,-7.43662445944628,136.444394929788));
#81162=CARTESIAN_POINT('Ctrl Pts',(79.438320463404,-7.43146552131711,136.443352520157));
#81163=CARTESIAN_POINT('Ctrl Pts',(79.5139091748129,-7.40516878178558,136.437784746751));
#81164=CARTESIAN_POINT('Ctrl Pts',(79.5764154898566,-7.38744135302447,136.43311246509));
#81165=CARTESIAN_POINT('Ctrl Pts',(79.7494091035494,-7.34913175896596,136.420251526671));
#81166=CARTESIAN_POINT('Ctrl Pts',(79.8612162704327,-7.33599692494895,136.412036337478));
#81167=CARTESIAN_POINT('Ctrl Pts',(80.0204666113632,-7.33346365173211,136.400809199551));
#81168=CARTESIAN_POINT('Ctrl Pts',(80.0674458954969,-7.3347030051546,136.397551241812));
#81169=CARTESIAN_POINT('Ctrl Pts',(80.1302139726367,-7.33902007246642,136.393269367407));
#81170=CARTESIAN_POINT('Ctrl Pts',(80.1460976857024,-7.34034175348256,136.392191843095));
#81171=CARTESIAN_POINT('Ctrl Pts',(80.1722874966879,-7.34289991754057,136.390424566541));
#81172=CARTESIAN_POINT('Ctrl Pts',(80.18260506101,-7.34400511326013,136.389730754153));
#81173=CARTESIAN_POINT('Ctrl Pts',(80.2027834139771,-7.34635745715489,136.388378324355));
#81174=CARTESIAN_POINT('Ctrl Pts',(80.2126446782996,-7.34759659266697,136.387719485578));
#81175=CARTESIAN_POINT('Ctrl Pts',(80.2360836498065,-7.35075516367826,136.386158194084));
#81176=CARTESIAN_POINT('Ctrl Pts',(80.2496500483913,-7.35275414957019,136.385258278319));
#81177=CARTESIAN_POINT('Ctrl Pts',(80.2963330040623,-7.360222793522,136.382173115089));
#81178=CARTESIAN_POINT('Ctrl Pts',(80.329309275834,-7.36652573256676,136.380014029814));
#81179=CARTESIAN_POINT('Ctrl Pts',(80.4103578132057,-7.38457147628857,136.374737537394));
#81180=CARTESIAN_POINT('Ctrl Pts',(80.4581406483268,-7.39746745960658,136.371653835184));
#81181=CARTESIAN_POINT('Ctrl Pts',(80.568175295527,-7.43248950156114,136.364530472941));
#81182=CARTESIAN_POINT('Ctrl Pts',(80.6298238840813,-7.45622723466822,136.360523291078));
#81183=CARTESIAN_POINT('Ctrl Pts',(80.7032606024939,-7.48963716094518,136.355584367573));
#81184=CARTESIAN_POINT('Ctrl Pts',(80.7165379694341,-7.49589072502501,136.354684415188));
#81185=CARTESIAN_POINT('Ctrl Pts',(80.7934704966602,-7.53337536449922,136.349420029075));
#81186=CARTESIAN_POINT('Ctrl Pts',(80.8551548081927,-7.56846551973307,136.345000035879));
#81187=CARTESIAN_POINT('Ctrl Pts',(80.9240868512756,-7.61372674247104,136.339605882579));
#81188=CARTESIAN_POINT('Ctrl Pts',(80.9336983049727,-7.62018207355534,136.338842858322));
#81189=CARTESIAN_POINT('Ctrl Pts',(80.9485397459497,-7.63037608542951,136.337646268045));
#81190=CARTESIAN_POINT('Ctrl Pts',(80.9538169101488,-7.63404589555177,136.33721712914));
#81191=CARTESIAN_POINT('Ctrl Pts',(80.963515219306,-7.64087383148488,136.33642140169));
#81192=CARTESIAN_POINT('Ctrl Pts',(80.9679423140171,-7.64402315897177,136.336055399488));
#81193=CARTESIAN_POINT('Ctrl Pts',(80.9781970271658,-7.65139392072596,136.335201200318));
#81194=CARTESIAN_POINT('Ctrl Pts',(80.9840127534341,-7.65563149498363,136.334711929063));
#81195=CARTESIAN_POINT('Ctrl Pts',(81.0025319242982,-7.66930986042372,136.333138875958));
#81196=CARTESIAN_POINT('Ctrl Pts',(81.0151279223944,-7.67889373537157,136.332046079795));
#81197=CARTESIAN_POINT('Ctrl Pts',(81.0841686419274,-7.73299483639653,136.325936774487));
#81198=CARTESIAN_POINT('Ctrl Pts',(81.1378178635452,-7.78094618354147,136.320742777989));
#81199=CARTESIAN_POINT('Ctrl Pts',(81.2811833912345,-7.92681659573577,136.305872744793));
#81200=CARTESIAN_POINT('Ctrl Pts',(81.3625548330531,-8.03221379828502,136.29621437872));
#81201=CARTESIAN_POINT('Ctrl Pts',(81.4442389121655,-8.1690717533662,136.285205465082));
#81202=CARTESIAN_POINT('Ctrl Pts',(81.4573606332714,-8.19230704256972,136.283381865019));
#81203=CARTESIAN_POINT('Ctrl Pts',(81.4758297153299,-8.22692798822632,136.280729134223));
#81204=CARTESIAN_POINT('Ctrl Pts',(81.4816148248892,-8.23807401298346,136.279884667254));
#81205=CARTESIAN_POINT('Ctrl Pts',(81.4916739838878,-8.25800263259035,136.278391355258));
#81206=CARTESIAN_POINT('Ctrl Pts',(81.495997807099,-8.26675929219515,136.277740791827));
#81207=CARTESIAN_POINT('Ctrl Pts',(81.5049629191842,-8.28532500014035,136.276373006485));
#81208=CARTESIAN_POINT('Ctrl Pts',(81.509585888601,-8.29514242724521,136.275656442947));
#81209=CARTESIAN_POINT('Ctrl Pts',(81.5216891100965,-8.32151042812492,136.273749232637));
#81210=CARTESIAN_POINT('Ctrl Pts',(81.5289953339168,-8.33813962355231,136.272564555453));
#81211=CARTESIAN_POINT('Ctrl Pts',(81.5682698759759,-8.43165296703818,136.265997024199));
#81212=CARTESIAN_POINT('Ctrl Pts',(81.5947133211053,-8.51073444073599,136.260803963161));
#81213=CARTESIAN_POINT('Ctrl Pts',(81.6324170442734,-8.65979738498129,136.251354757236));
#81214=CARTESIAN_POINT('Ctrl Pts',(81.6453461156356,-8.72915093698868,136.24708481809));
#81215=CARTESIAN_POINT('Ctrl Pts',(81.662459100545,-8.87003789992456,136.238356449962));
#81216=CARTESIAN_POINT('Ctrl Pts',(81.6665016739439,-8.94143385250075,136.233904390947));
#81217=CARTESIAN_POINT('Ctrl Pts',(81.6658609637158,-9.02444267643055,136.228474470825));
#81218=CARTESIAN_POINT('Ctrl Pts',(81.6656507377964,-9.03602493747524,136.227711051804));
#81219=CARTESIAN_POINT('Ctrl Pts',(81.6651360511147,-9.05403023032443,136.226513972609));
#81220=CARTESIAN_POINT('Ctrl Pts',(81.6649151504188,-9.06045554523203,136.226084745294));
#81221=CARTESIAN_POINT('Ctrl Pts',(81.6644389692623,-9.07230791960864,136.225288943578));
#81222=CARTESIAN_POINT('Ctrl Pts',(81.6641943252666,-9.07773520620492,136.224922956507));
#81223=CARTESIAN_POINT('Ctrl Pts',(81.6635640467441,-9.09034608125817,136.224068911169));
#81224=CARTESIAN_POINT('Ctrl Pts',(81.6631584265527,-9.09752843379783,136.223579779953));
#81225=CARTESIAN_POINT('Ctrl Pts',(81.6617122631881,-9.12049277594965,136.222007636225));
#81226=CARTESIAN_POINT('Ctrl Pts',(81.6604935238163,-9.13626212460825,136.220915623487));
#81227=CARTESIAN_POINT('Ctrl Pts',(81.6525016212957,-9.22348588014215,136.214815048416));
#81228=CARTESIAN_POINT('Ctrl Pts',(81.6413412605934,-9.29445608866452,136.20962951134));
#81229=CARTESIAN_POINT('Ctrl Pts',(81.5966984547348,-9.49357164199205,136.194793927766));
#81230=CARTESIAN_POINT('Ctrl Pts',(81.5524746229044,-9.61878398600857,136.185160501482));
#81231=CARTESIAN_POINT('Ctrl Pts',(81.4819404287675,-9.76166763579994,136.174149988258));
#81232=CARTESIAN_POINT('Ctrl Pts',(81.4694013042364,-9.78558575376171,136.172303953241));
#81233=CARTESIAN_POINT('Ctrl Pts',(81.4502237978625,-9.82009920015295,136.169634337258));
#81234=CARTESIAN_POINT('Ctrl Pts',(81.4440393996247,-9.83094042447244,136.168794889648));
#81235=CARTESIAN_POINT('Ctrl Pts',(81.4327914956574,-9.85015305454894,136.167305319371));
#81236=CARTESIAN_POINT('Ctrl Pts',(81.4277750405684,-9.85855117886512,136.166653541075));
#81237=CARTESIAN_POINT('Ctrl Pts',(81.4170751623764,-9.8761108398764,136.165289088098));
#81238=CARTESIAN_POINT('Ctrl Pts',(81.4113761758909,-9.88526240116317,136.164577019924));
#81239=CARTESIAN_POINT('Ctrl Pts',(81.3960152590079,-9.90940388130542,136.162695567703));
#81240=CARTESIAN_POINT('Ctrl Pts',(81.3862006265654,-9.92429534542364,136.161531866083));
#81241=CARTESIAN_POINT('Ctrl Pts',(81.3329812732045,-10.0022885708619,136.155414844941));
#81242=CARTESIAN_POINT('Ctrl Pts',(81.2855004283773,-10.0625028316024,136.150619806194));
#81243=CARTESIAN_POINT('Ctrl Pts',(81.1622164359776,-10.1984316536936,136.139310742078));
#81244=CARTESIAN_POINT('Ctrl Pts',(81.0829428853939,-10.2705186946937,136.132900500656));
#81245=CARTESIAN_POINT('Ctrl Pts',(80.9619576739437,-10.3609341645832,136.12344881136));
#81246=CARTESIAN_POINT('Ctrl Pts',(80.9255672361524,-10.3859397219893,136.12064048653));
#81247=CARTESIAN_POINT('Ctrl Pts',(80.8791713301346,-10.4151778832335,136.117044832342));
#81248=CARTESIAN_POINT('Ctrl Pts',(80.8700573069079,-10.4207994006373,136.116337790711));
#81249=CARTESIAN_POINT('Ctrl Pts',(80.8556068528442,-10.4295212462321,136.115214598171));
#81250=CARTESIAN_POINT('Ctrl Pts',(80.8503061137683,-10.4326805609976,136.114802133344));
#81251=CARTESIAN_POINT('Ctrl Pts',(80.8402100744248,-10.4386221764665,136.114015432708));
#81252=CARTESIAN_POINT('Ctrl Pts',(80.8354182834395,-10.441410081732,136.113641559589));
#81253=CARTESIAN_POINT('Ctrl Pts',(80.8239499223941,-10.4480060787172,136.112745703874));
#81254=CARTESIAN_POINT('Ctrl Pts',(80.8172608006503,-10.451791946709,136.112222348559));
#81255=CARTESIAN_POINT('Ctrl Pts',(80.7942092016864,-10.4646287567196,136.110416574757));
#81256=CARTESIAN_POINT('Ctrl Pts',(80.7777213447462,-10.473450062993,136.109121171448));
#81257=CARTESIAN_POINT('Ctrl Pts',(80.7364346084739,-10.4946532188458,136.105874305914));
#81258=CARTESIAN_POINT('Ctrl Pts',(80.7114690359023,-10.5066969882113,136.103908300771));
#81259=CARTESIAN_POINT('Ctrl Pts',(80.6072361076533,-10.5538123090927,136.095720779249));
#81260=CARTESIAN_POINT('Ctrl Pts',(80.5255923794135,-10.5832942288402,136.089364194733));
#81261=CARTESIAN_POINT('Ctrl Pts',(80.3467292457091,-10.6325146990658,136.075919808714));
#81262=CARTESIAN_POINT('Ctrl Pts',(80.2492730306803,-10.6502104482126,136.068886331677));
#81263=CARTESIAN_POINT('Ctrl Pts',(80.1320163222917,-10.6608683617966,136.060835965956));
#81264=CARTESIAN_POINT('Ctrl Pts',(80.1131968745165,-10.6622570628442,136.059555732243));
#81265=CARTESIAN_POINT('Ctrl Pts',(80.0833727029531,-10.663948929493,136.057544804656));
#81266=CARTESIAN_POINT('Ctrl Pts',(80.0723820770744,-10.6644632445714,136.056807589525));
#81267=CARTESIAN_POINT('Ctrl Pts',(80.0526286996157,-10.6651915898383,136.055489235069));
#81268=CARTESIAN_POINT('Ctrl Pts',(80.0438679172225,-10.6654454124197,136.054906876735));
#81269=CARTESIAN_POINT('Ctrl Pts',(80.0232836338115,-10.6658792538787,136.053543866153));
#81270=CARTESIAN_POINT('Ctrl Pts',(80.0114593086445,-10.6660025547435,136.052765009314));
#81271=CARTESIAN_POINT('Ctrl Pts',(79.9767941044868,-10.6659949478093,136.050492927875));
#81272=CARTESIAN_POINT('Ctrl Pts',(79.9539554752603,-10.6655202380111,136.049010396839));
#81273=CARTESIAN_POINT('Ctrl Pts',(79.848446760731,-10.6611551149451,136.042217403857));
#81274=CARTESIAN_POINT('Ctrl Pts',(79.7661255982622,-10.6515779678433,136.037083643217));
#81275=CARTESIAN_POINT('Ctrl Pts',(79.6286323979852,-10.625090677726,136.028499419117));
#81276=CARTESIAN_POINT('Ctrl Pts',(79.5730117706789,-10.6113704050205,136.025021688911));
#81277=CARTESIAN_POINT('Ctrl Pts',(79.4444914013148,-10.5725445346539,136.016782191104));
#81278=CARTESIAN_POINT('Ctrl Pts',(79.3724166335505,-10.5451932275107,136.012002132342));
#81279=CARTESIAN_POINT('Ctrl Pts',(79.2919807624931,-10.5081110617897,136.006208481804));
#81280=CARTESIAN_POINT('Ctrl Pts',(79.2815110756145,-10.5031513105747,136.005445005633));
#81281=CARTESIAN_POINT('Ctrl Pts',(79.2653129595804,-10.4952699721735,136.004247855657));
#81282=CARTESIAN_POINT('Ctrl Pts',(79.2595480455056,-10.4924236116674,136.003818615544));
#81283=CARTESIAN_POINT('Ctrl Pts',(79.2489423270313,-10.4871105840532,136.003022803071));
#81284=CARTESIAN_POINT('Ctrl Pts',(79.2440969360405,-10.4846535192165,136.002656818186));
#81285=CARTESIAN_POINT('Ctrl Pts',(79.2328638313419,-10.4788880439583,136.00180279509));
#81286=CARTESIAN_POINT('Ctrl Pts',(79.2264854694499,-10.4755619316208,136.001313684126));
#81287=CARTESIAN_POINT('Ctrl Pts',(79.2061540431883,-10.4647916918972,135.999741671881));
#81288=CARTESIAN_POINT('Ctrl Pts',(79.192285832796,-10.4571904070715,135.998649772408));
#81289=CARTESIAN_POINT('Ctrl Pts',(79.1161002628295,-10.4140107729154,135.99255045869));
#81290=CARTESIAN_POINT('Ctrl Pts',(79.0560290753016,-10.3746352535461,135.987366143711));
#81291=CARTESIAN_POINT('Ctrl Pts',(78.8929935452841,-10.2520311570916,135.972535528709));
#81292=CARTESIAN_POINT('Ctrl Pts',(78.7971169914575,-10.1602283871828,135.962905698296));
#81293=CARTESIAN_POINT('Ctrl Pts',(78.6959238483847,-10.03714652932,135.951894942957));
#81294=CARTESIAN_POINT('Ctrl Pts',(78.6792575030176,-10.0158380468731,135.950045661469));
#81295=CARTESIAN_POINT('Ctrl Pts',(78.6556642597566,-9.98411045439296,135.947372291279));
#81296=CARTESIAN_POINT('Ctrl Pts',(78.6483247491142,-9.97400513336739,135.946532272485));
#81297=CARTESIAN_POINT('Ctrl Pts',(78.6354396923509,-9.95583830969484,135.94504205554));
#81298=CARTESIAN_POINT('Ctrl Pts',(78.6298502933984,-9.94780878662706,135.944390196573));
#81299=CARTESIAN_POINT('Ctrl Pts',(78.6182533960129,-9.93083212674594,135.943025943599));
#81300=CARTESIAN_POINT('Ctrl Pts',(78.6122613093948,-9.92187497070461,135.942314152859));
#81301=CARTESIAN_POINT('Ctrl Pts',(78.5965961061624,-9.89795924788947,135.940434290283));
#81302=CARTESIAN_POINT('Ctrl Pts',(78.5870750962848,-9.88290234815893,135.93927188334));
#81303=CARTESIAN_POINT('Ctrl Pts',(78.5381038896986,-9.80263568816844,135.933180222101));
#81304=CARTESIAN_POINT('Ctrl Pts',(78.5029188790437,-9.73492485512945,135.928407576921));
#81305=CARTESIAN_POINT('Ctrl Pts',(78.4372856302942,-9.58417285838609,135.918273188005));
#81306=CARTESIAN_POINT('Ctrl Pts',(78.4085578727547,-9.5006450862159,135.91295397125));
#81307=CARTESIAN_POINT('Ctrl Pts',(78.3742897703535,-9.36749504146005,135.904457892236));
#81308=CARTESIAN_POINT('Ctrl Pts',(78.364128658753,-9.31923422752997,135.901373165135));
#81309=CARTESIAN_POINT('Ctrl Pts',(78.3529714837076,-9.25145472319147,135.896946575299));
#81310=CARTESIAN_POINT('Ctrl Pts',(78.3501550529687,-9.2322584406095,135.895682438179));
#81311=CARTESIAN_POINT('Ctrl Pts',(78.346649792503,-9.20506909276868,135.893871617067));
#81312=CARTESIAN_POINT('Ctrl Pts',(78.3456823723338,-9.19711271333548,135.893339270303));
#81313=CARTESIAN_POINT('Ctrl Pts',(78.3441430502629,-9.18364229216901,135.892433377276));
#81314=CARTESIAN_POINT('Ctrl Pts',(78.3435411767897,-9.17813168034955,135.89206147936));
#81315=CARTESIAN_POINT('Ctrl Pts',(78.3424380834556,-9.16754263219605,135.891344184262));
#81316=CARTESIAN_POINT('Ctrl Pts',(78.3419326795074,-9.16246476455477,135.890999052264));
#81317=CARTESIAN_POINT('Ctrl Pts',(78.3408841507623,-9.1514151756644,135.890245628202));
#81318=CARTESIAN_POINT('Ctrl Pts',(78.3403499245922,-9.14544270719875,135.889836863965));
#81319=CARTESIAN_POINT('Ctrl Pts',(78.3391176742243,-9.13077461965185,135.888829423074));
#81320=CARTESIAN_POINT('Ctrl Pts',(78.3384556941492,-9.12207625933092,135.888228950659));
#81321=CARTESIAN_POINT('Ctrl Pts',(78.3353083429498,-9.07593373282946,135.885028836512));
#81322=CARTESIAN_POINT('Ctrl Pts',(78.3340205656728,-9.03842192104802,135.882375972897));
#81323=CARTESIAN_POINT('Ctrl Pts',(78.3340002443612,-9.00090233676016,135.879690672883));
#81324=CARTESIAN_POINT('Ctrl Pts',(78.3340002456957,-9.00090479726252,135.879690848982));
#81325=CARTESIAN_POINT('Ctrl Pts',(78.3339486782985,-8.90595394516173,135.872895160915));
#81326=CARTESIAN_POINT('Ctrl Pts',(78.3420143785496,-8.81117037196368,135.86591863175));
#81327=CARTESIAN_POINT('Ctrl Pts',(78.3722930491939,-8.63513663529914,135.853006356088));
#81328=CARTESIAN_POINT('Ctrl Pts',(78.392666927927,-8.55386180232306,135.847062253801));
#81329=CARTESIAN_POINT('Ctrl Pts',(78.424631626278,-8.45770686105293,135.840094980782));
#81330=CARTESIAN_POINT('Ctrl Pts',(78.430463714507,-8.44105167753812,135.838890212765));
#81331=CARTESIAN_POINT('Ctrl Pts',(78.4365593748807,-8.42449204025778,135.837694108205));
#81332=CARTESIAN_POINT('',(78.3340003883624,-9.00113755153436,136.072462071471));
#81333=CARTESIAN_POINT('Ctrl Pts',(78.4365593762033,-8.4244920366647,136.032852185112));
#81334=CARTESIAN_POINT('Ctrl Pts',(78.4356277258545,-8.42702298340278,136.033046303352));
#81335=CARTESIAN_POINT('Ctrl Pts',(78.4347021631167,-8.42955635039758,136.033240322336));
#81336=CARTESIAN_POINT('Ctrl Pts',(78.4095803139013,-8.49883919715719,136.038538530477));
#81337=CARTESIAN_POINT('Ctrl Pts',(78.3896669126106,-8.56707202833529,136.04355275021));
#81338=CARTESIAN_POINT('Ctrl Pts',(78.3698143433768,-8.65583668041469,136.049800259074));
#81339=CARTESIAN_POINT('Ctrl Pts',(78.3658114692678,-8.67537472157639,136.051159057064));
#81340=CARTESIAN_POINT('Ctrl Pts',(78.3598903740665,-8.70716879080624,136.053344599856));
#81341=CARTESIAN_POINT('Ctrl Pts',(78.3577566165095,-8.71938213535617,136.054178076104));
#81342=CARTESIAN_POINT('Ctrl Pts',(78.3541893826516,-8.74123680834678,136.055659011553));
#81343=CARTESIAN_POINT('Ctrl Pts',(78.3527038238034,-8.75086892536187,136.056308088779));
#81344=CARTESIAN_POINT('Ctrl Pts',(78.3499924381886,-8.76953493586363,136.057559151771));
#81345=CARTESIAN_POINT('Ctrl Pts',(78.3487560759312,-8.77856692066546,136.058161447505));
#81346=CARTESIAN_POINT('Ctrl Pts',(78.3462230670659,-8.79827375592153,136.059469171345));
#81347=CARTESIAN_POINT('Ctrl Pts',(78.3449555037265,-8.80895198059508,136.060173671105));
#81348=CARTESIAN_POINT('Ctrl Pts',(78.3412526903109,-8.84295451651808,136.062404654891));
#81349=CARTESIAN_POINT('Ctrl Pts',(78.3392063991886,-8.86631895095113,136.063919165488));
#81350=CARTESIAN_POINT('Ctrl Pts',(78.3351936440725,-8.9268065492008,136.067799253375));
#81351=CARTESIAN_POINT('Ctrl Pts',(78.3339750077928,-8.96396647141597,136.070143170673));
#81352=CARTESIAN_POINT('Ctrl Pts',(78.3340003883624,-9.00113755153436,136.072462071471));
#81353=CARTESIAN_POINT('Ctrl Pts',(78.3340003869976,-9.0011355508379,136.072461946658));
#81354=CARTESIAN_POINT('Ctrl Pts',(78.3340531440873,-9.07853700943008,136.077290603074));
#81355=CARTESIAN_POINT('Ctrl Pts',(78.3394999153977,-9.15584584925452,136.081997884715));
#81356=CARTESIAN_POINT('Ctrl Pts',(78.3596031981819,-9.29848853188085,136.090799645083));
#81357=CARTESIAN_POINT('Ctrl Pts',(78.3728537737941,-9.36385567026177,136.094881813052));
#81358=CARTESIAN_POINT('Ctrl Pts',(78.3957719282622,-9.45001745767704,136.100524030258));
#81359=CARTESIAN_POINT('Ctrl Pts',(78.4020028926957,-9.47166573117722,136.101964505079));
#81360=CARTESIAN_POINT('Ctrl Pts',(78.4134188250564,-9.50850119330994,136.104465350293));
#81361=CARTESIAN_POINT('Ctrl Pts',(78.4183879578705,-9.5237524129145,136.105515643136));
#81362=CARTESIAN_POINT('Ctrl Pts',(78.4259160910296,-9.54577299776072,136.107057007256));
#81363=CARTESIAN_POINT('Ctrl Pts',(78.428300391788,-9.55260171396246,136.107538499868));
#81364=CARTESIAN_POINT('Ctrl Pts',(78.432554208905,-9.56453453188385,136.1083863974));
#81365=CARTESIAN_POINT('Ctrl Pts',(78.4344043523939,-9.56964533940766,136.108751668212));
#81366=CARTESIAN_POINT('Ctrl Pts',(78.438487380011,-9.58075407502649,136.109550328748));
#81367=CARTESIAN_POINT('Ctrl Pts',(78.4407297879627,-9.58674812351805,136.109984246605));
#81368=CARTESIAN_POINT('Ctrl Pts',(78.4470829183529,-9.6034366646677,136.111200383974));
#81369=CARTESIAN_POINT('Ctrl Pts',(78.4512694188528,-9.6141016525141,136.111986812549));
#81370=CARTESIAN_POINT('Ctrl Pts',(78.4799752262506,-9.68506797711475,136.1172778576));
#81371=CARTESIAN_POINT('Ctrl Pts',(78.5078983054853,-9.74392478991529,136.121945627329));
#81372=CARTESIAN_POINT('Ctrl Pts',(78.5496654074353,-9.82009781652399,136.128241581835));
#81373=CARTESIAN_POINT('Ctrl Pts',(78.5605161227628,-9.8389976198774,136.129826012431));
#81374=CARTESIAN_POINT('Ctrl Pts',(78.6072653212665,-9.91684758692653,136.136434504642));
#81375=CARTESIAN_POINT('Ctrl Pts',(78.6464406462863,-9.97375428776186,136.141461415257));
#81376=CARTESIAN_POINT('Ctrl Pts',(78.7180408791542,-10.0650569381424,136.149769373454));
#81377=CARTESIAN_POINT('Ctrl Pts',(78.7486014556983,-10.1008032590583,136.153093164816));
#81378=CARTESIAN_POINT('Ctrl Pts',(78.7957311118314,-10.1514266110471,136.157900603742));
#81379=CARTESIAN_POINT('Ctrl Pts',(78.8111492838832,-10.1673392182684,136.159427638254));
#81380=CARTESIAN_POINT('Ctrl Pts',(78.8396995725587,-10.1956524734418,136.162174645403));
#81381=CARTESIAN_POINT('Ctrl Pts',(78.8527244363873,-10.2081559273629,136.163398944764));
#81382=CARTESIAN_POINT('Ctrl Pts',(78.8736862406611,-10.2276338332598,136.165324893413));
#81383=CARTESIAN_POINT('Ctrl Pts',(78.8814903778884,-10.2347484550194,136.166032495897));
#81384=CARTESIAN_POINT('Ctrl Pts',(78.8966095381082,-10.248270819334,136.1673856338));
#81385=CARTESIAN_POINT('Ctrl Pts',(78.9039140238905,-10.2546896387645,136.168031618388));
#81386=CARTESIAN_POINT('Ctrl Pts',(78.9204810112987,-10.2689927869896,136.169479700536));
#81387=CARTESIAN_POINT('Ctrl Pts',(78.9297745660913,-10.2768404262507,136.170280267417));
#81388=CARTESIAN_POINT('Ctrl Pts',(78.9574861288122,-10.299725403546,136.172633801087));
#81389=CARTESIAN_POINT('Ctrl Pts',(78.9761415028634,-10.3144714396632,136.17417509808));
#81390=CARTESIAN_POINT('Ctrl Pts',(79.0768073905316,-10.3905983285773,136.182281225029));
#81391=CARTESIAN_POINT('Ctrl Pts',(79.1640349305834,-10.4447193506548,136.188562730292));
#81392=CARTESIAN_POINT('Ctrl Pts',(79.3266304206723,-10.5259151006111,136.199662489825));
#81393=CARTESIAN_POINT('Ctrl Pts',(79.4000042932717,-10.5562284169969,136.204481949268));
#81394=CARTESIAN_POINT('Ctrl Pts',(79.4987629040837,-10.5890031609177,136.211042952097));
#81395=CARTESIAN_POINT('Ctrl Pts',(79.5224442681842,-10.5962800709341,136.212621964881));
#81396=CARTESIAN_POINT('Ctrl Pts',(79.5628443217163,-10.6077149470157,136.215339150513));
#81397=CARTESIAN_POINT('Ctrl Pts',(79.5794817893799,-10.6121466483397,136.216464773764));
#81398=CARTESIAN_POINT('Ctrl Pts',(79.6034015617999,-10.6181226843057,136.218096513039));
#81399=CARTESIAN_POINT('Ctrl Pts',(79.6106308111568,-10.6198774559174,136.218591415872));
#81400=CARTESIAN_POINT('Ctrl Pts',(79.6232324725035,-10.6228470560656,136.219457524723));
#81401=CARTESIAN_POINT('Ctrl Pts',(79.6285995437493,-10.6240837531513,136.219827487251));
#81402=CARTESIAN_POINT('Ctrl Pts',(79.6401135767127,-10.6266767915208,136.22062361679));
#81403=CARTESIAN_POINT('Ctrl Pts',(79.646262020066,-10.628024895388,136.221050204735));
#81404=CARTESIAN_POINT('Ctrl Pts',(79.663165096473,-10.6316307817585,136.222226688523));
#81405=CARTESIAN_POINT('Ctrl Pts',(79.6739344330024,-10.6338170001975,136.222980381118));
#81406=CARTESIAN_POINT('Ctrl Pts',(79.7352872076183,-10.6456411241806,136.227294601405));
#81407=CARTESIAN_POINT('Ctrl Pts',(79.7862698313537,-10.6530353594936,136.230957677139));
#81408=CARTESIAN_POINT('Ctrl Pts',(79.9330579404276,-10.6674208787999,136.241586092992));
#81409=CARTESIAN_POINT('Ctrl Pts',(80.0292401159734,-10.6685082277759,136.248637952651));
#81410=CARTESIAN_POINT('Ctrl Pts',(80.177433543744,-10.657359317835,136.259325425901));
#81411=CARTESIAN_POINT('Ctrl Pts',(80.2296710641545,-10.6509314532033,136.26306103374));
#81412=CARTESIAN_POINT('Ctrl Pts',(80.3050175434361,-10.6380136151343,136.268388817616));
#81413=CARTESIAN_POINT('Ctrl Pts',(80.328425668977,-10.6334812469752,136.270035658001));
#81414=CARTESIAN_POINT('Ctrl Pts',(80.3706976159592,-10.6243509015645,136.272994937952));
#81415=CARTESIAN_POINT('Ctrl Pts',(80.3895933533836,-10.6199227290637,136.274312371937));
#81416=CARTESIAN_POINT('Ctrl Pts',(80.4191834297355,-10.6124406293078,136.276367763611));
#81417=CARTESIAN_POINT('Ctrl Pts',(80.4299314199239,-10.6096081869,136.277112743289));
#81418=CARTESIAN_POINT('Ctrl Pts',(80.4500246977973,-10.6040973340813,136.27850274619));
#81419=CARTESIAN_POINT('Ctrl Pts',(80.4593763907743,-10.6014442932179,136.279148556542));
#81420=CARTESIAN_POINT('Ctrl Pts',(80.4803368661032,-10.5952991686223,136.280593802909));
#81421=CARTESIAN_POINT('Ctrl Pts',(80.4919319126449,-10.5917619007353,136.281391734493));
#81422=CARTESIAN_POINT('Ctrl Pts',(80.5259613500972,-10.580973274519,136.283729736273));
#81423=CARTESIAN_POINT('Ctrl Pts',(80.5482821903339,-10.573371718859,136.285258371482));
#81424=CARTESIAN_POINT('Ctrl Pts',(80.6684995754837,-10.5295614105909,136.293478446592));
#81425=CARTESIAN_POINT('Ctrl Pts',(80.7629927560757,-10.4846869174966,136.299873544174));
#81426=CARTESIAN_POINT('Ctrl Pts',(80.919717190734,-10.3913182249627,136.311014259237));
#81427=CARTESIAN_POINT('Ctrl Pts',(80.9838666726462,-10.3467185230584,136.315760881859));
#81428=CARTESIAN_POINT('Ctrl Pts',(81.0637854840536,-10.2823883520391,136.322231817124));
#81429=CARTESIAN_POINT('Ctrl Pts',(81.0825773122126,-10.266564517711,136.323798067999));
#81430=CARTESIAN_POINT('Ctrl Pts',(81.113852828467,-10.2390240696416,136.326495418802));
#81431=CARTESIAN_POINT('Ctrl Pts',(81.126518660641,-10.2275196210859,136.327614208366));
#81432=CARTESIAN_POINT('Ctrl Pts',(81.1444201587758,-10.2107491774557,136.329237769508));
#81433=CARTESIAN_POINT('Ctrl Pts',(81.1498017746462,-10.2056396411621,136.329731481296));
#81434=CARTESIAN_POINT('Ctrl Pts',(81.1591162105398,-10.1966770333956,136.330596247874));
#81435=CARTESIAN_POINT('Ctrl Pts',(81.1630643522751,-10.1928401499102,136.330966071275));
#81436=CARTESIAN_POINT('Ctrl Pts',(81.1714931933473,-10.1845671995464,136.331762775723));
#81437=CARTESIAN_POINT('Ctrl Pts',(81.1759676771506,-10.1801253201649,136.332190085424));
#81438=CARTESIAN_POINT('Ctrl Pts',(81.1882038535997,-10.1678396175123,136.333370455408));
#81439=CARTESIAN_POINT('Ctrl Pts',(81.1959128292911,-10.1599440755418,136.334127352037));
#81440=CARTESIAN_POINT('Ctrl Pts',(81.2397086768444,-10.1141876432716,136.338501141757));
#81441=CARTESIAN_POINT('Ctrl Pts',(81.2740717816077,-10.0747239988735,136.342223789743));
#81442=CARTESIAN_POINT('Ctrl Pts',(81.3697297132629,-9.95382130089555,136.353338096539));
#81443=CARTESIAN_POINT('Ctrl Pts',(81.425483861494,-9.86829261827158,136.36082600959));
#81444=CARTESIAN_POINT('Ctrl Pts',(81.5071765192192,-9.71365588212225,136.373363998937));
#81445=CARTESIAN_POINT('Ctrl Pts',(81.5370020297739,-9.64692595342673,136.378494616416));
#81446=CARTESIAN_POINT('Ctrl Pts',(81.568476699323,-9.56191421255803,136.384681130756));
#81447=CARTESIAN_POINT('Ctrl Pts',(81.5743346100442,-9.5452864528588,136.385875477882));
#81448=CARTESIAN_POINT('Ctrl Pts',(81.5833334383259,-9.5183883231667,136.387783100725));
#81449=CARTESIAN_POINT('Ctrl Pts',(81.5866407641407,-9.50817548682752,136.388501802862));
#81450=CARTESIAN_POINT('Ctrl Pts',(81.5927753609326,-9.48858827446242,136.389869798529));
#81451=CARTESIAN_POINT('Ctrl Pts',(81.5956191430648,-9.47921958390969,136.390519607981));
#81452=CARTESIAN_POINT('Ctrl Pts',(81.601922400416,-9.45777547969089,136.39199697821));
#81453=CARTESIAN_POINT('Ctrl Pts',(81.6053282585027,-9.445684825389,136.392822769564));
#81454=CARTESIAN_POINT('Ctrl Pts',(81.614055890675,-9.4133032484279,136.39501615713));
#81455=CARTESIAN_POINT('Ctrl Pts',(81.6191318435975,-9.39294799830358,136.396375884072));
#81456=CARTESIAN_POINT('Ctrl Pts',(81.6509430449827,-9.25427546454901,136.405522926466));
#81457=CARTESIAN_POINT('Ctrl Pts',(81.6650725882106,-9.13343941731572,136.412888365569));
#81458=CARTESIAN_POINT('Ctrl Pts',(81.6664358878596,-8.94619840577459,136.424330670322));
#81459=CARTESIAN_POINT('Ctrl Pts',(81.6630015445271,-8.88030126193085,136.428371377915));
#81460=CARTESIAN_POINT('Ctrl Pts',(81.6531835309658,-8.79253553429311,136.433961442991));
#81461=CARTESIAN_POINT('Ctrl Pts',(81.6502462549271,-8.77033831438495,136.435393485661));
#81462=CARTESIAN_POINT('Ctrl Pts',(81.6444495029706,-8.73242423840711,136.437881089014));
#81463=CARTESIAN_POINT('Ctrl Pts',(81.6418095872274,-8.71667652858781,136.438926713713));
#81464=CARTESIAN_POINT('Ctrl Pts',(81.6376479532972,-8.69386717035036,136.44046246085));
#81465=CARTESIAN_POINT('Ctrl Pts',(81.6363059090365,-8.68677309252152,136.440943101831));
#81466=CARTESIAN_POINT('Ctrl Pts',(81.6338730173725,-8.67435526389663,136.441790060367));
#81467=CARTESIAN_POINT('Ctrl Pts',(81.6328021694493,-8.66902778776265,136.442155252426));
#81468=CARTESIAN_POINT('Ctrl Pts',(81.6304116565038,-8.65742898765019,136.442954426446));
#81469=CARTESIAN_POINT('Ctrl Pts',(81.6290818871377,-8.65116010877972,136.443388942784));
#81470=CARTESIAN_POINT('Ctrl Pts',(81.6252657202622,-8.63366751014333,136.44460833716));
#81471=CARTESIAN_POINT('Ctrl Pts',(81.6226993256684,-8.62246187642905,136.445397458953));
#81472=CARTESIAN_POINT('Ctrl Pts',(81.6044747703193,-8.54650899196724,136.450796521397));
#81473=CARTESIAN_POINT('Ctrl Pts',(81.5850629263057,-8.48273129030787,136.455577184603));
#81474=CARTESIAN_POINT('Ctrl Pts',(81.5543622918707,-8.40001519832784,136.461974559569));
#81475=CARTESIAN_POINT('Ctrl Pts',(81.5464413774292,-8.3798847325863,136.463547740871));
#81476=CARTESIAN_POINT('Ctrl Pts',(81.5104515909371,-8.29340098473167,136.470365403037));
#81477=CARTESIAN_POINT('Ctrl Pts',(81.4784854695449,-8.22874901729802,136.4756100113));
#81478=CARTESIAN_POINT('Ctrl Pts',(81.4089998191959,-8.10851825372225,136.485530350487));
#81479=CARTESIAN_POINT('Ctrl Pts',(81.3721140638212,-8.05272746631147,136.490211356849));
#81480=CARTESIAN_POINT('Ctrl Pts',(81.3216220970021,-7.98552086249892,136.4959444828));
#81481=CARTESIAN_POINT('Ctrl Pts',(81.3110590167478,-7.97190604464337,136.49711135142));
#81482=CARTESIAN_POINT('Ctrl Pts',(81.2936285718628,-7.95014547389772,136.498985922746));
#81483=CARTESIAN_POINT('Ctrl Pts',(81.2868912070567,-7.94189771844929,136.499698717918));
#81484=CARTESIAN_POINT('Ctrl Pts',(81.2737927021483,-7.92617296457323,136.501062389236));
#81485=CARTESIAN_POINT('Ctrl Pts',(81.2674436772684,-7.91868650149739,136.50171371616));
#81486=CARTESIAN_POINT('Ctrl Pts',(81.2527041082732,-7.90161451047526,136.503204122685));
#81487=CARTESIAN_POINT('Ctrl Pts',(81.2442689806765,-7.89206814957792,136.50404132054));
#81488=CARTESIAN_POINT('Ctrl Pts',(81.2166213009232,-7.86149224353199,136.506736223956));
#81489=CARTESIAN_POINT('Ctrl Pts',(81.1969781106936,-7.84085770590956,136.508575816671));
#81490=CARTESIAN_POINT('Ctrl Pts',(81.0842987360328,-7.7284123852319,136.518746710605));
#81491=CARTESIAN_POINT('Ctrl Pts',(80.981242331743,-7.64729726130296,136.526604738046));
#81492=CARTESIAN_POINT('Ctrl Pts',(80.808979475236,-7.54185516316771,136.538997038029));
#81493=CARTESIAN_POINT('Ctrl Pts',(80.7458826769845,-7.50859433325969,136.543414966816));
#81494=CARTESIAN_POINT('Ctrl Pts',(80.6664719662814,-7.47303581949627,136.549060246491));
#81495=CARTESIAN_POINT('Ctrl Pts',(80.6519948202777,-7.46679838230708,136.550092813866));
#81496=CARTESIAN_POINT('Ctrl Pts',(80.6307954069113,-7.45801921134401,136.551612839209));
#81497=CARTESIAN_POINT('Ctrl Pts',(80.6241412562447,-7.45531385534933,136.552091085096));
#81498=CARTESIAN_POINT('Ctrl Pts',(80.6124261365001,-7.4506389320905,136.552935412953));
#81499=CARTESIAN_POINT('Ctrl Pts',(80.6073727209619,-7.44865095224276,136.553300393657));
#81500=CARTESIAN_POINT('Ctrl Pts',(80.596311550661,-7.44436189304197,136.554101057231));
#81501=CARTESIAN_POINT('Ctrl Pts',(80.5903002525085,-7.44207092791004,136.554537292359));
#81502=CARTESIAN_POINT('Ctrl Pts',(80.5734064712943,-7.43574435151897,136.555766057923));
#81503=CARTESIAN_POINT('Ctrl Pts',(80.5624951118452,-7.43178765932048,136.556562932635));
#81504=CARTESIAN_POINT('Ctrl Pts',(80.4788920153318,-7.40245613263875,136.562688535492));
#81505=CARTESIAN_POINT('Ctrl Pts',(80.4045686724083,-7.382036628393,136.568244529526));
#81506=CARTESIAN_POINT('Ctrl Pts',(80.2729616517355,-7.35551571470066,136.578002964458));
#81507=CARTESIAN_POINT('Ctrl Pts',(80.2162661012459,-7.34710379394236,136.582182645411));
#81508=CARTESIAN_POINT('Ctrl Pts',(80.0769158166393,-7.33372233195937,136.5922985263));
#81509=CARTESIAN_POINT('Ctrl Pts',(79.9940981971669,-7.33195741347212,136.598172144181));
#81510=CARTESIAN_POINT('Ctrl Pts',(79.8886808228571,-7.33756643230204,136.605429645344));
#81511=CARTESIAN_POINT('Ctrl Pts',(79.8659069304871,-7.33924822305783,136.606985054866));
#81512=CARTESIAN_POINT('Ctrl Pts',(79.8314053839323,-7.34251045582481,136.609323612528));
#81513=CARTESIAN_POINT('Ctrl Pts',(79.8196488975306,-7.34374844122533,136.610117338724));
#81514=CARTESIAN_POINT('Ctrl Pts',(79.7992030170704,-7.34612172768013,136.611492535054));
#81515=CARTESIAN_POINT('Ctrl Pts',(79.7905076843217,-7.34720063446611,136.612075749085));
#81516=CARTESIAN_POINT('Ctrl Pts',(79.7709166399991,-7.34978855996296,136.61338625697));
#81517=CARTESIAN_POINT('Ctrl Pts',(79.7600264758242,-7.35133699619361,136.614112283122));
#81518=CARTESIAN_POINT('Ctrl Pts',(79.7305035798678,-7.35583348817845,136.616074387602));
#81519=CARTESIAN_POINT('Ctrl Pts',(79.7119039383535,-7.35899038840539,136.617303862332));
#81520=CARTESIAN_POINT('Ctrl Pts',(79.5960436052583,-7.38068593144789,136.624928347029));
#81521=CARTESIAN_POINT('Ctrl Pts',(79.5005386444308,-7.4075487987189,136.631046492309));
#81522=CARTESIAN_POINT('Ctrl Pts',(79.3412720498868,-7.46809734382974,136.641469246738));
#81523=CARTESIAN_POINT('Ctrl Pts',(79.2762702912745,-7.49771412304658,136.645796717367));
#81524=CARTESIAN_POINT('Ctrl Pts',(79.1806842162881,-7.54891332608269,136.652528739725));
#81525=CARTESIAN_POINT('Ctrl Pts',(79.1485939632716,-7.56750626756389,136.654857154041));
#81526=CARTESIAN_POINT('Ctrl Pts',(79.1038570540067,-7.59546106337106,136.658240131652));
#81527=CARTESIAN_POINT('Ctrl Pts',(79.0906797036811,-7.60395617395465,136.659254180049));
#81528=CARTESIAN_POINT('Ctrl Pts',(79.0674943722164,-7.61937070891527,136.661073578881));
#81529=CARTESIAN_POINT('Ctrl Pts',(79.0574384495355,-7.62621628790698,136.66187473324));
#81530=CARTESIAN_POINT('Ctrl Pts',(79.0421417763418,-7.63687651931365,136.663113513431));
#81531=CARTESIAN_POINT('Ctrl Pts',(79.0368465755623,-7.6406128301045,136.663546088036));
#81532=CARTESIAN_POINT('Ctrl Pts',(79.0271170197089,-7.64756342062821,136.664348132998));
#81533=CARTESIAN_POINT('Ctrl Pts',(79.0226765514367,-7.65076878616497,136.664717006978));
#81534=CARTESIAN_POINT('Ctrl Pts',(79.0125748345348,-7.6581367733994,136.665562611119));
#81535=CARTESIAN_POINT('Ctrl Pts',(79.0069240637365,-7.6623133563403,136.6660402723));
#81536=CARTESIAN_POINT('Ctrl Pts',(78.989037355094,-7.67570952944139,136.66756662675));
#81537=CARTESIAN_POINT('Ctrl Pts',(78.9769025005247,-7.68506190836095,136.66862375255));
#81538=CARTESIAN_POINT('Ctrl Pts',(78.8853942567783,-7.7576211424056,136.676751167105));
#81539=CARTESIAN_POINT('Ctrl Pts',(78.8118218810881,-7.82778818382988,136.684177266436));
#81540=CARTESIAN_POINT('Ctrl Pts',(78.6690211389724,-7.99132345046157,136.699968396462));
#81541=CARTESIAN_POINT('Ctrl Pts',(78.6022130327686,-8.08614326269147,136.708265359407));
#81542=CARTESIAN_POINT('Ctrl Pts',(78.5362713348221,-8.2041151402908,136.717514015289));
#81543=CARTESIAN_POINT('Ctrl Pts',(78.5270789898906,-8.22125866375,136.718834555279));
#81544=CARTESIAN_POINT('Ctrl Pts',(78.5131044634775,-8.24845398976563,136.720893666757));
#81545=CARTESIAN_POINT('Ctrl Pts',(78.5081194202886,-8.2583989695918,136.721639302626));
#81546=CARTESIAN_POINT('Ctrl Pts',(78.4989661055957,-8.27712538197755,136.72302990055));
#81547=CARTESIAN_POINT('Ctrl Pts',(78.4947743784798,-8.28589475516883,136.723675656225));
#81548=CARTESIAN_POINT('Ctrl Pts',(78.4855334629231,-8.30567030724916,136.725119970786));
#81549=CARTESIAN_POINT('Ctrl Pts',(78.4805270045569,-8.31669593649359,136.725917033893));
#81550=CARTESIAN_POINT('Ctrl Pts',(78.4661546731418,-8.34928711518128,136.728249928762));
#81551=CARTESIAN_POINT('Ctrl Pts',(78.4571243271641,-8.37099801904214,136.729774402218));
#81552=CARTESIAN_POINT('Ctrl Pts',(78.4444496060379,-8.40338792783224,136.7320090848));
#81553=CARTESIAN_POINT('Ctrl Pts',(78.440450520719,-8.41392124806094,136.732729718861));
#81554=CARTESIAN_POINT('Ctrl Pts',(78.4365593881204,-8.4244920042904,136.733447186333));
#81555=CARTESIAN_POINT('Origin',(80.,-9.,134.));
#81556=CARTESIAN_POINT('',(78.4365593939729,-8.42449198839149,137.430947540156));
#81557=CARTESIAN_POINT('',(78.4365593749625,-8.42449204003552,137.240217161908));
#81558=CARTESIAN_POINT('',(78.4365593749993,-8.42449203993574,134.));
#81559=CARTESIAN_POINT('Ctrl Pts',(78.4365593749625,-8.42449204003557,137.240217161908));
#81560=CARTESIAN_POINT('Ctrl Pts',(78.4426950514193,-8.40782369397956,137.239116598015));
#81561=CARTESIAN_POINT('Ctrl Pts',(78.4490997416212,-8.39124680179114,137.238009742291));
#81562=CARTESIAN_POINT('Ctrl Pts',(78.4662907046562,-8.34878773177696,137.235135251636));
#81563=CARTESIAN_POINT('Ctrl Pts',(78.4774630443045,-8.32307854127335,137.233356454132));
#81564=CARTESIAN_POINT('Ctrl Pts',(78.4972254658144,-8.28056959083472,137.230331063815));
#81565=CARTESIAN_POINT('Ctrl Pts',(78.5054622762946,-8.26361128913567,137.229101067464));
#81566=CARTESIAN_POINT('Ctrl Pts',(78.5174707414679,-8.23991944152322,137.227344819163));
#81567=CARTESIAN_POINT('Ctrl Pts',(78.5210044754583,-8.2330660456309,137.22683224986));
#81568=CARTESIAN_POINT('Ctrl Pts',(78.5271621613846,-8.22132453607942,137.225945842083));
#81569=CARTESIAN_POINT('Ctrl Pts',(78.5297631723509,-8.21642457495041,137.225573426403));
#81570=CARTESIAN_POINT('Ctrl Pts',(78.5353037595954,-8.20611155528073,137.224784156948));
#81571=CARTESIAN_POINT('Ctrl Pts',(78.5382488512281,-8.20070186082715,137.224366986071));
#81572=CARTESIAN_POINT('Ctrl Pts',(78.5463706967688,-8.18597825767548,137.223223174653));
#81573=CARTESIAN_POINT('Ctrl Pts',(78.5516068147169,-8.1766976774988,137.222492976522));
#81574=CARTESIAN_POINT('Ctrl Pts',(78.5785566029695,-8.12998427163418,137.218773010506));
#81575=CARTESIAN_POINT('Ctrl Pts',(78.6016321182466,-8.09336045565965,137.215710889432));
#81576=CARTESIAN_POINT('Ctrl Pts',(78.6990757537441,-7.95128837297588,137.203356731949));
#81577=CARTESIAN_POINT('Ctrl Pts',(78.7841597555164,-7.85372877195035,137.193826034099));
#81578=CARTESIAN_POINT('Ctrl Pts',(78.9225828363449,-7.72795764263543,137.180540971547));
#81579=CARTESIAN_POINT('Ctrl Pts',(78.9675177481265,-7.69122145478909,137.176496460323));
#81580=CARTESIAN_POINT('Ctrl Pts',(79.0276261909263,-7.64710712299797,137.17141694395));
#81581=CARTESIAN_POINT('Ctrl Pts',(79.0411155400122,-7.63751308705435,137.170296981442));
#81582=CARTESIAN_POINT('Ctrl Pts',(79.0622524086141,-7.62294932916238,137.168572142088));
#81583=CARTESIAN_POINT('Ctrl Pts',(79.0698012045732,-7.61783890160981,137.167961950662));
#81584=CARTESIAN_POINT('Ctrl Pts',(79.0850382616431,-7.60770500590972,137.166741735859));
#81585=CARTESIAN_POINT('Ctrl Pts',(79.0927268726588,-7.60268263755114,137.166131768532));
#81586=CARTESIAN_POINT('Ctrl Pts',(79.1106804612623,-7.5911656255291,137.1647204928));
#81587=CARTESIAN_POINT('Ctrl Pts',(79.1209758071485,-7.5847191027587,137.163920987391));
#81588=CARTESIAN_POINT('Ctrl Pts',(79.1515521806562,-7.5660358063852,137.161574346328));
#81589=CARTESIAN_POINT('Ctrl Pts',(79.172025225386,-7.55411795988559,137.160038772768));
#81590=CARTESIAN_POINT('Ctrl Pts',(79.2823685526551,-7.49299711604768,137.151936177905));
#81591=CARTESIAN_POINT('Ctrl Pts',(79.3763824843039,-7.45172448025189,137.145652897398));
#81592=CARTESIAN_POINT('Ctrl Pts',(79.5489222105686,-7.3942642999744,137.134546062335));
#81593=CARTESIAN_POINT('Ctrl Pts',(79.6259336842268,-7.374598219539,137.129721188107));
#81594=CARTESIAN_POINT('Ctrl Pts',(79.7284421092199,-7.35609403781579,137.123153422847));
#81595=CARTESIAN_POINT('Ctrl Pts',(79.7529309360415,-7.35223568187565,137.121573384306));
#81596=CARTESIAN_POINT('Ctrl Pts',(79.794567906668,-7.34662453757074,137.118854549447));
#81597=CARTESIAN_POINT('Ctrl Pts',(79.8116742817811,-7.34458883300667,137.117728320681));
#81598=CARTESIAN_POINT('Ctrl Pts',(79.8362110084004,-7.34205411701391,137.116095777721));
#81599=CARTESIAN_POINT('Ctrl Pts',(79.8436185684363,-7.34133902581075,137.115600689487));
#81600=CARTESIAN_POINT('Ctrl Pts',(79.8565179687512,-7.34018095510876,137.11473428551));
#81601=CARTESIAN_POINT('Ctrl Pts',(79.8620076124977,-7.33971554995454,137.114364214438));
#81602=CARTESIAN_POINT('Ctrl Pts',(79.8737757401039,-7.33877663250152,137.113567875109));
#81603=CARTESIAN_POINT('Ctrl Pts',(79.8800545256124,-7.33831148514745,137.113141185907));
#81604=CARTESIAN_POINT('Ctrl Pts',(79.8973011623914,-7.33713206982759,137.111964461905));
#81605=CARTESIAN_POINT('Ctrl Pts',(79.9082734499359,-7.3364907489447,137.111210629211));
#81606=CARTESIAN_POINT('Ctrl Pts',(79.9706870801465,-7.33346207287906,137.106896027397));
#81607=CARTESIAN_POINT('Ctrl Pts',(80.0222062908539,-7.33335255587465,137.103232702536));
#81608=CARTESIAN_POINT('Ctrl Pts',(80.1695302163405,-7.33987107846556,137.092605930355));
#81609=CARTESIAN_POINT('Ctrl Pts',(80.2648731906396,-7.35239210199664,137.085556050158));
#81610=CARTESIAN_POINT('Ctrl Pts',(80.409985060169,-7.38437757452937,137.074869708017));
#81611=CARTESIAN_POINT('Ctrl Pts',(80.4607981217731,-7.39812935833552,137.071133387273));
#81612=CARTESIAN_POINT('Ctrl Pts',(80.5335741141651,-7.42157573007627,137.06580459824));
#81613=CARTESIAN_POINT('Ctrl Pts',(80.5561102154883,-7.42937399787028,137.064157448522));
#81614=CARTESIAN_POINT('Ctrl Pts',(80.5966738226919,-7.4443930226246,137.061197602513));
#81615=CARTESIAN_POINT('Ctrl Pts',(80.6147569525622,-7.4514501418102,137.059879910339));
#81616=CARTESIAN_POINT('Ctrl Pts',(80.642997515347,-7.46304398699626,137.057824081614));
#81617=CARTESIAN_POINT('Ctrl Pts',(80.6532394096869,-7.46736896982468,137.057078920747));
#81618=CARTESIAN_POINT('Ctrl Pts',(80.672356381081,-7.47566820016619,137.055688555415));
#81619=CARTESIAN_POINT('Ctrl Pts',(80.6812413888095,-7.47961823340645,137.055042563662));
#81620=CARTESIAN_POINT('Ctrl Pts',(80.7011282510186,-7.48866872758541,137.053596874606));
#81621=CARTESIAN_POINT('Ctrl Pts',(80.7121101008661,-7.49381201154106,137.052798682987));
#81622=CARTESIAN_POINT('Ctrl Pts',(80.7442842046183,-7.50931112236119,137.050459779111));
#81623=CARTESIAN_POINT('Ctrl Pts',(80.7653143711202,-7.51999786823467,137.04893051222));
#81624=CARTESIAN_POINT('Ctrl Pts',(80.8774414618012,-7.58000608229351,137.040760427582));
#81625=CARTESIAN_POINT('Ctrl Pts',(80.9640177691385,-7.63729704266457,137.034410865706));
#81626=CARTESIAN_POINT('Ctrl Pts',(81.1059702794231,-7.75157350076364,137.023281539753));
#81627=CARTESIAN_POINT('Ctrl Pts',(81.1636488216443,-7.80515328309771,137.018500501604));
#81628=CARTESIAN_POINT('Ctrl Pts',(81.2341633547055,-7.88062286609127,137.011986918203));
#81629=CARTESIAN_POINT('Ctrl Pts',(81.2505991737976,-7.89901592559647,137.010414528358));
#81630=CARTESIAN_POINT('Ctrl Pts',(81.2777687528396,-7.93081452611746,137.007707578318));
#81631=CARTESIAN_POINT('Ctrl Pts',(81.2887149114812,-7.94403390962229,137.006585441913));
#81632=CARTESIAN_POINT('Ctrl Pts',(81.3041047672187,-7.9632155586324,137.004957795859));
#81633=CARTESIAN_POINT('Ctrl Pts',(81.3087162183797,-7.96904264090452,137.004463420134));
#81634=CARTESIAN_POINT('Ctrl Pts',(81.3166776270797,-7.97924225881998,137.003597819541));
#81635=CARTESIAN_POINT('Ctrl Pts',(81.3200451289696,-7.98360086762118,137.003227832105));
#81636=CARTESIAN_POINT('Ctrl Pts',(81.3272193920897,-7.99298242140102,137.002431150676));
#81637=CARTESIAN_POINT('Ctrl Pts',(81.3310192225362,-7.99801020749411,137.002004031134));
#81638=CARTESIAN_POINT('Ctrl Pts',(81.3413838291799,-8.01188723885079,137.000824990503));
#81639=CARTESIAN_POINT('Ctrl Pts',(81.347889344664,-8.02078005318047,137.000069247937));
#81640=CARTESIAN_POINT('Ctrl Pts',(81.3846160984488,-8.07204371315929,136.99571468891));
#81641=CARTESIAN_POINT('Ctrl Pts',(81.4129241435148,-8.11574389506282,136.992011142933));
#81642=CARTESIAN_POINT('Ctrl Pts',(81.4906692313515,-8.24905122007465,136.980887321945));
#81643=CARTESIAN_POINT('Ctrl Pts',(81.533956939151,-8.34197514854748,136.973368375761));
#81644=CARTESIAN_POINT('Ctrl Pts',(81.5930243260781,-8.50690503324851,136.96080970814));
#81645=CARTESIAN_POINT('Ctrl Pts',(81.6130734390434,-8.57707462971653,136.95568737143));
#81646=CARTESIAN_POINT('Ctrl Pts',(81.6321832050295,-8.66556825751299,136.949508938956));
#81647=CARTESIAN_POINT('Ctrl Pts',(81.6356298002149,-8.68285365641989,136.948314854678));
#81648=CARTESIAN_POINT('Ctrl Pts',(81.6407335345188,-8.71075145200543,136.946407420768));
#81649=CARTESIAN_POINT('Ctrl Pts',(81.642563407467,-8.72133045449254,136.94568864909));
#81650=CARTESIAN_POINT('Ctrl Pts',(81.6458668126839,-8.7415926652274,136.944320371805));
#81651=CARTESIAN_POINT('Ctrl Pts',(81.6473574585509,-8.75127258594335,136.943670351426));
#81652=CARTESIAN_POINT('Ctrl Pts',(81.6505659021743,-8.77340310262026,136.942192292773));
#81653=CARTESIAN_POINT('Ctrl Pts',(81.6522283581794,-8.78586121756385,136.94136602735));
#81654=CARTESIAN_POINT('Ctrl Pts',(81.6562911740907,-8.81917862691827,136.939170897462));
#81655=CARTESIAN_POINT('Ctrl Pts',(81.6584385088627,-8.84006689597057,136.937809920035));
#81656=CARTESIAN_POINT('Ctrl Pts',(81.6702856578205,-8.98155785591697,136.928681678237));
#81657=CARTESIAN_POINT('Ctrl Pts',(81.6672181616441,-9.10286759374759,136.92133377957));
#81658=CARTESIAN_POINT('Ctrl Pts',(81.6421933819359,-9.28832325615413,136.909898570094));
#81659=CARTESIAN_POINT('Ctrl Pts',(81.6294561155291,-9.35327172153023,136.905846244306));
#81660=CARTESIAN_POINT('Ctrl Pts',(81.6072764738956,-9.43900046420705,136.900241485791));
#81661=CARTESIAN_POINT('Ctrl Pts',(81.6012209198121,-9.46059802079472,136.898806991174));
#81662=CARTESIAN_POINT('Ctrl Pts',(81.5901049388938,-9.49737103224749,136.896315484499));
#81663=CARTESIAN_POINT('Ctrl Pts',(81.5852584361791,-9.51260833480376,136.895268448324));
#81664=CARTESIAN_POINT('Ctrl Pts',(81.577904757381,-9.53462583093099,136.893730925547));
#81665=CARTESIAN_POINT('Ctrl Pts',(81.57557140313,-9.54146371187931,136.893249948932));
#81666=CARTESIAN_POINT('Ctrl Pts',(81.5714046680247,-9.55341929879982,136.892402531769));
#81667=CARTESIAN_POINT('Ctrl Pts',(81.5695906049574,-9.55854353687809,136.892037219388));
#81668=CARTESIAN_POINT('Ctrl Pts',(81.565583310173,-9.56968935902594,136.891237933373));
#81669=CARTESIAN_POINT('Ctrl Pts',(81.5633804395223,-9.57570709978228,136.890803426458));
#81670=CARTESIAN_POINT('Ctrl Pts',(81.5571307728611,-9.59247936082111,136.889584395084));
#81671=CARTESIAN_POINT('Ctrl Pts',(81.5530074393112,-9.60320470152957,136.888795632103));
#81672=CARTESIAN_POINT('Ctrl Pts',(81.5243353306837,-9.67554157651748,136.88341713847));
#81673=CARTESIAN_POINT('Ctrl Pts',(81.4962397283866,-9.73567610515647,136.878658160536));
#81674=CARTESIAN_POINT('Ctrl Pts',(81.4542098855688,-9.81320879768197,136.872264086088));
#81675=CARTESIAN_POINT('Ctrl Pts',(81.4434022627158,-9.83224084803977,136.870672475403));
#81676=CARTESIAN_POINT('Ctrl Pts',(81.3961142480812,-9.91182094501964,136.863935160198));
#81677=CARTESIAN_POINT('Ctrl Pts',(81.356172711813,-9.97023146690618,136.858789052242));
#81678=CARTESIAN_POINT('Ctrl Pts',(81.2707344875501,-10.0795464616061,136.848870215821));
#81679=CARTESIAN_POINT('Ctrl Pts',(81.2255795816743,-10.1305501149061,136.844099710361));
#81680=CARTESIAN_POINT('Ctrl Pts',(81.1651733223514,-10.1908933739795,136.838275596081));
#81681=CARTESIAN_POINT('Ctrl Pts',(81.1527310720011,-10.2029409853636,136.837102701328));
#81682=CARTESIAN_POINT('Ctrl Pts',(81.1323226691134,-10.2220946034857,136.835220753704));
#81683=CARTESIAN_POINT('Ctrl Pts',(81.1244724042254,-10.2293216292539,136.83450653695));
#81684=CARTESIAN_POINT('Ctrl Pts',(81.1092701341845,-10.2430495013136,136.833141614853));
#81685=CARTESIAN_POINT('Ctrl Pts',(81.1019290860147,-10.2495617590704,136.832490444838));
#81686=CARTESIAN_POINT('Ctrl Pts',(81.0849533051084,-10.2643550578846,136.831002433068));
#81687=CARTESIAN_POINT('Ctrl Pts',(81.075280455923,-10.2725915851624,136.830167449989));
#81688=CARTESIAN_POINT('Ctrl Pts',(81.0437811266256,-10.2987979864457,136.827488467548));
#81689=CARTESIAN_POINT('Ctrl Pts',(81.0215904795059,-10.3163237796437,136.825662270724));
#81690=CARTESIAN_POINT('Ctrl Pts',(80.8941829600746,-10.4117843904456,136.815487987002));
#81691=CARTESIAN_POINT('Ctrl Pts',(80.7805155922315,-10.477665785899,136.807616109418));
#81692=CARTESIAN_POINT('Ctrl Pts',(80.5948102165628,-10.5578334716761,136.795205826581));
#81693=CARTESIAN_POINT('Ctrl Pts',(80.5275786266557,-10.5818668656425,136.790783731773));
#81694=CARTESIAN_POINT('Ctrl Pts',(80.4438609717809,-10.6058618263717,136.785133352981));
#81695=CARTESIAN_POINT('Ctrl Pts',(80.428638808202,-10.6099917687636,136.784100222729));
#81696=CARTESIAN_POINT('Ctrl Pts',(80.406399766443,-10.6156877382123,136.782579442641));
#81697=CARTESIAN_POINT('Ctrl Pts',(80.3994272362334,-10.6174255827648,136.782101015622));
#81698=CARTESIAN_POINT('Ctrl Pts',(80.387164519408,-10.6203978349666,136.781256399625));
#81699=CARTESIAN_POINT('Ctrl Pts',(80.3818792114243,-10.6216515579059,136.780891313014));
#81700=CARTESIAN_POINT('Ctrl Pts',(80.3703196916429,-10.6243339342483,136.780090444845));
#81701=CARTESIAN_POINT('Ctrl Pts',(80.3640434023766,-10.6257520726284,136.779654110995));
#81702=CARTESIAN_POINT('Ctrl Pts',(80.3464214875973,-10.629626616931,136.778425119894));
#81703=CARTESIAN_POINT('Ctrl Pts',(80.3350584324346,-10.6320007921896,136.777628117311));
#81704=CARTESIAN_POINT('Ctrl Pts',(80.2481873668732,-10.6492060058914,136.771505309369));
#81705=CARTESIAN_POINT('Ctrl Pts',(80.1717659562092,-10.6589066249809,136.765952496989));
#81706=CARTESIAN_POINT('Ctrl Pts',(80.0378293131449,-10.6665530998448,136.756201245071));
#81707=CARTESIAN_POINT('Ctrl Pts',(79.9805694525012,-10.6668692240055,136.752025590368));
#81708=CARTESIAN_POINT('Ctrl Pts',(79.8407066776633,-10.6604322746638,136.741907962373));
#81709=CARTESIAN_POINT('Ctrl Pts',(79.7583961203379,-10.6504668633876,136.736028769055));
#81710=CARTESIAN_POINT('Ctrl Pts',(79.6547453997424,-10.6299929870419,136.728765173955));
#81711=CARTESIAN_POINT('Ctrl Pts',(79.6324263275546,-10.6251054002649,136.727208925176));
#81712=CARTESIAN_POINT('Ctrl Pts',(79.5987168025749,-10.6169933927209,136.724869244062));
#81713=CARTESIAN_POINT('Ctrl Pts',(79.5872492926389,-10.6141043035424,136.724075221344));
#81714=CARTESIAN_POINT('Ctrl Pts',(79.5673378331323,-10.6088617907514,136.722699560353));
#81715=CARTESIAN_POINT('Ctrl Pts',(79.5588800167884,-10.606563406102,136.722116176556));
#81716=CARTESIAN_POINT('Ctrl Pts',(79.5398471622232,-10.601229652412,136.720805344988));
#81717=CARTESIAN_POINT('Ctrl Pts',(79.5292831919322,-10.5981560406459,136.720079165132));
#81718=CARTESIAN_POINT('Ctrl Pts',(79.5006887586706,-10.589528294682,136.718116776693));
#81719=CARTESIAN_POINT('Ctrl Pts',(79.482720595688,-10.5837720733188,136.716887172434));
#81720=CARTESIAN_POINT('Ctrl Pts',(79.3710001194815,-10.5458774279842,136.709256356354));
#81721=CARTESIAN_POINT('Ctrl Pts',(79.2801691849516,-10.5057307623201,136.703132604211));
#81722=CARTESIAN_POINT('Ctrl Pts',(79.1307980769976,-10.423084225761,136.692690283821));
#81723=CARTESIAN_POINT('Ctrl Pts',(79.0704611377027,-10.384426766757,136.688349133291));
#81724=CARTESIAN_POINT('Ctrl Pts',(78.9831009961099,-10.3201635222736,136.681614700908));
#81725=CARTESIAN_POINT('Ctrl Pts',(78.9541373767744,-10.2973381718092,136.679299001643));
#81726=CARTESIAN_POINT('Ctrl Pts',(78.9140155203406,-10.2635021618502,136.675932793283));
#81727=CARTESIAN_POINT('Ctrl Pts',(78.902217052264,-10.2532647623231,136.674922358475));
#81728=CARTESIAN_POINT('Ctrl Pts',(78.881514870769,-10.2347850724395,136.673108805605));
#81729=CARTESIAN_POINT('Ctrl Pts',(78.8725538246555,-10.2266084379607,136.672309844211));
#81730=CARTESIAN_POINT('Ctrl Pts',(78.8589482644406,-10.2139188024175,136.67107368102));
#81731=CARTESIAN_POINT('Ctrl Pts',(78.8542392234489,-10.2094751595079,136.670641495881));
#81732=CARTESIAN_POINT('Ctrl Pts',(78.8455932379682,-10.2012206497899,136.669839668113));
#81733=CARTESIAN_POINT('Ctrl Pts',(78.8416490461505,-10.197417674136,136.669470616557));
#81734=CARTESIAN_POINT('Ctrl Pts',(78.8326801841062,-10.1886841482209,136.668623952236));
#81735=CARTESIAN_POINT('Ctrl Pts',(78.8276679565666,-10.1837411593081,136.668145400797));
#81736=CARTESIAN_POINT('Ctrl Pts',(78.8118019440852,-10.1678947172797,136.666613717909));
#81737=CARTESIAN_POINT('Ctrl Pts',(78.8010681616062,-10.1568729816143,136.665552075737));
#81738=CARTESIAN_POINT('Ctrl Pts',(78.7015875274873,-10.0518520987993,136.655483808707));
#81739=CARTESIAN_POINT('Ctrl Pts',(78.6239166161286,-9.94797679901163,136.645917796238));
#81740=CARTESIAN_POINT('Ctrl Pts',(78.5140359773491,-9.75862128761004,136.630101981317));
#81741=CARTESIAN_POINT('Ctrl Pts',(78.4753620663599,-9.67755384702874,136.623750119211));
#81742=CARTESIAN_POINT('Ctrl Pts',(78.4368323410281,-9.57654332016253,136.616363176341));
#81743=CARTESIAN_POINT('Ctrl Pts',(78.4305529036133,-9.55922373788411,136.615113945007));
#81744=CARTESIAN_POINT('Ctrl Pts',(78.4210148636928,-9.53148931414127,136.613140230456));
#81745=CARTESIAN_POINT('Ctrl Pts',(78.4175692330125,-9.52114089189607,136.612409630781));
#81746=CARTESIAN_POINT('Ctrl Pts',(78.4112349081996,-9.50147445784116,136.611031945276));
#81747=CARTESIAN_POINT('Ctrl Pts',(78.4083259626888,-9.49216350398151,136.610384219371));
#81748=CARTESIAN_POINT('Ctrl Pts',(78.4018883936778,-9.47090391612322,136.608915284332));
#81749=CARTESIAN_POINT('Ctrl Pts',(78.3984116571421,-9.45894008165288,136.608095793143));
#81750=CARTESIAN_POINT('Ctrl Pts',(78.3896655905076,-9.42753342749442,136.605962376743));
#81751=CARTESIAN_POINT('Ctrl Pts',(78.3846140042365,-9.40803171779105,136.604655448837));
#81752=CARTESIAN_POINT('Ctrl Pts',(78.3492974627889,-9.26073649740845,136.594905558187));
#81753=CARTESIAN_POINT('Ctrl Pts',(78.3338838505488,-9.12985839975195,136.586972010518));
#81754=CARTESIAN_POINT('Ctrl Pts',(78.334019749062,-8.97705318451493,136.5776200138));
#81755=CARTESIAN_POINT('Ctrl Pts',(78.3344536807646,-8.95559071879492,136.576303216903));
#81756=CARTESIAN_POINT('Ctrl Pts',(78.3378839471517,-8.86888232659901,136.570951022189));
#81757=CARTESIAN_POINT('Ctrl Pts',(78.3443007974377,-8.80383754936091,136.566862976514));
#81758=CARTESIAN_POINT('Ctrl Pts',(78.3563104882211,-8.72802161356447,136.561840519403));
#81759=CARTESIAN_POINT('Ctrl Pts',(78.3582210876476,-8.7167166808898,136.561084779101));
#81760=CARTESIAN_POINT('Ctrl Pts',(78.361380210958,-8.69913095672272,136.559897211975));
#81761=CARTESIAN_POINT('Ctrl Pts',(78.3625485697071,-8.69283586757687,136.559469706871));
#81762=CARTESIAN_POINT('Ctrl Pts',(78.3647761196605,-8.68120786947389,136.558675339287));
#81763=CARTESIAN_POINT('Ctrl Pts',(78.3658251659638,-8.67587321933013,136.558309044853));
#81764=CARTESIAN_POINT('Ctrl Pts',(78.3683307942889,-8.66345292970111,136.557451946765));
#81765=CARTESIAN_POINT('Ctrl Pts',(78.3698074268084,-8.65637157157594,136.556960043696));
#81766=CARTESIAN_POINT('Ctrl Pts',(78.3747060489727,-8.63362208901498,136.555369833779));
#81767=CARTESIAN_POINT('Ctrl Pts',(78.3783080608523,-8.61799423022668,136.5542622448));
#81768=CARTESIAN_POINT('Ctrl Pts',(78.3875089984116,-8.58055287725605,136.551575912956));
#81769=CARTESIAN_POINT('Ctrl Pts',(78.3933256425078,-8.55879650374042,136.549987992049));
#81770=CARTESIAN_POINT('Ctrl Pts',(78.4105689037284,-8.49917160166134,136.545573099394));
#81771=CARTESIAN_POINT('Ctrl Pts',(78.4229034382648,-8.46159013275024,136.542719630848));
#81772=CARTESIAN_POINT('Ctrl Pts',(78.4365593622862,-8.42449207447235,136.539851301691));
#81773=CARTESIAN_POINT('Ctrl Pts',(78.4365593881204,-8.4244920042904,136.733447186333));
#81774=CARTESIAN_POINT('Ctrl Pts',(78.4030736945878,-8.51546014648167,136.739621454435));
#81775=CARTESIAN_POINT('Ctrl Pts',(78.3775820369106,-8.6092014352621,136.745546832545));
#81776=CARTESIAN_POINT('Ctrl Pts',(78.3470673853013,-8.7786056050962,136.756057576631));
#81777=CARTESIAN_POINT('Ctrl Pts',(78.3387660631224,-8.85336467809191,136.760635535814));
#81778=CARTESIAN_POINT('Ctrl Pts',(78.3345040617009,-8.95247331443709,136.766897335687));
#81779=CARTESIAN_POINT('Ctrl Pts',(78.3339912587448,-8.976542383031,136.768433278269));
#81780=CARTESIAN_POINT('Ctrl Pts',(78.3340063127194,-9.01746820049141,136.771083447886));
#81781=CARTESIAN_POINT('Ctrl Pts',(78.3342683081296,-9.03432173335585,136.772185923354));
#81782=CARTESIAN_POINT('Ctrl Pts',(78.3350100826228,-9.05846227663029,136.773784728963));
#81783=CARTESIAN_POINT('Ctrl Pts',(78.3352821544246,-9.06575524640231,136.774270308084));
#81784=CARTESIAN_POINT('Ctrl Pts',(78.3358435544196,-9.07854708528083,136.775126896748));
#81785=CARTESIAN_POINT('Ctrl Pts',(78.3361122407625,-9.0840466752278,136.775496764983));
#81786=CARTESIAN_POINT('Ctrl Pts',(78.3367468936854,-9.09583743544319,136.776293281405));
#81787=CARTESIAN_POINT('Ctrl Pts',(78.3371212848046,-9.10212778735096,136.776720355728));
#81788=CARTESIAN_POINT('Ctrl Pts',(78.3382678805403,-9.11970991711179,136.77791975653));
#81789=CARTESIAN_POINT('Ctrl Pts',(78.3391194647483,-9.1309959204132,136.778696218196));
#81790=CARTESIAN_POINT('Ctrl Pts',(78.3456209276976,-9.20684971771665,136.783955189898));
#81791=CARTESIAN_POINT('Ctrl Pts',(78.3549191552492,-9.27104252512709,136.788600551448));
#81792=CARTESIAN_POINT('Ctrl Pts',(78.3892327549589,-9.43845169740273,136.800982562631));
#81793=CARTESIAN_POINT('Ctrl Pts',(78.4204158893562,-9.54011910056802,136.808760889797));
#81794=CARTESIAN_POINT('Ctrl Pts',(78.4829022374298,-9.690813060589,136.820349834248));
#81795=CARTESIAN_POINT('Ctrl Pts',(78.5074386473511,-9.74234104091414,136.824328710901));
#81796=CARTESIAN_POINT('Ctrl Pts',(78.5427106347886,-9.80756198835594,136.829384765667));
#81797=CARTESIAN_POINT('Ctrl Pts',(78.5510800918421,-9.82248391877545,136.83054312028));
#81798=CARTESIAN_POINT('Ctrl Pts',(78.5650169043896,-9.8464587183596,136.832407449484));
#81799=CARTESIAN_POINT('Ctrl Pts',(78.5704434462281,-9.85559155861872,136.833118414691));
#81800=CARTESIAN_POINT('Ctrl Pts',(78.5810561551776,-9.87306980706646,136.834480806376));
#81801=CARTESIAN_POINT('Ctrl Pts',(78.5862295038704,-9.881422437934,136.83513266302));
#81802=CARTESIAN_POINT('Ctrl Pts',(78.5984297757597,-9.90073659966631,136.836642117404));
#81803=CARTESIAN_POINT('Ctrl Pts',(78.6055119745721,-9.91166259019809,136.837497634055));
#81804=CARTESIAN_POINT('Ctrl Pts',(78.6289516698963,-9.94691160386154,136.840264130959));
#81805=CARTESIAN_POINT('Ctrl Pts',(78.6458236350977,-9.9708870422807,136.842155868848));
#81806=CARTESIAN_POINT('Ctrl Pts',(78.687779259035,-10.0272837545402,136.846642823129));
#81807=CARTESIAN_POINT('Ctrl Pts',(78.7134440285047,-10.0592493898091,136.849216597647));
#81808=CARTESIAN_POINT('Ctrl Pts',(78.7883692976428,-10.1458232872106,136.856329676963));
#81809=CARTESIAN_POINT('Ctrl Pts',(78.8401032628258,-10.1981652664024,136.860796537195));
#81810=CARTESIAN_POINT('Ctrl Pts',(78.9595922688885,-10.3040424533988,136.870555924798));
#81811=CARTESIAN_POINT('Ctrl Pts',(79.028384029632,-10.3560728796528,136.87584406862));
#81812=CARTESIAN_POINT('Ctrl Pts',(79.114166368779,-10.4110648129433,136.882455015258));
#81813=CARTESIAN_POINT('Ctrl Pts',(79.1275739912358,-10.4193935125204,136.883488879084));
#81814=CARTESIAN_POINT('Ctrl Pts',(79.1471900400681,-10.4311959096451,136.885005410462));
#81815=CARTESIAN_POINT('Ctrl Pts',(79.1533060366019,-10.4348225978468,136.885478788803));
#81816=CARTESIAN_POINT('Ctrl Pts',(79.1641802255776,-10.4411770831021,136.886321761173));
#81817=CARTESIAN_POINT('Ctrl Pts',(79.1689289465603,-10.4439206983225,136.886690335297));
#81818=CARTESIAN_POINT('Ctrl Pts',(79.1792667995152,-10.449825590466,136.887493785354));
#81819=CARTESIAN_POINT('Ctrl Pts',(79.18486060001,-10.4529779710146,136.887929175106));
#81820=CARTESIAN_POINT('Ctrl Pts',(79.2008555866187,-10.4618704939397,136.889175660464));
#81821=CARTESIAN_POINT('Ctrl Pts',(79.211299890914,-10.4675316869695,136.889991408645));
#81822=CARTESIAN_POINT('Ctrl Pts',(79.2352487806186,-10.48018336694,136.891864560845));
#81823=CARTESIAN_POINT('Ctrl Pts',(79.2487901943231,-10.4871015496115,136.89292557646));
#81824=CARTESIAN_POINT('Ctrl Pts',(79.3926802361372,-10.5581468755979,136.904205445557));
#81825=CARTESIAN_POINT('Ctrl Pts',(79.5307877751497,-10.6051487126799,136.915012031052));
#81826=CARTESIAN_POINT('Ctrl Pts',(79.7375228892412,-10.646498846995,136.930069698027));
#81827=CARTESIAN_POINT('Ctrl Pts',(79.8025079980723,-10.6555517333834,136.934662415066));
#81828=CARTESIAN_POINT('Ctrl Pts',(79.8854547239337,-10.6621512331637,136.940341172531));
#81829=CARTESIAN_POINT('Ctrl Pts',(79.9030657133278,-10.6632712129491,136.941536703293));
#81830=CARTESIAN_POINT('Ctrl Pts',(79.9314178227011,-10.6646224179439,136.943445749573));
#81831=CARTESIAN_POINT('Ctrl Pts',(79.942148771015,-10.66502989583,136.944164706079));
#81832=CARTESIAN_POINT('Ctrl Pts',(79.9626686379264,-10.6656104593268,136.945532894171));
#81833=CARTESIAN_POINT('Ctrl Pts',(79.9724565693854,-10.6658010683219,136.946182644441));
#81834=CARTESIAN_POINT('Ctrl Pts',(79.9950118735277,-10.6660414490357,136.947673600115));
#81835=CARTESIAN_POINT('Ctrl Pts',(80.0077793809961,-10.6660307583072,136.948512888166));
#81836=CARTESIAN_POINT('Ctrl Pts',(80.0484004376635,-10.6655297644201,136.951169351394));
#81837=CARTESIAN_POINT('Ctrl Pts',(80.0762432688115,-10.6644876410038,136.952969411709));
#81838=CARTESIAN_POINT('Ctrl Pts',(80.17707580758,-10.6581779363621,136.959429051887));
#81839=CARTESIAN_POINT('Ctrl Pts',(80.2497269836236,-10.6488019685092,136.963966280212));
#81840=CARTESIAN_POINT('Ctrl Pts',(80.4498323691207,-10.6094423174595,136.976475569173));
#81841=CARTESIAN_POINT('Ctrl Pts',(80.5746952258867,-10.5691937199781,136.984278196408));
#81842=CARTESIAN_POINT('Ctrl Pts',(80.7072593246362,-10.5084984670799,136.993749889294));
#81843=CARTESIAN_POINT('Ctrl Pts',(80.7208831856639,-10.5020355425522,136.994738555911));
#81844=CARTESIAN_POINT('Ctrl Pts',(80.7407513367565,-10.4922778766141,136.996205607827));
#81845=CARTESIAN_POINT('Ctrl Pts',(80.7470658423804,-10.4891267328796,136.996675659482));
#81846=CARTESIAN_POINT('Ctrl Pts',(80.7582388396376,-10.4834620937601,136.997514468975));
#81847=CARTESIAN_POINT('Ctrl Pts',(80.7631052433752,-10.4809646543762,136.997882236156));
#81848=CARTESIAN_POINT('Ctrl Pts',(80.7737687639961,-10.4754256182811,136.998693515298));
#81849=CARTESIAN_POINT('Ctrl Pts',(80.7795602064822,-10.4723738438356,136.999137630889));
#81850=CARTESIAN_POINT('Ctrl Pts',(80.7963407056481,-10.4634046795101,137.000434326687));
#81851=CARTESIAN_POINT('Ctrl Pts',(80.8072811569883,-10.4573979847158,137.001292141429));
#81852=CARTESIAN_POINT('Ctrl Pts',(80.8970833642042,-10.4067720101496,137.008430061082));
#81853=CARTESIAN_POINT('Ctrl Pts',(80.9722441434968,-10.3559144171397,137.01501705316));
#81854=CARTESIAN_POINT('Ctrl Pts',(81.1403180900579,-10.2209993084927,137.030705606517));
#81855=CARTESIAN_POINT('Ctrl Pts',(81.2286584273756,-10.1320663474827,137.039739972988));
#81856=CARTESIAN_POINT('Ctrl Pts',(81.3190964111585,-10.0178262180048,137.049759134163));
#81857=CARTESIAN_POINT('Ctrl Pts',(81.3316568116364,-10.0013369837524,137.051172559126));
#81858=CARTESIAN_POINT('Ctrl Pts',(81.3512882083391,-9.97454203031362,137.053418518639));
#81859=CARTESIAN_POINT('Ctrl Pts',(81.3585563025847,-9.96438414456928,137.054258601021));
#81860=CARTESIAN_POINT('Ctrl Pts',(81.3713113262891,-9.94612732341943,137.055748741476));
#81861=CARTESIAN_POINT('Ctrl Pts',(81.3768423814852,-9.93806008831394,137.056400462165));
#81862=CARTESIAN_POINT('Ctrl Pts',(81.388314362337,-9.92100773224648,137.057764231038));
#81863=CARTESIAN_POINT('Ctrl Pts',(81.39423985985,-9.91201273780734,137.058475678021));
#81864=CARTESIAN_POINT('Ctrl Pts',(81.4097237013106,-9.88800440344568,137.06035416898));
#81865=CARTESIAN_POINT('Ctrl Pts',(81.4191295884013,-9.87289402885515,137.061515560676));
#81866=CARTESIAN_POINT('Ctrl Pts',(81.4674035912919,-9.79249929604251,137.067591076656));
#81867=CARTESIAN_POINT('Ctrl Pts',(81.5020166326017,-9.7247596804068,137.072349634004));
#81868=CARTESIAN_POINT('Ctrl Pts',(81.5734663343402,-9.55762699477199,137.083554347229));
#81869=CARTESIAN_POINT('Ctrl Pts',(81.6056856278077,-9.45663511974328,137.089898723803));
#81870=CARTESIAN_POINT('Ctrl Pts',(81.6378182559004,-9.30854847151764,137.09936819472));
#81871=CARTESIAN_POINT('Ctrl Pts',(81.6456753667433,-9.26344366715188,137.102276282563));
#81872=CARTESIAN_POINT('Ctrl Pts',(81.6530800128923,-9.20736267157802,137.105984314004));
#81873=CARTESIAN_POINT('Ctrl Pts',(81.6543903865843,-9.19663478889484,137.106697782848));
#81874=CARTESIAN_POINT('Ctrl Pts',(81.6562871041937,-9.17974248924931,137.107828819388));
#81875=CARTESIAN_POINT('Ctrl Pts',(81.6569436381821,-9.17358603264176,137.108242613114));
#81876=CARTESIAN_POINT('Ctrl Pts',(81.6581221064551,-9.16191886877446,137.109030039472));
#81877=CARTESIAN_POINT('Ctrl Pts',(81.6586509120692,-9.15640904111595,137.109403291966));
#81878=CARTESIAN_POINT('Ctrl Pts',(81.6598439596103,-9.14329115099583,137.110295138221));
#81879=CARTESIAN_POINT('Ctrl Pts',(81.6604833562444,-9.1356810308897,137.110815072687));
#81880=CARTESIAN_POINT('Ctrl Pts',(81.6624850134589,-9.10971888398158,137.112596910054));
#81881=CARTESIAN_POINT('Ctrl Pts',(81.663595457097,-9.09134954271517,137.113871358065));
#81882=CARTESIAN_POINT('Ctrl Pts',(81.6655890493043,-9.0458747670624,137.117054282046));
#81883=CARTESIAN_POINT('Ctrl Pts',(81.6661150297035,-9.0187594914234,137.118976628921));
#81884=CARTESIAN_POINT('Ctrl Pts',(81.665502353316,-8.89659148234794,137.127715518917));
#81885=CARTESIAN_POINT('Ctrl Pts',(81.6568917014446,-8.80175481881864,137.134699384888));
#81886=CARTESIAN_POINT('Ctrl Pts',(81.6241860233122,-8.61793103655888,137.148200103104));
#81887=CARTESIAN_POINT('Ctrl Pts',(81.6007092506829,-8.52915839469721,137.154701657713));
#81888=CARTESIAN_POINT('Ctrl Pts',(81.5637647548798,-8.42506688566657,137.162252692951));
#81889=CARTESIAN_POINT('Ctrl Pts',(81.5571880318334,-8.40748520854705,137.163526063361));
#81890=CARTESIAN_POINT('Ctrl Pts',(81.5462955055341,-8.37980103947063,137.165528628987));
#81891=CARTESIAN_POINT('Ctrl Pts',(81.5421746800608,-8.36962407466295,137.166264256121));
#81892=CARTESIAN_POINT('Ctrl Pts',(81.5345838467956,-8.35139747600969,137.167581030549));
#81893=CARTESIAN_POINT('Ctrl Pts',(81.5311503807921,-8.34333316408331,137.168163382486));
#81894=CARTESIAN_POINT('Ctrl Pts',(81.522925753619,-8.32443094134723,137.169527991053));
#81895=CARTESIAN_POINT('Ctrl Pts',(81.5180822481688,-8.31361621233241,137.170308435965));
#81896=CARTESIAN_POINT('Ctrl Pts',(81.5035097039028,-8.28198717541995,137.172590804864));
#81897=CARTESIAN_POINT('Ctrl Pts',(81.4934647746397,-8.26132084362126,137.174081880258));
#81898=CARTESIAN_POINT('Ctrl Pts',(81.4447953142107,-8.16624307054402,137.180951620334));
#81899=CARTESIAN_POINT('Ctrl Pts',(81.4010152041951,-8.09460346171918,137.186148617948));
#81900=CARTESIAN_POINT('Ctrl Pts',(81.3008705401275,-7.95551164674379,137.196652378125));
#81901=CARTESIAN_POINT('Ctrl Pts',(81.2442006213366,-7.88861193906081,137.20193831183));
#81902=CARTESIAN_POINT('Ctrl Pts',(81.1495068912117,-7.79319049627619,137.21033118623));
#81903=CARTESIAN_POINT('Ctrl Pts',(81.1150857141232,-7.76131592118927,137.213308127978));
#81904=CARTESIAN_POINT('Ctrl Pts',(81.0710771882292,-7.72388551734343,137.217094491853));
#81905=CARTESIAN_POINT('Ctrl Pts',(81.0627158218324,-7.71691403930226,137.217813057695));
#81906=CARTESIAN_POINT('Ctrl Pts',(81.0494797805833,-7.70609631889675,137.218950369127));
#81907=CARTESIAN_POINT('Ctrl Pts',(81.0446507239971,-7.70219438761639,137.219365270916));
#81908=CARTESIAN_POINT('Ctrl Pts',(81.0354791978529,-7.69486804724877,137.220153445191));
#81909=CARTESIAN_POINT('Ctrl Pts',(81.0311413471601,-7.69143815516734,137.220526324128));
#81910=CARTESIAN_POINT('Ctrl Pts',(81.0207998958806,-7.68334462915329,137.221415396917));
#81911=CARTESIAN_POINT('Ctrl Pts',(81.0147813537242,-7.67870041568294,137.221932908338));
#81912=CARTESIAN_POINT('Ctrl Pts',(80.9942551414701,-7.66308430727233,137.22369757671));
#81913=CARTESIAN_POINT('Ctrl Pts',(80.9796002248323,-7.65230931297159,137.224956966311));
#81914=CARTESIAN_POINT('Ctrl Pts',(80.9430135399167,-7.6263210689669,137.228094086435));
#81915=CARTESIAN_POINT('Ctrl Pts',(80.9208873689399,-7.61139111429586,137.229985214478));
#81916=CARTESIAN_POINT('Ctrl Pts',(80.8209939379261,-7.54742418886821,137.238466092561));
#81917=CARTESIAN_POINT('Ctrl Pts',(80.7396056100558,-7.50434271516757,137.245215577464));
#81918=CARTESIAN_POINT('Ctrl Pts',(80.5674640664469,-7.43072593788484,137.258770013421));
#81919=CARTESIAN_POINT('Ctrl Pts',(80.4767826088042,-7.40083757849732,137.265540872448));
#81920=CARTESIAN_POINT('Ctrl Pts',(80.3656505449698,-7.37451164804401,137.273349923768));
#81921=CARTESIAN_POINT('Ctrl Pts',(80.3471992399141,-7.37047079126015,137.274631403468));
#81922=CARTESIAN_POINT('Ctrl Pts',(80.3178947134579,-7.36457343749752,137.276643698277));
#81923=CARTESIAN_POINT('Ctrl Pts',(80.3070854331381,-7.36250934750913,137.277381052308));
#81924=CARTESIAN_POINT('Ctrl Pts',(80.2876348235573,-7.35899452629569,137.278699344028));
#81925=CARTESIAN_POINT('Ctrl Pts',(80.2790010878172,-7.35750459529958,137.279281503469));
#81926=CARTESIAN_POINT('Ctrl Pts',(80.2586983642431,-7.35416564350015,137.280643646055));
#81927=CARTESIAN_POINT('Ctrl Pts',(80.2470205646876,-7.35237248586113,137.281421839117));
#81928=CARTESIAN_POINT('Ctrl Pts',(80.2127545332068,-7.34748334988967,137.283690554916));
#81929=CARTESIAN_POINT('Ctrl Pts',(80.1901200915037,-7.34472654753425,137.285170430414));
#81930=CARTESIAN_POINT('Ctrl Pts',(80.0854031239648,-7.33414879322847,137.291941335192));
#81931=CARTESIAN_POINT('Ctrl Pts',(80.002864225,-7.33196281932455,137.297057058166));
#81932=CARTESIAN_POINT('Ctrl Pts',(79.7919194644137,-7.34204107561868,137.310005486723));
#81933=CARTESIAN_POINT('Ctrl Pts',(79.664509127047,-7.3630633913947,137.317694886708));
#81934=CARTESIAN_POINT('Ctrl Pts',(79.5273692636888,-7.40238562815179,137.326955958689));
#81935=CARTESIAN_POINT('Ctrl Pts',(79.5139785017933,-7.40640828107118,137.327871331792));
#81936=CARTESIAN_POINT('Ctrl Pts',(79.4940024158347,-7.41268438603332,137.329255760459));
#81937=CARTESIAN_POINT('Ctrl Pts',(79.4873776210148,-7.4148114604742,137.329718024127));
#81938=CARTESIAN_POINT('Ctrl Pts',(79.4754516813434,-7.41872319071898,137.330556189795));
#81939=CARTESIAN_POINT('Ctrl Pts',(79.4701457492388,-7.42049319157249,137.330931250759));
#81940=CARTESIAN_POINT('Ctrl Pts',(79.4592424670526,-7.42419152855173,137.331706602901));
#81941=CARTESIAN_POINT('Ctrl Pts',(79.4536463463172,-7.42612302562506,137.332107063082));
#81942=CARTESIAN_POINT('Ctrl Pts',(79.4390329966833,-7.43125414116497,137.333159158438));
#81943=CARTESIAN_POINT('Ctrl Pts',(79.4300329836935,-7.43450163274381,137.333813480159));
#81944=CARTESIAN_POINT('Ctrl Pts',(79.3889993801016,-7.44970860057302,137.33682431057));
#81945=CARTESIAN_POINT('Ctrl Pts',(79.3573129913227,-7.46257416219897,137.339226467524));
#81946=CARTESIAN_POINT('Ctrl Pts',(79.2627235372162,-7.50441517704138,137.346588336996));
#81947=CARTESIAN_POINT('Ctrl Pts',(79.2012105148663,-7.53634533445654,137.351635606992));
#81948=CARTESIAN_POINT('Ctrl Pts',(79.0420267517058,-7.63200485642804,137.365152648743));
#81949=CARTESIAN_POINT('Ctrl Pts',(78.9487381917789,-7.70231699241491,137.373548315926));
#81950=CARTESIAN_POINT('Ctrl Pts',(78.8480522834023,-7.79624712134135,137.383022913099));
#81951=CARTESIAN_POINT('Ctrl Pts',(78.8328425060737,-7.81098864997468,137.384467923748));
#81952=CARTESIAN_POINT('Ctrl Pts',(78.8090260155006,-7.83496945372168,137.386753858893));
#81953=CARTESIAN_POINT('Ctrl Pts',(78.8002364893233,-7.84402303692085,137.387602764272));
#81954=CARTESIAN_POINT('Ctrl Pts',(78.784805559936,-7.86028315769854,137.389102934962));
#81955=CARTESIAN_POINT('Ctrl Pts',(78.7781233786036,-7.86744998480212,137.389755943137));
#81956=CARTESIAN_POINT('Ctrl Pts',(78.76427297701,-7.88257020400818,137.391116832424));
#81957=CARTESIAN_POINT('Ctrl Pts',(78.7571173950721,-7.89053460454368,137.391824161008));
#81958=CARTESIAN_POINT('Ctrl Pts',(78.7410372318918,-7.90878318484026,137.393423843834));
#81959=CARTESIAN_POINT('Ctrl Pts',(78.7321608837218,-7.91910898683019,137.394314188008));
#81960=CARTESIAN_POINT('Ctrl Pts',(78.6928012258623,-7.96604787071688,137.398297492482));
#81961=CARTESIAN_POINT('Ctrl Pts',(78.6637685887258,-8.00385146548987,137.401332334813));
#81962=CARTESIAN_POINT('Ctrl Pts',(78.5872532638754,-8.11285925199138,137.409688507001));
#81963=CARTESIAN_POINT('Ctrl Pts',(78.5435757492815,-8.18654959279615,137.414890615171));
#81964=CARTESIAN_POINT('Ctrl Pts',(78.4798579573421,-8.31578365342842,137.423693429284));
#81965=CARTESIAN_POINT('Ctrl Pts',(78.4567655212686,-8.36959947731005,137.427276118832));
#81966=CARTESIAN_POINT('Ctrl Pts',(78.4365593939729,-8.42449198839149,137.430947540156));
#81967=CARTESIAN_POINT('Origin',(80.,-9.,134.));
#81968=CARTESIAN_POINT('',(78.4365594354234,-8.4244918757859,138.13187361233));
#81969=CARTESIAN_POINT('',(78.4365593741136,-8.42449204234183,137.937814844869));
#81970=CARTESIAN_POINT('',(78.4365593749993,-8.42449203993574,134.));
#81971=CARTESIAN_POINT('',(78.3340004536119,-9.00002839986701,137.276979779061));
#81972=CARTESIAN_POINT('Ctrl Pts',(78.4365593741136,-8.42449204234183,137.937814844869));
#81973=CARTESIAN_POINT('Ctrl Pts',(78.4603179885632,-8.35994874185208,137.933371985177));
#81974=CARTESIAN_POINT('Ctrl Pts',(78.4880534421214,-8.29693057726159,137.929060103377));
#81975=CARTESIAN_POINT('Ctrl Pts',(78.5665913610029,-8.14478919144876,137.918489342388));
#81976=CARTESIAN_POINT('Ctrl Pts',(78.6218616409535,-8.05831053718337,137.912339462922));
#81977=CARTESIAN_POINT('Ctrl Pts',(78.7166755345118,-7.93635294388492,137.902733463664));
#81978=CARTESIAN_POINT('Ctrl Pts',(78.7505374150341,-7.89677344010222,137.899441880882));
#81979=CARTESIAN_POINT('Ctrl Pts',(78.7937404515054,-7.8508197125464,137.895310731004));
#81980=CARTESIAN_POINT('Ctrl Pts',(78.8013677090719,-7.84286645257854,137.894583788391));
#81981=CARTESIAN_POINT('Ctrl Pts',(78.8134803043143,-7.83048440224266,137.893431927752));
#81982=CARTESIAN_POINT('Ctrl Pts',(78.8179130004964,-7.82600424022333,137.8930109256));
#81983=CARTESIAN_POINT('Ctrl Pts',(78.8262671466301,-7.81765591769989,137.892218210012));
#81984=CARTESIAN_POINT('Ctrl Pts',(78.8301824886623,-7.81378192280248,137.891846961148));
#81985=CARTESIAN_POINT('Ctrl Pts',(78.8394248594893,-7.80472741262935,137.890971326298));
#81986=CARTESIAN_POINT('Ctrl Pts',(78.8447674106453,-7.79956304867256,137.890465737291));
#81987=CARTESIAN_POINT('Ctrl Pts',(78.8625617832787,-7.78259095855185,137.888784199261));
#81988=CARTESIAN_POINT('Ctrl Pts',(78.8751610216921,-7.77094032418107,137.8875974761));
#81989=CARTESIAN_POINT('Ctrl Pts',(78.9062990152035,-7.74302655077145,137.884678692788));
#81990=CARTESIAN_POINT('Ctrl Pts',(78.9250229469967,-7.72697670799429,137.882935380343));
#81991=CARTESIAN_POINT('Ctrl Pts',(79.0048904208475,-7.66153426535988,137.875570584162));
#81992=CARTESIAN_POINT('Ctrl Pts',(79.0691322943938,-7.61608596866158,137.869821928419));
#81993=CARTESIAN_POINT('Ctrl Pts',(79.2249479352132,-7.52162681719461,137.856577649312));
#81994=CARTESIAN_POINT('Ctrl Pts',(79.3183877378418,-7.47628601570247,137.849147271052));
#81995=CARTESIAN_POINT('Ctrl Pts',(79.4375354997769,-7.43164226868499,137.840388318034));
#81996=CARTESIAN_POINT('Ctrl Pts',(79.4597959223641,-7.42383632174753,137.838779865323));
#81997=CARTESIAN_POINT('Ctrl Pts',(79.4937410107878,-7.41273667170991,137.836368001387));
#81998=CARTESIAN_POINT('Ctrl Pts',(79.5053074587709,-7.40909386177838,137.835553255619));
#81999=CARTESIAN_POINT('Ctrl Pts',(79.5262182966011,-7.40275817842931,137.83409266417));
#82000=CARTESIAN_POINT('Ctrl Pts',(79.5355483429084,-7.40002024883038,137.833445374592));
#82001=CARTESIAN_POINT('Ctrl Pts',(79.5555963550732,-7.39432724622947,137.832063666324));
#82002=CARTESIAN_POINT('Ctrl Pts',(79.5663210545656,-7.39139744679201,137.831330093915));
#82003=CARTESIAN_POINT('Ctrl Pts',(79.5958481947151,-7.38364791967222,137.829325128198));
#82004=CARTESIAN_POINT('Ctrl Pts',(79.6147071648056,-7.37904897929614,137.828060847683));
#82005=CARTESIAN_POINT('Ctrl Pts',(79.6569031637806,-7.3695371529798,137.825265231572));
#82006=CARTESIAN_POINT('Ctrl Pts',(79.6802741680488,-7.36479358733659,137.823739203859));
#82007=CARTESIAN_POINT('Ctrl Pts',(79.755511527174,-7.35119764114957,137.818887863544));
#82008=CARTESIAN_POINT('Ctrl Pts',(79.8076997016165,-7.34429922645207,137.815616521277));
#82009=CARTESIAN_POINT('Ctrl Pts',(79.9557637071104,-7.3318243898085,137.806469789002));
#82010=CARTESIAN_POINT('Ctrl Pts',(80.0519101041761,-7.33204596136709,137.800694915909));
#82011=CARTESIAN_POINT('Ctrl Pts',(80.1988056473655,-7.34510256166756,137.791520640568));
#82012=CARTESIAN_POINT('Ctrl Pts',(80.249868416941,-7.35203948084721,137.788262748334));
#82013=CARTESIAN_POINT('Ctrl Pts',(80.3113335539439,-7.36331180867816,137.784169521228));
#82014=CARTESIAN_POINT('Ctrl Pts',(80.3221247026131,-7.36540143230137,137.78344438159));
#82015=CARTESIAN_POINT('Ctrl Pts',(80.3390632593351,-7.36885569358066,137.782294758058));
#82016=CARTESIAN_POINT('Ctrl Pts',(80.3452251821864,-7.37014871460305,137.781874165202));
#82017=CARTESIAN_POINT('Ctrl Pts',(80.356765152495,-7.37263864444638,137.781081758952));
#82018=CARTESIAN_POINT('Ctrl Pts',(80.3621447715477,-7.3738273411217,137.780710405365));
#82019=CARTESIAN_POINT('Ctrl Pts',(80.374776833488,-7.37668434794355,137.779833896293));
#82020=CARTESIAN_POINT('Ctrl Pts',(80.3820240964597,-7.3783745914791,137.779327530361));
#82021=CARTESIAN_POINT('Ctrl Pts',(80.4060083025106,-7.3841380086455,137.777640697665));
#82022=CARTESIAN_POINT('Ctrl Pts',(80.4226927586246,-7.38842204942205,137.776449366821));
#82023=CARTESIAN_POINT('Ctrl Pts',(80.463216110517,-7.39949970298187,137.773516884167));
#82024=CARTESIAN_POINT('Ctrl Pts',(80.486975183291,-7.4065680418602,137.77176435114));
#82025=CARTESIAN_POINT('Ctrl Pts',(80.586115201697,-7.43848656424449,137.764334432047));
#82026=CARTESIAN_POINT('Ctrl Pts',(80.6598263802082,-7.46817640185108,137.758528000872));
#82027=CARTESIAN_POINT('Ctrl Pts',(80.8233416366015,-7.54803787661784,137.745303092223));
#82028=CARTESIAN_POINT('Ctrl Pts',(80.9112010692431,-7.60149919320195,137.737947919739));
#82029=CARTESIAN_POINT('Ctrl Pts',(81.0125322055783,-7.67678752968935,137.729257556827));
#82030=CARTESIAN_POINT('Ctrl Pts',(81.0311711755371,-7.69126060099015,137.727648481611));
#82031=CARTESIAN_POINT('Ctrl Pts',(81.0589161014918,-7.71376527330377,137.725235878649));
#82032=CARTESIAN_POINT('Ctrl Pts',(81.0682514425024,-7.72150793853002,137.724421005967));
#82033=CARTESIAN_POINT('Ctrl Pts',(81.0849174950513,-7.7356406480849,137.722960277211));
#82034=CARTESIAN_POINT('Ctrl Pts',(81.0922783040723,-7.74199417522227,137.722312976071));
#82035=CARTESIAN_POINT('Ctrl Pts',(81.1079340618461,-7.75574854717508,137.720931339293));
#82036=CARTESIAN_POINT('Ctrl Pts',(81.1162114484187,-7.76316873594401,137.720197849054));
#82037=CARTESIAN_POINT('Ctrl Pts',(81.1387317812083,-7.78376711748497,137.718193357637));
#82038=CARTESIAN_POINT('Ctrl Pts',(81.1528200250781,-7.79711241803091,137.716929463497));
#82039=CARTESIAN_POINT('Ctrl Pts',(81.1836869676044,-7.82739211890354,137.714134830555));
#82040=CARTESIAN_POINT('Ctrl Pts',(81.2003419860459,-7.84444676382978,137.712609393769));
#82041=CARTESIAN_POINT('Ctrl Pts',(81.252544940583,-7.90024931138634,137.707760653262));
#82042=CARTESIAN_POINT('Ctrl Pts',(81.2866278763551,-7.94032564594187,137.704491251537));
#82043=CARTESIAN_POINT('Ctrl Pts',(81.3774118072201,-8.05792514731249,137.695345823314));
#82044=CARTESIAN_POINT('Ctrl Pts',(81.4293852163419,-8.13882357268403,137.689570473641));
#82045=CARTESIAN_POINT('Ctrl Pts',(81.4981227558006,-8.26935530624059,137.680393395951));
#82046=CARTESIAN_POINT('Ctrl Pts',(81.5200097847314,-8.31605366175291,137.677133004696));
#82047=CARTESIAN_POINT('Ctrl Pts',(81.5438938458182,-8.37384614241747,137.673036972318));
#82048=CARTESIAN_POINT('Ctrl Pts',(81.5479919681851,-8.38404731425259,137.672311705972));
#82049=CARTESIAN_POINT('Ctrl Pts',(81.5542779882448,-8.40015370048978,137.671161925215));
#82050=CARTESIAN_POINT('Ctrl Pts',(81.556533957345,-8.40603225328301,137.670741303586));
#82051=CARTESIAN_POINT('Ctrl Pts',(81.5607012813342,-8.41707816568329,137.669948875646));
#82052=CARTESIAN_POINT('Ctrl Pts',(81.5626203935325,-8.42224238935577,137.669577529478));
#82053=CARTESIAN_POINT('Ctrl Pts',(81.5670712308611,-8.43440374223383,137.668701082127));
#82054=CARTESIAN_POINT('Ctrl Pts',(81.5695817285307,-8.44140841255747,137.66819477102));
#82055=CARTESIAN_POINT('Ctrl Pts',(81.577746548073,-8.46467917293505,137.666508312379));
#82056=CARTESIAN_POINT('Ctrl Pts',(81.5831953713264,-8.4810154951532,137.665317307131));
#82057=CARTESIAN_POINT('Ctrl Pts',(81.595864117891,-8.52105570413708,137.662385793131));
#82058=CARTESIAN_POINT('Ctrl Pts',(81.6028101877545,-8.5448414649516,137.660633912303));
#82059=CARTESIAN_POINT('Ctrl Pts',(81.6297523205309,-8.64538199089007,137.653208617));
#82060=CARTESIAN_POINT('Ctrl Pts',(81.6447840326573,-8.72335728513493,137.647406290558));
#82061=CARTESIAN_POINT('Ctrl Pts',(81.6664020641407,-8.90406102835186,137.634180005334));
#82062=CARTESIAN_POINT('Ctrl Pts',(81.6691489967224,-9.00694273567105,137.62681949545));
#82063=CARTESIAN_POINT('Ctrl Pts',(81.6608518938923,-9.13297993938015,137.618124264481));
#82064=CARTESIAN_POINT('Ctrl Pts',(81.6588020245364,-9.15648840202831,137.616515235326));
#82065=CARTESIAN_POINT('Ctrl Pts',(81.6549434666265,-9.19200312790644,137.614102687039));
#82066=CARTESIAN_POINT('Ctrl Pts',(81.6535019114694,-9.20404538983951,137.613287823738));
#82067=CARTESIAN_POINT('Ctrl Pts',(81.6506679019358,-9.22571224857844,137.611827105126));
#82068=CARTESIAN_POINT('Ctrl Pts',(81.6493224483708,-9.23534232474823,137.611179804832));
#82069=CARTESIAN_POINT('Ctrl Pts',(81.6462582981961,-9.25595542774813,137.609798162744));
#82070=CARTESIAN_POINT('Ctrl Pts',(81.6445138226447,-9.26693419147022,137.609064666414));
#82071=CARTESIAN_POINT('Ctrl Pts',(81.6394229160776,-9.29702695786795,137.607060139871));
#82072=CARTESIAN_POINT('Ctrl Pts',(81.6358521712444,-9.31610162342348,137.605796217122));
#82073=CARTESIAN_POINT('Ctrl Pts',(81.6271545213111,-9.35845819491181,137.603001511389));
#82074=CARTESIAN_POINT('Ctrl Pts',(81.6218594988519,-9.3817014077988,137.601476030854));
#82075=CARTESIAN_POINT('Ctrl Pts',(81.6032908287108,-9.45582801295078,137.596627097917));
#82076=CARTESIAN_POINT('Ctrl Pts',(81.5881063444686,-9.50620106787074,137.593357552564));
#82077=CARTESIAN_POINT('Ctrl Pts',(81.5385449689,-9.64625657447896,137.584212032637));
#82078=CARTESIAN_POINT('Ctrl Pts',(81.4987686054243,-9.7337979759346,137.578436722803));
#82079=CARTESIAN_POINT('Ctrl Pts',(81.4263875215395,-9.86234087892624,137.569259853466));
#82080=CARTESIAN_POINT('Ctrl Pts',(81.3990272266733,-9.90605455221021,137.565999642882));
#82081=CARTESIAN_POINT('Ctrl Pts',(81.3634298479079,-9.95746326678215,137.561903813327));
#82082=CARTESIAN_POINT('Ctrl Pts',(81.3570823258384,-9.96643903192347,137.561178556145));
#82083=CARTESIAN_POINT('Ctrl Pts',(81.3469603304609,-9.98045576929294,137.560028786756));
#82084=CARTESIAN_POINT('Ctrl Pts',(81.3432451750532,-9.98553946841378,137.559608167204));
#82085=CARTESIAN_POINT('Ctrl Pts',(81.3362254265296,-9.99503163972663,137.558815740828));
#82086=CARTESIAN_POINT('Ctrl Pts',(81.332927675076,-9.99944492796627,137.558444394122));
#82087=CARTESIAN_POINT('Ctrl Pts',(81.3251245264176,-10.0097803522191,137.557567942302));
#82088=CARTESIAN_POINT('Ctrl Pts',(81.3206012797656,-10.0156887440696,137.557061627227));
#82089=CARTESIAN_POINT('Ctrl Pts',(81.3054789367246,-10.0351701865493,137.555375141507));
#82090=CARTESIAN_POINT('Ctrl Pts',(81.2947093700716,-10.0486086775402,137.554184112689));
#82091=CARTESIAN_POINT('Ctrl Pts',(81.2679408902936,-10.0809698664641,137.551252528568));
#82092=CARTESIAN_POINT('Ctrl Pts',(81.2517246453798,-10.0997068856325,137.549500600528));
#82093=CARTESIAN_POINT('Ctrl Pts',(81.1818668571275,-10.1768763396028,137.542074970595));
#82094=CARTESIAN_POINT('Ctrl Pts',(81.1245069603111,-10.2317996712501,137.536272347099));
#82095=CARTESIAN_POINT('Ctrl Pts',(80.9844168316786,-10.3479697939445,137.523046161468));
#82096=CARTESIAN_POINT('Ctrl Pts',(80.8994764223209,-10.4060752746079,137.515686037849));
#82097=CARTESIAN_POINT('Ctrl Pts',(80.7890927013382,-10.4674622273336,137.506991159206));
#82098=CARTESIAN_POINT('Ctrl Pts',(80.7682306146954,-10.4784906159504,137.505382126755));
#82099=CARTESIAN_POINT('Ctrl Pts',(80.7363006627894,-10.4945114295537,137.502969574557));
#82100=CARTESIAN_POINT('Ctrl Pts',(80.7254016805974,-10.4998318220285,137.502154710589));
#82101=CARTESIAN_POINT('Ctrl Pts',(80.7056615158633,-10.5092025598581,137.500693991258));
#82102=CARTESIAN_POINT('Ctrl Pts',(80.6968412223297,-10.5132953642277,137.500046690908));
#82103=CARTESIAN_POINT('Ctrl Pts',(80.6778615439137,-10.5219012098366,137.498665049212));
#82104=CARTESIAN_POINT('Ctrl Pts',(80.6676917586815,-10.5263902812453,137.497931553325));
#82105=CARTESIAN_POINT('Ctrl Pts',(80.6396486594298,-10.5384349523762,137.495927029322));
#82106=CARTESIAN_POINT('Ctrl Pts',(80.6216867308017,-10.5457807638806,137.494663108639));
#82107=CARTESIAN_POINT('Ctrl Pts',(80.5813842192337,-10.5614469254257,137.491868408161));
#82108=CARTESIAN_POINT('Ctrl Pts',(80.5589849603961,-10.5696050491619,137.490342930784));
#82109=CARTESIAN_POINT('Ctrl Pts',(80.4866376839961,-10.5942096490248,137.485494011733));
#82110=CARTESIAN_POINT('Ctrl Pts',(80.4360820215044,-10.6087739849591,137.482224476744));
#82111=CARTESIAN_POINT('Ctrl Pts',(80.2915357794526,-10.6430992302992,137.473078963344));
#82112=CARTESIAN_POINT('Ctrl Pts',(80.196415390744,-10.6571625769103,137.467303650553));
#82113=CARTESIAN_POINT('Ctrl Pts',(80.0491639078534,-10.6660720528888,137.458126766072));
#82114=CARTESIAN_POINT('Ctrl Pts',(79.9975987042039,-10.6667952149265,137.454866542431));
#82115=CARTESIAN_POINT('Ctrl Pts',(79.9351009996958,-10.6647717493359,137.450770698221));
#82116=CARTESIAN_POINT('Ctrl Pts',(79.9241173812591,-10.664307264277,137.45004544038));
#82117=CARTESIAN_POINT('Ctrl Pts',(79.906851473015,-10.6634058432398,137.448895670176));
#82118=CARTESIAN_POINT('Ctrl Pts',(79.9005654597846,-10.6630419165931,137.448475050478));
#82119=CARTESIAN_POINT('Ctrl Pts',(79.8887833975199,-10.6622927605834,137.447682623994));
#82120=CARTESIAN_POINT('Ctrl Pts',(79.8832870131459,-10.6619158912876,137.447311277329));
#82121=CARTESIAN_POINT('Ctrl Pts',(79.8703716118011,-10.6609659391908,137.446434825838));
#82122=CARTESIAN_POINT('Ctrl Pts',(79.8629544605581,-10.6603704059653,137.445928511053));
#82123=CARTESIAN_POINT('Ctrl Pts',(79.8383854234812,-10.6582319792987,137.44424202731));
#82124=CARTESIAN_POINT('Ctrl Pts',(79.821254125865,-10.6564728863473,137.443051000212));
#82125=CARTESIAN_POINT('Ctrl Pts',(79.7795477949342,-10.6515358840836,137.440119421209));
#82126=CARTESIAN_POINT('Ctrl Pts',(79.7550108798058,-10.6480746799821,137.438367496614));
#82127=CARTESIAN_POINT('Ctrl Pts',(79.6522891087164,-10.6312401040158,137.430941891097));
#82128=CARTESIAN_POINT('Ctrl Pts',(79.5750355964759,-10.6128395902213,137.425139289275));
#82129=CARTESIAN_POINT('Ctrl Pts',(79.4015811272432,-10.5581934577351,137.411922708001));
#82130=CARTESIAN_POINT('Ctrl Pts',(79.3068124572052,-10.518410171439,137.404571830552));
#82131=CARTESIAN_POINT('Ctrl Pts',(79.1953997011355,-10.4590184686371,137.395879527354));
#82132=CARTESIAN_POINT('Ctrl Pts',(79.1747461828208,-10.4474366203254,137.394264815647));
#82133=CARTESIAN_POINT('Ctrl Pts',(79.1438820408187,-10.4292534857213,137.391845522519));
#82134=CARTESIAN_POINT('Ctrl Pts',(79.1334859648963,-10.4229746754583,137.39102950185));
#82135=CARTESIAN_POINT('Ctrl Pts',(79.1148905226113,-10.4114644099205,137.389567530062));
#82136=CARTESIAN_POINT('Ctrl Pts',(79.1066666384071,-10.4062738280228,137.38892012328));
#82137=CARTESIAN_POINT('Ctrl Pts',(79.0908010631536,-10.3960647763414,137.387669267592));
#82138=CARTESIAN_POINT('Ctrl Pts',(79.0831543226182,-10.3910548429111,137.387065533458));
#82139=CARTESIAN_POINT('Ctrl Pts',(79.0613036065022,-10.3764804020417,137.385337548237));
#82140=CARTESIAN_POINT('Ctrl Pts',(79.0472050647388,-10.3667593289274,137.384219186112));
#82141=CARTESIAN_POINT('Ctrl Pts',(78.980107724224,-10.3189521951582,137.378875766461));
#82142=CARTESIAN_POINT('Ctrl Pts',(78.9292244362571,-10.2779891673023,137.37476267311));
#82143=CARTESIAN_POINT('Ctrl Pts',(78.826413713766,-10.1847596594816,137.366159287972));
#82144=CARTESIAN_POINT('Ctrl Pts',(78.7752833995031,-10.1318258832438,137.361697107771));
#82145=CARTESIAN_POINT('Ctrl Pts',(78.715730127043,-10.0613940305427,137.356054411611));
#82146=CARTESIAN_POINT('Ctrl Pts',(78.7038858188533,-10.0468975155575,137.354907107612));
#82147=CARTESIAN_POINT('Ctrl Pts',(78.6490957049875,-9.97748331239432,137.349464333658));
#82148=CARTESIAN_POINT('Ctrl Pts',(78.6093854884828,-9.92011134664481,137.345114753188));
#82149=CARTESIAN_POINT('Ctrl Pts',(78.5674186914343,-9.85052951658297,137.339799249718));
#82150=CARTESIAN_POINT('Ctrl Pts',(78.5615510988413,-9.84056790604222,137.339037310898));
#82151=CARTESIAN_POINT('Ctrl Pts',(78.5525852761224,-9.8249775063575,137.337842065));
#82152=CARTESIAN_POINT('Ctrl Pts',(78.5494149980306,-9.81939027178488,137.33741316926));
#82153=CARTESIAN_POINT('Ctrl Pts',(78.5436229714813,-9.80904355662836,137.336617645717));
#82154=CARTESIAN_POINT('Ctrl Pts',(78.5409920968417,-9.80428941378284,137.336251601543));
#82155=CARTESIAN_POINT('Ctrl Pts',(78.5349285236896,-9.79320453248398,137.335396977686));
#82156=CARTESIAN_POINT('Ctrl Pts',(78.5315135841764,-9.78686434839327,137.334907320027));
#82157=CARTESIAN_POINT('Ctrl Pts',(78.5207105767518,-9.76649219355298,137.333331755857));
#82158=CARTESIAN_POINT('Ctrl Pts',(78.5134819663801,-9.75237727932634,137.332236796082));
#82159=CARTESIAN_POINT('Ctrl Pts',(78.4744668556548,-9.67343691879679,137.326103326881));
#82160=CARTESIAN_POINT('Ctrl Pts',(78.4467217555122,-9.60670693680316,137.32088590796));
#82161=CARTESIAN_POINT('Ctrl Pts',(78.3781212857171,-9.40582138687903,137.305451728632));
#82162=CARTESIAN_POINT('Ctrl Pts',(78.349741350932,-9.26803599819419,137.295262893656));
#82163=CARTESIAN_POINT('Ctrl Pts',(78.3373025807438,-9.10700372058145,137.284174400434));
#82164=CARTESIAN_POINT('Ctrl Pts',(78.3360669770646,-9.0856707241575,137.282720088802));
#82165=CARTESIAN_POINT('Ctrl Pts',(78.3347977443621,-9.05281937188488,137.280502099517));
#82166=CARTESIAN_POINT('Ctrl Pts',(78.3344726056708,-9.04131523314185,137.279729438107));
#82167=CARTESIAN_POINT('Ctrl Pts',(78.3341612568167,-9.02391663867215,137.278566770269));
#82168=CARTESIAN_POINT('Ctrl Pts',(78.3340870821118,-9.01802430146893,137.278174032471));
#82169=CARTESIAN_POINT('Ctrl Pts',(78.3340147926115,-9.00809726575708,137.277514048675));
#82170=CARTESIAN_POINT('Ctrl Pts',(78.3340000686888,-9.00406278471672,137.277246288591));
#82171=CARTESIAN_POINT('Ctrl Pts',(78.3340000002398,-9.00002826508004,137.276978983378));
#82172=CARTESIAN_POINT('Ctrl Pts',(78.334000000243,-9.0000284517738,137.276978995747));
#82173=CARTESIAN_POINT('Ctrl Pts',(78.3339998559323,-8.99157830878331,137.276419135442));
#82174=CARTESIAN_POINT('Ctrl Pts',(78.3340640017322,-8.98312812680701,137.275861279928));
#82175=CARTESIAN_POINT('Ctrl Pts',(78.3344125114647,-8.9602008431423,137.274352894817));
#82176=CARTESIAN_POINT('Ctrl Pts',(78.3348213222679,-8.94572617903658,137.273406244807));
#82177=CARTESIAN_POINT('Ctrl Pts',(78.337191248607,-8.88833837798755,137.269673328737));
#82178=CARTESIAN_POINT('Ctrl Pts',(78.340623104397,-8.84550060921749,137.266932401451));
#82179=CARTESIAN_POINT('Ctrl Pts',(78.3611175763466,-8.67353914507015,137.256037782249));
#82180=CARTESIAN_POINT('Ctrl Pts',(78.3916241621003,-8.54656426521876,137.248277246748));
#82181=CARTESIAN_POINT('Ctrl Pts',(78.4365593749625,-8.42449204003557,137.240217161908));
#82182=CARTESIAN_POINT('',(78.3340007164175,-8.99846998957594,137.471592638051));
#82183=CARTESIAN_POINT('Ctrl Pts',(78.4365593939729,-8.42449198839149,137.430947540156));
#82184=CARTESIAN_POINT('Ctrl Pts',(78.4253966868889,-8.45481689990651,137.432975786351));
#82185=CARTESIAN_POINT('Ctrl Pts',(78.4151148644401,-8.48547039210586,137.435031381114));
#82186=CARTESIAN_POINT('Ctrl Pts',(78.4011804947077,-8.53140879447188,137.438146593564));
#82187=CARTESIAN_POINT('Ctrl Pts',(78.396844163587,-8.54646626464699,137.439173120898));
#82188=CARTESIAN_POINT('Ctrl Pts',(78.3908552708693,-8.56842207113429,137.440680830275));
#82189=CARTESIAN_POINT('Ctrl Pts',(78.3890332220193,-8.57527384863215,137.441152873332));
#82190=CARTESIAN_POINT('Ctrl Pts',(78.3858798945934,-8.58744413339833,137.441994379246));
#82191=CARTESIAN_POINT('Ctrl Pts',(78.3845310535768,-8.5927578857862,137.442362835515));
#82192=CARTESIAN_POINT('Ctrl Pts',(78.3816559318007,-8.60432350412263,137.443167149854));
#82193=CARTESIAN_POINT('Ctrl Pts',(78.3801396609965,-8.61057749026454,137.443603532063));
#82194=CARTESIAN_POINT('Ctrl Pts',(78.3770706379162,-8.6235640505564,137.444512487288));
#82195=CARTESIAN_POINT('Ctrl Pts',(78.375523461572,-8.63029780852984,137.444985348976));
#82196=CARTESIAN_POINT('Ctrl Pts',(78.3716235762703,-8.64776848626763,137.446215862591));
#82197=CARTESIAN_POINT('Ctrl Pts',(78.369335201114,-8.65851923128557,137.446976657879));
#82198=CARTESIAN_POINT('Ctrl Pts',(78.3452056092581,-8.77765714383894,137.455441551978));
#82199=CARTESIAN_POINT('Ctrl Pts',(78.3341022436752,-8.88792624741543,137.463565331214));
#82200=CARTESIAN_POINT('Ctrl Pts',(78.3340007028461,-8.99846967886182,137.471592635464));
#82201=CARTESIAN_POINT('Ctrl Pts',(78.3340007025621,-8.99846998812028,137.471592657922));
#82202=CARTESIAN_POINT('Ctrl Pts',(78.333928799091,-9.07676423789923,137.477278131424));
#82203=CARTESIAN_POINT('Ctrl Pts',(78.3393761194856,-9.15497390237208,137.48290344457));
#82204=CARTESIAN_POINT('Ctrl Pts',(78.3549267449954,-9.26530406909678,137.49069054483));
#82205=CARTESIAN_POINT('Ctrl Pts',(78.3605243789937,-9.29794666877342,137.492976680033));
#82206=CARTESIAN_POINT('Ctrl Pts',(78.3695335593229,-9.34247161202522,137.496071652893));
#82207=CARTESIAN_POINT('Ctrl Pts',(78.3721093407894,-9.35451323671659,137.496906339278));
#82208=CARTESIAN_POINT('Ctrl Pts',(78.3769092493717,-9.37579613030707,137.49837769819));
#82209=CARTESIAN_POINT('Ctrl Pts',(78.3790793717241,-9.38504887956074,137.499016058276));
#82210=CARTESIAN_POINT('Ctrl Pts',(78.3836412988074,-9.4037772197593,137.500305658421));
#82211=CARTESIAN_POINT('Ctrl Pts',(78.3860375411522,-9.41325135515755,137.500956727615));
#82212=CARTESIAN_POINT('Ctrl Pts',(78.3912590264513,-9.43315732682523,137.50232217255));
#82213=CARTESIAN_POINT('Ctrl Pts',(78.3941027030309,-9.44358389355644,137.503035920355));
#82214=CARTESIAN_POINT('Ctrl Pts',(78.4019431644165,-9.47126754270717,137.504927593944));
#82215=CARTESIAN_POINT('Ctrl Pts',(78.4071180554961,-9.48847302714551,137.506099721521));
#82216=CARTESIAN_POINT('Ctrl Pts',(78.4340621327363,-9.57307053966714,137.511850440935));
#82217=CARTESIAN_POINT('Ctrl Pts',(78.4598359086686,-9.63911470235923,137.516296272916));
#82218=CARTESIAN_POINT('Ctrl Pts',(78.5347471334781,-9.79997299598436,137.527257932845));
#82219=CARTESIAN_POINT('Ctrl Pts',(78.5889268678075,-9.89207260534004,137.533650556547));
#82220=CARTESIAN_POINT('Ctrl Pts',(78.672937597443,-10.0078641137908,137.542564276164));
#82221=CARTESIAN_POINT('Ctrl Pts',(78.6953047169174,-10.0366554612219,137.544863923682));
#82222=CARTESIAN_POINT('Ctrl Pts',(78.7308642089458,-10.0794530321035,137.548451471454));
#82223=CARTESIAN_POINT('Ctrl Pts',(78.7433857141227,-10.0940040971263,137.549702827015));
#82224=CARTESIAN_POINT('Ctrl Pts',(78.7614188355533,-10.1142420296484,137.551493914495));
#82225=CARTESIAN_POINT('Ctrl Pts',(78.7667243878721,-10.1201115390208,137.552019566283));
#82226=CARTESIAN_POINT('Ctrl Pts',(78.775842217388,-10.1300552436493,137.552921171226));
#82227=CARTESIAN_POINT('Ctrl Pts',(78.7796336043926,-10.1341485749341,137.553295575405));
#82228=CARTESIAN_POINT('Ctrl Pts',(78.787592956522,-10.142655684411,137.554080695178));
#82229=CARTESIAN_POINT('Ctrl Pts',(78.7917645480015,-10.1470657966119,137.554491667892));
#82230=CARTESIAN_POINT('Ctrl Pts',(78.8030469045565,-10.1588634199501,137.555601545504));
#82231=CARTESIAN_POINT('Ctrl Pts',(78.8102017874062,-10.1662081027249,137.556303675397));
#82232=CARTESIAN_POINT('Ctrl Pts',(78.8442657579952,-10.2005359431904,137.559636446087));
#82233=CARTESIAN_POINT('Ctrl Pts',(78.8720256879978,-10.2266546519448,137.562323142642));
#82234=CARTESIAN_POINT('Ctrl Pts',(78.971029704128,-10.3136014398985,137.571736541764));
#82235=CARTESIAN_POINT('Ctrl Pts',(79.0464903694629,-10.3693602933498,137.578615294642));
#82236=CARTESIAN_POINT('Ctrl Pts',(79.2073280405334,-10.4684339838284,137.592289005479));
#82237=CARTESIAN_POINT('Ctrl Pts',(79.2925659184523,-10.5113470108072,137.599053773995));
#82238=CARTESIAN_POINT('Ctrl Pts',(79.3982889066405,-10.5536556263566,137.606836743984));
#82239=CARTESIAN_POINT('Ctrl Pts',(79.415674729862,-10.5602775626645,137.608098534098));
#82240=CARTESIAN_POINT('Ctrl Pts',(79.4434589669027,-10.5703304863871,137.610087200981));
#82241=CARTESIAN_POINT('Ctrl Pts',(79.4537861306055,-10.5739524061321,137.6108203581));
#82242=CARTESIAN_POINT('Ctrl Pts',(79.4733751346673,-10.5806065943856,137.612199981537));
#82243=CARTESIAN_POINT('Ctrl Pts',(79.4826293032467,-10.5836598511153,137.61284711601));
#82244=CARTESIAN_POINT('Ctrl Pts',(79.5037063460114,-10.5904093923997,137.614310821788));
#82245=CARTESIAN_POINT('Ctrl Pts',(79.5155448122557,-10.5940553978139,137.615125719673));
#82246=CARTESIAN_POINT('Ctrl Pts',(79.546509046066,-10.6032149271836,137.617239131014));
#82247=CARTESIAN_POINT('Ctrl Pts',(79.5656952382616,-10.6085184413274,137.618530862869));
#82248=CARTESIAN_POINT('Ctrl Pts',(79.7142085101317,-10.6467198437046,137.628405089555));
#82249=CARTESIAN_POINT('Ctrl Pts',(79.8469694289449,-10.6643162175775,137.636458087175));
#82250=CARTESIAN_POINT('Ctrl Pts',(80.0639419874605,-10.6668667430825,137.649743502432));
#82251=CARTESIAN_POINT('Ctrl Pts',(80.1474113668569,-10.6615653646854,137.654899393087));
#82252=CARTESIAN_POINT('Ctrl Pts',(80.2425442890156,-10.6482978077173,137.66117112114));
#82253=CARTESIAN_POINT('Ctrl Pts',(80.2549493250267,-10.646424675946,137.661996836986));
#82254=CARTESIAN_POINT('Ctrl Pts',(80.2738062985884,-10.6433591028779,137.66326569746));
#82255=CARTESIAN_POINT('Ctrl Pts',(80.2802746228279,-10.6422682979004,137.663703403915));
#82256=CARTESIAN_POINT('Ctrl Pts',(80.2921235769085,-10.6401980751279,137.664510012672));
#82257=CARTESIAN_POINT('Ctrl Pts',(80.2975060326865,-10.6392303277792,137.664878262565));
#82258=CARTESIAN_POINT('Ctrl Pts',(80.3098063428566,-10.6369561973641,137.665724009077));
#82259=CARTESIAN_POINT('Ctrl Pts',(80.3167207214058,-10.6356324594103,137.666202448748));
#82260=CARTESIAN_POINT('Ctrl Pts',(80.3383281723918,-10.6313536304051,137.66770659632));
#82261=CARTESIAN_POINT('Ctrl Pts',(80.352989417361,-10.6282441622426,137.668740284237));
#82262=CARTESIAN_POINT('Ctrl Pts',(80.4699427903108,-10.601786055276,137.677080485071));
#82263=CARTESIAN_POINT('Ctrl Pts',(80.5698548258405,-10.5690209530326,137.68476954026));
#82264=CARTESIAN_POINT('Ctrl Pts',(80.7694879020487,-10.4819540977734,137.700604123405));
#82265=CARTESIAN_POINT('Ctrl Pts',(80.8681249163085,-10.426417731538,137.708691301777));
#82266=CARTESIAN_POINT('Ctrl Pts',(80.9762107936308,-10.3501640350449,137.717741998127));
#82267=CARTESIAN_POINT('Ctrl Pts',(80.9918273040628,-10.3387341367218,137.719055607483));
#82268=CARTESIAN_POINT('Ctrl Pts',(81.0160854915727,-10.3203217579863,137.721106418013));
#82269=CARTESIAN_POINT('Ctrl Pts',(81.0248621149918,-10.313520813076,137.721850589115));
#82270=CARTESIAN_POINT('Ctrl Pts',(81.0411949528946,-10.3006012385433,137.7232398614));
#82271=CARTESIAN_POINT('Ctrl Pts',(81.0487668203291,-10.294503254171,137.723885741696));
#82272=CARTESIAN_POINT('Ctrl Pts',(81.0656721227355,-10.2806429158128,137.725332148854));
#82273=CARTESIAN_POINT('Ctrl Pts',(81.0749750347802,-10.2728440747457,137.726131160526));
#82274=CARTESIAN_POINT('Ctrl Pts',(81.1021548697266,-10.2495480551742,137.728475521489));
#82275=CARTESIAN_POINT('Ctrl Pts',(81.1197883473678,-10.2337705809647,137.73000933995));
#82276=CARTESIAN_POINT('Ctrl Pts',(81.2076057492842,-10.1517620098186,137.737727760093));
#82277=CARTESIAN_POINT('Ctrl Pts',(81.2722792657677,-10.079896229531,137.743664699698));
#82278=CARTESIAN_POINT('Ctrl Pts',(81.3809915161687,-9.9356762384391,137.754701511532));
#82279=CARTESIAN_POINT('Ctrl Pts',(81.426449643025,-9.86479308503417,137.759799131248));
#82280=CARTESIAN_POINT('Ctrl Pts',(81.4784810001691,-9.76831115862205,137.766702765309));
#82281=CARTESIAN_POINT('Ctrl Pts',(81.490083118573,-9.7455603688608,137.768328752891));
#82282=CARTESIAN_POINT('Ctrl Pts',(81.5087939315282,-9.7066872858138,137.77111878787));
#82283=CARTESIAN_POINT('Ctrl Pts',(81.5161783075457,-9.69070205376934,137.772269385));
#82284=CARTESIAN_POINT('Ctrl Pts',(81.5263467600307,-9.66774089378601,137.773930977843));
#82285=CARTESIAN_POINT('Ctrl Pts',(81.5293394500616,-9.66085790772632,137.774430191044));
#82286=CARTESIAN_POINT('Ctrl Pts',(81.5344508870818,-9.64888127413629,137.775301181211));
#82287=CARTESIAN_POINT('Ctrl Pts',(81.5365910089567,-9.64379694239568,137.775671670876));
#82288=CARTESIAN_POINT('Ctrl Pts',(81.5411051628852,-9.6329218301072,137.776465826167));
#82289=CARTESIAN_POINT('Ctrl Pts',(81.5434717912701,-9.62712836996598,137.776889885529));
#82290=CARTESIAN_POINT('Ctrl Pts',(81.5498442235546,-9.61127419997591,137.778052783553));
#82291=CARTESIAN_POINT('Ctrl Pts',(81.5537845831316,-9.60118775654959,137.778795281941));
#82292=CARTESIAN_POINT('Ctrl Pts',(81.5747287407027,-9.54599378242774,137.782870021529));
#82293=CARTESIAN_POINT('Ctrl Pts',(81.5898654126192,-9.50020682099157,137.786292169078));
#82294=CARTESIAN_POINT('Ctrl Pts',(81.630423819106,-9.35694952861181,137.797001885396));
#82295=CARTESIAN_POINT('Ctrl Pts',(81.6490137744856,-9.25777810040102,137.804405290629));
#82296=CARTESIAN_POINT('Ctrl Pts',(81.6634452195096,-9.1058401491153,137.815375771247));
#82297=CARTESIAN_POINT('Ctrl Pts',(81.6659361032245,-9.05394345424891,137.819061643048));
#82298=CARTESIAN_POINT('Ctrl Pts',(81.666027321704,-8.97836960669219,137.824327029546));
#82299=CARTESIAN_POINT('Ctrl Pts',(81.6655526361715,-8.95472944170512,137.825959785858));
#82300=CARTESIAN_POINT('Ctrl Pts',(81.6637776570495,-8.91184327006092,137.828896368364));
#82301=CARTESIAN_POINT('Ctrl Pts',(81.6626460493423,-8.89259483289745,137.830205073067));
#82302=CARTESIAN_POINT('Ctrl Pts',(81.6603377686136,-8.8623140109963,137.832250007524));
#82303=CARTESIAN_POINT('Ctrl Pts',(81.659384642876,-8.85126683379036,137.832993140685));
#82304=CARTESIAN_POINT('Ctrl Pts',(81.6573887946023,-8.83055110062724,137.834381479127));
#82305=CARTESIAN_POINT('Ctrl Pts',(81.6563715768038,-8.82088061975106,137.835027453212));
#82306=CARTESIAN_POINT('Ctrl Pts',(81.6538917617682,-8.79913705486678,137.836475370358));
#82307=CARTESIAN_POINT('Ctrl Pts',(81.6523815114681,-8.78706987996542,137.837275784262));
#82308=CARTESIAN_POINT('Ctrl Pts',(81.6475300510807,-8.75147339223351,137.839628415047));
#82309=CARTESIAN_POINT('Ctrl Pts',(81.6438172994119,-8.72799720293559,137.841168975842));
#82310=CARTESIAN_POINT('Ctrl Pts',(81.6221296287628,-8.60761778319821,137.849025220927));
#82311=CARTESIAN_POINT('Ctrl Pts',(81.596083933701,-8.51236537276604,137.855081390981));
#82312=CARTESIAN_POINT('Ctrl Pts',(81.5330995677683,-8.34277745190497,137.86613379942));
#82313=CARTESIAN_POINT('Ctrl Pts',(81.4987514403605,-8.26782650995303,137.871129874108));
#82314=CARTESIAN_POINT('Ctrl Pts',(81.4468114002514,-8.17360362600286,137.877908668892));
#82315=CARTESIAN_POINT('Ctrl Pts',(81.4341147571109,-8.15176128260955,137.879517827212));
#82316=CARTESIAN_POINT('Ctrl Pts',(81.4118071508072,-8.11531829323692,137.88228179177));
#82317=CARTESIAN_POINT('Ctrl Pts',(81.4024538216986,-8.10056441459199,137.883423474044));
#82318=CARTESIAN_POINT('Ctrl Pts',(81.3887657623159,-8.07970567877433,137.885074416134));
#82319=CARTESIAN_POINT('Ctrl Pts',(81.3846188239005,-8.07347817757043,137.885572098233));
#82320=CARTESIAN_POINT('Ctrl Pts',(81.3773434370146,-8.06271058116893,137.88644135031));
#82321=CARTESIAN_POINT('Ctrl Pts',(81.3742341711195,-8.05815774139058,137.886811648553));
#82322=CARTESIAN_POINT('Ctrl Pts',(81.3675400249508,-8.04845935182042,137.887606486348));
#82323=CARTESIAN_POINT('Ctrl Pts',(81.3639487349722,-8.04331866847154,137.888031429168));
#82324=CARTESIAN_POINT('Ctrl Pts',(81.3540446631058,-8.02931079687984,137.889199068998));
#82325=CARTESIAN_POINT('Ctrl Pts',(81.3476739977762,-8.02048519215416,137.889945473316));
#82326=CARTESIAN_POINT('Ctrl Pts',(81.3119591728061,-7.97201563722908,137.894101656577));
#82327=CARTESIAN_POINT('Ctrl Pts',(81.2809547211809,-7.93363104604614,137.897605550045));
#82328=CARTESIAN_POINT('Ctrl Pts',(81.1805132342218,-7.81999125222122,137.908521974782));
#82329=CARTESIAN_POINT('Ctrl Pts',(81.1058056445215,-7.74970903512104,137.916048330052));
#82330=CARTESIAN_POINT('Ctrl Pts',(80.9655955866681,-7.64026376568088,137.928816752154));
#82331=CARTESIAN_POINT('Ctrl Pts',(80.9029777016017,-7.59789741857565,137.934129787077));
#82332=CARTESIAN_POINT('Ctrl Pts',(80.8223309766096,-7.55098530545667,137.940498399085));
#82333=CARTESIAN_POINT('Ctrl Pts',(80.8068270766963,-7.54229566410665,137.941702676221));
#82334=CARTESIAN_POINT('Ctrl Pts',(80.7817126420186,-7.52874297347771,137.943622239956));
#82335=CARTESIAN_POINT('Ctrl Pts',(80.7721891980258,-7.52372233484165,137.944343075639));
#82336=CARTESIAN_POINT('Ctrl Pts',(80.7539203346258,-7.51431637884403,137.945712700113));
#82337=CARTESIAN_POINT('Ctrl Pts',(80.7451836834685,-7.50991511047496,137.946362027887));
#82338=CARTESIAN_POINT('Ctrl Pts',(80.7251958640092,-7.50006559668248,137.947835011013));
#82339=CARTESIAN_POINT('Ctrl Pts',(80.7139210395036,-7.49466647584213,137.948656934899));
#82340=CARTESIAN_POINT('Ctrl Pts',(80.6837599198264,-7.48063846516974,137.950832754035));
#82341=CARTESIAN_POINT('Ctrl Pts',(80.664770911554,-7.47223470462493,137.952178983401));
#82342=CARTESIAN_POINT('Ctrl Pts',(80.5308887424507,-7.41595293988394,137.961518941402));
#82343=CARTESIAN_POINT('Ctrl Pts',(80.4111035743345,-7.38072680830335,137.969064414489));
#82344=CARTESIAN_POINT('Ctrl Pts',(80.1983317311004,-7.34331578888048,137.982271404312));
#82345=CARTESIAN_POINT('Ctrl Pts',(80.1070201845569,-7.33492342684084,137.987893836029));
#82346=CARTESIAN_POINT('Ctrl Pts',(80.0033286260467,-7.33395888718647,137.994670080333));
#82347=CARTESIAN_POINT('Ctrl Pts',(79.9911603387355,-7.33397901919427,137.99547145766));
#82348=CARTESIAN_POINT('Ctrl Pts',(79.9725128395491,-7.33421415974513,137.996710511161));
#82349=CARTESIAN_POINT('Ctrl Pts',(79.9660325437043,-7.33433370150281,137.997143132654));
#82350=CARTESIAN_POINT('Ctrl Pts',(79.9540782141347,-7.33462401144572,137.997945218567));
#82351=CARTESIAN_POINT('Ctrl Pts',(79.948604125208,-7.33478396156473,137.998314086096));
#82352=CARTESIAN_POINT('Ctrl Pts',(79.9361091842425,-7.33521072614168,137.999159617112));
#82353=CARTESIAN_POINT('Ctrl Pts',(79.9290891657766,-7.33549496492269,137.999637210981));
#82354=CARTESIAN_POINT('Ctrl Pts',(79.9073131556326,-7.33651467401116,138.001126184783));
#82355=CARTESIAN_POINT('Ctrl Pts',(79.8925654632131,-7.3374020137617,138.002145250694));
#82356=CARTESIAN_POINT('Ctrl Pts',(79.7725952931103,-7.34622317902403,138.010511833729));
#82357=CARTESIAN_POINT('Ctrl Pts',(79.6683405938783,-7.36394096014155,138.018246555101));
#82358=CARTESIAN_POINT('Ctrl Pts',(79.4580716482882,-7.42060974519864,138.034078191174));
#82359=CARTESIAN_POINT('Ctrl Pts',(79.3528848377405,-7.460711014358,138.042119080553));
#82360=CARTESIAN_POINT('Ctrl Pts',(79.2351910414667,-7.51979760909405,138.051130306956));
#82361=CARTESIAN_POINT('Ctrl Pts',(79.2180173470157,-7.52879809454356,138.052446467466));
#82362=CARTESIAN_POINT('Ctrl Pts',(79.1912545939545,-7.54342514353333,138.054500334068));
#82363=CARTESIAN_POINT('Ctrl Pts',(79.1815585142408,-7.54885114856061,138.055245044792));
#82364=CARTESIAN_POINT('Ctrl Pts',(79.16348225366,-7.5592055821618,138.056634804679));
#82365=CARTESIAN_POINT('Ctrl Pts',(79.155089574531,-7.56411112052619,138.057280638303));
#82366=CARTESIAN_POINT('Ctrl Pts',(79.1363239101879,-7.57530119325411,138.058726270384));
#82367=CARTESIAN_POINT('Ctrl Pts',(79.1259755728194,-7.58162614528763,138.059524560838));
#82368=CARTESIAN_POINT('Ctrl Pts',(79.0956931542708,-7.6005921803549,138.061864673503));
#82369=CARTESIAN_POINT('Ctrl Pts',(79.0759570725515,-7.61354485292491,138.063395028967));
#82370=CARTESIAN_POINT('Ctrl Pts',(78.972722802962,-7.68448087179511,138.071441705272));
#82371=CARTESIAN_POINT('Ctrl Pts',(78.8943842881878,-7.74959758800389,138.077679052033));
#82372=CARTESIAN_POINT('Ctrl Pts',(78.7657869538816,-7.87808503629385,138.088782369142));
#82373=CARTESIAN_POINT('Ctrl Pts',(78.7132728669344,-7.93872410145422,138.093649710774));
#82374=CARTESIAN_POINT('Ctrl Pts',(78.6504216108429,-8.02285388397609,138.100269843259));
#82375=CARTESIAN_POINT('Ctrl Pts',(78.635964887324,-8.04313823348432,138.101857140033));
#82376=CARTESIAN_POINT('Ctrl Pts',(78.6122543102871,-8.07803648285834,138.104587190866));
#82377=CARTESIAN_POINT('Ctrl Pts',(78.6027631538214,-8.09248473037824,138.105717238794));
#82378=CARTESIAN_POINT('Ctrl Pts',(78.5895054421188,-8.11336782102481,138.107354271195));
#82379=CARTESIAN_POINT('Ctrl Pts',(78.5855542415546,-8.11968488041981,138.107849942608));
#82380=CARTESIAN_POINT('Ctrl Pts',(78.5787554361119,-8.13071854765846,138.108716919122));
#82381=CARTESIAN_POINT('Ctrl Pts',(78.5758886399612,-8.13542311678905,138.109086972922));
#82382=CARTESIAN_POINT('Ctrl Pts',(78.5697998012233,-8.14552768918537,138.109882738041));
#82383=CARTESIAN_POINT('Ctrl Pts',(78.5665850315755,-8.15093164966051,138.11030886536));
#82384=CARTESIAN_POINT('Ctrl Pts',(78.5578510209819,-8.16580431479997,138.111482871798));
#82385=CARTESIAN_POINT('Ctrl Pts',(78.5523946208913,-8.17530928871096,138.11223452253));
#82386=CARTESIAN_POINT('Ctrl Pts',(78.5221398794056,-8.22923810541439,138.116503867796));
#82387=CARTESIAN_POINT('Ctrl Pts',(78.4992951965933,-8.27472179707336,138.120121681014));
#82388=CARTESIAN_POINT('Ctrl Pts',(78.4634101512892,-8.35514979643572,138.126466083823));
#82389=CARTESIAN_POINT('Ctrl Pts',(78.4494000929481,-8.38960860654049,138.129168419324));
#82390=CARTESIAN_POINT('Ctrl Pts',(78.4365594354234,-8.42449187578589,138.13187361233));
#82391=CARTESIAN_POINT('Origin',(80.,-9.,134.));
#82392=CARTESIAN_POINT('',(78.4365593750041,-8.42449203992252,138.833737849951));
#82393=CARTESIAN_POINT('',(78.436559345854,-8.42449211911253,138.638847691527));
#82394=CARTESIAN_POINT('',(78.4365593749993,-8.42449203993574,134.));
#82395=CARTESIAN_POINT('Ctrl Pts',(78.436559345854,-8.42449211911253,138.638847691527));
#82396=CARTESIAN_POINT('Ctrl Pts',(78.4434608386264,-8.40574333263555,138.63740036079));
#82397=CARTESIAN_POINT('Ctrl Pts',(78.4507011944744,-8.38711431632311,138.635956897866));
#82398=CARTESIAN_POINT('Ctrl Pts',(78.478217800435,-8.31992405170581,138.630735319541));
#82399=CARTESIAN_POINT('Ctrl Pts',(78.5004548885466,-8.27220215182169,138.626998446861));
#82400=CARTESIAN_POINT('Ctrl Pts',(78.5359994117821,-8.20449582377853,138.621668964208));
#82401=CARTESIAN_POINT('Ctrl Pts',(78.5475358445659,-8.18362227306315,138.620021657096));
#82402=CARTESIAN_POINT('Ctrl Pts',(78.5692688525915,-8.14621949086728,138.617061556459));
#82403=CARTESIAN_POINT('Ctrl Pts',(78.5793136655477,-8.12960746307735,138.615743765781));
#82404=CARTESIAN_POINT('Ctrl Pts',(78.5955648023106,-8.10376265788315,138.613687817337));
#82405=CARTESIAN_POINT('Ctrl Pts',(78.6015768985399,-8.09441044750361,138.612942633952));
#82406=CARTESIAN_POINT('Ctrl Pts',(78.6130217290521,-8.07699305790112,138.611552245553));
#82407=CARTESIAN_POINT('Ctrl Pts',(78.6184322973563,-8.06891395182371,138.610906253053));
#82408=CARTESIAN_POINT('Ctrl Pts',(78.6307485453104,-8.05086698277575,138.609460586652));
#82409=CARTESIAN_POINT('Ctrl Pts',(78.6376929919388,-8.04092614501287,138.608662418179));
#82410=CARTESIAN_POINT('Ctrl Pts',(78.6584620210802,-8.01187649078897,138.606323658837));
#82411=CARTESIAN_POINT('Ctrl Pts',(78.6725848901082,-7.99298389592706,138.604794511063));
#82412=CARTESIAN_POINT('Ctrl Pts',(78.750998140174,-7.89260552361618,138.596611537474));
#82413=CARTESIAN_POINT('Ctrl Pts',(78.8223970604525,-7.81696032970234,138.590250266556));
#82414=CARTESIAN_POINT('Ctrl Pts',(78.9593334832886,-7.69664747395032,138.579118180237));
#82415=CARTESIAN_POINT('Ctrl Pts',(79.0218699622572,-7.64908382375167,138.574346148211));
#82416=CARTESIAN_POINT('Ctrl Pts',(79.1081348243836,-7.59261249238801,138.567843704408));
#82417=CARTESIAN_POINT('Ctrl Pts',(79.1290454399641,-7.57957713537964,138.566272894509));
#82418=CARTESIAN_POINT('Ctrl Pts',(79.1649872963638,-7.55826358366812,138.563568399681));
#82419=CARTESIAN_POINT('Ctrl Pts',(79.1798718133722,-7.54974491525152,138.562447108845));
#82420=CARTESIAN_POINT('Ctrl Pts',(79.2013882609893,-7.53786783131661,138.560820473376));
#82421=CARTESIAN_POINT('Ctrl Pts',(79.2079158569174,-7.53432135396445,138.560326243612));
#82422=CARTESIAN_POINT('Ctrl Pts',(79.219323999269,-7.52822171547543,138.559460806323));
#82423=CARTESIAN_POINT('Ctrl Pts',(79.2241938354606,-7.52564891190675,138.559090834731));
#82424=CARTESIAN_POINT('Ctrl Pts',(79.2346645379832,-7.52018333386636,138.558294079285));
#82425=CARTESIAN_POINT('Ctrl Pts',(79.2402689975685,-7.51729823112319,138.557866868923));
#82426=CARTESIAN_POINT('Ctrl Pts',(79.2557197346365,-7.5094549924992,138.556687340246));
#82427=CARTESIAN_POINT('Ctrl Pts',(79.2655988547602,-7.50456278151904,138.555931195485));
#82428=CARTESIAN_POINT('Ctrl Pts',(79.3223560191607,-7.47715425293571,138.551578890084));
#82429=CARTESIAN_POINT('Ctrl Pts',(79.370215206549,-7.45674676918163,138.547878181303));
#82430=CARTESIAN_POINT('Ctrl Pts',(79.5149160171262,-7.40289776301465,138.53674916697));
#82431=CARTESIAN_POINT('Ctrl Pts',(79.6139828650921,-7.37610512135498,138.529221755229));
#82432=CARTESIAN_POINT('Ctrl Pts',(79.786623253287,-7.34611715486538,138.516660911712));
#82433=CARTESIAN_POINT('Ctrl Pts',(79.8591121163593,-7.3383708786738,138.511544095369));
#82434=CARTESIAN_POINT('Ctrl Pts',(79.9494895583125,-7.33467266240074,138.505371191486));
#82435=CARTESIAN_POINT('Ctrl Pts',(79.967105186019,-7.33423158311541,138.504177419419));
#82436=CARTESIAN_POINT('Ctrl Pts',(79.9954593124748,-7.3339716043367,138.50227036102));
#82437=CARTESIAN_POINT('Ctrl Pts',(80.0061944363775,-7.33397692954553,138.50155165648));
#82438=CARTESIAN_POINT('Ctrl Pts',(80.0267223977116,-7.33418553422263,138.500183429913));
#82439=CARTESIAN_POINT('Ctrl Pts',(80.0365149210737,-7.33437141341169,138.499533393843));
#82440=CARTESIAN_POINT('Ctrl Pts',(80.0588703600664,-7.33499300885727,138.498055194475));
#82441=CARTESIAN_POINT('Ctrl Pts',(80.0714312232682,-7.33548457664384,138.497228805245));
#82442=CARTESIAN_POINT('Ctrl Pts',(80.1049615143958,-7.33717704190505,138.495033111872));
#82443=CARTESIAN_POINT('Ctrl Pts',(80.1259162276642,-7.33863240784865,138.493671701344));
#82444=CARTESIAN_POINT('Ctrl Pts',(80.2672375367983,-7.35113690819438,138.484550788982));
#82445=CARTESIAN_POINT('Ctrl Pts',(80.3861216598723,-7.37486021889751,138.477209685945));
#82446=CARTESIAN_POINT('Ctrl Pts',(80.5645438658497,-7.43116916736222,138.465777060569));
#82447=CARTESIAN_POINT('Ctrl Pts',(80.62643700612,-7.45484131225998,138.461720066128));
#82448=CARTESIAN_POINT('Ctrl Pts',(80.7072016229514,-7.49138287629356,138.456109433669));
#82449=CARTESIAN_POINT('Ctrl Pts',(80.7274605479272,-7.501046761181,138.454673988079));
#82450=CARTESIAN_POINT('Ctrl Pts',(80.7618138964147,-7.51829439139616,138.452180987866));
#82451=CARTESIAN_POINT('Ctrl Pts',(80.7760059856607,-7.52567758361189,138.451133425087));
#82452=CARTESIAN_POINT('Ctrl Pts',(80.7964511678912,-7.53669081840668,138.449595268841));
#82453=CARTESIAN_POINT('Ctrl Pts',(80.8027909110374,-7.54015926481604,138.449114196331));
#82454=CARTESIAN_POINT('Ctrl Pts',(80.8138598112878,-7.54630891859968,138.448266673758));
#82455=CARTESIAN_POINT('Ctrl Pts',(80.8185987148561,-7.54897219344509,138.447901352834));
#82456=CARTESIAN_POINT('Ctrl Pts',(80.828894873633,-7.55482515148955,138.447102125861));
#82457=CARTESIAN_POINT('Ctrl Pts',(80.8344467008278,-7.55802366374395,138.446667687241));
#82458=CARTESIAN_POINT('Ctrl Pts',(80.849899348852,-7.56704534861054,138.445449026636));
#82459=CARTESIAN_POINT('Ctrl Pts',(80.8597583783436,-7.57293887702075,138.444660570075));
#82460=CARTESIAN_POINT('Ctrl Pts',(80.9259763525672,-7.61345788121388,138.439294622351));
#82461=CARTESIAN_POINT('Ctrl Pts',(80.9802851901333,-7.65130795039124,138.434548768141));
#82462=CARTESIAN_POINT('Ctrl Pts',(81.0494939380594,-7.70593500960563,138.428156629021));
#82463=CARTESIAN_POINT('Ctrl Pts',(81.0665206734937,-7.71993150217568,138.426553800348));
#82464=CARTESIAN_POINT('Ctrl Pts',(81.1369212003291,-7.78018280586612,138.41980969693));
#82465=CARTESIAN_POINT('Ctrl Pts',(81.187606613277,-7.82947215992488,138.414667977005));
#82466=CARTESIAN_POINT('Ctrl Pts',(81.2807389945504,-7.93233655596453,138.404747316231));
#82467=CARTESIAN_POINT('Ctrl Pts',(81.323329006124,-7.9856035669354,138.399971005538));
#82468=CARTESIAN_POINT('Ctrl Pts',(81.3725098713493,-8.05550397657339,138.394141012636));
#82469=CARTESIAN_POINT('Ctrl Pts',(81.3822567335077,-8.06982665742033,138.392967746781));
#82470=CARTESIAN_POINT('Ctrl Pts',(81.3976439983137,-8.09321384810194,138.391085353149));
#82471=CARTESIAN_POINT('Ctrl Pts',(81.4034235669459,-8.10218477836519,138.390371057));
#82472=CARTESIAN_POINT('Ctrl Pts',(81.4143515263168,-8.11951033732702,138.389006078594));
#82473=CARTESIAN_POINT('Ctrl Pts',(81.4195130574064,-8.1278561053661,138.388354930774));
#82474=CARTESIAN_POINT('Ctrl Pts',(81.4311857622385,-8.1471080739557,138.386867102131));
#82475=CARTESIAN_POINT('Ctrl Pts',(81.4376466055814,-8.15804419602341,138.386032278416));
#82476=CARTESIAN_POINT('Ctrl Pts',(81.458075420221,-8.19354447769681,138.383354379379));
#82477=CARTESIAN_POINT('Ctrl Pts',(81.4715441897384,-8.21839121760763,138.381529085882));
#82478=CARTESIAN_POINT('Ctrl Pts',(81.5438289532878,-8.36023867017505,138.371354561212));
#82479=CARTESIAN_POINT('Ctrl Pts',(81.5893207665385,-8.48350766445429,138.363481739732));
#82480=CARTESIAN_POINT('Ctrl Pts',(81.6365740009059,-8.68020229686246,138.351070222903));
#82481=CARTESIAN_POINT('Ctrl Pts',(81.6487634832857,-8.75055726931617,138.346647835921));
#82482=CARTESIAN_POINT('Ctrl Pts',(81.6580966694744,-8.83714970725488,138.340997106757));
#82483=CARTESIAN_POINT('Ctrl Pts',(81.6595640601898,-8.85285425929765,138.33996394504));
#82484=CARTESIAN_POINT('Ctrl Pts',(81.6613750744937,-8.87574018888127,138.338443127261));
#82485=CARTESIAN_POINT('Ctrl Pts',(81.6618955800766,-8.88290723770163,138.337964694672));
#82486=CARTESIAN_POINT('Ctrl Pts',(81.6627281080705,-8.89549762033381,138.337120072694));
#82487=CARTESIAN_POINT('Ctrl Pts',(81.6630599964519,-8.90091944868504,138.336754985731));
#82488=CARTESIAN_POINT('Ctrl Pts',(81.6637270982145,-8.91276728910201,138.33595412142));
#82489=CARTESIAN_POINT('Ctrl Pts',(81.6640515969898,-8.9191935507508,138.335517791822));
#82490=CARTESIAN_POINT('Ctrl Pts',(81.6648571046909,-8.93721805853627,138.334288824208));
#82491=CARTESIAN_POINT('Ctrl Pts',(81.6652541190076,-8.94881942246295,138.333491841116));
#82492=CARTESIAN_POINT('Ctrl Pts',(81.6673560871115,-9.03727841390818,138.327374187734));
#82493=CARTESIAN_POINT('Ctrl Pts',(81.6638602753966,-9.11415912409219,138.321826942408));
#82494=CARTESIAN_POINT('Ctrl Pts',(81.6485394998224,-9.24725678906403,138.312088770737));
#82495=CARTESIAN_POINT('Ctrl Pts',(81.6390939687503,-9.3036274436794,138.30792068187));
#82496=CARTESIAN_POINT('Ctrl Pts',(81.6088803119067,-9.44038431505247,138.297799254905));
#82497=CARTESIAN_POINT('Ctrl Pts',(81.5849649046377,-9.51992698704693,138.29190908635));
#82498=CARTESIAN_POINT('Ctrl Pts',(81.5470215729409,-9.61871075116403,138.284633845712));
#82499=CARTESIAN_POINT('Ctrl Pts',(81.5383847161538,-9.63988381438838,138.283076281886));
#82500=CARTESIAN_POINT('Ctrl Pts',(81.5246220019957,-9.67173184891744,138.280735047203));
#82501=CARTESIAN_POINT('Ctrl Pts',(81.5198140171293,-9.68254032237748,138.279940764566));
#82502=CARTESIAN_POINT('Ctrl Pts',(81.5112438553686,-9.70126658874638,138.278564817294));
#82503=CARTESIAN_POINT('Ctrl Pts',(81.5075336055757,-9.70920748161489,138.277981404823));
#82504=CARTESIAN_POINT('Ctrl Pts',(81.499026415129,-9.72704661579931,138.276670717998));
#82505=CARTESIAN_POINT('Ctrl Pts',(81.4941937393209,-9.73692744143512,138.275944709717));
#82506=CARTESIAN_POINT('Ctrl Pts',(81.4808128369563,-9.76361297905029,138.273983308478));
#82507=CARTESIAN_POINT('Ctrl Pts',(81.4720764779417,-9.78032193991025,138.272754508241));
#82508=CARTESIAN_POINT('Ctrl Pts',(81.4178318295768,-9.87991424152801,138.265418864789));
#82509=CARTESIAN_POINT('Ctrl Pts',(81.3656165050383,-9.95895311903628,138.259561907776));
#82510=CARTESIAN_POINT('Ctrl Pts',(81.2495545732988,-10.1057764438651,138.248102500175));
#82511=CARTESIAN_POINT('Ctrl Pts',(81.186188023533,-10.1734921905774,138.242514313668));
#82512=CARTESIAN_POINT('Ctrl Pts',(81.0976679062517,-10.2535543146676,138.235011266274));
#82513=CARTESIAN_POINT('Ctrl Pts',(81.0773761295718,-10.2710364939648,138.233308855011));
#82514=CARTESIAN_POINT('Ctrl Pts',(81.0425742000378,-10.2995874716513,138.230400768338));
#82515=CARTESIAN_POINT('Ctrl Pts',(81.0282871355572,-10.3109210728568,138.229210074329));
#82516=CARTESIAN_POINT('Ctrl Pts',(81.0077780479651,-10.3266489115807,138.227500577077));
#82517=CARTESIAN_POINT('Ctrl Pts',(81.0017069209194,-10.3312389595983,138.226994498134));
#82518=CARTESIAN_POINT('Ctrl Pts',(80.9911686592186,-10.339093461734,138.22611557854));
#82519=CARTESIAN_POINT('Ctrl Pts',(80.986716357711,-10.3423775321488,138.225744094408));
#82520=CARTESIAN_POINT('Ctrl Pts',(80.9772341857389,-10.3492990304779,138.224952477717));
#82521=CARTESIAN_POINT('Ctrl Pts',(80.9722004020218,-10.3529304869702,138.224531991428));
#82522=CARTESIAN_POINT('Ctrl Pts',(80.9582917627374,-10.3628467116179,138.223369763879));
#82523=CARTESIAN_POINT('Ctrl Pts',(80.9493756678044,-10.3690727108579,138.222624278211));
#82524=CARTESIAN_POINT('Ctrl Pts',(80.9018947684799,-10.4015412007286,138.218654700848));
#82525=CARTESIAN_POINT('Ctrl Pts',(80.8623047052113,-10.4262403921482,138.215346547015));
#82526=CARTESIAN_POINT('Ctrl Pts',(80.7454339453908,-10.4925072199919,138.205691384427));
#82527=CARTESIAN_POINT('Ctrl Pts',(80.6658362202949,-10.5296770218662,138.199255542834));
#82528=CARTESIAN_POINT('Ctrl Pts',(80.5122979459122,-10.587109161112,138.187404044057));
#82529=CARTESIAN_POINT('Ctrl Pts',(80.4391581917112,-10.6088839199372,138.181977622184));
#82530=CARTESIAN_POINT('Ctrl Pts',(80.3375096411757,-10.631693630497,138.174771394722));
#82531=CARTESIAN_POINT('Ctrl Pts',(80.3100928388688,-10.6371253636595,138.172859390139));
#82532=CARTESIAN_POINT('Ctrl Pts',(80.2699517562068,-10.6440332989691,138.170104352569));
#82533=CARTESIAN_POINT('Ctrl Pts',(80.2573278065656,-10.6460564554662,138.16924423978));
#82534=CARTESIAN_POINT('Ctrl Pts',(80.2349937357081,-10.6493725674169,138.167733322795));
#82535=CARTESIAN_POINT('Ctrl Pts',(80.2252932949809,-10.6507255557019,138.167080654889));
#82536=CARTESIAN_POINT('Ctrl Pts',(80.2049370835632,-10.653381994793,138.165718283175));
#82537=CARTESIAN_POINT('Ctrl Pts',(80.1942794804908,-10.6546681605338,138.165009151354));
#82538=CARTESIAN_POINT('Ctrl Pts',(80.1660986948024,-10.6577930024467,138.163144526125));
#82539=CARTESIAN_POINT('Ctrl Pts',(80.1485571947301,-10.6594569032775,138.161994530635));
#82540=CARTESIAN_POINT('Ctrl Pts',(80.0662023256179,-10.6659523016728,138.156640816002));
#82541=CARTESIAN_POINT('Ctrl Pts',(80.0011647255404,-10.6672671971632,138.152547223699));
#82542=CARTESIAN_POINT('Ctrl Pts',(79.7906320968475,-10.6592001775789,138.139491356231));
#82543=CARTESIAN_POINT('Ctrl Pts',(79.6464361269822,-10.6345525797856,138.130893657106));
#82544=CARTESIAN_POINT('Ctrl Pts',(79.4858722721177,-10.584844454118,138.120105926452));
#82545=CARTESIAN_POINT('Ctrl Pts',(79.4645796308183,-10.5777782396883,138.118648339947));
#82546=CARTESIAN_POINT('Ctrl Pts',(79.4356664268688,-10.5675304121401,138.116623579734));
#82547=CARTESIAN_POINT('Ctrl Pts',(79.4279161747799,-10.564718525695,138.116076309569));
#82548=CARTESIAN_POINT('Ctrl Pts',(79.4148987023142,-10.5598859879694,138.115148944494));
#82549=CARTESIAN_POINT('Ctrl Pts',(79.4096201605108,-10.5578958463197,138.114770624443));
#82550=CARTESIAN_POINT('Ctrl Pts',(79.3987912128859,-10.553750123733,138.113989623443));
#82551=CARTESIAN_POINT('Ctrl Pts',(79.3932421260253,-10.5515915481405,138.113586783608));
#82552=CARTESIAN_POINT('Ctrl Pts',(79.3786664088957,-10.545831497834,138.112521934093));
#82553=CARTESIAN_POINT('Ctrl Pts',(79.3696596741634,-10.5421807654733,138.111857123389));
#82554=CARTESIAN_POINT('Ctrl Pts',(79.3307974762706,-10.5260313066563,138.108960583435));
#82555=CARTESIAN_POINT('Ctrl Pts',(79.3012798319572,-10.5127436550002,138.106688593166));
#82556=CARTESIAN_POINT('Ctrl Pts',(79.2486156407491,-10.4871661761695,138.102526226925));
#82557=CARTESIAN_POINT('Ctrl Pts',(79.2253348701368,-10.4751730474593,138.100646276896));
#82558=CARTESIAN_POINT('Ctrl Pts',(79.1163605275306,-10.4157436165353,138.091683399061));
#82559=CARTESIAN_POINT('Ctrl Pts',(79.0346706200088,-10.3613557689784,138.08449168696));
#82560=CARTESIAN_POINT('Ctrl Pts',(78.9010168983634,-10.2542597921801,138.072211178715));
#82561=CARTESIAN_POINT('Ctrl Pts',(78.8468840465849,-10.2046816029801,138.067057796581));
#82562=CARTESIAN_POINT('Ctrl Pts',(78.783986813428,-10.1389378491472,138.060848291008));
#82563=CARTESIAN_POINT('Ctrl Pts',(78.7719891160083,-10.1259914762317,138.059652463455));
#82564=CARTESIAN_POINT('Ctrl Pts',(78.753024188109,-10.1048632017148,138.057742933131));
#82565=CARTESIAN_POINT('Ctrl Pts',(78.7459267043359,-10.0968005964589,138.05702378686));
#82566=CARTESIAN_POINT('Ctrl Pts',(78.7325087113124,-10.0812574716588,138.055655226475));
#82567=CARTESIAN_POINT('Ctrl Pts',(78.7261752385491,-10.0737887925549,138.055005293519));
#82568=CARTESIAN_POINT('Ctrl Pts',(78.7118711291791,-10.05661615227,138.053528018844));
#82569=CARTESIAN_POINT('Ctrl Pts',(78.7039435560626,-10.0468769696414,138.052702443199));
#82570=CARTESIAN_POINT('Ctrl Pts',(78.683080955167,-10.0206465865431,138.050510451186));
#82571=CARTESIAN_POINT('Ctrl Pts',(78.670345463884,-10.0039990550955,138.049151885297));
#82572=CARTESIAN_POINT('Ctrl Pts',(78.5858580102951,-9.88913065055669,138.039984103861));
#82573=CARTESIAN_POINT('Ctrl Pts',(78.5247345555471,-9.78354744866699,138.032599506894));
#82574=CARTESIAN_POINT('Ctrl Pts',(78.4491360085769,-9.61212248495406,138.021150117326));
#82575=CARTESIAN_POINT('Ctrl Pts',(78.4262054564742,-9.5504930016204,138.017122819631));
#82576=CARTESIAN_POINT('Ctrl Pts',(78.4004337605245,-9.46630806743096,138.011549560494));
#82577=CARTESIAN_POINT('Ctrl Pts',(78.3943233224832,-9.44481195594943,138.010120178699));
#82578=CARTESIAN_POINT('Ctrl Pts',(78.3845969542231,-9.40777842962082,138.007636704069));
#82579=CARTESIAN_POINT('Ctrl Pts',(78.3807683309085,-9.39229963562683,138.006592501605));
#82580=CARTESIAN_POINT('Ctrl Pts',(78.375530452953,-9.36973879727022,138.005058389208));
#82581=CARTESIAN_POINT('Ctrl Pts',(78.3739440148056,-9.36269824330599,138.004577930402));
#82582=CARTESIAN_POINT('Ctrl Pts',(78.3712431190839,-9.35033778703886,138.003731083528));
#82583=CARTESIAN_POINT('Ctrl Pts',(78.3701088740253,-9.34502240275204,138.003365818387));
#82584=CARTESIAN_POINT('Ctrl Pts',(78.3676928827579,-9.33342256871863,138.002566217251));
#82585=CARTESIAN_POINT('Ctrl Pts',(78.3664214291154,-9.32713633795341,138.002131344157));
#82586=CARTESIAN_POINT('Ctrl Pts',(78.3629688734555,-9.30954429387675,138.000910318892));
#82587=CARTESIAN_POINT('Ctrl Pts',(78.3608686863847,-9.29822323430471,138.000119906912));
#82588=CARTESIAN_POINT('Ctrl Pts',(78.3472941221451,-9.22056960548436,137.994670699723));
#82589=CARTESIAN_POINT('Ctrl Pts',(78.3397332654653,-9.15362294499791,137.989837623539));
#82590=CARTESIAN_POINT('Ctrl Pts',(78.3347732356146,-9.05812245807967,137.982902254536));
#82591=CARTESIAN_POINT('Ctrl Pts',(78.3340257365145,-9.02980136265055,137.980840097936));
#82592=CARTESIAN_POINT('Ctrl Pts',(78.3338937191599,-8.88071687455458,137.969987743028));
#82593=CARTESIAN_POINT('Ctrl Pts',(78.3469166497543,-8.76028325719652,137.96126889487));
#82594=CARTESIAN_POINT('Ctrl Pts',(78.3773635481472,-8.62178279113277,137.951513814421));
#82595=CARTESIAN_POINT('Ctrl Pts',(78.3822617998227,-8.60135166197025,137.950080742957));
#82596=CARTESIAN_POINT('Ctrl Pts',(78.3907068956839,-8.56885067699838,137.947809787927));
#82597=CARTESIAN_POINT('Ctrl Pts',(78.3940061041705,-8.55671943882072,137.946964089689));
#82598=CARTESIAN_POINT('Ctrl Pts',(78.4001194486049,-8.53520526474169,137.945467425903));
#82599=CARTESIAN_POINT('Ctrl Pts',(78.4028795813367,-8.52580773942798,137.944814747905));
#82600=CARTESIAN_POINT('Ctrl Pts',(78.4088380700724,-8.50616305216194,137.943452398024));
#82601=CARTESIAN_POINT('Ctrl Pts',(78.4120529215466,-8.49592133210179,137.942743297751));
#82602=CARTESIAN_POINT('Ctrl Pts',(78.4208046914339,-8.46895526421802,137.940878853581));
#82603=CARTESIAN_POINT('Ctrl Pts',(78.4265083702413,-8.45228614804004,137.939729005626));
#82604=CARTESIAN_POINT('Ctrl Pts',(78.433823490773,-8.43196568807629,137.938329369574));
#82605=CARTESIAN_POINT('Ctrl Pts',(78.4351847763598,-8.42822631211844,137.938071894579));
#82606=CARTESIAN_POINT('Ctrl Pts',(78.4365593741136,-8.42449204234183,137.937814844869));
#82607=CARTESIAN_POINT('Ctrl Pts',(78.4365594354234,-8.42449187578589,138.13187361233));
#82608=CARTESIAN_POINT('Ctrl Pts',(78.4162408380163,-8.4796899139457,138.136154213031));
#82609=CARTESIAN_POINT('Ctrl Pts',(78.3988502582591,-8.53595084181721,138.140440641763));
#82610=CARTESIAN_POINT('Ctrl Pts',(78.3715300080598,-8.64440579812346,138.148485977305));
#82611=CARTESIAN_POINT('Ctrl Pts',(78.3610470722338,-8.69636212694456,138.152248990963));
#82612=CARTESIAN_POINT('Ctrl Pts',(78.3494451869366,-8.77240761653733,138.157611105667));
#82613=CARTESIAN_POINT('Ctrl Pts',(78.3463441283616,-8.7961573093358,138.159265662141));
#82614=CARTESIAN_POINT('Ctrl Pts',(78.3416515914771,-8.83932701747486,138.162237367125));
#82615=CARTESIAN_POINT('Ctrl Pts',(78.339886678227,-8.85872344118776,138.163559574137));
#82616=CARTESIAN_POINT('Ctrl Pts',(78.337648209532,-8.88924630923566,138.16562068145));
#82617=CARTESIAN_POINT('Ctrl Pts',(78.3369454406017,-8.90035363447742,138.16636666894));
#82618=CARTESIAN_POINT('Ctrl Pts',(78.3358375461699,-8.92117245425774,138.167757585857));
#82619=CARTESIAN_POINT('Ctrl Pts',(78.3354060060516,-8.93088200769565,138.168403312385));
#82620=CARTESIAN_POINT('Ctrl Pts',(78.3346279522514,-8.95268846264312,138.169847129197));
#82621=CARTESIAN_POINT('Ctrl Pts',(78.3343282238388,-8.96478656519042,138.170643728318));
#82622=CARTESIAN_POINT('Ctrl Pts',(78.3338346509293,-9.00036039841419,138.172973899075));
#82623=CARTESIAN_POINT('Ctrl Pts',(78.334005132081,-9.02383880690506,138.174496153192));
#82624=CARTESIAN_POINT('Ctrl Pts',(78.3372811617206,-9.13916410223909,138.181909022735));
#82625=CARTESIAN_POINT('Ctrl Pts',(78.3474859608974,-9.23065282536611,138.187577559313));
#82626=CARTESIAN_POINT('Ctrl Pts',(78.3797605383403,-9.39510428146941,138.197826704273));
#82627=CARTESIAN_POINT('Ctrl Pts',(78.3993774358818,-9.46828379149291,138.202414086921));
#82628=CARTESIAN_POINT('Ctrl Pts',(78.4347717964449,-9.57161383638414,138.209220657374));
#82629=CARTESIAN_POINT('Ctrl Pts',(78.4466000024374,-9.60301730952699,138.211335740606));
#82630=CARTESIAN_POINT('Ctrl Pts',(78.467528952769,-9.65387184785785,138.214870435589));
#82631=CARTESIAN_POINT('Ctrl Pts',(78.4760722519293,-9.67354288487014,138.216265358164));
#82632=CARTESIAN_POINT('Ctrl Pts',(78.4883633259994,-9.70041147377598,138.218216451382));
#82633=CARTESIAN_POINT('Ctrl Pts',(78.4917879523247,-9.70775566359377,138.218754544787));
#82634=CARTESIAN_POINT('Ctrl Pts',(78.4976753745127,-9.72014459103995,138.219670874305));
#82635=CARTESIAN_POINT('Ctrl Pts',(78.5001103985647,-9.72520251988738,138.22004743184));
#82636=CARTESIAN_POINT('Ctrl Pts',(78.5052004481131,-9.73564005329026,138.220829765833));
#82637=CARTESIAN_POINT('Ctrl Pts',(78.5078590190368,-9.74101773149138,138.221235740676));
#82638=CARTESIAN_POINT('Ctrl Pts',(78.5149940884378,-9.7552562456191,138.222318122792));
#82639=CARTESIAN_POINT('Ctrl Pts',(78.5195207618503,-9.76409146524403,138.222997494212));
#82640=CARTESIAN_POINT('Ctrl Pts',(78.5401181263322,-9.80342344633525,138.226054891001));
#82641=CARTESIAN_POINT('Ctrl Pts',(78.5570529769975,-9.83345534985851,138.228478683909));
#82642=CARTESIAN_POINT('Ctrl Pts',(78.5872318929872,-9.88329417236705,138.23262873011));
#82643=CARTESIAN_POINT('Ctrl Pts',(78.5999925923471,-9.9033833621558,138.234338253884));
#82644=CARTESIAN_POINT('Ctrl Pts',(78.6663398912396,-10.0030504792924,138.242984226519));
#82645=CARTESIAN_POINT('Ctrl Pts',(78.7263031982461,-10.0781731988061,138.250026907009));
#82646=CARTESIAN_POINT('Ctrl Pts',(78.8267376140599,-10.1838479474004,138.260489784493));
#82647=CARTESIAN_POINT('Ctrl Pts',(78.8626831996413,-10.2184218720492,138.264022441926));
#82648=CARTESIAN_POINT('Ctrl Pts',(78.9254731741463,-10.2736116935564,138.269841119918));
#82649=CARTESIAN_POINT('Ctrl Pts',(78.951490614769,-10.2951150526434,138.272160049775));
#82650=CARTESIAN_POINT('Ctrl Pts',(78.9889948813682,-10.3242406758455,138.27537855041));
#82651=CARTESIAN_POINT('Ctrl Pts',(78.999948857413,-10.3325323445636,138.276304339618));
#82652=CARTESIAN_POINT('Ctrl Pts',(79.0190041344841,-10.346588998651,138.277890905895));
#82653=CARTESIAN_POINT('Ctrl Pts',(79.0270566402004,-10.3524185910603,138.278554171431));
#82654=CARTESIAN_POINT('Ctrl Pts',(79.0436103339799,-10.3641782238089,138.279903295275));
#82655=CARTESIAN_POINT('Ctrl Pts',(79.0521156581689,-10.3701017123973,138.280588882975));
#82656=CARTESIAN_POINT('Ctrl Pts',(79.0737995389116,-10.3849047634619,138.282318041019));
#82657=CARTESIAN_POINT('Ctrl Pts',(79.0870510677369,-10.3936759930543,138.28335751218));
#82658=CARTESIAN_POINT('Ctrl Pts',(79.1396108269839,-10.4273940525248,138.287415930332));
#82659=CARTESIAN_POINT('Ctrl Pts',(79.179833989079,-10.4508796050651,138.290381556378));
#82660=CARTESIAN_POINT('Ctrl Pts',(79.32056975265,-10.5253265657428,138.300373902286));
#82661=CARTESIAN_POINT('Ctrl Pts',(79.4252318929986,-10.5677655049789,138.307143184363));
#82662=CARTESIAN_POINT('Ctrl Pts',(79.5958292560824,-10.6175395647836,138.318076734668));
#82663=CARTESIAN_POINT('Ctrl Pts',(79.6592880574734,-10.6320850874439,138.322129520577));
#82664=CARTESIAN_POINT('Ctrl Pts',(79.738340761138,-10.6453933188223,138.327336953533));
#82665=CARTESIAN_POINT('Ctrl Pts',(79.7532876126986,-10.647700728144,138.328328495682));
#82666=CARTESIAN_POINT('Ctrl Pts',(79.7752600163266,-10.6507870431205,138.329799023082));
#82667=CARTESIAN_POINT('Ctrl Pts',(79.7822629023838,-10.6517253021591,138.330269618447));
#82668=CARTESIAN_POINT('Ctrl Pts',(79.7941816947229,-10.6532450902334,138.331074150936));
#82669=CARTESIAN_POINT('Ctrl Pts',(79.7990945678788,-10.6538493007611,138.331406819084));
#82670=CARTESIAN_POINT('Ctrl Pts',(79.810285203852,-10.6551749831075,138.33216702983));
#82671=CARTESIAN_POINT('Ctrl Pts',(79.8165642818435,-10.6558826234256,138.332595312));
#82672=CARTESIAN_POINT('Ctrl Pts',(79.8338809064756,-10.6577344732874,138.333780918482));
#82673=CARTESIAN_POINT('Ctrl Pts',(79.8449258580662,-10.6588041268058,138.334542132722));
#82674=CARTESIAN_POINT('Ctrl Pts',(79.9085243171649,-10.6643226433761,138.338950985471));
#82675=CARTESIAN_POINT('Ctrl Pts',(79.9612500247842,-10.6663837943462,138.342706003469));
#82676=CARTESIAN_POINT('Ctrl Pts',(80.1158374726023,-10.6650866694285,138.353853764988));
#82677=CARTESIAN_POINT('Ctrl Pts',(80.2174106677104,-10.6548916397337,138.361340095339));
#82678=CARTESIAN_POINT('Ctrl Pts',(80.3886112914624,-10.6216648825184,138.373839403056));
#82679=CARTESIAN_POINT('Ctrl Pts',(80.4588362841796,-10.6032116494468,138.378934977978));
#82680=CARTESIAN_POINT('Ctrl Pts',(80.544336970477,-10.5746628182562,138.38508639419));
#82681=CARTESIAN_POINT('Ctrl Pts',(80.5609412639335,-10.5688246136208,138.386278758174));
#82682=CARTESIAN_POINT('Ctrl Pts',(80.5875138613088,-10.5590056323754,138.388183997746));
#82683=CARTESIAN_POINT('Ctrl Pts',(80.5975412679014,-10.5551898731265,138.388902275348));
#82684=CARTESIAN_POINT('Ctrl Pts',(80.6166491724863,-10.5477065885507,138.390269954034));
#82685=CARTESIAN_POINT('Ctrl Pts',(80.6257355252957,-10.5440553570189,138.390919866397));
#82686=CARTESIAN_POINT('Ctrl Pts',(80.6464137681153,-10.5355335612935,138.392398140205));
#82687=CARTESIAN_POINT('Ctrl Pts',(80.6579838635581,-10.5306114226591,138.393224724461));
#82688=CARTESIAN_POINT('Ctrl Pts',(80.6887451802089,-10.5171116982725,138.395421714864));
#82689=CARTESIAN_POINT('Ctrl Pts',(80.7078320268624,-10.5083009359409,138.396784209767));
#82690=CARTESIAN_POINT('Ctrl Pts',(80.8352048575512,-10.4465532195802,138.405884162082));
#82691=CARTESIAN_POINT('Ctrl Pts',(80.9376382540033,-10.3823609225986,138.413205954785));
#82692=CARTESIAN_POINT('Ctrl Pts',(81.0844094952207,-10.2665018248198,138.424631601502));
#82693=CARTESIAN_POINT('Ctrl Pts',(81.1340493662402,-10.222252669018,138.42870222721));
#82694=CARTESIAN_POINT('Ctrl Pts',(81.1967735684444,-10.1592216096295,138.434329931317));
#82695=CARTESIAN_POINT('Ctrl Pts',(81.2123110473044,-10.1429626144115,138.435768066381));
#82696=CARTESIAN_POINT('Ctrl Pts',(81.2383451425973,-10.1145913818378,138.43826523838));
#82697=CARTESIAN_POINT('Ctrl Pts',(81.2490050868428,-10.1026327073994,138.439314237175));
#82698=CARTESIAN_POINT('Ctrl Pts',(81.2642226788876,-10.0850572719499,138.440854044841));
#82699=CARTESIAN_POINT('Ctrl Pts',(81.2689191772768,-10.0795611987909,138.441335302064));
#82700=CARTESIAN_POINT('Ctrl Pts',(81.2770836122515,-10.0698798945819,138.442182939146));
#82701=CARTESIAN_POINT('Ctrl Pts',(81.280567065107,-10.0657079956872,138.442548187269));
#82702=CARTESIAN_POINT('Ctrl Pts',(81.2881093726586,-10.0565847016777,138.443346985021));
#82703=CARTESIAN_POINT('Ctrl Pts',(81.2921600560248,-10.0516270127352,138.443781064482));
#82704=CARTESIAN_POINT('Ctrl Pts',(81.3033865396136,-10.0377239711607,138.444998089986));
#82705=CARTESIAN_POINT('Ctrl Pts',(81.3104985386231,-10.0287278911602,138.445785254614));
#82706=CARTESIAN_POINT('Ctrl Pts',(81.3576051003872,-9.96786081399175,138.451105045985));
#82707=CARTESIAN_POINT('Ctrl Pts',(81.3945994656451,-9.91374864267551,138.455802824427));
#82708=CARTESIAN_POINT('Ctrl Pts',(81.4392456805557,-9.83939219079096,138.462089307413));
#82709=CARTESIAN_POINT('Ctrl Pts',(81.4498327865488,-9.82097031100142,138.463634071691));
#82710=CARTESIAN_POINT('Ctrl Pts',(81.4930625739267,-9.74230366163525,138.470166397353));
#82711=CARTESIAN_POINT('Ctrl Pts',(81.522326526334,-9.68027453639487,138.475157104236));
#82712=CARTESIAN_POINT('Ctrl Pts',(81.5740833076893,-9.55036673136398,138.485172991431));
#82713=CARTESIAN_POINT('Ctrl Pts',(81.5962000233244,-9.48248291686422,138.49018060228));
#82714=CARTESIAN_POINT('Ctrl Pts',(81.6182480663619,-9.39640425338043,138.496243725862));
#82715=CARTESIAN_POINT('Ctrl Pts',(81.6223285704271,-9.37935891541123,138.497430985418));
#82716=CARTESIAN_POINT('Ctrl Pts',(81.6284687982065,-9.35179558137282,138.499330080579));
#82717=CARTESIAN_POINT('Ctrl Pts',(81.6306972451329,-9.34131695210185,138.50004725577));
#82718=CARTESIAN_POINT('Ctrl Pts',(81.6347697947028,-9.32121595399975,138.501414100116));
#82719=CARTESIAN_POINT('Ctrl Pts',(81.6366303867693,-9.31159742436894,138.502064268603));
#82720=CARTESIAN_POINT('Ctrl Pts',(81.6406906590706,-9.28956698441122,138.50354485532));
#82721=CARTESIAN_POINT('Ctrl Pts',(81.6428345543528,-9.27714530261816,138.50437347627));
#82722=CARTESIAN_POINT('Ctrl Pts',(81.6481949467874,-9.24383602047196,138.506579763343));
#82723=CARTESIAN_POINT('Ctrl Pts',(81.6511554036219,-9.22290914042401,138.507949409065));
#82724=CARTESIAN_POINT('Ctrl Pts',(81.6680483973525,-9.08456358618208,138.51690793204));
#82725=CARTESIAN_POINT('Ctrl Pts',(81.6698456203906,-8.9660018533556,138.5240992852));
#82726=CARTESIAN_POINT('Ctrl Pts',(81.6501770088163,-8.75098256066482,138.537289425265));
#82727=CARTESIAN_POINT('Ctrl Pts',(81.6327473246685,-8.65471109099327,138.543263811233));
#82728=CARTESIAN_POINT('Ctrl Pts',(81.6038688700322,-8.54911094842004,138.550422975132));
#82729=CARTESIAN_POINT('Ctrl Pts',(81.6006228756811,-8.53772012885398,138.551203440306));
#82730=CARTESIAN_POINT('Ctrl Pts',(81.5954325132745,-8.52021647805795,138.552416843218));
#82731=CARTESIAN_POINT('Ctrl Pts',(81.5935737520238,-8.51407837488094,138.552845045651));
#82732=CARTESIAN_POINT('Ctrl Pts',(81.5900594521317,-8.50271031434071,138.553643365241));
#82733=CARTESIAN_POINT('Ctrl Pts',(81.5884134676726,-8.49747761716935,138.554012934576));
#82734=CARTESIAN_POINT('Ctrl Pts',(81.5845712890876,-8.48547056017931,138.554865747976));
#82735=CARTESIAN_POINT('Ctrl Pts',(81.5823574762219,-8.47870207421528,138.555349985149));
#82736=CARTESIAN_POINT('Ctrl Pts',(81.5750782316615,-8.45692024145689,138.556919160484));
#82737=CARTESIAN_POINT('Ctrl Pts',(81.5698421648651,-8.441965420673,138.558013186098));
#82738=CARTESIAN_POINT('Ctrl Pts',(81.534719793454,-8.34606021026865,138.565127151807));
#82739=CARTESIAN_POINT('Ctrl Pts',(81.4987980591139,-8.26746762889686,138.571403106748));
#82740=CARTESIAN_POINT('Ctrl Pts',(81.421387860257,-8.12788116124493,138.58302200605));
#82741=CARTESIAN_POINT('Ctrl Pts',(81.3816206262326,-8.0661581589655,138.588352384458));
#82742=CARTESIAN_POINT('Ctrl Pts',(81.3135217447979,-7.97438210084636,138.59648960147));
#82743=CARTESIAN_POINT('Ctrl Pts',(81.287926120545,-7.94241869640054,138.599369002259));
#82744=CARTESIAN_POINT('Ctrl Pts',(81.2420410227901,-7.88925798838842,138.604233970561));
#82745=CARTESIAN_POINT('Ctrl Pts',(81.2223226334362,-7.86759491075819,138.606239982383));
#82746=CARTESIAN_POINT('Ctrl Pts',(81.1930300845942,-7.83707066942061,138.60910302719));
#82747=CARTESIAN_POINT('Ctrl Pts',(81.1839079980817,-7.8277853100051,138.609979090436));
#82748=CARTESIAN_POINT('Ctrl Pts',(81.1677113960768,-7.81168076386031,138.611508022467));
#82749=CARTESIAN_POINT('Ctrl Pts',(81.1606837334129,-7.80481558343157,138.612162905309));
#82750=CARTESIAN_POINT('Ctrl Pts',(81.1459301255889,-7.79065595012923,138.613520407573));
#82751=CARTESIAN_POINT('Ctrl Pts',(81.1381942801273,-7.78337241803148,138.614222537639));
#82752=CARTESIAN_POINT('Ctrl Pts',(81.1178162367899,-7.76455036630309,138.616047582469));
#82753=CARTESIAN_POINT('Ctrl Pts',(81.1050647698006,-7.75313159209656,138.617165421521));
#82754=CARTESIAN_POINT('Ctrl Pts',(81.0490050659694,-7.70446651354744,138.621980260943));
#82755=CARTESIAN_POINT('Ctrl Pts',(81.0039709766193,-7.66926262617503,138.62559422336));
#82756=CARTESIAN_POINT('Ctrl Pts',(80.8704583063733,-7.57553737992661,138.635751020503));
#82757=CARTESIAN_POINT('Ctrl Pts',(80.7780919607908,-7.52305585898818,138.642118464408));
#82758=CARTESIAN_POINT('Ctrl Pts',(80.6270110757672,-7.4553443511373,138.652335002728));
#82759=CARTESIAN_POINT('Ctrl Pts',(80.5713939399396,-7.43391845206384,138.656062169448));
#82760=CARTESIAN_POINT('Ctrl Pts',(80.5009487293594,-7.4110326858951,138.660879192669));
#82761=CARTESIAN_POINT('Ctrl Pts',(80.487084210346,-7.40672799191786,138.661831798766));
#82762=CARTESIAN_POINT('Ctrl Pts',(80.4665008344863,-7.40063097107062,138.663255206706));
#82763=CARTESIAN_POINT('Ctrl Pts',(80.4598237340371,-7.3986985141548,138.663718365233));
#82764=CARTESIAN_POINT('Ctrl Pts',(80.4483835429749,-7.39546499659551,138.664514644571));
#82765=CARTESIAN_POINT('Ctrl Pts',(80.4436264545524,-7.39414323598432,138.6648465691));
#82766=CARTESIAN_POINT('Ctrl Pts',(80.4326911864844,-7.39115716278059,138.665611504384));
#82767=CARTESIAN_POINT('Ctrl Pts',(80.426509381775,-7.38950731713928,138.666045311097));
#82768=CARTESIAN_POINT('Ctrl Pts',(80.4092392091179,-7.38500453207709,138.667260796942));
#82769=CARTESIAN_POINT('Ctrl Pts',(80.3981309546554,-7.38223029558075,138.668046677816));
#82770=CARTESIAN_POINT('Ctrl Pts',(80.3239741758767,-7.36451996800702,138.673316204635));
#82771=CARTESIAN_POINT('Ctrl Pts',(80.2601352780521,-7.35316000409785,138.677961507062));
#82772=CARTESIAN_POINT('Ctrl Pts',(80.1728225135298,-7.34282650960915,138.684332877029));
#82773=CARTESIAN_POINT('Ctrl Pts',(80.1497859762565,-7.34058572493441,138.686015810713));
#82774=CARTESIAN_POINT('Ctrl Pts',(80.0554444741208,-7.33338957486402,138.692901841891));
#82775=CARTESIAN_POINT('Ctrl Pts',(79.98389831609,-7.33254497208265,138.698105649573));
#82776=CARTESIAN_POINT('Ctrl Pts',(79.867632732577,-7.33865868101431,138.706427078755));
#82777=CARTESIAN_POINT('Ctrl Pts',(79.8228604510651,-7.34283427505929,138.709599800144));
#82778=CARTESIAN_POINT('Ctrl Pts',(79.7472398062837,-7.35298726597787,138.714897355868));
#82779=CARTESIAN_POINT('Ctrl Pts',(79.7162933957214,-7.35803488049326,138.71704786435));
#82780=CARTESIAN_POINT('Ctrl Pts',(79.6723866033942,-7.36647499557967,138.720075906184));
#82781=CARTESIAN_POINT('Ctrl Pts',(79.6592977296486,-7.36915467970334,138.72097565453));
#82782=CARTESIAN_POINT('Ctrl Pts',(79.6365901829645,-7.37408891250029,138.722531887723));
#82783=CARTESIAN_POINT('Ctrl Pts',(79.6269568673208,-7.37627207083083,138.723190610427));
#82784=CARTESIAN_POINT('Ctrl Pts',(79.6083649157451,-7.38065968284363,138.724459269741));
#82785=CARTESIAN_POINT('Ctrl Pts',(79.5994040807519,-7.38285312439915,138.725069532154));
#82786=CARTESIAN_POINT('Ctrl Pts',(79.575597584752,-7.3888905239227,138.726687934529));
#82787=CARTESIAN_POINT('Ctrl Pts',(79.5607857617665,-7.39286527240194,138.727691844057));
#82788=CARTESIAN_POINT('Ctrl Pts',(79.5056283885136,-7.40848626607871,138.731421240146));
#82789=CARTESIAN_POINT('Ctrl Pts',(79.4656710068684,-7.42145249105214,138.7341042228));
#82790=CARTESIAN_POINT('Ctrl Pts',(79.3594316509531,-7.46042450719096,138.741233517957));
#82791=CARTESIAN_POINT('Ctrl Pts',(79.2942554315006,-7.48919023149188,138.74560004529));
#82792=CARTESIAN_POINT('Ctrl Pts',(79.1304105993628,-7.57442764320174,138.756885153246));
#82793=CARTESIAN_POINT('Ctrl Pts',(79.0353381914595,-7.6369657403136,138.763738793941));
#82794=CARTESIAN_POINT('Ctrl Pts',(78.9362642613365,-7.71772555263,138.772054323678));
#82795=CARTESIAN_POINT('Ctrl Pts',(78.9252712137089,-7.72692518593542,138.772995183921));
#82796=CARTESIAN_POINT('Ctrl Pts',(78.9091524749974,-7.74077185919534,138.774404348627));
#82797=CARTESIAN_POINT('Ctrl Pts',(78.9039344851552,-7.74531110776139,138.774865228488));
#82798=CARTESIAN_POINT('Ctrl Pts',(78.8946460068597,-7.75349352568745,138.775694417824));
#82799=CARTESIAN_POINT('Ctrl Pts',(78.8905649680532,-7.75712440338631,138.7760618307));
#82800=CARTESIAN_POINT('Ctrl Pts',(78.8815462931104,-7.7652280820378,138.776880724837));
#82801=CARTESIAN_POINT('Ctrl Pts',(78.8766176535488,-7.76971040658603,138.777332891113));
#82802=CARTESIAN_POINT('Ctrl Pts',(78.8621153960861,-7.78305920548846,138.778676836857));
#82803=CARTESIAN_POINT('Ctrl Pts',(78.8526191752965,-7.79200849095004,138.779574428366));
#82804=CARTESIAN_POINT('Ctrl Pts',(78.8308736699423,-7.81298929850626,138.781668925739));
#82805=CARTESIAN_POINT('Ctrl Pts',(78.8187034532117,-7.82510034502003,138.782870699949));
#82806=CARTESIAN_POINT('Ctrl Pts',(78.7769632552624,-7.86794179975979,138.787090302782));
#82807=CARTESIAN_POINT('Ctrl Pts',(78.748389024546,-7.89961636345954,138.790154663125));
#82808=CARTESIAN_POINT('Ctrl Pts',(78.6542158893786,-8.01242624549054,138.800794974995));
#82809=CARTESIAN_POINT('Ctrl Pts',(78.5950305976655,-8.09861169058053,138.808446732508));
#82810=CARTESIAN_POINT('Ctrl Pts',(78.5148468736009,-8.24267426842422,138.82018529873));
#82811=CARTESIAN_POINT('Ctrl Pts',(78.4883035625149,-8.29715043875238,138.824416774424));
#82812=CARTESIAN_POINT('Ctrl Pts',(78.4580734001981,-8.36887655595176,138.829725783489));
#82813=CARTESIAN_POINT('Ctrl Pts',(78.4516117542697,-8.38489974774697,138.83089576422));
#82814=CARTESIAN_POINT('Ctrl Pts',(78.442394503203,-8.40882235253628,138.83261952162));
#82815=CARTESIAN_POINT('Ctrl Pts',(78.4394474475768,-8.41664622318104,138.833179667397));
#82816=CARTESIAN_POINT('Ctrl Pts',(78.4365593750041,-8.42449203992252,138.833737849951));
#82817=CARTESIAN_POINT('Origin',(80.,-9.,134.));
#82818=CARTESIAN_POINT('',(78.4365593777415,-8.42449203248626,139.531855306428));
#82819=CARTESIAN_POINT('',(78.4365593749993,-8.42449203993574,139.340802385574));
#82820=CARTESIAN_POINT('',(78.4365593749993,-8.42449203993574,134.));
#82821=CARTESIAN_POINT('',(81.2690708798523,-7.92064134695145,140.));
#82822=CARTESIAN_POINT('Ctrl Pts',(78.4365593777415,-8.42449203248626,139.531855306428));
#82823=CARTESIAN_POINT('Ctrl Pts',(78.4333404532528,-8.43323665044058,139.532424409646));
#82824=CARTESIAN_POINT('Ctrl Pts',(78.4301945868942,-8.44200910936127,139.532993870147));
#82825=CARTESIAN_POINT('Ctrl Pts',(78.419533560236,-8.47254216118274,139.534972166137));
#82826=CARTESIAN_POINT('Ctrl Pts',(78.4123963589365,-8.49443043612462,139.53638376207));
#82827=CARTESIAN_POINT('Ctrl Pts',(78.3869901806648,-8.57819727689475,139.541783446891));
#82828=CARTESIAN_POINT('Ctrl Pts',(78.3718694226088,-8.64096375128971,139.545823316546));
#82829=CARTESIAN_POINT('Ctrl Pts',(78.3584038607409,-8.71566193855221,139.550790121101));
#82830=CARTESIAN_POINT('Ctrl Pts',(78.3564963028477,-8.72690368481098,139.551541807271));
#82831=CARTESIAN_POINT('Ctrl Pts',(78.3537028346285,-8.74445694919823,139.552723318112));
#82832=CARTESIAN_POINT('Ctrl Pts',(78.3527374544938,-8.75075572163072,139.55314884938));
#82833=CARTESIAN_POINT('Ctrl Pts',(78.3510874949719,-8.76194962470796,139.553908104212));
#82834=CARTESIAN_POINT('Ctrl Pts',(78.3503885288946,-8.76684249475162,139.554241014478));
#82835=CARTESIAN_POINT('Ctrl Pts',(78.3487556593623,-8.77864783270122,139.555046693432));
#82836=CARTESIAN_POINT('Ctrl Pts',(78.3478433887019,-8.78556310529877,139.555520644395));
#82837=CARTESIAN_POINT('Ctrl Pts',(78.3451603527288,-8.80693553532605,139.556991210515));
#82838=CARTESIAN_POINT('Ctrl Pts',(78.3435357886257,-8.82140989323287,139.55799527747));
#82839=CARTESIAN_POINT('Ctrl Pts',(78.3362143639208,-8.89537946819798,139.563161766661));
#82840=CARTESIAN_POINT('Ctrl Pts',(78.3335328311396,-8.95512395476671,139.567449646769));
#82841=CARTESIAN_POINT('Ctrl Pts',(78.3350143225227,-9.12102457025296,139.579471606928));
#82842=CARTESIAN_POINT('Ctrl Pts',(78.3461055098331,-9.2268498508276,139.587254390769));
#82843=CARTESIAN_POINT('Ctrl Pts',(78.3785495197234,-9.38694126747906,139.598859494532));
#82844=CARTESIAN_POINT('Ctrl Pts',(78.3927843424843,-9.44236223395556,139.602849199311));
#82845=CARTESIAN_POINT('Ctrl Pts',(78.414967988087,-9.51334659543113,139.607921300435));
#82846=CARTESIAN_POINT('Ctrl Pts',(78.4203465767135,-9.52966622165135,139.609084890794));
#82847=CARTESIAN_POINT('Ctrl Pts',(78.4294758192753,-9.55598905041998,139.610958279747));
#82848=CARTESIAN_POINT('Ctrl Pts',(78.4330717802038,-9.56604415867437,139.611673081819));
#82849=CARTESIAN_POINT('Ctrl Pts',(78.4401816178468,-9.58533775889907,139.613043317199));
#82850=CARTESIAN_POINT('Ctrl Pts',(78.4436815065165,-9.59458088707646,139.61369917853));
#82851=CARTESIAN_POINT('Ctrl Pts',(78.4520149054745,-9.61601138314027,139.615218747307));
#82852=CARTESIAN_POINT('Ctrl Pts',(78.4569104788238,-9.62817403868894,139.616080350495));
#82853=CARTESIAN_POINT('Ctrl Pts',(78.4733198428754,-9.66759197542188,139.618871246148));
#82854=CARTESIAN_POINT('Ctrl Pts',(78.4854165423551,-9.69459950202579,139.620781023888));
#82855=CARTESIAN_POINT('Ctrl Pts',(78.5161794770682,-9.75865156375282,139.625317420193));
#82856=CARTESIAN_POINT('Ctrl Pts',(78.5355223305134,-9.79534964308775,139.627922145527));
#82857=CARTESIAN_POINT('Ctrl Pts',(78.5938125526467,-9.8965881322203,139.635181163493));
#82858=CARTESIAN_POINT('Ctrl Pts',(78.6357970808385,-9.95926234849222,139.639759744868));
#82859=CARTESIAN_POINT('Ctrl Pts',(78.7324626387119,-10.0843181441866,139.64943615499));
#82860=CARTESIAN_POINT('Ctrl Pts',(78.7878422340391,-10.145891371441,139.654528457406));
#82861=CARTESIAN_POINT('Ctrl Pts',(78.8590300667545,-10.2140824047719,139.660923745035));
#82862=CARTESIAN_POINT('Ctrl Pts',(78.8706606701187,-10.2249086118572,139.661964395625));
#82863=CARTESIAN_POINT('Ctrl Pts',(78.8877588598309,-10.2403737368211,139.66349137245));
#82864=CARTESIAN_POINT('Ctrl Pts',(78.8931047534505,-10.2451466858936,139.663968395241));
#82865=CARTESIAN_POINT('Ctrl Pts',(78.902651876943,-10.2535605298944,139.664819947933));
#82866=CARTESIAN_POINT('Ctrl Pts',(78.9068407711754,-10.2572150984051,139.665193475063));
#82867=CARTESIAN_POINT('Ctrl Pts',(78.9160225930382,-10.2651451251798,139.666012050725));
#82868=CARTESIAN_POINT('Ctrl Pts',(78.9210225264198,-10.2694119955457,139.666457661981));
#82869=CARTESIAN_POINT('Ctrl Pts',(78.9354062854157,-10.2815405124402,139.667738863739));
#82870=CARTESIAN_POINT('Ctrl Pts',(78.9448514640773,-10.289328277783,139.668579292777));
#82871=CARTESIAN_POINT('Ctrl Pts',(79.0247596891575,-10.3537483479579,139.675676174776));
#82872=CARTESIAN_POINT('Ctrl Pts',(79.0996323539212,-10.4046576322554,139.682231424069));
#82873=CARTESIAN_POINT('Ctrl Pts',(79.2831586925251,-10.5087204662582,139.697540687089));
#82874=CARTESIAN_POINT('Ctrl Pts',(79.3942290091503,-10.5566470847077,139.70623242643));
#82875=CARTESIAN_POINT('Ctrl Pts',(79.5292493320315,-10.598241575332,139.715941521078));
#82876=CARTESIAN_POINT('Ctrl Pts',(79.5490938718281,-10.6039532578404,139.717348999701));
#82877=CARTESIAN_POINT('Ctrl Pts',(79.5812738151483,-10.6125708589054,139.719600829134));
#82878=CARTESIAN_POINT('Ctrl Pts',(79.5935446215182,-10.6157074095775,139.720452417016));
#82879=CARTESIAN_POINT('Ctrl Pts',(79.6154318062779,-10.6210368758597,139.721959161735));
#82880=CARTESIAN_POINT('Ctrl Pts',(79.6250340115783,-10.6232848681485,139.722616040514));
#82881=CARTESIAN_POINT('Ctrl Pts',(79.6453625097835,-10.6278540093104,139.723998184974));
#82882=CARTESIAN_POINT('Ctrl Pts',(79.6560929535699,-10.6301547098796,139.724722774618));
#82883=CARTESIAN_POINT('Ctrl Pts',(79.6848887083222,-10.6360317814155,139.726654451821));
#82884=CARTESIAN_POINT('Ctrl Pts',(79.7029922193621,-10.6394149986532,139.727855427068));
#82885=CARTESIAN_POINT('Ctrl Pts',(79.80609941461,-10.6569197897013,139.734625618059));
#82886=CARTESIAN_POINT('Ctrl Pts',(79.8920465002447,-10.6647310559526,139.73999125171));
#82887=CARTESIAN_POINT('Ctrl Pts',(80.0471568259668,-10.6667588570442,139.749512297185));
#82888=CARTESIAN_POINT('Ctrl Pts',(80.1160802829024,-10.6633803019553,139.753688354109));
#82889=CARTESIAN_POINT('Ctrl Pts',(80.255326852766,-10.6478559797584,139.762303379854));
#82890=CARTESIAN_POINT('Ctrl Pts',(80.3254717545605,-10.6354469398585,139.766738371423));
#82891=CARTESIAN_POINT('Ctrl Pts',(80.4048523298509,-10.6160946675892,139.772083026492));
#82892=CARTESIAN_POINT('Ctrl Pts',(80.4150815615746,-10.6134976501151,139.772778121658));
#82893=CARTESIAN_POINT('Ctrl Pts',(80.4317945780882,-10.6090850720961,139.773925300364));
#82894=CARTESIAN_POINT('Ctrl Pts',(80.4382934288413,-10.6073270336747,139.774374244738));
#82895=CARTESIAN_POINT('Ctrl Pts',(80.4499604164394,-10.6040949178373,139.775185664697));
#82896=CARTESIAN_POINT('Ctrl Pts',(80.4551324609957,-10.6026351183594,139.775547309249));
#82897=CARTESIAN_POINT('Ctrl Pts',(80.4664515220898,-10.5993811248984,139.776343207569));
#82898=CARTESIAN_POINT('Ctrl Pts',(80.4725953572075,-10.5975764860549,139.776778100029));
#82899=CARTESIAN_POINT('Ctrl Pts',(80.4910290637525,-10.592046287383,139.778091308662));
#82900=CARTESIAN_POINT('Ctrl Pts',(80.5032860892827,-10.5882140939152,139.778975718084));
#82901=CARTESIAN_POINT('Ctrl Pts',(80.5316807680756,-10.5789747317609,139.781048723281));
#82902=CARTESIAN_POINT('Ctrl Pts',(80.5477820863235,-10.5734612723499,139.782242558027));
#82903=CARTESIAN_POINT('Ctrl Pts',(80.6040227226354,-10.5532353608266,139.786470410536));
#82904=CARTESIAN_POINT('Ctrl Pts',(80.6436755877561,-10.5372263174946,139.789555500521));
#82905=CARTESIAN_POINT('Ctrl Pts',(80.8031867408985,-10.4655727008004,139.802285631473));
#82906=CARTESIAN_POINT('Ctrl Pts',(80.916861725362,-10.3972782344416,139.812067228599));
#82907=CARTESIAN_POINT('Ctrl Pts',(81.0569037537876,-10.2886209102246,139.824567590418));
#82908=CARTESIAN_POINT('Ctrl Pts',(81.09139649508,-10.2595411021694,139.827694743806));
#82909=CARTESIAN_POINT('Ctrl Pts',(81.1360059875825,-10.218721668253,139.831808648112));
#82910=CARTESIAN_POINT('Ctrl Pts',(81.1471984318728,-10.2081919942998,139.832847146247));
#82911=CARTESIAN_POINT('Ctrl Pts',(81.1654081336394,-10.1905793642854,139.8345478695));
#82912=CARTESIAN_POINT('Ctrl Pts',(81.1725101327028,-10.1835857962451,139.835214050844));
#82913=CARTESIAN_POINT('Ctrl Pts',(81.1862643397577,-10.1697962802914,139.836510136405));
#82914=CARTESIAN_POINT('Ctrl Pts',(81.1929219523482,-10.1630062955044,139.837140275669));
#82915=CARTESIAN_POINT('Ctrl Pts',(81.2085741248112,-10.1467670900775,139.838628692959));
#82916=CARTESIAN_POINT('Ctrl Pts',(81.2175166437438,-10.1372683996353,139.839484625874));
#82917=CARTESIAN_POINT('Ctrl Pts',(81.2476218982996,-10.1045286482221,139.842386641424));
#82918=CARTESIAN_POINT('Ctrl Pts',(81.2682389071128,-10.0807933287107,139.844409213305));
#82919=CARTESIAN_POINT('Ctrl Pts',(81.317167239161,-10.0211351116341,139.849315314171));
#82920=CARTESIAN_POINT('Ctrl Pts',(81.3446951156404,-9.9846024383433,139.852169779538));
#82921=CARTESIAN_POINT('Ctrl Pts',(81.409852720479,-9.89029153035011,139.859248722404));
#82922=CARTESIAN_POINT('Ctrl Pts',(81.4454646417108,-9.8312255412782,139.863425417562));
#82923=CARTESIAN_POINT('Ctrl Pts',(81.4839812445956,-9.75733976711819,139.868518094815));
#82924=CARTESIAN_POINT('Ctrl Pts',(81.4904794658724,-9.74446948335571,139.869400718296));
#82925=CARTESIAN_POINT('Ctrl Pts',(81.5285336112064,-9.66660410584125,139.874722682628));
#82926=CARTESIAN_POINT('Ctrl Pts',(81.5559972010636,-9.59970490934644,139.87921868466));
#82927=CARTESIAN_POINT('Ctrl Pts',(81.582651234163,-9.52048060172039,139.884691847716));
#82928=CARTESIAN_POINT('Ctrl Pts',(81.5861624602782,-9.50967991654074,139.885441157944));
#82929=CARTESIAN_POINT('Ctrl Pts',(81.5914414359383,-9.49285851692904,139.886614321777));
#82930=CARTESIAN_POINT('Ctrl Pts',(81.593286137095,-9.48686203767098,139.887033737411));
#82931=CARTESIAN_POINT('Ctrl Pts',(81.5966781112051,-9.47561015774045,139.887823253749));
#82932=CARTESIAN_POINT('Ctrl Pts',(81.5982334227164,-9.47035724404381,139.888192863062));
#82933=CARTESIAN_POINT('Ctrl Pts',(81.6017740074708,-9.45817892996487,139.889051990876));
#82934=CARTESIAN_POINT('Ctrl Pts',(81.6037403070411,-9.4512481862311,139.889542587414));
#82935=CARTESIAN_POINT('Ctrl Pts',(81.6096079798025,-9.43004316939073,139.891048240973));
#82936=CARTESIAN_POINT('Ctrl Pts',(81.613364050977,-9.41572993291234,139.892070949335));
#82937=CARTESIAN_POINT('Ctrl Pts',(81.6219042834181,-9.38132533032869,139.894541696425));
#82938=CARTESIAN_POINT('Ctrl Pts',(81.6265063838393,-9.36119165346352,139.89599768361));
#82939=CARTESIAN_POINT('Ctrl Pts',(81.6422617977123,-9.28584128035031,139.901472849812));
#82940=CARTESIAN_POINT('Ctrl Pts',(81.6509861812045,-9.23015824787884,139.90556977086));
#82941=CARTESIAN_POINT('Ctrl Pts',(81.6677889480927,-9.07029076048419,139.917325727882));
#82942=CARTESIAN_POINT('Ctrl Pts',(81.6689168362063,-8.96562969149369,139.924999074863));
#82943=CARTESIAN_POINT('Ctrl Pts',(81.6551768070528,-8.800869347878,139.936777989476));
#82944=CARTESIAN_POINT('Ctrl Pts',(81.6467937830021,-8.74051000832748,139.941032702189));
#82945=CARTESIAN_POINT('Ctrl Pts',(81.6315698865677,-8.662539577122,139.946457704903));
#82946=CARTESIAN_POINT('Ctrl Pts',(81.6277127861067,-8.64440055848037,139.947714881212));
#82947=CARTESIAN_POINT('Ctrl Pts',(81.6209329203193,-8.61494288553508,139.949749699927));
#82948=CARTESIAN_POINT('Ctrl Pts',(81.6181925528292,-8.60358432602193,139.950532639646));
#82949=CARTESIAN_POINT('Ctrl Pts',(81.6126529634537,-8.58163853294764,139.95204256836));
#82950=CARTESIAN_POINT('Ctrl Pts',(81.6098684122609,-8.57104825252114,139.952769942825));
#82951=CARTESIAN_POINT('Ctrl Pts',(81.6030790560553,-8.54622456803031,139.954472453299));
#82952=CARTESIAN_POINT('Ctrl Pts',(81.5989887458851,-8.53201537012094,139.95544506176));
#82953=CARTESIAN_POINT('Ctrl Pts',(81.5845145593896,-8.48414083252938,139.958717660399));
#82954=CARTESIAN_POINT('Ctrl Pts',(81.5732519240165,-8.45074988184117,139.960992615474));
#82955=CARTESIAN_POINT('Ctrl Pts',(81.5311907017559,-8.33799111482543,139.968685337612));
#82956=CARTESIAN_POINT('Ctrl Pts',(81.4953746470215,-8.2606377492648,139.973974787409));
#82957=CARTESIAN_POINT('Ctrl Pts',(81.4131957273197,-8.11380195118367,139.984466512586));
#82958=CARTESIAN_POINT('Ctrl Pts',(81.3672181484585,-8.0443948701926,139.989655600748));
#82959=CARTESIAN_POINT('Ctrl Pts',(81.3076666935999,-7.96764335815803,139.995977687977));
#82960=CARTESIAN_POINT('Ctrl Pts',(81.2989362273536,-7.95667978529728,139.996895849814));
#82961=CARTESIAN_POINT('Ctrl Pts',(81.286298471537,-7.94121402256193,139.998214628889));
#82962=CARTESIAN_POINT('Ctrl Pts',(81.2825035135694,-7.93662036906806,139.998609354866));
#82963=CARTESIAN_POINT('Ctrl Pts',(81.2754966558533,-7.92823089946848,139.999336000877));
#82964=CARTESIAN_POINT('Ctrl Pts',(81.2722922328498,-7.92442889733726,139.999667500718));
#82965=CARTESIAN_POINT('Ctrl Pts',(81.2690708798523,-7.92064134695143,140.));
#82966=CARTESIAN_POINT('',(78.7475353758638,-7.90141528989,140.));
#82967=CARTESIAN_POINT('Origin',(80.,-9.,140.));
#82968=CARTESIAN_POINT('Ctrl Pts',(78.7475353758638,-7.90141528989007,140.));
#82969=CARTESIAN_POINT('Ctrl Pts',(78.7493539374217,-7.89934200050503,139.999810165109));
#82970=CARTESIAN_POINT('Ctrl Pts',(78.7511776339592,-7.89727324164226,139.999620003453));
#82971=CARTESIAN_POINT('Ctrl Pts',(78.7714683906298,-7.87437077097766,139.99750663889));
#82972=CARTESIAN_POINT('Ctrl Pts',(78.7904485659617,-7.85399991429323,139.995551875342));
#82973=CARTESIAN_POINT('Ctrl Pts',(78.8893648755144,-7.75303154664668,139.985514608203));
#82974=CARTESIAN_POINT('Ctrl Pts',(78.9768777152484,-7.68027976303666,139.977138092156));
#82975=CARTESIAN_POINT('Ctrl Pts',(79.142409596094,-7.56910092884384,139.962753900001));
#82976=CARTESIAN_POINT('Ctrl Pts',(79.2173174159119,-7.52679071308032,139.956681272142));
#82977=CARTESIAN_POINT('Ctrl Pts',(79.3118446016702,-7.48265463169636,139.949554808457));
#82978=CARTESIAN_POINT('Ctrl Pts',(79.3286516293955,-7.47514386544472,139.948306776368));
#82979=CARTESIAN_POINT('Ctrl Pts',(79.3556723006463,-7.46360218460404,139.94632971417));
#82980=CARTESIAN_POINT('Ctrl Pts',(79.3658068692669,-7.45939118718801,139.945594676906));
#82981=CARTESIAN_POINT('Ctrl Pts',(79.3851293206591,-7.45158553196245,139.944205258331));
#82982=CARTESIAN_POINT('Ctrl Pts',(79.3943089232454,-7.44797176451418,139.943550264081));
#82983=CARTESIAN_POINT('Ctrl Pts',(79.4153537960536,-7.43990210610232,139.942059914676));
#82984=CARTESIAN_POINT('Ctrl Pts',(79.4272389915304,-7.43549961199141,139.941226347614));
#82985=CARTESIAN_POINT('Ctrl Pts',(79.4586396099145,-7.42427404545535,139.939044453311));
#82986=CARTESIAN_POINT('Ctrl Pts',(79.4782341544611,-7.417677713767,139.937703460455));
#82987=CARTESIAN_POINT('Ctrl Pts',(79.6370652727423,-7.36748004867061,139.926983720903));
#82988=CARTESIAN_POINT('Ctrl Pts',(79.7813497621902,-7.34197805747743,139.918238931225));
#82989=CARTESIAN_POINT('Ctrl Pts',(79.988096548862,-7.33292471575854,139.905450729332));
#82990=CARTESIAN_POINT('Ctrl Pts',(80.0491711394147,-7.33360798749068,139.901630822285));
#82991=CARTESIAN_POINT('Ctrl Pts',(80.1248019355846,-7.33861544217696,139.896701509358));
#82992=CARTESIAN_POINT('Ctrl Pts',(80.1395260822402,-7.33978717976292,139.895732384367));
#82993=CARTESIAN_POINT('Ctrl Pts',(80.1598973328611,-7.34168120815393,139.89437603223));
#82994=CARTESIAN_POINT('Ctrl Pts',(80.1655597417161,-7.34223694634459,139.893997352313));
#82995=CARTESIAN_POINT('Ctrl Pts',(80.1713966207971,-7.34284001067116,139.893605180919));
#82996=CARTESIAN_POINT('Ctrl Pts',(80.1715741468675,-7.34285838143518,139.89359325146));
#82997=CARTESIAN_POINT('Ctrl Pts',(80.1719290400283,-7.34289516415132,139.89356939974));
#82998=CARTESIAN_POINT('Ctrl Pts',(80.1721064070974,-7.34291357605161,139.893557477482));
#82999=CARTESIAN_POINT('Ctrl Pts',(80.1724636059533,-7.34295071367453,139.893533463782));
#83000=CARTESIAN_POINT('Ctrl Pts',(80.1726434376896,-7.34296944019948,139.893521372293));
#83001=CARTESIAN_POINT('Ctrl Pts',(80.1730086392265,-7.34300753004428,139.8934968133));
#83002=CARTESIAN_POINT('Ctrl Pts',(80.1731940087945,-7.34302689519276,139.8934843457));
#83003=CARTESIAN_POINT('Ctrl Pts',(80.1735741281947,-7.34306666990928,139.893458775678));
#83004=CARTESIAN_POINT('Ctrl Pts',(80.1737688776887,-7.34308708270748,139.893445673082));
#83005=CARTESIAN_POINT('Ctrl Pts',(80.1741729016833,-7.34312950276752,139.893418486269));
#83006=CARTESIAN_POINT('Ctrl Pts',(80.1743821755901,-7.34315151534109,139.893404401766));
#83007=CARTESIAN_POINT('Ctrl Pts',(80.1748226712495,-7.34319793346448,139.893374750478));
#83008=CARTESIAN_POINT('Ctrl Pts',(80.1750538920419,-7.3432223477666,139.893359183218));
#83009=CARTESIAN_POINT('Ctrl Pts',(80.1755499662663,-7.34327483260521,139.893325777907));
#83010=CARTESIAN_POINT('Ctrl Pts',(80.1758148180392,-7.34330291824578,139.893307939033));
#83011=CARTESIAN_POINT('Ctrl Pts',(80.1763987565177,-7.34336498236033,139.893268599647));
#83012=CARTESIAN_POINT('Ctrl Pts',(80.1767178400715,-7.34339898950561,139.893247097567));
#83013=CARTESIAN_POINT('Ctrl Pts',(80.1774533982222,-7.34347759843096,139.89319751729));
#83014=CARTESIAN_POINT('Ctrl Pts',(80.1778698656223,-7.34352226506263,139.893169435538));
#83015=CARTESIAN_POINT('Ctrl Pts',(80.1786060166775,-7.34360149897452,139.893119780657));
#83016=CARTESIAN_POINT('Ctrl Pts',(80.1789257074836,-7.34363600178163,139.893098211078));
#83017=CARTESIAN_POINT('Ctrl Pts',(80.1845660015237,-7.34424638561685,139.892717557303));
#83018=CARTESIAN_POINT('Ctrl Pts',(80.1898835646255,-7.34484778045083,139.892357056154));
#83019=CARTESIAN_POINT('Ctrl Pts',(80.202241442798,-7.34630574251937,139.891515478632));
#83020=CARTESIAN_POINT('Ctrl Pts',(80.2092791952211,-7.34718164570595,139.891033373285));
#83021=CARTESIAN_POINT('Ctrl Pts',(80.2320080471498,-7.35015791997912,139.889467683694));
#83022=CARTESIAN_POINT('Ctrl Pts',(80.2476743224481,-7.35243694878018,139.888375082349));
#83023=CARTESIAN_POINT('Ctrl Pts',(80.3436670236751,-7.36780133731417,139.88160715832));
#83024=CARTESIAN_POINT('Ctrl Pts',(80.4229709614544,-7.386534002239,139.875705596791));
#83025=CARTESIAN_POINT('Ctrl Pts',(80.5733653283458,-7.43391200677015,139.86423832153));
#83026=CARTESIAN_POINT('Ctrl Pts',(80.6444937978286,-7.46181645134146,139.858687852615));
#83027=CARTESIAN_POINT('Ctrl Pts',(80.7511590581591,-7.51236554098703,139.850279500871));
#83028=CARTESIAN_POINT('Ctrl Pts',(80.7881741408623,-7.53164097920583,139.847343477006));
#83029=CARTESIAN_POINT('Ctrl Pts',(80.8502528406159,-7.56699294134065,139.842392437584));
#83030=CARTESIAN_POINT('Ctrl Pts',(80.8756797404288,-7.58238781401237,139.840356228927));
#83031=CARTESIAN_POINT('Ctrl Pts',(80.9117323051127,-7.60555648306264,139.837455245878));
#83032=CARTESIAN_POINT('Ctrl Pts',(80.92269787575,-7.61278798835659,139.83657096411));
#83033=CARTESIAN_POINT('Ctrl Pts',(80.9417675197182,-7.62569008931478,139.835029367443));
#83034=CARTESIAN_POINT('Ctrl Pts',(80.9499086298742,-7.63130449189569,139.834370000928));
#83035=CARTESIAN_POINT('Ctrl Pts',(80.9667309752048,-7.64312818410487,139.833004693084));
#83036=CARTESIAN_POINT('Ctrl Pts',(80.9754035235131,-7.64934909084074,139.832299231685));
#83037=CARTESIAN_POINT('Ctrl Pts',(80.9978512458042,-7.66578005352087,139.830468599966));
#83038=CARTESIAN_POINT('Ctrl Pts',(81.011529865795,-7.67612034519384,139.829348479924));
#83039=CARTESIAN_POINT('Ctrl Pts',(81.0706009549604,-7.72222501529789,139.824486973085));
#83040=CARTESIAN_POINT('Ctrl Pts',(81.1142773684257,-7.7601280995592,139.82083041753));
#83041=CARTESIAN_POINT('Ctrl Pts',(81.2321348644005,-7.87367583325694,139.810639881814));
#83042=CARTESIAN_POINT('Ctrl Pts',(81.301194414478,-7.95422028329682,139.804277854754));
#83043=CARTESIAN_POINT('Ctrl Pts',(81.3964412667812,-8.08947486500636,139.794065804642));
#83044=CARTESIAN_POINT('Ctrl Pts',(81.428097786748,-8.13997707231692,139.790337199806));
#83045=CARTESIAN_POINT('Ctrl Pts',(81.4640323750513,-8.20477881642482,139.785517398176));
#83046=CARTESIAN_POINT('Ctrl Pts',(81.4709184258613,-8.21758931795455,139.784562892861));
#83047=CARTESIAN_POINT('Ctrl Pts',(81.4808560567645,-8.23667179246633,139.783136125072));
#83048=CARTESIAN_POINT('Ctrl Pts',(81.4840375926609,-8.24287581434837,139.782671497275));
#83049=CARTESIAN_POINT('Ctrl Pts',(81.4894081394236,-8.25351233634473,139.781873301335));
#83050=CARTESIAN_POINT('Ctrl Pts',(81.491616518262,-8.25793490886457,139.781540938579));
#83051=CARTESIAN_POINT('Ctrl Pts',(81.4966290701098,-8.2680859999423,139.780776879659));
#83052=CARTESIAN_POINT('Ctrl Pts',(81.4994199852038,-8.27382069602188,139.78034440212));
#83053=CARTESIAN_POINT('Ctrl Pts',(81.5071171990913,-8.28987028125186,139.779132004655));
#83054=CARTESIAN_POINT('Ctrl Pts',(81.5119503355289,-8.30021958151238,139.778347884258));
#83055=CARTESIAN_POINT('Ctrl Pts',(81.5437425051465,-8.37016395834686,139.773036908064));
#83056=CARTESIAN_POINT('Ctrl Pts',(81.5672753021543,-8.43124647300328,139.768344596779));
#83057=CARTESIAN_POINT('Ctrl Pts',(81.5936445312741,-8.51388391484801,139.76205551411));
#83058=CARTESIAN_POINT('Ctrl Pts',(81.5997426392731,-8.53434432298382,139.760502821396));
#83059=CARTESIAN_POINT('Ctrl Pts',(81.6236911077188,-8.62072795225309,139.753977179407));
#83060=CARTESIAN_POINT('Ctrl Pts',(81.6378733378574,-8.68760290840882,139.749001061225));
#83061=CARTESIAN_POINT('Ctrl Pts',(81.658428839337,-8.82595425033272,139.738979311701));
#83062=CARTESIAN_POINT('Ctrl Pts',(81.6643753463769,-8.89735807836616,139.733952586272));
#83063=CARTESIAN_POINT('Ctrl Pts',(81.6660363813183,-8.98641542707321,139.727874803751));
#83064=CARTESIAN_POINT('Ctrl Pts',(81.6660872038639,-9.00390311487463,139.726690230643));
#83065=CARTESIAN_POINT('Ctrl Pts',(81.6657257179225,-9.03205716930825,139.724796787155));
#83066=CARTESIAN_POINT('Ctrl Pts',(81.6654862641975,-9.042724026385,139.724082559602));
#83067=CARTESIAN_POINT('Ctrl Pts',(81.6648321378074,-9.06312586766012,139.722722273661));
#83068=CARTESIAN_POINT('Ctrl Pts',(81.6644345034237,-9.07286091527993,139.722075709121));
#83069=CARTESIAN_POINT('Ctrl Pts',(81.6633310817852,-9.09509113086167,139.720604732979));
#83070=CARTESIAN_POINT('Ctrl Pts',(81.6625698515538,-9.10758305536424,139.719782094138));
#83071=CARTESIAN_POINT('Ctrl Pts',(81.6596923497431,-9.1474067527764,139.717171187968));
#83072=CARTESIAN_POINT('Ctrl Pts',(81.6570421866931,-9.17469624225397,139.715399629821));
#83073=CARTESIAN_POINT('Ctrl Pts',(81.6376675935821,-9.33338213563908,139.705176503311));
#83074=CARTESIAN_POINT('Ctrl Pts',(81.6059960250623,-9.46246963972847,139.697221498124));
#83075=CARTESIAN_POINT('Ctrl Pts',(81.5340375636779,-9.65380674706418,139.684692600514));
#83076=CARTESIAN_POINT('Ctrl Pts',(81.5043714871238,-9.71944321177551,139.680236223466));
#83077=CARTESIAN_POINT('Ctrl Pts',(81.4631342160772,-9.79689645532444,139.674544848725));
#83078=CARTESIAN_POINT('Ctrl Pts',(81.4555103463818,-9.8107374923517,139.67351001607));
#83079=CARTESIAN_POINT('Ctrl Pts',(81.4441457382448,-9.83069272989906,139.671988907977));
#83080=CARTESIAN_POINT('Ctrl Pts',(81.4405603271241,-9.83689501371369,139.67151197667));
#83081=CARTESIAN_POINT('Ctrl Pts',(81.4341711126735,-9.84778479128826,139.67066689137));
#83082=CARTESIAN_POINT('Ctrl Pts',(81.4313840996893,-9.8524819002305,139.670299812345));
#83083=CARTESIAN_POINT('Ctrl Pts',(81.4252633112822,-9.86268296529061,139.66949693088));
#83084=CARTESIAN_POINT('Ctrl Pts',(81.4219207676737,-9.8681812783333,139.669060589968));
#83085=CARTESIAN_POINT('Ctrl Pts',(81.4124587001724,-9.88354467303419,139.667831556611));
#83086=CARTESIAN_POINT('Ctrl Pts',(81.4062679313666,-9.89336512989974,139.667034518386));
#83087=CARTESIAN_POINT('Ctrl Pts',(81.3582665633542,-9.96777467357826,139.660912350089));
#83088=CARTESIAN_POINT('Ctrl Pts',(81.3121335585872,-10.0294555433507,139.655360272685));
#83089=CARTESIAN_POINT('Ctrl Pts',(81.224574894705,-10.1310360235524,139.64561226723));
#83090=CARTESIAN_POINT('Ctrl Pts',(81.1850326540324,-10.1724009684961,139.641439164999));
#83091=CARTESIAN_POINT('Ctrl Pts',(81.0831203649265,-10.2685761049912,139.631312567974));
#83092=CARTESIAN_POINT('Ctrl Pts',(81.0186258244716,-10.3209239592282,139.625422222657));
#83093=CARTESIAN_POINT('Ctrl Pts',(80.9316990406666,-10.3813096806829,139.61814547709));
#83094=CARTESIAN_POINT('Ctrl Pts',(80.9126396640306,-10.3939757781732,139.616586736671));
#83095=CARTESIAN_POINT('Ctrl Pts',(80.88332798228,-10.4125961682517,139.614243379646));
#83096=CARTESIAN_POINT('Ctrl Pts',(80.8732637576959,-10.4188399067106,139.613448152337));
#83097=CARTESIAN_POINT('Ctrl Pts',(80.8556259343521,-10.4295234538503,139.612070402855));
#83098=CARTESIAN_POINT('Ctrl Pts',(80.8480823472263,-10.4340116394292,139.611486132631));
#83099=CARTESIAN_POINT('Ctrl Pts',(80.8309899761645,-10.4439989849271,139.610173280854));
#83100=CARTESIAN_POINT('Ctrl Pts',(80.8214213359579,-10.4494634895677,139.60944596923));
#83101=CARTESIAN_POINT('Ctrl Pts',(80.7952964116793,-10.4640412386552,139.607480322099));
#83102=CARTESIAN_POINT('Ctrl Pts',(80.7786378300618,-10.4729685358751,139.606248601722));
#83103=CARTESIAN_POINT('Ctrl Pts',(80.6672862837081,-10.5302244591373,139.598149482522));
#83104=CARTESIAN_POINT('Ctrl Pts',(80.5683018071055,-10.5696799064406,139.591605797225));
#83105=CARTESIAN_POINT('Ctrl Pts',(80.3868728384437,-10.6225647751614,139.580054269002));
#83106=CARTESIAN_POINT('Ctrl Pts',(80.3059193113103,-10.6397556394334,139.575038406747));
#83107=CARTESIAN_POINT('Ctrl Pts',(80.1867389325085,-10.6559290088295,139.567459809341));
#83108=CARTESIAN_POINT('Ctrl Pts',(80.1492892276118,-10.6597242386087,139.565050148035));
#83109=CARTESIAN_POINT('Ctrl Pts',(80.1018887090753,-10.6629107935685,139.56192866627));
#83110=CARTESIAN_POINT('Ctrl Pts',(80.0920254534338,-10.6634857740933,139.561275235901));
#83111=CARTESIAN_POINT('Ctrl Pts',(80.0761657650853,-10.6642688395286,139.560217438356));
#83112=CARTESIAN_POINT('Ctrl Pts',(80.0701721292605,-10.664532325736,139.55981604875));
#83113=CARTESIAN_POINT('Ctrl Pts',(80.0586142721602,-10.6649778859173,139.559038658183));
#83114=CARTESIAN_POINT('Ctrl Pts',(80.0530503747249,-10.6651644505984,139.558662903994));
#83115=CARTESIAN_POINT('Ctrl Pts',(80.0406583130797,-10.6655178035376,139.557822758591));
#83116=CARTESIAN_POINT('Ctrl Pts',(80.0338298527203,-10.6656704924212,139.55735761325));
#83117=CARTESIAN_POINT('Ctrl Pts',(80.0135582978902,-10.6659990758735,139.555970603341));
#83118=CARTESIAN_POINT('Ctrl Pts',(80.0001141668264,-10.666054232988,139.555042724803));
#83119=CARTESIAN_POINT('Ctrl Pts',(79.8797192190196,-10.6650909972192,139.546670132137));
#83120=CARTESIAN_POINT('Ctrl Pts',(79.7731070624113,-10.6539381911227,139.538826489691));
#83121=CARTESIAN_POINT('Ctrl Pts',(79.5948262185852,-10.6177183907781,139.525604967858));
#83122=CARTESIAN_POINT('Ctrl Pts',(79.5224286645308,-10.5978442683703,139.520201217202));
#83123=CARTESIAN_POINT('Ctrl Pts',(79.4098980719767,-10.5586170294244,139.511825874485));
#83124=CARTESIAN_POINT('Ctrl Pts',(79.3687777189582,-10.5424222471287,139.508769413966));
#83125=CARTESIAN_POINT('Ctrl Pts',(79.3144780077489,-10.5185009892293,139.504736806741));
#83126=CARTESIAN_POINT('Ctrl Pts',(79.3006933409563,-10.51220232744,139.50371331105));
#83127=CARTESIAN_POINT('Ctrl Pts',(79.2777614702244,-10.5013433675697,139.502010535763));
#83128=CARTESIAN_POINT('Ctrl Pts',(79.268567060679,-10.4968855215201,139.501327784579));
#83129=CARTESIAN_POINT('Ctrl Pts',(79.250511446633,-10.4879252950346,139.4999867176));
#83130=CARTESIAN_POINT('Ctrl Pts',(79.2416483802354,-10.4834276535451,139.499328271847));
#83131=CARTESIAN_POINT('Ctrl Pts',(79.2201831894907,-10.4722922929816,139.497732909068));
#83132=CARTESIAN_POINT('Ctrl Pts',(79.2076247658292,-10.4655716846842,139.496798942487));
#83133=CARTESIAN_POINT('Ctrl Pts',(79.1648496281197,-10.4419701014166,139.493614107054));
#83134=CARTESIAN_POINT('Ctrl Pts',(79.1350724031962,-10.4243084060242,139.49139090862));
#83135=CARTESIAN_POINT('Ctrl Pts',(79.0013682029356,-10.339263981473,139.481338055479));
#83136=CARTESIAN_POINT('Ctrl Pts',(78.9046097132845,-10.2613544837943,139.473895916739));
#83137=CARTESIAN_POINT('Ctrl Pts',(78.7643378022569,-10.1199844952839,139.461665141977));
#83138=CARTESIAN_POINT('Ctrl Pts',(78.7149912630022,-10.0630032548102,139.456984431318));
#83139=CARTESIAN_POINT('Ctrl Pts',(78.6626901949287,-9.99362621672947,139.451299624925));
#83140=CARTESIAN_POINT('Ctrl Pts',(78.655804128079,-9.984290613936,139.450534889118));
#83141=CARTESIAN_POINT('Ctrl Pts',(78.6452925823987,-9.96972383101064,139.44934067692));
#83142=CARTESIAN_POINT('Ctrl Pts',(78.6415984885356,-9.96454228835086,139.448915699367));
#83143=CARTESIAN_POINT('Ctrl Pts',(78.6347703390119,-9.95484771667766,139.448119969966));
#83144=CARTESIAN_POINT('Ctrl Pts',(78.6316288152713,-9.95034019526756,139.447749729091));
#83145=CARTESIAN_POINT('Ctrl Pts',(78.6244222472155,-9.93989025030038,139.446890838975));
#83146=CARTESIAN_POINT('Ctrl Pts',(78.6203733753413,-9.93393694020989,139.446401145726));
#83147=CARTESIAN_POINT('Ctrl Pts',(78.607628919214,-9.91493424557989,139.44483732186));
#83148=CARTESIAN_POINT('Ctrl Pts',(78.5990792227414,-9.90178868475456,139.443754406159));
#83149=CARTESIAN_POINT('Ctrl Pts',(78.5460195224288,-9.81763106810065,139.436824197599));
#83150=CARTESIAN_POINT('Ctrl Pts',(78.5067396813834,-9.74347208501618,139.430735165811));
#83151=CARTESIAN_POINT('Ctrl Pts',(78.4427471723247,-9.59692053708474,139.41909468941));
#83152=CARTESIAN_POINT('Ctrl Pts',(78.4171005623256,-9.52514896290282,139.413558127237));
#83153=CARTESIAN_POINT('Ctrl Pts',(78.3854031808042,-9.4126648612746,139.405238430763));
#83154=CARTESIAN_POINT('Ctrl Pts',(78.375796006304,-9.37306435634014,139.402373508329));
#83155=CARTESIAN_POINT('Ctrl Pts',(78.3618144405452,-9.30455795812348,139.39753025958));
#83156=CARTESIAN_POINT('Ctrl Pts',(78.3567311832555,-9.27581743740151,139.395531716406));
#83157=CARTESIAN_POINT('Ctrl Pts',(78.3504789830638,-9.23410527786678,139.392677437512));
#83158=CARTESIAN_POINT('Ctrl Pts',(78.348703093463,-9.22123157442661,139.391802816204));
#83159=CARTESIAN_POINT('Ctrl Pts',(78.3458501729191,-9.19859694577888,139.390275725099));
#83160=CARTESIAN_POINT('Ctrl Pts',(78.3447084900745,-9.18884496703559,139.389621251908));
#83161=CARTESIAN_POINT('Ctrl Pts',(78.3425106384797,-9.16851696823571,139.388263968104));
#83162=CARTESIAN_POINT('Ctrl Pts',(78.3414693272939,-9.15793976280069,139.387561652264));
#83163=CARTESIAN_POINT('Ctrl Pts',(78.3390131582086,-9.13027871935646,139.385734751878));
#83164=CARTESIAN_POINT('Ctrl Pts',(78.337760598814,-9.11318145650967,139.384615269562));
#83165=CARTESIAN_POINT('Ctrl Pts',(78.333402259759,-9.03772492201462,139.379713473445));
#83166=CARTESIAN_POINT('Ctrl Pts',(78.3331042642608,-8.97924171468461,139.376018617256));
#83167=CARTESIAN_POINT('Ctrl Pts',(78.3408870781395,-8.81559126377517,139.365826235957));
#83168=CARTESIAN_POINT('Ctrl Pts',(78.3558698957589,-8.71103966773445,139.359496202171));
#83169=CARTESIAN_POINT('Ctrl Pts',(78.3957049617281,-8.54622470714689,139.349030076711));
#83170=CARTESIAN_POINT('Ctrl Pts',(78.4143720525308,-8.48477518134467,139.345008201278));
#83171=CARTESIAN_POINT('Ctrl Pts',(78.4365419168178,-8.42453946871522,139.340805694646));
#83172=CARTESIAN_POINT('Ctrl Pts',(78.4365506456816,-8.42451575423836,139.340804040149));
#83173=CARTESIAN_POINT('Ctrl Pts',(78.4365593749993,-8.42449203993574,139.340802385574));
#83174=CARTESIAN_POINT('Origin',(-1.54592528053767,-30.,55.));
#83175=CARTESIAN_POINT('',(9.49394873724561,-31.2520475724682,56.6292251037768));
#83176=CARTESIAN_POINT('',(9.55204617751071,-31.254042933277,56.631836765028));
#83177=CARTESIAN_POINT('',(-1.54592528053767,-31.2520475724682,56.6292251037768));
#83178=CARTESIAN_POINT('',(10.,-27.9466241674713,54.9248651020699));
#83179=CARTESIAN_POINT('Ctrl Pts',(9.55204617751071,-31.254042933277,56.631836765028));
#83180=CARTESIAN_POINT('Ctrl Pts',(9.5531837572224,-31.2706395868589,56.6191575655763));
#83181=CARTESIAN_POINT('Ctrl Pts',(9.5913664272136,-31.8206121569964,56.184448873392));
#83182=CARTESIAN_POINT('Ctrl Pts',(9.66659418748433,-32.4128254657117,54.7282396369248));
#83183=CARTESIAN_POINT('Ctrl Pts',(9.77772945832288,-31.081050325948,52.8236098971708));
#83184=CARTESIAN_POINT('Ctrl Pts',(9.88886472916145,-28.7562331488978,52.91517862984));
#83185=CARTESIAN_POINT('Ctrl Pts',(9.96295490972048,-27.9716077196437,54.242084880697));
#83186=CARTESIAN_POINT('Ctrl Pts',(10.,-27.9466241674713,54.9248651020699));
#83187=CARTESIAN_POINT('',(9.99999281491357,-28.1818141229585,55.9591738002264));
#83188=CARTESIAN_POINT('Origin',(10.,-30.,55.));
#83189=CARTESIAN_POINT('',(9.9459252805888,-27.9452500000283,55.0000107795145));
#83190=CARTESIAN_POINT('Ctrl Pts',(9.9459252805888,-27.9452500000283,55.0000107795145));
#83191=CARTESIAN_POINT('Ctrl Pts',(9.94992922500024,-27.9452503895637,55.0742625308859));
#83192=CARTESIAN_POINT('Ctrl Pts',(9.95393316941168,-27.9492798952893,55.1484430447576));
#83193=CARTESIAN_POINT('Ctrl Pts',(9.95793711382313,-27.9572896739692,55.222108276359));
#83194=CARTESIAN_POINT('Ctrl Pts',(9.96195101270092,-27.9653193662803,55.295956651879));
#83195=CARTESIAN_POINT('Ctrl Pts',(9.96596491157871,-27.9773490514669,55.3692867586229));
#83196=CARTESIAN_POINT('Ctrl Pts',(9.9699788104565,-27.9932783699437,55.4416626110102));
#83197=CARTESIAN_POINT('Ctrl Pts',(9.97399811839586,-28.009229154498,55.5141359958598));
#83198=CARTESIAN_POINT('Ctrl Pts',(9.97801742633522,-28.0290899299268,55.5856521509838));
#83199=CARTESIAN_POINT('Ctrl Pts',(9.98203673427458,-28.0527106422095,55.6557909114464));
#83200=CARTESIAN_POINT('Ctrl Pts',(9.98606633320141,-28.0763918326784,55.7261092543437));
#83201=CARTESIAN_POINT('Ctrl Pts',(9.99009593212824,-28.1038520364647,55.7950427573651));
#83202=CARTESIAN_POINT('Ctrl Pts',(9.99412553105508,-28.1348932435125,55.8621915966911));
#83203=CARTESIAN_POINT('Ctrl Pts',(9.9960804898642,-28.1499528765593,55.8947688375892));
#83204=CARTESIAN_POINT('Ctrl Pts',(9.99803544867332,-28.1658546891076,55.9269264110958));
#83205=CARTESIAN_POINT('Ctrl Pts',(9.99999040748243,-28.1825723553983,55.9586210508524));
#83206=CARTESIAN_POINT('Ctrl Pts',(9.49394873724561,-31.2520475724682,56.6292251037768));
#83207=CARTESIAN_POINT('Ctrl Pts',(9.49780465159691,-31.3085979756072,56.5857665327002));
#83208=CARTESIAN_POINT('Ctrl Pts',(9.50166056594821,-31.3628989655048,56.5393479980115));
#83209=CARTESIAN_POINT('Ctrl Pts',(9.50551648029951,-31.4146337209008,56.4902378998638));
#83210=CARTESIAN_POINT('Ctrl Pts',(9.50937266007019,-31.4663720374253,56.4411244212542));
#83211=CARTESIAN_POINT('Ctrl Pts',(9.51322883984087,-31.515543418208,56.3893193473735));
#83212=CARTESIAN_POINT('Ctrl Pts',(9.51708501961154,-31.56186724767,56.3351285567898));
#83213=CARTESIAN_POINT('Ctrl Pts',(9.52094529470732,-31.6082402737858,56.2808802147127));
#83214=CARTESIAN_POINT('Ctrl Pts',(9.52480556980309,-31.651759396774,56.2242414689498));
#83215=CARTESIAN_POINT('Ctrl Pts',(9.52866584489886,-31.692184336313,56.1655512577476));
#83216=CARTESIAN_POINT('Ctrl Pts',(9.53252840685189,-31.7326332239033,56.1068262780038));
#83217=CARTESIAN_POINT('Ctrl Pts',(9.53639096880491,-31.7699840254071,56.0460478276773));
#83218=CARTESIAN_POINT('Ctrl Pts',(9.54025353075794,-31.8040413147177,55.9835814644916));
#83219=CARTESIAN_POINT('Ctrl Pts',(9.54412271723623,-31.8381570143209,55.9210079677488));
#83220=CARTESIAN_POINT('Ctrl Pts',(9.54799190371453,-31.8689677171337,55.8567412175391));
#83221=CARTESIAN_POINT('Ctrl Pts',(9.55186109019283,-31.8963255363346,55.7911681381005));
#83222=CARTESIAN_POINT('Ctrl Pts',(9.55378515750059,-31.9099300203342,55.7585599867167));
#83223=CARTESIAN_POINT('Ctrl Pts',(9.55570922480834,-31.922681421013,55.7256290564944));
#83224=CARTESIAN_POINT('Ctrl Pts',(9.5576332921161,-31.9345661853751,55.6924241741181));
#83225=CARTESIAN_POINT('Ctrl Pts',(9.56150301975733,-31.9584690919815,55.6256417644604));
#83226=CARTESIAN_POINT('Ctrl Pts',(9.56537274739856,-31.9789565387339,55.557489844211));
#83227=CARTESIAN_POINT('Ctrl Pts',(9.5692424750398,-31.9958734322516,55.4883511082534));
#83228=CARTESIAN_POINT('Ctrl Pts',(9.57310644880504,-32.0127651721366,55.4193151742885));
#83229=CARTESIAN_POINT('Ctrl Pts',(9.57697042257028,-32.0260967827392,55.3492958050351));
#83230=CARTESIAN_POINT('Ctrl Pts',(9.58083439633552,-32.0357622033577,55.2786930459845));
#83231=CARTESIAN_POINT('Ctrl Pts',(9.58469385125523,-32.0454163204464,55.2081728555487));
#83232=CARTESIAN_POINT('Ctrl Pts',(9.58855330617495,-32.0514126985859,55.1370711093101));
#83233=CARTESIAN_POINT('Ctrl Pts',(9.59241276109466,-32.0536962063712,55.0657985899276));
#83234=CARTESIAN_POINT('Ctrl Pts',(9.59626979277466,-32.0559782804083,54.9945708204913));
#83235=CARTESIAN_POINT('Ctrl Pts',(9.60012682445465,-32.0545520937131,54.9231729748411));
#83236=CARTESIAN_POINT('Ctrl Pts',(9.60398385613465,-32.0494144274265,54.8520200447484));
#83237=CARTESIAN_POINT('Ctrl Pts',(9.60783975505705,-32.0442782700023,54.7808880113007));
#83238=CARTESIAN_POINT('Ctrl Pts',(9.61169565397945,-32.0354328319464,54.7100012346741));
#83239=CARTESIAN_POINT('Ctrl Pts',(9.61555155290186,-32.0229269368548,54.6397720573759));
#83240=CARTESIAN_POINT('Ctrl Pts',(9.61940760794305,-32.0104205354208,54.5695400366178));
#83241=CARTESIAN_POINT('Ctrl Pts',(9.62326366298424,-31.9942534700028,54.4999661457278));
#83242=CARTESIAN_POINT('Ctrl Pts',(9.62711971802543,-31.9745258093191,54.4314532641615));
#83243=CARTESIAN_POINT('Ctrl Pts',(9.63097981215373,-31.9547774845788,54.3628686176712));
#83244=CARTESIAN_POINT('Ctrl Pts',(9.63483990628203,-31.9314612540917,54.2953476666301));
#83245=CARTESIAN_POINT('Ctrl Pts',(9.63870000041033,-31.9047270402197,54.2292779588231));
#83246=CARTESIAN_POINT('Ctrl Pts',(9.64256228268184,-31.8779776717203,54.1631707985661));
#83247=CARTESIAN_POINT('Ctrl Pts',(9.64642456495335,-31.8478066682151,54.0985169594539));
#83248=CARTESIAN_POINT('Ctrl Pts',(9.65028684722486,-31.8144109346917,54.0356813169023));
#83249=CARTESIAN_POINT('Ctrl Pts',(9.65415588300166,-31.7809568060931,53.9727358012717));
#83250=CARTESIAN_POINT('Ctrl Pts',(9.65802491877847,-31.7442669396311,53.9116152461669));
#83251=CARTESIAN_POINT('Ctrl Pts',(9.66189395455528,-31.7045823754473,53.8526567698311));
#83252=CARTESIAN_POINT('Ctrl Pts',(9.6641854906884,-31.6810781697485,53.817737093025));
#83253=CARTESIAN_POINT('Ctrl Pts',(9.66647702682152,-31.6565242523107,53.7835752583064));
#83254=CARTESIAN_POINT('Ctrl Pts',(9.66876856295464,-31.6309771514931,53.750235584677));
#83255=CARTESIAN_POINT('Ctrl Pts',(9.67263320043979,-31.5878923918726,53.6940087809235));
#83256=CARTESIAN_POINT('Ctrl Pts',(9.67649783792494,-31.5418110729999,53.6399009041512));
#83257=CARTESIAN_POINT('Ctrl Pts',(9.68036247541009,-31.4929694991081,53.5882494422764));
#83258=CARTESIAN_POINT('Ctrl Pts',(9.68422133661275,-31.444200926301,53.536675181287));
#83259=CARTESIAN_POINT('Ctrl Pts',(9.68808019781541,-31.3926806189403,53.4875503988675));
#83260=CARTESIAN_POINT('Ctrl Pts',(9.69193905901806,-31.3386861089886,53.441180875117));
#83261=CARTESIAN_POINT('Ctrl Pts',(9.69579339263811,-31.2847549505261,53.3948657564974));
#83262=CARTESIAN_POINT('Ctrl Pts',(9.69964772625817,-31.2283557229377,53.3512997914991));
#83263=CARTESIAN_POINT('Ctrl Pts',(9.70350205987822,-31.1698026561876,53.3107518512438));
#83264=CARTESIAN_POINT('Ctrl Pts',(9.70735396752099,-31.1112864436448,53.2702294324902));
#83265=CARTESIAN_POINT('Ctrl Pts',(9.71120587516376,-31.050619480747,53.2327215466549));
#83266=CARTESIAN_POINT('Ctrl Pts',(9.71505778280652,-30.988147735328,53.1984557691619));
#83267=CARTESIAN_POINT('Ctrl Pts',(9.7189085623831,-30.925694285328,53.1642000267135));
#83268=CARTESIAN_POINT('Ctrl Pts',(9.72275934195968,-30.8614375288067,53.1331847418678));
#83269=CARTESIAN_POINT('Ctrl Pts',(9.72661012153625,-30.7957494675024,53.1055923491841));
#83270=CARTESIAN_POINT('Ctrl Pts',(9.73046106935284,-30.730058536296,53.0779987509928));
#83271=CARTESIAN_POINT('Ctrl Pts',(9.73431201716944,-30.6629366260364,53.0538285284208));
#83272=CARTESIAN_POINT('Ctrl Pts',(9.73816296498603,-30.5947755996095,53.0332159374733));
#83273=CARTESIAN_POINT('Ctrl Pts',(9.74201800536427,-30.5265421356383,53.0125814406721));
#83274=CARTESIAN_POINT('Ctrl Pts',(9.74587304574251,-30.4572678182304,52.9955122640044));
#83275=CARTESIAN_POINT('Ctrl Pts',(9.74972808612076,-30.3873586781989,52.982092465715));
#83276=CARTESIAN_POINT('Ctrl Pts',(9.75358533703476,-30.3174094512581,52.9686649723198));
#83277=CARTESIAN_POINT('Ctrl Pts',(9.75744258794876,-30.2468251597645,52.9588910892792));
#83278=CARTESIAN_POINT('Ctrl Pts',(9.76129983886276,-30.1760182474746,52.9528031020305));
#83279=CARTESIAN_POINT('Ctrl Pts',(9.76516393339993,-30.1050857079345,52.946704313335));
#83280=CARTESIAN_POINT('Ctrl Pts',(9.76902802793711,-30.0339302458983,52.9443044929261));
#83281=CARTESIAN_POINT('Ctrl Pts',(9.77289212247429,-29.9629649002034,52.9455837900067));
#83282=CARTESIAN_POINT('Ctrl Pts',(9.77522935958062,-29.9200407849609,52.9463575859318));
#83283=CARTESIAN_POINT('Ctrl Pts',(9.77756659668694,-29.8771861604196,52.9484763944796));
#83284=CARTESIAN_POINT('Ctrl Pts',(9.77990383379327,-29.8344910055602,52.9519266772746));
#83285=CARTESIAN_POINT('Ctrl Pts',(9.78377991894163,-29.7636851574035,52.9576486426939));
#83286=CARTESIAN_POINT('Ctrl Pts',(9.78765600408998,-29.6930399153945,52.9670577757194));
#83287=CARTESIAN_POINT('Ctrl Pts',(9.79153208923833,-29.6229689292378,52.9801373476942));
#83288=CARTESIAN_POINT('Ctrl Pts',(9.79540239074575,-29.5530024984272,52.9931974031865));
#83289=CARTESIAN_POINT('Ctrl Pts',(9.79927269225317,-29.483609094309,53.0099169371265));
#83290=CARTESIAN_POINT('Ctrl Pts',(9.80314299376058,-29.4151979308667,53.0302273982925));
#83291=CARTESIAN_POINT('Ctrl Pts',(9.8070087021416,-29.3468679551871,53.0505137557769));
#83292=CARTESIAN_POINT('Ctrl Pts',(9.81087441052261,-29.2795183660661,53.0743824373223));
#83293=CARTESIAN_POINT('Ctrl Pts',(9.81474011890363,-29.2135471460565,53.1017140702665));
#83294=CARTESIAN_POINT('Ctrl Pts',(9.81860335462269,-29.1476181238822,53.1290282208033));
#83295=CARTESIAN_POINT('Ctrl Pts',(9.82246659034176,-29.0830661673647,53.1598007427907));
#83296=CARTESIAN_POINT('Ctrl Pts',(9.82632982606082,-29.0202717074698,53.1938632290671));
#83297=CARTESIAN_POINT('Ctrl Pts',(9.83019187065583,-28.9574966085452,53.2279152130988));
#83298=CARTESIAN_POINT('Ctrl Pts',(9.83405391525085,-28.8964783554352,53.2652549167899));
#83299=CARTESIAN_POINT('Ctrl Pts',(9.83791595984586,-28.8375735449655,53.3056675948516));
#83300=CARTESIAN_POINT('Ctrl Pts',(9.84177809319259,-28.7786673808338,53.3460812016169));
#83301=CARTESIAN_POINT('Ctrl Pts',(9.84564022653931,-28.7218751535432,53.3895676474181));
#83302=CARTESIAN_POINT('Ctrl Pts',(9.84950235988604,-28.6675237625811,53.4358693663207));
#83303=CARTESIAN_POINT('Ctrl Pts',(9.85336838840979,-28.6131175552078,53.482217783091));
#83304=CARTESIAN_POINT('Ctrl Pts',(9.85723441693354,-28.5611574676679,53.5313868268505));
#83305=CARTESIAN_POINT('Ctrl Pts',(9.8611004454573,-28.5119359268435,53.5830797917028));
#83306=CARTESIAN_POINT('Ctrl Pts',(9.86496858955252,-28.462687450965,53.6348010440241));
#83307=CARTESIAN_POINT('Ctrl Pts',(9.86883673364774,-28.4161808209744,53.6890486000156));
#83308=CARTESIAN_POINT('Ctrl Pts',(9.87270487774297,-28.372668511454,53.7454922125046));
#83309=CARTESIAN_POINT('Ctrl Pts',(9.87657959820511,-28.329082225136,53.8020317867512));
#83310=CARTESIAN_POINT('Ctrl Pts',(9.88045431866725,-28.2885006989418,53.8607744738912));
#83311=CARTESIAN_POINT('Ctrl Pts',(9.88432903912939,-28.2511329827409,53.9213611733099));
#83312=CARTESIAN_POINT('Ctrl Pts',(9.8865657276302,-28.2295624096003,53.956334941151));
#83313=CARTESIAN_POINT('Ctrl Pts',(9.88880241613101,-28.2090618900528,53.9919226987536));
#83314=CARTESIAN_POINT('Ctrl Pts',(9.89103910463182,-28.1896644294155,54.0280521184876));
#83315=CARTESIAN_POINT('Ctrl Pts',(9.89510093082391,-28.1544386419854,54.0936631426994));
#83316=CARTESIAN_POINT('Ctrl Pts',(9.899162757016,-28.1227297888941,54.1612912760284));
#83317=CARTESIAN_POINT('Ctrl Pts',(9.9032245832081,-28.094761105567,54.2305441418511));
#83318=CARTESIAN_POINT('Ctrl Pts',(9.90727491540929,-28.0668715668848,54.2996010387249));
#83319=CARTESIAN_POINT('Ctrl Pts',(9.91132524761048,-28.0427012767271,54.3702731296961));
#83320=CARTESIAN_POINT('Ctrl Pts',(9.91537557981167,-28.0224268197389,54.442145288438));
#83321=CARTESIAN_POINT('Ctrl Pts',(9.91941896482588,-28.0021871377856,54.5138941710383));
#83322=CARTESIAN_POINT('Ctrl Pts',(9.92346234984009,-27.985830114662,54.5868386314102));
#83323=CARTESIAN_POINT('Ctrl Pts',(9.9275057348543,-27.9734837874876,54.6605451386057));
#83324=CARTESIAN_POINT('Ctrl Pts',(9.9315405950777,-27.9611634904479,54.7340962481446));
#83325=CARTESIAN_POINT('Ctrl Pts',(9.93557545530109,-27.9528371217764,54.8084057976557));
#83326=CARTESIAN_POINT('Ctrl Pts',(9.93961031552448,-27.9485821515478,54.8830283215822));
#83327=CARTESIAN_POINT('Ctrl Pts',(9.94171530386221,-27.9463623317244,54.9219589248499));
#83328=CARTESIAN_POINT('Ctrl Pts',(9.94382029219994,-27.9452497952564,54.9609745046743));
#83329=CARTESIAN_POINT('Ctrl Pts',(9.94592528053768,-27.9452500000283,55.0000107785665));
#83330=CARTESIAN_POINT('Origin',(-1.54592528053767,-30.,55.));
#83331=CARTESIAN_POINT('',(8.79398090556005,-31.2520475724682,56.6292251037768));
#83332=CARTESIAN_POINT('',(8.85202116861107,-31.2520475724682,56.6292251037768));
#83333=CARTESIAN_POINT('',(-1.54592528053767,-31.2520475724682,56.6292251037768));
#83334=CARTESIAN_POINT('',(9.30407471946232,-27.9452508243762,55.0018405904705));
#83335=CARTESIAN_POINT('Ctrl Pts',(8.85202116861107,-31.2520475724682,56.6292251037768));
#83336=CARTESIAN_POINT('Ctrl Pts',(8.85588129510045,-31.308611520277,56.5857561237206));
#83337=CARTESIAN_POINT('Ctrl Pts',(8.85974142158982,-31.3628714284232,56.5393669395893));
#83338=CARTESIAN_POINT('Ctrl Pts',(8.8636015480792,-31.4145245822312,56.4903414940086));
#83339=CARTESIAN_POINT('Ctrl Pts',(8.86746436482228,-31.4662137348823,56.4412818809242));
#83340=CARTESIAN_POINT('Ctrl Pts',(8.87132718156535,-31.5152921853506,56.3895827035034));
#83341=CARTESIAN_POINT('Ctrl Pts',(8.87518999830842,-31.5614959281433,56.3355628135329));
#83342=CARTESIAN_POINT('Ctrl Pts',(8.87905908132929,-31.6077746228446,56.2814552922664));
#83343=CARTESIAN_POINT('Ctrl Pts',(8.88292816435016,-31.6511690154702,56.2250199351042));
#83344=CARTESIAN_POINT('Ctrl Pts',(8.88679724737102,-31.6914575926751,56.166605663745));
#83345=CARTESIAN_POINT('Ctrl Pts',(8.88741392878548,-31.6978790668702,56.1572951901025));
#83346=CARTESIAN_POINT('Ctrl Pts',(8.88803061019994,-31.7042217349627,56.1479344948192));
#83347=CARTESIAN_POINT('Ctrl Pts',(8.8886472916144,-31.7104848088554,56.1385250463537));
#83348=CARTESIAN_POINT('Ctrl Pts',(8.89251644611531,-31.7497803024012,56.0794887124745));
#83349=CARTESIAN_POINT('Ctrl Pts',(8.89638560061622,-31.7860927622602,56.0182999805595));
#83350=CARTESIAN_POINT('Ctrl Pts',(8.90025475511712,-31.8191793429239,55.9552926676046));
#83351=CARTESIAN_POINT('Ctrl Pts',(8.90411814418484,-31.8522166212218,55.8923792419455));
#83352=CARTESIAN_POINT('Ctrl Pts',(8.90798153325255,-31.8820373378707,55.8276530408393));
#83353=CARTESIAN_POINT('Ctrl Pts',(8.91184492232026,-31.9084420372948,55.7614765608907));
#83354=CARTESIAN_POINT('Ctrl Pts',(8.91570377839669,-31.9348157555596,55.6953777271231));
#83355=CARTESIAN_POINT('Ctrl Pts',(8.91956263447312,-31.9577812388704,55.6278324435397));
#83356=CARTESIAN_POINT('Ctrl Pts',(8.92342149054955,-31.9771858609769,55.5592259236239));
#83357=CARTESIAN_POINT('Ctrl Pts',(8.92727791500854,-31.9965782554656,55.4906626353825));
#83358=CARTESIAN_POINT('Ctrl Pts',(8.93113433946754,-32.0124141086027,55.4210399038763));
#83359=CARTESIAN_POINT('Ctrl Pts',(8.93499076392654,-32.0245901542657,55.3507595611677));
#83360=CARTESIAN_POINT('Ctrl Pts',(8.93884604822064,-32.0367626000397,55.2804999970795));
#83361=CARTESIAN_POINT('Ctrl Pts',(8.94270133251474,-32.0452773036021,55.2095836861502));
#83362=CARTESIAN_POINT('Ctrl Pts',(8.94655661680884,-32.0500821415544,55.1384224525854));
#83363=CARTESIAN_POINT('Ctrl Pts',(8.95041205077674,-32.054887166045,55.0672584563261));
#83364=CARTESIAN_POINT('Ctrl Pts',(8.95426748474464,-32.055982008449,54.9958500033625));
#83365=CARTESIAN_POINT('Ctrl Pts',(8.95812291871254,-32.0533665594502,54.9246121028825));
#83366=CARTESIAN_POINT('Ctrl Pts',(8.96198238635905,-32.0507483740847,54.8532996710272));
#83367=CARTESIAN_POINT('Ctrl Pts',(8.96584185400557,-32.044412166173,54.782158634289));
#83368=CARTESIAN_POINT('Ctrl Pts',(8.96970132165209,-32.0344099065248,54.7116011533762));
#83369=CARTESIAN_POINT('Ctrl Pts',(8.97356297345388,-32.0244019863839,54.6410037424761));
#83370=CARTESIAN_POINT('Ctrl Pts',(8.97742462525567,-32.0107239775958,54.5709910218015));
#83371=CARTESIAN_POINT('Ctrl Pts',(8.98128627705745,-31.9934789159077,54.5019644848691));
#83372=CARTESIAN_POINT('Ctrl Pts',(8.98515468302837,-31.9762036919809,54.4328172180189));
#83373=CARTESIAN_POINT('Ctrl Pts',(8.98902308899929,-31.9553491011636,54.3646600433246));
#83374=CARTESIAN_POINT('Ctrl Pts',(8.99289149497021,-31.9310677072978,54.2978781641827));
#83375=CARTESIAN_POINT('Ctrl Pts',(8.99518851746446,-31.9166496476834,54.2582237225985));
#83376=CARTESIAN_POINT('Ctrl Pts',(8.99748553995872,-31.9010242638133,54.2190538077006));
#83377=CARTESIAN_POINT('Ctrl Pts',(8.99978256245297,-31.8842312012679,54.1804450337722));
#83378=CARTESIAN_POINT('Ctrl Pts',(9.00365176190955,-31.8559442738922,54.1154108221018));
#83379=CARTESIAN_POINT('Ctrl Pts',(9.00752096136614,-31.8242310367163,54.0517155014003));
#83380=CARTESIAN_POINT('Ctrl Pts',(9.01139016082272,-31.7892402531975,53.9897441517923));
#83381=CARTESIAN_POINT('Ctrl Pts',(9.01525359672947,-31.7543015918623,53.9278651145518));
#83382=CARTESIAN_POINT('Ctrl Pts',(9.01911703263621,-31.7160953121696,53.8677053704774));
#83383=CARTESIAN_POINT('Ctrl Pts',(9.02298046854296,-31.6748178047568,53.8096290984027));
#83384=CARTESIAN_POINT('Ctrl Pts',(9.02683937399512,-31.6335887013754,53.7516209294154));
#83385=CARTESIAN_POINT('Ctrl Pts',(9.03069827944728,-31.589295804072,53.6956917734453));
#83386=CARTESIAN_POINT('Ctrl Pts',(9.03455718489944,-31.5421799864629,53.6421787850187));
#83387=CARTESIAN_POINT('Ctrl Pts',(9.03841366026827,-31.4950938392783,53.5886994955316));
#83388=CARTESIAN_POINT('Ctrl Pts',(9.0422701356371,-31.4451886189367,53.5376337185791));
#83389=CARTESIAN_POINT('Ctrl Pts',(9.04612661100593,-31.3927459309374,53.4892861507362));
#83390=CARTESIAN_POINT('Ctrl Pts',(9.04998194765525,-31.3403187279357,53.4409528587057));
#83391=CARTESIAN_POINT('Ctrl Pts',(9.05383728430456,-31.2853559016916,53.3953365114308));
#83392=CARTESIAN_POINT('Ctrl Pts',(9.05769262095387,-31.2281751891768,53.3527042563065));
#83393=CARTESIAN_POINT('Ctrl Pts',(9.06154810863517,-31.1709922366198,53.3100703310729));
#83394=CARTESIAN_POINT('Ctrl Pts',(9.06540359631647,-31.1115916160343,53.2704210186607));
#83395=CARTESIAN_POINT('Ctrl Pts',(9.06925908399777,-31.0503219494664,53.2339814935938));
#83396=CARTESIAN_POINT('Ctrl Pts',(9.07311860703276,-30.9889881548826,53.197503829027));
#83397=CARTESIAN_POINT('Ctrl Pts',(9.07697813006775,-30.9257818275672,53.1642429069912));
#83398=CARTESIAN_POINT('Ctrl Pts',(9.08083765310275,-30.8610774416811,53.1343786016643));
#83399=CARTESIAN_POINT('Ctrl Pts',(9.08469936132035,-30.7963364215018,53.1044973877816));
#83400=CARTESIAN_POINT('Ctrl Pts',(9.08856106953795,-30.7300961055593,53.0780167993037));
#83401=CARTESIAN_POINT('Ctrl Pts',(9.09242277775555,-30.6627497006221,53.0550680225712));
#83402=CARTESIAN_POINT('Ctrl Pts',(9.09629124113087,-30.5952854888593,53.0320791023069));
#83403=CARTESIAN_POINT('Ctrl Pts',(9.10015970450618,-30.5267117925989,53.0126344610694));
#83404=CARTESIAN_POINT('Ctrl Pts',(9.10402816788149,-30.4574349938009,52.9968148390759));
#83405=CARTESIAN_POINT('Ctrl Pts',(9.10632472301817,-30.4163080726706,52.9874233493229));
#83406=CARTESIAN_POINT('Ctrl Pts',(9.10862127815485,-30.3749335317263,52.9793084532619));
#83407=CARTESIAN_POINT('Ctrl Pts',(9.11091783329152,-30.3333971860964,52.9724783900528));
#83408=CARTESIAN_POINT('Ctrl Pts',(9.11478631670382,-30.2634303642635,52.9609733380697));
#83409=CARTESIAN_POINT('Ctrl Pts',(9.11865480011613,-30.1927300179298,52.9530716431946));
#83410=CARTESIAN_POINT('Ctrl Pts',(9.12252328352843,-30.1217002072108,52.9488572399599));
#83411=CARTESIAN_POINT('Ctrl Pts',(9.12638600086703,-30.0507762682456,52.9446491184013));
#83412=CARTESIAN_POINT('Ctrl Pts',(9.13024871820564,-29.9795243207904,52.9441174077245));
#83413=CARTESIAN_POINT('Ctrl Pts',(9.13411143554424,-29.9083567087272,52.9472946948808));
#83414=CARTESIAN_POINT('Ctrl Pts',(9.13796962214508,-29.8372725720414,52.9504682552681));
#83415=CARTESIAN_POINT('Ctrl Pts',(9.14182780874593,-29.7662730573655,52.9573421505805));
#83416=CARTESIAN_POINT('Ctrl Pts',(9.14568599534678,-29.6957719407134,52.9678969390204));
#83417=CARTESIAN_POINT('Ctrl Pts',(9.14954175207606,-29.6253152254023,52.9784450800937));
#83418=CARTESIAN_POINT('Ctrl Pts',(9.15339750880534,-29.5553567648275,52.9926694432706));
#83419=CARTESIAN_POINT('Ctrl Pts',(9.15725326553462,-29.4863051646889,53.0104987613287));
#83420=CARTESIAN_POINT('Ctrl Pts',(9.16110788480679,-29.4172739349313,53.0283228196969));
#83421=CARTESIAN_POINT('Ctrl Pts',(9.16496250407896,-29.3491495047654,53.0497496002636));
#83422=CARTESIAN_POINT('Ctrl Pts',(9.16881712335113,-29.2823285343048,53.0746571136998));
#83423=CARTESIAN_POINT('Ctrl Pts',(9.17267189596913,-29.2155049055486,53.0995656180154));
#83424=CARTESIAN_POINT('Ctrl Pts',(9.17652666858713,-29.1499852940231,53.1279549583208));
#83425=CARTESIAN_POINT('Ctrl Pts',(9.18038144120513,-29.0861478495278,53.1596544320217));
#83426=CARTESIAN_POINT('Ctrl Pts',(9.18424025761134,-29.0222434373716,53.1913871595538));
#83427=CARTESIAN_POINT('Ctrl Pts',(9.18809907401755,-28.9600251510098,53.2264367356658));
#83428=CARTESIAN_POINT('Ctrl Pts',(9.19195789042377,-28.8998471034632,53.2645861684481));
#83429=CARTESIAN_POINT('Ctrl Pts',(9.19581889570076,-28.839634920587,53.3027572410728));
#83430=CARTESIAN_POINT('Ctrl Pts',(9.19967990097776,-28.7814656768177,53.3440313893116));
#83431=CARTESIAN_POINT('Ctrl Pts',(9.20354090625475,-28.7256627373057,53.3881494785779));
#83432=CARTESIAN_POINT('Ctrl Pts',(9.20740868014233,-28.6697619713626,53.4323449099207));
#83433=CARTESIAN_POINT('Ctrl Pts',(9.2112764540299,-28.6162361569351,53.4793939152693));
#83434=CARTESIAN_POINT('Ctrl Pts',(9.21514422791748,-28.5653734201062,53.52899893312));
#83435=CARTESIAN_POINT('Ctrl Pts',(9.21744718665501,-28.5350886134965,53.558534865831));
#83436=CARTESIAN_POINT('Ctrl Pts',(9.21975014539255,-28.5057472096071,53.5889762917178));
#83437=CARTESIAN_POINT('Ctrl Pts',(9.22205310413009,-28.4774031176423,53.6202549886538));
#83438=CARTESIAN_POINT('Ctrl Pts',(9.22588186911175,-28.4302798822223,53.6722571272716));
#83439=CARTESIAN_POINT('Ctrl Pts',(9.22971063409341,-28.3857218334432,53.7267889522));
#83440=CARTESIAN_POINT('Ctrl Pts',(9.23353939907507,-28.3440162798996,53.7835644360417));
#83441=CARTESIAN_POINT('Ctrl Pts',(9.23736291406493,-28.302367912894,53.8402620694994));
#83442=CARTESIAN_POINT('Ctrl Pts',(9.2411864290548,-28.2635645787771,53.8991968672192));
#83443=CARTESIAN_POINT('Ctrl Pts',(9.24500994404467,-28.2278554195201,53.9600475259052));
#83444=CARTESIAN_POINT('Ctrl Pts',(9.24882955990619,-28.1921826756022,54.0208361305575));
#83445=CARTESIAN_POINT('Ctrl Pts',(9.25264917576771,-28.1595980989182,54.0835362956583));
#83446=CARTESIAN_POINT('Ctrl Pts',(9.25646879162923,-28.1303082181272,54.1477968532696));
#83447=CARTESIAN_POINT('Ctrl Pts',(9.26043595228199,-28.0998869226853,54.2145396789678));
#83448=CARTESIAN_POINT('Ctrl Pts',(9.26440311293475,-28.0730203785571,54.2829654537267));
#83449=CARTESIAN_POINT('Ctrl Pts',(9.26837027358751,-28.0498874430765,54.3526526605991));
#83450=CARTESIAN_POINT('Ctrl Pts',(9.27218706938689,-28.0276313010401,54.4196985560749));
#83451=CARTESIAN_POINT('Ctrl Pts',(9.27600386518627,-28.0088309596904,54.4879114610378));
#83452=CARTESIAN_POINT('Ctrl Pts',(9.27982066098565,-27.9935957073492,54.5568980061743));
#83453=CARTESIAN_POINT('Ctrl Pts',(9.28363747690964,-27.9783603746778,54.6258849150525));
#83454=CARTESIAN_POINT('Ctrl Pts',(9.28745429283363,-27.9666902652569,54.6956449850153));
#83455=CARTESIAN_POINT('Ctrl Pts',(9.29127110875762,-27.9586435999298,54.765774445475));
#83456=CARTESIAN_POINT('Ctrl Pts',(9.29509049516895,-27.9505915154649,54.8359511355874));
#83457=CARTESIAN_POINT('Ctrl Pts',(9.29890988158028,-27.9461677832664,54.9064972176053));
#83458=CARTESIAN_POINT('Ctrl Pts',(9.30272926799162,-27.9453786732185,54.977005086767));
#83459=CARTESIAN_POINT('Ctrl Pts',(9.30317775181519,-27.9452860135467,54.9852843325273));
#83460=CARTESIAN_POINT('Ctrl Pts',(9.30362623563875,-27.945243409575,54.9935630529975));
#83461=CARTESIAN_POINT('Ctrl Pts',(9.30407471946232,-27.9452508243762,55.0018405904705));
#83462=CARTESIAN_POINT('Ctrl Pts',(9.30407500815832,-27.9458343182313,55.0018453946623));
#83463=CARTESIAN_POINT('Ctrl Pts',(9.31377946376176,-27.9442447038212,55.180908445478));
#83464=CARTESIAN_POINT('Ctrl Pts',(9.36052900964471,-28.0476742131919,56.041715898022));
#83465=CARTESIAN_POINT('Ctrl Pts',(9.44318606609553,-29.2381700604055,57.2943385069855));
#83466=CARTESIAN_POINT('Ctrl Pts',(9.51613866694288,-30.7301723791876,57.0320535442367));
#83467=CARTESIAN_POINT('Ctrl Pts',(9.55204617751071,-31.254042933277,56.631836765028));
#83468=CARTESIAN_POINT('',(9.24592528058113,-27.9452507889202,54.9981994259027));
#83469=CARTESIAN_POINT('Ctrl Pts',(9.24592528058113,-27.9452507889202,54.9981994259027));
#83470=CARTESIAN_POINT('Ctrl Pts',(9.24973102059823,-27.9451893827432,55.0682739060629));
#83471=CARTESIAN_POINT('Ctrl Pts',(9.25353676061533,-27.9487168964303,55.1384663033952));
#83472=CARTESIAN_POINT('Ctrl Pts',(9.25734250063243,-27.9558428982201,55.2083729966738));
#83473=CARTESIAN_POINT('Ctrl Pts',(9.26114492409795,-27.9629626899818,55.27821876904));
#83474=CARTESIAN_POINT('Ctrl Pts',(9.26494734756347,-27.9736747051185,55.3477788345256));
#83475=CARTESIAN_POINT('Ctrl Pts',(9.26874977102899,-27.9879364790639,55.416650873296));
#83476=CARTESIAN_POINT('Ctrl Pts',(9.27255023950047,-28.0021909204007,55.4854875019058));
#83477=CARTESIAN_POINT('Ctrl Pts',(9.27635070797195,-28.0199914006488,55.5536363151698));
#83478=CARTESIAN_POINT('Ctrl Pts',(9.28015117644343,-28.0412440363914,55.6207033409992));
#83479=CARTESIAN_POINT('Ctrl Pts',(9.28395104864064,-28.062493337703,55.6877598443519));
#83480=CARTESIAN_POINT('Ctrl Pts',(9.28775092083786,-28.0871935671388,55.7537344197391));
#83481=CARTESIAN_POINT('Ctrl Pts',(9.29155079303508,-28.1152010131206,55.8182483373392));
#83482=CARTESIAN_POINT('Ctrl Pts',(9.29535403744921,-28.1432333144602,55.8828195081608));
#83483=CARTESIAN_POINT('Ctrl Pts',(9.29915728186334,-28.1745784953574,55.9459269708964));
#83484=CARTESIAN_POINT('Ctrl Pts',(9.30296052627747,-28.209045142649,56.0072131161929));
#83485=CARTESIAN_POINT('Ctrl Pts',(9.30676541262342,-28.2435266698375,56.0685257198656));
#83486=CARTESIAN_POINT('Ctrl Pts',(9.31057029896936,-28.2811320775326,56.128015016866));
#83487=CARTESIAN_POINT('Ctrl Pts',(9.3143751853153,-28.3216260647905,56.1853516339506));
#83488=CARTESIAN_POINT('Ctrl Pts',(9.31818690208205,-28.3621927456712,56.2427911800549));
#83489=CARTESIAN_POINT('Ctrl Pts',(9.32199861884879,-28.405658051256,56.2980699343737));
#83490=CARTESIAN_POINT('Ctrl Pts',(9.32581033561554,-28.4517462499833,56.3508915160216));
#83491=CARTESIAN_POINT('Ctrl Pts',(9.32899447389002,-28.490246276756,56.3950163107365));
#83492=CARTESIAN_POINT('Ctrl Pts',(9.3321786121645,-28.5305757983056,56.4374269739367));
#83493=CARTESIAN_POINT('Ctrl Pts',(9.33536275043899,-28.5725559515922,56.4779719385581));
#83494=CARTESIAN_POINT('Ctrl Pts',(9.33923123501024,-28.6235586283883,56.5272309708483));
#83495=CARTESIAN_POINT('Ctrl Pts',(9.34309971958148,-28.6772141652392,56.573943517376));
#83496=CARTESIAN_POINT('Ctrl Pts',(9.34696820415272,-28.7332379698518,56.6178107186797));
#83497=CARTESIAN_POINT('Ctrl Pts',(9.35083092265192,-28.7891782695964,56.6616125348336));
#83498=CARTESIAN_POINT('Ctrl Pts',(9.35469364115112,-28.8474794508072,56.7025771269198));
#83499=CARTESIAN_POINT('Ctrl Pts',(9.35855635965032,-28.9078209020442,56.7404431563508));
#83500=CARTESIAN_POINT('Ctrl Pts',(9.36241454740881,-28.968091576322,56.7782647711653));
#83501=CARTESIAN_POINT('Ctrl Pts',(9.36627273516731,-29.0303973575254,56.8129947854112));
#83502=CARTESIAN_POINT('Ctrl Pts',(9.3701309229258,-29.0943868629872,56.8444138387493));
#83503=CARTESIAN_POINT('Ctrl Pts',(9.3739866808103,-29.1583360680684,56.8758131044706));
#83504=CARTESIAN_POINT('Ctrl Pts',(9.3778424386948,-29.223966458435,56.9039053326329));
#83505=CARTESIAN_POINT('Ctrl Pts',(9.3816981965793,-29.290901426245,56.9285167293022));
#83506=CARTESIAN_POINT('Ctrl Pts',(9.38555281700262,-29.3578166480206,56.9531208655291));
#83507=CARTESIAN_POINT('Ctrl Pts',(9.38940743742595,-29.4260352273575,56.9742460412247));
#83508=CARTESIAN_POINT('Ctrl Pts',(9.39326205784927,-29.4951615313425,56.9917669750911));
#83509=CARTESIAN_POINT('Ctrl Pts',(9.39711683161271,-29.5642905852315,57.0092886059553));
#83510=CARTESIAN_POINT('Ctrl Pts',(9.40097160537615,-29.634326963864,57.0232055930722));
#83511=CARTESIAN_POINT('Ctrl Pts',(9.40482637913959,-29.704862551242,57.0334432494763));
#83512=CARTESIAN_POINT('Ctrl Pts',(9.40868519667478,-29.7754721325385,57.0436916454849));
#83513=CARTESIAN_POINT('Ctrl Pts',(9.41254401420997,-29.8465814860722,57.05025293598));
#83514=CARTESIAN_POINT('Ctrl Pts',(9.41640283174516,-29.9177759369013,57.0531041780552));
#83515=CARTESIAN_POINT('Ctrl Pts',(9.42026383814357,-29.9890107718411,57.0559570374597));
#83516=CARTESIAN_POINT('Ctrl Pts',(9.42412484454199,-30.0603303140259,57.055095665034));
#83517=CARTESIAN_POINT('Ctrl Pts',(9.4279858509404,-30.1313212078869,57.0505492685764));
#83518=CARTESIAN_POINT('Ctrl Pts',(9.43185362592536,-30.2024365532404,57.0459949020004));
#83519=CARTESIAN_POINT('Ctrl Pts',(9.43572140091031,-30.2732216171642,57.0377426700059));
#83520=CARTESIAN_POINT('Ctrl Pts',(9.43958917589527,-30.3432701708816,57.0258734294824));
#83521=CARTESIAN_POINT('Ctrl Pts',(9.44189212435604,-30.3849784423271,57.0188062527981));
#83522=CARTESIAN_POINT('Ctrl Pts',(9.4441950728168,-30.4264258160014,57.010457737578));
#83523=CARTESIAN_POINT('Ctrl Pts',(9.44649802127757,-30.4675291496378,57.0008533321408));
#83524=CARTESIAN_POINT('Ctrl Pts',(9.45045224760824,-30.5381047126224,56.9843623018302));
#83525=CARTESIAN_POINT('Ctrl Pts',(9.45440647393891,-30.6079477242885,56.9640996491157));
#83526=CARTESIAN_POINT('Ctrl Pts',(9.45836070026958,-30.6766255095933,56.9401483145027));
#83527=CARTESIAN_POINT('Ctrl Pts',(9.46222412309782,-30.7437262017013,56.9167469901543));
#83528=CARTESIAN_POINT('Ctrl Pts',(9.46608754592607,-30.8097141140611,56.8898247287655));
#83529=CARTESIAN_POINT('Ctrl Pts',(9.46995096875432,-30.8741961087912,56.8595103457293));
#83530=CARTESIAN_POINT('Ctrl Pts',(9.4739505968362,-30.9409514209492,56.8281272269079));
#83531=CARTESIAN_POINT('Ctrl Pts',(9.47795022491808,-31.0060921252477,56.7931084436052));
#83532=CARTESIAN_POINT('Ctrl Pts',(9.48194985299997,-31.0692017699715,56.7546524264337));
#83533=CARTESIAN_POINT('Ctrl Pts',(9.48594948108185,-31.1323114146954,56.7161964092622));
#83534=CARTESIAN_POINT('Ctrl Pts',(9.48994910916373,-31.1933894800341,56.6743034186563));
#83535=CARTESIAN_POINT('Ctrl Pts',(9.49394873724561,-31.2520475724682,56.6292251037768));
#83536=CARTESIAN_POINT('Ctrl Pts',(8.79398090556005,-31.2520475724682,56.6292251037768));
#83537=CARTESIAN_POINT('Ctrl Pts',(8.79801593729024,-31.3109357776389,56.5839699489427));
#83538=CARTESIAN_POINT('Ctrl Pts',(8.80205096902044,-31.3674561592778,56.5354495907487));
#83539=CARTESIAN_POINT('Ctrl Pts',(8.80608600075064,-31.421231125295,56.4839473208281));
#83540=CARTESIAN_POINT('Ctrl Pts',(8.80994398323754,-31.4726465517402,56.4347048690519));
#83541=CARTESIAN_POINT('Ctrl Pts',(8.81380196572444,-31.5215520411688,56.3827370741503));
#83542=CARTESIAN_POINT('Ctrl Pts',(8.81765994821134,-31.56765065383,56.3283331622927));
#83543=CARTESIAN_POINT('Ctrl Pts',(8.82151585711969,-31.6137244895268,56.2739584913103));
#83544=CARTESIAN_POINT('Ctrl Pts',(8.82537176602805,-31.6569941284217,56.2171506714122));
#83545=CARTESIAN_POINT('Ctrl Pts',(8.8292276749364,-31.6972009450905,56.1582342226354));
#83546=CARTESIAN_POINT('Ctrl Pts',(8.83308280124164,-31.7373996013021,56.0993297316608));
#83547=CARTESIAN_POINT('Ctrl Pts',(8.83693792754688,-31.7745363962181,56.0383178629856));
#83548=CARTESIAN_POINT('Ctrl Pts',(8.84079305385212,-31.8083953414219,55.9755531003609));
#83549=CARTESIAN_POINT('Ctrl Pts',(8.84464868727536,-31.8422587405603,55.91278008142));
#83550=CARTESIAN_POINT('Ctrl Pts',(8.84850432069861,-31.8728432056857,55.8482541395236));
#83551=CARTESIAN_POINT('Ctrl Pts',(8.85235995412186,-31.8999789486164,55.7823538568414));
#83552=CARTESIAN_POINT('Ctrl Pts',(8.85621984162051,-31.9271446315033,55.7163808637275));
#83553=CARTESIAN_POINT('Ctrl Pts',(8.86007972911915,-31.9508538154152,55.649030954446));
#83554=CARTESIAN_POINT('Ctrl Pts',(8.86393961661779,-31.9709854350814,55.5807012805194));
#83555=CARTESIAN_POINT('Ctrl Pts',(8.86780200960935,-31.9911301223903,55.5123272530943));
#83556=CARTESIAN_POINT('Ctrl Pts',(8.8716644026009,-32.0076925122235,55.4429726678314));
#83557=CARTESIAN_POINT('Ctrl Pts',(8.87552679559246,-32.0206024973771,55.3730457211834));
#83558=CARTESIAN_POINT('Ctrl Pts',(8.87939562662056,-32.0335340015621,55.3030022166817));
#83559=CARTESIAN_POINT('Ctrl Pts',(8.88326445764865,-32.0428008922359,55.2323849281591));
#83560=CARTESIAN_POINT('Ctrl Pts',(8.88713328867675,-32.0483848997645,55.1616071313926));
#83561=CARTESIAN_POINT('Ctrl Pts',(8.88836274814608,-32.0501594179285,55.1391149543445));
#83562=CARTESIAN_POINT('Ctrl Pts',(8.88959220761542,-32.0515624047983,55.1166065609287));
#83563=CARTESIAN_POINT('Ctrl Pts',(8.89082166708475,-32.052594374007,55.0940951555338));
#83564=CARTESIAN_POINT('Ctrl Pts',(8.89469076155227,-32.0558419689506,55.0232520279301));
#83565=CARTESIAN_POINT('Ctrl Pts',(8.89855985601979,-32.0554240053786,54.9521018207862));
#83566=CARTESIAN_POINT('Ctrl Pts',(8.90242895048731,-32.0513044211451,54.8810557513345));
#83567=CARTESIAN_POINT('Ctrl Pts',(8.90629228017547,-32.0471909749095,54.810115537379));
#83568=CARTESIAN_POINT('Ctrl Pts',(8.91015560986364,-32.039386883526,54.7392796341407));
#83569=CARTESIAN_POINT('Ctrl Pts',(8.9140189395518,-32.0279080492904,54.6689614733551));
#83570=CARTESIAN_POINT('Ctrl Pts',(8.91787773748938,-32.0164426799201,54.5987257969528));
#83571=CARTESIAN_POINT('Ctrl Pts',(8.92173653542695,-32.001311207765,54.5290071337659));
#83572=CARTESIAN_POINT('Ctrl Pts',(8.92559533336452,-31.9825813738596,54.4602142475714));
#83573=CARTESIAN_POINT('Ctrl Pts',(8.92945170047951,-31.9638633386813,54.3914646969712));
#83574=CARTESIAN_POINT('Ctrl Pts',(8.93330806759449,-31.9415515662884,54.3236402339398));
#83575=CARTESIAN_POINT('Ctrl Pts',(8.93716443470947,-31.9157646621692,54.2571384236051));
#83576=CARTESIAN_POINT('Ctrl Pts',(8.94101966253136,-31.8899853763189,54.1906562600135));
#83577=CARTESIAN_POINT('Ctrl Pts',(8.94487489035324,-31.8607331724859,54.1254964260389));
#83578=CARTESIAN_POINT('Ctrl Pts',(8.94873011817513,-31.8281756328998,54.0620386906853));
#83579=CARTESIAN_POINT('Ctrl Pts',(8.95258549662043,-31.7956168212935,53.9985784760435));
#83580=CARTESIAN_POINT('Ctrl Pts',(8.95644087506573,-31.7597526412559,53.9368209232596));
#83581=CARTESIAN_POINT('Ctrl Pts',(8.96029625351103,-31.7207968899626,53.8771217225384));
#83582=CARTESIAN_POINT('Ctrl Pts',(8.96415566745054,-31.6818003629812,53.8173600335862));
#83583=CARTESIAN_POINT('Ctrl Pts',(8.96801508139005,-31.6397060709665,53.7596614052524));
#83584=CARTESIAN_POINT('Ctrl Pts',(8.97187449532956,-31.5947709730042,53.7043522445652));
#83585=CARTESIAN_POINT('Ctrl Pts',(8.97573609436686,-31.5498104339814,53.6490117692984));
#83586=CARTESIAN_POINT('Ctrl Pts',(8.97959769340417,-31.5020062128951,53.5960638155294));
#83587=CARTESIAN_POINT('Ctrl Pts',(8.98345929244148,-31.4516535306604,53.5457993297274));
#83588=CARTESIAN_POINT('Ctrl Pts',(8.98732764769787,-31.4012127518238,53.4954469016312));
#83589=CARTESIAN_POINT('Ctrl Pts',(8.99119600295426,-31.3482149711079,53.4477876400769));
#83590=CARTESIAN_POINT('Ctrl Pts',(8.99506435821066,-31.2929894562316,53.4030730046198));
#83591=CARTESIAN_POINT('Ctrl Pts',(8.99736188478154,-31.260189447078,53.3765157066829));
#83592=CARTESIAN_POINT('Ctrl Pts',(8.99965941135243,-31.2266041943995,53.3509963236269));
#83593=CARTESIAN_POINT('Ctrl Pts',(9.00195693792331,-31.1923072097097,53.3265601055986));
#83594=CARTESIAN_POINT('Ctrl Pts',(9.00582593499164,-31.1345516499269,53.2854099151674));
#83595=CARTESIAN_POINT('Ctrl Pts',(9.00969493205998,-31.0745501065352,53.2471725977323));
#83596=CARTESIAN_POINT('Ctrl Pts',(9.01356392912831,-31.0126284809632,53.2121014788187));
#83597=CARTESIAN_POINT('Ctrl Pts',(9.01742716115078,-30.9507991224581,53.1770826180499));
#83598=CARTESIAN_POINT('Ctrl Pts',(9.02129039317326,-30.887055780123,53.1452208285152));
#83599=CARTESIAN_POINT('Ctrl Pts',(9.02515362519573,-30.8217544008784,53.1167269801919));
#83600=CARTESIAN_POINT('Ctrl Pts',(9.02901232554179,-30.756529621931,53.0882665559292));
#83601=CARTESIAN_POINT('Ctrl Pts',(9.03287102588784,-30.6897508794427,53.0631664188339));
#83602=CARTESIAN_POINT('Ctrl Pts',(9.03672972623389,-30.6217983152514,53.0415913558068));
#83603=CARTESIAN_POINT('Ctrl Pts',(9.04058599585565,-30.5538885566509,53.0200298836329));
#83604=CARTESIAN_POINT('Ctrl Pts',(9.04444226547741,-30.4848069052957,53.0019892266398));
#83605=CARTESIAN_POINT('Ctrl Pts',(9.04829853509917,-30.4149516824997,52.9875853648687));
#83606=CARTESIAN_POINT('Ctrl Pts',(9.05215366566829,-30.345117093317,52.9731857576644));
#83607=CARTESIAN_POINT('Ctrl Pts',(9.05600879623741,-30.2745098618575,52.9624209111053));
#83608=CARTESIAN_POINT('Ctrl Pts',(9.05986392680652,-30.2035399219365,52.9553560058832));
#83609=CARTESIAN_POINT('Ctrl Pts',(9.06371920838183,-30.1325672021095,52.9482908239274));
#83610=CARTESIAN_POINT('Ctrl Pts',(9.06757448995713,-30.0612322292501,52.944925916974));
#83611=CARTESIAN_POINT('Ctrl Pts',(9.07142977153244,-29.9899497730715,52.9452745790645));
#83612=CARTESIAN_POINT('Ctrl Pts',(9.07528908984937,-29.9185926793205,52.9456236062278));
#83613=CARTESIAN_POINT('Ctrl Pts',(9.0791484081663,-29.8472886988166,52.9496939620888));
#83614=CARTESIAN_POINT('Ctrl Pts',(9.08300772648323,-29.7764514087396,52.9574467963244));
#83615=CARTESIAN_POINT('Ctrl Pts',(9.08686923045711,-29.7055740012111,52.9652040212411));
#83616=CARTESIAN_POINT('Ctrl Pts',(9.09073073443099,-29.6351642899932,52.9766477981494));
#83617=CARTESIAN_POINT('Ctrl Pts',(9.09459223840487,-29.5656268115988,52.9916878988319));
#83618=CARTESIAN_POINT('Ctrl Pts',(9.09846050051131,-29.4959676336023,53.0067543216405));
#83619=CARTESIAN_POINT('Ctrl Pts',(9.10232876261775,-29.4271842051521,53.025429507103));
#83620=CARTESIAN_POINT('Ctrl Pts',(9.1061970247242,-29.3596663533093,53.0475732066436));
#83621=CARTESIAN_POINT('Ctrl Pts',(9.10849541940342,-29.3195494565847,53.0607302678257));
#83622=CARTESIAN_POINT('Ctrl Pts',(9.11079381408265,-29.2798789969184,53.0751109003345));
#83623=CARTESIAN_POINT('Ctrl Pts',(9.11309220876187,-29.2407329502307,53.0906778402704));
#83624=CARTESIAN_POINT('Ctrl Pts',(9.11696136315485,-29.1748338686332,53.1168834761355));
#83625=CARTESIAN_POINT('Ctrl Pts',(9.12083051754782,-29.1101640263347,53.1465561390878));
#83626=CARTESIAN_POINT('Ctrl Pts',(9.12469967194079,-29.0471130310267,53.1795593976016));
#83627=CARTESIAN_POINT('Ctrl Pts',(9.12856306090183,-28.9841559880878,53.2125134779173));
#83628=CARTESIAN_POINT('Ctrl Pts',(9.13242644986287,-28.9228134307589,53.2487880790794));
#83629=CARTESIAN_POINT('Ctrl Pts',(9.13628983882391,-28.8634555918223,53.2881985013618));
#83630=CARTESIAN_POINT('Ctrl Pts',(9.14014869479598,-28.8041673985856,53.3275626826338));
#83631=CARTESIAN_POINT('Ctrl Pts',(9.14400755076807,-28.7468597008544,53.3700551092534));
#83632=CARTESIAN_POINT('Ctrl Pts',(9.14786640674014,-28.691877136126,53.4154457612596));
#83633=CARTESIAN_POINT('Ctrl Pts',(9.15172283109628,-28.6369292180602,53.4608078108423));
#83634=CARTESIAN_POINT('Ctrl Pts',(9.15557925545242,-28.5843038998644,53.5090641539634));
#83635=CARTESIAN_POINT('Ctrl Pts',(9.15943567980856,-28.5343146735652,53.5599430266917));
#83636=CARTESIAN_POINT('Ctrl Pts',(9.16329096400142,-28.4843402267287,53.6108068569308));
#83637=CARTESIAN_POINT('Ctrl Pts',(9.16714624819429,-28.4370006647841,53.664291331159));
#83638=CARTESIAN_POINT('Ctrl Pts',(9.17100153238715,-28.3925730990924,53.7200873776939));
#83639=CARTESIAN_POINT('Ctrl Pts',(9.17485696625558,-28.3481438085678,53.7758855904256));
#83640=CARTESIAN_POINT('Ctrl Pts',(9.178712400124,-28.3066270396117,53.8339951722531));
#83641=CARTESIAN_POINT('Ctrl Pts',(9.18256783399242,-28.2682589344091,53.894074846906));
#83642=CARTESIAN_POINT('Ctrl Pts',(9.18642730154279,-28.2298506872306,53.954217378894));
#83643=CARTESIAN_POINT('Ctrl Pts',(9.19028676909316,-28.1945979418333,54.0163337080404));
#83644=CARTESIAN_POINT('Ctrl Pts',(9.19414623664353,-28.1626923851445,54.0800552783488));
#83645=CARTESIAN_POINT('Ctrl Pts',(9.1980078883509,-28.1307687724041,54.1438129100859));
#83646=CARTESIAN_POINT('Ctrl Pts',(9.20186954005828,-28.1021963139035,54.2091771461072));
#83647=CARTESIAN_POINT('Ctrl Pts',(9.20573119176565,-28.0771186290985,54.2757591588843));
#83648=CARTESIAN_POINT('Ctrl Pts',(9.20959959764587,-28.0519970824875,54.3424576260849));
#83649=CARTESIAN_POINT('Ctrl Pts',(9.2134680035261,-28.0303826606991,54.4103776594867));
#83650=CARTESIAN_POINT('Ctrl Pts',(9.21733640940633,-28.0123689814919,54.4791156589371));
#83651=CARTESIAN_POINT('Ctrl Pts',(9.21963343280437,-28.0016726264804,54.5199316430815));
#83652=CARTESIAN_POINT('Ctrl Pts',(9.2219304562024,-27.9922448704791,54.5610358236325));
#83653=CARTESIAN_POINT('Ctrl Pts',(9.22422747960044,-27.9840966829305,54.6023426365223));
#83654=CARTESIAN_POINT('Ctrl Pts',(9.22983463137485,-27.9642065397518,54.7031746826342));
#83655=CARTESIAN_POINT('Ctrl Pts',(9.23544178314927,-27.9518767132062,54.8055436423064));
#83656=CARTESIAN_POINT('Ctrl Pts',(9.24104893492368,-27.947287515211,54.9085176667792));
#83657=CARTESIAN_POINT('Ctrl Pts',(9.24267438346168,-27.9459571597165,54.938368647146));
#83658=CARTESIAN_POINT('Ctrl Pts',(9.24429983199968,-27.9452770157847,54.9682703020373));
#83659=CARTESIAN_POINT('Ctrl Pts',(9.24592528053768,-27.9452507889209,54.9981994251026));
#83660=CARTESIAN_POINT('Origin',(-1.54592528053767,-30.,55.));
#83661=CARTESIAN_POINT('',(8.09385946080458,-31.2520475724682,56.6292251037768));
#83662=CARTESIAN_POINT('',(8.15211404571458,-31.2520475724682,56.6292251037768));
#83663=CARTESIAN_POINT('',(-1.54592528053767,-31.2520475724682,56.6292251037768));
#83664=CARTESIAN_POINT('',(8.60407471942946,-27.9452501088858,54.9993310708367));
#83665=CARTESIAN_POINT('Ctrl Pts',(8.15211404571458,-31.2520475724682,56.6292251037768));
#83666=CARTESIAN_POINT('Ctrl Pts',(8.15596957845487,-31.308571006352,56.5857872583755));
#83667=CARTESIAN_POINT('Ctrl Pts',(8.15982511119515,-31.362858995009,56.5393831792067));
#83668=CARTESIAN_POINT('Ctrl Pts',(8.16368064393543,-31.4145918930459,56.4902776045518));
#83669=CARTESIAN_POINT('Ctrl Pts',(8.1675357777639,-31.4663194385503,56.4411771105941));
#83670=CARTESIAN_POINT('Ctrl Pts',(8.17139091159237,-31.515492066891,56.3893760114549));
#83671=CARTESIAN_POINT('Ctrl Pts',(8.17524604542084,-31.5618258017338,56.3351770397736));
#83672=CARTESIAN_POINT('Ctrl Pts',(8.17912851385102,-31.608488063223,56.2805937734425));
#83673=CARTESIAN_POINT('Ctrl Pts',(8.18301098228121,-31.6522706727025,56.2235788607262));
#83674=CARTESIAN_POINT('Ctrl Pts',(8.18689345071139,-31.6929251008616,56.1644750600046));
#83675=CARTESIAN_POINT('Ctrl Pts',(8.1907539689977,-31.7333496828382,56.1057054118854));
#83676=CARTESIAN_POINT('Ctrl Pts',(8.19461448728401,-31.7706811538646,56.0448708815817));
#83677=CARTESIAN_POINT('Ctrl Pts',(8.19847500557032,-31.8047201484561,55.9823353542739));
#83678=CARTESIAN_POINT('Ctrl Pts',(8.20236844907244,-31.8390494515399,55.9192664799956));
#83679=CARTESIAN_POINT('Ctrl Pts',(8.20626189257456,-31.8700296290214,55.8544679084298));
#83680=CARTESIAN_POINT('Ctrl Pts',(8.21015533607669,-31.8975055949884,55.788333736109));
#83681=CARTESIAN_POINT('Ctrl Pts',(8.21404877957881,-31.9249815609555,55.7221995637882));
#83682=CARTESIAN_POINT('Ctrl Pts',(8.21794222308093,-31.9489532088339,55.6547302832358));
#83683=CARTESIAN_POINT('Ctrl Pts',(8.22183566658305,-31.9693172416555,55.5863336628732));
#83684=CARTESIAN_POINT('Ctrl Pts',(8.22570474058959,-31.9895538137326,55.5183651445588));
#83685=CARTESIAN_POINT('Ctrl Pts',(8.22957381459614,-32.0063071206436,55.449214604025));
#83686=CARTESIAN_POINT('Ctrl Pts',(8.23344288860268,-32.01944299116,55.3792724191852));
#83687=CARTESIAN_POINT('Ctrl Pts',(8.23730619764667,-32.0325592890859,55.3094344489653));
#83688=CARTESIAN_POINT('Ctrl Pts',(8.24116950669066,-32.0420687607178,55.2388076493788));
#83689=CARTESIAN_POINT('Ctrl Pts',(8.24503281573465,-32.0478871312764,55.1677970799878));
#83690=CARTESIAN_POINT('Ctrl Pts',(8.24889159285783,-32.0536986764959,55.0968698107608));
#83691=CARTESIAN_POINT('Ctrl Pts',(8.252750369981,-32.0558276818286,55.0255601477677));
#83692=CARTESIAN_POINT('Ctrl Pts',(8.25660914710418,-32.0542413068434,54.9542811225153));
#83693=CARTESIAN_POINT('Ctrl Pts',(8.26046549331127,-32.0526559312277,54.8830470009523));
#83694=CARTESIAN_POINT('Ctrl Pts',(8.26432183951836,-32.0473598297511,54.8118439633547));
#83695=CARTESIAN_POINT('Ctrl Pts',(8.26817818572546,-32.0383722258364,54.7410864402188));
#83696=CARTESIAN_POINT('Ctrl Pts',(8.2720333925775,-32.0293872773037,54.6703498223484));
#83697=CARTESIAN_POINT('Ctrl Pts',(8.27588859942954,-32.0167130527585,54.6000589392748));
#83698=CARTESIAN_POINT('Ctrl Pts',(8.27974380628158,-32.0004205986065,54.5306227624065));
#83699=CARTESIAN_POINT('Ctrl Pts',(8.28359916372655,-31.9841275080351,54.4611838732073));
#83700=CARTESIAN_POINT('Ctrl Pts',(8.28745452117151,-31.9642160203678,54.3926002289364));
#83701=CARTESIAN_POINT('Ctrl Pts',(8.29130987861647,-31.9408078398956,54.3252685785442));
#83702=CARTESIAN_POINT('Ctrl Pts',(8.29516927165503,-31.9173751569214,54.2578664487783));
#83703=CARTESIAN_POINT('Ctrl Pts',(8.2990286646936,-31.8904386344849,54.1917193887793));
#83704=CARTESIAN_POINT('Ctrl Pts',(8.30288805773216,-31.8601689269621,54.1272061379314));
#83705=CARTESIAN_POINT('Ctrl Pts',(8.3067496358931,-31.8298820812483,54.0626563607835));
#83706=CARTESIAN_POINT('Ctrl Pts',(8.31061121405404,-31.7962585227126,53.9997426628865));
#83707=CARTESIAN_POINT('Ctrl Pts',(8.31447279221498,-31.7595145901036,53.9388185971698));
#83708=CARTESIAN_POINT('Ctrl Pts',(8.31834112686172,-31.7227063677537,53.8777879344692));
#83709=CARTESIAN_POINT('Ctrl Pts',(8.32220946150847,-31.6827671433323,53.8187542567448));
#83710=CARTESIAN_POINT('Ctrl Pts',(8.32607779615521,-31.6399558203565,53.7620410064227));
#83711=CARTESIAN_POINT('Ctrl Pts',(8.32837550991068,-31.6145267469504,53.7283544649824));
#83712=CARTESIAN_POINT('Ctrl Pts',(8.33067322366614,-31.5880851306643,53.6954859602816));
#83713=CARTESIAN_POINT('Ctrl Pts',(8.33297093742161,-31.5606914159249,53.6634971504862));
#83714=CARTESIAN_POINT('Ctrl Pts',(8.33684001407394,-31.514563658772,53.6096317998433));
#83715=CARTESIAN_POINT('Ctrl Pts',(8.34070909072628,-31.4655536320953,53.5580518103859));
#83716=CARTESIAN_POINT('Ctrl Pts',(8.34457816737861,-31.4139165404304,53.5090816322825));
#83717=CARTESIAN_POINT('Ctrl Pts',(8.34844147909947,-31.3623563881289,53.4601844198363));
#83718=CARTESIAN_POINT('Ctrl Pts',(8.35230479082034,-31.30817729029,53.41388963149));
#83719=CARTESIAN_POINT('Ctrl Pts',(8.3561681025412,-31.2516738481402,53.3704877599779));
#83720=CARTESIAN_POINT('Ctrl Pts',(8.36002688237409,-31.1952366877943,53.3271368013699));
#83721=CARTESIAN_POINT('Ctrl Pts',(8.36388566220698,-31.1364809824483,53.2866723133255));
#83722=CARTESIAN_POINT('Ctrl Pts',(8.36774444203987,-31.0757359270089,53.2493459000013));
#83723=CARTESIAN_POINT('Ctrl Pts',(8.37160079097541,-31.0150291388458,53.2120430010218));
#83724=CARTESIAN_POINT('Ctrl Pts',(8.37545713991095,-30.9523358998726,53.1778745083927));
#83725=CARTESIAN_POINT('Ctrl Pts',(8.3793134888465,-30.8880148178725,53.1470490438927));
#83726=CARTESIAN_POINT('Ctrl Pts',(8.38316869844154,-30.8237127392392,53.116232686634));
#83727=CARTESIAN_POINT('Ctrl Pts',(8.38702390803659,-30.7577842102125,53.088757606512));
#83728=CARTESIAN_POINT('Ctrl Pts',(8.39087911763163,-30.690611359049,53.06478592573));
#83729=CARTESIAN_POINT('Ctrl Pts',(8.39473447783001,-30.6234358837856,53.040813308497));
#83730=CARTESIAN_POINT('Ctrl Pts',(8.39858983802839,-30.5550164481427,53.0203445235216));
#83731=CARTESIAN_POINT('Ctrl Pts',(8.40244519822677,-30.4857523867497,53.0034925040794));
#83732=CARTESIAN_POINT('Ctrl Pts',(8.40630459401537,-30.4164158233452,52.9866228448212));
#83733=CARTESIAN_POINT('Ctrl Pts',(8.41016398980398,-30.3462333422905,52.9733776235643));
#83734=CARTESIAN_POINT('Ctrl Pts',(8.41402338559259,-30.2756156963431,52.9638188807404));
#83735=CARTESIAN_POINT('Ctrl Pts',(8.4178849665058,-30.204958067879,52.954254725918));
#83736=CARTESIAN_POINT('Ctrl Pts',(8.42174654741902,-30.1338652684148,52.9483812445603));
#83737=CARTESIAN_POINT('Ctrl Pts',(8.42560812833224,-30.0627516680271,52.9462084354395));
#83738=CARTESIAN_POINT('Ctrl Pts',(8.42947646570466,-29.9915136429154,52.9440318246384));
#83739=CARTESIAN_POINT('Ctrl Pts',(8.43334480307707,-29.9202552300438,52.9455688029681));
#83740=CARTESIAN_POINT('Ctrl Pts',(8.43721314044949,-29.8493885879424,52.95077727783));
#83741=CARTESIAN_POINT('Ctrl Pts',(8.43951082971972,-29.8072956918226,52.9538709730411));
#83742=CARTESIAN_POINT('Ctrl Pts',(8.44180851898994,-29.7653408945803,52.9582589957021));
#83743=CARTESIAN_POINT('Ctrl Pts',(8.44410620826017,-29.7236087780448,52.9639240056112));
#83744=CARTESIAN_POINT('Ctrl Pts',(8.44797527191515,-29.6533363450292,52.9734632780571));
#83745=CARTESIAN_POINT('Ctrl Pts',(8.45184433557013,-29.5834206956311,52.9866635450178));
#83746=CARTESIAN_POINT('Ctrl Pts',(8.45571339922511,-29.514272826168,53.0034863699185));
#83747=CARTESIAN_POINT('Ctrl Pts',(8.45957669792241,-29.4452279879746,53.0202841285804));
#83748=CARTESIAN_POINT('Ctrl Pts',(8.46343999661971,-29.3769491270779,53.040693617078));
#83749=CARTESIAN_POINT('Ctrl Pts',(8.46730329531701,-29.3098400782369,53.0646248826411));
#83750=CARTESIAN_POINT('Ctrl Pts',(8.47116206214992,-29.2428097520452,53.0885280754978));
#83751=CARTESIAN_POINT('Ctrl Pts',(8.47502082898283,-29.1769469674925,53.1159446770033));
#83752=CARTESIAN_POINT('Ctrl Pts',(8.47887959581574,-29.1126416498874,53.1467345789161));
#83753=CARTESIAN_POINT('Ctrl Pts',(8.48273593177282,-29.048376842178,53.1775050843658));
#83754=CARTESIAN_POINT('Ctrl Pts',(8.48659226772991,-28.9856679919586,53.2116444648626));
#83755=CARTESIAN_POINT('Ctrl Pts',(8.49044860368699,-28.9248848657667,53.248964588981));
#83756=CARTESIAN_POINT('Ctrl Pts',(8.49430380034396,-28.8641196970928,53.2862736873947));
#83757=CARTESIAN_POINT('Ctrl Pts',(8.49815899700094,-28.8052795367251,53.3267614098114));
#83758=CARTESIAN_POINT('Ctrl Pts',(8.50201419365791,-28.748707841602,53.3701946444953));
#83759=CARTESIAN_POINT('Ctrl Pts',(8.50586954097745,-28.6921339356353,53.4136295765668));
#83760=CARTESIAN_POINT('Ctrl Pts',(8.509724888297,-28.6378290549019,53.4600099518644));
#83761=CARTESIAN_POINT('Ctrl Pts',(8.51358023561654,-28.5861046627145,53.509061524508));
#83762=CARTESIAN_POINT('Ctrl Pts',(8.51743961870478,-28.5343261255524,53.558164444225));
#83763=CARTESIAN_POINT('Ctrl Pts',(8.52129900179303,-28.4851338224501,53.6099438081762));
#83764=CARTESIAN_POINT('Ctrl Pts',(8.52515838488127,-28.4388026522076,53.6640881751606));
#83765=CARTESIAN_POINT('Ctrl Pts',(8.5290199531756,-28.3924452489757,53.7182631990135));
#83766=CARTESIAN_POINT('Ctrl Pts',(8.53288152146993,-28.3489524998295,53.7748055063574));
#83767=CARTESIAN_POINT('Ctrl Pts',(8.53674308976426,-28.3085575429557,53.8333723914599));
#83768=CARTESIAN_POINT('Ctrl Pts',(8.54061141478311,-28.2680919055774,53.8920417531414));
#83769=CARTESIAN_POINT('Ctrl Pts',(8.54447973980196,-28.2307351369873,53.9527423513882));
#83770=CARTESIAN_POINT('Ctrl Pts',(8.54834806482081,-28.1966754116349,54.0151050860635));
#83771=CARTESIAN_POINT('Ctrl Pts',(8.55064586958012,-28.1764437613382,54.0521488680213));
#83772=CARTESIAN_POINT('Ctrl Pts',(8.55294367433942,-28.1573745478791,54.0897786837591));
#83773=CARTESIAN_POINT('Ctrl Pts',(8.55524147909873,-28.1394990816289,54.1279140551298));
#83774=CARTESIAN_POINT('Ctrl Pts',(8.55943211157693,-28.1068986141053,54.1974636220317));
#83775=CARTESIAN_POINT('Ctrl Pts',(8.56362274405514,-28.0781594760249,54.2689335413495));
#83776=CARTESIAN_POINT('Ctrl Pts',(8.56781337653335,-28.0534920738987,54.3418932790764));
#83777=CARTESIAN_POINT('Ctrl Pts',(8.5719933930468,-28.0288871607341,54.4146681907637));
#83778=CARTESIAN_POINT('Ctrl Pts',(8.57617340956025,-28.0083335647055,54.4889250761304));
#83779=CARTESIAN_POINT('Ctrl Pts',(8.5803534260737,-27.9919942666101,54.5642127386292));
#83780=CARTESIAN_POINT('Ctrl Pts',(8.58451639467447,-27.9757216072291,54.6391933455236));
#83781=CARTESIAN_POINT('Ctrl Pts',(8.58867936327524,-27.9636290821987,54.7151960112602));
#83782=CARTESIAN_POINT('Ctrl Pts',(8.59284233187601,-27.9558297509936,54.7917560191092));
#83783=CARTESIAN_POINT('Ctrl Pts',(8.59658646106049,-27.948815116394,54.8606132667231));
#83784=CARTESIAN_POINT('Ctrl Pts',(8.60033059024498,-27.9452727055362,54.9299209337767));
#83785=CARTESIAN_POINT('Ctrl Pts',(8.60407471942946,-27.9452501088858,54.9993310708368));
#83786=CARTESIAN_POINT('Ctrl Pts',(8.60407471946233,-27.9452501088856,54.9993310714461));
#83787=CARTESIAN_POINT('Ctrl Pts',(8.60802536616343,-27.9452262658779,55.0725697113247));
#83788=CARTESIAN_POINT('Ctrl Pts',(8.61197601286453,-27.9491224942341,55.1457764209575));
#83789=CARTESIAN_POINT('Ctrl Pts',(8.61592665956562,-27.9569024004591,55.2185171875399));
#83790=CARTESIAN_POINT('Ctrl Pts',(8.61988032372518,-27.964688248887,55.2913135126822));
#83791=CARTESIAN_POINT('Ctrl Pts',(8.62383398788475,-27.9763636264396,55.3636427387966));
#83792=CARTESIAN_POINT('Ctrl Pts',(8.62778765204431,-27.9918406472823,55.4350788165292));
#83793=CARTESIAN_POINT('Ctrl Pts',(8.63174855419895,-28.0073460019935,55.5066456726886));
#83794=CARTESIAN_POINT('Ctrl Pts',(8.63570945635358,-28.0266667958937,55.5773156752853));
#83795=CARTESIAN_POINT('Ctrl Pts',(8.63967035850822,-28.0496647215581,55.6466760117438));
#83796=CARTESIAN_POINT('Ctrl Pts',(8.64363545525019,-28.072687001979,55.7161098006577));
#83797=CARTESIAN_POINT('Ctrl Pts',(8.64760055199216,-28.0993940051616,55.7842307419675));
#83798=CARTESIAN_POINT('Ctrl Pts',(8.65156564873413,-28.1295995338212,55.8506466120653));
#83799=CARTESIAN_POINT('Ctrl Pts',(8.65553891552182,-28.1598673006975,55.9171993314586));
#83800=CARTESIAN_POINT('Ctrl Pts',(8.6595121823095,-28.1936477762703,55.9820395665411));
#83801=CARTESIAN_POINT('Ctrl Pts',(8.66348544909719,-28.2307093656716,56.0448005617236));
#83802=CARTESIAN_POINT('Ctrl Pts',(8.66444921604389,-28.2396991307103,56.0600240480715));
#83803=CARTESIAN_POINT('Ctrl Pts',(8.66541298299059,-28.2488817522033,56.0751253418758));
#83804=CARTESIAN_POINT('Ctrl Pts',(8.66637674993729,-28.2582535611019,56.090099493205));
#83805=CARTESIAN_POINT('Ctrl Pts',(8.67024584448533,-28.2958771949471,56.1502140338289));
#83806=CARTESIAN_POINT('Ctrl Pts',(8.67411493903338,-28.3366903556877,56.208496216297));
#83807=CARTESIAN_POINT('Ctrl Pts',(8.67798403358143,-28.3804888083777,56.2645873092476));
#83808=CARTESIAN_POINT('Ctrl Pts',(8.6818473633506,-28.4242220033203,56.3205948289634));
#83809=CARTESIAN_POINT('Ctrl Pts',(8.68571069311978,-28.4709313646131,56.3744173595926));
#83810=CARTESIAN_POINT('Ctrl Pts',(8.68957402288896,-28.5203686578006,56.4257239051378));
#83811=CARTESIAN_POINT('Ctrl Pts',(8.69343282090788,-28.5697479602187,56.4769702672493));
#83812=CARTESIAN_POINT('Ctrl Pts',(8.6972916189268,-28.6218485029957,56.5257061584302));
#83813=CARTESIAN_POINT('Ctrl Pts',(8.70115041694573,-28.6763820702183,56.5716339072635));
#83814=CARTESIAN_POINT('Ctrl Pts',(8.70500678414222,-28.7308812844071,56.6175327242373));
#83815=CARTESIAN_POINT('Ctrl Pts',(8.70886315133872,-28.7878101115706,56.6606265962843));
#83816=CARTESIAN_POINT('Ctrl Pts',(8.71271951853521,-28.84684487025,56.7006559937951));
#83817=CARTESIAN_POINT('Ctrl Pts',(8.71657474643865,-28.9058621881913,56.7406735653536));
#83818=CARTESIAN_POINT('Ctrl Pts',(8.72042997434208,-28.9669838006437,56.7776281872548));
#83819=CARTESIAN_POINT('Ctrl Pts',(8.72428520224552,-29.0298558657819,56.8113028243069));
#83820=CARTESIAN_POINT('Ctrl Pts',(8.7281405807723,-29.0927303873249,56.8449787770235));
#83821=CARTESIAN_POINT('Ctrl Pts',(8.73199595929907,-29.1573550680685,56.8753742630506));
#83822=CARTESIAN_POINT('Ctrl Pts',(8.73585133782585,-29.2233517508641,56.9023183381375));
#83823=CARTESIAN_POINT('Ctrl Pts',(8.73971075184615,-29.2894175135656,56.9292906160687));
#83824=CARTESIAN_POINT('Ctrl Pts',(8.74357016586645,-29.3568576944318,56.9528040874015));
#83825=CARTESIAN_POINT('Ctrl Pts',(8.74742957988676,-29.4252752922519,56.9727364428134));
#83826=CARTESIAN_POINT('Ctrl Pts',(8.7512911790046,-29.4937316262956,56.9926800833945));
#83827=CARTESIAN_POINT('Ctrl Pts',(8.75515277812243,-29.5631660058587,57.0090384604104));
#83828=CARTESIAN_POINT('Ctrl Pts',(8.75901437724027,-29.6331701295281,57.0217401931578));
#83829=CARTESIAN_POINT('Ctrl Pts',(8.76288273257591,-29.7032967317593,57.0344641487383));
#83830=CARTESIAN_POINT('Ctrl Pts',(8.76675108791155,-29.7739945862777,57.0435186252626));
#83831=CARTESIAN_POINT('Ctrl Pts',(8.77061944324719,-29.8448498484024,57.048884084803));
#83832=CARTESIAN_POINT('Ctrl Pts',(8.77291696909007,-29.8869327962474,57.0520707832533));
#83833=CARTESIAN_POINT('Ctrl Pts',(8.77521449493296,-29.9290712407228,57.0539571768661));
#83834=CARTESIAN_POINT('Ctrl Pts',(8.77751202077585,-29.9711789821164,57.0545478605835));
#83835=CARTESIAN_POINT('Ctrl Pts',(8.78138026094705,-30.0420738785901,57.0555423679972));
#83836=CARTESIAN_POINT('Ctrl Pts',(8.78524850111824,-30.1131591787548,57.0528650336868));
#83837=CARTESIAN_POINT('Ctrl Pts',(8.78911674128944,-30.1840229876492,57.046492878687));
#83838=CARTESIAN_POINT('Ctrl Pts',(8.79297960149185,-30.2547882387852,57.0401295861139));
#83839=CARTESIAN_POINT('Ctrl Pts',(8.79684246169427,-30.3253321302883,57.0300817109936));
#83840=CARTESIAN_POINT('Ctrl Pts',(8.80070532189668,-30.3952420799265,57.0163782533928));
#83841=CARTESIAN_POINT('Ctrl Pts',(8.80456410253959,-30.4650781977964,57.0026892679882));
#83842=CARTESIAN_POINT('Ctrl Pts',(8.8084228831825,-30.5342812283326,56.9853524557353));
#83843=CARTESIAN_POINT('Ctrl Pts',(8.81228166382541,-30.602444754302,56.9644484927109));
#83844=CARTESIAN_POINT('Ctrl Pts',(8.81613799809855,-30.6705650663122,56.9435577822727));
#83845=CARTESIAN_POINT('Ctrl Pts',(8.81999433237169,-30.7376467179062,56.919104550155));
#83846=CARTESIAN_POINT('Ctrl Pts',(8.82385066664483,-30.8032961041465,56.8912199585355));
#83847=CARTESIAN_POINT('Ctrl Pts',(8.82770557351924,-30.868921190665,56.8633456882283));
#83848=CARTESIAN_POINT('Ctrl Pts',(8.83156048039366,-30.9331146192322,56.8320427739045));
#83849=CARTESIAN_POINT('Ctrl Pts',(8.83541538726808,-30.9955022105465,56.7974907263452));
#83850=CARTESIAN_POINT('Ctrl Pts',(8.83927123894508,-31.0579050924915,56.7629302103936));
#83851=CARTESIAN_POINT('Ctrl Pts',(8.84312709062208,-31.1185008279476,56.7251192060502));
#83852=CARTESIAN_POINT('Ctrl Pts',(8.84698294229908,-31.176940552369,56.6842827846562));
#83853=CARTESIAN_POINT('Ctrl Pts',(8.84866235106974,-31.2023938617725,56.6664965599784));
#83854=CARTESIAN_POINT('Ctrl Pts',(8.85034175984041,-31.2274385369056,56.6481369675613));
#83855=CARTESIAN_POINT('Ctrl Pts',(8.85202116861107,-31.2520475724682,56.6292251037768));
#83856=CARTESIAN_POINT('',(8.54592528048674,-27.9452503479084,55.0011957129338));
#83857=CARTESIAN_POINT('Ctrl Pts',(8.54592528053768,-27.9452503479089,55.0011957138689));
#83858=CARTESIAN_POINT('Ctrl Pts',(8.54975547188148,-27.9452912658151,55.0715102394494));
#83859=CARTESIAN_POINT('Ctrl Pts',(8.55358566322528,-27.9489412102894,55.1417182661176));
#83860=CARTESIAN_POINT('Ctrl Pts',(8.55741585456908,-27.956169205503,55.21154963003));
#83861=CARTESIAN_POINT('Ctrl Pts',(8.56128493120739,-27.9634705815735,55.2820899436809));
#83862=CARTESIAN_POINT('Ctrl Pts',(8.5651540078457,-27.974442464725,55.3523899847241));
#83863=CARTESIAN_POINT('Ctrl Pts',(8.56902308448401,-27.9890594966833,55.4220377407537));
#83864=CARTESIAN_POINT('Ctrl Pts',(8.57288639619077,-28.0036547492363,55.4915817214946));
#83865=CARTESIAN_POINT('Ctrl Pts',(8.57674970789754,-28.0218842706945,55.5604748748738));
#83866=CARTESIAN_POINT('Ctrl Pts',(8.58061301960431,-28.0436709850475,55.6283107095657));
#83867=CARTESIAN_POINT('Ctrl Pts',(8.58447179942306,-28.0654321423248,55.6960669689011));
#83868=CARTESIAN_POINT('Ctrl Pts',(8.58833057924181,-28.0907420560937,55.7627679129253));
#83869=CARTESIAN_POINT('Ctrl Pts',(8.59218935906055,-28.1194730782315,55.8280193590755));
#83870=CARTESIAN_POINT('Ctrl Pts',(8.59604570798193,-28.1481860008224,55.8932296990791));
#83871=CARTESIAN_POINT('Ctrl Pts',(8.59990205690332,-28.1803155606427,55.9569919093067));
#83872=CARTESIAN_POINT('Ctrl Pts',(8.6037584058247,-28.2156854700809,56.0189304298232));
#83873=CARTESIAN_POINT('Ctrl Pts',(8.60761361540559,-28.2510449296426,56.0808506508897));
#83874=CARTESIAN_POINT('Ctrl Pts',(8.61146882498649,-28.2896425974598,56.1409478302951));
#83875=CARTESIAN_POINT('Ctrl Pts',(8.61532403456738,-28.3312563923001,56.1988712751003));
#83876=CARTESIAN_POINT('Ctrl Pts',(8.61917939475162,-28.3728718127788,56.2567969826786));
#83877=CARTESIAN_POINT('Ctrl Pts',(8.62303475493585,-28.4175033089793,56.3125483938257));
#83878=CARTESIAN_POINT('Ctrl Pts',(8.62689011512009,-28.4648866696248,56.3658054859329));
#83879=CARTESIAN_POINT('Ctrl Pts',(8.6307495108947,-28.512319628706,56.4191183247921));
#83880=CARTESIAN_POINT('Ctrl Pts',(8.6346089066693,-28.5625098788081,56.4699312689458));
#83881=CARTESIAN_POINT('Ctrl Pts',(8.63846830244391,-28.6151548701809,56.5179596598449));
#83882=CARTESIAN_POINT('Ctrl Pts',(8.64232988334319,-28.6678296682582,56.5660152436072));
#83883=CARTESIAN_POINT('Ctrl Pts',(8.64619146424246,-28.7229615987137,56.6112828272418));
#83884=CARTESIAN_POINT('Ctrl Pts',(8.65005304514174,-28.7802155359329,56.6535184981489));
#83885=CARTESIAN_POINT('Ctrl Pts',(8.65392138250044,-28.8375696481618,56.6958280671833));
#83886=CARTESIAN_POINT('Ctrl Pts',(8.65778971985915,-28.8970527743099,56.7350948645475));
#83887=CARTESIAN_POINT('Ctrl Pts',(8.66165805721786,-28.9583019787723,56.7711190798674));
#83888=CARTESIAN_POINT('Ctrl Pts',(8.66395574661445,-28.9946823754629,56.7925165046227));
#83889=CARTESIAN_POINT('Ctrl Pts',(8.66625343601104,-29.031685386149,56.8127708165083));
#83890=CARTESIAN_POINT('Ctrl Pts',(8.66855112540763,-29.0692315807068,56.8318481684207));
#83891=CARTESIAN_POINT('Ctrl Pts',(8.67242018909353,-29.1324553646189,56.8639723927031));
#83892=CARTESIAN_POINT('Ctrl Pts',(8.67628925277942,-29.1974680298235,56.8928825728788));
#83893=CARTESIAN_POINT('Ctrl Pts',(8.68015831646531,-29.2639096761121,56.9183765526034));
#83894=CARTESIAN_POINT('Ctrl Pts',(8.68402161519355,-29.3302523234416,56.9438325459506));
#83895=CARTESIAN_POINT('Ctrl Pts',(8.68788491392178,-29.3980192755995,56.9658822701096));
#83896=CARTESIAN_POINT('Ctrl Pts',(8.69174821265001,-29.4668272208466,56.9843700133972));
#83897=CARTESIAN_POINT('Ctrl Pts',(8.69560697951371,-29.5355544505424,57.0028360695324));
#83898=CARTESIAN_POINT('Ctrl Pts',(8.69946574637741,-29.605319780853,57.0177483190721));
#83899=CARTESIAN_POINT('Ctrl Pts',(8.70332451324111,-29.6757228125058,57.0290002139406));
#83900=CARTESIAN_POINT('Ctrl Pts',(8.70718084922889,-29.7460814929344,57.0402450205445));
#83901=CARTESIAN_POINT('Ctrl Pts',(8.71103718521667,-29.8170765991176,57.0478339708275));
#83902=CARTESIAN_POINT('Ctrl Pts',(8.71489352120445,-29.8882969970362,57.0517114810881));
#83903=CARTESIAN_POINT('Ctrl Pts',(8.71874871789197,-29.9594963538895,57.0555878457929));
#83904=CARTESIAN_POINT('Ctrl Pts',(8.7226039145795,-30.0309203855335,57.0557549209219));
#83905=CARTESIAN_POINT('Ctrl Pts',(8.72645911126702,-30.1021540129104,57.0522090829509));
#83906=CARTESIAN_POINT('Ctrl Pts',(8.73031445861694,-30.1733904241217,57.0486631064074));
#83907=CARTESIAN_POINT('Ctrl Pts',(8.73416980596685,-30.2444359312142,57.0414039550345));
#83908=CARTESIAN_POINT('Ctrl Pts',(8.73802515331677,-30.3148783727667,57.0304800350813));
#83909=CARTESIAN_POINT('Ctrl Pts',(8.74188453643489,-30.3853945532952,57.0195446799954));
#83910=CARTESIAN_POINT('Ctrl Pts',(8.74574391955302,-30.4553059270577,57.0049369728678));
#83911=CARTESIAN_POINT('Ctrl Pts',(8.74960330267114,-30.5242092501069,56.9867567099679));
#83912=CARTESIAN_POINT('Ctrl Pts',(8.75346487099512,-30.5931515866305,56.9685661532941));
#83913=CARTESIAN_POINT('Ctrl Pts',(8.75732643931909,-30.6610842733858,56.9467991623766));
#83914=CARTESIAN_POINT('Ctrl Pts',(8.76118800764307,-30.727620630972,56.9216050010041));
#83915=CARTESIAN_POINT('Ctrl Pts',(8.76505633269088,-30.7942734095965,56.8963667565087));
#83916=CARTESIAN_POINT('Ctrl Pts',(8.7689246577387,-30.8595245362443,56.8676895646065));
#83917=CARTESIAN_POINT('Ctrl Pts',(8.77279298278651,-30.9230093006504,56.8357699729032));
#83918=CARTESIAN_POINT('Ctrl Pts',(8.77509078727307,-30.9607195692233,56.8168095752844));
#83919=CARTESIAN_POINT('Ctrl Pts',(8.77738859175963,-30.9978070811695,56.7967059942276));
#83920=CARTESIAN_POINT('Ctrl Pts',(8.77968639624619,-31.0342003092193,56.7755076127437));
#83921=CARTESIAN_POINT('Ctrl Pts',(8.78355540384214,-31.0954786627907,56.7398141064151));
#83922=CARTESIAN_POINT('Ctrl Pts',(8.78742441143808,-31.155027029067,56.7008746007601));
#83923=CARTESIAN_POINT('Ctrl Pts',(8.79129341903402,-31.2124803894351,56.6588818124675));
#83924=CARTESIAN_POINT('Ctrl Pts',(8.79218924787603,-31.2257831230203,56.6491588150383));
#83925=CARTESIAN_POINT('Ctrl Pts',(8.79308507671804,-31.2389736349695,56.6392723290926));
#83926=CARTESIAN_POINT('Ctrl Pts',(8.79398090556005,-31.2520475724682,56.6292251037768));
#83927=CARTESIAN_POINT('Ctrl Pts',(8.09385946080458,-31.2520475724682,56.6292251037768));
#83928=CARTESIAN_POINT('Ctrl Pts',(8.09772772586411,-31.3085644633221,56.5857922866461));
#83929=CARTESIAN_POINT('Ctrl Pts',(8.10159599092365,-31.3627460064793,56.5394711533693));
#83930=CARTESIAN_POINT('Ctrl Pts',(8.10546425598318,-31.4142995210562,56.4905550735347));
#83931=CARTESIAN_POINT('Ctrl Pts',(8.10793442772706,-31.4472202317744,56.4593185588778));
#83932=CARTESIAN_POINT('Ctrl Pts',(8.11040459947095,-31.4790700476866,56.4270246328561));
#83933=CARTESIAN_POINT('Ctrl Pts',(8.11287477121484,-31.509781418586,56.3937566611832));
#83934=CARTESIAN_POINT('Ctrl Pts',(8.11674384460076,-31.5578851782077,56.3416484528685));
#83935=CARTESIAN_POINT('Ctrl Pts',(8.12061291798669,-31.6033823195331,56.286944893517));
#83936=CARTESIAN_POINT('Ctrl Pts',(8.12448199137262,-31.6459804498429,56.2299373647609));
#83937=CARTESIAN_POINT('Ctrl Pts',(8.12834529980472,-31.6885151085589,56.1730147777307));
#83938=CARTESIAN_POINT('Ctrl Pts',(8.13220860823683,-31.7281590420354,56.1137954215491));
#83939=CARTESIAN_POINT('Ctrl Pts',(8.13607191666893,-31.7646581875197,56.0526058349257));
#83940=CARTESIAN_POINT('Ctrl Pts',(8.13993069319594,-31.8011145171983,55.9914880275569));
#83941=CARTESIAN_POINT('Ctrl Pts',(8.14378946972296,-31.8344331389063,55.9284049957583));
#83942=CARTESIAN_POINT('Ctrl Pts',(8.14764824624997,-31.8644026557454,55.8637130887913));
#83943=CARTESIAN_POINT('Ctrl Pts',(8.1515045918709,-31.8943532927452,55.7990619356616));
#83944=CARTESIAN_POINT('Ctrl Pts',(8.15536093749182,-31.9209588070259,55.7328043579523));
#83945=CARTESIAN_POINT('Ctrl Pts',(8.15921728311275,-31.9440539276629,55.6653208916294));
#83946=CARTESIAN_POINT('Ctrl Pts',(8.16307248938938,-31.9671422249244,55.5978573630688));
#83947=CARTESIAN_POINT('Ctrl Pts',(8.16692769566601,-31.9867220303301,55.5291691242961));
#83948=CARTESIAN_POINT('Ctrl Pts',(8.17078290194264,-32.0026770032117,55.4596546348149));
#83949=CARTESIAN_POINT('Ctrl Pts',(8.17463825882374,-32.0186325993778,55.3901374297353));
#83950=CARTESIAN_POINT('Ctrl Pts',(8.17849361570483,-32.0309629753566,55.3197943838317));
#83951=CARTESIAN_POINT('Ctrl Pts',(8.18234897258592,-32.0396026535511,55.2490352949432));
#83952=CARTESIAN_POINT('Ctrl Pts',(8.18620836508193,-32.0482513753737,55.1782021386094));
#83953=CARTESIAN_POINT('Ctrl Pts',(8.19006775757793,-32.0532016284849,55.1069525531374));
#83954=CARTESIAN_POINT('Ctrl Pts',(8.19392715007394,-32.0544398139621,55.0357017269505));
#83955=CARTESIAN_POINT('Ctrl Pts',(8.19778872770351,-32.0556787004825,54.9644105595513));
#83956=CARTESIAN_POINT('Ctrl Pts',(8.20165030533308,-32.0532013523708,54.8931186357618));
#83957=CARTESIAN_POINT('Ctrl Pts',(8.20551188296266,-32.0470462784205,54.8222386529506));
#83958=CARTESIAN_POINT('Ctrl Pts',(8.20938021710133,-32.040880435086,54.7512346531456));
#83959=CARTESIAN_POINT('Ctrl Pts',(8.21324855124,-32.0310240857909,54.680644514615));
#83960=CARTESIAN_POINT('Ctrl Pts',(8.21711688537867,-32.0175672150315,54.6108726489568));
#83961=CARTESIAN_POINT('Ctrl Pts',(8.21941460427025,-32.0095740828313,54.5694294519433));
#83962=CARTESIAN_POINT('Ctrl Pts',(8.22171232316183,-32.0003116078501,54.5282747183277));
#83963=CARTESIAN_POINT('Ctrl Pts',(8.2240100420534,-31.9898069000022,54.4874904262323));
#83964=CARTESIAN_POINT('Ctrl Pts',(8.2278791158888,-31.9721182739341,54.4188147331265));
#83965=CARTESIAN_POINT('Ctrl Pts',(8.23174818972419,-31.9508354434352,54.3509213488541));
#83966=CARTESIAN_POINT('Ctrl Pts',(8.23561726355958,-31.9260446276857,54.2842139602764));
#83967=CARTESIAN_POINT('Ctrl Pts',(8.239480572445,-31.9012907504436,54.2176059662243));
#83968=CARTESIAN_POINT('Ctrl Pts',(8.24334388133041,-31.8730394310988,54.1521809117855));
#83969=CARTESIAN_POINT('Ctrl Pts',(8.24720719021583,-31.8414272146186,54.0883293490729));
#83970=CARTESIAN_POINT('Ctrl Pts',(8.25106596719964,-31.8098520812346,54.0245526882147));
#83971=CARTESIAN_POINT('Ctrl Pts',(8.25492474418344,-31.774924096428,53.9623462859312));
#83972=CARTESIAN_POINT('Ctrl Pts',(8.25878352116725,-31.7368279907332,53.9020810170574));
#83973=CARTESIAN_POINT('Ctrl Pts',(8.26263986724686,-31.6987558843479,53.841853713346));
#83974=CARTESIAN_POINT('Ctrl Pts',(8.26649621332647,-31.657519875693,53.7835655265795));
#83975=CARTESIAN_POINT('Ctrl Pts',(8.27035255940609,-31.6133500326752,53.7275616971473));
#83976=CARTESIAN_POINT('Ctrl Pts',(8.27420776614261,-31.5691932394731,53.6715744138379));
#83977=CARTESIAN_POINT('Ctrl Pts',(8.27806297287914,-31.5221046333941,53.6178705292117));
#83978=CARTESIAN_POINT('Ctrl Pts',(8.28191817961566,-31.4723558787003,53.5667638962973));
#83979=CARTESIAN_POINT('Ctrl Pts',(8.28577353695716,-31.4226051805542,53.5156552668848));
#83980=CARTESIAN_POINT('Ctrl Pts',(8.28962889429866,-31.3701944678999,53.4671444371841));
#83981=CARTESIAN_POINT('Ctrl Pts',(8.29348425164016,-31.3154325171293,53.4215086774458));
#83982=CARTESIAN_POINT('Ctrl Pts',(8.29734364459416,-31.2606132440424,53.3758251482724));
#83983=CARTESIAN_POINT('Ctrl Pts',(8.30120303754816,-31.2034381937461,53.3330230083174));
#83984=CARTESIAN_POINT('Ctrl Pts',(8.30506243050216,-31.1442488086253,53.2933388659551));
#83985=CARTESIAN_POINT('Ctrl Pts',(8.30892400858906,-31.0850259113242,53.2536322550009));
#83986=CARTESIAN_POINT('Ctrl Pts',(8.31278558667596,-31.0237868260713,53.2170474051958));
#83987=CARTESIAN_POINT('Ctrl Pts',(8.31664716476286,-30.960899163762,53.1837757958937));
#83988=CARTESIAN_POINT('Ctrl Pts',(8.32051549935281,-30.8979014685404,53.1504459721195));
#83989=CARTESIAN_POINT('Ctrl Pts',(8.32438383394277,-30.8332498781125,53.1204411674763));
#83990=CARTESIAN_POINT('Ctrl Pts',(8.32825216853272,-30.76733296071,53.0939051204339));
#83991=CARTESIAN_POINT('Ctrl Pts',(8.33054988331913,-30.7281796061413,53.0781432295622));
#83992=CARTESIAN_POINT('Ctrl Pts',(8.33284759810555,-30.6885801579557,53.0636042166874));
#83993=CARTESIAN_POINT('Ctrl Pts',(8.33514531289196,-30.648618192526,53.0503097674696));
#83994=CARTESIAN_POINT('Ctrl Pts',(8.33901438504392,-30.5813271046607,53.027923532438));
#83995=CARTESIAN_POINT('Ctrl Pts',(8.34288345719589,-30.5127439015,53.0089812381448));
#83996=CARTESIAN_POINT('Ctrl Pts',(8.34675252934785,-30.4432544997986,52.99362939343));
#83997=CARTESIAN_POINT('Ctrl Pts',(8.3506158365476,-30.3738686379293,52.9783004231015));
#83998=CARTESIAN_POINT('Ctrl Pts',(8.35447914374734,-30.3035797281994,52.9665513870857));
#83999=CARTESIAN_POINT('Ctrl Pts',(8.35834245094709,-30.2327899472138,52.9584793895294));
#84000=CARTESIAN_POINT('Ctrl Pts',(8.36220122624996,-30.1620832069936,52.9504168609225));
#84001=CARTESIAN_POINT('Ctrl Pts',(8.36606000155283,-30.0908772429123,52.9460228576887));
#84002=CARTESIAN_POINT('Ctrl Pts',(8.36991877685571,-30.0195838339789,52.9453433289363));
#84003=CARTESIAN_POINT('Ctrl Pts',(8.37377512125821,-29.9483353375269,52.9446642282644));
#84004=CARTESIAN_POINT('Ctrl Pts',(8.37763146566071,-29.8769999901311,52.9476949641797));
#84005=CARTESIAN_POINT('Ctrl Pts',(8.38148781006321,-29.8059926235627,52.9544294926872));
#84006=CARTESIAN_POINT('Ctrl Pts',(8.38534301512887,-29.7350062357504,52.9611620315134));
#84007=CARTESIAN_POINT('Ctrl Pts',(8.38919822019453,-29.6643481197445,52.9715961446681));
#84008=CARTESIAN_POINT('Ctrl Pts',(8.3930534252602,-29.5944292978043,52.9856738178685));
#84009=CARTESIAN_POINT('Ctrl Pts',(8.39690878093952,-29.5245077443027,52.9997520410499));
#84010=CARTESIAN_POINT('Ctrl Pts',(8.40076413661884,-29.4553260180037,53.0174740088399));
#84011=CARTESIAN_POINT('Ctrl Pts',(8.40461949229815,-29.3872845346697,53.0387306862531));
#84012=CARTESIAN_POINT('Ctrl Pts',(8.40847888361457,-29.3191718281447,53.0600096143335));
#84013=CARTESIAN_POINT('Ctrl Pts',(8.41233827493098,-29.2522022118387,53.0848304929071));
#84014=CARTESIAN_POINT('Ctrl Pts',(8.41619766624739,-29.1867596565612,53.1130347893235));
#84015=CARTESIAN_POINT('Ctrl Pts',(8.42005924270809,-29.1212800484394,53.1412550546977));
#84016=CARTESIAN_POINT('Ctrl Pts',(8.42392081916879,-29.0573296582121,53.172862336044));
#84017=CARTESIAN_POINT('Ctrl Pts',(8.42778239562949,-28.9952687346829,53.2076516390516));
#84018=CARTESIAN_POINT('Ctrl Pts',(8.43165072862884,-28.9330992241472,53.242501812347));
#84019=CARTESIAN_POINT('Ctrl Pts',(8.43551906162818,-28.8728261917055,53.2805448636724));
#84020=CARTESIAN_POINT('Ctrl Pts',(8.43938739462753,-28.8147811434618,53.3215322986109));
#84021=CARTESIAN_POINT('Ctrl Pts',(8.44168512432852,-28.7803032866259,53.3458781981604));
#84022=CARTESIAN_POINT('Ctrl Pts',(8.44398285402952,-28.7466108877596,53.3712621390403));
#84023=CARTESIAN_POINT('Ctrl Pts',(8.44628058373051,-28.713767495987,53.39762566542));
#84024=CARTESIAN_POINT('Ctrl Pts',(8.45010049356798,-28.6591662975635,53.4414542731647));
#84025=CARTESIAN_POINT('Ctrl Pts',(8.45392040340544,-28.6066877347304,53.4881735901039));
#84026=CARTESIAN_POINT('Ctrl Pts',(8.4577403132429,-28.5566598033146,53.5375477309901));
#84027=CARTESIAN_POINT('Ctrl Pts',(8.46155371487502,-28.5067171074317,53.5868377502448));
#84028=CARTESIAN_POINT('Ctrl Pts',(8.46536711650714,-28.4592171051878,53.6387732652591));
#84029=CARTESIAN_POINT('Ctrl Pts',(8.46918051813926,-28.4144553668289,53.6930777457238));
#84030=CARTESIAN_POINT('Ctrl Pts',(8.47299028959279,-28.3697362395348,53.7473305308832));
#84031=CARTESIAN_POINT('Ctrl Pts',(8.47680006104632,-28.3277505256955,53.803947428803));
#84032=CARTESIAN_POINT('Ctrl Pts',(8.48060983249986,-28.2887564798592,53.8626156422404));
#84033=CARTESIAN_POINT('Ctrl Pts',(8.48441732945581,-28.2497857141235,53.9212488297686));
#84034=CARTESIAN_POINT('Ctrl Pts',(8.48822482641176,-28.2138033505418,53.98193048944));
#84035=CARTESIAN_POINT('Ctrl Pts',(8.49203232336772,-28.1810257351875,54.0443169006151));
#84036=CARTESIAN_POINT('Ctrl Pts',(8.49583889832167,-28.1482560570759,54.1066882046485));
#84037=CARTESIAN_POINT('Ctrl Pts',(8.49964547327562,-28.1186898182962,54.1707629985846));
#84038=CARTESIAN_POINT('Ctrl Pts',(8.50345204822957,-28.0924976487741,54.2361725701655));
#84039=CARTESIAN_POINT('Ctrl Pts',(8.50726133448231,-28.0662868234265,54.3016287308442));
#84040=CARTESIAN_POINT('Ctrl Pts',(8.51107062073505,-28.0434550559848,54.3684211046283));
#84041=CARTESIAN_POINT('Ctrl Pts',(8.51487990698779,-28.0241245176057,54.4361616893354));
#84042=CARTESIAN_POINT('Ctrl Pts',(8.51869055154789,-28.0047870863836,54.503926428839));
#84043=CARTESIAN_POINT('Ctrl Pts',(8.52250119610798,-27.988953484362,54.5726395657635));
#84044=CARTESIAN_POINT('Ctrl Pts',(8.52631184066808,-27.9766950474164,54.6419013664494));
#84045=CARTESIAN_POINT('Ctrl Pts',(8.53012846727584,-27.9644173668618,54.7112718960882));
#84046=CARTESIAN_POINT('Ctrl Pts',(8.5339450938836,-27.9557261209346,54.7811923133063));
#84047=CARTESIAN_POINT('Ctrl Pts',(8.53776172049136,-27.9506408049551,54.8512570936646));
#84048=CARTESIAN_POINT('Ctrl Pts',(8.54048290715649,-27.9470150654072,54.9012120317815));
#84049=CARTESIAN_POINT('Ctrl Pts',(8.54320409382162,-27.9452212775139,54.95124025844));
#84050=CARTESIAN_POINT('Ctrl Pts',(8.54592528048675,-27.9452503479084,55.0011957129338));
#84051=CARTESIAN_POINT('Origin',(-1.54592528053767,-30.,55.));
#84052=CARTESIAN_POINT('',(7.39391310379067,-31.2520475724682,56.6292251037768));
#84053=CARTESIAN_POINT('',(7.45211324645396,-31.2520475724682,56.6292251037768));
#84054=CARTESIAN_POINT('',(-1.54592528053767,-31.2520475724682,56.6292251037768));
#84055=CARTESIAN_POINT('',(7.9040747195078,-27.9452505543666,54.9984906394943));
#84056=CARTESIAN_POINT('Ctrl Pts',(7.45211324645396,-31.2520475724682,56.6292251037768));
#84057=CARTESIAN_POINT('Ctrl Pts',(7.45597808729066,-31.3083605687531,56.5859489781306));
#84058=CARTESIAN_POINT('Ctrl Pts',(7.45984292812737,-31.362520824477,56.5396778615538));
#84059=CARTESIAN_POINT('Ctrl Pts',(7.46370776896407,-31.4141940637171,56.4906551286757));
#84060=CARTESIAN_POINT('Ctrl Pts',(7.4675674980657,-31.4657989586397,56.4416972344893));
#84061=CARTESIAN_POINT('Ctrl Pts',(7.47142722716733,-31.5149230210412,56.3899952859469));
#84062=CARTESIAN_POINT('Ctrl Pts',(7.47528695626896,-31.561264698516,56.3358331122066));
#84063=CARTESIAN_POINT('Ctrl Pts',(7.47914387729268,-31.6075726609198,56.2817103432016));
#84064=CARTESIAN_POINT('Ctrl Pts',(7.4830007983164,-31.6511019392643,56.2251312676947));
#84065=CARTESIAN_POINT('Ctrl Pts',(7.48685771934013,-31.6915885447453,56.1664157739788));
#84066=CARTESIAN_POINT('Ctrl Pts',(7.49071312456391,-31.7320592386756,56.1077233559083));
#84067=CARTESIAN_POINT('Ctrl Pts',(7.49456852978768,-31.7694893575694,56.0468965856172));
#84068=CARTESIAN_POINT('Ctrl Pts',(7.49842393501146,-31.8036569179452,55.9842861803603));
#84069=CARTESIAN_POINT('Ctrl Pts',(7.5022791147205,-31.8378224797533,55.9216794373824));
#84070=CARTESIAN_POINT('Ctrl Pts',(7.50613429442953,-31.8687256306425,55.8572896937603));
#84071=CARTESIAN_POINT('Ctrl Pts',(7.50998947413857,-31.8961900876794,55.7914927124658));
#84072=CARTESIAN_POINT('Ctrl Pts',(7.51384844789869,-31.9236815736905,55.7256309774823));
#84073=CARTESIAN_POINT('Ctrl Pts',(7.51770742165881,-31.947727418207,55.658359687754));
#84074=CARTESIAN_POINT('Ctrl Pts',(7.52156639541893,-31.9681996651815,55.5900742669186));
#84075=CARTESIAN_POINT('Ctrl Pts',(7.52542721647184,-31.9886817122315,55.5217561578159));
#84076=CARTESIAN_POINT('Ctrl Pts',(7.52928803752475,-32.0055866384878,55.4524234231595));
#84077=CARTESIAN_POINT('Ctrl Pts',(7.53314885857766,-32.018837251576,55.3824836129156));
#84078=CARTESIAN_POINT('Ctrl Pts',(7.53701679393931,-32.032112281479,55.3124149250582));
#84079=CARTESIAN_POINT('Ctrl Pts',(7.54088472930095,-32.0417194785206,55.2417374091514));
#84080=CARTESIAN_POINT('Ctrl Pts',(7.5447526646626,-32.0476334237151,55.1708652234503));
#84081=CARTESIAN_POINT('Ctrl Pts',(7.54817645695896,-32.0528682888576,55.1081310718315));
#84082=CARTESIAN_POINT('Ctrl Pts',(7.55160024925533,-32.0552101424747,55.0452446703328));
#84083=CARTESIAN_POINT('Ctrl Pts',(7.55502404155169,-32.054675403713,54.9824914912987));
#84084=CARTESIAN_POINT('Ctrl Pts',(7.55889311489863,-32.0540711195416,54.9115769522672));
#84085=CARTESIAN_POINT('Ctrl Pts',(7.56276218824557,-32.049790052573,54.840554831208));
#84086=CARTESIAN_POINT('Ctrl Pts',(7.5666312615925,-32.0418185215203,54.7698376927544));
#84087=CARTESIAN_POINT('Ctrl Pts',(7.57049456998682,-32.0338588681175,54.6992259234463));
#84088=CARTESIAN_POINT('Ctrl Pts',(7.57435787838114,-32.0222197196123,54.6289187135154));
#84089=CARTESIAN_POINT('Ctrl Pts',(7.57822118677546,-32.0069394027378,54.5593280174115));
#84090=CARTESIAN_POINT('Ctrl Pts',(7.58207996326664,-31.9916770106337,54.4898189555605));
#84091=CARTESIAN_POINT('Ctrl Pts',(7.58593873975781,-31.9727820381229,54.4210252101677));
#84092=CARTESIAN_POINT('Ctrl Pts',(7.58979751624899,-31.9503443207461,54.3533512599304));
#84093=CARTESIAN_POINT('Ctrl Pts',(7.59365386183529,-31.9279207384083,54.2857199421016));
#84094=CARTESIAN_POINT('Ctrl Pts',(7.5975102074216,-31.9019589916094,54.2192074798691));
#84095=CARTESIAN_POINT('Ctrl Pts',(7.6013665530079,-31.8725990972371,54.1542044079526));
#84096=CARTESIAN_POINT('Ctrl Pts',(7.60522175925117,-31.843247877137,54.0892205409531));
#84097=CARTESIAN_POINT('Ctrl Pts',(7.60907696549444,-31.8105007024769,54.0257456214283));
#84098=CARTESIAN_POINT('Ctrl Pts',(7.61293217173771,-31.7745455283029,53.9641497548004));
#84099=CARTESIAN_POINT('Ctrl Pts',(7.61678752858674,-31.7385889495202,53.902551481896));
#84100=CARTESIAN_POINT('Ctrl Pts',(7.62064288543577,-31.6994243692117,53.8428328260564));
#84101=CARTESIAN_POINT('Ctrl Pts',(7.6244982422848,-31.6572845816706,53.7853373398935));
#84102=CARTESIAN_POINT('Ctrl Pts',(7.62835763475092,-31.615100684063,53.7277816699978));
#84103=CARTESIAN_POINT('Ctrl Pts',(7.63221702721703,-31.5699356501099,53.6724542078444));
#84104=CARTESIAN_POINT('Ctrl Pts',(7.63607641968315,-31.522063782187,53.6196669222776));
#84105=CARTESIAN_POINT('Ctrl Pts',(7.63993799728402,-31.4741648098732,53.5668497492782));
#84106=CARTESIAN_POINT('Ctrl Pts',(7.64379957488489,-31.4235562975153,53.5165759584269));
#84107=CARTESIAN_POINT('Ctrl Pts',(7.64766115248575,-31.3705488271908,53.4691200325349));
#84108=CARTESIAN_POINT('Ctrl Pts',(7.65152948659789,-31.3174486109455,53.4215810741284));
#84109=CARTESIAN_POINT('Ctrl Pts',(7.65539782071002,-31.2619414349407,53.3768701291034));
#84110=CARTESIAN_POINT('Ctrl Pts',(7.65926615482215,-31.2043697334878,53.3352204027084));
#84111=CARTESIAN_POINT('Ctrl Pts',(7.66156387401152,-31.1701732035712,53.3104812326171));
#84112=CARTESIAN_POINT('Ctrl Pts',(7.66386159320088,-31.135248827559,53.286821267397));
#84113=CARTESIAN_POINT('Ctrl Pts',(7.66615931239025,-31.0996724855831,53.2642817086429));
#84114=CARTESIAN_POINT('Ctrl Pts',(7.6700283858083,-31.0397663492338,53.2263278942544));
#84115=CARTESIAN_POINT('Ctrl Pts',(7.67389745922635,-30.9777756735512,53.1914047567586));
#84116=CARTESIAN_POINT('Ctrl Pts',(7.67776653264439,-30.9140396518326,53.1597475506394));
#84117=CARTESIAN_POINT('Ctrl Pts',(7.68162984111029,-30.8503985973261,53.1281375140253));
#84118=CARTESIAN_POINT('Ctrl Pts',(7.68549314957619,-30.7850177903921,53.0997839637252));
#84119=CARTESIAN_POINT('Ctrl Pts',(7.68935645804209,-30.7182641189677,53.0748781290777));
#84120=CARTESIAN_POINT('Ctrl Pts',(7.69321523460519,-30.6515887537808,53.0500015105341));
#84121=CARTESIAN_POINT('Ctrl Pts',(7.69707401116829,-30.5835441759438,53.0285647431122));
#84122=CARTESIAN_POINT('Ctrl Pts',(7.70093278773139,-30.5145189292144,53.0107117267776));
#84123=CARTESIAN_POINT('Ctrl Pts',(7.7047891333898,-30.4455371661628,52.9928699572672));
#84124=CARTESIAN_POINT('Ctrl Pts',(7.7086454790482,-30.3755764291012,52.9786075810634));
#84125=CARTESIAN_POINT('Ctrl Pts',(7.7125018247066,-30.3050407634035,52.9680187758835));
#84126=CARTESIAN_POINT('Ctrl Pts',(7.71635703102204,-30.2345259372057,52.9574330991265));
#84127=CARTESIAN_POINT('Ctrl Pts',(7.72021223733748,-30.1634369997333,52.950518910766));
#84128=CARTESIAN_POINT('Ctrl Pts',(7.72406744365292,-30.0921868327526,52.947319033467));
#84129=CARTESIAN_POINT('Ctrl Pts',(7.72792280057407,-30.0209338823456,52.9441190311629));
#84130=CARTESIAN_POINT('Ctrl Pts',(7.73177815749522,-29.949520175321,52.944633647595));
#84131=CARTESIAN_POINT('Ctrl Pts',(7.73563351441637,-29.8783606044694,52.9488536327324));
#84132=CARTESIAN_POINT('Ctrl Pts',(7.73949290695406,-29.8071265469369,52.953078035163));
#84133=CARTESIAN_POINT('Ctrl Pts',(7.74335229949174,-29.7361476425378,52.9610155200702));
#84134=CARTESIAN_POINT('Ctrl Pts',(7.74721169202943,-29.6658347616567,52.9726048347737));
#84135=CARTESIAN_POINT('Ctrl Pts',(7.75107326970165,-29.5954820705973,52.9842007111865));
#84136=CARTESIAN_POINT('Ctrl Pts',(7.75493484737387,-29.5257966285102,52.9994524294679));
#84137=CARTESIAN_POINT('Ctrl Pts',(7.7587964250461,-29.4571774889379,53.018247925702));
#84138=CARTESIAN_POINT('Ctrl Pts',(7.76266475922848,-29.3884382880972,53.0370763079667));
#84139=CARTESIAN_POINT('Ctrl Pts',(7.76653309341087,-29.3207695760174,53.0594606949769));
#84140=CARTESIAN_POINT('Ctrl Pts',(7.77040142759325,-29.2545530026706,53.0852398749001));
#84141=CARTESIAN_POINT('Ctrl Pts',(7.77269914613844,-29.2152215898702,53.1005522282275));
#84142=CARTESIAN_POINT('Ctrl Pts',(7.77499686468362,-29.1764021062297,53.1170613980521));
#84143=CARTESIAN_POINT('Ctrl Pts',(7.77729458322881,-29.1381703215976,53.1347259804724));
#84144=CARTESIAN_POINT('Ctrl Pts',(7.78116365643188,-29.0737927355196,53.1644709475523));
#84145=CARTESIAN_POINT('Ctrl Pts',(7.78503272963494,-29.010830773603,53.1976109569));
#84146=CARTESIAN_POINT('Ctrl Pts',(7.78890180283801,-28.9496660496235,53.233988631071));
#84147=CARTESIAN_POINT('Ctrl Pts',(7.79276511108878,-28.8885924616079,53.2703121021951));
#84148=CARTESIAN_POINT('Ctrl Pts',(7.79662841933955,-28.8293112100936,53.3098634160455));
#84149=CARTESIAN_POINT('Ctrl Pts',(7.80049172759033,-28.772181941995,53.3524380500458));
#84150=CARTESIAN_POINT('Ctrl Pts',(7.80435050393912,-28.7151196900976,53.3949627413402));
#84151=CARTESIAN_POINT('Ctrl Pts',(7.80820928028792,-28.6602047949092,53.4405034192765));
#84152=CARTESIAN_POINT('Ctrl Pts',(7.81206805663672,-28.6077688852181,53.4888116975264));
#84153=CARTESIAN_POINT('Ctrl Pts',(7.81592440208143,-28.5553660084511,53.5370895431262));
#84154=CARTESIAN_POINT('Ctrl Pts',(7.81978074752615,-28.5054393752643,53.5881312015924));
#84155=CARTESIAN_POINT('Ctrl Pts',(7.82363709297087,-28.4582872481402,53.6416482954504));
#84156=CARTESIAN_POINT('Ctrl Pts',(7.82749229907355,-28.4111490519259,53.6951495778943));
#84157=CARTESIAN_POINT('Ctrl Pts',(7.83134750517623,-28.3667840553773,53.751124479488));
#84158=CARTESIAN_POINT('Ctrl Pts',(7.83520271127891,-28.3254521679029,53.8092493457827));
#84159=CARTESIAN_POINT('Ctrl Pts',(7.83905806798854,-28.2841186657627,53.8673764827754));
#84160=CARTESIAN_POINT('Ctrl Pts',(7.84291342469817,-28.2458187876686,53.9276533540459));
#84161=CARTESIAN_POINT('Ctrl Pts',(7.8467687814078,-28.2107697851967,53.9897263732359));
#84162=CARTESIAN_POINT('Ctrl Pts',(7.85062817373729,-28.1756840949522,54.0518643677649));
#84163=CARTESIAN_POINT('Ctrl Pts',(7.85448756606678,-28.1438563125732,54.1158018394962));
#84164=CARTESIAN_POINT('Ctrl Pts',(7.85834695839627,-28.1154578183361,54.1811603771009));
#84165=CARTESIAN_POINT('Ctrl Pts',(7.86220853586187,-28.087043245253,54.2465559198318));
#84166=CARTESIAN_POINT('Ctrl Pts',(7.86607011332747,-28.0620619956734,54.3133736748834));
#84167=CARTESIAN_POINT('Ctrl Pts',(7.86993169079306,-28.0406363521104,54.3812176005826));
#84168=CARTESIAN_POINT('Ctrl Pts',(7.87380002477352,-28.0191732205828,54.4491802312659));
#84169=CARTESIAN_POINT('Ctrl Pts',(7.87766835875397,-28.0012782378103,54.5181721469249));
#84170=CARTESIAN_POINT('Ctrl Pts',(7.88153669273442,-27.9870229559283,54.5877852713206));
#84171=CARTESIAN_POINT('Ctrl Pts',(7.88383441317874,-27.978555576228,54.6291342085956));
#84172=CARTESIAN_POINT('Ctrl Pts',(7.88613213362306,-27.9713713483028,54.6707021625493));
#84173=CARTESIAN_POINT('Ctrl Pts',(7.88842985406737,-27.9654765817855,54.7124030194235));
#84174=CARTESIAN_POINT('Ctrl Pts',(7.89364480919903,-27.9520976944732,54.8070481700501));
#84175=CARTESIAN_POINT('Ctrl Pts',(7.89885976433068,-27.9453209576453,54.9026480509693));
#84176=CARTESIAN_POINT('Ctrl Pts',(7.90407471946233,-27.9452505543672,54.9984906386586));
#84177=CARTESIAN_POINT('Ctrl Pts',(7.9040747195078,-27.9452505543666,54.9984906394943));
#84178=CARTESIAN_POINT('Ctrl Pts',(7.90805348639939,-27.9451968399875,55.0716140518884));
#84179=CARTESIAN_POINT('Ctrl Pts',(7.91203225329098,-27.9490515818689,55.1448858516351));
#84180=CARTESIAN_POINT('Ctrl Pts',(7.91601102018257,-27.9568307713825,55.2178464269405));
#84181=CARTESIAN_POINT('Ctrl Pts',(7.91981486835398,-27.9642679640135,55.2875994329654));
#84182=CARTESIAN_POINT('Ctrl Pts',(7.92361871652539,-27.9752917462574,55.3570674381771));
#84183=CARTESIAN_POINT('Ctrl Pts',(7.9274225646968,-27.989862959598,55.4258481434781));
#84184=CARTESIAN_POINT('Ctrl Pts',(7.93122379837303,-28.004424157721,55.4945815738054));
#84185=CARTESIAN_POINT('Ctrl Pts',(7.93502503204926,-28.022527850686,55.5626281516843));
#84186=CARTESIAN_POINT('Ctrl Pts',(7.93882626572548,-28.0440833851904,55.6295933278012));
#84187=CARTESIAN_POINT('Ctrl Pts',(7.94262624479675,-28.0656318052465,55.6965364019246));
#84188=CARTESIAN_POINT('Ctrl Pts',(7.94642622386803,-28.0906296533896,55.7623983055293));
#84189=CARTESIAN_POINT('Ctrl Pts',(7.9502262029393,-28.1189362790883,55.8267991535855));
#84190=CARTESIAN_POINT('Ctrl Pts',(7.95402628536166,-28.147243674665,55.8912017532035));
#84191=CARTESIAN_POINT('Ctrl Pts',(7.95782636778403,-28.1788598217366,55.954142760903));
#84192=CARTESIAN_POINT('Ctrl Pts',(7.96162645020639,-28.2135965196232,56.0152635952291));
#84193=CARTESIAN_POINT('Ctrl Pts',(7.96543037542274,-28.2483683446356,56.0764462373657));
#84194=CARTESIAN_POINT('Ctrl Pts',(7.96923430063909,-28.2862667667487,56.1358045983047));
#84195=CARTESIAN_POINT('Ctrl Pts',(7.97303822585543,-28.3270589327906,56.1930070193189));
#84196=CARTESIAN_POINT('Ctrl Pts',(7.97684442148116,-28.3678754460295,56.2502435821487));
#84197=CARTESIAN_POINT('Ctrl Pts',(7.98065061710689,-28.4115888246903,56.3053212553387));
#84198=CARTESIAN_POINT('Ctrl Pts',(7.98445681273261,-28.4579262184841,56.3579418304409));
#84199=CARTESIAN_POINT('Ctrl Pts',(7.98826926304463,-28.5043397580912,56.4106488764506));
#84200=CARTESIAN_POINT('Ctrl Pts',(7.99208171335666,-28.5533855611436,56.460890416352));
#84201=CARTESIAN_POINT('Ctrl Pts',(7.99589416366868,-28.6047551136808,56.5084062018237));
#84202=CARTESIAN_POINT('Ctrl Pts',(7.99711781741443,-28.6212428158763,56.5236569891432));
#84203=CARTESIAN_POINT('Ctrl Pts',(7.99834147116018,-28.6379696641195,56.5386273004937));
#84204=CARTESIAN_POINT('Ctrl Pts',(7.99956512490593,-28.6549248140595,56.5533094690586));
#84205=CARTESIAN_POINT('Ctrl Pts',(8.00343419874366,-28.7085353450415,56.5997330545484));
#84206=CARTESIAN_POINT('Ctrl Pts',(8.00730327258139,-28.7646570840593,56.6434688627344));
#84207=CARTESIAN_POINT('Ctrl Pts',(8.01117234641911,-28.8229895049232,56.6842339080362));
#84208=CARTESIAN_POINT('Ctrl Pts',(8.01503565530687,-28.8812350100284,56.724938213105));
#84209=CARTESIAN_POINT('Ctrl Pts',(8.01889896419463,-28.941684263671,56.7626802656851));
#84210=CARTESIAN_POINT('Ctrl Pts',(8.02276227308239,-29.0040028183901,56.7972165080271));
#84211=CARTESIAN_POINT('Ctrl Pts',(8.02662105006854,-29.0662482695686,56.8317122372088));
#84212=CARTESIAN_POINT('Ctrl Pts',(8.0304798270547,-29.1303582433312,56.8630093916739));
#84213=CARTESIAN_POINT('Ctrl Pts',(8.03433860404085,-29.1959698525558,56.8909080052982));
#84214=CARTESIAN_POINT('Ctrl Pts',(8.03819495012281,-29.2615401285971,56.9187890437019));
#84215=CARTESIAN_POINT('Ctrl Pts',(8.04205129620478,-29.3286097172951,56.9432755992752));
#84216=CARTESIAN_POINT('Ctrl Pts',(8.04590764228674,-29.3967930228278,56.964214577176));
#84217=CARTESIAN_POINT('Ctrl Pts',(8.0497628490256,-29.4649561838567,56.9851473687338));
#84218=CARTESIAN_POINT('Ctrl Pts',(8.05361805576447,-29.5342319443494,57.0025345208916));
#84219=CARTESIAN_POINT('Ctrl Pts',(8.05747326250334,-29.6042183489008,57.0162724139246));
#84220=CARTESIAN_POINT('Ctrl Pts',(8.06132861984717,-29.6742074874951,57.030010843633));
#84221=CARTESIAN_POINT('Ctrl Pts',(8.06518397719101,-29.7449068481516,57.0400996397737));
#84222=CARTESIAN_POINT('Ctrl Pts',(8.06903933453485,-29.8159047591773,57.046486380313));
#84223=CARTESIAN_POINT('Ctrl Pts',(8.07289872749117,-29.8869769875828,57.0528798062013));
#84224=CARTESIAN_POINT('Ctrl Pts',(8.07675812044748,-29.9583479053718,57.0555633972186));
#84225=CARTESIAN_POINT('Ctrl Pts',(8.0806175134038,-30.029602101583,57.0545367551061));
#84226=CARTESIAN_POINT('Ctrl Pts',(8.084479091493,-30.1008966408971,57.0535095317236));
#84227=CARTESIAN_POINT('Ctrl Pts',(8.0883406695822,-30.1720738421352,57.0487679257093));
#84228=CARTESIAN_POINT('Ctrl Pts',(8.0922022476714,-30.2427224400021,57.0403635410435));
#84229=CARTESIAN_POINT('Ctrl Pts',(8.09607058226361,-30.3134946498881,57.0319444514438));
#84230=CARTESIAN_POINT('Ctrl Pts',(8.09993891685583,-30.3837359309531,57.0198498705582));
#84231=CARTESIAN_POINT('Ctrl Pts',(8.10380725144805,-30.4530449352733,57.0041825887686));
#84232=CARTESIAN_POINT('Ctrl Pts',(8.10610496621353,-30.4942131224637,56.9948765311242));
#84233=CARTESIAN_POINT('Ctrl Pts',(8.10840268097901,-30.5350526561088,56.984310943053));
#84234=CARTESIAN_POINT('Ctrl Pts',(8.11070039574449,-30.5754824614278,56.9725155256902));
#84235=CARTESIAN_POINT('Ctrl Pts',(8.11456845415834,-30.6435434979776,56.952658681812));
#84236=CARTESIAN_POINT('Ctrl Pts',(8.11843651257219,-30.7107088762612,56.9292361830766));
#84237=CARTESIAN_POINT('Ctrl Pts',(8.12230457098605,-30.7765781669856,56.9023469486561));
#84238=CARTESIAN_POINT('Ctrl Pts',(8.12616758929688,-30.8423616296342,56.8754927510674));
#84239=CARTESIAN_POINT('Ctrl Pts',(8.13003060760772,-30.9068519077994,56.8451809567541));
#84240=CARTESIAN_POINT('Ctrl Pts',(8.13389362591856,-30.9696630675606,56.8115604041569));
#84241=CARTESIAN_POINT('Ctrl Pts',(8.13775232708986,-31.0324040323294,56.777977424412));
#84242=CARTESIAN_POINT('Ctrl Pts',(8.14161102826117,-31.0934691786952,56.7410932568684));
#84243=CARTESIAN_POINT('Ctrl Pts',(8.14546972943248,-31.1524937026271,56.7011042965982));
#84244=CARTESIAN_POINT('Ctrl Pts',(8.14768450152651,-31.1863719074076,56.6781519016487));
#84245=CARTESIAN_POINT('Ctrl Pts',(8.14989927362054,-31.2195782530622,56.6541775381873));
#84246=CARTESIAN_POINT('Ctrl Pts',(8.15211404571458,-31.2520475724682,56.6292251037768));
#84247=CARTESIAN_POINT('',(7.84592528058377,-27.9452502651294,55.0010438147507));
#84248=CARTESIAN_POINT('Ctrl Pts',(7.84592528058377,-27.9452502651294,55.0010438147507));
#84249=CARTESIAN_POINT('Ctrl Pts',(7.85018308153832,-27.945290341015,55.0799332108689));
#84250=CARTESIAN_POINT('Ctrl Pts',(7.85444088249287,-27.9498778523315,55.1586663192291));
#84251=CARTESIAN_POINT('Ctrl Pts',(7.85869868344743,-27.9589342275273,55.2367447463844));
#84252=CARTESIAN_POINT('Ctrl Pts',(7.86297170270191,-27.9680229721636,55.3151022426966));
#84253=CARTESIAN_POINT('Ctrl Pts',(7.86724472195638,-27.981612447429,55.3928000839964));
#84254=CARTESIAN_POINT('Ctrl Pts',(7.87151774121087,-27.9995732784147,55.4693511415428));
#84255=CARTESIAN_POINT('Ctrl Pts',(7.87581130775173,-28.0176204760456,55.5462703033284));
#84256=CARTESIAN_POINT('Ctrl Pts',(7.88010487429258,-28.0400810290445,55.6220313489469));
#84257=CARTESIAN_POINT('Ctrl Pts',(7.88439844083344,-28.0667754154102,55.6961610934531));
#84258=CARTESIAN_POINT('Ctrl Pts',(7.8864670370682,-28.0796364964253,55.7318760425309));
#84259=CARTESIAN_POINT('Ctrl Pts',(7.88853563330296,-28.0934796387085,55.7672126691396));
#84260=CARTESIAN_POINT('Ctrl Pts',(7.89060422953772,-28.1082809506136,55.8021200662548));
#84261=CARTESIAN_POINT('Ctrl Pts',(7.89447330295539,-28.1359651170432,55.8674103727869));
#84262=CARTESIAN_POINT('Ctrl Pts',(7.89834237637307,-28.167087596891,55.9313936569422));
#84263=CARTESIAN_POINT('Ctrl Pts',(7.90221144979074,-28.2015032190154,55.9936834965361));
#84264=CARTESIAN_POINT('Ctrl Pts',(7.90607475825627,-28.2358675615715,56.0558805237416));
#84265=CARTESIAN_POINT('Ctrl Pts',(7.90993806672179,-28.2735150735108,56.1163886932215));
#84266=CARTESIAN_POINT('Ctrl Pts',(7.91380137518732,-28.3142527643123,56.1748420403915));
#84267=CARTESIAN_POINT('Ctrl Pts',(7.91766015175004,-28.354942667251,56.2332268181242));
#84268=CARTESIAN_POINT('Ctrl Pts',(7.92151892831277,-28.3987152722196,56.2895611648753));
#84269=CARTESIAN_POINT('Ctrl Pts',(7.9253777048755,-28.4453328567444,56.3435057261439));
#84270=CARTESIAN_POINT('Ctrl Pts',(7.92923405053353,-28.4919210736956,56.39741630408));
#84271=CARTESIAN_POINT('Ctrl Pts',(7.93309039619156,-28.5413503975354,56.4489397167099));
#84272=CARTESIAN_POINT('Ctrl Pts',(7.93694674184959,-28.5933420745337,56.4977686881568));
#84273=CARTESIAN_POINT('Ctrl Pts',(7.94080194816466,-28.6453183907847,56.5465832332658));
#84274=CARTESIAN_POINT('Ctrl Pts',(7.94465715447972,-28.6998552033538,56.5927045852142));
#84275=CARTESIAN_POINT('Ctrl Pts',(7.94851236079479,-28.7566372805762,56.6358626808039));
#84276=CARTESIAN_POINT('Ctrl Pts',(7.95236771771557,-28.8134215760212,56.679022462388));
#84277=CARTESIAN_POINT('Ctrl Pts',(7.95622307463635,-28.872450922176,56.7192184655813));
#84278=CARTESIAN_POINT('Ctrl Pts',(7.96007843155713,-28.9333788150103,56.7562223123031));
#84279=CARTESIAN_POINT('Ctrl Pts',(7.96393782409444,-28.9943704844591,56.7932648930095));
#84280=CARTESIAN_POINT('Ctrl Pts',(7.96779721663176,-29.0572642516549,56.8271083943555));
#84281=CARTESIAN_POINT('Ctrl Pts',(7.97165660916908,-29.1216873424442,56.8575694975094));
#84282=CARTESIAN_POINT('Ctrl Pts',(7.97551818684094,-29.1861469086943,56.8880478473175));
#84283=CARTESIAN_POINT('Ctrl Pts',(7.9793797645128,-29.25213707264,56.9151398020442));
#84284=CARTESIAN_POINT('Ctrl Pts',(7.98324134218466,-29.3192658784659,56.9387105555702));
#84285=CARTESIAN_POINT('Ctrl Pts',(7.98710967636669,-29.386512137959,56.9623225502803));
#84286=CARTESIAN_POINT('Ctrl Pts',(7.99097801054871,-29.4549005506657,56.9824009063602));
#84287=CARTESIAN_POINT('Ctrl Pts',(7.99484634473073,-29.5240255201802,56.9988611400146));
#84288=CARTESIAN_POINT('Ctrl Pts',(7.99714406327925,-29.5650844662653,57.0086382126253));
#84289=CARTESIAN_POINT('Ctrl Pts',(7.99944178182776,-29.6064030937439,57.0171397434781));
#84290=CARTESIAN_POINT('Ctrl Pts',(8.00173950037628,-29.6478955330734,57.0243566896351));
#84291=CARTESIAN_POINT('Ctrl Pts',(8.00560732707807,-29.717741147918,57.0365052171688));
#84292=CARTESIAN_POINT('Ctrl Pts',(8.00947515377985,-29.7883529993774,57.0450585066243));
#84293=CARTESIAN_POINT('Ctrl Pts',(8.01334298048164,-29.8593280936835,57.0499290176182));
#84294=CARTESIAN_POINT('Ctrl Pts',(8.01720559810006,-29.9302076006711,57.054792969141));
#84295=CARTESIAN_POINT('Ctrl Pts',(8.02106821571849,-30.0014489001652,57.0559839468319));
#84296=CARTESIAN_POINT('Ctrl Pts',(8.02493083333691,-30.0726400820925,57.0534656025786));
#84297=CARTESIAN_POINT('Ctrl Pts',(8.02878954136419,-30.1437592070777,57.0509498072954));
#84298=CARTESIAN_POINT('Ctrl Pts',(8.03264824939147,-30.2148278322896,57.0447321564718));
#84299=CARTESIAN_POINT('Ctrl Pts',(8.03650695741876,-30.2854319409786,57.0348282899471));
#84300=CARTESIAN_POINT('Ctrl Pts',(8.04036305078271,-30.355988208273,57.0249311342896));
#84301=CARTESIAN_POINT('Ctrl Pts',(8.04421914414666,-30.4260801040577,57.011352788786));
#84302=CARTESIAN_POINT('Ctrl Pts',(8.04807523751061,-30.4952983625841,56.9941607494185));
#84303=CARTESIAN_POINT('Ctrl Pts',(8.05193146499299,-30.5645190285843,56.9769681120964));
#84304=CARTESIAN_POINT('Ctrl Pts',(8.05578769247537,-30.6328655206172,56.9561616284351));
#84305=CARTESIAN_POINT('Ctrl Pts',(8.05964391995774,-30.6999396536652,56.9318597370739));
#84306=CARTESIAN_POINT('Ctrl Pts',(8.06349994384164,-30.7670102453788,56.9075591287873));
#84307=CARTESIAN_POINT('Ctrl Pts',(8.06735596772554,-30.8328081570226,56.8797636523508));
#84308=CARTESIAN_POINT('Ctrl Pts',(8.07121199160944,-30.8969533847305,56.8486406324975));
#84309=CARTESIAN_POINT('Ctrl Pts',(8.07507195420201,-30.9611641331332,56.8174858222528));
#84310=CARTESIAN_POINT('Ctrl Pts',(8.07893191679458,-31.0237183897864,56.7829968969806));
#84311=CARTESIAN_POINT('Ctrl Pts',(8.08279187938714,-31.0842598013465,56.7453877064091));
#84312=CARTESIAN_POINT('Ctrl Pts',(8.08648107319296,-31.1421227974679,56.7094423858081));
#84313=CARTESIAN_POINT('Ctrl Pts',(8.09017026699877,-31.1981469838444,56.6706473117852));
#84314=CARTESIAN_POINT('Ctrl Pts',(8.09385946080458,-31.2520475724682,56.6292251037768));
#84315=CARTESIAN_POINT('Ctrl Pts',(7.39391310379067,-31.2520475724682,56.6292251037768));
#84316=CARTESIAN_POINT('Ctrl Pts',(7.39776854030701,-31.3086015795504,56.5857637630962));
#84317=CARTESIAN_POINT('Ctrl Pts',(7.40162397682335,-31.3628830545341,56.5393596382812));
#84318=CARTESIAN_POINT('Ctrl Pts',(7.40547941333968,-31.414581229404,56.4902877265541));
#84319=CARTESIAN_POINT('Ctrl Pts',(7.40933896024307,-31.4663345211219,56.4411634979105));
#84320=CARTESIAN_POINT('Ctrl Pts',(7.41319850714646,-31.5154986629533,56.3893661408871));
#84321=CARTESIAN_POINT('Ctrl Pts',(7.41705805404985,-31.5617995710039,56.335207722608));
#84322=CARTESIAN_POINT('Ctrl Pts',(7.42091989399772,-31.6081279874757,56.2810171275823));
#84323=CARTESIAN_POINT('Ctrl Pts',(7.42478173394559,-31.6515894883817,56.2244630645941));
#84324=CARTESIAN_POINT('Ctrl Pts',(7.42864357389346,-31.691951840923,56.1658887298954));
#84325=CARTESIAN_POINT('Ctrl Pts',(7.43251206089659,-31.7323836657343,56.1072135761974));
#84326=CARTESIAN_POINT('Ctrl Pts',(7.43638054789972,-31.7697054404123,56.0465116235778));
#84327=CARTESIAN_POINT('Ctrl Pts',(7.44024903490285,-31.8037299979096,55.9841522530284));
#84328=CARTESIAN_POINT('Ctrl Pts',(7.44218707199639,-31.8207756424906,55.9529114156785));
#84329=CARTESIAN_POINT('Ctrl Pts',(7.44412510908994,-31.8369944921675,55.9212549384705));
#84330=CARTESIAN_POINT('Ctrl Pts',(7.44606314618348,-31.8523676042235,55.8892310280929));
#84331=CARTESIAN_POINT('Ctrl Pts',(7.44993221953076,-31.8830582955001,55.8252988884398));
#84332=CARTESIAN_POINT('Ctrl Pts',(7.45380129287804,-31.9104954100641,55.7596507813513));
#84333=CARTESIAN_POINT('Ctrl Pts',(7.45767036622532,-31.9344849573745,55.6926510753559));
#84334=CARTESIAN_POINT('Ctrl Pts',(7.46153367462015,-31.9584387600538,55.6257511994968));
#84335=CARTESIAN_POINT('Ctrl Pts',(7.46539698301498,-31.9789550296681,55.5575041758803));
#84336=CARTESIAN_POINT('Ctrl Pts',(7.4692602914098,-31.9958867364297,55.488296731347));
#84337=CARTESIAN_POINT('Ctrl Pts',(7.47311906790172,-32.0127985812379,55.419170471484));
#84338=CARTESIAN_POINT('Ctrl Pts',(7.47697784439365,-32.0261341006974,55.3490864981594));
#84339=CARTESIAN_POINT('Ctrl Pts',(7.48083662088557,-32.0357958014218,55.2784475128517));
#84340=CARTESIAN_POINT('Ctrl Pts',(7.48469296647276,-32.0454514155864,55.2078530278264));
#84341=CARTESIAN_POINT('Ctrl Pts',(7.48854931205996,-32.0514377370475,55.1367047046642));
#84342=CARTESIAN_POINT('Ctrl Pts',(7.49240565764715,-32.053708465876,55.0654148277488));
#84343=CARTESIAN_POINT('Ctrl Pts',(7.49626086389146,-32.055978523826,54.994146013161));
#84344=CARTESIAN_POINT('Ctrl Pts',(7.50011607013577,-32.0545351530398,54.9227362131225));
#84345=CARTESIAN_POINT('Ctrl Pts',(7.50397127638008,-32.0493840895025,54.8516004845229));
#84346=CARTESIAN_POINT('Ctrl Pts',(7.50782663323027,-32.044232824736,54.7804619769644));
#84347=CARTESIAN_POINT('Ctrl Pts',(7.51168199008047,-32.0353736169328,54.7095980464599));
#84348=CARTESIAN_POINT('Ctrl Pts',(7.51553734693067,-32.0228641528445,54.6394196599415));
#84349=CARTESIAN_POINT('Ctrl Pts',(7.51939673939817,-32.0103415944016,54.5691678137871));
#84350=CARTESIAN_POINT('Ctrl Pts',(7.52325613186567,-31.9941612376679,54.4996034233314));
#84351=CARTESIAN_POINT('Ctrl Pts',(7.52711552433317,-31.9744319452988,54.4311273816719));
#84352=CARTESIAN_POINT('Ctrl Pts',(7.53097710193553,-31.9546914824762,54.3626125698208));
#84353=CARTESIAN_POINT('Ctrl Pts',(7.53483867953788,-31.9313982427059,54.2951877928218));
#84354=CARTESIAN_POINT('Ctrl Pts',(7.53870025714024,-31.9047101701479,54.2292362682149));
#84355=CARTESIAN_POINT('Ctrl Pts',(7.54256859125404,-31.8779754020975,54.1631693497778));
#84356=CARTESIAN_POINT('Ctrl Pts',(7.54643692536784,-31.8478341476564,54.0985812705662));
#84357=CARTESIAN_POINT('Ctrl Pts',(7.55030525948163,-31.8144911274965,54.0358322185758));
#84358=CARTESIAN_POINT('Ctrl Pts',(7.55260297866177,-31.7946859879477,53.9985604379972));
#84359=CARTESIAN_POINT('Ctrl Pts',(7.5549006978419,-31.7737520802405,53.9619369825755));
#84360=CARTESIAN_POINT('Ctrl Pts',(7.55719841702204,-31.7517393817971,53.9260322627001));
#84361=CARTESIAN_POINT('Ctrl Pts',(7.56106749037986,-31.7146727350905,53.8655731794967));
#84362=CARTESIAN_POINT('Ctrl Pts',(7.56493656373769,-31.6743998062233,53.8069168887164));
#84363=CARTESIAN_POINT('Ctrl Pts',(7.56880563709551,-31.6311215035676,53.7504239906675));
#84364=CARTESIAN_POINT('Ctrl Pts',(7.57266894550093,-31.5879076859531,53.6940152675199));
#84365=CARTESIAN_POINT('Ctrl Pts',(7.57653225390636,-31.5416976763381,53.6397639210884));
#84366=CARTESIAN_POINT('Ctrl Pts',(7.58039556231178,-31.4927366371123,53.588003224252));
#84367=CARTESIAN_POINT('Ctrl Pts',(7.58425433881433,-31.4438330322539,53.5363032459569));
#84368=CARTESIAN_POINT('Ctrl Pts',(7.58811311531688,-31.3921851401621,53.4870884649974));
#84369=CARTESIAN_POINT('Ctrl Pts',(7.59197189181942,-31.3380784109807,53.440659200634));
#84370=CARTESIAN_POINT('Ctrl Pts',(7.59582823741726,-31.2840057672932,53.3942591852094));
#84371=CARTESIAN_POINT('Ctrl Pts',(7.59968458301509,-31.2274777274727,53.3506415205165));
#84372=CARTESIAN_POINT('Ctrl Pts',(7.60354092861292,-31.1688155581712,53.310068713386));
#84373=CARTESIAN_POINT('Ctrl Pts',(7.60739613486786,-31.1101707203885,53.2695078933397));
#84374=CARTESIAN_POINT('Ctrl Pts',(7.6112513411228,-31.0493934042002,53.231990421099));
#84375=CARTESIAN_POINT('Ctrl Pts',(7.61510654737773,-30.9868354279729,53.1977365895637));
#84376=CARTESIAN_POINT('Ctrl Pts',(7.61896190423855,-30.9242750078818,53.1634814198825));
#84377=CARTESIAN_POINT('Ctrl Pts',(7.62281726109936,-30.8599342167953,53.1324903754099));
#84378=CARTESIAN_POINT('Ctrl Pts',(7.62667261796017,-30.7941896131577,53.1049378846981));
#84379=CARTESIAN_POINT('Ctrl Pts',(7.63053201043819,-30.7283761909742,53.0773565532565));
#84380=CARTESIAN_POINT('Ctrl Pts',(7.6343914029162,-30.6611564718399,53.0532211487873));
#84381=CARTESIAN_POINT('Ctrl Pts',(7.63825079539421,-30.5929263067048,53.0326576410504));
#84382=CARTESIAN_POINT('Ctrl Pts',(7.64211237300705,-30.5246575105906,53.0120824905388));
#84383=CARTESIAN_POINT('Ctrl Pts',(7.6459739506199,-30.4553776016146,52.9950833784695));
#84384=CARTESIAN_POINT('Ctrl Pts',(7.64983552823274,-30.3854942007663,52.9817354525049));
#84385=CARTESIAN_POINT('Ctrl Pts',(7.65370386235683,-30.3154885265802,52.9683641719892));
#84386=CARTESIAN_POINT('Ctrl Pts',(7.65757219648092,-30.2448777337682,52.9586568983752));
#84387=CARTESIAN_POINT('Ctrl Pts',(7.661440530605,-30.1740754650965,52.9526369899426));
#84388=CARTESIAN_POINT('Ctrl Pts',(7.6637382496902,-30.132020224059,52.9490612754223));
#84389=CARTESIAN_POINT('Ctrl Pts',(7.6660359687754,-30.0898974659227,52.9467855163727));
#84390=CARTESIAN_POINT('Ctrl Pts',(7.6683336878606,-30.0477934514707,52.9458059126517));
#84391=CARTESIAN_POINT('Ctrl Pts',(7.67220276119183,-29.9768955246948,52.9441563817512));
#84392=CARTESIAN_POINT('Ctrl Pts',(7.67607183452307,-29.9057732300604,52.9461783579695));
#84393=CARTESIAN_POINT('Ctrl Pts',(7.6799409078543,-29.8348384890744,52.9518986260908));
#84394=CARTESIAN_POINT('Ctrl Pts',(7.68380421623315,-29.7640094414595,52.9576103709636));
#84395=CARTESIAN_POINT('Ctrl Pts',(7.687667524612,-29.6933678730486,52.9670094308489));
#84396=CARTESIAN_POINT('Ctrl Pts',(7.69153083299085,-29.6233267481749,52.980070589387));
#84397=CARTESIAN_POINT('Ctrl Pts',(7.69538960946695,-29.5533677859286,52.9931164263678));
#84398=CARTESIAN_POINT('Ctrl Pts',(7.69924838594304,-29.4840083433624,53.009815740327));
#84399=CARTESIAN_POINT('Ctrl Pts',(7.70310716241913,-29.4156555496703,53.0300915945484));
#84400=CARTESIAN_POINT('Ctrl Pts',(7.70696350799061,-29.3473458160319,53.0503546756361));
#84401=CARTESIAN_POINT('Ctrl Pts',(7.71081985356208,-29.2800419377385,53.0741896890378));
#84402=CARTESIAN_POINT('Ctrl Pts',(7.71467619913355,-29.2141387017029,53.1014690989245));
#84403=CARTESIAN_POINT('Ctrl Pts',(7.71853140536226,-29.1482549365299,53.1287404492123));
#84404=CARTESIAN_POINT('Ctrl Pts',(7.72238661159097,-29.0837714406864,53.1594539900072));
#84405=CARTESIAN_POINT('Ctrl Pts',(7.72624181781968,-29.0210641054759,53.1934336223343));
#84406=CARTESIAN_POINT('Ctrl Pts',(7.73009717465446,-28.9583543205637,53.2274145820972));
#84407=CARTESIAN_POINT('Ctrl Pts',(7.73395253148923,-28.8974212601037,53.2646616533317));
#84408=CARTESIAN_POINT('Ctrl Pts',(7.737807888324,-28.8386157008929,53.3049530766709));
#84409=CARTESIAN_POINT('Ctrl Pts',(7.74166728077639,-28.7797485866145,53.3452866752962));
#84410=CARTESIAN_POINT('Ctrl Pts',(7.74552667322878,-28.7230138206927,53.3886707122444));
#84411=CARTESIAN_POINT('Ctrl Pts',(7.74938606568117,-28.6687319311445,53.4348409373658));
#84412=CARTESIAN_POINT('Ctrl Pts',(7.75324764326858,-28.6144193079356,53.4810373034349));
#84413=CARTESIAN_POINT('Ctrl Pts',(7.757109220856,-28.56256267905,53.5300226642511));
#84414=CARTESIAN_POINT('Ctrl Pts',(7.76097079844341,-28.5134462582933,53.5814953170617));
#84415=CARTESIAN_POINT('Ctrl Pts',(7.76483913254268,-28.4642438996857,53.6330580303673));
#84416=CARTESIAN_POINT('Ctrl Pts',(7.76870746664195,-28.4177916382251,53.6871163559143));
#84417=CARTESIAN_POINT('Ctrl Pts',(7.77257580074122,-28.374333443196,53.7433354430919));
#84418=CARTESIAN_POINT('Ctrl Pts',(7.77487352006053,-28.3485200745111,53.7767285470501));
#84419=CARTESIAN_POINT('Ctrl Pts',(7.77717123937985,-28.323762236405,53.8108834243806));
#84420=CARTESIAN_POINT('Ctrl Pts',(7.77946895869916,-28.3001035209765,53.8457255425578));
#84421=CARTESIAN_POINT('Ctrl Pts',(7.78339694508641,-28.2596585843988,53.905288677512));
#84422=CARTESIAN_POINT('Ctrl Pts',(7.78732493147366,-28.2222729068542,53.9670902448233));
#84423=CARTESIAN_POINT('Ctrl Pts',(7.79125291786091,-28.1881978041484,54.0307887920545));
#84424=CARTESIAN_POINT('Ctrl Pts',(7.79517455595449,-28.1541777726005,54.094384391606));
#84425=CARTESIAN_POINT('Ctrl Pts',(7.79909619404806,-28.1234579082038,54.1598704747613));
#84426=CARTESIAN_POINT('Ctrl Pts',(7.80301783214163,-28.0962464206018,54.2268765483904));
#84427=CARTESIAN_POINT('Ctrl Pts',(7.80693336842876,-28.0690772722537,54.2937783650529));
#84428=CARTESIAN_POINT('Ctrl Pts',(7.81084890471589,-28.0454058198635,54.3621950395434));
#84429=CARTESIAN_POINT('Ctrl Pts',(7.81476444100302,-28.0253936651134,54.4317329987358));
#84430=CARTESIAN_POINT('Ctrl Pts',(7.81867638568786,-28.0053998669039,54.5012071728743));
#84431=CARTESIAN_POINT('Ctrl Pts',(7.82258833037271,-27.9890588284757,54.5718001425285));
#84432=CARTESIAN_POINT('Ctrl Pts',(7.82650027505756,-27.9764831073348,54.6431009279941));
#84433=CARTESIAN_POINT('Ctrl Pts',(7.83040988908206,-27.9639148785634,54.7143592338423));
#84434=CARTESIAN_POINT('Ctrl Pts',(7.83431950310656,-27.9551075922549,54.7863240593652));
#84435=CARTESIAN_POINT('Ctrl Pts',(7.83822911713106,-27.9501229158777,54.8585733317576));
#84436=CARTESIAN_POINT('Ctrl Pts',(7.84079450493327,-27.9468520999107,54.9059814392977));
#84437=CARTESIAN_POINT('Ctrl Pts',(7.84335989273547,-27.9452261188372,54.9535117905147));
#84438=CARTESIAN_POINT('Ctrl Pts',(7.84592528053768,-27.945250265129,55.0010438138967));
#84439=CARTESIAN_POINT('Origin',(-1.54592528053767,-30.,55.));
#84440=CARTESIAN_POINT('',(6.69398930341886,-31.2520475724682,56.6292251037768));
#84441=CARTESIAN_POINT('',(6.75200712063213,-31.2520475724682,56.6292251037768));
#84442=CARTESIAN_POINT('',(-1.54592528053767,-31.2520475724682,56.6292251037768));
#84443=CARTESIAN_POINT('',(7.20407471942299,-27.945250640964,55.0016229729599));
#84444=CARTESIAN_POINT('Ctrl Pts',(6.75200712063213,-31.2520475724682,56.6292251037768));
#84445=CARTESIAN_POINT('Ctrl Pts',(6.75587000360825,-31.3085547924693,56.5857997186257));
#84446=CARTESIAN_POINT('Ctrl Pts',(6.75973288658436,-31.3627396230512,56.5394776578832));
#84447=CARTESIAN_POINT('Ctrl Pts',(6.76359576956048,-31.4143063307506,56.490548612189));
#84448=CARTESIAN_POINT('Ctrl Pts',(6.76746491972785,-31.4659567009429,56.4415401833789));
#84449=CARTESIAN_POINT('Ctrl Pts',(6.77133406989522,-31.5149801444479,56.3899166863317));
#84450=CARTESIAN_POINT('Ctrl Pts',(6.77520322006258,-31.5611200623353,56.3360021382745));
#84451=CARTESIAN_POINT('Ctrl Pts',(6.77582786193565,-31.5685689654498,56.3272980862665));
#84452=CARTESIAN_POINT('Ctrl Pts',(6.77645250380871,-31.575942805177,56.318534383896));
#84453=CARTESIAN_POINT('Ctrl Pts',(6.77707714568177,-31.5832406084852,56.3097124639185));
#84454=CARTESIAN_POINT('Ctrl Pts',(6.78094621902978,-31.6284436880358,56.2550689042481));
#84455=CARTESIAN_POINT('Ctrl Pts',(6.78481529237778,-31.6709030568371,56.1979753737613));
#84456=CARTESIAN_POINT('Ctrl Pts',(6.78868436572578,-31.7103425768957,56.1387387023185));
#84457=CARTESIAN_POINT('Ctrl Pts',(6.79254767412136,-31.7497233317315,56.0795902940235));
#84458=CARTESIAN_POINT('Ctrl Pts',(6.79641098251693,-31.7860929023769,56.0183054844465));
#84459=CARTESIAN_POINT('Ctrl Pts',(6.80027429091251,-31.8192153334279,55.9552241271664));
#84460=CARTESIAN_POINT('Ctrl Pts',(6.80413306740521,-31.8522989097914,55.8922167682719));
#84461=CARTESIAN_POINT('Ctrl Pts',(6.80799184389792,-31.8821426879791,55.8274174758218));
#84462=CARTESIAN_POINT('Ctrl Pts',(6.81185062039062,-31.9085549343264,55.7611935530194));
#84463=CARTESIAN_POINT('Ctrl Pts',(6.81570696597862,-31.9349505418106,55.6950113491521));
#84464=CARTESIAN_POINT('Ctrl Pts',(6.81956331156662,-31.9579187268033,55.6274067456564));
#84465=CARTESIAN_POINT('Ctrl Pts',(6.82341965715462,-31.9773151269939,55.5587686919119));
#84466=CARTESIAN_POINT('Ctrl Pts',(6.82727486339975,-31.9967057965908,55.4901509170234));
#84467=CARTESIAN_POINT('Ctrl Pts',(6.83113006964488,-32.0125266443568,55.4205007652728));
#84468=CARTESIAN_POINT('Ctrl Pts',(6.83498527589,-32.0246831393636,55.3502224260052));
#84469=CARTESIAN_POINT('Ctrl Pts',(6.83884063274105,-32.036840109271,55.2799413412726));
#84470=CARTESIAN_POINT('Ctrl Pts',(6.84269598959209,-32.0453323615838,55.2090324993541));
#84471=CARTESIAN_POINT('Ctrl Pts',(6.84655134644314,-32.0501167691132,55.1379086491154));
#84472=CARTESIAN_POINT('Ctrl Pts',(6.8504107389115,-32.0549061847492,55.0667103495708));
#84473=CARTESIAN_POINT('Ctrl Pts',(6.85427013137986,-32.0559799751667,54.995297078117));
#84474=CARTESIAN_POINT('Ctrl Pts',(6.85812952384822,-32.0533471080334,54.9240841490139));
#84475=CARTESIAN_POINT('Ctrl Pts',(6.86199110145146,-32.0507127502069,54.8528309001309));
#84476=CARTESIAN_POINT('Ctrl Pts',(6.8658526790547,-32.0443676002785,54.7817787034946));
#84477=CARTESIAN_POINT('Ctrl Pts',(6.86971425665794,-32.0343725214679,54.7113375563115));
#84478=CARTESIAN_POINT('Ctrl Pts',(6.87358259077263,-32.0243599545033,54.6407731599113));
#84479=CARTESIAN_POINT('Ctrl Pts',(6.87745092488731,-32.0106848016684,54.5708224244431));
#84480=CARTESIAN_POINT('Ctrl Pts',(6.88131925900199,-31.993458875977,54.501884278216));
#84481=CARTESIAN_POINT('Ctrl Pts',(6.88361697817477,-31.983226993581,54.4609362898505));
#84482=CARTESIAN_POINT('Ctrl Pts',(6.88591469734756,-31.9717433059069,54.4203452700944));
#84483=CARTESIAN_POINT('Ctrl Pts',(6.88821241652034,-31.9590393346448,54.3801916039498));
#84484=CARTESIAN_POINT('Ctrl Pts',(6.89208148986834,-31.9376474268756,54.3125778235781));
#84485=CARTESIAN_POINT('Ctrl Pts',(6.89595056321633,-31.9127091017352,54.2459403779375));
#84486=CARTESIAN_POINT('Ctrl Pts',(6.89981963656433,-31.8843323730244,54.1806776760809));
#84487=CARTESIAN_POINT('Ctrl Pts',(6.90368294495989,-31.8559979258825,54.1155122162092));
#84488=CARTESIAN_POINT('Ctrl Pts',(6.90754625335546,-31.8242354368057,54.051717876011));
#84489=CARTESIAN_POINT('Ctrl Pts',(6.91140956175102,-31.7892024578523,53.9896772162743));
#84490=CARTESIAN_POINT('Ctrl Pts',(6.9152683382437,-31.7542105747789,53.9277093341199));
#84491=CARTESIAN_POINT('Ctrl Pts',(6.91912711473639,-31.715956060097,53.8674914671294));
#84492=CARTESIAN_POINT('Ctrl Pts',(6.92298589122908,-31.6746435117732,53.8093839111721));
#84493=CARTESIAN_POINT('Ctrl Pts',(6.92684223681705,-31.6333569890222,53.7513129611006));
#84494=CARTESIAN_POINT('Ctrl Pts',(6.93069858240503,-31.5890165355209,53.6953500794837));
#84495=CARTESIAN_POINT('Ctrl Pts',(6.93455492799301,-31.5418706276525,53.6418275035614));
#84496=CARTESIAN_POINT('Ctrl Pts',(6.93841013423812,-31.4947386488662,53.5883207406838));
#84497=CARTESIAN_POINT('Ctrl Pts',(6.94226534048322,-31.4448031821568,53.5372532164894));
#84498=CARTESIAN_POINT('Ctrl Pts',(6.94612054672832,-31.3923525344185,53.4889235683135));
#84499=CARTESIAN_POINT('Ctrl Pts',(6.94997590357934,-31.3398998376646,53.4405920321113));
#84500=CARTESIAN_POINT('Ctrl Pts',(6.95383126043035,-31.2849321235481,53.3949989118376));
#84501=CARTESIAN_POINT('Ctrl Pts',(6.95768661728136,-31.2277727697314,53.3524043006835));
#84502=CARTESIAN_POINT('Ctrl Pts',(6.96154600974969,-31.1705535840271,53.3097651033713));
#84503=CARTESIAN_POINT('Ctrl Pts',(6.96540540221802,-31.1111385693846,53.270130971609));
#84504=CARTESIAN_POINT('Ctrl Pts',(6.96926479468635,-31.049881513145,53.2337196228072));
#84505=CARTESIAN_POINT('Ctrl Pts',(6.97312637228955,-30.9885897740035,53.1972876584011));
#84506=CARTESIAN_POINT('Ctrl Pts',(6.97698794989275,-30.9254543472475,53.1640823355941));
#84507=CARTESIAN_POINT('Ctrl Pts',(6.98084952749596,-30.8608526994133,53.1342748883041));
#84508=CARTESIAN_POINT('Ctrl Pts',(6.9847178616106,-30.7961380195966,53.1044152876251));
#84509=CARTESIAN_POINT('Ctrl Pts',(6.98858619572524,-30.7299524480231,53.0779656125225));
#84510=CARTESIAN_POINT('Ctrl Pts',(6.99245452983988,-30.662691785105,53.0550482884004));
#84511=CARTESIAN_POINT('Ctrl Pts',(6.99475224901289,-30.6227401909056,53.0414358202245));
#84512=CARTESIAN_POINT('Ctrl Pts',(6.99704996818589,-30.5824095673591,53.029068655143));
#84513=CARTESIAN_POINT('Ctrl Pts',(6.9993476873589,-30.5417845456398,53.0179639083493));
#84514=CARTESIAN_POINT('Ctrl Pts',(7.00321676070842,-30.4733770610767,52.9992648957034));
#84515=CARTESIAN_POINT('Ctrl Pts',(7.00708583405794,-30.4038663884346,52.984074911664));
#84516=CARTESIAN_POINT('Ctrl Pts',(7.01095490740745,-30.3336458313196,52.9725192918937));
#84517=CARTESIAN_POINT('Ctrl Pts',(7.01481821580455,-30.2635299034361,52.9609808900959));
#84518=CARTESIAN_POINT('Ctrl Pts',(7.01868152420164,-30.1927066660855,52.9530661817184));
#84519=CARTESIAN_POINT('Ctrl Pts',(7.02254483259873,-30.121582975828,52.9488502876463));
#84520=CARTESIAN_POINT('Ctrl Pts',(7.02640360909295,-30.0505427181167,52.9446393390821));
#84521=CARTESIAN_POINT('Ctrl Pts',(7.03026238558716,-29.9792031901646,52.9441186148241));
#84522=CARTESIAN_POINT('Ctrl Pts',(7.03412116208138,-29.9079780588148,52.9473116347481));
#84523=CARTESIAN_POINT('Ctrl Pts',(7.03797750767089,-29.8367977970001,52.9505026431725));
#84524=CARTESIAN_POINT('Ctrl Pts',(7.0418338532604,-29.7657322729608,52.9574027324669));
#84525=CARTESIAN_POINT('Ctrl Pts',(7.04569019884991,-29.6951953783404,52.9679833403451));
#84526=CARTESIAN_POINT('Ctrl Pts',(7.04954540509654,-29.6246793235816,52.9785608222223));
#84527=CARTESIAN_POINT('Ctrl Pts',(7.05340061134318,-29.5546920683275,52.9928165918795));
#84528=CARTESIAN_POINT('Ctrl Pts',(7.05725581758981,-29.4856408781172,53.0106704003017));
#84529=CARTESIAN_POINT('Ctrl Pts',(7.06111117444235,-29.4165869903813,53.0285249061934));
#84530=CARTESIAN_POINT('Ctrl Pts',(7.06496653129489,-29.3484697100577,53.0499776061749));
#84531=CARTESIAN_POINT('Ctrl Pts',(7.06882188814743,-29.2816829411958,53.0748978817915));
#84532=CARTESIAN_POINT('Ctrl Pts',(7.07268128061727,-29.2148262628937,53.0998442428521));
#84533=CARTESIAN_POINT('Ctrl Pts',(7.07654067308711,-29.1493033323038,53.1282652550815));
#84534=CARTESIAN_POINT('Ctrl Pts',(7.08040006555694,-29.0854889448541,53.1599817684284));
#84535=CARTESIAN_POINT('Ctrl Pts',(7.08426164316165,-29.0216384265771,53.1917162392283));
#84536=CARTESIAN_POINT('Ctrl Pts',(7.08812322076635,-28.9594988005098,53.2267496868236));
#84537=CARTESIAN_POINT('Ctrl Pts',(7.09198479837105,-28.8994186520185,53.2648578562621));
#84538=CARTESIAN_POINT('Ctrl Pts',(7.09585313248717,-28.839233382706,53.3030327026674));
#84539=CARTESIAN_POINT('Ctrl Pts',(7.09972146660328,-28.7811151815409,53.3442927304759));
#84540=CARTESIAN_POINT('Ctrl Pts',(7.1035898007194,-28.7253815713666,53.3883718096632));
#84541=CARTESIAN_POINT('Ctrl Pts',(7.10588751987875,-28.6922768342696,53.4145539701838));
#84542=CARTESIAN_POINT('Ctrl Pts',(7.10818523903811,-28.6600127586308,53.4417299774308));
#84543=CARTESIAN_POINT('Ctrl Pts',(7.11048295819746,-28.6286496245778,53.4698380117356));
#84544=CARTESIAN_POINT('Ctrl Pts',(7.11438261491519,-28.5754205535222,53.5175425731711));
#84545=CARTESIAN_POINT('Ctrl Pts',(7.11828227163292,-28.524561791378,53.5681375184189));
#84546=CARTESIAN_POINT('Ctrl Pts',(7.12218192835065,-28.476409230357,53.6213525725703));
#84547=CARTESIAN_POINT('Ctrl Pts',(7.12598698948115,-28.4294247259409,53.6732767671252));
#84548=CARTESIAN_POINT('Ctrl Pts',(7.12979205061164,-28.3850169998589,53.7276950180236));
#84549=CARTESIAN_POINT('Ctrl Pts',(7.13359711174214,-28.3434646904989,53.7843156944025));
#84550=CARTESIAN_POINT('Ctrl Pts',(7.13739855500299,-28.3019518892661,53.8408825355815));
#84551=CARTESIAN_POINT('Ctrl Pts',(7.14119999826383,-28.2632894190354,53.8996472498018));
#84552=CARTESIAN_POINT('Ctrl Pts',(7.14500144152468,-28.2277166035742,53.9602841132053));
#84553=CARTESIAN_POINT('Ctrl Pts',(7.14880063065914,-28.1921648815811,54.0208850210138));
#84554=CARTESIAN_POINT('Ctrl Pts',(7.15259981979359,-28.1596994343324,54.0833554448165));
#84555=CARTESIAN_POINT('Ctrl Pts',(7.15639900892805,-28.1305159753065,54.1473411913809));
#84556=CARTESIAN_POINT('Ctrl Pts',(7.16037198480262,-28.0999975739994,54.2142538452186));
#84557=CARTESIAN_POINT('Ctrl Pts',(7.1643449606772,-28.0730689420862,54.2828232869358));
#84558=CARTESIAN_POINT('Ctrl Pts',(7.16831793655178,-28.0498988920081,54.3526181720895));
#84559=CARTESIAN_POINT('Ctrl Pts',(7.1721185069018,-28.0277342959684,54.4193843391825));
#84560=CARTESIAN_POINT('Ctrl Pts',(7.17591907725183,-28.009008924759,54.4872712685952));
#84561=CARTESIAN_POINT('Ctrl Pts',(7.17971964760185,-27.9938195467796,54.5558856547957));
#84562=CARTESIAN_POINT('Ctrl Pts',(7.18352169694533,-27.9786242578476,54.6245267423119));
#84563=CARTESIAN_POINT('Ctrl Pts',(7.18732374628881,-27.9669677847835,54.6938953556263));
#84564=CARTESIAN_POINT('Ctrl Pts',(7.1911257956323,-27.9588954503991,54.7635898054259));
#84565=CARTESIAN_POINT('Ctrl Pts',(7.19493249872832,-27.9508132353837,54.8333695620411));
#84566=CARTESIAN_POINT('Ctrl Pts',(7.19873920182434,-27.9463239372981,54.9034754508827));
#84567=CARTESIAN_POINT('Ctrl Pts',(7.20254590492036,-27.9454208415896,54.9735038809335));
#84568=CARTESIAN_POINT('Ctrl Pts',(7.20305550975457,-27.9452999438134,54.9828786142883));
#84569=CARTESIAN_POINT('Ctrl Pts',(7.20356511458877,-27.9452432391406,54.9922519653909));
#84570=CARTESIAN_POINT('Ctrl Pts',(7.20407471942298,-27.945250640964,55.0016229729598));
#84571=CARTESIAN_POINT('Ctrl Pts',(7.20407471946233,-27.9452506409646,55.0016229736833));
#84572=CARTESIAN_POINT('Ctrl Pts',(7.20992255598689,-27.9453355786842,55.109157511533));
#84573=CARTESIAN_POINT('Ctrl Pts',(7.21577039251146,-27.953864093232,55.2163661668599));
#84574=CARTESIAN_POINT('Ctrl Pts',(7.22161822903602,-27.9706730699848,55.3222262770401));
#84575=CARTESIAN_POINT('Ctrl Pts',(7.22548730238329,-27.9817943049366,55.3922659454058));
#84576=CARTESIAN_POINT('Ctrl Pts',(7.22935637573056,-27.9965675768626,55.4618663739711));
#84577=CARTESIAN_POINT('Ctrl Pts',(7.23322544907783,-28.0149451914136,55.5306175359032));
#84578=CARTESIAN_POINT('Ctrl Pts',(7.23708875747265,-28.0332954231614,55.5992662580147));
#84579=CARTESIAN_POINT('Ctrl Pts',(7.24095206586747,-28.0552392128128,55.6670677598203));
#84580=CARTESIAN_POINT('Ctrl Pts',(7.24481537426229,-28.0806775244038,55.7336203358492));
#84581=CARTESIAN_POINT('Ctrl Pts',(7.2486741507542,-28.1060859952609,55.8000948415347));
#84582=CARTESIAN_POINT('Ctrl Pts',(7.25253292724611,-28.1349806728731,55.8653228799988));
#84583=CARTESIAN_POINT('Ctrl Pts',(7.25639170373802,-28.1672126921902,55.9289177826004));
#84584=CARTESIAN_POINT('Ctrl Pts',(7.26024804932521,-28.1994244063747,55.9924726224646));
#84585=CARTESIAN_POINT('Ctrl Pts',(7.2641043949124,-28.2349690720051,56.0543959353494));
#84586=CARTESIAN_POINT('Ctrl Pts',(7.26796074049958,-28.273650267584,56.1143222890561));
#84587=CARTESIAN_POINT('Ctrl Pts',(7.27181594674388,-28.3123200349483,56.1742309377457));
#84588=CARTESIAN_POINT('Ctrl Pts',(7.27567115298818,-28.3541242292472,56.2321433906359));
#84589=CARTESIAN_POINT('Ctrl Pts',(7.27952635923247,-28.3988220533025,56.2877215325953));
#84590=CARTESIAN_POINT('Ctrl Pts',(7.28338171608267,-28.4435216235047,56.3433018457475));
#84591=CARTESIAN_POINT('Ctrl Pts',(7.28723707293288,-28.4911147417313,56.396547289749));
#84592=CARTESIAN_POINT('Ctrl Pts',(7.29109242978307,-28.5413202084445,56.4471526623711));
#84593=CARTESIAN_POINT('Ctrl Pts',(7.29495182225056,-28.5915782280232,56.4978110064623));
#84594=CARTESIAN_POINT('Ctrl Pts',(7.29881121471805,-28.6444537119087,56.5458234170178));
#84595=CARTESIAN_POINT('Ctrl Pts',(7.30267060718554,-28.6996290990732,56.5909220856229));
#84596=CARTESIAN_POINT('Ctrl Pts',(7.3065321847879,-28.754835725782,56.6360462884731));
#84597=CARTESIAN_POINT('Ctrl Pts',(7.31039376239025,-28.8123444561797,56.6782531777261));
#84598=CARTESIAN_POINT('Ctrl Pts',(7.31425533999261,-28.871807414128,56.717317399808));
#84599=CARTESIAN_POINT('Ctrl Pts',(7.31812367410639,-28.931374413014,56.7564499716398));
#84600=CARTESIAN_POINT('Ctrl Pts',(7.32199200822018,-28.9929020466295,56.7924286527882));
#84601=CARTESIAN_POINT('Ctrl Pts',(7.32586034233397,-29.0560170648301,56.8250736370371));
#84602=CARTESIAN_POINT('Ctrl Pts',(7.32815806151417,-29.0935062225947,56.8444641561184));
#84603=CARTESIAN_POINT('Ctrl Pts',(7.33045578069437,-29.1315550145839,56.8626794081666));
#84604=CARTESIAN_POINT('Ctrl Pts',(7.33275349987457,-29.1700822865709,56.8796899083191));
#84605=CARTESIAN_POINT('Ctrl Pts',(7.33662257323245,-29.2349574213919,56.9083334751706));
#84606=CARTESIAN_POINT('Ctrl Pts',(7.34049164659033,-29.3014442654214,56.9336705787694));
#84607=CARTESIAN_POINT('Ctrl Pts',(7.34436071994821,-29.3691724695526,56.9555189053879));
#84608=CARTESIAN_POINT('Ctrl Pts',(7.34822402835369,-29.4367997580803,56.9773346778129));
#84609=CARTESIAN_POINT('Ctrl Pts',(7.35208733675917,-29.5056642766728,56.9956718438265));
#84610=CARTESIAN_POINT('Ctrl Pts',(7.35595064516465,-29.5753748215141,57.0103957372358));
#84611=CARTESIAN_POINT('Ctrl Pts',(7.35980942166726,-29.6450035915175,57.0251023585954));
#84612=CARTESIAN_POINT('Ctrl Pts',(7.36366819816986,-29.7154759434518,57.0362040267315));
#84613=CARTESIAN_POINT('Ctrl Pts',(7.36752697467247,-29.7863862810899,57.0436160944741));
#84614=CARTESIAN_POINT('Ctrl Pts',(7.37138332027036,-29.8572519475029,57.0510234928531));
#84615=CARTESIAN_POINT('Ctrl Pts',(7.37523966586826,-29.9285545701936,57.0547458518867));
#84616=CARTESIAN_POINT('Ctrl Pts',(7.37909601146615,-29.9998806016868,57.054749996531));
#84617=CARTESIAN_POINT('Ctrl Pts',(7.38295121772115,-30.0711855601706,57.0547541399507));
#84618=CARTESIAN_POINT('Ctrl Pts',(7.38680642397615,-30.1425134282052,57.0510422498442));
#84619=CARTESIAN_POINT('Ctrl Pts',(7.39066163023115,-30.2134495407978,57.0436332489058));
#84620=CARTESIAN_POINT('Ctrl Pts',(7.39451698709202,-30.2843884245509,57.0362239585305));
#84621=CARTESIAN_POINT('Ctrl Pts',(7.39837234395289,-30.3549350395487,57.0251173232316));
#84622=CARTESIAN_POINT('Ctrl Pts',(7.40222770081377,-30.4246804595726,57.0103840602624));
#84623=CARTESIAN_POINT('Ctrl Pts',(7.40608709329184,-30.4944988860202,56.9956353751646));
#84624=CARTESIAN_POINT('Ctrl Pts',(7.40994648576991,-30.5635139670784,56.9772525849503));
#84625=CARTESIAN_POINT('Ctrl Pts',(7.41380587824798,-30.6313284715343,56.9553572368062));
#84626=CARTESIAN_POINT('Ctrl Pts',(7.41766745586088,-30.6991813716279,56.9334494918177));
#84627=CARTESIAN_POINT('Ctrl Pts',(7.42152903347377,-30.7658318878465,56.9080254031064));
#84628=CARTESIAN_POINT('Ctrl Pts',(7.42539061108667,-30.8309020153114,56.8792550128845));
#84629=CARTESIAN_POINT('Ctrl Pts',(7.42925894521082,-30.8960859944432,56.8504342837896));
#84630=CARTESIAN_POINT('Ctrl Pts',(7.43312727933496,-30.9596836304835,56.8182557830043));
#84631=CARTESIAN_POINT('Ctrl Pts',(7.43699561345911,-31.0213414229231,56.7829355738));
#84632=CARTESIAN_POINT('Ctrl Pts',(7.43929333254379,-31.0579650138179,56.7619560213211));
#84633=CARTESIAN_POINT('Ctrl Pts',(7.44159105162846,-31.0939047372455,56.7398688732165));
#84634=CARTESIAN_POINT('Ctrl Pts',(7.44388877071314,-31.1290918065592,56.7167263191496));
#84635=CARTESIAN_POINT('Ctrl Pts',(7.44663026262674,-31.1710747742032,56.6891140991626));
#84636=CARTESIAN_POINT('Ctrl Pts',(7.44937175454035,-31.2121024284199,56.6599226547301));
#84637=CARTESIAN_POINT('Ctrl Pts',(7.45211324645396,-31.2520475724682,56.6292251037768));
#84638=CARTESIAN_POINT('',(7.14592528050079,-27.9452507538412,54.9982399120147));
#84639=CARTESIAN_POINT('Ctrl Pts',(7.14592528053768,-27.9452507538406,54.9982399126965));
#84640=CARTESIAN_POINT('Ctrl Pts',(7.14975890798127,-27.9451900689549,55.0690842525566));
#84641=CARTESIAN_POINT('Ctrl Pts',(7.15359253542486,-27.948797567142,55.1399937211669));
#84642=CARTESIAN_POINT('Ctrl Pts',(7.15742616286845,-27.9560667657204,55.2105575843025));
#84643=CARTESIAN_POINT('Ctrl Pts',(7.16125834634855,-27.9633332263026,55.281094869049));
#84644=CARTESIAN_POINT('Ctrl Pts',(7.16509052982866,-27.9742586004218,55.3512863175633));
#84645=CARTESIAN_POINT('Ctrl Pts',(7.16892271330876,-27.9887844405815,55.420725012393));
#84646=CARTESIAN_POINT('Ctrl Pts',(7.1727547734992,-28.0033098134134,55.4901614732291));
#84647=CARTESIAN_POINT('Ctrl Pts',(7.17658683368964,-28.0214353197262,55.5588447472065));
#84648=CARTESIAN_POINT('Ctrl Pts',(7.18041889388008,-28.0430515099035,55.6263786152231));
#84649=CARTESIAN_POINT('Ctrl Pts',(7.184254856409,-28.0646897127022,55.693981255649));
#84650=CARTESIAN_POINT('Ctrl Pts',(7.18809081893791,-28.0898255470869,55.7604316831495));
#84651=CARTESIAN_POINT('Ctrl Pts',(7.19192678146683,-28.1183001035102,55.8253502662811));
#84652=CARTESIAN_POINT('Ctrl Pts',(7.19576473620228,-28.1467894481899,55.8903025648687));
#84653=CARTESIAN_POINT('Ctrl Pts',(7.19960269093773,-28.1786207452875,55.9537209954183));
#84654=CARTESIAN_POINT('Ctrl Pts',(7.20344064567318,-28.2135887279427,56.0152498852827));
#84655=CARTESIAN_POINT('Ctrl Pts',(7.20728565488564,-28.2486209846309,56.0768918703159));
#84656=CARTESIAN_POINT('Ctrl Pts',(7.2111306640981,-28.2868011751235,56.13663696377));
#84657=CARTESIAN_POINT('Ctrl Pts',(7.21497567331056,-28.3278806170888,56.1941584198894));
#84658=CARTESIAN_POINT('Ctrl Pts',(7.21791465037583,-28.3592801615682,56.2381256072106));
#84659=CARTESIAN_POINT('Ctrl Pts',(7.2208536274411,-28.3923726831846,56.280794230244));
#84660=CARTESIAN_POINT('Ctrl Pts',(7.22379260450636,-28.4270322754391,56.3220325638916));
#84661=CARTESIAN_POINT('Ctrl Pts',(7.22766167785587,-28.472660567773,56.3763215679058));
#84662=CARTESIAN_POINT('Ctrl Pts',(7.23153075120538,-28.521192108488,56.4283519319452));
#84663=CARTESIAN_POINT('Ctrl Pts',(7.23539982455489,-28.5723747010563,56.4777968630078));
#84664=CARTESIAN_POINT('Ctrl Pts',(7.23926313295198,-28.6234810311232,56.5271681206997));
#84665=CARTESIAN_POINT('Ctrl Pts',(7.24312644134906,-28.6772302256901,56.5739612573856));
#84666=CARTESIAN_POINT('Ctrl Pts',(7.24698974974614,-28.7333303795716,56.6178830721606));
#84667=CARTESIAN_POINT('Ctrl Pts',(7.25084852624035,-28.7893647244566,56.6617533638942));
#84668=CARTESIAN_POINT('Ctrl Pts',(7.25470730273456,-28.8477441700428,56.7027587261681));
#84669=CARTESIAN_POINT('Ctrl Pts',(7.25856607922877,-28.9081418597549,56.7406445254792));
#84670=CARTESIAN_POINT('Ctrl Pts',(7.26242242481827,-28.968501500871,56.7785064579589));
#84671=CARTESIAN_POINT('Ctrl Pts',(7.26627877040777,-29.0308764530672,56.8132524689205));
#84672=CARTESIAN_POINT('Ctrl Pts',(7.27013511599727,-29.0949100511598,56.844670633747));
#84673=CARTESIAN_POINT('Ctrl Pts',(7.27399032224389,-29.1589247307653,56.8760795161942));
#84674=CARTESIAN_POINT('Ctrl Pts',(7.27784552849051,-29.2245966475194,56.9041622905641));
#84675=CARTESIAN_POINT('Ctrl Pts',(7.28170073473713,-29.2915451873075,56.9287533126019));
#84676=CARTESIAN_POINT('Ctrl Pts',(7.28555609158967,-29.3584963424798,56.9533452953025));
#84677=CARTESIAN_POINT('Ctrl Pts',(7.2894114484422,-29.4267237629434,56.9744450894259));
#84678=CARTESIAN_POINT('Ctrl Pts',(7.29326680529473,-29.4958291746578,56.9919360786365));
#84679=CARTESIAN_POINT('Ctrl Pts',(7.29712619776456,-29.5650069228655,57.0094453766422));
#84680=CARTESIAN_POINT('Ctrl Pts',(7.30098559023439,-29.6350640250389,57.0233382094805));
#84681=CARTESIAN_POINT('Ctrl Pts',(7.30484498270421,-29.7055903194803,57.0335487460389));
#84682=CARTESIAN_POINT('Ctrl Pts',(7.30870656030891,-29.7761565449383,57.0437650636625));
#84683=CARTESIAN_POINT('Ctrl Pts',(7.3125681379136,-29.8471920075161,57.0502948901935));
#84684=CARTESIAN_POINT('Ctrl Pts',(7.3164297155183,-29.9182824477439,57.0531244005547));
#84685=CARTESIAN_POINT('Ctrl Pts',(7.3202980496344,-29.9894972732411,57.0559588616436));
#84686=CARTESIAN_POINT('Ctrl Pts',(7.32416638375051,-30.0607667825374,57.0550800863142));
#84687=CARTESIAN_POINT('Ctrl Pts',(7.32803471786662,-30.1316784465509,57.0505263590634));
#84688=CARTESIAN_POINT('Ctrl Pts',(7.33033243702605,-30.1737986678505,57.047821529016));
#84689=CARTESIAN_POINT('Ctrl Pts',(7.33263015618548,-30.2157927466636,57.0438211176024));
#84690=CARTESIAN_POINT('Ctrl Pts',(7.33492787534492,-30.2575759412518,57.0385416838976));
#84691=CARTESIAN_POINT('Ctrl Pts',(7.33879679455246,-30.3279308422981,57.0296521281913));
#84692=CARTESIAN_POINT('Ctrl Pts',(7.34266571376,-30.397962804919,57.0170987141503));
#84693=CARTESIAN_POINT('Ctrl Pts',(7.34653463296754,-30.4672605428605,57.0009160770971));
#84694=CARTESIAN_POINT('Ctrl Pts',(7.35048283886946,-30.5379784160581,56.98440180536));
#84695=CARTESIAN_POINT('Ctrl Pts',(7.35443104477139,-30.6079311216361,56.9641078764496));
#84696=CARTESIAN_POINT('Ctrl Pts',(7.35837925067332,-30.6766868505021,56.9401269208115));
#84697=CARTESIAN_POINT('Ctrl Pts',(7.36223788201552,-30.7438826900678,56.9166900309076));
#84698=CARTESIAN_POINT('Ctrl Pts',(7.36609651335773,-30.8099348054257,56.8897318132154));
#84699=CARTESIAN_POINT('Ctrl Pts',(7.36995514469993,-30.8744523799092,56.8593898455599));
#84700=CARTESIAN_POINT('Ctrl Pts',(7.37394813788172,-30.9412165281709,56.8279913368074));
#84701=CARTESIAN_POINT('Ctrl Pts',(7.37794113106351,-31.0063367702874,56.7929692085721));
#84702=CARTESIAN_POINT('Ctrl Pts',(7.3819341242453,-31.0694017134189,56.7545305747797));
#84703=CARTESIAN_POINT('Ctrl Pts',(7.38592711742709,-31.1324666565503,56.7160919409874));
#84704=CARTESIAN_POINT('Ctrl Pts',(7.38992011060888,-31.1934757962958,56.6742370852408));
#84705=CARTESIAN_POINT('Ctrl Pts',(7.39391310379067,-31.2520475724682,56.6292251037768));
#84706=CARTESIAN_POINT('Ctrl Pts',(6.69398930341885,-31.2520475724682,56.6292251037768));
#84707=CARTESIAN_POINT('Ctrl Pts',(6.69784740330321,-31.308493025076,56.5858471864156));
#84708=CARTESIAN_POINT('Ctrl Pts',(6.70170550318757,-31.3627399888065,56.5394875421447));
#84709=CARTESIAN_POINT('Ctrl Pts',(6.70556360307192,-31.414461700709,56.4904011740895));
#84710=CARTESIAN_POINT('Ctrl Pts',(6.70941957071704,-31.4661548277986,56.4413419343833));
#84711=CARTESIAN_POINT('Ctrl Pts',(6.71327553836214,-31.5153251205055,56.389559294783));
#84712=CARTESIAN_POINT('Ctrl Pts',(6.71713150600726,-31.5616800291382,56.3353475386921));
#84713=CARTESIAN_POINT('Ctrl Pts',(6.72098663248669,-31.6080248256118,56.2811476087037));
#84714=CARTESIAN_POINT('Ctrl Pts',(6.72484175896612,-31.6515551421313,56.2245199837088));
#84715=CARTESIAN_POINT('Ctrl Pts',(6.72869688544555,-31.6920175240008,56.1657934040705));
#84716=CARTESIAN_POINT('Ctrl Pts',(6.73255246051975,-31.7324846142015,56.1070599908209));
#84717=CARTESIAN_POINT('Ctrl Pts',(6.73640803559394,-31.7698827875426,56.0462275395085));
#84718=CARTESIAN_POINT('Ctrl Pts',(6.74026361066813,-31.8040018700035,55.9836538087783));
#84719=CARTESIAN_POINT('Ctrl Pts',(6.74412340477226,-31.8381582878624,55.9210116056574));
#84720=CARTESIAN_POINT('Ctrl Pts',(6.74798319887639,-31.8690282224839,55.8566247484985));
#84721=CARTESIAN_POINT('Ctrl Pts',(6.75184299298052,-31.8964478925107,55.7908748026658));
#84722=CARTESIAN_POINT('Ctrl Pts',(6.75570523999021,-31.9238849877834,55.7250830726333));
#84723=CARTESIAN_POINT('Ctrl Pts',(6.7595674869999,-31.947867292199,55.6579269875362));
#84724=CARTESIAN_POINT('Ctrl Pts',(6.7634297340096,-31.9682804681214,55.5898046806459));
#84725=CARTESIAN_POINT('Ctrl Pts',(6.76729847021428,-31.9887279414562,55.5215679173444));
#84726=CARTESIAN_POINT('Ctrl Pts',(6.77116720641896,-32.0055942063419,55.4523621643166));
#84727=CARTESIAN_POINT('Ctrl Pts',(6.77503594262364,-32.018815894643,55.3825963225603));
#84728=CARTESIAN_POINT('Ctrl Pts',(6.77644113546647,-32.0236182437276,55.3572561452198));
#84729=CARTESIAN_POINT('Ctrl Pts',(6.7778463283093,-32.0279402711051,55.3318421247497));
#84730=CARTESIAN_POINT('Ctrl Pts',(6.77925152115213,-32.0317806392833,55.3063739485232));
#84731=CARTESIAN_POINT('Ctrl Pts',(6.78312059450031,-32.042354751044,55.2362495934447));
#84732=CARTESIAN_POINT('Ctrl Pts',(6.78698966784849,-32.0493149318717,55.1654398123004));
#84733=CARTESIAN_POINT('Ctrl Pts',(6.79085874119666,-32.0525826818245,55.094349863667));
#84734=CARTESIAN_POINT('Ctrl Pts',(6.79472204959242,-32.0558455628019,55.0233658396658));
#84735=CARTESIAN_POINT('Ctrl Pts',(6.79858535798817,-32.0554269116062,54.9521029581258));
#84736=CARTESIAN_POINT('Ctrl Pts',(6.80244866638393,-32.0512996831102,54.8809740676497));
#84737=CARTESIAN_POINT('Ctrl Pts',(6.8063074428768,-32.0471772961119,54.8099286158201));
#84738=CARTESIAN_POINT('Ctrl Pts',(6.81016621936967,-32.0393550011702,54.7390173254582));
#84739=CARTESIAN_POINT('Ctrl Pts',(6.81402499586255,-32.0278577964953,54.6686537767027));
#84740=CARTESIAN_POINT('Ctrl Pts',(6.81788134145071,-32.0163678346884,54.5983345547129));
#84741=CARTESIAN_POINT('Ctrl Pts',(6.82173768703888,-32.0012076343708,54.5285628680314));
#84742=CARTESIAN_POINT('Ctrl Pts',(6.82559403262705,-31.982453945114,54.4597464317546));
#84743=CARTESIAN_POINT('Ctrl Pts',(6.82944923887234,-31.9637057965646,54.3909503270365));
#84744=CARTESIAN_POINT('Ctrl Pts',(6.83330444511763,-31.9413663944681,54.3231093808663));
#84745=CARTESIAN_POINT('Ctrl Pts',(6.83715965136292,-31.9155630461784,54.2566186855888));
#84746=CARTESIAN_POINT('Ctrl Pts',(6.84101500821413,-31.8897586898656,54.1901253928129));
#84747=CARTESIAN_POINT('Ctrl Pts',(6.84487036506534,-31.8604902965015,54.1249829077371));
#84748=CARTESIAN_POINT('Ctrl Pts',(6.84872572191655,-31.8279336356115,54.0615671647368));
#84749=CARTESIAN_POINT('Ctrl Pts',(6.85258511438507,-31.7953428958465,53.998085040937));
#84750=CARTESIAN_POINT('Ctrl Pts',(6.85644450685359,-31.7594572398435,53.9363337003911));
#84751=CARTESIAN_POINT('Ctrl Pts',(6.8603038993221,-31.7204984022283,53.876664426616));
#84752=CARTESIAN_POINT('Ctrl Pts',(6.8641654769255,-31.6815175066557,53.8169613689197));
#84753=CARTESIAN_POINT('Ctrl Pts',(6.8680270545289,-31.6394602522241,53.7593431172581));
#84754=CARTESIAN_POINT('Ctrl Pts',(6.87188863213229,-31.5945901053133,53.7041296521114));
#84755=CARTESIAN_POINT('Ctrl Pts',(6.87575696624712,-31.5496414501626,53.6488195812642));
#84756=CARTESIAN_POINT('Ctrl Pts',(6.87962530036195,-31.501870402007,53.5959230581635));
#84757=CARTESIAN_POINT('Ctrl Pts',(6.88349363447679,-31.4515783840528,53.5457243186209));
#84758=CARTESIAN_POINT('Ctrl Pts',(6.88579135364809,-31.4217058522635,53.515907192489));
#84759=CARTESIAN_POINT('Ctrl Pts',(6.88808907281939,-31.3909445592811,53.4870411428943));
#84760=CARTESIAN_POINT('Ctrl Pts',(6.89038679199069,-31.3593629475622,53.4591788100837));
#84761=CARTESIAN_POINT('Ctrl Pts',(6.89425586533907,-31.306183440803,53.4122621064901));
#84762=CARTESIAN_POINT('Ctrl Pts',(6.89812493868745,-31.2504680114044,53.3680098732096));
#84763=CARTESIAN_POINT('Ctrl Pts',(6.90199401203584,-31.1925145591998,53.3267078591601));
#84764=CARTESIAN_POINT('Ctrl Pts',(6.9058573204318,-31.1346474581352,53.2854673854652));
#84765=CARTESIAN_POINT('Ctrl Pts',(6.90972062882776,-31.0745493458754,53.2471686849971));
#84766=CARTESIAN_POINT('Ctrl Pts',(6.91358393722373,-31.0125524062089,53.2120583938002));
#84767=CARTESIAN_POINT('Ctrl Pts',(6.91744271371681,-30.9506281928385,53.1769892891753));
#84768=CARTESIAN_POINT('Ctrl Pts',(6.92130149020989,-30.8868099971729,53.1451014027383));
#84769=CARTESIAN_POINT('Ctrl Pts',(6.92516026670297,-30.8214588440329,53.1165980434171));
#84770=CARTESIAN_POINT('Ctrl Pts',(6.92901661229135,-30.7561488600111,53.0881126402929));
#84771=CARTESIAN_POINT('Ctrl Pts',(6.93287295787973,-30.6893082786984,53.0630077278985));
#84772=CARTESIAN_POINT('Ctrl Pts',(6.93672930346811,-30.6213212655178,53.0414399556012));
#84773=CARTESIAN_POINT('Ctrl Pts',(6.94058450971361,-30.553354338846,53.0198785554216));
#84774=CARTESIAN_POINT('Ctrl Pts',(6.94443971595911,-30.4842421155299,53.001852367469));
#84775=CARTESIAN_POINT('Ctrl Pts',(6.94829492220461,-30.4143855767945,52.9874687191885));
#84776=CARTESIAN_POINT('Ctrl Pts',(6.95215027905603,-30.3445263090721,52.9730845090023));
#84777=CARTESIAN_POINT('Ctrl Pts',(6.95600563590744,-30.2739231444505,52.9623432168141));
#84778=CARTESIAN_POINT('Ctrl Pts',(6.95986099275886,-30.2029872528514,52.9553010642934));
#84779=CARTESIAN_POINT('Ctrl Pts',(6.96372038522758,-30.1319771086933,52.9482515403583));
#84780=CARTESIAN_POINT('Ctrl Pts',(6.96757977769631,-30.0606340267051,52.9449089337532));
#84781=CARTESIAN_POINT('Ctrl Pts',(6.97143917016503,-29.9893733963683,52.9452774791239));
#84782=CARTESIAN_POINT('Ctrl Pts',(6.97530074776863,-29.9180724192437,52.94564623316));
#84783=CARTESIAN_POINT('Ctrl Pts',(6.97916232537224,-29.846854471921,52.9497302941936));
#84784=CARTESIAN_POINT('Ctrl Pts',(6.98302390297584,-29.7761312786414,52.9574818585635));
#84785=CARTESIAN_POINT('Ctrl Pts',(6.98689223709087,-29.7052843426554,52.965246985663));
#84786=CARTESIAN_POINT('Ctrl Pts',(6.9907605712059,-29.6349343686608,52.9766923496816));
#84787=CARTESIAN_POINT('Ctrl Pts',(6.99462890532094,-29.5654836366656,52.9917188711501));
#84788=CARTESIAN_POINT('Ctrl Pts',(6.99692662449037,-29.5242311818642,53.0006443479578));
#84789=CARTESIAN_POINT('Ctrl Pts',(6.99922434365981,-29.4832957357369,53.0108323415112));
#84790=CARTESIAN_POINT('Ctrl Pts',(7.00152206282925,-29.4427586443784,53.0222539005006));
#84791=CARTESIAN_POINT('Ctrl Pts',(7.00539113617725,-29.3744992235288,53.0414863855086));
#84792=CARTESIAN_POINT('Ctrl Pts',(7.00926020952525,-29.3071029468862,53.0642945225907));
#84793=CARTESIAN_POINT('Ctrl Pts',(7.01312928287325,-29.2409714547338,53.0905830130715));
#84794=CARTESIAN_POINT('Ctrl Pts',(7.01699259126881,-29.1749384990712,53.1168323334763));
#84795=CARTESIAN_POINT('Ctrl Pts',(7.02085589966438,-29.1101670348887,53.1465515357107));
#84796=CARTESIAN_POINT('Ctrl Pts',(7.02471920805995,-29.0470444364269,53.1795953042372));
#84797=CARTESIAN_POINT('Ctrl Pts',(7.02857798455265,-28.983995884729,53.2126003103524));
#84798=CARTESIAN_POINT('Ctrl Pts',(7.03243676104536,-28.9225927850239,53.2489219119851));
#84799=CARTESIAN_POINT('Ctrl Pts',(7.03629553753807,-28.8632017528946,53.2883670639187));
#84800=CARTESIAN_POINT('Ctrl Pts',(7.04015188312606,-28.8038481351997,53.3277873666791));
#84801=CARTESIAN_POINT('Ctrl Pts',(7.04400822871406,-28.7465044740157,53.3703270476567));
#84802=CARTESIAN_POINT('Ctrl Pts',(7.04786457430206,-28.6915107348276,53.4157483137366));
#84803=CARTESIAN_POINT('Ctrl Pts',(7.05171978054718,-28.636533243334,53.4611561602734));
#84804=CARTESIAN_POINT('Ctrl Pts',(7.0555749867923,-28.5839046698531,53.5094435925543));
#84805=CARTESIAN_POINT('Ctrl Pts',(7.05943019303743,-28.5339326626621,53.5603319393378));
#84806=CARTESIAN_POINT('Ctrl Pts',(7.06328554988848,-28.4839587032848,53.6112222741048));
#84807=CARTESIAN_POINT('Ctrl Pts',(7.06714090673953,-28.4366418550357,53.6647133769478));
#84808=CARTESIAN_POINT('Ctrl Pts',(7.07099626359058,-28.3922523559867,53.72049029872));
#84809=CARTESIAN_POINT('Ctrl Pts',(7.07485565605895,-28.3478163919701,53.776325605311));
#84810=CARTESIAN_POINT('Ctrl Pts',(7.07871504852731,-28.3063141971478,53.8344511263024));
#84811=CARTESIAN_POINT('Ctrl Pts',(7.08257444099567,-28.2679746215663,53.894520171617));
#84812=CARTESIAN_POINT('Ctrl Pts',(7.08643601859892,-28.2296133386449,53.9546232271981));
#84813=CARTESIAN_POINT('Ctrl Pts',(7.09029759620216,-28.1944184793473,54.0166715749077));
#84814=CARTESIAN_POINT('Ctrl Pts',(7.0941591738054,-28.1625731861767,54.0802933802874));
#84815=CARTESIAN_POINT('Ctrl Pts',(7.09802750792009,-28.1306721740462,54.1440265032425));
#84816=CARTESIAN_POINT('Ctrl Pts',(7.10189584203478,-28.1021326235921,54.2093381351123));
#84817=CARTESIAN_POINT('Ctrl Pts',(7.10576417614946,-28.0770894760653,54.2758365657938));
#84818=CARTESIAN_POINT('Ctrl Pts',(7.10806189532224,-28.0622143079664,54.3153354080879));
#84819=CARTESIAN_POINT('Ctrl Pts',(7.11035961449502,-28.0485717693018,54.3552526613278));
#84820=CARTESIAN_POINT('Ctrl Pts',(7.1126573336678,-28.0361816560159,54.3955042809652));
#84821=CARTESIAN_POINT('Ctrl Pts',(7.11737359946004,-28.0107498851777,54.4781241846623));
#84822=CARTESIAN_POINT('Ctrl Pts',(7.12208986525227,-27.9905162579312,54.5624145979724));
#84823=CARTESIAN_POINT('Ctrl Pts',(7.12680613104451,-27.9756629418006,54.6477826845532));
#84824=CARTESIAN_POINT('Ctrl Pts',(7.13145774528264,-27.9610132380222,54.7319805276169));
#84825=CARTESIAN_POINT('Ctrl Pts',(7.13610935952078,-27.9515973927135,54.8172267077131));
#84826=CARTESIAN_POINT('Ctrl Pts',(7.14076097375891,-27.9475440844109,54.9029315856555));
#84827=CARTESIAN_POINT('Ctrl Pts',(7.14248240933954,-27.9460440655413,54.9346486238212));
#84828=CARTESIAN_POINT('Ctrl Pts',(7.14420384492016,-27.9452780035318,54.9664282743128));
#84829=CARTESIAN_POINT('Ctrl Pts',(7.14592528050078,-27.9452507538412,54.9982399120147));
#84830=CARTESIAN_POINT('Origin',(-1.54592528053767,-30.,55.));
#84831=CARTESIAN_POINT('',(5.99388650793247,-31.2520475724682,56.6292251037768));
#84832=CARTESIAN_POINT('',(6.05208116158501,-31.2520475724682,56.6292251037768));
#84833=CARTESIAN_POINT('',(-1.54592528053767,-31.2520475724682,56.6292251037768));
#84834=CARTESIAN_POINT('',(6.50407471951138,-27.9452500572952,55.0004852364684));
#84835=CARTESIAN_POINT('Ctrl Pts',(6.05208116158501,-31.2520475724682,56.6292251037768));
#84836=CARTESIAN_POINT('Ctrl Pts',(6.0559362959734,-31.3085979670454,56.5857665392798));
#84837=CARTESIAN_POINT('Ctrl Pts',(6.05979143036179,-31.3628880122941,56.5393564204563));
#84838=CARTESIAN_POINT('Ctrl Pts',(6.06364656475018,-31.4146037916008,56.4902663101904));
#84839=CARTESIAN_POINT('Ctrl Pts',(6.06753147774187,-31.4667190443164,56.4407970082357));
#84840=CARTESIAN_POINT('Ctrl Pts',(6.07141639073356,-31.5162197110505,56.3886064605778));
#84841=CARTESIAN_POINT('Ctrl Pts',(6.07530130372524,-31.5628224452354,56.3340103324819));
#84842=CARTESIAN_POINT('Ctrl Pts',(6.07916181883121,-31.6091325066665,56.2797570769541));
#84843=CARTESIAN_POINT('Ctrl Pts',(6.08302233393717,-31.6525806774308,56.22312879422));
#84844=CARTESIAN_POINT('Ctrl Pts',(6.08688284904313,-31.6929308605673,56.1644666864445));
#84845=CARTESIAN_POINT('Ctrl Pts',(6.09077996097768,-31.7336635545073,56.1052484748735));
#84846=CARTESIAN_POINT('Ctrl Pts',(6.09467707291223,-31.7712389448945,56.0439581022323));
#84847=CARTESIAN_POINT('Ctrl Pts',(6.09857418484678,-31.8054613055032,55.9809724954507));
#84848=CARTESIAN_POINT('Ctrl Pts',(6.10247129678132,-31.8396836661119,55.917986888669));
#84849=CARTESIAN_POINT('Ctrl Pts',(6.10636840871587,-31.8705528390726,55.8533065288065));
#84850=CARTESIAN_POINT('Ctrl Pts',(6.11026552065042,-31.8979233773647,55.7873273881637));
#84851=CARTESIAN_POINT('Ctrl Pts',(6.11413459399863,-31.9250969925984,55.7218229482382));
#84852=CARTESIAN_POINT('Ctrl Pts',(6.11800366734685,-31.9489286475827,55.6547817560974));
#84853=CARTESIAN_POINT('Ctrl Pts',(6.12187274069506,-31.9692444247994,55.5865781771397));
#84854=CARTESIAN_POINT('Ctrl Pts',(6.12573604909085,-31.989529931334,55.5184762220989));
#84855=CARTESIAN_POINT('Ctrl Pts',(6.12959935748663,-32.0063098212,55.4492157799231));
#84856=CARTESIAN_POINT('Ctrl Pts',(6.13346266588242,-32.0194582824912,55.379190991161));
#84857=CARTESIAN_POINT('Ctrl Pts',(6.13732144237533,-32.0325913198133,55.3092483458648));
#84858=CARTESIAN_POINT('Ctrl Pts',(6.14118021886824,-32.0421013009359,55.2385436101106));
#84859=CARTESIAN_POINT('Ctrl Pts',(6.14503899536115,-32.0479127447516,55.167484185474));
#84860=CARTESIAN_POINT('Ctrl Pts',(6.14889534094935,-32.0537205275452,55.0964695259825));
#84861=CARTESIAN_POINT('Ctrl Pts',(6.15275168653756,-32.0558343561298,55.0251011039399));
#84862=CARTESIAN_POINT('Ctrl Pts',(6.15660803212577,-32.0542303877086,54.9537931096617));
#84863=CARTESIAN_POINT('Ctrl Pts',(6.1604632383711,-32.0526268931738,54.8825061830636));
#84864=CARTESIAN_POINT('Ctrl Pts',(6.16431844461643,-32.0473077931978,54.8112801341851));
#84865=CARTESIAN_POINT('Ctrl Pts',(6.16817365086176,-32.0383013546747,54.740529095983));
#84866=CARTESIAN_POINT('Ctrl Pts',(6.17202900771301,-32.0292945643097,54.6697752938498));
#84867=CARTESIAN_POINT('Ctrl Pts',(6.17588436456425,-32.0166002129385,54.5994970208538));
#84868=CARTESIAN_POINT('Ctrl Pts',(6.17973972141549,-32.0002982194621,54.5301015048793));
#84869=CARTESIAN_POINT('Ctrl Pts',(6.18359911388405,-31.9839791617788,54.460633348743));
#84870=CARTESIAN_POINT('Ctrl Pts',(6.18745850635261,-31.9640450349276,54.3920502680834));
#84871=CARTESIAN_POINT('Ctrl Pts',(6.19131789882116,-31.9406263111478,54.3247466527437));
#84872=CARTESIAN_POINT('Ctrl Pts',(6.19517947642459,-31.9171943280091,54.2574049310237));
#84873=CARTESIAN_POINT('Ctrl Pts',(6.19904105402802,-31.8902740038575,54.1913445667913));
#84874=CARTESIAN_POINT('Ctrl Pts',(6.20290263163145,-31.8600438601551,54.126939635077));
#84875=CARTESIAN_POINT('Ctrl Pts',(6.20677096574632,-31.8297608234817,54.0624220155696));
#84876=CARTESIAN_POINT('Ctrl Pts',(6.21063929986119,-31.7961566342393,53.9995660400106));
#84877=CARTESIAN_POINT('Ctrl Pts',(6.21450763397606,-31.7594552707764,53.9387202477022));
#84878=CARTESIAN_POINT('Ctrl Pts',(6.21680535314703,-31.7376553372842,53.9025789684568));
#84879=CARTESIAN_POINT('Ctrl Pts',(6.21910307231801,-31.7147635080574,53.8671463546765));
#84880=CARTESIAN_POINT('Ctrl Pts',(6.22140079148898,-31.6908335103588,53.8324899988661));
#84881=CARTESIAN_POINT('Ctrl Pts',(6.22526986483718,-31.6505383700789,53.7741330054153));
#84882=CARTESIAN_POINT('Ctrl Pts',(6.22913893818539,-31.60713957811,53.7177502591309));
#84883=CARTESIAN_POINT('Ctrl Pts',(6.2330080115336,-31.5608573285146,53.6636909180425));
#84884=CARTESIAN_POINT('Ctrl Pts',(6.23687131992938,-31.5146440398674,53.6097121258351));
#84885=CARTESIAN_POINT('Ctrl Pts',(6.24073462832517,-31.4655561351378,53.5580502330749));
#84886=CARTESIAN_POINT('Ctrl Pts',(6.24459793672096,-31.4138565131095,53.5090247075026));
#84887=CARTESIAN_POINT('Ctrl Pts',(6.24845671321387,-31.3622175379781,53.4600566919444));
#84888=CARTESIAN_POINT('Ctrl Pts',(6.25231548970677,-31.3079732818955,53.4137192332199));
#84889=CARTESIAN_POINT('Ctrl Pts',(6.25617426619967,-31.251425082429,53.3702967062783));
#84890=CARTESIAN_POINT('Ctrl Pts',(6.26003061178787,-31.194912506504,53.3269015341278));
#84891=CARTESIAN_POINT('Ctrl Pts',(6.26388695737607,-31.1360992511543,53.2864179457087));
#84892=CARTESIAN_POINT('Ctrl Pts',(6.26774330296427,-31.0753203642288,53.249090614345));
#84893=CARTESIAN_POINT('Ctrl Pts',(6.27159850920959,-31.014559434198,53.2117743112016));
#84894=CARTESIAN_POINT('Ctrl Pts',(6.27545371545491,-30.9518344392441,53.1776126679242));
#84895=CARTESIAN_POINT('Ctrl Pts',(6.27930892170023,-30.8875086414516,53.1468065471061));
#84896=CARTESIAN_POINT('Ctrl Pts',(6.28316427855146,-30.8231803307336,53.1159992228286));
#84897=CARTESIAN_POINT('Ctrl Pts',(6.2870196354027,-30.7572515321044,53.0885478891026));
#84898=CARTESIAN_POINT('Ctrl Pts',(6.29087499225394,-30.6901077205897,53.0646062683571));
#84899=CARTESIAN_POINT('Ctrl Pts',(6.29473438472249,-30.6228936258978,53.0406395865802));
#84900=CARTESIAN_POINT('Ctrl Pts',(6.29859377719104,-30.5544624379835,53.0201901150296));
#84901=CARTESIAN_POINT('Ctrl Pts',(6.30245316965959,-30.4852162643896,53.0033621411804));
#84902=CARTESIAN_POINT('Ctrl Pts',(6.30631474726301,-30.4159308845658,52.9865246395641));
#84903=CARTESIAN_POINT('Ctrl Pts',(6.31017632486644,-30.3458300780981,52.9733128074614));
#84904=CARTESIAN_POINT('Ctrl Pts',(6.31403790246986,-30.2753249453433,52.9637795460777));
#84905=CARTESIAN_POINT('Ctrl Pts',(6.31790623658473,-30.2046964514173,52.9542296045709));
#84906=CARTESIAN_POINT('Ctrl Pts',(6.32177457069959,-30.1336627030752,52.9483711240021));
#84907=CARTESIAN_POINT('Ctrl Pts',(6.32564290481446,-30.0626380011789,52.9462049656043));
#84908=CARTESIAN_POINT('Ctrl Pts',(6.32794062398548,-30.0204506372341,52.9449183074382));
#84909=CARTESIAN_POINT('Ctrl Pts',(6.33023834315651,-29.9782664489834,52.9449333531371));
#84910=CARTESIAN_POINT('Ctrl Pts',(6.33253606232754,-29.9361713635722,52.9462416238341));
#84911=CARTESIAN_POINT('Ctrl Pts',(6.33640513567578,-29.8652884745271,52.948444588996));
#84912=CARTESIAN_POINT('Ctrl Pts',(6.34027420902402,-29.7943809273119,52.9543258278911));
#84913=CARTESIAN_POINT('Ctrl Pts',(6.34414328237226,-29.7238614901472,52.9638897166714));
#84914=CARTESIAN_POINT('Ctrl Pts',(6.34800659076806,-29.6534471275482,52.9734393551756));
#84915=CARTESIAN_POINT('Ctrl Pts',(6.35186989916386,-29.5834202045728,52.986660686914));
#84916=CARTESIAN_POINT('Ctrl Pts',(6.35573320755966,-29.514191706844,53.0035061069964));
#84917=CARTESIAN_POINT('Ctrl Pts',(6.3595919840526,-29.4450444184816,53.0203317663452));
#84918=CARTESIAN_POINT('Ctrl Pts',(6.36345076054553,-29.3766941646777,53.0407729552545));
#84919=CARTESIAN_POINT('Ctrl Pts',(6.36730953703847,-29.3095432958884,53.0647307416674));
#84920=CARTESIAN_POINT('Ctrl Pts',(6.37116588262669,-29.2424347299802,53.0886734354476));
#84921=CARTESIAN_POINT('Ctrl Pts',(6.37502222821492,-29.1765245064967,53.1161281686743));
#84922=CARTESIAN_POINT('Ctrl Pts',(6.37887857380315,-29.1121999040753,53.1469461550791));
#84923=CARTESIAN_POINT('Ctrl Pts',(6.3827337800485,-29.047894306117,53.1777550364251));
#84924=CARTESIAN_POINT('Ctrl Pts',(6.38658898629385,-28.9851738370485,53.2119249884776));
#84925=CARTESIAN_POINT('Ctrl Pts',(6.3904441925392,-28.9244042705919,53.2492597595934));
#84926=CARTESIAN_POINT('Ctrl Pts',(6.39429954939044,-28.8636323301366,53.2865959892138));
#84927=CARTESIAN_POINT('Ctrl Pts',(6.39815490624169,-28.8048118563631,53.3270970271894));
#84928=CARTESIAN_POINT('Ctrl Pts',(6.40201026309293,-28.7482810659899,53.3705223926851));
#84929=CARTESIAN_POINT('Ctrl Pts',(6.40586965556151,-28.6916911016811,53.4139932139362));
#84930=CARTESIAN_POINT('Ctrl Pts',(6.4097290480301,-28.6373959912352,53.460394176726));
#84931=CARTESIAN_POINT('Ctrl Pts',(6.41358844049868,-28.5857014397924,53.5094440147734));
#84932=CARTESIAN_POINT('Ctrl Pts',(6.41745001810214,-28.5339776196065,53.5585216241637));
#84933=CARTESIAN_POINT('Ctrl Pts',(6.4213115957056,-28.4848576241816,53.6102507419261));
#84934=CARTESIAN_POINT('Ctrl Pts',(6.42517317330906,-28.4386088641938,53.6643146764579));
#84935=CARTESIAN_POINT('Ctrl Pts',(6.42904150742395,-28.3922791838392,53.7184732053833));
#84936=CARTESIAN_POINT('Ctrl Pts',(6.43290984153884,-28.3488310651725,53.7749743220315));
#84937=CARTESIAN_POINT('Ctrl Pts',(6.43677817565373,-28.3084899336607,53.8334704213039));
#84938=CARTESIAN_POINT('Ctrl Pts',(6.43907589482452,-28.2845280450304,53.8682160261878));
#84939=CARTESIAN_POINT('Ctrl Pts',(6.44137361399531,-28.2616614968995,53.9036649604587));
#84940=CARTESIAN_POINT('Ctrl Pts',(6.4436713331661,-28.2399297696001,53.9397404343464));
#84941=CARTESIAN_POINT('Ctrl Pts',(6.44766818401096,-28.2021277293329,54.0024932242084));
#84942=CARTESIAN_POINT('Ctrl Pts',(6.45166503485582,-28.1676219954086,54.0673751957459));
#84943=CARTESIAN_POINT('Ctrl Pts',(6.45566188570067,-28.1366498578021,54.1340185856088));
#84944=CARTESIAN_POINT('Ctrl Pts',(6.45969628851415,-28.1053867249134,54.2012881160463));
#84945=CARTESIAN_POINT('Ctrl Pts',(6.46373069132762,-28.0777242453427,54.2703519944481));
#84946=CARTESIAN_POINT('Ctrl Pts',(6.46776509414109,-28.0538611856042,54.3408025503673));
#84947=CARTESIAN_POINT('Ctrl Pts',(6.4717464869999,-28.0303116740595,54.4103274226233));
#84948=CARTESIAN_POINT('Ctrl Pts',(6.4757278798587,-28.0104625063917,54.4812023266614));
#84949=CARTESIAN_POINT('Ctrl Pts',(6.47970927271751,-27.9944576731887,54.5530128213601));
#84950=CARTESIAN_POINT('Ctrl Pts',(6.48377018050831,-27.9781331972706,54.6262574891748));
#84951=CARTESIAN_POINT('Ctrl Pts',(6.48783108829911,-27.9658084880446,54.7004751038003));
#84952=CARTESIAN_POINT('Ctrl Pts',(6.49189199608992,-27.9575832299835,54.7752083185357));
#84953=CARTESIAN_POINT('Ctrl Pts',(6.49595290388072,-27.9493579719225,54.8499415332711));
#84954=CARTESIAN_POINT('Ctrl Pts',(6.50001381167153,-27.9452322760607,54.9251898673996));
#84955=CARTESIAN_POINT('Ctrl Pts',(6.50407471946233,-27.9452500572949,55.000485235559));
#84956=CARTESIAN_POINT('Ctrl Pts',(6.50407471951138,-27.9452500572952,55.0004852364684));
#84957=CARTESIAN_POINT('Ctrl Pts',(6.50830237655248,-27.9452685686983,55.078872387755));
#84958=CARTESIAN_POINT('Ctrl Pts',(6.51253003359359,-27.9497773969995,55.1571404354878));
#84959=CARTESIAN_POINT('Ctrl Pts',(6.5167576906347,-27.9587077545003,55.2347840091714));
#84960=CARTESIAN_POINT('Ctrl Pts',(6.52089243721875,-27.9674418511433,55.3107212240261));
#84961=CARTESIAN_POINT('Ctrl Pts',(6.52502718380281,-27.9804049307443,55.3860607936642));
#84962=CARTESIAN_POINT('Ctrl Pts',(6.52916193038687,-27.9974813727946,55.4603441214953));
#84963=CARTESIAN_POINT('Ctrl Pts',(6.5334360426565,-28.0151333930587,55.537131241687));
#84964=CARTESIAN_POINT('Ctrl Pts',(6.53771015492613,-28.0371808331558,55.6127892221116));
#84965=CARTESIAN_POINT('Ctrl Pts',(6.54198426719577,-28.0634417891518,55.6868332101001));
#84966=CARTESIAN_POINT('Ctrl Pts',(6.5462583794654,-28.0897027451478,55.7608771980886));
#84967=CARTESIAN_POINT('Ctrl Pts',(6.55053249173503,-28.1201769686499,55.8333068289191));
#84968=CARTESIAN_POINT('Ctrl Pts',(6.55480660400466,-28.1546308748034,55.903664956868));
#84969=CARTESIAN_POINT('Ctrl Pts',(6.55867567735284,-28.1858197349993,55.967355552833));
#84970=CARTESIAN_POINT('Ctrl Pts',(6.56254475070101,-28.2203708581139,56.0295543399142));
#84971=CARTESIAN_POINT('Ctrl Pts',(6.56641382404919,-28.2581183028436,56.0898833495433));
#84972=CARTESIAN_POINT('Ctrl Pts',(6.57027713244494,-28.2958095035574,56.1501224684313));
#84973=CARTESIAN_POINT('Ctrl Pts',(6.57414044084069,-28.3366873167933,56.2084969315059));
#84974=CARTESIAN_POINT('Ctrl Pts',(6.57800374923644,-28.3805391633643,56.2646517944095));
#84975=CARTESIAN_POINT('Ctrl Pts',(6.58186252572931,-28.4243395689709,56.3207407841395));
#84976=CARTESIAN_POINT('Ctrl Pts',(6.58572130222218,-28.4711067805808,56.3746149645711));
#84977=CARTESIAN_POINT('Ctrl Pts',(6.58958007871506,-28.5205849981006,56.4259483913014));
#84978=CARTESIAN_POINT('Ctrl Pts',(6.59343642430322,-28.5700320459395,56.4772494796288));
#84979=CARTESIAN_POINT('Ctrl Pts',(6.59729276989139,-28.622186375022,56.5260126408675));
#84980=CARTESIAN_POINT('Ctrl Pts',(6.60114911547956,-28.6767529565492,56.5719461900774));
#84981=CARTESIAN_POINT('Ctrl Pts',(6.60500432172485,-28.7313034165841,56.6178661683919));
#84982=CARTESIAN_POINT('Ctrl Pts',(6.60885952797014,-28.7882643427362,56.6609578816927));
#84983=CARTESIAN_POINT('Ctrl Pts',(6.61271473421543,-28.8473063029057,56.7009687837168));
#84984=CARTESIAN_POINT('Ctrl Pts',(6.61657009106664,-28.9063505695843,56.7409812487906));
#84985=CARTESIAN_POINT('Ctrl Pts',(6.62042544791785,-28.9674756283041,56.7779123929436));
#84986=CARTESIAN_POINT('Ctrl Pts',(6.62428080476905,-29.0303230844249,56.8115529917451));
#84987=CARTESIAN_POINT('Ctrl Pts',(6.62814019723757,-29.0932363264876,56.84522880404));
#84988=CARTESIAN_POINT('Ctrl Pts',(6.63199958970609,-29.157875135837,56.87560696547));
#84989=CARTESIAN_POINT('Ctrl Pts',(6.63585898217461,-29.2238573333837,56.9025246709459));
#84990=CARTESIAN_POINT('Ctrl Pts',(6.639720559778,-29.2898768891422,56.929457616856));
#84991=CARTESIAN_POINT('Ctrl Pts',(6.64358213738139,-29.3572408882721,56.9529260466306));
#84992=CARTESIAN_POINT('Ctrl Pts',(6.64744371498479,-29.425550632775,56.9728166379557));
#84993=CARTESIAN_POINT('Ctrl Pts',(6.65131204909962,-29.4939798972298,56.9927420313802));
#84994=CARTESIAN_POINT('Ctrl Pts',(6.65518038321445,-29.5633577378047,57.0090769765956));
#84995=CARTESIAN_POINT('Ctrl Pts',(6.65904871732928,-29.633274568757,57.0217591401004));
#84996=CARTESIAN_POINT('Ctrl Pts',(6.6613464365006,-29.6748038777845,57.0292921114917));
#84997=CARTESIAN_POINT('Ctrl Pts',(6.6636441556719,-29.7165232177405,57.0355373207604));
#84998=CARTESIAN_POINT('Ctrl Pts',(6.66594187484321,-29.7583463546465,57.0404904013955));
#84999=CARTESIAN_POINT('Ctrl Pts',(6.66980984683663,-29.8287512693327,57.048828399101));
#85000=CARTESIAN_POINT('Ctrl Pts',(6.67367781883005,-29.8997260959449,57.0535345806531));
#85001=CARTESIAN_POINT('Ctrl Pts',(6.67754579082347,-29.9708636354741,57.0545434127227));
#85002=CARTESIAN_POINT('Ctrl Pts',(6.68140849503898,-30.04190429303,57.0555508708674));
#85003=CARTESIAN_POINT('Ctrl Pts',(6.68527119925449,-30.1131067427456,57.0528709610101));
#85004=CARTESIAN_POINT('Ctrl Pts',(6.68913390347,-30.184057680519,57.0464897587679));
#85005=CARTESIAN_POINT('Ctrl Pts',(6.69299263966152,-30.2549357328196,57.0401151117167));
#85006=CARTESIAN_POINT('Ctrl Pts',(6.69685137585305,-30.3255623046268,57.0300467605916));
#85007=CARTESIAN_POINT('Ctrl Pts',(6.70071011204457,-30.3955248305998,57.0163228091947));
#85008=CARTESIAN_POINT('Ctrl Pts',(6.70456617531123,-30.4654388939246,57.0026083643018));
#85009=CARTESIAN_POINT('Ctrl Pts',(6.7084222385779,-30.5346893492482,56.9852434401783));
#85010=CARTESIAN_POINT('Ctrl Pts',(6.71227830184456,-30.6028712102003,56.9643176592424));
#85011=CARTESIAN_POINT('Ctrl Pts',(6.71613400849585,-30.6710467655764,56.9433938135588));
#85012=CARTESIAN_POINT('Ctrl Pts',(6.71998971514715,-30.7381534548819,56.9189098952706));
#85013=CARTESIAN_POINT('Ctrl Pts',(6.72384542179844,-30.803800270683,56.8910057343514));
#85014=CARTESIAN_POINT('Ctrl Pts',(6.72770090164934,-30.8694432250069,56.8631032148109));
#85015=CARTESIAN_POINT('Ctrl Pts',(6.73155638150024,-30.9336260323887,56.8317810498497));
#85016=CARTESIAN_POINT('Ctrl Pts',(6.73541186135113,-30.9959784893288,56.797226866952));
#85017=CARTESIAN_POINT('Ctrl Pts',(6.7392700583216,-31.0583748886803,56.7626483322615));
#85018=CARTESIAN_POINT('Ctrl Pts',(6.74312825529208,-31.1189379422677,56.7248334770738));
#85019=CARTESIAN_POINT('Ctrl Pts',(6.74698645226255,-31.1773238940585,56.6840148488));
#85020=CARTESIAN_POINT('Ctrl Pts',(6.74866000838574,-31.2026497568582,56.666309100283));
#85021=CARTESIAN_POINT('Ctrl Pts',(6.75033356450893,-31.2275663741968,56.6480387255383));
#85022=CARTESIAN_POINT('Ctrl Pts',(6.75200712063213,-31.2520475724682,56.6292251037768));
#85023=CARTESIAN_POINT('',(6.44592528053626,-27.9452500000201,54.999990915418));
#85024=CARTESIAN_POINT('Ctrl Pts',(6.44592528053768,-27.9452500000201,54.999990915444));
#85025=CARTESIAN_POINT('Ctrl Pts',(6.44979385259826,-27.9452496865186,55.0708988474439));
#85026=CARTESIAN_POINT('Ctrl Pts',(6.45366242465885,-27.9489241543316,55.1419458653842));
#85027=CARTESIAN_POINT('Ctrl Pts',(6.45753099671943,-27.9562906464585,55.2127196294351));
#85028=CARTESIAN_POINT('Ctrl Pts',(6.4613938042328,-27.9636461617984,55.28338793372));
#85029=CARTESIAN_POINT('Ctrl Pts',(6.46525661174617,-27.9746827313674,55.3537833129638));
#85030=CARTESIAN_POINT('Ctrl Pts',(6.46911941925954,-27.9893655867764,55.4234935877451));
#85031=CARTESIAN_POINT('Ctrl Pts',(6.47297769671014,-28.0040312230369,55.493122110609));
#85032=CARTESIAN_POINT('Ctrl Pts',(6.47683597416074,-28.0223345516742,55.5620666517312));
#85033=CARTESIAN_POINT('Ctrl Pts',(6.48069425161134,-28.0441892329501,55.6299220634266));
#85034=CARTESIAN_POINT('Ctrl Pts',(6.48455010010934,-28.0660301557584,55.6977347572041));
#85035=CARTESIAN_POINT('Ctrl Pts',(6.48840594860733,-28.0914178469666,55.7644592204328));
#85036=CARTESIAN_POINT('Ctrl Pts',(6.49226179710533,-28.1202156677511,55.8297038186796));
#85037=CARTESIAN_POINT('Ctrl Pts',(6.4961165089705,-28.1490049994706,55.8949291840255));
#85038=CARTESIAN_POINT('Ctrl Pts',(6.49997122083567,-28.1812022689765,55.958675106127));
#85039=CARTESIAN_POINT('Ctrl Pts',(6.50382593270084,-28.2166227266648,56.020569969895));
#85040=CARTESIAN_POINT('Ctrl Pts',(6.5076807986421,-28.2520446001387,56.0824673076531));
#85041=CARTESIAN_POINT('Ctrl Pts',(6.51153566458336,-28.2906896742964,56.1425130195333));
#85042=CARTESIAN_POINT('Ctrl Pts',(6.51539053052463,-28.3323281363288,56.2003616611753));
#85043=CARTESIAN_POINT('Ctrl Pts',(6.519249432972,-28.3740101988156,56.2582708772701));
#85044=CARTESIAN_POINT('Ctrl Pts',(6.52310833541937,-28.4186916216786,56.3139780354875));
#85045=CARTESIAN_POINT('Ctrl Pts',(6.52696723786674,-28.4661008192273,56.3671689236246));
#85046=CARTESIAN_POINT('Ctrl Pts',(6.53082833001039,-28.5135369186594,56.4203899944086));
#85047=CARTESIAN_POINT('Ctrl Pts',(6.53468942215403,-28.5637035320734,56.471091607219));
#85048=CARTESIAN_POINT('Ctrl Pts',(6.53855051429768,-28.6162924800363,56.5189967286653));
#85049=CARTESIAN_POINT('Ctrl Pts',(6.54241835505556,-28.6689733456508,56.5669855811318));
#85050=CARTESIAN_POINT('Ctrl Pts',(6.54628619581344,-28.724084622834,56.6121678755227));
#85051=CARTESIAN_POINT('Ctrl Pts',(6.55015403657131,-28.7812859390421,56.6543075893326));
#85052=CARTESIAN_POINT('Ctrl Pts',(6.55242968420588,-28.8149403855593,56.6791005283536));
#85053=CARTESIAN_POINT('Ctrl Pts',(6.55470533184044,-28.8493177649882,56.7028410824421));
#85054=CARTESIAN_POINT('Ctrl Pts',(6.55698097947501,-28.884344705424,56.7254885760806));
#85055=CARTESIAN_POINT('Ctrl Pts',(6.56085005282324,-28.9438977749117,56.7639940163386));
#85056=CARTESIAN_POINT('Ctrl Pts',(6.56471912617148,-29.0055632836953,56.7994881602144));
#85057=CARTESIAN_POINT('Ctrl Pts',(6.56858819951972,-29.0690042255801,56.8317326307385));
#85058=CARTESIAN_POINT('Ctrl Pts',(6.57245150791552,-29.132350639918,56.8639290567254));
#85059=CARTESIAN_POINT('Ctrl Pts',(6.57631481631132,-29.1974668067599,56.8928852023626));
#85060=CARTESIAN_POINT('Ctrl Pts',(6.58017812470713,-29.2639876198707,56.9184064581825));
#85061=CARTESIAN_POINT('Ctrl Pts',(6.58403690120006,-29.3304303998987,56.9438977759699));
#85062=CARTESIAN_POINT('Ctrl Pts',(6.587895677693,-29.3982741018804,56.9659620344099));
#85063=CARTESIAN_POINT('Ctrl Pts',(6.59175445418593,-29.4671315275863,56.9844517513932));
#85064=CARTESIAN_POINT('Ctrl Pts',(6.59561079977416,-29.5359455753353,57.0029298204513));
#85065=CARTESIAN_POINT('Ctrl Pts',(6.59946714536239,-29.6057716117535,57.0178376899947));
#85066=CARTESIAN_POINT('Ctrl Pts',(6.60332349095062,-29.6762064784604,57.0290774548816));
#85067=CARTESIAN_POINT('Ctrl Pts',(6.60717869719598,-29.7466205354494,57.0403138990221));
#85068=CARTESIAN_POINT('Ctrl Pts',(6.61103390344134,-29.8176425861672,57.0478843134957));
#85069=CARTESIAN_POINT('Ctrl Pts',(6.61488910968669,-29.8888601619433,57.0517420644167));
#85070=CARTESIAN_POINT('Ctrl Pts',(6.61874446653797,-29.9600805198763,57.0555999660429));
#85071=CARTESIAN_POINT('Ctrl Pts',(6.62259982338924,-30.0314959328385,57.0557448920874));
#85072=CARTESIAN_POINT('Ctrl Pts',(6.62645518024051,-30.1026914403188,57.0521822605668));
#85073=CARTESIAN_POINT('Ctrl Pts',(6.63031457270909,-30.1739614721126,57.0486158998409));
#85074=CARTESIAN_POINT('Ctrl Pts',(6.63417396517767,-30.2450106527457,57.0413342587147));
#85075=CARTESIAN_POINT('Ctrl Pts',(6.63803335764625,-30.3154275636869,57.0303947927845));
#85076=CARTESIAN_POINT('Ctrl Pts',(6.64189493524971,-30.3858843437134,57.0194491330794));
#85077=CARTESIAN_POINT('Ctrl Pts',(6.64575651285316,-30.4557076656982,57.0048416253513));
#85078=CARTESIAN_POINT('Ctrl Pts',(6.64961809045662,-30.524497458196,56.9866806433964));
#85079=CARTESIAN_POINT('Ctrl Pts',(6.65348642457151,-30.5934076105746,56.9684878855988));
#85080=CARTESIAN_POINT('Ctrl Pts',(6.65735475868641,-30.6612801603151,56.9467293886402));
#85081=CARTESIAN_POINT('Ctrl Pts',(6.6612230928013,-30.7277319849103,56.9215628328625));
#85082=CARTESIAN_POINT('Ctrl Pts',(6.66352081197206,-30.7672031440111,56.9066143625508));
#85083=CARTESIAN_POINT('Ctrl Pts',(6.66581853114281,-30.8061734483572,56.890464398356));
#85084=CARTESIAN_POINT('Ctrl Pts',(6.66811625031357,-30.8445667488952,56.8731536427001));
#85085=CARTESIAN_POINT('Ctrl Pts',(6.67198550519571,-30.9092193258676,56.8440031152172));
#85086=CARTESIAN_POINT('Ctrl Pts',(6.67585476007784,-30.9724875627591,56.8114442962675));
#85087=CARTESIAN_POINT('Ctrl Pts',(6.67972401495998,-31.0339883551208,56.7756310551392));
#85088=CARTESIAN_POINT('Ctrl Pts',(6.68358710202869,-31.0953911117043,56.7398749023641));
#85089=CARTESIAN_POINT('Ctrl Pts',(6.68745018909739,-31.1550316024593,56.7008748722445));
#85090=CARTESIAN_POINT('Ctrl Pts',(6.6913132761661,-31.2125483695227,56.6588321235338));
#85091=CARTESIAN_POINT('Ctrl Pts',(6.69220528525035,-31.2258293227616,56.6491242103779));
#85092=CARTESIAN_POINT('Ctrl Pts',(6.6930972943346,-31.238997144019,56.6392542625601));
#85093=CARTESIAN_POINT('Ctrl Pts',(6.69398930341885,-31.2520475724682,56.6292251037768));
#85094=CARTESIAN_POINT('Ctrl Pts',(5.99388650793247,-31.2520475724682,56.6292251037768));
#85095=CARTESIAN_POINT('Ctrl Pts',(5.99635921371572,-31.2880679719405,56.6015436903158));
#85096=CARTESIAN_POINT('Ctrl Pts',(5.99883191949896,-31.3231309837129,56.5726970835974));
#85097=CARTESIAN_POINT('Ctrl Pts',(6.00130462528221,-31.3571605423515,56.5427614283434));
#85098=CARTESIAN_POINT('Ctrl Pts',(6.00517369863043,-31.4104070139992,56.4959207379994));
#85099=CARTESIAN_POINT('Ctrl Pts',(6.00904277197864,-31.4613299633521,56.4462284604087));
#85100=CARTESIAN_POINT('Ctrl Pts',(6.01291184532686,-31.509608366483,56.3939440958463));
#85101=CARTESIAN_POINT('Ctrl Pts',(6.01677515372265,-31.5578148343796,56.3417376354349));
#85102=CARTESIAN_POINT('Ctrl Pts',(6.02063846211843,-31.6033842507581,56.2869471084688));
#85103=CARTESIAN_POINT('Ctrl Pts',(6.02450177051422,-31.6460300705182,56.2298709564218));
#85104=CARTESIAN_POINT('Ctrl Pts',(6.02836054700713,-31.688625864059,56.1728617582782));
#85105=CARTESIAN_POINT('Ctrl Pts',(6.03221932350004,-31.7283045838956,56.1135726480542));
#85106=CARTESIAN_POINT('Ctrl Pts',(6.03607809999295,-31.7648190305379,56.0523361401906));
#85107=CARTESIAN_POINT('Ctrl Pts',(6.03993444558116,-31.8013104742567,55.9911382093516));
#85108=CARTESIAN_POINT('Ctrl Pts',(6.04379079116937,-31.8346413514287,55.9279957310735));
#85109=CARTESIAN_POINT('Ctrl Pts',(6.04764713675758,-31.8646078326563,55.8632700579175));
#85110=CARTESIAN_POINT('Ctrl Pts',(6.05150234300291,-31.8945654603992,55.7985635077193));
#85111=CARTESIAN_POINT('Ctrl Pts',(6.05535754924824,-31.9211604615754,55.7322751318466));
#85112=CARTESIAN_POINT('Ctrl Pts',(6.05921275549357,-31.9442358153366,55.6647891822694));
#85113=CARTESIAN_POINT('Ctrl Pts',(6.06306811234482,-31.9673120705502,55.5973005963137));
#85114=CARTESIAN_POINT('Ctrl Pts',(6.06692346919606,-31.9868682502803,55.5286148041408));
#85115=CARTESIAN_POINT('Ctrl Pts',(6.07077882604731,-32.0027967472951,55.4591326077771));
#85116=CARTESIAN_POINT('Ctrl Pts',(6.07463821851587,-32.0187419175572,55.3895776805184));
#85117=CARTESIAN_POINT('Ctrl Pts',(6.07849761098443,-32.0310517160728,55.3192251594079));
#85118=CARTESIAN_POINT('Ctrl Pts',(6.08235700345299,-32.0396695759423,55.2484865861077));
#85119=CARTESIAN_POINT('Ctrl Pts',(6.08621858105642,-32.0482923151253,55.1777079616013));
#85120=CARTESIAN_POINT('Ctrl Pts',(6.09008015865986,-32.0532189209047,55.1065433346406));
#85121=CARTESIAN_POINT('Ctrl Pts',(6.09394173626329,-32.0544449115844,55.0354071710931));
#85122=CARTESIAN_POINT('Ctrl Pts',(6.09781007037817,-32.0556730473512,54.9641465422746));
#85123=CARTESIAN_POINT('Ctrl Pts',(6.10167840449304,-32.0531876576792,54.8929149619447));
#85124=CARTESIAN_POINT('Ctrl Pts',(6.10554673860791,-32.0470363181879,54.8221239911635));
#85125=CARTESIAN_POINT('Ctrl Pts',(6.10784445777886,-32.0433825358991,54.7800754591949));
#85126=CARTESIAN_POINT('Ctrl Pts',(6.11014217694982,-32.0384363455578,54.7381822477433));
#85127=CARTESIAN_POINT('Ctrl Pts',(6.11243989612077,-32.0322162126119,54.6965287036682));
#85128=CARTESIAN_POINT('Ctrl Pts',(6.11630896946898,-32.0217422822432,54.626389315323));
#85129=CARTESIAN_POINT('Ctrl Pts',(6.12017804281719,-32.0076124141733,54.5566554207575));
#85130=CARTESIAN_POINT('Ctrl Pts',(6.12404711616541,-31.9898705140381,54.4877374697857));
#85131=CARTESIAN_POINT('Ctrl Pts',(6.12791042456119,-31.9721550494861,54.4189222071512));
#85132=CARTESIAN_POINT('Ctrl Pts',(6.13177373295698,-31.9508383560286,54.3509209414693));
#85133=CARTESIAN_POINT('Ctrl Pts',(6.13563704135276,-31.9260157555761,54.2841362756973));
#85134=CARTESIAN_POINT('Ctrl Pts',(6.13949581784567,-31.9012222735897,54.2174299525239));
#85135=CARTESIAN_POINT('Ctrl Pts',(6.14335459433858,-31.8729312221433,54.1519378476021));
#85136=CARTESIAN_POINT('Ctrl Pts',(6.1472133708315,-31.8412878889772,54.088047987882));
#85137=CARTESIAN_POINT('Ctrl Pts',(6.1510697164197,-31.8096644900901,54.0241983767125));
#85138=CARTESIAN_POINT('Ctrl Pts',(6.15492606200791,-31.7746932144135,53.9619494424752));
#85139=CARTESIAN_POINT('Ctrl Pts',(6.15878240759611,-31.7365671002288,53.9016684157766));
#85140=CARTESIAN_POINT('Ctrl Pts',(6.16263761384144,-31.698452250262,53.8414051988816));
#85141=CARTESIAN_POINT('Ctrl Pts',(6.16649282008677,-31.6571846717615,53.7831091456009));
#85142=CARTESIAN_POINT('Ctrl Pts',(6.1703480263321,-31.6130020290762,53.727120580457));
#85143=CARTESIAN_POINT('Ctrl Pts',(6.17420338318335,-31.5688176603697,53.6711298280867));
#85144=CARTESIAN_POINT('Ctrl Pts',(6.17805874003459,-31.5217183040516,53.617447122804));
#85145=CARTESIAN_POINT('Ctrl Pts',(6.18191409688583,-31.4719823290645,53.5663802507562));
#85146=CARTESIAN_POINT('Ctrl Pts',(6.18577348935439,-31.4221942926549,53.5152599241617));
#85147=CARTESIAN_POINT('Ctrl Pts',(6.18963288182295,-31.3697644678361,53.4667612454627));
#85148=CARTESIAN_POINT('Ctrl Pts',(6.19349227429151,-31.3150079288294,53.4211549443927));
#85149=CARTESIAN_POINT('Ctrl Pts',(6.19735385189494,-31.2602203874244,53.3755228216629));
#85150=CARTESIAN_POINT('Ctrl Pts',(6.20121542949838,-31.2031038985306,53.3327866277354));
#85151=CARTESIAN_POINT('Ctrl Pts',(6.20507700710181,-31.144004242266,53.2931749192793));
#85152=CARTESIAN_POINT('Ctrl Pts',(6.20894534121668,-31.084801180724,53.2534939031493));
#85153=CARTESIAN_POINT('Ctrl Pts',(6.21281367533155,-31.0236084412542,53.2169485363527));
#85154=CARTESIAN_POINT('Ctrl Pts',(6.21668200944642,-30.9607975975375,53.1837220644774));
#85155=CARTESIAN_POINT('Ctrl Pts',(6.21897972861739,-30.9234891139714,53.1639861525462));
#85156=CARTESIAN_POINT('Ctrl Pts',(6.22127744778836,-30.8856101662258,53.1454202891853));
#85157=CARTESIAN_POINT('Ctrl Pts',(6.22357516695934,-30.8472416327671,53.1280547074751));
#85158=CARTESIAN_POINT('Ctrl Pts',(6.22744424030755,-30.7826337937888,53.0988132273933));
#85159=CARTESIAN_POINT('Ctrl Pts',(6.23131331365577,-30.7163837784897,53.0728631850843));
#85160=CARTESIAN_POINT('Ctrl Pts',(6.23518238700399,-30.6488602364774,53.050390306749));
#85161=CARTESIAN_POINT('Ctrl Pts',(6.23904569539978,-30.5814373051211,53.0279509131948));
#85162=CARTESIAN_POINT('Ctrl Pts',(6.24290900379557,-30.5127450708393,53.0089785516209));
#85163=CARTESIAN_POINT('Ctrl Pts',(6.24677231219135,-30.4431734770941,52.9936114953229));
#85164=CARTESIAN_POINT('Ctrl Pts',(6.25063108868427,-30.3736834951887,52.9782624655451));
#85165=CARTESIAN_POINT('Ctrl Pts',(6.25448986517719,-30.3033166748645,52.9665104445909));
#85166=CARTESIAN_POINT('Ctrl Pts',(6.2583486416701,-30.2324778133167,52.9584438217831));
#85167=CARTESIAN_POINT('Ctrl Pts',(6.26220498725831,-30.1616835779663,52.9503822806875));
#85168=CARTESIAN_POINT('Ctrl Pts',(6.26606133284652,-30.0904183728966,52.9460015863917));
#85169=CARTESIAN_POINT('Ctrl Pts',(6.26991767843473,-30.019095421567,52.9453387317187));
#85170=CARTESIAN_POINT('Ctrl Pts',(6.27377288468006,-29.9477935423365,52.9446760728837));
#85171=CARTESIAN_POINT('Ctrl Pts',(6.2776280909254,-29.8764344362172,52.9477290775123));
#85172=CARTESIAN_POINT('Ctrl Pts',(6.28148329717073,-29.8054329252716,52.9544826532313));
#85173=CARTESIAN_POINT('Ctrl Pts',(6.28533865402198,-29.73442864061,52.9612364927828));
#85174=CARTESIAN_POINT('Ctrl Pts',(6.28919401087323,-29.6637824622517,52.971691142247));
#85175=CARTESIAN_POINT('Ctrl Pts',(6.29304936772448,-29.5939039520625,52.9857796639023));
#85176=CARTESIAN_POINT('Ctrl Pts',(6.29690876019304,-29.5239522961346,52.9998829327999));
#85177=CARTESIAN_POINT('Ctrl Pts',(6.30076815266161,-29.4547703896441,53.0176275708756));
#85178=CARTESIAN_POINT('Ctrl Pts',(6.30462754513017,-29.3867565693747,53.038895704636));
#85179=CARTESIAN_POINT('Ctrl Pts',(6.30848912273361,-29.3187042406167,53.060175880121));
#85180=CARTESIAN_POINT('Ctrl Pts',(6.31235070033705,-29.251821770313,53.0849833536128));
#85181=CARTESIAN_POINT('Ctrl Pts',(6.31621227794049,-29.1864887175942,53.1131515811018));
#85182=CARTESIAN_POINT('Ctrl Pts',(6.32008061205536,-29.121041353171,53.1413690938754));
#85183=CARTESIAN_POINT('Ctrl Pts',(6.32394894617024,-29.0571492544873,53.1729588853264));
#85184=CARTESIAN_POINT('Ctrl Pts',(6.32781728028511,-28.995167902363,53.2077081660459));
#85185=CARTESIAN_POINT('Ctrl Pts',(6.33011499945604,-28.9583521215161,53.2283485983649));
#85186=CARTESIAN_POINT('Ctrl Pts',(6.33241271862696,-28.9222099501555,53.2501028948124));
#85187=CARTESIAN_POINT('Ctrl Pts',(6.33471043779788,-28.8868106539845,53.2729195032027));
#85188=CARTESIAN_POINT('Ctrl Pts',(6.3385795111461,-28.8272026413545,53.3113398343453));
#85189=CARTESIAN_POINT('Ctrl Pts',(6.34244858449431,-28.7694692515091,53.352924986983));
#85190=CARTESIAN_POINT('Ctrl Pts',(6.34631765784252,-28.7139664634267,53.3974659737439));
#85191=CARTESIAN_POINT('Ctrl Pts',(6.35018096623831,-28.6585463749739,53.441940594053));
#85192=CARTESIAN_POINT('Ctrl Pts',(6.35404427463409,-28.6053506667861,53.4893620046678));
#85193=CARTESIAN_POINT('Ctrl Pts',(6.35790758302988,-28.5547069996109,53.53947759157));
#85194=CARTESIAN_POINT('Ctrl Pts',(6.36176635952279,-28.5041227406313,53.5895343897478));
#85195=CARTESIAN_POINT('Ctrl Pts',(6.3656251360157,-28.4560849197777,53.6422787464759));
#85196=CARTESIAN_POINT('Ctrl Pts',(6.36948391250861,-28.4108873442306,53.6974185131926));
#85197=CARTESIAN_POINT('Ctrl Pts',(6.37334025809681,-28.365718241698,53.752523543635));
#85198=CARTESIAN_POINT('Ctrl Pts',(6.37719660368501,-28.3233861418328,53.8100206153616));
#85199=CARTESIAN_POINT('Ctrl Pts',(6.38105294927322,-28.2841462414807,53.8695826249233));
#85200=CARTESIAN_POINT('Ctrl Pts',(6.38490815551855,-28.2449179344104,53.9291270371122));
#85201=CARTESIAN_POINT('Ctrl Pts',(6.38876336176388,-28.2087802802552,53.9907347705192));
#85202=CARTESIAN_POINT('Ctrl Pts',(6.39261856800921,-28.1759455838436,54.0540491294996));
#85203=CARTESIAN_POINT('Ctrl Pts',(6.39647392486045,-28.1431096047252,54.1173659618929));
#85204=CARTESIAN_POINT('Ctrl Pts',(6.4003292817117,-28.1135770612139,54.1823891199659));
#85205=CARTESIAN_POINT('Ctrl Pts',(6.40418463856294,-28.0875138476605,54.248738208339));
#85206=CARTESIAN_POINT('Ctrl Pts',(6.40804403103149,-28.0614233522861,54.315156748008));
#85207=CARTESIAN_POINT('Ctrl Pts',(6.41190342350005,-28.0388096142203,54.3829035355095));
#85208=CARTESIAN_POINT('Ctrl Pts',(6.4157628159686,-28.0197896463723,54.4515799804112));
#85209=CARTESIAN_POINT('Ctrl Pts',(6.41962439357204,-28.0007589096804,54.5202953089704));
#85210=CARTESIAN_POINT('Ctrl Pts',(6.42348597117547,-27.9853260988985,54.5899408682425));
#85211=CARTESIAN_POINT('Ctrl Pts',(6.42734754877891,-27.9735571523901,54.6601074465793));
#85212=CARTESIAN_POINT('Ctrl Pts',(6.43121588289378,-27.9617676140331,54.7303967937266));
#85213=CARTESIAN_POINT('Ctrl Pts',(6.43508421700865,-27.9536547941648,54.8012084972218));
#85214=CARTESIAN_POINT('Ctrl Pts',(6.43895255112351,-27.9492327191636,54.8721284928109));
#85215=CARTESIAN_POINT('Ctrl Pts',(6.44125027029449,-27.9466060881116,54.9142536631379));
#85216=CARTESIAN_POINT('Ctrl Pts',(6.44354798946547,-27.9452806044252,54.9564170246933));
#85217=CARTESIAN_POINT('Ctrl Pts',(6.44584570863644,-27.9452505240975,54.9985324242889));
#85218=CARTESIAN_POINT('Ctrl Pts',(6.44587223260258,-27.9452501768621,54.9990185878926));
#85219=CARTESIAN_POINT('Ctrl Pts',(6.44589875656871,-27.9452500021695,54.9995047516196));
#85220=CARTESIAN_POINT('Ctrl Pts',(6.44592528053485,-27.9452500000201,54.999990915392));
#85221=CARTESIAN_POINT('Origin',(-1.54592528053767,-30.,55.));
#85222=CARTESIAN_POINT('',(5.29388070614408,-31.2520475724682,56.6292251037768));
#85223=CARTESIAN_POINT('',(5.35213793236373,-31.2520475724682,56.6292251037768));
#85224=CARTESIAN_POINT('',(-1.54592528053767,-31.2520475724682,56.6292251037768));
#85225=CARTESIAN_POINT('',(5.80407471943462,-27.9452508587686,54.9981214077886));
#85226=CARTESIAN_POINT('Ctrl Pts',(5.35213793236373,-31.2520475724682,56.6292251037768));
#85227=CARTESIAN_POINT('Ctrl Pts',(5.35599766139006,-31.3084496151558,56.5858805466216));
#85228=CARTESIAN_POINT('Ctrl Pts',(5.35985739041638,-31.362668650072,56.5395495461331));
#85229=CARTESIAN_POINT('Ctrl Pts',(5.3637171194427,-31.4143753267133,56.4904831423685));
#85230=CARTESIAN_POINT('Ctrl Pts',(5.36757404042557,-31.466044385534,56.441452435564));
#85231=CARTESIAN_POINT('Ctrl Pts',(5.37143096140844,-31.5152043607371,56.3896906066652));
#85232=CARTESIAN_POINT('Ctrl Pts',(5.37528788239131,-31.5615595250372,56.335488454561));
#85233=CARTESIAN_POINT('Ctrl Pts',(5.3791432876086,-31.6078964718101,56.2813076038413));
#85234=CARTESIAN_POINT('Ctrl Pts',(5.38299869282588,-31.6514304799869,56.2246887021999));
#85235=CARTESIAN_POINT('Ctrl Pts',(5.38685409804317,-31.6919044054673,56.165957565806));
#85236=CARTESIAN_POINT('Ctrl Pts',(5.39070927778001,-31.7323759638609,56.1072298642581));
#85237=CARTESIAN_POINT('Ctrl Pts',(5.39456445751685,-31.7697875205517,56.0463905741253));
#85238=CARTESIAN_POINT('Ctrl Pts',(5.39841963725369,-31.8039247894515,55.9837951598288));
#85239=CARTESIAN_POINT('Ctrl Pts',(5.40227861106393,-31.8380956545289,55.9211381422837));
#85240=CARTESIAN_POINT('Ctrl Pts',(5.40613758487416,-31.8689855617635,55.8567219757467));
#85241=CARTESIAN_POINT('Ctrl Pts',(5.40999655868439,-31.8964262535003,55.7909266891026));
#85242=CARTESIAN_POINT('Ctrl Pts',(5.41385737981818,-31.9238800813295,55.7250999056955));
#85243=CARTESIAN_POINT('Ctrl Pts',(5.41771820095197,-31.9478812405932,55.6578931451431));
#85244=CARTESIAN_POINT('Ctrl Pts',(5.42157902208576,-31.9683107067605,55.5897037596555));
#85245=CARTESIAN_POINT('Ctrl Pts',(5.42544695749405,-31.9887778179845,55.5213887226577));
#85246=CARTESIAN_POINT('Ctrl Pts',(5.42931489290235,-32.0056599709901,55.452087916219));
#85247=CARTESIAN_POINT('Ctrl Pts',(5.43318282831064,-32.0188889506662,55.3822106322144));
#85248=CARTESIAN_POINT('Ctrl Pts',(5.43660651741345,-32.0305985344048,55.3203590058229));
#85249=CARTESIAN_POINT('Ctrl Pts',(5.44003020651626,-32.0394466489614,55.2580560764145));
#85250=CARTESIAN_POINT('Ctrl Pts',(5.44345389561907,-32.0454200326909,55.1955874545234));
#85251=CARTESIAN_POINT('Ctrl Pts',(5.44732296896728,-32.0521704878556,55.1249923529236));
#85252=CARTESIAN_POINT('Ctrl Pts',(5.4511920423155,-32.0552751231039,55.0539090886279));
#85253=CARTESIAN_POINT('Ctrl Pts',(5.45506111566371,-32.0546775616078,54.9827465851108));
#85254=CARTESIAN_POINT('Ctrl Pts',(5.4589244240595,-32.0540808904835,54.9116901143335));
#85255=CARTESIAN_POINT('Ctrl Pts',(5.46278773245529,-32.0497929763707,54.8405551205058));
#85256=CARTESIAN_POINT('Ctrl Pts',(5.46665104085107,-32.0418092335022,54.7697553117114));
#85257=CARTESIAN_POINT('Ctrl Pts',(5.47050981734399,-32.0338348560645,54.69903855553));
#85258=CARTESIAN_POINT('Ctrl Pts',(5.4743685938369,-32.0221733156894,54.6286566837511));
#85259=CARTESIAN_POINT('Ctrl Pts',(5.47822737032981,-32.0068720328791,54.5590213087375));
#85260=CARTESIAN_POINT('Ctrl Pts',(5.48208371591802,-31.9915803893835,54.4894298017639));
#85261=CARTESIAN_POINT('Ctrl Pts',(5.48594006150623,-31.9726536565796,54.4205843318947));
#85262=CARTESIAN_POINT('Ctrl Pts',(5.48979640709443,-31.9501906114715,54.3528878447839));
#85263=CARTESIAN_POINT('Ctrl Pts',(5.49365161333977,-31.927734202986,54.2852113583468));
#85264=CARTESIAN_POINT('Ctrl Pts',(5.4975068195851,-31.9017437093017,54.2186836415556));
#85265=CARTESIAN_POINT('Ctrl Pts',(5.50136202583043,-31.8723677051339,54.1536922904336));
#85266=CARTESIAN_POINT('Ctrl Pts',(5.50521738268168,-31.8429905533751,54.0886984003859));
#85267=CARTESIAN_POINT('Ctrl Pts',(5.50907273953293,-31.8102278306458,54.025241436927));
#85268=CARTESIAN_POINT('Ctrl Pts',(5.51292809638417,-31.7742754619635,53.9636872346756));
#85269=CARTESIAN_POINT('Ctrl Pts',(5.51678748885273,-31.7382854599292,53.9020686002033));
#85270=CARTESIAN_POINT('Ctrl Pts',(5.52064688132129,-31.6990993924937,53.8423571232074));
#85271=CARTESIAN_POINT('Ctrl Pts',(5.52450627378985,-31.6569577433031,53.7848915277195));
#85272=CARTESIAN_POINT('Ctrl Pts',(5.52836785139329,-31.614792234091,53.7273933960027));
#85273=CARTESIAN_POINT('Ctrl Pts',(5.53222942899673,-31.5696681193188,53.6721440535542));
#85274=CARTESIAN_POINT('Ctrl Pts',(5.53609100660016,-31.5218658529192,53.6194487013448));
#85275=CARTESIAN_POINT('Ctrl Pts',(5.53995934071503,-31.4739799480193,53.5666611493181));
#85276=CARTESIAN_POINT('Ctrl Pts',(5.54382767482991,-31.4234068807573,53.5164368517537));
#85277=CARTESIAN_POINT('Ctrl Pts',(5.54769600894478,-31.3704630647951,53.469043256479));
#85278=CARTESIAN_POINT('Ctrl Pts',(5.54999372811573,-31.3390154138666,53.4408923343485));
#85279=CARTESIAN_POINT('Ctrl Pts',(5.55229144728667,-31.3067319607144,53.4137393489292));
#85280=CARTESIAN_POINT('Ctrl Pts',(5.55458916645762,-31.2736839053951,53.3876331460745));
#85281=CARTESIAN_POINT('Ctrl Pts',(5.55845823980584,-31.2180350899685,53.3436735469358));
#85282=CARTESIAN_POINT('Ctrl Pts',(5.56232731315406,-31.1599987860129,53.3025121980011));
#85283=CARTESIAN_POINT('Ctrl Pts',(5.56619638650227,-31.0998879711845,53.2644182493055));
#85284=CARTESIAN_POINT('Ctrl Pts',(5.57005969489806,-31.039866721985,53.2263810609198));
#85285=CARTESIAN_POINT('Ctrl Pts',(5.57392300329384,-30.977777504523,53.1914024584711));
#85286=CARTESIAN_POINT('Ctrl Pts',(5.57778631168963,-30.9139654058247,53.1597106750688));
#85287=CARTESIAN_POINT('Ctrl Pts',(5.58164508818254,-30.8502281627174,53.1280560681146));
#85288=CARTESIAN_POINT('Ctrl Pts',(5.58550386467545,-30.7847724858293,53.099680836624));
#85289=CARTESIAN_POINT('Ctrl Pts',(5.58936264116837,-30.7179699078131,53.0747683843301));
#85290=CARTESIAN_POINT('Ctrl Pts',(5.59321898675657,-30.6512094132659,53.0498716260775));
#85291=CARTESIAN_POINT('Ctrl Pts',(5.59707533234478,-30.5831041550984,53.0284334884236));
#85292=CARTESIAN_POINT('Ctrl Pts',(5.60093167793299,-30.5140462386054,53.0105895277556));
#85293=CARTESIAN_POINT('Ctrl Pts',(5.60478688417832,-30.4450087250154,52.9927508390191));
#85294=CARTESIAN_POINT('Ctrl Pts',(5.60864209042365,-30.3750195819568,52.9785043405957));
#85295=CARTESIAN_POINT('Ctrl Pts',(5.61249729666899,-30.3044850273214,52.9679354265582));
#85296=CARTESIAN_POINT('Ctrl Pts',(5.61635265352023,-30.2339477172119,52.9573660996399));
#85297=CARTESIAN_POINT('Ctrl Pts',(5.62020801037148,-30.1628654339729,52.9504747121478));
#85298=CARTESIAN_POINT('Ctrl Pts',(5.62406336722272,-30.0916517938954,52.9472950744991));
#85299=CARTESIAN_POINT('Ctrl Pts',(5.62792275969128,-30.0203636105239,52.944112108546));
#85300=CARTESIAN_POINT('Ctrl Pts',(5.63178215215984,-29.948944282133,52.9446486700726));
#85301=CARTESIAN_POINT('Ctrl Pts',(5.6356415446284,-29.8778088152285,52.9488864300424));
#85302=CARTESIAN_POINT('Ctrl Pts',(5.63950312223184,-29.8066330724021,52.9531265893736));
#85303=CARTESIAN_POINT('Ctrl Pts',(5.64336469983527,-29.7357419939951,52.9610720646429));
#85304=CARTESIAN_POINT('Ctrl Pts',(5.64722627743871,-29.6655441007778,52.9726527643308));
#85305=CARTESIAN_POINT('Ctrl Pts',(5.65109461155358,-29.5952233839591,52.9842537264964));
#85306=CARTESIAN_POINT('Ctrl Pts',(5.65496294566845,-29.5255987485088,52.9995025079733));
#85307=CARTESIAN_POINT('Ctrl Pts',(5.65883127978332,-29.4570665004026,53.0182783299578));
#85308=CARTESIAN_POINT('Ctrl Pts',(5.66112899895428,-29.4163596080747,53.0294308221788));
#85309=CARTESIAN_POINT('Ctrl Pts',(5.66342671812523,-29.3760378167379,53.0418267532859));
#85310=CARTESIAN_POINT('Ctrl Pts',(5.66572443729619,-29.3361807802747,53.0554327972468));
#85311=CARTESIAN_POINT('Ctrl Pts',(5.66959351064441,-29.2690664873413,53.0783436832807));
#85312=CARTESIAN_POINT('Ctrl Pts',(5.67346258399262,-29.2030082382591,53.1047780728359));
#85313=CARTESIAN_POINT('Ctrl Pts',(5.67733165734084,-29.1384019055368,53.1346189970632));
#85314=CARTESIAN_POINT('Ctrl Pts',(5.68119496573662,-29.0738918368037,53.1644154580578));
#85315=CARTESIAN_POINT('Ctrl Pts',(5.68505827413241,-29.0108298276283,53.1976081764318));
#85316=CARTESIAN_POINT('Ctrl Pts',(5.68892158252819,-28.9495947893964,53.2340310149845));
#85317=CARTESIAN_POINT('Ctrl Pts',(5.69278035902111,-28.888431583702,53.2704111272649));
#85318=CARTESIAN_POINT('Ctrl Pts',(5.69663913551402,-28.8290915074133,53.310013586091));
#85319=CARTESIAN_POINT('Ctrl Pts',(5.70049791200693,-28.7719301519625,53.3526257222959));
#85320=CARTESIAN_POINT('Ctrl Pts',(5.70435425759514,-28.7148048063217,53.3952110142296));
#85321=CARTESIAN_POINT('Ctrl Pts',(5.70821060318334,-28.6598558470069,53.4408019322546));
#85322=CARTESIAN_POINT('Ctrl Pts',(5.71206694877155,-28.6074098246734,53.489142572549));
#85323=CARTESIAN_POINT('Ctrl Pts',(5.71592215501688,-28.554979297321,53.5374689307821));
#85324=CARTESIAN_POINT('Ctrl Pts',(5.71977736126222,-28.5050505958746,53.5885430693972));
#85325=CARTESIAN_POINT('Ctrl Pts',(5.72363256750755,-28.4579157816097,53.6420700217273));
#85326=CARTESIAN_POINT('Ctrl Pts',(5.7274879243588,-28.4107791259953,53.6955990651196));
#85327=CARTESIAN_POINT('Ctrl Pts',(5.73134328121005,-28.3664368936453,53.7515807464295));
#85328=CARTESIAN_POINT('Ctrl Pts',(5.7351986380613,-28.3251418207853,53.8096859061502));
#85329=CARTESIAN_POINT('Ctrl Pts',(5.73905803052986,-28.2838035220665,53.8678518877862));
#85330=CARTESIAN_POINT('Ctrl Pts',(5.74291742299841,-28.2455190320516,53.9281453881854));
#85331=CARTESIAN_POINT('Ctrl Pts',(5.74677681546697,-28.210498036343,53.9902078012939));
#85332=CARTESIAN_POINT('Ctrl Pts',(5.75063839307041,-28.1754572122287,54.0523053532862));
#85333=CARTESIAN_POINT('Ctrl Pts',(5.75449997067384,-28.1436837771895,54.1161733765903));
#85334=CARTESIAN_POINT('Ctrl Pts',(5.75836154827728,-28.1153404112806,54.1814306399896));
#85335=CARTESIAN_POINT('Ctrl Pts',(5.76222988239215,-28.0869474536515,54.2468020824865));
#85336=CARTESIAN_POINT('Ctrl Pts',(5.76609821650702,-28.061996717454,54.3135671628903));
#85337=CARTESIAN_POINT('Ctrl Pts',(5.76996655062189,-28.0406016732822,54.3813274212027));
#85338=CARTESIAN_POINT('Ctrl Pts',(5.77226426979284,-28.0278934113543,54.4215757658208));
#85339=CARTESIAN_POINT('Ctrl Pts',(5.77456198896379,-28.0164386815437,54.4621749669161));
#85340=CARTESIAN_POINT('Ctrl Pts',(5.77685970813473,-28.0062526866041,54.5030400289492));
#85341=CARTESIAN_POINT('Ctrl Pts',(5.78191177765104,-27.9838564098189,54.5928913636073));
#85342=CARTESIAN_POINT('Ctrl Pts',(5.78696384716734,-27.9675248955209,54.6843103064913));
#85343=CARTESIAN_POINT('Ctrl Pts',(5.79201591668364,-27.9574316008769,54.7765902925033));
#85344=CARTESIAN_POINT('Ctrl Pts',(5.79603551760063,-27.9494010272129,54.8500114351059));
#85345=CARTESIAN_POINT('Ctrl Pts',(5.80005511851763,-27.9453186462865,54.9239774059998));
#85346=CARTESIAN_POINT('Ctrl Pts',(5.80407471943462,-27.9452508587686,54.9981214077886));
#85347=CARTESIAN_POINT('Ctrl Pts',(5.80407471946232,-27.9452508587681,54.9981214082995));
#85348=CARTESIAN_POINT('Ctrl Pts',(5.80788808427066,-27.9451865492831,55.0684612587007));
#85349=CARTESIAN_POINT('Ctrl Pts',(5.81170144907901,-27.9487383877838,55.1388965966684));
#85350=CARTESIAN_POINT('Ctrl Pts',(5.81551481388735,-27.9559090953207,55.209021376676));
#85351=CARTESIAN_POINT('Ctrl Pts',(5.81932566294071,-27.9630750721948,55.2790998939277));
#85352=CARTESIAN_POINT('Ctrl Pts',(5.82313651199406,-27.9738551346034,55.3488677648099));
#85353=CARTESIAN_POINT('Ctrl Pts',(5.82694736104741,-27.9881999804144,55.4179213367314));
#85354=CARTESIAN_POINT('Ctrl Pts',(5.8307570439826,-28.0025404367088,55.4869537782898));
#85355=CARTESIAN_POINT('Ctrl Pts',(5.83456672691779,-28.0204434107704,55.5552718667557));
#85356=CARTESIAN_POINT('Ctrl Pts',(5.83837640985297,-28.0418083477083,55.622481337387));
#85357=CARTESIAN_POINT('Ctrl Pts',(5.8421862745413,-28.0631743039291,55.6896940144616));
#85358=CARTESIAN_POINT('Ctrl Pts',(5.84599613922963,-28.0880023967574,55.7557974946326));
#85359=CARTESIAN_POINT('Ctrl Pts',(5.84980600391796,-28.1161425514219,55.8204137224211));
#85360=CARTESIAN_POINT('Ctrl Pts',(5.85361981396671,-28.1443118470301,55.8850968644778));
#85361=CARTESIAN_POINT('Ctrl Pts',(5.85743362401546,-28.1757998467947,55.9482892241738));
#85362=CARTESIAN_POINT('Ctrl Pts',(5.8612474340642,-28.2104092282856,56.0096348014479));
#85363=CARTESIAN_POINT('Ctrl Pts',(5.86506356527384,-28.2450396737366,56.0710177148643));
#85364=CARTESIAN_POINT('Ctrl Pts',(5.86887969648348,-28.2827950106825,56.1305511908721));
#85365=CARTESIAN_POINT('Ctrl Pts',(5.87269582769311,-28.3234345959172,56.1879082491222));
#85366=CARTESIAN_POINT('Ctrl Pts',(5.87651830066247,-28.3641417172167,56.2453606250284));
#85367=CARTESIAN_POINT('Ctrl Pts',(5.88034077363183,-28.4077423369056,56.3006289805386));
#85368=CARTESIAN_POINT('Ctrl Pts',(5.88416324660119,-28.453956286233,56.3534202590554));
#85369=CARTESIAN_POINT('Ctrl Pts',(5.88544049072523,-28.4693982516047,56.371059978375));
#85370=CARTESIAN_POINT('Ctrl Pts',(5.88671773484926,-28.4851317023626,56.3884234488368));
#85371=CARTESIAN_POINT('Ctrl Pts',(5.8879949789733,-28.5011453432884,56.4055007223598));
#85372=CARTESIAN_POINT('Ctrl Pts',(5.89186405232151,-28.5496544341879,56.4572318069697));
#85373=CARTESIAN_POINT('Ctrl Pts',(5.89573312566972,-28.6009398356743,56.5065499255198));
#85374=CARTESIAN_POINT('Ctrl Pts',(5.89960219901794,-28.6547319770887,56.5531424625682));
#85375=CARTESIAN_POINT('Ctrl Pts',(5.90346550741372,-28.7084439677517,56.5996655763374));
#85376=CARTESIAN_POINT('Ctrl Pts',(5.90732881580951,-28.7646549201418,56.6434708543949));
#85377=CARTESIAN_POINT('Ctrl Pts',(5.9111921242053,-28.8230574377306,56.6842813801793));
#85378=CARTESIAN_POINT('Ctrl Pts',(5.91505090069821,-28.881391445506,56.7250440326592));
#85379=CARTESIAN_POINT('Ctrl Pts',(5.91890967719112,-28.9419115156489,56.7628186340326));
#85380=CARTESIAN_POINT('Ctrl Pts',(5.92276845368403,-29.0042774461901,56.7973686762415));
#85381=CARTESIAN_POINT('Ctrl Pts',(5.92662479927223,-29.0666040882069,56.8318969530385));
#85382=CARTESIAN_POINT('Ctrl Pts',(5.93048114486044,-29.1307738596501,56.8632044660195));
#85383=CARTESIAN_POINT('Ctrl Pts',(5.93433749044864,-29.1964191132021,56.8910989717286));
#85384=CARTESIAN_POINT('Ctrl Pts',(5.93819269669397,-29.2620449721096,56.9189852361104));
#85385=CARTESIAN_POINT('Ctrl Pts',(5.9420479029393,-29.3291450008409,56.9434603052146));
#85386=CARTESIAN_POINT('Ctrl Pts',(5.94590310918463,-29.3973301517084,56.9643794481872));
#85387=CARTESIAN_POINT('Ctrl Pts',(5.94975846603587,-29.4655179662692,56.9852994083785));
#85388=CARTESIAN_POINT('Ctrl Pts',(5.95361382288712,-29.5347905220613,57.002663026264));
#85389=CARTESIAN_POINT('Ctrl Pts',(5.95746917973836,-29.6047437999568,57.0163754855749));
#85390=CARTESIAN_POINT('Ctrl Pts',(5.96132857220692,-29.6747703018546,57.0301022984827));
#85391=CARTESIAN_POINT('Ctrl Pts',(5.96518796467547,-29.7454784705751,57.0401702298633));
#85392=CARTESIAN_POINT('Ctrl Pts',(5.96904735714403,-29.8164551747293,57.046535819285));
#85393=CARTESIAN_POINT('Ctrl Pts',(5.97290893474746,-29.8874720649161,57.0529050128157));
#85394=CARTESIAN_POINT('Ctrl Pts',(5.9767705123509,-29.9587573075259,57.0555676733289));
#85395=CARTESIAN_POINT('Ctrl Pts',(5.98063208995433,-30.0298965035958,57.0545324922164));
#85396=CARTESIAN_POINT('Ctrl Pts',(5.9845004240692,-30.1011601702425,57.0534954998718));
#85397=CARTESIAN_POINT('Ctrl Pts',(5.98836875818407,-30.1722767953068,57.0487477806749));
#85398=CARTESIAN_POINT('Ctrl Pts',(5.99223709229894,-30.2428365374342,57.0403499647332));
#85399=CARTESIAN_POINT('Ctrl Pts',(5.99453481146991,-30.2847477238444,57.0353618168353));
#85400=CARTESIAN_POINT('Ctrl Pts',(5.99683253064089,-30.3264625982631,57.0290868493545));
#85401=CARTESIAN_POINT('Ctrl Pts',(5.99913024981186,-30.3678974432214,57.0215461987724));
#85402=CARTESIAN_POINT('Ctrl Pts',(6.00299944641651,-30.437670792137,57.0088482764164));
#85403=CARTESIAN_POINT('Ctrl Pts',(6.00686864302115,-30.5069226410627,56.9925089162004));
#85404=CARTESIAN_POINT('Ctrl Pts',(6.0107378396258,-30.5752441037058,56.9725850510565));
#85405=CARTESIAN_POINT('Ctrl Pts',(6.01460043061989,-30.6434489258622,56.9526952005435));
#85406=CARTESIAN_POINT('Ctrl Pts',(6.01846302161398,-30.7107260550316,56.9292331382206));
#85407=CARTESIAN_POINT('Ctrl Pts',(6.02232561260807,-30.7766763424025,56.9023068684238));
#85408=CARTESIAN_POINT('Ctrl Pts',(6.02618437399535,-30.8425612426614,56.8754072949627));
#85409=CARTESIAN_POINT('Ctrl Pts',(6.03004313538263,-30.9071214635225,56.8450505102865));
#85410=CARTESIAN_POINT('Ctrl Pts',(6.03390189676991,-30.9699737925889,56.811394049949));
#85411=CARTESIAN_POINT('Ctrl Pts',(6.03775817547521,-31.0327856832016,56.7777592437847));
#85412=CARTESIAN_POINT('Ctrl Pts',(6.04161445418052,-31.0938914352708,56.7408292034246));
#85413=CARTESIAN_POINT('Ctrl Pts',(6.04547073288583,-31.1529301526205,56.7008085211682));
#85414=CARTESIAN_POINT('Ctrl Pts',(6.04767420911889,-31.1866648539873,56.677940718055));
#85415=CARTESIAN_POINT('Ctrl Pts',(6.04987768535195,-31.2197251064094,56.6540646824644));
#85416=CARTESIAN_POINT('Ctrl Pts',(6.05208116158501,-31.2520475724682,56.6292251037768));
#85417=CARTESIAN_POINT('',(5.74592528057396,-27.9452507587439,55.0017658022555));
#85418=CARTESIAN_POINT('Ctrl Pts',(5.74592528057397,-27.9452507587439,55.0017658022555));
#85419=CARTESIAN_POINT('Ctrl Pts',(5.75057817989358,-27.9453246481722,55.0877461243749));
#85420=CARTESIAN_POINT('Ctrl Pts',(5.75523107921319,-27.9507990871283,55.1734909003221));
#85421=CARTESIAN_POINT('Ctrl Pts',(5.75988397853281,-27.9615629769875,55.2584029135126));
#85422=CARTESIAN_POINT('Ctrl Pts',(5.76460377517754,-27.9724816252865,55.3445357540116));
#85423=CARTESIAN_POINT('Ctrl Pts',(5.76932357182228,-27.9888428428115,55.4298117229022));
#85424=CARTESIAN_POINT('Ctrl Pts',(5.77404336846702,-28.0104818888369,55.5136294849929));
#85425=CARTESIAN_POINT('Ctrl Pts',(5.77570694017971,-28.0181089345694,55.5431724650257));
#85426=CARTESIAN_POINT('Ctrl Pts',(5.7773705118924,-28.0263912273234,55.5725344843005));
#85427=CARTESIAN_POINT('Ctrl Pts',(5.77903408360509,-28.0353201550615,55.6016898448475));
#85428=CARTESIAN_POINT('Ctrl Pts',(5.7829031569533,-28.0560867238101,55.6694983003469));
#85429=CARTESIAN_POINT('Ctrl Pts',(5.78677223030152,-28.080408575338,55.7363632146234));
#85430=CARTESIAN_POINT('Ctrl Pts',(5.79064130364973,-28.1081813798379,55.8018851980852));
#85431=CARTESIAN_POINT('Ctrl Pts',(5.79450461204551,-28.1359128026213,55.8673095532304));
#85432=CARTESIAN_POINT('Ctrl Pts',(5.7983679204413,-28.1670847837136,55.9313945058252));
#85433=CARTESIAN_POINT('Ctrl Pts',(5.80223122883708,-28.2015433108007,55.9937560563711));
#85434=CARTESIAN_POINT('Ctrl Pts',(5.80609000532999,-28.2359614158759,56.0560444529099));
#85435=CARTESIAN_POINT('Ctrl Pts',(5.80994878182291,-28.2736581751631,56.1166130399684));
#85436=CARTESIAN_POINT('Ctrl Pts',(5.81380755831582,-28.314432326825,56.1750996475394));
#85437=CARTESIAN_POINT('Ctrl Pts',(5.81766390390403,-28.3551807920867,56.2335494104344));
#85438=CARTESIAN_POINT('Ctrl Pts',(5.82152024949223,-28.3990025262958,56.2899193984337));
#85439=CARTESIAN_POINT('Ctrl Pts',(5.82537659508044,-28.4456521319429,56.3438750937368));
#85440=CARTESIAN_POINT('Ctrl Pts',(5.82923180132577,-28.4922879551384,56.3978148480317));
#85441=CARTESIAN_POINT('Ctrl Pts',(5.8330870075711,-28.5417496735576,56.4493413584357));
#85442=CARTESIAN_POINT('Ctrl Pts',(5.83694221381643,-28.5937517505766,56.4981533377774));
#85443=CARTESIAN_POINT('Ctrl Pts',(5.84079757066768,-28.6457558590875,56.546967223988));
#85444=CARTESIAN_POINT('Ctrl Pts',(5.84465292751893,-28.7003001675251,56.5930660377377));
#85445=CARTESIAN_POINT('Ctrl Pts',(5.84850828437018,-28.7570637140299,56.63618671047));
#85446=CARTESIAN_POINT('Ctrl Pts',(5.85236767683874,-28.8138866781086,56.6793525200184));
#85447=CARTESIAN_POINT('Ctrl Pts',(5.8562270693073,-28.8729331298637,56.7195336710872));
#85448=CARTESIAN_POINT('Ctrl Pts',(5.86008646177586,-28.9338513077055,56.7565091882535));
#85449=CARTESIAN_POINT('Ctrl Pts',(5.86394803937929,-28.9948039765808,56.7935056404484));
#85450=CARTESIAN_POINT('Ctrl Pts',(5.86780961698273,-29.0576300531253,56.8272926154683));
#85451=CARTESIAN_POINT('Ctrl Pts',(5.87167119458616,-29.1219536682789,56.8576954007186));
#85452=CARTESIAN_POINT('Ctrl Pts',(5.87553952870103,-29.1863898289479,56.8881513810067));
#85453=CARTESIAN_POINT('Ctrl Pts',(5.87940786281591,-29.2523283099901,56.9152111651145));
#85454=CARTESIAN_POINT('Ctrl Pts',(5.88327619693078,-29.3193744584956,56.9387486775629));
#85455=CARTESIAN_POINT('Ctrl Pts',(5.88557391610173,-29.3591986350495,56.9527295261616));
#85456=CARTESIAN_POINT('Ctrl Pts',(5.88787163527269,-29.3994133254085,56.9654686251861));
#85457=CARTESIAN_POINT('Ctrl Pts',(5.89016935444365,-29.4399340600699,56.9769480785873));
#85458=CARTESIAN_POINT('Ctrl Pts',(5.89403860384479,-29.5081690429625,56.9962789301377));
#85459=CARTESIAN_POINT('Ctrl Pts',(5.89790785324593,-29.5775396769516,57.0121107721141));
#85460=CARTESIAN_POINT('Ctrl Pts',(5.90177710264707,-29.6476537787499,57.0243146254648));
#85461=CARTESIAN_POINT('Ctrl Pts',(5.90563962090613,-29.7176459065084,57.0364972483747));
#85462=CARTESIAN_POINT('Ctrl Pts',(5.9095021391652,-29.788378457524,57.0450643409053));
#85463=CARTESIAN_POINT('Ctrl Pts',(5.91336465742426,-29.8594455361168,57.049937073469));
#85464=CARTESIAN_POINT('Ctrl Pts',(5.91722337851854,-29.9304427500797,57.0548050157463));
#85465=CARTESIAN_POINT('Ctrl Pts',(5.92108209961282,-30.001773357262,57.0559857693842));
#85466=CARTESIAN_POINT('Ctrl Pts',(5.92494082070709,-30.0730239443259,57.0534519877648));
#85467=CARTESIAN_POINT('Ctrl Pts',(5.9287970392771,-30.1442283227317,57.0509198493971));
#85468=CARTESIAN_POINT('Ctrl Pts',(5.9326532578471,-30.2153522997328,57.044677973616));
#85469=CARTESIAN_POINT('Ctrl Pts',(5.93650947641711,-30.2859817780574,57.0347510867718));
#85470=CARTESIAN_POINT('Ctrl Pts',(5.94036448407723,-30.3565890776771,57.0248273171175));
#85471=CARTESIAN_POINT('Ctrl Pts',(5.94421949173735,-30.426701706356,57.0112209023426));
#85472=CARTESIAN_POINT('Ctrl Pts',(5.94807449939747,-30.4959117356517,56.9940083031279));
#85473=CARTESIAN_POINT('Ctrl Pts',(5.95193183773627,-30.5651636082728,56.9767852974389));
#85474=CARTESIAN_POINT('Ctrl Pts',(5.95578917607507,-30.6335113173793,56.9559518624058));
#85475=CARTESIAN_POINT('Ctrl Pts',(5.95964651441388,-30.7005591600954,56.9316351688935));
#85476=CARTESIAN_POINT('Ctrl Pts',(5.96350485094006,-30.7676243531979,56.9073121827996));
#85477=CARTESIAN_POINT('Ctrl Pts',(5.96736318746624,-30.8333885587031,56.8795043250434));
#85478=CARTESIAN_POINT('Ctrl Pts',(5.97122152399242,-30.8974756542452,56.8483871381659));
#85479=CARTESIAN_POINT('Ctrl Pts',(5.97508578920568,-30.9616612254731,56.8172221368838));
#85480=CARTESIAN_POINT('Ctrl Pts',(5.97895005441895,-31.0241641074325,56.7827378750177));
#85481=CARTESIAN_POINT('Ctrl Pts',(5.98281431963221,-31.0846329359057,56.7451558546012));
#85482=CARTESIAN_POINT('Ctrl Pts',(5.98650504906563,-31.1423862402814,56.7092615613103));
#85483=CARTESIAN_POINT('Ctrl Pts',(5.99019577849905,-31.1982839789842,56.6705420320225));
#85484=CARTESIAN_POINT('Ctrl Pts',(5.99388650793247,-31.2520475724682,56.6292251037768));
#85485=CARTESIAN_POINT('Ctrl Pts',(5.29388070614408,-31.2520475724682,56.6292251037768));
#85486=CARTESIAN_POINT('Ctrl Pts',(5.29774024882555,-31.3086258322378,56.5857451250834));
#85487=CARTESIAN_POINT('Ctrl Pts',(5.30159979150703,-31.3629068090275,56.5393373691093));
#85488=CARTESIAN_POINT('Ctrl Pts',(5.3054593341885,-31.4145854558055,56.4902837148421));
#85489=CARTESIAN_POINT('Ctrl Pts',(5.30932116705353,-31.4662947677677,56.4412009530143));
#85490=CARTESIAN_POINT('Ctrl Pts',(5.31318299991856,-31.5153983418367,56.3894695204074));
#85491=CARTESIAN_POINT('Ctrl Pts',(5.31704483278359,-31.5616295181324,56.3354066087143));
#85492=CARTESIAN_POINT('Ctrl Pts',(5.3209133155756,-31.6079403027274,56.281250602776));
#85493=CARTESIAN_POINT('Ctrl Pts',(5.32478179836762,-31.6513685208432,56.2247554891651));
#85494=CARTESIAN_POINT('Ctrl Pts',(5.32865028115963,-31.6916896102803,56.1662691906115));
#85495=CARTESIAN_POINT('Ctrl Pts',(5.33059785419004,-31.7119891102565,56.1368244848094));
#85496=CARTESIAN_POINT('Ctrl Pts',(5.33254542722045,-31.7315017941742,56.1068755173923));
#85497=CARTESIAN_POINT('Ctrl Pts',(5.33449300025085,-31.7502034628656,56.0764689503526));
#85498=CARTESIAN_POINT('Ctrl Pts',(5.33836207359907,-31.7873564357047,56.0160628776113));
#85499=CARTESIAN_POINT('Ctrl Pts',(5.34223114694728,-31.8214512506892,55.9536127950323));
#85500=CARTESIAN_POINT('Ctrl Pts',(5.34610022029549,-31.852257189563,55.8894609975778));
#85501=CARTESIAN_POINT('Ctrl Pts',(5.34996352869128,-31.8830172273241,55.8254047868509));
#85502=CARTESIAN_POINT('Ctrl Pts',(5.35382683708707,-31.9104979076634,55.7596523286277));
#85503=CARTESIAN_POINT('Ctrl Pts',(5.35769014548285,-31.9345129022427,55.6925730239886));
#85504=CARTESIAN_POINT('Ctrl Pts',(5.36154892197577,-31.9584997257282,55.6255724075779));
#85505=CARTESIAN_POINT('Ctrl Pts',(5.36540769846868,-31.9790287759016,55.5572484915747));
#85506=CARTESIAN_POINT('Ctrl Pts',(5.36926647496159,-31.9959613378884,55.4879917009078));
#85507=CARTESIAN_POINT('Ctrl Pts',(5.3731228205498,-32.0128832329073,55.4187785397848));
#85508=CARTESIAN_POINT('Ctrl Pts',(5.37697916613801,-32.0262130196965,55.348634140719));
#85509=CARTESIAN_POINT('Ctrl Pts',(5.38083551172622,-32.0358619075835,55.2779637669743));
#85510=CARTESIAN_POINT('Ctrl Pts',(5.38469071797155,-32.0455079447426,55.2073142725271));
#85511=CARTESIAN_POINT('Ctrl Pts',(5.38854592421687,-32.0514751763228,55.1361395929657));
#85512=CARTESIAN_POINT('Ctrl Pts',(5.3924011304622,-32.0537262797841,55.0648531435188));
#85513=CARTESIAN_POINT('Ctrl Pts',(5.39625648731346,-32.055977471186,54.9935639092244));
#85514=CARTESIAN_POINT('Ctrl Pts',(5.40011184416471,-32.0545122331165,54.9221633819892));
#85515=CARTESIAN_POINT('Ctrl Pts',(5.40396720101597,-32.0493453378879,54.8510662946903));
#85516=CARTESIAN_POINT('Ctrl Pts',(5.40782659348453,-32.0441730341815,54.7798947860999));
#85517=CARTESIAN_POINT('Ctrl Pts',(5.41168598595309,-32.0352913737649,54.7090278370028));
#85518=CARTESIAN_POINT('Ctrl Pts',(5.41554537842165,-32.0227670734455,54.6388754659609));
#85519=CARTESIAN_POINT('Ctrl Pts',(5.41940695602509,-32.0102356820395,54.5686833756125));
#85520=CARTESIAN_POINT('Ctrl Pts',(5.42326853362853,-31.9940576553269,54.4992071420743));
#85521=CARTESIAN_POINT('Ctrl Pts',(5.42713011123197,-31.9743503595407,54.4308442917079));
#85522=CARTESIAN_POINT('Ctrl Pts',(5.43099844534684,-31.9546085823629,54.3623618284715));
#85523=CARTESIAN_POINT('Ctrl Pts',(5.43486677946171,-31.9313253661281,54.2949970970472));
#85524=CARTESIAN_POINT('Ctrl Pts',(5.43873511357658,-31.9046669889523,54.2291295675047));
#85525=CARTESIAN_POINT('Ctrl Pts',(5.44103283274752,-31.888832404223,54.1900054688932));
#85526=CARTESIAN_POINT('Ctrl Pts',(5.44333055191846,-31.8718079232593,54.1514091865266));
#85527=CARTESIAN_POINT('Ctrl Pts',(5.44562827108941,-31.8536359549886,54.1134159324275));
#85528=CARTESIAN_POINT('Ctrl Pts',(5.44949734443762,-31.8230366202179,54.0494400172218));
#85529=CARTESIAN_POINT('Ctrl Pts',(5.45336641778584,-31.7890613887607,53.9869247961122));
#85530=CARTESIAN_POINT('Ctrl Pts',(5.45723549113406,-31.7518727042285,53.9262497540493));
#85531=CARTESIAN_POINT('Ctrl Pts',(5.46109879952985,-31.7147394311547,53.8656651183187));
#85532=CARTESIAN_POINT('Ctrl Pts',(5.46496210792565,-31.6744024609844,53.8069156298799));
#85533=CARTESIAN_POINT('Ctrl Pts',(5.46882541632145,-31.6310710858572,53.7503581811652));
#85534=CARTESIAN_POINT('Ctrl Pts',(5.47268419281436,-31.5877905411488,53.6938670778826));
#85535=CARTESIAN_POINT('Ctrl Pts',(5.47654296930727,-31.5415228627517,53.6395632904017));
#85536=CARTESIAN_POINT('Ctrl Pts',(5.48040174580018,-31.492520829689,53.58777511159));
#85537=CARTESIAN_POINT('Ctrl Pts',(5.48425809138839,-31.4435496663262,53.5360195576603));
#85538=CARTESIAN_POINT('Ctrl Pts',(5.4881144369766,-31.3918478989097,53.486776820306));
#85539=CARTESIAN_POINT('Ctrl Pts',(5.49197078256481,-31.337707849888,53.440341296678));
#85540=CARTESIAN_POINT('Ctrl Pts',(5.49582598881014,-31.2835837963413,53.3939194922518));
#85541=CARTESIAN_POINT('Ctrl Pts',(5.49968119505547,-31.2270232598805,53.3503035710914));
#85542=CARTESIAN_POINT('Ctrl Pts',(5.50353640130079,-31.1683533262419,53.3097491110609));
#85543=CARTESIAN_POINT('Ctrl Pts',(5.50739175815205,-31.1096811006274,53.2691930667462));
#85544=CARTESIAN_POINT('Ctrl Pts',(5.5112471150033,-31.0488997150942,53.2316989954185));
#85545=CARTESIAN_POINT('Ctrl Pts',(5.51510247185456,-30.9863656167692,53.1974794224321));
#85546=CARTESIAN_POINT('Ctrl Pts',(5.51896186432312,-30.9237660605114,53.1632240299079));
#85547=CARTESIAN_POINT('Ctrl Pts',(5.52282125679167,-30.8594105560905,53.1322502116607));
#85548=CARTESIAN_POINT('Ctrl Pts',(5.52668064926023,-30.7936797627601,53.1047242953372));
#85549=CARTESIAN_POINT('Ctrl Pts',(5.53054222686366,-30.7279117535598,53.077182794219));
#85550=CARTESIAN_POINT('Ctrl Pts',(5.53440380446709,-30.6607673628243,53.0530932452879));
#85551=CARTESIAN_POINT('Ctrl Pts',(5.53826538207053,-30.5926442249953,53.0325726480808));
#85552=CARTESIAN_POINT('Ctrl Pts',(5.5421337161854,-30.5244018937155,53.0120161464678));
#85553=CARTESIAN_POINT('Ctrl Pts',(5.54600205030027,-30.4551778682624,52.9950411796584));
#85554=CARTESIAN_POINT('Ctrl Pts',(5.54987038441514,-30.3853811412491,52.9817138611016));
#85555=CARTESIAN_POINT('Ctrl Pts',(5.55216810358608,-30.343923171755,52.973797679501));
#85556=CARTESIAN_POINT('Ctrl Pts',(5.55446582275703,-30.3022632866961,52.9671674501318));
#85557=CARTESIAN_POINT('Ctrl Pts',(5.55676354192797,-30.2604876760479,52.9618283357069));
#85558=CARTESIAN_POINT('Ctrl Pts',(5.56063261527618,-30.1901427427731,52.9528379309675));
#85559=CARTESIAN_POINT('Ctrl Pts',(5.5645016886244,-30.1191940371152,52.9474759921008));
#85560=CARTESIAN_POINT('Ctrl Pts',(5.56837076197261,-30.0480484844917,52.9458118621611));
#85561=CARTESIAN_POINT('Ctrl Pts',(5.5722340703684,-29.977008939351,52.9441502117893));
#85562=CARTESIAN_POINT('Ctrl Pts',(5.57609737876418,-29.9057736111407,52.946175444879));
#85563=CARTESIAN_POINT('Ctrl Pts',(5.57996068715997,-29.8347558532785,52.9519052916249));
#85564=CARTESIAN_POINT('Ctrl Pts',(5.58381946365288,-29.7638214036972,52.9576284169014));
#85565=CARTESIAN_POINT('Ctrl Pts',(5.58767824014579,-29.6931044993658,52.967047484839));
#85566=CARTESIAN_POINT('Ctrl Pts',(5.5915370166387,-29.623018051686,52.9801281790308));
#85567=CARTESIAN_POINT('Ctrl Pts',(5.59539336222691,-29.5529757562073,52.9932006328072));
#85568=CARTESIAN_POINT('Ctrl Pts',(5.59924970781511,-29.4835636058177,53.0099300474539));
#85569=CARTESIAN_POINT('Ctrl Pts',(5.60310605340332,-29.4151874815847,53.0302305005903));
#85570=CARTESIAN_POINT('Ctrl Pts',(5.60696125964865,-29.3468315588217,53.0505249560337));
#85571=CARTESIAN_POINT('Ctrl Pts',(5.61081646589399,-29.2795115199829,53.074388217214));
#85572=CARTESIAN_POINT('Ctrl Pts',(5.61467167213932,-29.2136194867206,53.1016841014113));
#85573=CARTESIAN_POINT('Ctrl Pts',(5.61852702899056,-29.1477248793473,53.1289810519384));
#85574=CARTESIAN_POINT('Ctrl Pts',(5.62238238584179,-29.0832588362648,53.1597107037637));
#85575=CARTESIAN_POINT('Ctrl Pts',(5.62623774269303,-29.0205932334006,53.1936888562489));
#85576=CARTESIAN_POINT('Ctrl Pts',(5.63009713516159,-28.9578620349503,53.227702575564));
#85577=CARTESIAN_POINT('Ctrl Pts',(5.63395652763014,-28.8969354667709,53.2649713514488));
#85578=CARTESIAN_POINT('Ctrl Pts',(5.6378159200987,-28.8381597238713,53.3052655856255));
#85579=CARTESIAN_POINT('Ctrl Pts',(5.64167749770213,-28.7793507029555,53.3455826338427));
#85580=CARTESIAN_POINT('Ctrl Pts',(5.64553907530556,-28.7226953175213,53.3889282550317));
#85581=CARTESIAN_POINT('Ctrl Pts',(5.64940065290899,-28.6685075266163,53.4350318355243));
#85582=CARTESIAN_POINT('Ctrl Pts',(5.65326898702387,-28.614224924609,53.4812160823665));
#85583=CARTESIAN_POINT('Ctrl Pts',(5.65713732113874,-28.5624188903338,53.530167589093));
#85584=CARTESIAN_POINT('Ctrl Pts',(5.66100565525361,-28.5133667914838,53.5815786007548));
#85585=CARTESIAN_POINT('Ctrl Pts',(5.66330337442458,-28.4842307487953,53.6121157941787));
#85586=CARTESIAN_POINT('Ctrl Pts',(5.66560109359555,-28.45606557884,53.6435200799697));
#85587=CARTESIAN_POINT('Ctrl Pts',(5.66789881276653,-28.428922365385,53.6757218462451));
#85588=CARTESIAN_POINT('Ctrl Pts',(5.67174314546748,-28.3835088333867,53.7295988842594));
#85589=CARTESIAN_POINT('Ctrl Pts',(5.67558747816844,-28.3407741615804,53.7859284481419));
#85590=CARTESIAN_POINT('Ctrl Pts',(5.67943181086939,-28.3009964282985,53.844411653812));
#85591=CARTESIAN_POINT('Ctrl Pts',(5.68327073565046,-28.2612746513585,53.9028125896799));
#85592=CARTESIAN_POINT('Ctrl Pts',(5.68710966043153,-28.2245018386303,53.9633607567452));
#85593=CARTESIAN_POINT('Ctrl Pts',(5.6909485852126,-28.1909165779055,54.0257234815502));
#85594=CARTESIAN_POINT('Ctrl Pts',(5.69478343427785,-28.1573669740341,54.0880199969975));
#85595=CARTESIAN_POINT('Ctrl Pts',(5.6986182833431,-28.1269984405792,54.1521268173286));
#85596=CARTESIAN_POINT('Ctrl Pts',(5.70245313240835,-28.1000058717308,54.217683008594));
#85597=CARTESIAN_POINT('Ctrl Pts',(5.70628582152484,-28.0730285062359,54.2832022758471));
#85598=CARTESIAN_POINT('Ctrl Pts',(5.71011851064132,-28.0494235257525,54.350168842789));
#85599=CARTESIAN_POINT('Ctrl Pts',(5.71395119975781,-28.0293387874977,54.4181993915102));
#85600=CARTESIAN_POINT('Ctrl Pts',(5.71778249936709,-28.0092613307855,54.4862052763635));
#85601=CARTESIAN_POINT('Ctrl Pts',(5.72161379897638,-27.9927017184508,54.5552739041778));
#85602=CARTESIAN_POINT('Ctrl Pts',(5.72544509858566,-27.9797581310333,54.6250061955525));
#85603=CARTESIAN_POINT('Ctrl Pts',(5.7292781028654,-27.9668087845906,54.6947695131036));
#85604=CARTESIAN_POINT('Ctrl Pts',(5.73311110714515,-27.9574787693276,54.7651965997995));
#85605=CARTESIAN_POINT('Ctrl Pts',(5.73694411142489,-27.9518149998429,54.8358788020042));
#85606=CARTESIAN_POINT('Ctrl Pts',(5.73993783446249,-27.947391379114,54.8910843070453));
#85607=CARTESIAN_POINT('Ctrl Pts',(5.74293155750008,-27.9452032175471,54.9464451824547));
#85608=CARTESIAN_POINT('Ctrl Pts',(5.74592528053768,-27.9452507587434,55.001765801585));
#85609=CARTESIAN_POINT('Origin',(-1.54592528053767,-30.,55.));
#85610=CARTESIAN_POINT('',(4.59397380331217,-31.2520475724682,56.6292251037768));
#85611=CARTESIAN_POINT('',(4.65201752376309,-31.2520475724682,56.6292251037768));
#85612=CARTESIAN_POINT('',(-1.54592528053767,-31.2520475724682,56.6292251037768));
#85613=CARTESIAN_POINT('',(5.10407471942444,-27.9452501074214,55.0006644157262));
#85614=CARTESIAN_POINT('Ctrl Pts',(4.65201752376309,-31.2520475724682,56.6292251037768));
#85615=CARTESIAN_POINT('Ctrl Pts',(4.65588667239735,-31.3085034428774,56.5858391804114));
#85616=CARTESIAN_POINT('Ctrl Pts',(4.65975582103161,-31.3626178531137,56.5395797614622));
#85617=CARTESIAN_POINT('Ctrl Pts',(4.66362496966587,-31.4141019698079,56.490742493352));
#85618=CARTESIAN_POINT('Ctrl Pts',(4.66425231302696,-31.4224495991866,56.4828240237302));
#85619=CARTESIAN_POINT('Ctrl Pts',(4.66487965638806,-31.430728164715,56.4748378560675));
#85620=CARTESIAN_POINT('Ctrl Pts',(4.66550699974915,-31.4389365354664,56.4667853317374));
#85621=CARTESIAN_POINT('Ctrl Pts',(4.66937607309736,-31.4895607876317,56.417122245773));
#85622=CARTESIAN_POINT('Ctrl Pts',(4.67324514644558,-31.5377100925752,56.3647379575139));
#85623=CARTESIAN_POINT('Ctrl Pts',(4.67711421979379,-31.5830779920416,56.3099090173037));
#85624=CARTESIAN_POINT('Ctrl Pts',(4.68097752818958,-31.6283782929492,56.2551617726842));
#85625=CARTESIAN_POINT('Ctrl Pts',(4.68484083658537,-31.6709051075678,56.1979774777012));
#85626=CARTESIAN_POINT('Ctrl Pts',(4.68870414498115,-31.710388520268,56.1386696940885));
#85627=CARTESIAN_POINT('Ctrl Pts',(4.69256292147407,-31.7498256164505,56.0794314822229));
#85628=CARTESIAN_POINT('Ctrl Pts',(4.69642169796698,-31.7862261342444,56.0180751320759));
#85629=CARTESIAN_POINT('Ctrl Pts',(4.70028047445989,-31.8193612958817,55.9549460914354));
#85630=CARTESIAN_POINT('Ctrl Pts',(4.7041368200481,-31.852475583436,55.8918568200541));
#85631=CARTESIAN_POINT('Ctrl Pts',(4.7079931656363,-31.88232837079,55.8269975028873));
#85632=CARTESIAN_POINT('Ctrl Pts',(4.71184951122451,-31.9087357523067,55.7607400281082));
#85633=CARTESIAN_POINT('Ctrl Pts',(4.71570471746984,-31.9351353318614,55.6945021288521));
#85634=CARTESIAN_POINT('Ctrl Pts',(4.71955992371517,-31.9580913466993,55.626867343082));
#85635=CARTESIAN_POINT('Ctrl Pts',(4.72341512996051,-31.9774678741999,55.5582278826853));
#85636=CARTESIAN_POINT('Ctrl Pts',(4.72727048681175,-31.996845158656,55.4895857408473));
#85637=CARTESIAN_POINT('Ctrl Pts',(4.731125843663,-32.0126425482941,55.4199393145738));
#85638=CARTESIAN_POINT('Ctrl Pts',(4.73498120051425,-32.0247743599362,55.3496946580158));
#85639=CARTESIAN_POINT('Ctrl Pts',(4.7388405929828,-32.0369188706231,55.2793764724531));
#85640=CARTESIAN_POINT('Ctrl Pts',(4.74269998545136,-32.0453900610246,55.2084592862478));
#85641=CARTESIAN_POINT('Ctrl Pts',(4.74655937791992,-32.0501537961901,55.1373571056304));
#85642=CARTESIAN_POINT('Ctrl Pts',(4.75042095552336,-32.0549202285169,55.0662146679373));
#85643=CARTESIAN_POINT('Ctrl Pts',(4.7542825331268,-32.0559750197405,54.9948875132876));
#85644=CARTESIAN_POINT('Ctrl Pts',(4.75814411073023,-32.0533362020556,54.9237897393517));
#85645=CARTESIAN_POINT('Ctrl Pts',(4.7620124448451,-32.0506927672934,54.8525675673143));
#85646=CARTESIAN_POINT('Ctrl Pts',(4.76588077895997,-32.0443428641057,54.7815760612898));
#85647=CARTESIAN_POINT('Ctrl Pts',(4.76974911307484,-32.0343563474449,54.7112235914919));
#85648=CARTESIAN_POINT('Ctrl Pts',(4.7720468322458,-32.0284245405995,54.6694355210258));
#85649=CARTESIAN_POINT('Ctrl Pts',(4.77434455141676,-32.0212106673078,54.6278727252012));
#85650=CARTESIAN_POINT('Ctrl Pts',(4.77664227058771,-32.0127377461673,54.586618423665));
#85651=CARTESIAN_POINT('Ctrl Pts',(4.78051134393593,-31.9984704006273,54.5171513101072));
#85652=CARTESIAN_POINT('Ctrl Pts',(4.78438041728414,-31.9805745320216,54.4482876251215));
#85653=CARTESIAN_POINT('Ctrl Pts',(4.78824949063236,-31.9591162703888,54.3804348286113));
#85654=CARTESIAN_POINT('Ctrl Pts',(4.79211279902815,-31.9376899817496,54.3126831333491));
#85655=CARTESIAN_POINT('Ctrl Pts',(4.79597610742393,-31.9127119815914,54.2459397961355));
#85656=CARTESIAN_POINT('Ctrl Pts',(4.79983941581972,-31.8842993142413,54.180601649471));
#85657=CARTESIAN_POINT('Ctrl Pts',(4.80369819231263,-31.8559199767307,54.1153401485474));
#85658=CARTESIAN_POINT('Ctrl Pts',(4.80755696880554,-31.8241141679264,54.0514810072649));
#85659=CARTESIAN_POINT('Ctrl Pts',(4.81141574529846,-31.7890480327174,53.9894037902653));
#85660=CARTESIAN_POINT('Ctrl Pts',(4.81527209088666,-31.7540039880423,53.9273656799098));
#85661=CARTESIAN_POINT('Ctrl Pts',(4.81912843647487,-31.7157039302291,53.8671076886751));
#85662=CARTESIAN_POINT('Ctrl Pts',(4.82298478206308,-31.6743605549183,53.8089860224861));
#85663=CARTESIAN_POINT('Ctrl Pts',(4.82683998830841,-31.6330293943531,53.7508815281258));
#85664=CARTESIAN_POINT('Ctrl Pts',(4.83069519455374,-31.588656982753,53.694912501404));
#85665=CARTESIAN_POINT('Ctrl Pts',(4.83455040079908,-31.5414991148609,53.6414058584761));
#85666=CARTESIAN_POINT('Ctrl Pts',(4.83840575765032,-31.4943394047187,53.5878971252795));
#85667=CARTESIAN_POINT('Ctrl Pts',(4.84226111450157,-31.4443943450982,53.5368513298448));
#85668=CARTESIAN_POINT('Ctrl Pts',(4.84611647135282,-31.3919586083003,53.4885606875304));
#85669=CARTESIAN_POINT('Ctrl Pts',(4.84997586382138,-31.3394679840886,53.440219496704));
#85670=CARTESIAN_POINT('Ctrl Pts',(4.85383525628994,-31.2844818363485,53.3946395458178));
#85671=CARTESIAN_POINT('Ctrl Pts',(4.8576946487585,-31.2273294761762,53.3520740552413));
#85672=CARTESIAN_POINT('Ctrl Pts',(4.86155622636193,-31.1701447571246,53.30948446467));
#85673=CARTESIAN_POINT('Ctrl Pts',(4.86541780396537,-31.1107917884792,53.2699130016197));
#85674=CARTESIAN_POINT('Ctrl Pts',(4.8692793815688,-31.0496282517455,53.2335691081625));
#85675=CARTESIAN_POINT('Ctrl Pts',(4.87314771568367,-30.9883576986112,53.1971616246504));
#85676=CARTESIAN_POINT('Ctrl Pts',(4.87701604979855,-30.925270682684,53.1639932116718));
#85677=CARTESIAN_POINT('Ctrl Pts',(4.88088438391342,-30.8607481803857,53.1342266663759));
#85678=CARTESIAN_POINT('Ctrl Pts',(4.88318210308436,-30.8224230031684,53.1165458870667));
#85679=CARTESIAN_POINT('Ctrl Pts',(4.88547982225531,-30.7835917421944,53.1000644084989));
#85680=CARTESIAN_POINT('Ctrl Pts',(4.88777754142626,-30.7443367983747,53.0848080270935));
#85681=CARTESIAN_POINT('Ctrl Pts',(4.89164661477447,-30.6782363545785,53.0591181780328));
#85682=CARTESIAN_POINT('Ctrl Pts',(4.89551568812269,-30.6106748968163,53.0368040872381));
#85683=CARTESIAN_POINT('Ctrl Pts',(4.8993847614709,-30.5420306164589,53.0180311876013));
#85684=CARTESIAN_POINT('Ctrl Pts',(4.90324806986669,-30.4734886166672,52.9992862597457));
#85685=CARTESIAN_POINT('Ctrl Pts',(4.90711137826248,-30.403867461625,52.9840721766353));
#85686=CARTESIAN_POINT('Ctrl Pts',(4.91097468665826,-30.3335640282406,52.9725058319285));
#85687=CARTESIAN_POINT('Ctrl Pts',(4.91483346315117,-30.2633430651898,52.960953055269));
#85688=CARTESIAN_POINT('Ctrl Pts',(4.91869223964408,-30.1924418905885,52.9530395958994));
#85689=CARTESIAN_POINT('Ctrl Pts',(4.922551016137,-30.1212695042465,52.9488317304912));
#85690=CARTESIAN_POINT('Ctrl Pts',(4.9264073617252,-30.0501419542119,52.9446265159024));
#85691=CARTESIAN_POINT('Ctrl Pts',(4.93026370731341,-29.9787440152021,52.9441222924568));
#85692=CARTESIAN_POINT('Ctrl Pts',(4.93412005290161,-29.9074903098069,52.9473335585828));
#85693=CARTESIAN_POINT('Ctrl Pts',(4.93797525914695,-29.8362576560524,52.9505438759522));
#85694=CARTESIAN_POINT('Ctrl Pts',(4.94183046539228,-29.7651696363424,52.9574674817409));
#85695=CARTESIAN_POINT('Ctrl Pts',(4.94568567163761,-29.6946396410612,52.9680667792251));
#85696=CARTESIAN_POINT('Ctrl Pts',(4.94954102848885,-29.6241068904839,52.9786664907771));
#85697=CARTESIAN_POINT('Ctrl Pts',(4.9533963853401,-29.5541326876797,52.9929421047381));
#85698=CARTESIAN_POINT('Ctrl Pts',(4.95725174219134,-29.4851223551726,53.0108045411883));
#85699=CARTESIAN_POINT('Ctrl Pts',(4.9611111346599,-29.4160397856968,53.0286856752482));
#85700=CARTESIAN_POINT('Ctrl Pts',(4.96497052712846,-29.3479235718339,53.0501610047003));
#85701=CARTESIAN_POINT('Ctrl Pts',(4.96882991959702,-29.2811650615579,53.0750911985824));
#85702=CARTESIAN_POINT('Ctrl Pts',(4.97269149720045,-29.2143687535325,53.1000355075971));
#85703=CARTESIAN_POINT('Ctrl Pts',(4.97655307480389,-29.1489321251945,53.1284383815136));
#85704=CARTESIAN_POINT('Ctrl Pts',(4.98041465240732,-29.0852251315543,53.1601129103773));
#85705=CARTESIAN_POINT('Ctrl Pts',(4.98428298652219,-29.021406671287,53.1918428594186));
#85706=CARTESIAN_POINT('Ctrl Pts',(4.98815132063707,-28.9593243110823,53.2268556535021));
#85707=CARTESIAN_POINT('Ctrl Pts',(4.99201965475194,-28.8993214518452,53.2649195130681));
#85708=CARTESIAN_POINT('Ctrl Pts',(4.9943173739229,-28.8636808593091,53.2875287441346));
#85709=CARTESIAN_POINT('Ctrl Pts',(4.99661509309386,-28.8287733699117,53.3112136158591));
#85710=CARTESIAN_POINT('Ctrl Pts',(4.99891281226483,-28.7946653476447,53.3359188906993));
#85711=CARTESIAN_POINT('Ctrl Pts',(5.00275064676246,-28.7376953984199,53.3771836184579));
#85712=CARTESIAN_POINT('Ctrl Pts',(5.00658848126009,-28.6827265110719,53.4214646825556));
#85713=CARTESIAN_POINT('Ctrl Pts',(5.01042631575773,-28.6300997290131,53.4685396479014));
#85714=CARTESIAN_POINT('Ctrl Pts',(5.01432833257717,-28.5765928388975,53.5164018750681));
#85715=CARTESIAN_POINT('Ctrl Pts',(5.01823034939662,-28.5255075807004,53.5671520862871));
#85716=CARTESIAN_POINT('Ctrl Pts',(5.02213236621606,-28.477171663074,53.620510449929));
#85717=CARTESIAN_POINT('Ctrl Pts',(5.02595997436977,-28.4297574767738,53.6728513077967));
#85718=CARTESIAN_POINT('Ctrl Pts',(5.02978758252349,-28.3849890497206,53.7277013416823));
#85719=CARTESIAN_POINT('Ctrl Pts',(5.0336151906772,-28.3431406316787,53.7847573920793));
#85720=CARTESIAN_POINT('Ctrl Pts',(5.03744050268939,-28.3013173180588,53.841779215157));
#85721=CARTESIAN_POINT('Ctrl Pts',(5.04126581470158,-28.2624108313474,53.9010040323731));
#85722=CARTESIAN_POINT('Ctrl Pts',(5.04509112671377,-28.2266549764503,53.9620958666854));
#85723=CARTESIAN_POINT('Ctrl Pts',(5.04891547573736,-28.1909081227747,54.0231723216666));
#85724=CARTESIAN_POINT('Ctrl Pts',(5.05273982476095,-28.1583105759941,54.0861144340417));
#85725=CARTESIAN_POINT('Ctrl Pts',(5.05656417378455,-28.1290516520463,54.1505591004728));
#85726=CARTESIAN_POINT('Ctrl Pts',(5.06052338592121,-28.098760931695,54.2172763650067));
#85727=CARTESIAN_POINT('Ctrl Pts',(5.06448259805786,-28.0720489807079,54.2856036450338));
#85728=CARTESIAN_POINT('Ctrl Pts',(5.06844181019452,-28.0490719088945,54.3551146258167));
#85729=CARTESIAN_POINT('Ctrl Pts',(5.07227054686684,-28.0268520443261,54.4223348787524));
#85730=CARTESIAN_POINT('Ctrl Pts',(5.07609928353915,-28.0081247870476,54.4906615152341));
#85731=CARTESIAN_POINT('Ctrl Pts',(5.07992802021147,-27.9929800396064,54.5596950589858));
#85732=CARTESIAN_POINT('Ctrl Pts',(5.0839524700803,-27.9770611394391,54.632257384336));
#85733=CARTESIAN_POINT('Ctrl Pts',(5.08797691994913,-27.9651009153748,54.7056002068222));
#85734=CARTESIAN_POINT('Ctrl Pts',(5.09200136981795,-27.9571422025373,54.779252221198));
#85735=CARTESIAN_POINT('Ctrl Pts',(5.09602581968678,-27.9491834896999,54.8529042355738));
#85736=CARTESIAN_POINT('Ctrl Pts',(5.10005026955561,-27.9452262438762,54.9268648126139));
#85737=CARTESIAN_POINT('Ctrl Pts',(5.10407471942444,-27.9452501074214,55.0006644157262));
#85738=CARTESIAN_POINT('Ctrl Pts',(5.10407471946233,-27.9452501074216,55.000664416421));
#85739=CARTESIAN_POINT('Ctrl Pts',(5.10606584067601,-27.9452619140691,55.0371772219238));
#85740=CARTESIAN_POINT('Ctrl Pts',(5.1080569618897,-27.9462469037348,55.0736730530943));
#85741=CARTESIAN_POINT('Ctrl Pts',(5.11004808310338,-27.9482027488899,55.1101163150356));
#85742=CARTESIAN_POINT('Ctrl Pts',(5.1139171564516,-27.9520032751014,55.1809315183137));
#85743=CARTESIAN_POINT('Ctrl Pts',(5.11778622979981,-27.959481696,55.2516884433728));
#85744=CARTESIAN_POINT('Ctrl Pts',(5.12165530314803,-27.97063308038,55.32197432825));
#85745=CARTESIAN_POINT('Ctrl Pts',(5.12551861154382,-27.9817678491018,55.3921554865566));
#85746=CARTESIAN_POINT('Ctrl Pts',(5.1293819199396,-27.9965646425545,55.4618665219658));
#85747=CARTESIAN_POINT('Ctrl Pts',(5.13324522833539,-28.0149666018932,55.5306976266206));
#85748=CARTESIAN_POINT('Ctrl Pts',(5.1371040048283,-28.0333469745804,55.5994479880758));
#85749=CARTESIAN_POINT('Ctrl Pts',(5.14096278132121,-28.0553239879001,55.667320002077));
#85750=CARTESIAN_POINT('Ctrl Pts',(5.14482155781412,-28.0807896635758,55.733913650958));
#85751=CARTESIAN_POINT('Ctrl Pts',(5.14867790340233,-28.1062392966974,55.8004653479885));
#85752=CARTESIAN_POINT('Ctrl Pts',(5.15253424899053,-28.1351730587826,55.8657398249893));
#85753=CARTESIAN_POINT('Ctrl Pts',(5.15639059457874,-28.1674334698244,55.9293532562919));
#85754=CARTESIAN_POINT('Ctrl Pts',(5.16024580082407,-28.1996843496485,55.9929478932442));
#85755=CARTESIAN_POINT('Ctrl Pts',(5.16410100706941,-28.2352597076089,56.0548820257512));
#85756=CARTESIAN_POINT('Ctrl Pts',(5.16795621331474,-28.2739550952372,56.1147943977444));
#85757=CARTESIAN_POINT('Ctrl Pts',(5.17181157016599,-28.3126519945236,56.1747091102498));
#85758=CARTESIAN_POINT('Ctrl Pts',(5.17566692701723,-28.3544689000551,56.2326014985562));
#85759=CARTESIAN_POINT('Ctrl Pts',(5.17952228386848,-28.3991577667128,56.2881388537824));
#85760=CARTESIAN_POINT('Ctrl Pts',(5.18338167633704,-28.4438934117027,56.3437343430598));
#85761=CARTESIAN_POINT('Ctrl Pts',(5.1872410688056,-28.4915067137864,56.3969694990263));
#85762=CARTESIAN_POINT('Ctrl Pts',(5.19110046127416,-28.5417095857703,56.4475450356606));
#85763=CARTESIAN_POINT('Ctrl Pts',(5.19496203887759,-28.591940881929,56.4981492074674));
#85764=CARTESIAN_POINT('Ctrl Pts',(5.19882361648103,-28.6447643068034,56.5460904356484));
#85765=CARTESIAN_POINT('Ctrl Pts',(5.20268519408446,-28.6998572202674,56.5911085176094));
#85766=CARTESIAN_POINT('Ctrl Pts',(5.20655352819934,-28.7550465285054,56.6362053666489));
#85767=CARTESIAN_POINT('Ctrl Pts',(5.21042186231421,-28.812512861496,56.6783685706392));
#85768=CARTESIAN_POINT('Ctrl Pts',(5.21429019642908,-28.8719036200713,56.7173805984964));
#85769=CARTESIAN_POINT('Ctrl Pts',(5.21658791560004,-28.9071806360952,56.7405530240531));
#85770=CARTESIAN_POINT('Ctrl Pts',(5.21888563477099,-28.9431361072497,56.7626145303181));
#85771=CARTESIAN_POINT('Ctrl Pts',(5.22118335394195,-28.9796923731628,56.7835273782922));
#85772=CARTESIAN_POINT('Ctrl Pts',(5.22505242729016,-29.0412485789612,56.8187420136377));
#85773=CARTESIAN_POINT('Ctrl Pts',(5.22892150063838,-29.1047505806775,56.8508350814401));
#85774=CARTESIAN_POINT('Ctrl Pts',(5.2327905739866,-29.1698489244987,56.8795868573557));
#85775=CARTESIAN_POINT('Ctrl Pts',(5.23665388238238,-29.23485027123,56.9082957928788));
#85776=CARTESIAN_POINT('Ctrl Pts',(5.24051719077816,-29.3014427979312,56.9336731241379));
#85777=CARTESIAN_POINT('Ctrl Pts',(5.24438049917394,-29.3692513689758,56.9555443556619));
#85778=CARTESIAN_POINT('Ctrl Pts',(5.24823927566685,-29.436980396317,56.9773899308606));
#85779=CARTESIAN_POINT('Ctrl Pts',(5.25209805215977,-29.5059221744099,56.9957374274861));
#85780=CARTESIAN_POINT('Ctrl Pts',(5.25595682865268,-29.5756820674498,57.0104606075764));
#85781=CARTESIAN_POINT('Ctrl Pts',(5.25981317424088,-29.6453980140075,57.0251745125381));
#85782=CARTESIAN_POINT('Ctrl Pts',(5.26366951982909,-29.7159305788035,57.0362685307208));
#85783=CARTESIAN_POINT('Ctrl Pts',(5.2675258654173,-29.7868718816747,57.0436667946804));
#85784=CARTESIAN_POINT('Ctrl Pts',(5.27138107166263,-29.8577922252033,57.0510628728505));
#85785=CARTESIAN_POINT('Ctrl Pts',(5.27523627790796,-29.9291205841624,57.0547653141544));
#85786=CARTESIAN_POINT('Ctrl Pts',(5.27909148415329,-30.0004425660863,57.0547499523385));
#85787=CARTESIAN_POINT('Ctrl Pts',(5.28294684100454,-30.0717673342457,57.0547345899226));
#85788=CARTESIAN_POINT('Ctrl Pts',(5.28680219785578,-30.1430852390898,57.0510011383428));
#85789=CARTESIAN_POINT('Ctrl Pts',(5.29065755470703,-30.2139822266312,57.04357754176));
#85790=CARTESIAN_POINT('Ctrl Pts',(5.29451694717559,-30.2849534260086,57.0361461744842));
#85791=CARTESIAN_POINT('Ctrl Pts',(5.29837633964415,-30.3555023444169,57.0250170021201));
#85792=CARTESIAN_POINT('Ctrl Pts',(5.30223573211271,-30.4252212904858,57.0102697372784));
#85793=CARTESIAN_POINT('Ctrl Pts',(5.30609730971614,-30.4949797104621,56.9955141227385));
#85794=CARTESIAN_POINT('Ctrl Pts',(5.30995888731957,-30.5639067530248,56.9771364629712));
#85795=CARTESIAN_POINT('Ctrl Pts',(5.31382046492301,-30.6316088222237,56.9552666974582));
#85796=CARTESIAN_POINT('Ctrl Pts',(5.31768879903788,-30.6994293481395,56.9333586669313));
#85797=CARTESIAN_POINT('Ctrl Pts',(5.32155713315275,-30.766020167512,56.9079465050118));
#85798=CARTESIAN_POINT('Ctrl Pts',(5.32542546726762,-30.8310072858769,56.8792084645721));
#85799=CARTESIAN_POINT('Ctrl Pts',(5.32772318643858,-30.8696084364751,56.8621385981922));
#85800=CARTESIAN_POINT('Ctrl Pts',(5.33002090560954,-30.9076442250829,56.8438962093788));
#85801=CARTESIAN_POINT('Ctrl Pts',(5.3323186247805,-30.9450408253263,56.8245260757157));
#85802=CARTESIAN_POINT('Ctrl Pts',(5.33618678846697,-31.007997244408,56.7919168480152));
#85803=CARTESIAN_POINT('Ctrl Pts',(5.34005495215343,-31.069387166087,56.7559814127803));
#85804=CARTESIAN_POINT('Ctrl Pts',(5.34392311583989,-31.1288367206716,56.7168940621259));
#85805=CARTESIAN_POINT('Ctrl Pts',(5.34666138801451,-31.1709210465449,56.6892241356823));
#85806=CARTESIAN_POINT('Ctrl Pts',(5.34939966018912,-31.2120333271599,56.6599757585428));
#85807=CARTESIAN_POINT('Ctrl Pts',(5.35213793236373,-31.2520475724682,56.6292251037768));
#85808=CARTESIAN_POINT('',(5.04592528049197,-27.9452502582983,54.9989697199742));
#85809=CARTESIAN_POINT('Ctrl Pts',(5.04592528053768,-27.9452502582979,54.9989697208212));
#85810=CARTESIAN_POINT('Ctrl Pts',(5.04983580638859,-27.9452139274514,55.0714265840048));
#85811=CARTESIAN_POINT('Ctrl Pts',(5.0537463322395,-27.9490145212746,55.1438783326772));
#85812=CARTESIAN_POINT('Ctrl Pts',(5.05765685809041,-27.9566240457995,55.2158987547329));
#85813=CARTESIAN_POINT('Ctrl Pts',(5.06156889758459,-27.9642365157354,55.2879470536603));
#85814=CARTESIAN_POINT('Ctrl Pts',(5.06548093707878,-27.9756607961671,55.3595632307951));
#85815=CARTESIAN_POINT('Ctrl Pts',(5.06939297657296,-27.9908172317786,55.4303279753656));
#85816=CARTESIAN_POINT('Ctrl Pts',(5.07331083119316,-28.0059961969641,55.5011979095459));
#85817=CARTESIAN_POINT('Ctrl Pts',(5.07722868581337,-28.0249182944707,55.5712134277549));
#85818=CARTESIAN_POINT('Ctrl Pts',(5.08114654043358,-28.0474531999293,55.6399676210822));
#85819=CARTESIAN_POINT('Ctrl Pts',(5.08506751736907,-28.0700060644718,55.7087766077313));
#85820=CARTESIAN_POINT('Ctrl Pts',(5.08898849430456,-28.0961773017066,55.7763218332449));
#85821=CARTESIAN_POINT('Ctrl Pts',(5.09290947124006,-28.1257883534145,55.8422162823784));
#85822=CARTESIAN_POINT('Ctrl Pts',(5.09683849198264,-28.1554601516128,55.9082459126787));
#85823=CARTESIAN_POINT('Ctrl Pts',(5.10076751272523,-28.1885856454507,55.9726175877542));
#85824=CARTESIAN_POINT('Ctrl Pts',(5.10469653346781,-28.2249403918811,56.0349690575687));
#85825=CARTESIAN_POINT('Ctrl Pts',(5.10720517516979,-28.2481525454773,56.0747798673363));
#85826=CARTESIAN_POINT('Ctrl Pts',(5.10971381687176,-28.272680273511,56.1137676684776));
#85827=CARTESIAN_POINT('Ctrl Pts',(5.11222245857373,-28.2984564079793,56.1518450273163));
#85828=CARTESIAN_POINT('Ctrl Pts',(5.11609153192195,-28.3382108913768,56.2105716657746));
#85829=CARTESIAN_POINT('Ctrl Pts',(5.11996060527016,-28.3810871266736,56.2673528041018));
#85830=CARTESIAN_POINT('Ctrl Pts',(5.12382967861838,-28.4268681537415,56.3218372656221));
#85831=CARTESIAN_POINT('Ctrl Pts',(5.12769298701417,-28.472580966687,56.3762405448282));
#85832=CARTESIAN_POINT('Ctrl Pts',(5.13155629540996,-28.5211896701546,56.4283535710454));
#85833=CARTESIAN_POINT('Ctrl Pts',(5.13541960380575,-28.5724343269205,56.477854462234));
#85834=CARTESIAN_POINT('Ctrl Pts',(5.13927838029866,-28.6236188704922,56.5272972857749));
#85835=CARTESIAN_POINT('Ctrl Pts',(5.14313715679158,-28.6774328776295,56.5741337249527));
#85836=CARTESIAN_POINT('Ctrl Pts',(5.14699593328449,-28.7335776498748,56.6180766340329));
#85837=CARTESIAN_POINT('Ctrl Pts',(5.1508522788727,-28.7896870527249,56.6619918604981));
#85838=CARTESIAN_POINT('Ctrl Pts',(5.15470862446091,-28.8481239259431,56.703016874631));
#85839=CARTESIAN_POINT('Ctrl Pts',(5.15856497004911,-28.9085554955761,56.7409039193083));
#85840=CARTESIAN_POINT('Ctrl Pts',(5.16242017629444,-28.9689692109279,56.7787797703999));
#85841=CARTESIAN_POINT('Ctrl Pts',(5.16627538253978,-29.0313760413579,56.8135192346887));
#85842=CARTESIAN_POINT('Ctrl Pts',(5.17013058878511,-29.0954145952794,56.8449181033494));
#85843=CARTESIAN_POINT('Ctrl Pts',(5.17398594563635,-29.159455650905,56.8763181986256));
#85844=CARTESIAN_POINT('Ctrl Pts',(5.1778413024876,-29.225128119431,56.904377227293));
#85845=CARTESIAN_POINT('Ctrl Pts',(5.18169665933885,-29.2920479619277,56.9289379135393));
#85846=CARTESIAN_POINT('Ctrl Pts',(5.1855560518074,-29.3590378531605,56.9535243088274));
#85847=CARTESIAN_POINT('Ctrl Pts',(5.18941544427596,-29.4272772678509,56.9746048839808));
#85848=CARTESIAN_POINT('Ctrl Pts',(5.19327483674452,-29.4963650787195,56.9920716424283));
#85849=CARTESIAN_POINT('Ctrl Pts',(5.19713641434796,-29.5654920061554,57.0095482903138));
#85850=CARTESIAN_POINT('Ctrl Pts',(5.20099799195139,-29.6354678092425,57.0234069539317));
#85851=CARTESIAN_POINT('Ctrl Pts',(5.20485956955483,-29.7058818937089,57.0335909377384));
#85852=CARTESIAN_POINT('Ctrl Pts',(5.2087279036697,-29.7764191800413,57.0437927402219));
#85853=CARTESIAN_POINT('Ctrl Pts',(5.21259623778457,-29.8473957948861,57.0503069817964));
#85854=CARTESIAN_POINT('Ctrl Pts',(5.21646457189944,-29.918397463003,57.0531289751147));
#85855=CARTESIAN_POINT('Ctrl Pts',(5.21876229107039,-29.9605711453059,57.0548051871365));
#85856=CARTESIAN_POINT('Ctrl Pts',(5.22106001024135,-30.0027536735451,57.0551797214769));
#85857=CARTESIAN_POINT('Ctrl Pts',(5.2233577294123,-30.0448590459357,57.0542602630869));
#85858=CARTESIAN_POINT('Ctrl Pts',(5.22722618551046,-30.1157479459585,57.052712256498));
#85859=CARTESIAN_POINT('Ctrl Pts',(5.23109464160863,-30.1866954538954,57.0474875355491));
#85860=CARTESIAN_POINT('Ctrl Pts',(5.23496309770679,-30.2572890573119,57.0385779120474));
#85861=CARTESIAN_POINT('Ctrl Pts',(5.23882613522196,-30.3277837796012,57.0296807683395));
#85862=CARTESIAN_POINT('Ctrl Pts',(5.24268917273712,-30.3979251031771,57.0171090230145));
#85863=CARTESIAN_POINT('Ctrl Pts',(5.24655221025229,-30.467301706206,57.00090646405));
#85864=CARTESIAN_POINT('Ctrl Pts',(5.2504962515766,-30.538133063192,56.9843641545682));
#85865=CARTESIAN_POINT('Ctrl Pts',(5.25444029290092,-30.6081667459654,56.9640370267955));
#85866=CARTESIAN_POINT('Ctrl Pts',(5.25838433422523,-30.6769723099905,56.9400273333142));
#85867=CARTESIAN_POINT('Ctrl Pts',(5.26224054826836,-30.7442456878335,56.9165522960211));
#85868=CARTESIAN_POINT('Ctrl Pts',(5.26609676231149,-30.8103446016693,56.88955719285));
#85869=CARTESIAN_POINT('Ctrl Pts',(5.26995297635461,-30.8748808360116,56.859188286667));
#85870=CARTESIAN_POINT('Ctrl Pts',(5.27394093131952,-30.941621839826,56.8277818790254));
#85871=CARTESIAN_POINT('Ctrl Pts',(5.27792888628444,-31.0066909351777,56.792767130044));
#85872=CARTESIAN_POINT('Ctrl Pts',(5.28191684124935,-31.0696823161643,56.7543595141776));
#85873=CARTESIAN_POINT('Ctrl Pts',(5.28590479621426,-31.1326736971508,56.7159518983112));
#85874=CARTESIAN_POINT('Ctrl Pts',(5.28989275117917,-31.1935868763248,56.6741517210512));
#85875=CARTESIAN_POINT('Ctrl Pts',(5.29388070614408,-31.2520475724682,56.6292251037768));
#85876=CARTESIAN_POINT('Ctrl Pts',(4.59397380331217,-31.2520475724682,56.6292251037768));
#85877=CARTESIAN_POINT('Ctrl Pts',(4.59782977348395,-31.3085555898331,56.5857991058575));
#85878=CARTESIAN_POINT('Ctrl Pts',(4.60168574365573,-31.3628372624389,56.5394024325893));
#85879=CARTESIAN_POINT('Ctrl Pts',(4.60554171382751,-31.4145710538178,56.4902973851553));
#85880=CARTESIAN_POINT('Ctrl Pts',(4.60939684064206,-31.4662935302577,56.4412030777154));
#85881=CARTESIAN_POINT('Ctrl Pts',(4.61325196745661,-31.5154688799484,56.3894019068612));
#85882=CARTESIAN_POINT('Ctrl Pts',(4.61710709427116,-31.5618108701437,56.3351945058309));
#85883=CARTESIAN_POINT('Ctrl Pts',(4.62096266749001,-31.6081582265084,56.2809808278561));
#85884=CARTESIAN_POINT('Ctrl Pts',(4.62481824070887,-31.6516712583411,56.2243607374448));
#85885=CARTESIAN_POINT('Ctrl Pts',(4.62867381392772,-31.6921037647007,56.1656682255195));
#85886=CARTESIAN_POINT('Ctrl Pts',(4.63253360485403,-31.7325805011846,56.1069115083955));
#85887=CARTESIAN_POINT('Ctrl Pts',(4.63639339578033,-31.7699697123549,56.04607824704));
#85888=CARTESIAN_POINT('Ctrl Pts',(4.64025318670663,-31.8040688655624,55.9835309302754));
#85889=CARTESIAN_POINT('Ctrl Pts',(4.64411542856985,-31.8381896714642,55.9209438964562));
#85890=CARTESIAN_POINT('Ctrl Pts',(4.64797767043306,-31.8690160524473,55.8566410793345));
#85891=CARTESIAN_POINT('Ctrl Pts',(4.65183991229628,-31.8963929309228,55.7910065828084));
#85892=CARTESIAN_POINT('Ctrl Pts',(4.65570864526733,-31.9238158205691,55.7252617771379));
#85893=CARTESIAN_POINT('Ctrl Pts',(4.65957737823839,-31.947777476992,55.6581812831638));
#85894=CARTESIAN_POINT('Ctrl Pts',(4.66344611120945,-31.9681723975461,55.5901652107992));
#85895=CARTESIAN_POINT('Ctrl Pts',(4.66485786587946,-31.9756147887766,55.565345196465));
#85896=CARTESIAN_POINT('Ctrl Pts',(4.66626962054948,-31.982582718124,55.5404006983024));
#85897=CARTESIAN_POINT('Ctrl Pts',(4.6676813752195,-31.9890727647973,55.515351432366));
#85898=CARTESIAN_POINT('Ctrl Pts',(4.67155044856771,-32.0068594717553,55.4467010858964));
#85899=CARTESIAN_POINT('Ctrl Pts',(4.67541952191592,-32.0211227752712,55.3769943617174));
#85900=CARTESIAN_POINT('Ctrl Pts',(4.67928859526414,-32.0317425864936,55.3066261970678));
#85901=CARTESIAN_POINT('Ctrl Pts',(4.68315190365992,-32.0423465741064,55.2363628815863));
#85902=CARTESIAN_POINT('Ctrl Pts',(4.6870152120557,-32.0493177736078,55.1654405583601));
#85903=CARTESIAN_POINT('Ctrl Pts',(4.69087852045148,-32.0525864868934,55.0942670479159));
#85904=CARTESIAN_POINT('Ctrl Pts',(4.69473729694439,-32.0558513657733,55.02317702846));
#85905=CARTESIAN_POINT('Ctrl Pts',(4.69859607343731,-32.0554223634192,54.9518368899964));
#85906=CARTESIAN_POINT('Ctrl Pts',(4.70245484993022,-32.0512814688225,54.8806605758122));
#85907=CARTESIAN_POINT('Ctrl Pts',(4.70631119551842,-32.0471431828558,54.8095291004098));
#85908=CARTESIAN_POINT('Ctrl Pts',(4.71016754110663,-32.0392976720871,54.7385617283511));
#85909=CARTESIAN_POINT('Ctrl Pts',(4.71402388669483,-32.0277790060474,54.6681719343797));
#85910=CARTESIAN_POINT('Ctrl Pts',(4.71787909294016,-32.0162637431545,54.5978029368095));
#85911=CARTESIAN_POINT('Ctrl Pts',(4.7217342991855,-32.0010775578611,54.5280116577008));
#85912=CARTESIAN_POINT('Ctrl Pts',(4.72558950543083,-31.9823061136394,54.4592042582196));
#85913=CARTESIAN_POINT('Ctrl Pts',(4.72944486228207,-31.9635339361002,54.3903941707365));
#85914=CARTESIAN_POINT('Ctrl Pts',(4.73330021913332,-31.9411763515419,54.3225685072694));
#85915=CARTESIAN_POINT('Ctrl Pts',(4.73715557598456,-31.9153692105435,54.2561193981545));
#85916=CARTESIAN_POINT('Ctrl Pts',(4.74101496845312,-31.8895350557694,54.1896007330463));
#85917=CARTESIAN_POINT('Ctrl Pts',(4.74487436092168,-31.86024431273,54.1244619524446));
#85918=CARTESIAN_POINT('Ctrl Pts',(4.74873375339024,-31.8276811049241,54.0610754336991));
#85919=CARTESIAN_POINT('Ctrl Pts',(4.75259533099367,-31.7950994602784,53.9976530263795));
#85920=CARTESIAN_POINT('Ctrl Pts',(4.7564569085971,-31.7592419067675,53.9359852760462));
#85921=CARTESIAN_POINT('Ctrl Pts',(4.76031848620054,-31.720337319883,53.8764177518678));
#85922=CARTESIAN_POINT('Ctrl Pts',(4.76418682031541,-31.6813646625586,53.8167460037945));
#85923=CARTESIAN_POINT('Ctrl Pts',(4.76805515443027,-31.639334614274,53.7591822110137));
#85924=CARTESIAN_POINT('Ctrl Pts',(4.77192348854514,-31.5945175083743,53.7040403254778));
#85925=CARTESIAN_POINT('Ctrl Pts',(4.77422120771611,-31.5678969734476,53.6712870617325));
#85926=CARTESIAN_POINT('Ctrl Pts',(4.77651892688708,-31.5402938708371,53.6393876151711));
#85927=CARTESIAN_POINT('Ctrl Pts',(4.77881664605805,-31.5117708171909,53.6084014376301));
#85928=CARTESIAN_POINT('Ctrl Pts',(4.78268571940627,-31.4637415418701,53.5562245679752));
#85929=CARTESIAN_POINT('Ctrl Pts',(4.78655479275449,-31.4129137901361,53.5064349216958));
#85930=CARTESIAN_POINT('Ctrl Pts',(4.79042386610271,-31.3595542340858,53.4593475904412));
#85931=CARTESIAN_POINT('Ctrl Pts',(4.79428717449848,-31.3062741842312,53.4123304197136));
#85932=CARTESIAN_POINT('Ctrl Pts',(4.79815048289426,-31.2504701794635,53.3680078903843));
#85933=CARTESIAN_POINT('Ctrl Pts',(4.80201379129003,-31.1924470458222,53.3266597460738));
#85934=CARTESIAN_POINT('Ctrl Pts',(4.80587256778294,-31.134491976953,53.2853601057278));
#85935=CARTESIAN_POINT('Ctrl Pts',(4.80973134427586,-31.0743233436933,53.2470282003396));
#85936=CARTESIAN_POINT('Ctrl Pts',(4.81359012076877,-31.0122791493054,53.2119036697142));
#85937=CARTESIAN_POINT('Ctrl Pts',(4.81744646635698,-30.9502740407582,53.1768012664099));
#85938=CARTESIAN_POINT('Ctrl Pts',(4.82130281194519,-30.886396136989,53.1449024679027));
#85939=CARTESIAN_POINT('Ctrl Pts',(4.8251591575334,-30.8210112942301,53.1164029047467));
#85940=CARTESIAN_POINT('Ctrl Pts',(4.82901436377874,-30.7556457691784,53.0879117616801));
#85941=CARTESIAN_POINT('Ctrl Pts',(4.83286957002408,-30.6887746341001,53.0628180541669));
#85942=CARTESIAN_POINT('Ctrl Pts',(4.83672477626942,-30.6207855834735,53.041270099822));
#85943=CARTESIAN_POINT('Ctrl Pts',(4.84058013312066,-30.5527938768146,53.0197213036935));
#85944=CARTESIAN_POINT('Ctrl Pts',(4.8444354899719,-30.4836846316526,53.0017186804076));
#85945=CARTESIAN_POINT('Ctrl Pts',(4.84829084682314,-30.4138609742388,52.9873607733868));
#85946=CARTESIAN_POINT('Ctrl Pts',(4.8521502392917,-30.3439642285034,52.9729878371429));
#85947=CARTESIAN_POINT('Ctrl Pts',(4.85600963176026,-30.2733520545143,52.9622673310628));
#85948=CARTESIAN_POINT('Ctrl Pts',(4.85986902422882,-30.2024371646762,52.9552465290755));
#85949=CARTESIAN_POINT('Ctrl Pts',(4.86373060183226,-30.131482123804,52.9482217520068));
#85950=CARTESIAN_POINT('Ctrl Pts',(4.8675921794357,-30.0602245113805,52.944900871601));
#85951=CARTESIAN_POINT('Ctrl Pts',(4.87145375703914,-29.9890787889633,52.9452790238941));
#85952=CARTESIAN_POINT('Ctrl Pts',(4.87532209115401,-29.9178085845504,52.9456578378314));
#85953=CARTESIAN_POINT('Ctrl Pts',(4.87919042526888,-29.8466511461461,52.949748578334));
#85954=CARTESIAN_POINT('Ctrl Pts',(4.88305875938375,-29.7760168575584,52.9574944028468));
#85955=CARTESIAN_POINT('Ctrl Pts',(4.8853564785547,-29.734061391925,52.9620952798522));
#85956=CARTESIAN_POINT('Ctrl Pts',(4.88765419772566,-29.6922903458756,52.9679847345439));
#85957=CARTESIAN_POINT('Ctrl Pts',(4.88995191689662,-29.6507876285087,52.9751424044893));
#85958=CARTESIAN_POINT('Ctrl Pts',(4.89382099024483,-29.5809022135838,52.9871950305765));
#85959=CARTESIAN_POINT('Ctrl Pts',(4.89769006359305,-29.5115046159001,53.0028935228187));
#85960=CARTESIAN_POINT('Ctrl Pts',(4.90155913694126,-29.4430041910448,53.0221847327654));
#85961=CARTESIAN_POINT('Ctrl Pts',(4.90542244533705,-29.3746058324094,53.041447198644));
#85962=CARTESIAN_POINT('Ctrl Pts',(4.90928575373283,-29.3071024568889,53.0642916257024));
#85963=CARTESIAN_POINT('Ctrl Pts',(4.91314906212861,-29.2408944159804,53.0906136391997));
#85964=CARTESIAN_POINT('Ctrl Pts',(4.91700783862152,-29.1747640412532,53.1169047753256));
#85965=CARTESIAN_POINT('Ctrl Pts',(4.92086661511443,-29.1099264321078,53.1466652161715));
#85966=CARTESIAN_POINT('Ctrl Pts',(4.92472539160735,-29.046766241213,53.1797409624977));
#85967=CARTESIAN_POINT('Ctrl Pts',(4.92858173719555,-28.9836458392008,53.2127958721708));
#85968=CARTESIAN_POINT('Ctrl Pts',(4.93243808278376,-28.922201188255,53.2491617188718));
#85969=CARTESIAN_POINT('Ctrl Pts',(4.93629442837197,-28.8627950734064,53.2886372338305));
#85970=CARTESIAN_POINT('Ctrl Pts',(4.9401496346173,-28.803406509872,53.3281010858961));
#85971=CARTESIAN_POINT('Ctrl Pts',(4.94400484086263,-28.7460556911282,53.3706725135537));
#85972=CARTESIAN_POINT('Ctrl Pts',(4.94786004710796,-28.6910774968246,53.4161062399324));
#85973=CARTESIAN_POINT('Ctrl Pts',(4.95171540395921,-28.6360971547653,53.4615417412066));
#85974=CARTESIAN_POINT('Ctrl Pts',(4.95557076081046,-28.5834899942286,53.5098394520461));
#85975=CARTESIAN_POINT('Ctrl Pts',(4.95942611766171,-28.5335574470369,53.5607141349408));
#85976=CARTESIAN_POINT('Ctrl Pts',(4.96328551013027,-28.4835726326598,53.611642071207));
#85977=CARTESIAN_POINT('Ctrl Pts',(4.96714490259882,-28.4362683613669,53.6651520168576));
#85978=CARTESIAN_POINT('Ctrl Pts',(4.97100429506738,-28.3919081904314,53.7209228739054));
#85979=CARTESIAN_POINT('Ctrl Pts',(4.97486587267082,-28.3475229033779,53.7767253076446));
#85980=CARTESIAN_POINT('Ctrl Pts',(4.97872745027425,-28.3060853173042,53.8347908054496));
#85981=CARTESIAN_POINT('Ctrl Pts',(4.98258902787768,-28.267816134846,53.8947685220733));
#85982=CARTESIAN_POINT('Ctrl Pts',(4.98645736199256,-28.2294799937001,53.9548511802959));
#85983=CARTESIAN_POINT('Ctrl Pts',(4.99032569610743,-28.1943235639806,54.0168523145396));
#85984=CARTESIAN_POINT('Ctrl Pts',(4.9941940302223,-28.1625216672198,54.0803963141312));
#85985=CARTESIAN_POINT('Ctrl Pts',(4.99649174939326,-28.1436319266519,54.1181402787747));
#85986=CARTESIAN_POINT('Ctrl Pts',(4.99878946856422,-28.1259247988858,54.1564281827511));
#85987=CARTESIAN_POINT('Ctrl Pts',(5.00108718773517,-28.1094286858362,54.1951784865196));
#85988=CARTESIAN_POINT('Ctrl Pts',(5.00537446195647,-28.0786488755256,54.2674820040745));
#85989=CARTESIAN_POINT('Ctrl Pts',(5.00966173617776,-28.0519849253721,54.3416372137349));
#85990=CARTESIAN_POINT('Ctrl Pts',(5.01394901039905,-28.0296387343026,54.4171843815242));
#85991=CARTESIAN_POINT('Ctrl Pts',(5.01822262075576,-28.0073637622205,54.492490774822));
#85992=CARTESIAN_POINT('Ctrl Pts',(5.02249623111247,-27.9893792307943,54.5691800046957));
#85993=CARTESIAN_POINT('Ctrl Pts',(5.02676984146917,-27.9758386929292,54.6467740589123));
#85994=CARTESIAN_POINT('Ctrl Pts',(5.03102083155028,-27.9623698253084,54.7239574067835));
#85995=CARTESIAN_POINT('Ctrl Pts',(5.03527182163138,-27.9532981584277,54.8020357440809));
#85996=CARTESIAN_POINT('Ctrl Pts',(5.03952281171248,-27.9487267011557,54.88052022787));
#85997=CARTESIAN_POINT('Ctrl Pts',(5.04165696797231,-27.9464316583615,54.919922378706));
#85998=CARTESIAN_POINT('Ctrl Pts',(5.04379112423214,-27.9452700857513,54.9594266319027));
#85999=CARTESIAN_POINT('Ctrl Pts',(5.04592528049197,-27.9452502582983,54.9989697199742));
#86000=CARTESIAN_POINT('Origin',(-1.54592528053767,-30.,55.));
#86001=CARTESIAN_POINT('',(3.89394682683029,-31.2520475724682,56.6292251037768));
#86002=CARTESIAN_POINT('',(3.95204618803132,-31.2520475724682,56.6292251037768));
#86003=CARTESIAN_POINT('',(-1.54592528053767,-31.2520475724682,56.6292251037768));
#86004=CARTESIAN_POINT('',(4.4040747195126,-27.9452505182989,55.0014594345581));
#86005=CARTESIAN_POINT('Ctrl Pts',(3.95204618803132,-31.2520475724682,56.6292251037768));
#86006=CARTESIAN_POINT('Ctrl Pts',(3.9559336202552,-31.3090593123265,56.5854119988066));
#86007=CARTESIAN_POINT('Ctrl Pts',(3.95982105247907,-31.3637505089491,56.5386167090834));
#86008=CARTESIAN_POINT('Ctrl Pts',(3.96370848470294,-31.4158059227235,56.4891242902059));
#86009=CARTESIAN_POINT('Ctrl Pts',(3.96756899535413,-31.467500837967,56.4399746203913));
#86010=CARTESIAN_POINT('Ctrl Pts',(3.97142950600532,-31.5165960683909,56.3881654587326));
#86011=CARTESIAN_POINT('Ctrl Pts',(3.97529001665651,-31.5628213390034,56.3340116284559));
#86012=CARTESIAN_POINT('Ctrl Pts',(3.97919090966672,-31.609530142921,56.2792913292287));
#86013=CARTESIAN_POINT('Ctrl Pts',(3.98309180267694,-31.653308281332,56.2221774226634));
#86014=CARTESIAN_POINT('Ctrl Pts',(3.98699269568715,-31.6939212592051,56.1630255070775));
#86015=CARTESIAN_POINT('Ctrl Pts',(3.99089358869737,-31.7345342370783,56.1038735914916));
#86016=CARTESIAN_POINT('Ctrl Pts',(3.99479448170758,-31.7719818464491,56.0426841312037));
#86017=CARTESIAN_POINT('Ctrl Pts',(3.9986953747178,-31.8060778097422,55.9798369801435));
#86018=CARTESIAN_POINT('Ctrl Pts',(4.00256444806601,-31.8398956515835,55.9175024745466));
#86019=CARTESIAN_POINT('Ctrl Pts',(4.00643352141423,-31.8705488495701,55.8532930462969));
#86020=CARTESIAN_POINT('Ctrl Pts',(4.01030259476244,-31.8978256139735,55.7875630142701));
#86021=CARTESIAN_POINT('Ctrl Pts',(4.01416590315824,-31.9250617357643,55.7219309205539));
#86022=CARTESIAN_POINT('Ctrl Pts',(4.01802921155403,-31.9489312255174,55.6547831654668));
#86023=CARTESIAN_POINT('Ctrl Pts',(4.02189251994982,-31.9692680899005,55.5864987234424));
#86024=CARTESIAN_POINT('Ctrl Pts',(4.02575129644273,-31.9895810978671,55.5182943833482));
#86025=CARTESIAN_POINT('Ctrl Pts',(4.02961007293565,-32.0063695738439,55.4489564682266));
#86026=CARTESIAN_POINT('Ctrl Pts',(4.03346884942856,-32.0195162093906,55.378882359722));
#86027=CARTESIAN_POINT('Ctrl Pts',(4.03732519501676,-32.0326545629811,55.3088523956452));
#86028=CARTESIAN_POINT('Ctrl Pts',(4.04118154060496,-32.0421555385165,55.2380876346409));
#86029=CARTESIAN_POINT('Ctrl Pts',(4.04503788619317,-32.0479524838775,55.1669975636946));
#86030=CARTESIAN_POINT('Ctrl Pts',(4.0488930924385,-32.0537477165527,55.0959284960438));
#86031=CARTESIAN_POINT('Ctrl Pts',(4.05274829868383,-32.0558410521646,55.0245347931743));
#86032=CARTESIAN_POINT('Ctrl Pts',(4.05660350492916,-32.0542176734686,54.9532312870673));
#86033=CARTESIAN_POINT('Ctrl Pts',(4.06045886178041,-32.0525942313542,54.8819249954465));
#86034=CARTESIAN_POINT('Ctrl Pts',(4.06431421863166,-32.0472537999241,54.8107093931939));
#86035=CARTESIAN_POINT('Ctrl Pts',(4.06816957548291,-32.0382336514703,54.7399977990204));
#86036=CARTESIAN_POINT('Ctrl Pts',(4.07202896795147,-32.0292040611233,54.6692121870726));
#86037=CARTESIAN_POINT('Ctrl Pts',(4.07588836042003,-32.0164871263596,54.5989321192276));
#86038=CARTESIAN_POINT('Ctrl Pts',(4.07974775288859,-32.0001717313108,54.5295633860283));
#86039=CARTESIAN_POINT('Ctrl Pts',(4.08360933049202,-31.9838470987099,54.4601553772073));
#86040=CARTESIAN_POINT('Ctrl Pts',(4.08747090809546,-31.9639200857577,54.3916601968677));
#86041=CARTESIAN_POINT('Ctrl Pts',(4.09133248569889,-31.9405294728948,54.3244684113035));
#86042=CARTESIAN_POINT('Ctrl Pts',(4.09520081981376,-31.9170979340271,54.2571590618537));
#86043=CARTESIAN_POINT('Ctrl Pts',(4.09906915392864,-31.8901908793728,54.1911581102852));
#86044=CARTESIAN_POINT('Ctrl Pts',(4.10293748804351,-31.8599949485488,54.1268354371181));
#86045=CARTESIAN_POINT('Ctrl Pts',(4.10523520721445,-31.8420591221496,54.0886289547219));
#86046=CARTESIAN_POINT('Ctrl Pts',(4.1075329263854,-31.8229638179775,54.0510141262206));
#86047=CARTESIAN_POINT('Ctrl Pts',(4.10983064555634,-31.8027554667187,54.0140637496694));
#86048=CARTESIAN_POINT('Ctrl Pts',(4.11369971890456,-31.7687271162329,53.9518439105661));
#86049=CARTESIAN_POINT('Ctrl Pts',(4.11756879225277,-31.7314071723879,53.8912659359024));
#86050=CARTESIAN_POINT('Ctrl Pts',(4.12143786560099,-31.6909784467622,53.8326999292873));
#86051=CARTESIAN_POINT('Ctrl Pts',(4.12530117399678,-31.6506099602838,53.7742211865236));
#86052=CARTESIAN_POINT('Ctrl Pts',(4.12916448239257,-31.6071421603617,53.7177488576869));
#86053=CARTESIAN_POINT('Ctrl Pts',(4.13302779078836,-31.5608034111033,53.663627943128));
#86054=CARTESIAN_POINT('Ctrl Pts',(4.13688656728128,-31.514519020102,53.6095705157939));
#86055=CARTESIAN_POINT('Ctrl Pts',(4.14074534377419,-31.4653706837742,53.5578593909247));
#86056=CARTESIAN_POINT('Ctrl Pts',(4.14460412026711,-31.4136286358637,53.5088086499828));
#86057=CARTESIAN_POINT('Ctrl Pts',(4.14846046585532,-31.3619191837743,53.4597888094254));
#86058=CARTESIAN_POINT('Ctrl Pts',(4.15231681144352,-31.3076196135571,53.413426361147));
#86059=CARTESIAN_POINT('Ctrl Pts',(4.15617315703173,-31.2510378033498,53.3699993935308));
#86060=CARTESIAN_POINT('Ctrl Pts',(4.16002836327706,-31.1944727100266,53.3265852562499));
#86061=CARTESIAN_POINT('Ctrl Pts',(4.16388356952239,-31.1356271005005,53.2861051734572));
#86062=CARTESIAN_POINT('Ctrl Pts',(4.16773877576772,-31.074841456847,53.2487965837336));
#86063=CARTESIAN_POINT('Ctrl Pts',(4.17159413261897,-31.0140534385661,53.2114865365278));
#86064=CARTESIAN_POINT('Ctrl Pts',(4.17544948947023,-30.9513256508629,53.1773484806088));
#86065=CARTESIAN_POINT('Ctrl Pts',(4.17930484632148,-30.8870255559426,53.1465752711252));
#86066=CARTESIAN_POINT('Ctrl Pts',(4.18316423879004,-30.8226581545222,53.1157698496047));
#86067=CARTESIAN_POINT('Ctrl Pts',(4.1870236312586,-30.7567155995411,53.0883365157088));
#86068=CARTESIAN_POINT('Ctrl Pts',(4.19088302372716,-30.6895870208706,53.0644206802234));
#86069=CARTESIAN_POINT('Ctrl Pts',(4.1947446013306,-30.6224204349232,53.0404913039213));
#86070=CARTESIAN_POINT('Ctrl Pts',(4.19860617893403,-30.5540669542196,53.020083529651));
#86071=CARTESIAN_POINT('Ctrl Pts',(4.20246775653747,-30.4849299800429,53.0032925910501));
#86072=CARTESIAN_POINT('Ctrl Pts',(4.20633609065234,-30.4156720385299,52.9864722737391));
#86073=CARTESIAN_POINT('Ctrl Pts',(4.21020442476722,-30.3456283441276,52.9732815166488));
#86074=CARTESIAN_POINT('Ctrl Pts',(4.21407275888209,-30.2752108761978,52.9637641256175));
#86075=CARTESIAN_POINT('Ctrl Pts',(4.21637047805303,-30.2333841980396,52.9581109707501));
#86076=CARTESIAN_POINT('Ctrl Pts',(4.21866819722397,-30.1914257349881,52.9537528354883));
#86077=CARTESIAN_POINT('Ctrl Pts',(4.22096591639491,-30.1494218301972,52.9506901944409));
#86078=CARTESIAN_POINT('Ctrl Pts',(4.22483498974313,-30.0786924779758,52.9455330877756));
#86079=CARTESIAN_POINT('Ctrl Pts',(4.22870406309134,-30.0075572855653,52.9440318803733));
#86080=CARTESIAN_POINT('Ctrl Pts',(4.23257313643956,-29.9364263435633,52.9462337151693));
#86081=CARTESIAN_POINT('Ctrl Pts',(4.23643644483534,-29.8654013872743,52.9484322692126));
#86082=CARTESIAN_POINT('Ctrl Pts',(4.24029975323112,-29.7943811504202,52.9543228983359));
#86083=CARTESIAN_POINT('Ctrl Pts',(4.24416306162689,-29.7237793393138,52.963900859705));
#86084=CARTESIAN_POINT('Ctrl Pts',(4.24802183811981,-29.6532603485566,52.9734675855252));
#86085=CARTESIAN_POINT('Ctrl Pts',(4.25188061461272,-29.5831592876136,52.9867129867537));
#86086=CARTESIAN_POINT('Ctrl Pts',(4.25573939110563,-29.5138865950799,53.0035803747566));
#86087=CARTESIAN_POINT('Ctrl Pts',(4.25959573669383,-29.4446575421079,53.0204371368492));
#86088=CARTESIAN_POINT('Ctrl Pts',(4.26345208228203,-29.3762562930918,53.0409112441354));
#86089=CARTESIAN_POINT('Ctrl Pts',(4.26730842787023,-29.3090834642402,53.064894859933));
#86090=CARTESIAN_POINT('Ctrl Pts',(4.27116363411557,-29.2419304813494,53.0888713898611));
#86091=CARTESIAN_POINT('Ctrl Pts',(4.2750188403609,-29.1760056553523,53.1163552065662));
#86092=CARTESIAN_POINT('Ctrl Pts',(4.27887404660624,-29.1116931339928,53.1471890343846));
#86093=CARTESIAN_POINT('Ctrl Pts',(4.28272940345747,-29.0473781002269,53.1780240667447));
#86094=CARTESIAN_POINT('Ctrl Pts',(4.28658476030871,-28.9846759332392,53.2122091580431));
#86095=CARTESIAN_POINT('Ctrl Pts',(4.29044011715995,-28.9239479573436,53.2495401849814));
#86096=CARTESIAN_POINT('Ctrl Pts',(4.29429950962851,-28.8631564140842,53.2869102883904));
#86097=CARTESIAN_POINT('Ctrl Pts',(4.29815890209707,-28.8043436018006,53.3274326461376));
#86098=CARTESIAN_POINT('Ctrl Pts',(4.30201829456563,-28.7478427364951,53.3708591988561));
#86099=CARTESIAN_POINT('Ctrl Pts',(4.30587987216906,-28.6913098811777,53.4143103390906));
#86100=CARTESIAN_POINT('Ctrl Pts',(4.30974144977248,-28.6370919480339,53.4606686317744));
#86101=CARTESIAN_POINT('Ctrl Pts',(4.31360302737591,-28.5854877373587,53.5096468132227));
#86102=CARTESIAN_POINT('Ctrl Pts',(4.31747136149078,-28.5337932360106,53.5587106906423));
#86103=CARTESIAN_POINT('Ctrl Pts',(4.32133969560566,-28.484721922155,53.6104032563999));
#86104=CARTESIAN_POINT('Ctrl Pts',(4.32520802972053,-28.4385340417942,53.664402147402));
#86105=CARTESIAN_POINT('Ctrl Pts',(4.32750574889151,-28.4110992921008,53.6964764934597));
#86106=CARTESIAN_POINT('Ctrl Pts',(4.32980346806249,-28.3846810693941,53.7293639298705));
#86107=CARTESIAN_POINT('Ctrl Pts',(4.33210118723346,-28.3593266018392,53.7629921734008));
#86108=CARTESIAN_POINT('Ctrl Pts',(4.33598223894953,-28.3165006546754,53.8197932628943));
#86109=CARTESIAN_POINT('Ctrl Pts',(4.3398632906656,-28.276542709681,53.8789338902987));
#86110=CARTESIAN_POINT('Ctrl Pts',(4.34374434238166,-28.239716878203,53.9400939222665));
#86111=CARTESIAN_POINT('Ctrl Pts',(4.3476196054084,-28.202945973408,54.0011627324598));
#86112=CARTESIAN_POINT('Ctrl Pts',(4.35149486843514,-28.1692981577279,54.0642445616429));
#86113=CARTESIAN_POINT('Ctrl Pts',(4.35537013146187,-28.1389961109829,54.1289878947091));
#86114=CARTESIAN_POINT('Ctrl Pts',(4.35942884712858,-28.1072595834212,54.1967961385411));
#86115=CARTESIAN_POINT('Ctrl Pts',(4.36348756279528,-28.0791938035533,54.2664266821926));
#86116=CARTESIAN_POINT('Ctrl Pts',(4.36754627846199,-28.0550020434944,54.3374439558126));
#86117=CARTESIAN_POINT('Ctrl Pts',(4.37141366678501,-28.031950679948,54.4051134841278));
#86118=CARTESIAN_POINT('Ctrl Pts',(4.37528105510803,-28.0124165131011,54.4740414408055));
#86119=CARTESIAN_POINT('Ctrl Pts',(4.37914844343105,-27.9965263590061,54.5438301496782));
#86120=CARTESIAN_POINT('Ctrl Pts',(4.38301406018559,-27.9806434838534,54.6135868898248));
#86121=CARTESIAN_POINT('Ctrl Pts',(4.38687967694012,-27.9684014102057,54.6842031295399));
#86122=CARTESIAN_POINT('Ctrl Pts',(4.39074529369465,-27.9598764862882,54.7552682870977));
#86123=CARTESIAN_POINT('Ctrl Pts',(4.39461092103558,-27.9513515390242,54.8263336392748));
#86124=CARTESIAN_POINT('Ctrl Pts',(4.3984765483765,-27.9465438214084,54.8978474341102));
#86125=CARTESIAN_POINT('Ctrl Pts',(4.40234217571742,-27.9454779738573,54.9693927035768));
#86126=CARTESIAN_POINT('Ctrl Pts',(4.40291969029905,-27.9453187390298,54.980081379106));
#86127=CARTESIAN_POINT('Ctrl Pts',(4.40349720488069,-27.9452429264143,54.9907707532347));
#86128=CARTESIAN_POINT('Ctrl Pts',(4.40407471946232,-27.9452505182983,55.0014594336275));
#86129=CARTESIAN_POINT('Ctrl Pts',(4.4040747195126,-27.9452505182989,55.0014594345581));
#86130=CARTESIAN_POINT('Ctrl Pts',(4.4084909580683,-27.9453085732694,55.08319548757));
#86131=CARTESIAN_POINT('Ctrl Pts',(4.412907196624,-27.9502477237087,55.1647368982363));
#86132=CARTESIAN_POINT('Ctrl Pts',(4.4173234351797,-27.9599745962983,55.2455481923198));
#86133=CARTESIAN_POINT('Ctrl Pts',(4.42177971598848,-27.9697896629219,55.3270922063976));
#86134=CARTESIAN_POINT('Ctrl Pts',(4.42623599679726,-27.9844795567315,55.4078926142017));
#86135=CARTESIAN_POINT('Ctrl Pts',(4.43069227760603,-28.0038986271126,55.4874185795155));
#86136=CARTESIAN_POINT('Ctrl Pts',(4.4348736710947,-28.0221198249975,55.5620389564201));
#86137=CARTESIAN_POINT('Ctrl Pts',(4.43905506458337,-28.0445042064936,55.6355373428858));
#86138=CARTESIAN_POINT('Ctrl Pts',(4.44323645807203,-28.0708935156209,55.7074925684604));
#86139=CARTESIAN_POINT('Ctrl Pts',(4.44710553142025,-28.0953117323947,55.7740732541313));
#86140=CARTESIAN_POINT('Ctrl Pts',(4.45097460476847,-28.1232287475473,55.8395187237065));
#86141=CARTESIAN_POINT('Ctrl Pts',(4.45484367811668,-28.1545186966464,55.9034358424772));
#86142=CARTESIAN_POINT('Ctrl Pts',(4.45870698651247,-28.1857620234534,55.9672577241934));
#86143=CARTESIAN_POINT('Ctrl Pts',(4.46257029490826,-28.2203680964815,56.0295553426381));
#86144=CARTESIAN_POINT('Ctrl Pts',(4.46643360330405,-28.2581622778494,56.0899536284601));
#86145=CARTESIAN_POINT('Ctrl Pts',(4.47029237979696,-28.2959121242739,56.1502810633075));
#86146=CARTESIAN_POINT('Ctrl Pts',(4.47415115628987,-28.3368423939923,56.2087131813576));
#86147=CARTESIAN_POINT('Ctrl Pts',(4.47800993278279,-28.3807324547549,56.2648992763916));
#86148=CARTESIAN_POINT('Ctrl Pts',(4.48186627837099,-28.4245948661951,56.3210499759982));
#86149=CARTESIAN_POINT('Ctrl Pts',(4.4857226239592,-28.4714130710555,56.3749570778475));
#86150=CARTESIAN_POINT('Ctrl Pts',(4.48957896954741,-28.5209238681732,56.4262998838815));
#86151=CARTESIAN_POINT('Ctrl Pts',(4.49343417579274,-28.5704200375111,56.4776275208756));
#86152=CARTESIAN_POINT('Ctrl Pts',(4.49728938203808,-28.6226068827627,56.5263920166291));
#86153=CARTESIAN_POINT('Ctrl Pts',(4.50114458828341,-28.6771829274445,56.5723080344054));
#86154=CARTESIAN_POINT('Ctrl Pts',(4.50499994513465,-28.7317611041718,56.6182258459181));
#86155=CARTESIAN_POINT('Ctrl Pts',(4.5088553019859,-28.78872829249,56.6612946474706));
#86156=CARTESIAN_POINT('Ctrl Pts',(4.51271065883715,-28.8477497183875,56.7012691882897));
#86157=CARTESIAN_POINT('Ctrl Pts',(4.5165700513057,-28.9068329253074,56.741285572693));
#86158=CARTESIAN_POINT('Ctrl Pts',(4.52042944377426,-28.9679742592192,56.7782009577455));
#86159=CARTESIAN_POINT('Ctrl Pts',(4.52428883624282,-29.0308104776657,56.8118137962543));
#86160=CARTESIAN_POINT('Ctrl Pts',(4.52815041384626,-29.093682273114,56.8454456658895));
#86161=CARTESIAN_POINT('Ctrl Pts',(4.5320119914497,-29.1582504234921,56.875771060062));
#86162=CARTESIAN_POINT('Ctrl Pts',(4.53587356905313,-29.2241301267154,56.9026359352828));
#86163=CARTESIAN_POINT('Ctrl Pts',(4.53974190316801,-29.2901250981046,56.9295478153433));
#86164=CARTESIAN_POINT('Ctrl Pts',(4.54361023728288,-29.3574357450478,56.9529869280872));
#86165=CARTESIAN_POINT('Ctrl Pts',(4.54747857139775,-29.4256611505313,56.9728488154167));
#86166=CARTESIAN_POINT('Ctrl Pts',(4.5497762905687,-29.4661857839962,56.9846464104364));
#86167=CARTESIAN_POINT('Ctrl Pts',(4.55207400973964,-29.5070329226997,56.995182881589));
#86168=CARTESIAN_POINT('Ctrl Pts',(4.55437172891058,-29.5481172499469,57.0044449462892));
#86169=CARTESIAN_POINT('Ctrl Pts',(4.5584403036961,-29.6208653298829,57.0208452981589));
#86170=CARTESIAN_POINT('Ctrl Pts',(4.56250887848163,-29.694657290038,57.0333138861912));
#86171=CARTESIAN_POINT('Ctrl Pts',(4.56657745326715,-29.7690292171383,57.0417272246714));
#86172=CARTESIAN_POINT('Ctrl Pts',(4.57043978099225,-29.8396310300953,57.0497140682679));
#86173=CARTESIAN_POINT('Ctrl Pts',(4.57430210871735,-29.9107548818677,57.0540466921404));
#86174=CARTESIAN_POINT('Ctrl Pts',(4.57816443644246,-29.9819907734414,57.0546710759289));
#86175=CARTESIAN_POINT('Ctrl Pts',(4.58202297528157,-30.0531567836661,57.0552948472062));
#86176=CARTESIAN_POINT('Ctrl Pts',(4.58588151412069,-30.1244341324307,57.0522175912601));
#86177=CARTESIAN_POINT('Ctrl Pts',(4.5897400529598,-30.195408480989,57.0454371386228));
#86178=CARTESIAN_POINT('Ctrl Pts',(4.59359609750262,-30.2663369492122,57.0386610691105));
#86179=CARTESIAN_POINT('Ctrl Pts',(4.59745214204543,-30.3369623236069,57.0281866006375));
#86180=CARTESIAN_POINT('Ctrl Pts',(4.60130818658824,-30.4068727827817,57.0140635792178));
#86181=CARTESIAN_POINT('Ctrl Pts',(4.60516302838442,-30.4767614360441,56.9999449629381));
#86182=CARTESIAN_POINT('Ctrl Pts',(4.6090178701806,-30.5459351414517,56.9821801512765));
#86183=CARTESIAN_POINT('Ctrl Pts',(4.61287271197679,-30.6139914127986,56.9608702423948));
#86184=CARTESIAN_POINT('Ctrl Pts',(4.61672933960932,-30.6820792126415,56.9395504612507));
#86185=CARTESIAN_POINT('Ctrl Pts',(4.62058596724186,-30.7490480793185,56.9146824445157));
#86186=CARTESIAN_POINT('Ctrl Pts',(4.6244425948744,-30.8145110068051,56.8864170753821));
#86187=CARTESIAN_POINT('Ctrl Pts',(4.62830025678897,-30.8799914903373,56.8581441259565));
#86188=CARTESIAN_POINT('Ctrl Pts',(4.63215791870355,-30.9439647915131,56.8264722186575));
#86189=CARTESIAN_POINT('Ctrl Pts',(4.63601558061812,-31.0060663917418,56.7915992793891));
#86190=CARTESIAN_POINT('Ctrl Pts',(4.63987770191324,-31.0682397801868,56.7566860276956));
#86191=CARTESIAN_POINT('Ctrl Pts',(4.64373982320836,-31.1285367355297,56.7185646133584));
#86192=CARTESIAN_POINT('Ctrl Pts',(4.64760194450348,-31.1866206266542,56.6774769896779));
#86193=CARTESIAN_POINT('Ctrl Pts',(4.64907380425668,-31.208756477686,56.6618184396146));
#86194=CARTESIAN_POINT('Ctrl Pts',(4.65054566400989,-31.2305712397288,56.6457295083612));
#86195=CARTESIAN_POINT('Ctrl Pts',(4.65201752376309,-31.2520475724682,56.6292251037768));
#86196=CARTESIAN_POINT('',(4.34592528058805,-27.945250355841,54.9987907322123));
#86197=CARTESIAN_POINT('Ctrl Pts',(4.34592528058805,-27.945250355841,54.9987907322123));
#86198=CARTESIAN_POINT('Ctrl Pts',(4.34974237135585,-27.9452091140517,55.0688674784532));
#86199=CARTESIAN_POINT('Ctrl Pts',(4.35355946212366,-27.9487570283881,55.1390874484566));
#86200=CARTESIAN_POINT('Ctrl Pts',(4.35737655289147,-27.9559116838072,55.2090466888138));
#86201=CARTESIAN_POINT('Ctrl Pts',(4.36118805254387,-27.9630558593854,55.2789034557927));
#86202=CARTESIAN_POINT('Ctrl Pts',(4.36499955219628,-27.9737962381248,55.3484997581351));
#86203=CARTESIAN_POINT('Ctrl Pts',(4.36881105184868,-27.9880983872791,55.4174319863537));
#86204=CARTESIAN_POINT('Ctrl Pts',(4.37261948474161,-28.0023890288235,55.4863087512157));
#86205=CARTESIAN_POINT('Ctrl Pts',(4.37642791763454,-28.0202356597722,55.5545220139039));
#86206=CARTESIAN_POINT('Ctrl Pts',(4.38023635052746,-28.0415522620219,55.6216751725046));
#86207=CARTESIAN_POINT('Ctrl Pts',(4.38404307118795,-28.0628592805455,55.6887981397326));
#86208=CARTESIAN_POINT('Ctrl Pts',(4.38784979184843,-28.0876330256997,55.754861472588));
#86209=CARTESIAN_POINT('Ctrl Pts',(4.39165651250891,-28.1157372762022,55.8194824892615));
#86210=CARTESIAN_POINT('Ctrl Pts',(4.39546287300828,-28.1438388677079,55.8840973920172));
#86211=CARTESIAN_POINT('Ctrl Pts',(4.39926923350764,-28.1752701383301,55.94726979215));
#86212=CARTESIAN_POINT('Ctrl Pts',(4.40307559400701,-28.2098469931588,56.0086375833754));
#86213=CARTESIAN_POINT('Ctrl Pts',(4.40688551322989,-28.244456175316,56.0700627498815));
#86214=CARTESIAN_POINT('Ctrl Pts',(4.41069543245276,-28.2822165682394,56.1296795024771));
#86215=CARTESIAN_POINT('Ctrl Pts',(4.41450535167564,-28.3228989571176,56.187151908756));
#86216=CARTESIAN_POINT('Ctrl Pts',(4.41831711300167,-28.3636010160079,56.2446521030519));
#86217=CARTESIAN_POINT('Ctrl Pts',(4.42212887432769,-28.4072275723938,56.3000054956357));
#86218=CARTESIAN_POINT('Ctrl Pts',(4.42594063565372,-28.4535088401571,56.352908960362));
#86219=CARTESIAN_POINT('Ctrl Pts',(4.42975910316214,-28.4998715323844,56.4059055002451));
#86220=CARTESIAN_POINT('Ctrl Pts',(4.43357757067055,-28.5488979118374,56.4564431490458));
#86221=CARTESIAN_POINT('Ctrl Pts',(4.43739603817897,-28.6002816355939,56.5042559831506));
#86222=CARTESIAN_POINT('Ctrl Pts',(4.44006763663344,-28.6362323610277,56.5377083284741));
#86223=CARTESIAN_POINT('Ctrl Pts',(4.44273923508791,-28.673336292221,56.569827654895));
#86224=CARTESIAN_POINT('Ctrl Pts',(4.44541083354238,-28.7114798816251,56.6005353688822));
#86225=CARTESIAN_POINT('Ctrl Pts',(4.44927990689059,-28.766720348216,56.6450070212647));
#86226=CARTESIAN_POINT('Ctrl Pts',(4.45314898023881,-28.8243740439197,56.6867025917087));
#86227=CARTESIAN_POINT('Ctrl Pts',(4.45701805358702,-28.8841304900814,56.7253500512459));
#86228=CARTESIAN_POINT('Ctrl Pts',(4.46088136198281,-28.9437978986266,56.7639399257373));
#86229=CARTESIAN_POINT('Ctrl Pts',(4.4647446703786,-29.0055614338965,56.7994904428258));
#86230=CARTESIAN_POINT('Ctrl Pts',(4.46860797877438,-29.0690781313598,56.8317701921877));
#86231=CARTESIAN_POINT('Ctrl Pts',(4.4724667552673,-29.1325203197562,56.8640120753805));
#86232=CARTESIAN_POINT('Ctrl Pts',(4.47632553176021,-29.1977111543371,56.8929905930389));
#86233=CARTESIAN_POINT('Ctrl Pts',(4.48018430825312,-29.2642808120641,56.9185189180727));
#86234=CARTESIAN_POINT('Ctrl Pts',(4.48404065384133,-29.3308085330541,56.9440311610853));
#86235=CARTESIAN_POINT('Ctrl Pts',(4.48789699942954,-29.3987129013682,56.9660973501538));
#86236=CARTESIAN_POINT('Ctrl Pts',(4.49175334501774,-29.467603080323,56.984578313501));
#86237=CARTESIAN_POINT('Ctrl Pts',(4.49560855126307,-29.5364729059322,57.0030538167168));
#86238=CARTESIAN_POINT('Ctrl Pts',(4.4994637575084,-29.6063274950219,57.0179460712977));
#86239=CARTESIAN_POINT('Ctrl Pts',(4.50331896375372,-29.6767614356548,57.0291659353094));
#86240=CARTESIAN_POINT('Ctrl Pts',(4.50717432060498,-29.7471981278316,57.0403862376318));
#86241=CARTESIAN_POINT('Ctrl Pts',(4.51102967745623,-29.818213736402,57.0479337903106));
#86242=CARTESIAN_POINT('Ctrl Pts',(4.51488503430748,-29.8893949749598,57.0517709645416));
#86243=CARTESIAN_POINT('Ctrl Pts',(4.51874442677604,-29.9606507228948,57.0556121553571));
#86244=CARTESIAN_POINT('Ctrl Pts',(4.5226038192446,-30.0320719608352,57.0557351884641));
#86245=CARTESIAN_POINT('Ctrl Pts',(4.52646321171316,-30.1032435307008,57.0521545594493));
#86246=CARTESIAN_POINT('Ctrl Pts',(4.5303247893166,-30.1744553969293,57.0485719031316));
#86247=CARTESIAN_POINT('Ctrl Pts',(4.53418636692003,-30.2454168302103,57.0412814599577));
#86248=CARTESIAN_POINT('Ctrl Pts',(4.53804794452347,-30.3157186798858,57.0303495456869));
#86249=CARTESIAN_POINT('Ctrl Pts',(4.54191627863834,-30.3861435350528,57.0193985041031));
#86250=CARTESIAN_POINT('Ctrl Pts',(4.54578461275322,-30.4559060268755,57.0047933703203));
#86251=CARTESIAN_POINT('Ctrl Pts',(4.54965294686809,-30.5246087508623,56.9866512580266));
#86252=CARTESIAN_POINT('Ctrl Pts',(4.55195066603904,-30.5654169027212,56.9758751776828));
#86253=CARTESIAN_POINT('Ctrl Pts',(4.55424838520998,-30.6058514534182,56.9638521549951));
#86254=CARTESIAN_POINT('Ctrl Pts',(4.55654610438093,-30.6458324446948,56.9506147789555));
#86255=CARTESIAN_POINT('Ctrl Pts',(4.56041440940484,-30.7131420930502,56.9283291102433));
#86256=CARTESIAN_POINT('Ctrl Pts',(4.56428271442874,-30.7794286896822,56.90251174025));
#86257=CARTESIAN_POINT('Ctrl Pts',(4.56815101945265,-30.8442955339711,56.8732759043495));
#86258=CARTESIAN_POINT('Ctrl Pts',(4.57201426849278,-30.9090775954649,56.8440782805111));
#86259=CARTESIAN_POINT('Ctrl Pts',(4.57587751753291,-30.9724431452942,56.8114712484202));
#86260=CARTESIAN_POINT('Ctrl Pts',(4.57974076657305,-31.0340117676843,56.7756174212905));
#86261=CARTESIAN_POINT('Ctrl Pts',(4.58359955334054,-31.0955092748095,56.7398050073729));
#86262=CARTESIAN_POINT('Ctrl Pts',(4.58745834010803,-31.1552135590635,56.7007534901102));
#86263=CARTESIAN_POINT('Ctrl Pts',(4.59131712687552,-31.2127670719809,56.6586722375499));
#86264=CARTESIAN_POINT('Ctrl Pts',(4.59220268568774,-31.2259751147179,56.6490149472462));
#86265=CARTESIAN_POINT('Ctrl Pts',(4.59308824449995,-31.239069989523,56.6391982813232));
#86266=CARTESIAN_POINT('Ctrl Pts',(4.59397380331217,-31.2520475724682,56.6292251037768));
#86267=CARTESIAN_POINT('Ctrl Pts',(3.89394682683029,-31.2520475724682,56.6292251037768));
#86268=CARTESIAN_POINT('Ctrl Pts',(3.89781364274067,-31.3083220096347,56.585978610531));
#86269=CARTESIAN_POINT('Ctrl Pts',(3.90168045865106,-31.3624548341262,56.5397349396832));
#86270=CARTESIAN_POINT('Ctrl Pts',(3.90554727456145,-31.4141101763284,56.4907347086938));
#86271=CARTESIAN_POINT('Ctrl Pts',(3.90951904437923,-31.4671675583813,56.4404045034247));
#86272=CARTESIAN_POINT('Ctrl Pts',(3.91349081419701,-31.5176105505212,56.3871661673033));
#86273=CARTESIAN_POINT('Ctrl Pts',(3.91746258401478,-31.5651093206311,56.3313265478363));
#86274=CARTESIAN_POINT('Ctrl Pts',(3.92132025531689,-31.6112435758234,56.2770910539831));
#86275=CARTESIAN_POINT('Ctrl Pts',(3.925177926619,-31.6546001507359,56.2204021165531));
#86276=CARTESIAN_POINT('Ctrl Pts',(3.9290355979211,-31.6949138887671,56.1615784399533));
#86277=CARTESIAN_POINT('Ctrl Pts',(3.93289134398468,-31.7352075075202,56.102784120341));
#86278=CARTESIAN_POINT('Ctrl Pts',(3.93674709004826,-31.7724610285617,56.0418575757432));
#86279=CARTESIAN_POINT('Ctrl Pts',(3.94060283611184,-31.8064511104346,55.9791485832649));
#86280=CARTESIAN_POINT('Ctrl Pts',(3.94445794771281,-31.840435599243,55.9164499095448));
#86281=CARTESIAN_POINT('Ctrl Pts',(3.94831305931377,-31.8711574843615,55.8519697976937));
#86282=CARTESIAN_POINT('Ctrl Pts',(3.95216817091473,-31.8984389755367,55.7860833407873));
#86283=CARTESIAN_POINT('Ctrl Pts',(3.95622663585418,-31.9271595384907,55.7167214381973));
#86284=CARTESIAN_POINT('Ctrl Pts',(3.96028510079364,-31.9520664883309,55.6458012669927));
#86285=CARTESIAN_POINT('Ctrl Pts',(3.96434356573309,-31.9730105582645,55.573782972453));
#86286=CARTESIAN_POINT('Ctrl Pts',(3.96820378433556,-31.9929315603121,55.5052825999111));
#86287=CARTESIAN_POINT('Ctrl Pts',(3.97206400293803,-32.0092677198864,55.4357893832784));
#86288=CARTESIAN_POINT('Ctrl Pts',(3.9759242215405,-32.0219428275483,55.3657113132323));
#86289=CARTESIAN_POINT('Ctrl Pts',(3.97978713969793,-32.0346267992547,55.2955842357021));
#86290=CARTESIAN_POINT('Ctrl Pts',(3.98365005785536,-32.0436445648653,55.2248719723876));
#86291=CARTESIAN_POINT('Ctrl Pts',(3.98751297601278,-32.0489717734689,55.1539877723317));
#86292=CARTESIAN_POINT('Ctrl Pts',(3.99138214984943,-32.05430760905,55.0829887811258));
#86293=CARTESIAN_POINT('Ctrl Pts',(3.99525132368607,-32.0559409588887,55.0118177819486));
#86294=CARTESIAN_POINT('Ctrl Pts',(3.99912049752272,-32.0538995184525,54.9408871367581));
#86295=CARTESIAN_POINT('Ctrl Pts',(3.99970358174452,-32.053591873524,54.9301978935761));
#86296=CARTESIAN_POINT('Ctrl Pts',(4.00028666596633,-32.0532008679053,54.9195140956756));
#86297=CARTESIAN_POINT('Ctrl Pts',(4.00086975018814,-32.052726697614,54.90883713803));
#86298=CARTESIAN_POINT('Ctrl Pts',(4.00473882353635,-32.0495803260131,54.837989856074));
#86299=CARTESIAN_POINT('Ctrl Pts',(4.00860789688457,-32.0427556783592,54.7671668837602));
#86300=CARTESIAN_POINT('Ctrl Pts',(4.01247697023278,-32.0322538737086,54.6967810109899));
#86301=CARTESIAN_POINT('Ctrl Pts',(4.01634027862857,-32.021767716837,54.6265000137729));
#86302=CARTESIAN_POINT('Ctrl Pts',(4.02020358702435,-32.0076153497239,54.5566552998756));
#86303=CARTESIAN_POINT('Ctrl Pts',(4.02406689542014,-31.9898498441324,54.4876571847812));
#86304=CARTESIAN_POINT('Ctrl Pts',(4.02792567191305,-31.9721051785923,54.4187400088001));
#86305=CARTESIAN_POINT('Ctrl Pts',(4.03178444840596,-31.9507559140857,54.3506679271215));
#86306=CARTESIAN_POINT('Ctrl Pts',(4.03564322489888,-31.9259063300413,54.2838419375536));
#86307=CARTESIAN_POINT('Ctrl Pts',(4.03949957048708,-31.9010724004332,54.2170580462034));
#86308=CARTESIAN_POINT('Ctrl Pts',(4.04335591607529,-31.8727426950614,54.1515191437889));
#86309=CARTESIAN_POINT('Ctrl Pts',(4.04721226166349,-31.8410711425108,54.0876104939698));
#86310=CARTESIAN_POINT('Ctrl Pts',(4.05106746790882,-31.8094089472018,54.0237207257222));
#86311=CARTESIAN_POINT('Ctrl Pts',(4.05492267415416,-31.7744070804402,53.9614606888879));
#86312=CARTESIAN_POINT('Ctrl Pts',(4.05877788039949,-31.7362666457037,53.9011935122521));
#86313=CARTESIAN_POINT('Ctrl Pts',(4.06263323725073,-31.6981247209885,53.8409239812434));
#86314=CARTESIAN_POINT('Ctrl Pts',(4.06648859410198,-31.6568442465144,53.7826478743105));
#86315=CARTESIAN_POINT('Ctrl Pts',(4.07034395095323,-31.6126701841896,53.7267001768924));
#86316=CARTESIAN_POINT('Ctrl Pts',(4.07420334342179,-31.5684498824069,53.670693915895));
#86317=CARTESIAN_POINT('Ctrl Pts',(4.07806273589035,-31.5213302481,53.6170213118137));
#86318=CARTESIAN_POINT('Ctrl Pts',(4.0819221283589,-31.4715965922107,53.5659842984493));
#86319=CARTESIAN_POINT('Ctrl Pts',(4.08578370596234,-31.4218347778102,53.5149183886306));
#86320=CARTESIAN_POINT('Ctrl Pts',(4.08964528356578,-31.3694563524205,53.4664913700495));
#86321=CARTESIAN_POINT('Ctrl Pts',(4.09350686116921,-31.3147815393855,53.4209664138496));
#86322=CARTESIAN_POINT('Ctrl Pts',(4.09737519528408,-31.2600110631172,53.3753618037054));
#86323=CARTESIAN_POINT('Ctrl Pts',(4.10124352939895,-31.2029365664032,53.332669684726));
#86324=CARTESIAN_POINT('Ctrl Pts',(4.10511186351382,-31.1439086244318,53.2931108350421));
#86325=CARTESIAN_POINT('Ctrl Pts',(4.10740958268478,-31.1088471147839,53.2696136073983));
#86326=CARTESIAN_POINT('Ctrl Pts',(4.10970730185574,-31.0730969193769,53.2472209860021));
#86327=CARTESIAN_POINT('Ctrl Pts',(4.1120050210267,-31.036735346744,53.2259714254524));
#86328=CARTESIAN_POINT('Ctrl Pts',(4.11587409437492,-30.9755069802181,53.1901898080018));
#86329=CARTESIAN_POINT('Ctrl Pts',(4.11974316772313,-30.9123040724541,53.1575116551603));
#86330=CARTESIAN_POINT('Ctrl Pts',(4.12361224107135,-30.8474740331644,53.1281599091771));
#86331=CARTESIAN_POINT('Ctrl Pts',(4.12747554946714,-30.7827405911886,53.0988518975468));
#86332=CARTESIAN_POINT('Ctrl Pts',(4.13133885786292,-30.7163852690689,53.0728606532385));
#86333=CARTESIAN_POINT('Ctrl Pts',(4.13520216625871,-30.6487815749337,53.0503641287341));
#86334=CARTESIAN_POINT('Ctrl Pts',(4.13906094275162,-30.5812571841686,53.027893994063));
#86335=CARTESIAN_POINT('Ctrl Pts',(4.14291971924454,-30.5124877889161,53.008910588793));
#86336=CARTESIAN_POINT('Ctrl Pts',(4.14677849573745,-30.4428668423189,52.9935437900431));
#86337=CARTESIAN_POINT('Ctrl Pts',(4.15063484132565,-30.373289754672,52.9781866718808));
#86338=CARTESIAN_POINT('Ctrl Pts',(4.15449118691386,-30.3028626532351,52.9664417444936));
#86339=CARTESIAN_POINT('Ctrl Pts',(4.15834753250207,-30.2319927001259,52.9583886389451));
#86340=CARTESIAN_POINT('Ctrl Pts',(4.1622027387474,-30.1611436852792,52.9503379126565));
#86341=CARTESIAN_POINT('Ctrl Pts',(4.16605794499273,-30.0898525609284,52.9459768976138));
#86342=CARTESIAN_POINT('Ctrl Pts',(4.16991315123807,-30.018533478687,52.945333586037));
#86343=CARTESIAN_POINT('Ctrl Pts',(4.17376850808931,-29.9472116103234,52.9446902493287));
#86344=CARTESIAN_POINT('Ctrl Pts',(4.17762386494056,-29.8758622676869,52.9477649066092));
#86345=CARTESIAN_POINT('Ctrl Pts',(4.18147922179181,-29.8048997451773,52.9545334387803));
#86346=CARTESIAN_POINT('Ctrl Pts',(4.18533861426037,-29.7338629422326,52.9613090559519));
#86347=CARTESIAN_POINT('Ctrl Pts',(4.18919800672893,-29.6632142522808,52.9717862203667));
#86348=CARTESIAN_POINT('Ctrl Pts',(4.19305739919749,-29.5933620854676,52.9858889879243));
#86349=CARTESIAN_POINT('Ctrl Pts',(4.19691897680093,-29.5234703693193,52.9999997402747));
#86350=CARTESIAN_POINT('Ctrl Pts',(4.20078055440436,-29.4543765448197,53.0177400613253));
#86351=CARTESIAN_POINT('Ctrl Pts',(4.2046421320078,-29.3864753911509,53.0389836520731));
#86352=CARTESIAN_POINT('Ctrl Pts',(4.20851046612267,-29.3184554324318,53.0602644122316));
#86353=CARTESIAN_POINT('Ctrl Pts',(4.21237880023754,-29.251632766462,53.085060510933));
#86354=CARTESIAN_POINT('Ctrl Pts',(4.21624713435242,-29.1863830179574,53.11319715682));
#86355=CARTESIAN_POINT('Ctrl Pts',(4.21854485352336,-29.1476258698967,53.1299098059194));
#86356=CARTESIAN_POINT('Ctrl Pts',(4.22084257269431,-29.1094232312377,53.1478001486803));
#86357=CARTESIAN_POINT('Ctrl Pts',(4.22314029186526,-29.0718493387358,53.1668240912299));
#86358=CARTESIAN_POINT('Ctrl Pts',(4.22700936521348,-29.0085795763097,53.1988580447381));
#86359=CARTESIAN_POINT('Ctrl Pts',(4.23087843856169,-28.9468462494311,53.2342341040927));
#86360=CARTESIAN_POINT('Ctrl Pts',(4.23474751190991,-28.8870250841456,53.2727813111309));
#86361=CARTESIAN_POINT('Ctrl Pts',(4.2386108203057,-28.8272930529087,53.3112710825003));
#86362=CARTESIAN_POINT('Ctrl Pts',(4.24247412870148,-28.7694679328314,53.3529223615004));
#86363=CARTESIAN_POINT('Ctrl Pts',(4.24633743709726,-28.7139018069396,53.3975178627183));
#86364=CARTESIAN_POINT('Ctrl Pts',(4.25019621359018,-28.6584008635959,53.4420610506184));
#86365=CARTESIAN_POINT('Ctrl Pts',(4.25405499008309,-28.6051540277786,53.4895412978216));
#86366=CARTESIAN_POINT('Ctrl Pts',(4.25791376657601,-28.5544838097663,53.5396984878894));
#86367=CARTESIAN_POINT('Ctrl Pts',(4.26177011216421,-28.5038455123568,53.5898240805457));
#86368=CARTESIAN_POINT('Ctrl Pts',(4.26562645775242,-28.4557809568072,53.6426229293585));
#86369=CARTESIAN_POINT('Ctrl Pts',(4.26948280334063,-28.4105778747521,53.6977961487261));
#86370=CARTESIAN_POINT('Ctrl Pts',(4.27333800958596,-28.3653881477785,53.7529530673726));
#86371=CARTESIAN_POINT('Ctrl Pts',(4.27719321583129,-28.3230585236238,53.8104825883364));
#86372=CARTESIAN_POINT('Ctrl Pts',(4.28104842207662,-28.2838371407325,53.8700519467822));
#86373=CARTESIAN_POINT('Ctrl Pts',(4.28490377892787,-28.2446142256346,53.9296236323401));
#86374=CARTESIAN_POINT('Ctrl Pts',(4.28875913577911,-28.2085000581779,53.9912349066408));
#86375=CARTESIAN_POINT('Ctrl Pts',(4.29261449263036,-28.1756990732606,54.0545246215803));
#86376=CARTESIAN_POINT('Ctrl Pts',(4.29647388509892,-28.1428637537207,54.1178805853988));
#86377=CARTESIAN_POINT('Ctrl Pts',(4.30033327756748,-28.1133487638018,54.1829180648716));
#86378=CARTESIAN_POINT('Ctrl Pts',(4.30419267003604,-28.0873118065526,54.249252747493));
#86379=CARTESIAN_POINT('Ctrl Pts',(4.30805424763947,-28.0612601075366,54.3156249878983));
#86380=CARTESIAN_POINT('Ctrl Pts',(4.3119158252429,-28.0386905150585,54.3832954324832));
#86381=CARTESIAN_POINT('Ctrl Pts',(4.31577740284633,-28.0197110338744,54.4518639100176));
#86382=CARTESIAN_POINT('Ctrl Pts',(4.3196457369612,-28.0006983447388,54.5205523602032));
#86383=CARTESIAN_POINT('Ctrl Pts',(4.32351407107608,-27.9852884132227,54.5901415059717));
#86384=CARTESIAN_POINT('Ctrl Pts',(4.32738240519095,-27.973538114849,54.6602209680831));
#86385=CARTESIAN_POINT('Ctrl Pts',(4.32968012436191,-27.9665586541727,54.7018468770149));
#86386=CARTESIAN_POINT('Ctrl Pts',(4.33197784353286,-27.9608693712245,54.7436456571904));
#86387=CARTESIAN_POINT('Ctrl Pts',(4.33427556270382,-27.9564734841711,54.7855310241448));
#86388=CARTESIAN_POINT('Ctrl Pts',(4.33815880198177,-27.9490442554461,54.8563190056286));
#86389=CARTESIAN_POINT('Ctrl Pts',(4.34204204125972,-27.9452923123651,54.9274995857473));
#86390=CARTESIAN_POINT('Ctrl Pts',(4.34592528053768,-27.9452503558416,54.9987907312877));
#86391=CARTESIAN_POINT('Origin',(-1.54592528053767,-30.,55.));
#86392=CARTESIAN_POINT('',(3.19386027023256,-31.2520475724682,56.6292251037768));
#86393=CARTESIAN_POINT('',(3.25213375229793,-31.2520475724682,56.6292251037768));
#86394=CARTESIAN_POINT('',(-1.54592528053767,-31.2520475724682,56.6292251037768));
#86395=CARTESIAN_POINT('',(3.70407471941232,-27.9452505355246,54.9985165115458));
#86396=CARTESIAN_POINT('Ctrl Pts',(3.25213375229793,-31.2520475724682,56.6292251037768));
#86397=CARTESIAN_POINT('Ctrl Pts',(3.25599067575063,-31.3085261850896,56.5858217031878));
#86398=CARTESIAN_POINT('Ctrl Pts',(3.25984759920333,-31.3627927451719,56.5394415114278));
#86399=CARTESIAN_POINT('Ctrl Pts',(3.26370452265604,-31.414522935898,56.4903430565874));
#86400=CARTESIAN_POINT('Ctrl Pts',(3.26755992886839,-31.4662327769507,56.4412639161457));
#86401=CARTESIAN_POINT('Ctrl Pts',(3.27141533508075,-31.5154078769165,56.389468969029));
#86402=CARTESIAN_POINT('Ctrl Pts',(3.2752707412931,-31.5617586582873,56.3352555769458));
#86403=CARTESIAN_POINT('Ctrl Pts',(3.27912592055178,-31.6081067111569,56.2810453762069));
#86404=CARTESIAN_POINT('Ctrl Pts',(3.28298109981045,-31.6516304610639,56.2244173834216));
#86405=CARTESIAN_POINT('Ctrl Pts',(3.28683627906913,-31.6920798789517,56.1657028977174));
#86406=CARTESIAN_POINT('Ctrl Pts',(3.29069525143292,-31.7325690949614,56.1069306429184));
#86407=CARTESIAN_POINT('Ctrl Pts',(3.29455422379671,-31.769977660405,56.0460681954318));
#86408=CARTESIAN_POINT('Ctrl Pts',(3.29841319616051,-31.8040987756994,55.9834760647926));
#86409=CARTESIAN_POINT('Ctrl Pts',(3.30227401452487,-31.8382362133698,55.9208539922161));
#86410=CARTESIAN_POINT('Ctrl Pts',(3.30613483288923,-31.869082857657,55.8565010268448));
#86411=CARTESIAN_POINT('Ctrl Pts',(3.30999565125359,-31.8964790776824,55.7908000192291));
#86412=CARTESIAN_POINT('Ctrl Pts',(3.31386358533863,-31.9239257905907,55.724977920701));
#86413=CARTESIAN_POINT('Ctrl Pts',(3.31773151942368,-31.9479092094712,55.6578032745301));
#86414=CARTESIAN_POINT('Ctrl Pts',(3.32159945350872,-31.9683189986739,55.5896760822345));
#86415=CARTESIAN_POINT('Ctrl Pts',(3.32502755223462,-31.9864079243958,55.5292958544507));
#86416=CARTESIAN_POINT('Ctrl Pts',(3.32845565096053,-32.0016904370004,55.4681678305888));
#86417=CARTESIAN_POINT('Ctrl Pts',(3.33188374968643,-32.014123551826,55.4065757991813));
#86418=CARTESIAN_POINT('Ctrl Pts',(3.33575282303467,-32.0281560045216,55.3370608562826));
#86419=CARTESIAN_POINT('Ctrl Pts',(3.3396218963829,-32.0386128869442,55.2666824303766));
#86420=CARTESIAN_POINT('Ctrl Pts',(3.34349096973113,-32.0453957342307,55.1958413972863));
#86421=CARTESIAN_POINT('Ctrl Pts',(3.34735427812694,-32.0521684750165,55.125105917942));
#86422=CARTESIAN_POINT('Ctrl Pts',(3.35121758652275,-32.0552780011611,55.0539096792667));
#86423=CARTESIAN_POINT('Ctrl Pts',(3.35508089491855,-32.0546768638109,54.9826636849271));
#86424=CARTESIAN_POINT('Ctrl Pts',(3.35893967141149,-32.0540764316324,54.9115012666039));
#86425=CARTESIAN_POINT('Ctrl Pts',(3.36279844790443,-32.0497739862521,54.840289691963));
#86426=CARTESIAN_POINT('Ctrl Pts',(3.36665722439736,-32.041774022137,54.7694432715655));
#86427=CARTESIAN_POINT('Ctrl Pts',(3.37051356998559,-32.0337790977413,54.6986414821275));
#86428=CARTESIAN_POINT('Ctrl Pts',(3.37436991557382,-32.0220913303187,54.6282048721235));
#86429=CARTESIAN_POINT('Ctrl Pts',(3.37822626116204,-32.0067671925835,54.5585444560653));
#86430=CARTESIAN_POINT('Ctrl Pts',(3.38208146740739,-31.9914475823074,54.4889046209165));
#86431=CARTESIAN_POINT('Ctrl Pts',(3.38593667365274,-31.9724938389174,54.4200409986262));
#86432=CARTESIAN_POINT('Ctrl Pts',(3.38979187989809,-31.95001355578,54.3523544991478));
#86433=CARTESIAN_POINT('Ctrl Pts',(3.39364723674936,-31.927532394437,54.284665355456));
#86434=CARTESIAN_POINT('Ctrl Pts',(3.39750259360064,-31.901524575037,54.2181538862032));
#86435=CARTESIAN_POINT('Ctrl Pts',(3.40135795045191,-31.8721470420644,54.1532042658411));
#86436=CARTESIAN_POINT('Ctrl Pts',(3.40521734292049,-31.8427387579875,54.0881866590845));
#86437=CARTESIAN_POINT('Ctrl Pts',(3.40907673538907,-31.8099539197302,54.0247346083171));
#86438=CARTESIAN_POINT('Ctrl Pts',(3.41293612785765,-31.7739966007954,53.9632099427239));
#86439=CARTESIAN_POINT('Ctrl Pts',(3.41679770546111,-31.7380189233216,53.9016504427123));
#86440=CARTESIAN_POINT('Ctrl Pts',(3.42065928306457,-31.6988654562192,53.8420209065002));
#86441=CARTESIAN_POINT('Ctrl Pts',(3.42452086066803,-31.6567835031492,53.784653964423));
#86442=CARTESIAN_POINT('Ctrl Pts',(3.42838919478292,-31.6146279202765,53.7271866487577));
#86443=CARTESIAN_POINT('Ctrl Pts',(3.43225752889782,-31.5695339288584,53.6719902074217));
#86444=CARTESIAN_POINT('Ctrl Pts',(3.43612586301271,-31.5217885122851,53.6193634488479));
#86445=CARTESIAN_POINT('Ctrl Pts',(3.43842358218347,-31.4934286147897,53.5881041241675));
#86446=CARTESIAN_POINT('Ctrl Pts',(3.44072130135423,-31.4641339653967,53.5577507144535));
#86447=CARTESIAN_POINT('Ctrl Pts',(3.44301902052499,-31.4339703168495,53.5283591834641));
#86448=CARTESIAN_POINT('Ctrl Pts',(3.44688809387321,-31.383178483729,53.4788675002933));
#86449=CARTESIAN_POINT('Ctrl Pts',(3.45075716722142,-31.3297219400212,53.4319114872837));
#86450=CARTESIAN_POINT('Ctrl Pts',(3.45462624056964,-31.2738840751609,53.3877912897049));
#86451=CARTESIAN_POINT('Ctrl Pts',(3.45848954896542,-31.2181294091975,53.3437368315983));
#86452=CARTESIAN_POINT('Ctrl Pts',(3.4623528573612,-31.1600008431914,53.3025101003627));
#86453=CARTESIAN_POINT('Ctrl Pts',(3.46621616575699,-31.0998179446717,53.2643738734745));
#86454=CARTESIAN_POINT('Ctrl Pts',(3.47007494224989,-31.039705644464,53.2262823827706));
#86455=CARTESIAN_POINT('Ctrl Pts',(3.4739337187428,-30.9775442068879,53.1912744539901));
#86456=CARTESIAN_POINT('Ctrl Pts',(3.4777924952357,-30.9136841499305,53.1595710183042));
#86457=CARTESIAN_POINT('Ctrl Pts',(3.4816488408239,-30.8498643227489,53.1278875547601));
#86458=CARTESIAN_POINT('Ctrl Pts',(3.4855051864121,-30.7843484332854,53.099504669707));
#86459=CARTESIAN_POINT('Ctrl Pts',(3.4893615320003,-30.7175124215068,53.0745978374679));
#86460=CARTESIAN_POINT('Ctrl Pts',(3.49321673824563,-30.6506961561778,53.0496983638591));
#86461=CARTESIAN_POINT('Ctrl Pts',(3.49707194449096,-30.5825609977991,53.0282730737537));
#86462=CARTESIAN_POINT('Ctrl Pts',(3.50092715073629,-30.5135021230636,53.0104490124379));
#86463=CARTESIAN_POINT('Ctrl Pts',(3.50478250758753,-30.4444405505021,52.9926242548147));
#86464=CARTESIAN_POINT('Ctrl Pts',(3.50863786443877,-30.3744556608628,52.9784011245609));
#86465=CARTESIAN_POINT('Ctrl Pts',(3.51249322129001,-30.3039553368884,52.9678561282042));
#86466=CARTESIAN_POINT('Ctrl Pts',(3.51635261375857,-30.2333812162879,52.957300093811));
#86467=CARTESIAN_POINT('Ctrl Pts',(3.52021200622712,-30.1622910657473,52.9504299510044));
#86468=CARTESIAN_POINT('Ctrl Pts',(3.52407139869567,-30.0910995558641,52.9472704919008));
#86469=CARTESIAN_POINT('Ctrl Pts',(3.5279329762991,-30.0198677383285,52.9441092439549));
#86470=CARTESIAN_POINT('Ctrl Pts',(3.53179455390252,-29.9485349332096,52.9446628582596));
#86471=CARTESIAN_POINT('Ctrl Pts',(3.53565613150594,-29.8775147263652,52.9489039709846));
#86472=CARTESIAN_POINT('Ctrl Pts',(3.53952446562081,-29.8063702571363,52.9531525042848));
#86473=CARTESIAN_POINT('Ctrl Pts',(3.54339279973568,-29.735539961084,52.9611013632752));
#86474=CARTESIAN_POINT('Ctrl Pts',(3.54726113385054,-29.6654305296723,52.9726715036717));
#86475=CARTESIAN_POINT('Ctrl Pts',(3.54955885302155,-29.6237868195274,52.9795439538301));
#86476=CARTESIAN_POINT('Ctrl Pts',(3.55185657219255,-29.5823972321482,52.9876930655165));
#86477=CARTESIAN_POINT('Ctrl Pts',(3.55415429136356,-29.5413444470519,52.9970939497196));
#86478=CARTESIAN_POINT('Ctrl Pts',(3.55802336471177,-29.4722166621205,53.0129238696588));
#86479=CARTESIAN_POINT('Ctrl Pts',(3.56189243805998,-29.4037739608207,53.0323677854612));
#86480=CARTESIAN_POINT('Ctrl Pts',(3.5657615114082,-29.336422208519,53.0553503973329));
#86481=CARTESIAN_POINT('Ctrl Pts',(3.56962481980398,-29.2691708109051,53.0782987649162));
#86482=CARTESIAN_POINT('Ctrl Pts',(3.57348812819977,-29.2030075916814,53.1047752068269));
#86483=CARTESIAN_POINT('Ctrl Pts',(3.57735143659555,-29.1383266436026,53.1346537615298));
#86484=CARTESIAN_POINT('Ctrl Pts',(3.58121021308847,-29.0737215703296,53.1644972668155));
#86485=CARTESIAN_POINT('Ctrl Pts',(3.58506898958138,-29.0105957532292,53.197734754904));
#86486=CARTESIAN_POINT('Ctrl Pts',(3.58892776607429,-28.9493249145688,53.2341915654992));
#86487=CARTESIAN_POINT('Ctrl Pts',(3.59278411166249,-28.8880926745604,53.2706254094797));
#86488=CARTESIAN_POINT('Ctrl Pts',(3.59664045725069,-28.8287135110421,53.3102743044957));
#86489=CARTESIAN_POINT('Ctrl Pts',(3.60049680283889,-28.7715387439723,53.3529175779765));
#86490=CARTESIAN_POINT('Ctrl Pts',(3.60435200908422,-28.7143808689733,53.3955482526618));
#86491=CARTESIAN_POINT('Ctrl Pts',(3.60820721532955,-28.6594264866429,53.4411712592055));
#86492=CARTESIAN_POINT('Ctrl Pts',(3.61206242157488,-28.6069966629057,53.4895234972552));
#86493=CARTESIAN_POINT('Ctrl Pts',(3.61591777842612,-28.5545647909664,53.5378776242137));
#86494=CARTESIAN_POINT('Ctrl Pts',(3.61977313527735,-28.5046580290391,53.5889608634019));
#86495=CARTESIAN_POINT('Ctrl Pts',(3.62362849212859,-28.4575618745408,53.6424720291538));
#86496=CARTESIAN_POINT('Ctrl Pts',(3.62748788459715,-28.4104164218675,53.6960392080311));
#86497=CARTESIAN_POINT('Ctrl Pts',(3.6313472770657,-28.3660877711614,53.752039021358));
#86498=CARTESIAN_POINT('Ctrl Pts',(3.63520666953425,-28.3248216537988,53.8101365326565));
#86499=CARTESIAN_POINT('Ctrl Pts',(3.63906824713769,-28.2835321721287,53.868266937966));
#86500=CARTESIAN_POINT('Ctrl Pts',(3.64292982474112,-28.2453089360108,53.9284969952101));
#86501=CARTESIAN_POINT('Ctrl Pts',(3.64679140234455,-28.2103532700148,53.9904643917358));
#86502=CARTESIAN_POINT('Ctrl Pts',(3.65065973645941,-28.1753364429128,54.0525402111567));
#86503=CARTESIAN_POINT('Ctrl Pts',(3.65452807057428,-28.1435988168513,54.1163590037658));
#86504=CARTESIAN_POINT('Ctrl Pts',(3.65839640468915,-28.115294558128,54.1815362195686));
#86505=CARTESIAN_POINT('Ctrl Pts',(3.66069412386014,-28.0984823500927,54.2202502845419));
#86506=CARTESIAN_POINT('Ctrl Pts',(3.66299184303113,-28.0828805480779,54.2594432652727));
#86507=CARTESIAN_POINT('Ctrl Pts',(3.66528956220211,-28.0685130841418,54.2990322001912));
#86508=CARTESIAN_POINT('Ctrl Pts',(3.66976608681325,-28.0405217148215,54.3761612261093));
#86509=CARTESIAN_POINT('Ctrl Pts',(3.67424261142439,-28.0171274210087,54.4550424288448));
#86510=CARTESIAN_POINT('Ctrl Pts',(3.67871913603553,-27.9985204841622,54.535158833383));
#86511=CARTESIAN_POINT('Ctrl Pts',(3.68315616207699,-27.980077725435,54.6145683316352));
#86512=CARTESIAN_POINT('Ctrl Pts',(3.68759318811845,-27.9663383039406,54.6951911642614));
#86513=CARTESIAN_POINT('Ctrl Pts',(3.69203021415991,-27.9574411612528,54.7765029021317));
#86514=CARTESIAN_POINT('Ctrl Pts',(3.69604504924405,-27.9493905975919,54.8500776828302));
#86515=CARTESIAN_POINT('Ctrl Pts',(3.70005988432819,-27.9453041789034,54.9242161665679));
#86516=CARTESIAN_POINT('Ctrl Pts',(3.70407471941232,-27.9452505355246,54.9985165115458));
#86517=CARTESIAN_POINT('Ctrl Pts',(3.70407471946232,-27.9452505355239,54.9985165124711));
#86518=CARTESIAN_POINT('Ctrl Pts',(3.70793830290604,-27.9451989130944,55.0700177265206));
#86519=CARTESIAN_POINT('Ctrl Pts',(3.71180188634977,-27.94888376533,55.1415522381297));
#86520=CARTESIAN_POINT('Ctrl Pts',(3.71566546979349,-27.9562889262005,55.2127031013631));
#86521=CARTESIAN_POINT('Ctrl Pts',(3.71952882663493,-27.9636936527524,55.2838497915411));
#86522=CARTESIAN_POINT('Ctrl Pts',(3.72339218347637,-27.9748182037558,55.3546123983527));
#86523=CARTESIAN_POINT('Ctrl Pts',(3.72725554031781,-27.9895945586331,55.4245792315016));
#86524=CARTESIAN_POINT('Ctrl Pts',(3.73111993974998,-28.0043749011542,55.4945649463574));
#86525=CARTESIAN_POINT('Ctrl Pts',(3.73498433918215,-28.0228089023201,55.563753989815));
#86526=CARTESIAN_POINT('Ctrl Pts',(3.73884873861432,-28.0447778295687,55.6317466476002));
#86527=CARTESIAN_POINT('Ctrl Pts',(3.74271803189464,-28.0667745781118,55.6998254108072));
#86528=CARTESIAN_POINT('Ctrl Pts',(3.74658732517497,-28.0923150338194,55.7667043065627));
#86529=CARTESIAN_POINT('Ctrl Pts',(3.7504566184553,-28.12123143394,55.8320013447614));
#86530=CARTESIAN_POINT('Ctrl Pts',(3.75432884727621,-28.1501697722442,55.8973479222667));
#86531=CARTESIAN_POINT('Ctrl Pts',(3.75820107609713,-28.1824889322493,55.961109825256));
#86532=CARTESIAN_POINT('Ctrl Pts',(3.76207330491805,-28.2179753493682,56.022929961943));
#86533=CARTESIAN_POINT('Ctrl Pts',(3.76595231070722,-28.2535238729207,56.0848582929343));
#86534=CARTESIAN_POINT('Ctrl Pts',(3.76983131649638,-28.2922504492782,56.144837675185));
#86535=CARTESIAN_POINT('Ctrl Pts',(3.77371032228555,-28.3338989370465,56.202540980809));
#86536=CARTESIAN_POINT('Ctrl Pts',(3.77461515920393,-28.3436140783418,56.2160011518113));
#86537=CARTESIAN_POINT('Ctrl Pts',(3.7755199961223,-28.3534880425275,56.2293376254159));
#86538=CARTESIAN_POINT('Ctrl Pts',(3.77642483304068,-28.3635172836502,56.242546530955));
#86539=CARTESIAN_POINT('Ctrl Pts',(3.78029390638889,-28.4064022154458,56.2990276750626));
#86540=CARTESIAN_POINT('Ctrl Pts',(3.78416297973711,-28.4522986437702,56.3533966652134));
#86541=CARTESIAN_POINT('Ctrl Pts',(3.78803205308532,-28.5009708582321,56.4053146247836));
#86542=CARTESIAN_POINT('Ctrl Pts',(3.79189536148111,-28.5495705506776,56.4571552261493));
#86543=CARTESIAN_POINT('Ctrl Pts',(3.7957586698769,-28.6009374899869,56.5065516946496));
#86544=CARTESIAN_POINT('Ctrl Pts',(3.79962197827268,-28.6547946429132,56.5531967389114));
#86545=CARTESIAN_POINT('Ctrl Pts',(3.80348075476559,-28.7085886180236,56.5997870656129));
#86546=CARTESIAN_POINT('Ctrl Pts',(3.80733953125851,-28.7648666388802,56.6436320626764));
#86547=CARTESIAN_POINT('Ctrl Pts',(3.81119830775142,-28.8233148545278,56.6844612286797));
#86548=CARTESIAN_POINT('Ctrl Pts',(3.81505465333963,-28.8817262496851,56.7252646736255));
#86549=CARTESIAN_POINT('Ctrl Pts',(3.81891099892784,-28.9423047299241,56.7630557792996));
#86550=CARTESIAN_POINT('Ctrl Pts',(3.82276734451604,-29.0047045580452,56.797605225216));
#86551=CARTESIAN_POINT('Ctrl Pts',(3.82662255076137,-29.0670859503705,56.8321444636279));
#86552=CARTESIAN_POINT('Ctrl Pts',(3.8304777570067,-29.1312871975198,56.8634437084732));
#86553=CARTESIAN_POINT('Ctrl Pts',(3.83433296325203,-29.196936351747,56.8913186773663));
#86554=CARTESIAN_POINT('Ctrl Pts',(3.83818832010328,-29.2625880705973,56.9191947352115));
#86555=CARTESIAN_POINT('Ctrl Pts',(3.84204367695452,-29.3296873608164,56.9436460636853));
#86556=CARTESIAN_POINT('Ctrl Pts',(3.84589903380577,-29.3978422093976,56.9645364740103));
#86557=CARTESIAN_POINT('Ctrl Pts',(3.84975842627433,-29.4660683994648,56.9854487514944));
#86558=CARTESIAN_POINT('Ctrl Pts',(3.85361781874289,-29.5353518881371,57.0027925274235));
#86559=CARTESIAN_POINT('Ctrl Pts',(3.85747721121144,-29.6052862753475,57.0164817475174));
#86560=CARTESIAN_POINT('Ctrl Pts',(3.86133878881488,-29.6752602584451,57.0301787182593));
#86561=CARTESIAN_POINT('Ctrl Pts',(3.86520036641832,-29.7458853925299,57.0402169457162));
#86562=CARTESIAN_POINT('Ctrl Pts',(3.86906194402176,-29.8167486103775,57.0465621150362));
#86563=CARTESIAN_POINT('Ctrl Pts',(3.87293027813663,-29.8877358159293,57.0529183863495));
#86564=CARTESIAN_POINT('Ctrl Pts',(3.8767986122515,-29.958961451333,57.0555686805711));
#86565=CARTESIAN_POINT('Ctrl Pts',(3.88066694636637,-30.0300115980961,57.0545308141957));
#86566=CARTESIAN_POINT('Ctrl Pts',(3.88296466553733,-30.0722140758214,57.0539143406966));
#86567=CARTESIAN_POINT('Ctrl Pts',(3.88526238470828,-30.1143546997391,57.0519976298562));
#86568=CARTESIAN_POINT('Ctrl Pts',(3.88756010387923,-30.1563480122918,57.0487930255525));
#86569=CARTESIAN_POINT('Ctrl Pts',(3.89142879126951,-30.2270524747003,57.0433974087089));
#86570=CARTESIAN_POINT('Ctrl Pts',(3.89529747865978,-30.297615780284,57.0343268801616));
#86571=CARTESIAN_POINT('Ctrl Pts',(3.89916616605005,-30.3676255066587,57.0215956691074));
#86572=CARTESIAN_POINT('Ctrl Pts',(3.90302937622956,-30.4375361146533,57.008882482649));
#86573=CARTESIAN_POINT('Ctrl Pts',(3.90689258640907,-30.5068942246873,56.9925189834919));
#86574=CARTESIAN_POINT('Ctrl Pts',(3.91075579658857,-30.5752914454823,56.9725712446588));
#86575=CARTESIAN_POINT('Ctrl Pts',(3.91461452942219,-30.6436093959294,56.9526466246627));
#86576=CARTESIAN_POINT('Ctrl Pts',(3.91847326225581,-30.7109682049742,56.9291461509408));
#86577=CARTESIAN_POINT('Ctrl Pts',(3.92233199508943,-30.7769704028753,56.90218678251));
#86578=CARTESIAN_POINT('Ctrl Pts',(3.9261881038184,-30.8429277164369,56.8752457476118));
#86579=CARTESIAN_POINT('Ctrl Pts',(3.93004421254737,-30.9075298017762,56.8448506709041));
#86580=CARTESIAN_POINT('Ctrl Pts',(3.93390032127633,-30.9703965480012,56.8111676074089));
#86581=CARTESIAN_POINT('Ctrl Pts',(3.93775577559097,-31.0332526252066,56.7774902602151));
#86582=CARTESIAN_POINT('Ctrl Pts',(3.9416112299056,-31.0943735163416,56.7405262564677));
#86583=CARTESIAN_POINT('Ctrl Pts',(3.94546668422024,-31.1534025934277,56.7004881710774));
#86584=CARTESIAN_POINT('Ctrl Pts',(3.94765985215727,-31.1869811729291,56.6777125814913));
#86585=CARTESIAN_POINT('Ctrl Pts',(3.9498530200943,-31.2198833281314,56.6539430902286));
#86586=CARTESIAN_POINT('Ctrl Pts',(3.95204618803132,-31.2520475724682,56.6292251037768));
#86587=CARTESIAN_POINT('',(3.64592528049244,-27.9452507844795,55.001795499335));
#86588=CARTESIAN_POINT('Ctrl Pts',(3.64592528053768,-27.9452507844802,55.001795500168));
#86589=CARTESIAN_POINT('Ctrl Pts',(3.65155534725541,-27.9453413655908,55.1054554547427));
#86590=CARTESIAN_POINT('Ctrl Pts',(3.65718541397315,-27.9532796299172,55.2087840265977));
#86591=CARTESIAN_POINT('Ctrl Pts',(3.66281548069089,-27.968896452778,55.3108310521202));
#86592=CARTESIAN_POINT('Ctrl Pts',(3.66436496635141,-27.973194455679,55.3389160483864));
#86593=CARTESIAN_POINT('Ctrl Pts',(3.66591445201194,-27.9780738114728,55.3669041565418));
#86594=CARTESIAN_POINT('Ctrl Pts',(3.66746393767247,-27.9835304264076,55.3947759127352));
#86595=CARTESIAN_POINT('Ctrl Pts',(3.67133301102068,-27.9971556208533,55.4643718256261));
#86596=CARTESIAN_POINT('Ctrl Pts',(3.67520208436889,-28.0144147564084,55.5333978458128));
#86597=CARTESIAN_POINT('Ctrl Pts',(3.6790711577171,-28.0352454688278,55.6014459200446));
#86598=CARTESIAN_POINT('Ctrl Pts',(3.68293446611288,-28.0560451433073,55.6693926020628));
#86599=CARTESIAN_POINT('Ctrl Pts',(3.68679777450866,-28.0804056902296,55.7363637697989));
#86600=CARTESIAN_POINT('Ctrl Pts',(3.69066108290444,-28.1082137350863,55.8019615267479));
#86601=CARTESIAN_POINT('Ctrl Pts',(3.69451985939735,-28.1359891593636,55.8674823334168));
#86602=CARTESIAN_POINT('Ctrl Pts',(3.69837863589025,-28.1672038598827,55.9316324843949));
#86603=CARTESIAN_POINT('Ctrl Pts',(3.70223741238316,-28.201695204195,55.9940308968461));
#86604=CARTESIAN_POINT('Ctrl Pts',(3.70609375797136,-28.236164820073,56.0563900003104));
#86605=CARTESIAN_POINT('Ctrl Pts',(3.70995010355956,-28.2739067499908,56.1169991304989));
#86606=CARTESIAN_POINT('Ctrl Pts',(3.71380644914776,-28.3147115970108,56.1755001323905));
#86607=CARTESIAN_POINT('Ctrl Pts',(3.71766165539308,-28.3555043883915,56.23398385038));
#86608=CARTESIAN_POINT('Ctrl Pts',(3.72151686163841,-28.3993580225816,56.2903602783593));
#86609=CARTESIAN_POINT('Ctrl Pts',(3.72537206788373,-28.4460197348827,56.3443001517987));
#86610=CARTESIAN_POINT('Ctrl Pts',(3.72922742473497,-28.4926832700512,56.3982421324311));
#86611=CARTESIAN_POINT('Ctrl Pts',(3.73308278158621,-28.5421547816376,56.4497470035929));
#86612=CARTESIAN_POINT('Ctrl Pts',(3.73693813843745,-28.5941423085746,56.4985198410298));
#86613=CARTESIAN_POINT('Ctrl Pts',(3.74079753090601,-28.6461842537591,56.5473437317192));
#86614=CARTESIAN_POINT('Ctrl Pts',(3.74465692337456,-28.7007471166513,56.5934295468804));
#86615=CARTESIAN_POINT('Ctrl Pts',(3.74851631584311,-28.7575039387394,56.6365210356888));
#86616=CARTESIAN_POINT('Ctrl Pts',(3.75237789344654,-28.8142928957587,56.6796369223049));
#86617=CARTESIAN_POINT('Ctrl Pts',(3.75623947104997,-28.8732778829159,56.719754834327));
#86618=CARTESIAN_POINT('Ctrl Pts',(3.7601010486534,-28.9341031681986,56.7566620353544));
#86619=CARTESIAN_POINT('Ctrl Pts',(3.76396938276827,-28.9950348780511,56.7936338120428));
#86620=CARTESIAN_POINT('Ctrl Pts',(3.76783771688313,-29.0578128866956,56.8273834317255));
#86621=CARTESIAN_POINT('Ctrl Pts',(3.771706050998,-29.1220577374214,56.8577445858025));
#86622=CARTESIAN_POINT('Ctrl Pts',(3.774003770169,-29.1602179947229,56.8757785517695));
#86623=CARTESIAN_POINT('Ctrl Pts',(3.77630148934001,-29.1988953899806,56.8926179419242));
#86624=CARTESIAN_POINT('Ctrl Pts',(3.77859920851102,-29.2380077640327,56.9082361999568));
#86625=CARTESIAN_POINT('Ctrl Pts',(3.78246828185923,-29.303868138068,56.9345354042555));
#86626=CARTESIAN_POINT('Ctrl Pts',(3.78633735520744,-29.3712206395652,56.957472487004));
#86627=CARTESIAN_POINT('Ctrl Pts',(3.79020642855566,-29.4396886210873,56.9768785296929));
#86628=CARTESIAN_POINT('Ctrl Pts',(3.79406973695144,-29.5080545847304,56.996255657212));
#86629=CARTESIAN_POINT('Ctrl Pts',(3.79793304534722,-29.577532265659,57.0121120567743));
#86630=CARTESIAN_POINT('Ctrl Pts',(3.80179635374301,-29.647725883426,57.0243271744686));
#86631=CARTESIAN_POINT('Ctrl Pts',(3.80565513023592,-29.7178371596801,57.0365279630643));
#86632=CARTESIAN_POINT('Ctrl Pts',(3.80951390672883,-29.7886622282982,57.0450958714596));
#86633=CARTESIAN_POINT('Ctrl Pts',(3.81337268322174,-29.8597927189909,57.0499608486144));
#86634=CARTESIAN_POINT('Ctrl Pts',(3.81722902880994,-29.9308783997692,57.0548227609906));
#86635=CARTESIAN_POINT('Ctrl Pts',(3.82108537439815,-30.0022686373837,57.0559863371499));
#86636=CARTESIAN_POINT('Ctrl Pts',(3.82494171998635,-30.0735489608221,57.0534332501598));
#86637=CARTESIAN_POINT('Ctrl Pts',(3.82879692623168,-30.1448082247557,57.0508809174698));
#86638=CARTESIAN_POINT('Ctrl Pts',(3.83265213247701,-30.2159571537724,57.0446141189907));
#86639=CARTESIAN_POINT('Ctrl Pts',(3.83650733872234,-30.2865820279039,57.0346666321003));
#86640=CARTESIAN_POINT('Ctrl Pts',(3.84036269557359,-30.357209661038,57.0247187566055));
#86641=CARTESIAN_POINT('Ctrl Pts',(3.84421805242483,-30.4273127179108,57.0110899771617));
#86642=CARTESIAN_POINT('Ctrl Pts',(3.84807340927607,-30.4964850706127,56.9938656266556));
#86643=CARTESIAN_POINT('Ctrl Pts',(3.85193280174463,-30.565729829879,56.9766232464599));
#86644=CARTESIAN_POINT('Ctrl Pts',(3.85579219421319,-30.6340414678546,56.9557778996609));
#86645=CARTESIAN_POINT('Ctrl Pts',(3.85965158668174,-30.7010273665057,56.9314652971022));
#86646=CARTESIAN_POINT('Ctrl Pts',(3.86351316428518,-30.7680511916503,56.9071389290827));
#86647=CARTESIAN_POINT('Ctrl Pts',(3.86737474188861,-30.8337473356286,56.8793415867398));
#86648=CARTESIAN_POINT('Ctrl Pts',(3.87123631949205,-30.8977441330565,56.8482567554489));
#86649=CARTESIAN_POINT('Ctrl Pts',(3.87510465360692,-30.9618529041745,56.8171175357605));
#86650=CARTESIAN_POINT('Ctrl Pts',(3.87897298772178,-31.0242559669955,56.7826795777974));
#86651=CARTESIAN_POINT('Ctrl Pts',(3.88284132183665,-31.0846077947287,56.7451714798591));
#86652=CARTESIAN_POINT('Ctrl Pts',(3.88513904100763,-31.1204556681202,56.7228923609567));
#86653=CARTESIAN_POINT('Ctrl Pts',(3.8874367601786,-31.1555804033927,56.6995308769136));
#86654=CARTESIAN_POINT('Ctrl Pts',(3.88973447934958,-31.1899151292547,56.6751416500317));
#86655=CARTESIAN_POINT('Ctrl Pts',(3.89113859517648,-31.210896776013,56.66023760958));
#86656=CARTESIAN_POINT('Ctrl Pts',(3.89254271100338,-31.2316132332841,56.6449287439375));
#86657=CARTESIAN_POINT('Ctrl Pts',(3.89394682683029,-31.2520475724682,56.6292251037768));
#86658=CARTESIAN_POINT('Ctrl Pts',(3.19386027023256,-31.2520475724682,56.6292251037768));
#86659=CARTESIAN_POINT('Ctrl Pts',(3.1977220959346,-31.3085779768709,56.5857819015827));
#86660=CARTESIAN_POINT('Ctrl Pts',(3.20158392163664,-31.3627920617531,56.5394335086125));
#86661=CARTESIAN_POINT('Ctrl Pts',(3.20544574733867,-31.4143916292804,56.490467672082));
#86662=CARTESIAN_POINT('Ctrl Pts',(3.20931422587572,-31.4660800882896,56.4414174812444));
#86663=CARTESIAN_POINT('Ctrl Pts',(3.21318270441277,-31.5151447051828,56.3897411985227));
#86664=CARTESIAN_POINT('Ctrl Pts',(3.21705118294981,-31.5613259547182,56.3357615152501));
#86665=CARTESIAN_POINT('Ctrl Pts',(3.21900840673928,-31.5846909648513,56.3084509539436));
#86666=CARTESIAN_POINT('Ctrl Pts',(3.22096563052875,-31.6073185673067,56.280551271071));
#86667=CARTESIAN_POINT('Ctrl Pts',(3.22292285431822,-31.6291794168843,56.2521070202265));
#86668=CARTESIAN_POINT('Ctrl Pts',(3.2267919276666,-31.6723943169528,56.195877940318));
#86669=CARTESIAN_POINT('Ctrl Pts',(3.23066100101498,-31.7127794322327,56.1372988340834));
#86670=CARTESIAN_POINT('Ctrl Pts',(3.23453007436335,-31.750069802935,56.076686234404));
#86671=CARTESIAN_POINT('Ctrl Pts',(3.2383933827593,-31.7873046106655,56.0161639480173));
#86672=CARTESIAN_POINT('Ctrl Pts',(3.24225669115525,-31.8214535744354,55.9536145928793));
#86673=CARTESIAN_POINT('Ctrl Pts',(3.2461199995512,-31.8522930751998,55.8893862637049));
#86674=CARTESIAN_POINT('Ctrl Pts',(3.24997877604428,-31.883096399297,55.8252332783859));
#86675=CARTESIAN_POINT('Ctrl Pts',(3.25383755253736,-31.9105977625169,55.759405667002));
#86676=CARTESIAN_POINT('Ctrl Pts',(3.25769632903044,-31.9346187232656,55.6922773707773));
#86677=CARTESIAN_POINT('Ctrl Pts',(3.26155267461882,-31.9586245515839,55.6251913632135));
#86678=CARTESIAN_POINT('Ctrl Pts',(3.2654090202072,-31.9791541641155,55.5568067527675));
#86679=CARTESIAN_POINT('Ctrl Pts',(3.26926536579557,-31.996077236238,55.4875174145326));
#86680=CARTESIAN_POINT('Ctrl Pts',(3.27312057204107,-32.0129953085021,55.4182485475735));
#86681=CARTESIAN_POINT('Ctrl Pts',(3.27697577828658,-32.0263088405503,55.3480759551444));
#86682=CARTESIAN_POINT('Ctrl Pts',(3.28083098453208,-32.0359378534985,55.2774069559185));
#86683=CARTESIAN_POINT('Ctrl Pts',(3.2846863413835,-32.0455672426098,55.2067351959663));
#86684=CARTESIAN_POINT('Ctrl Pts',(3.28854169823492,-32.0515117634489,55.135567472352));
#86685=CARTESIAN_POINT('Ctrl Pts',(3.29239705508634,-32.0537431147051,55.0643178148044));
#86686=CARTESIAN_POINT('Ctrl Pts',(3.29625644755507,-32.0559768016414,54.9929935762614));
#86687=CARTESIAN_POINT('Ctrl Pts',(3.3001158400238,-32.0544895448673,54.9215877191223));
#86688=CARTESIAN_POINT('Ctrl Pts',(3.30397523249253,-32.0493051964124,54.8505149691207));
#86689=CARTESIAN_POINT('Ctrl Pts',(3.30783681009614,-32.0441179126508,54.7794019787067));
#86690=CARTESIAN_POINT('Ctrl Pts',(3.31169838769975,-32.035229430767,54.7086229531046));
#86691=CARTESIAN_POINT('Ctrl Pts',(3.31555996530336,-32.0227152743479,54.638585443819));
#86692=CARTESIAN_POINT('Ctrl Pts',(3.31942829941841,-32.0101792222039,54.5684253915519));
#86693=CARTESIAN_POINT('Ctrl Pts',(3.32329663353345,-31.9940049403023,54.499009919188));
#86694=CARTESIAN_POINT('Ctrl Pts',(3.3271649676485,-31.9743184724179,54.4307336897642));
#86695=CARTESIAN_POINT('Ctrl Pts',(3.32946268681792,-31.9626250733238,54.390178867844));
#86696=CARTESIAN_POINT('Ctrl Pts',(3.33176040598735,-31.9496934720379,54.3500256656002));
#86697=CARTESIAN_POINT('Ctrl Pts',(3.33405812515678,-31.9355580520016,54.310353286217));
#86698=CARTESIAN_POINT('Ctrl Pts',(3.33792719850496,-31.9117557624724,54.2435499327991));
#86699=CARTESIAN_POINT('Ctrl Pts',(3.34179627185313,-31.8844443398247,54.1778494349639));
#86700=CARTESIAN_POINT('Ctrl Pts',(3.3456653452013,-31.8537460124458,54.1136460730379));
#86701=CARTESIAN_POINT('Ctrl Pts',(3.34952865359705,-31.8230934258378,54.0495383746712));
#86702=CARTESIAN_POINT('Ctrl Pts',(3.3533919619928,-31.7890641595386,53.9869238189406));
#86703=CARTESIAN_POINT('Ctrl Pts',(3.35725527038854,-31.7518293801418,53.9261790720181));
#86704=CARTESIAN_POINT('Ctrl Pts',(3.36111404688141,-31.7146382794749,53.8655055824908));
#86705=CARTESIAN_POINT('Ctrl Pts',(3.36497282337429,-31.6742493875157,53.8066979570904));
#86706=CARTESIAN_POINT('Ctrl Pts',(3.36883159986716,-31.6308800882627,53.7501089246626));
#86707=CARTESIAN_POINT('Ctrl Pts',(3.37268794545532,-31.5875381102692,53.6935555414996));
#86708=CARTESIAN_POINT('Ctrl Pts',(3.37654429104349,-31.5412197448334,53.6392183630728));
#86709=CARTESIAN_POINT('Ctrl Pts',(3.38040063663165,-31.4921852201833,53.587420504479));
#86710=CARTESIAN_POINT('Ctrl Pts',(3.38425584287695,-31.4431651826,53.5356379493686));
#86711=CARTESIAN_POINT('Ctrl Pts',(3.38811104912224,-31.3914309127271,53.4863935772636));
#86712=CARTESIAN_POINT('Ctrl Pts',(3.39196625536753,-31.3372812390496,53.4399754969277));
#86713=CARTESIAN_POINT('Ctrl Pts',(3.39582161221873,-31.2831294499831,53.3935556032421));
#86714=CARTESIAN_POINT('Ctrl Pts',(3.39967696906994,-31.2265624400304,53.3499625350207));
#86715=CARTESIAN_POINT('Ctrl Pts',(3.40353232592114,-31.1679127039866,53.3094446242827));
#86716=CARTESIAN_POINT('Ctrl Pts',(3.40739171838966,-31.109201575989,53.2688843011849));
#86717=CARTESIAN_POINT('Ctrl Pts',(3.41125111085818,-31.0484037704212,53.231405837981));
#86718=CARTESIAN_POINT('Ctrl Pts',(3.4151105033267,-30.9858806529212,53.1972141278855));
#86719=CARTESIAN_POINT('Ctrl Pts',(3.41897208093009,-30.9233221356929,53.1630030589145));
#86720=CARTESIAN_POINT('Ctrl Pts',(3.42283365853349,-30.8590367999157,53.1320826582239));
#86721=CARTESIAN_POINT('Ctrl Pts',(3.42669523613688,-30.7934080086418,53.1046105164576));
#86722=CARTESIAN_POINT('Ctrl Pts',(3.43056357025171,-30.7276643882165,53.0770903073315));
#86723=CARTESIAN_POINT('Ctrl Pts',(3.43443190436654,-30.6605730766457,53.0530305668983));
#86724=CARTESIAN_POINT('Ctrl Pts',(3.43830023848138,-30.5925340091539,53.0325394513495));
#86725=CARTESIAN_POINT('Ctrl Pts',(3.4405979576527,-30.5521200570149,53.0203681063621));
#86726=CARTESIAN_POINT('Ctrl Pts',(3.44289567682402,-30.5113719666599,53.0094548530609));
#86727=CARTESIAN_POINT('Ctrl Pts',(3.44519339599535,-30.4703749284781,52.9998137613814));
#86728=CARTESIAN_POINT('Ctrl Pts',(3.44906246934355,-30.4013410144281,52.9835793619255));
#86729=CARTESIAN_POINT('Ctrl Pts',(3.45293154269174,-30.3313304296172,52.9708912873145));
#86730=CARTESIAN_POINT('Ctrl Pts',(3.45680061603994,-30.2607407184097,52.9618606916447));
#86731=CARTESIAN_POINT('Ctrl Pts',(3.46066392443571,-30.1902561864765,52.9528435516397));
#86732=CARTESIAN_POINT('Ctrl Pts',(3.46452723283147,-30.1191947189186,52.9474731342666));
#86733=CARTESIAN_POINT('Ctrl Pts',(3.46839054122724,-30.0479656040068,52.9458099252181));
#86734=CARTESIAN_POINT('Ctrl Pts',(3.47224931772014,-29.9768200453109,52.9441486672182));
#86735=CARTESIAN_POINT('Ctrl Pts',(3.47610809421303,-29.9055077131926,52.9461859906645));
#86736=CARTESIAN_POINT('Ctrl Pts',(3.47996687070592,-29.834442851793,52.9519305692488));
#86737=CARTESIAN_POINT('Ctrl Pts',(3.48382321629411,-29.7634227589635,52.9576715289339));
#86738=CARTESIAN_POINT('Ctrl Pts',(3.48767956188229,-29.6926503106142,52.9671150712111));
#86739=CARTESIAN_POINT('Ctrl Pts',(3.49153590747048,-29.6225381082574,52.9802178130348));
#86740=CARTESIAN_POINT('Ctrl Pts',(3.49539111371579,-29.5524466202884,52.9933166837024));
#86741=CARTESIAN_POINT('Ctrl Pts',(3.4992463199611,-29.4830154683081,53.0100725184488));
#86742=CARTESIAN_POINT('Ctrl Pts',(3.50310152620641,-29.4146487788767,53.0303905182932));
#86743=CARTESIAN_POINT('Ctrl Pts',(3.50695688305764,-29.34627941866,53.0507093118723));
#86744=CARTESIAN_POINT('Ctrl Pts',(3.51081223990887,-29.278975068581,53.0745904063289));
#86745=CARTESIAN_POINT('Ctrl Pts',(3.51466759676009,-29.2131246964214,53.1018891446709));
#86746=CARTESIAN_POINT('Ctrl Pts',(3.51852698922863,-29.1472053949999,53.1292164581269));
#86747=CARTESIAN_POINT('Ctrl Pts',(3.52238638169717,-29.0827435593446,53.1599683704247));
#86748=CARTESIAN_POINT('Ctrl Pts',(3.5262457741657,-29.0201073209133,53.1939524092726));
#86749=CARTESIAN_POINT('Ctrl Pts',(3.53010735176912,-28.9574356187063,53.2279556894153));
#86750=CARTESIAN_POINT('Ctrl Pts',(3.53396892937253,-28.896591985895,53.2651944853309));
#86751=CARTESIAN_POINT('Ctrl Pts',(3.53783050697594,-28.8379167435952,53.305432188526));
#86752=CARTESIAN_POINT('Ctrl Pts',(3.54169884109079,-28.7791388386051,53.3457402946833));
#86753=CARTESIAN_POINT('Ctrl Pts',(3.54556717520564,-28.7225372848209,53.3890574888132));
#86754=CARTESIAN_POINT('Ctrl Pts',(3.54943550932049,-28.6684198594727,53.4351064279468));
#86755=CARTESIAN_POINT('Ctrl Pts',(3.55173322849163,-28.6362751061957,53.4624586491139));
#86756=CARTESIAN_POINT('Ctrl Pts',(3.55403094766277,-28.6050061059768,53.4907739380974));
#86757=CARTESIAN_POINT('Ctrl Pts',(3.55632866683391,-28.5746708837891,53.5199883537683));
#86758=CARTESIAN_POINT('Ctrl Pts',(3.56013990426076,-28.5243537103042,53.5684464402949));
#86759=CARTESIAN_POINT('Ctrl Pts',(3.56395114168762,-28.4763982156425,53.6195819833469));
#86760=CARTESIAN_POINT('Ctrl Pts',(3.56776237911448,-28.4311089343791,53.673132114069));
#86761=CARTESIAN_POINT('Ctrl Pts',(3.57156855056509,-28.3858798525725,53.726611064841));
#86762=CARTESIAN_POINT('Ctrl Pts',(3.5753747220157,-28.3433102826234,53.7824978653988));
#86763=CARTESIAN_POINT('Ctrl Pts',(3.57918089346632,-28.3036692051413,53.8404917434904));
#86764=CARTESIAN_POINT('Ctrl Pts',(3.58298336737586,-28.264066637357,53.8984292828833));
#86765=CARTESIAN_POINT('Ctrl Pts',(3.5867858412854,-28.2273872042853,53.95846943092));
#86766=CARTESIAN_POINT('Ctrl Pts',(3.59058831519494,-28.1938594686743,54.0202786398151));
#86767=CARTESIAN_POINT('Ctrl Pts',(3.59438845464257,-28.1603523168263,54.0820499020345));
#86768=CARTESIAN_POINT('Ctrl Pts',(3.5981885940902,-28.1299932630392,54.1455876312835));
#86769=CARTESIAN_POINT('Ctrl Pts',(3.60198873353783,-28.1029663477994,54.2105312641285));
#86770=CARTESIAN_POINT('Ctrl Pts',(3.60578956781203,-28.0759344908939,54.2754867714223));
#86771=CARTESIAN_POINT('Ctrl Pts',(3.60959040208624,-28.0522361979825,54.3418482392768));
#86772=CARTESIAN_POINT('Ctrl Pts',(3.61339123636044,-28.0320078938971,54.4092338594531));
#86773=CARTESIAN_POINT('Ctrl Pts',(3.61719222217697,-28.0117787832929,54.4766221663485));
#86774=CARTESIAN_POINT('Ctrl Pts',(3.6209932079935,-27.995020070069,54.5450342228542));
#86775=CARTESIAN_POINT('Ctrl Pts',(3.62479419381004,-27.981817936286,54.6140742037604));
#86776=CARTESIAN_POINT('Ctrl Pts',(3.62859963984793,-27.968600310617,54.6831951988067));
#86777=CARTESIAN_POINT('Ctrl Pts',(3.63240508588582,-27.9589476807169,54.7529450939116));
#86778=CARTESIAN_POINT('Ctrl Pts',(3.63621053192372,-27.9528946642777,54.8229200548982));
#86779=CARTESIAN_POINT('Ctrl Pts',(3.63944878144662,-27.9477438416405,54.8824653438798));
#86780=CARTESIAN_POINT('Ctrl Pts',(3.64268703096953,-27.9451986849012,54.9421733287143));
#86781=CARTESIAN_POINT('Ctrl Pts',(3.64592528049244,-27.9452507844795,55.001795499335));
#86782=CARTESIAN_POINT('Origin',(-1.54592528053767,-30.,55.));
#86783=CARTESIAN_POINT('',(2.4939437805615,-31.2520475724682,56.6292251037768));
#86784=CARTESIAN_POINT('',(2.55206205584979,-31.2520475724682,56.6292251037768));
#86785=CARTESIAN_POINT('',(-1.54592528053767,-31.2520475724682,56.6292251037768));
#86786=CARTESIAN_POINT('',(3.00407471949931,-27.9452500948919,54.9993755336174));
#86787=CARTESIAN_POINT('Ctrl Pts',(2.55206205584979,-31.2520475724682,56.6292251037768));
#86788=CARTESIAN_POINT('Ctrl Pts',(2.55268698850536,-31.2611355765577,56.6222410391239));
#86789=CARTESIAN_POINT('Ctrl Pts',(2.55331192116094,-31.2701623751725,56.615183057574));
#86790=CARTESIAN_POINT('Ctrl Pts',(2.55393685381652,-31.279126718988,56.6080523621048));
#86791=CARTESIAN_POINT('Ctrl Pts',(2.55780592716298,-31.334626625123,56.563904911119));
#86792=CARTESIAN_POINT('Ctrl Pts',(2.56167500050945,-31.3879470171915,56.5167943495909));
#86793=CARTESIAN_POINT('Ctrl Pts',(2.56554407385591,-31.4387544190205,56.4669639682859));
#86794=CARTESIAN_POINT('Ctrl Pts',(2.56940738224991,-31.4894861173851,56.4172078346763));
#86795=CARTESIAN_POINT('Ctrl Pts',(2.5732706906439,-31.5377119139981,56.3647402628776));
#86796=CARTESIAN_POINT('Ctrl Pts',(2.5771339990379,-31.583130841571,56.3098451438879));
#86797=CARTESIAN_POINT('Ctrl Pts',(2.58099277552898,-31.6284964898948,56.2550144203138));
#86798=CARTESIAN_POINT('Ctrl Pts',(2.58485155202006,-31.6710615012904,56.1977621784434));
#86799=CARTESIAN_POINT('Ctrl Pts',(2.58871032851114,-31.7105625191579,56.1384082881603));
#86800=CARTESIAN_POINT('Ctrl Pts',(2.59256667409748,-31.7500386526582,56.0790917889138));
#86801=CARTESIAN_POINT('Ctrl Pts',(2.59642301968382,-31.7864543536427,56.0176766714479));
#86802=CARTESIAN_POINT('Ctrl Pts',(2.60027936527017,-31.8195881548854,55.9545137553229));
#86803=CARTESIAN_POINT('Ctrl Pts',(2.60413457151361,-31.8527121668703,55.8913695004457));
#86804=CARTESIAN_POINT('Ctrl Pts',(2.60798977775706,-31.8825559785433,55.8264789020223));
#86805=CARTESIAN_POINT('Ctrl Pts',(2.6118449840005,-31.9089437402716,55.7602179680708));
#86806=CARTESIAN_POINT('Ctrl Pts',(2.61570034084984,-31.9353325328533,55.6939544455971));
#86807=CARTESIAN_POINT('Ctrl Pts',(2.61955569769918,-31.9582648297553,55.626320933442));
#86808=CARTESIAN_POINT('Ctrl Pts',(2.62341105454852,-31.977613315118,55.5577124154687));
#86809=CARTESIAN_POINT('Ctrl Pts',(2.62727044701515,-31.9969820536207,55.4890320811287));
#86810=CARTESIAN_POINT('Ctrl Pts',(2.63112983948178,-32.0127593598703,55.4193751721447));
#86811=CARTESIAN_POINT('Ctrl Pts',(2.63498923194841,-32.0248683641302,55.3491499254542));
#86812=CARTESIAN_POINT('Ctrl Pts',(2.6388508095499,-32.0369842243416,55.2788849181961));
#86813=CARTESIAN_POINT('Ctrl Pts',(2.64271238715139,-32.0454275904864,55.2080514152564));
#86814=CARTESIAN_POINT('Ctrl Pts',(2.64657396475289,-32.0501734694218,55.1370631525213));
#86815=CARTESIAN_POINT('Ctrl Pts',(2.65044229886581,-32.0549276521099,55.0659506832939));
#86816=CARTESIAN_POINT('Ctrl Pts',(2.65431063297874,-32.0559714241148,54.9946833995398));
#86817=CARTESIAN_POINT('Ctrl Pts',(2.65817896709166,-32.053331929582,54.923674712847));
#86818=CARTESIAN_POINT('Ctrl Pts',(2.66047668627947,-32.051764118463,54.8814968613088));
#86819=CARTESIAN_POINT('Ctrl Pts',(2.66277440546727,-32.0488977950453,54.8394101629232));
#86820=CARTESIAN_POINT('Ctrl Pts',(2.66507212465508,-32.04474722679,54.7974997752229));
#86821=CARTESIAN_POINT('Ctrl Pts',(2.66894119800453,-32.0377581860459,54.726927894648));
#86822=CARTESIAN_POINT('Ctrl Pts',(2.67281027135398,-32.027097616907,54.6565800340403));
#86823=CARTESIAN_POINT('Ctrl Pts',(2.67667934470343,-32.012789053044,54.5868683134323));
#86824=CARTESIAN_POINT('Ctrl Pts',(2.68054265310047,-31.9985018090636,54.5172604638848));
#86825=CARTESIAN_POINT('Ctrl Pts',(2.68440596149751,-31.9805774566371,54.4482873448619));
#86826=CARTESIAN_POINT('Ctrl Pts',(2.68826926989455,-31.9590912711106,54.3803557843743));
#86827=CARTESIAN_POINT('Ctrl Pts',(2.69212804638873,-31.9376302902261,54.3125039118642));
#86828=CARTESIAN_POINT('Ctrl Pts',(2.69598682288292,-31.9126159214519,54.2456916318767));
#86829=CARTESIAN_POINT('Ctrl Pts',(2.69984559937711,-31.8841740662498,54.1803136877001));
#86830=CARTESIAN_POINT('Ctrl Pts',(2.7037019449666,-31.8557501284988,54.1149769295191));
#86831=CARTESIAN_POINT('Ctrl Pts',(2.70755829055609,-31.8239031814823,54.0510731588554));
#86832=CARTESIAN_POINT('Ctrl Pts',(2.71141463614558,-31.7888078481252,53.9889787119028));
#86833=CARTESIAN_POINT('Ctrl Pts',(2.71526984239221,-31.753722883553,53.9269026105221));
#86834=CARTESIAN_POINT('Ctrl Pts',(2.71912504863884,-31.7153916768536,53.8666351942883));
#86835=CARTESIAN_POINT('Ctrl Pts',(2.72298025488547,-31.6740347542169,53.8085281353829));
#86836=CARTESIAN_POINT('Ctrl Pts',(2.72683561173802,-31.6326762159473,53.7504188064907));
#86837=CARTESIAN_POINT('Ctrl Pts',(2.73069096859058,-31.5882920105504,53.6944703969831));
#86838=CARTESIAN_POINT('Ctrl Pts',(2.73454632544313,-31.5411449296255,53.6410040955214));
#86839=CARTESIAN_POINT('Ctrl Pts',(2.738405717913,-31.493948497218,53.5874818278961));
#86840=CARTESIAN_POINT('Ctrl Pts',(2.74226511038287,-31.4439837380421,53.5364472199356));
#86841=CARTESIAN_POINT('Ctrl Pts',(2.74612450285274,-31.3915519383472,53.4881862663072));
#86842=CARTESIAN_POINT('Ctrl Pts',(2.74998608045749,-31.3390904524892,53.4398979879914));
#86843=CARTESIAN_POINT('Ctrl Pts',(2.75384765806223,-31.2841595197586,53.3943868002742));
#86844=CARTESIAN_POINT('Ctrl Pts',(2.75770923566698,-31.2270931823125,53.3518980964691));
#86845=CARTESIAN_POINT('Ctrl Pts',(2.76157756978316,-31.1699269972392,53.3093350511792));
#86846=CARTESIAN_POINT('Ctrl Pts',(2.76544590389934,-31.1106183522403,53.2698053176905));
#86847=CARTESIAN_POINT('Ctrl Pts',(2.76931423801552,-31.0495292944085,53.2335103106221));
#86848=CARTESIAN_POINT('Ctrl Pts',(2.77161195717489,-31.013243520121,53.2119517454553));
#86849=CARTESIAN_POINT('Ctrl Pts',(2.77390967633427,-30.9763300611485,53.1915335551999));
#86850=CARTESIAN_POINT('Ctrl Pts',(2.77620739549364,-30.9388682001987,53.1722899395266));
#86851=CARTESIAN_POINT('Ctrl Pts',(2.78007646884163,-30.8757870846606,53.1398860836347));
#86852=CARTESIAN_POINT('Ctrl Pts',(2.78394554218962,-30.8109028729154,53.1106883390548));
#86853=CARTESIAN_POINT('Ctrl Pts',(2.7878146155376,-30.7445745687712,53.0849004532298));
#86854=CARTESIAN_POINT('Ctrl Pts',(2.79167792393316,-30.6783450943683,53.0591509915757));
#86855=CARTESIAN_POINT('Ctrl Pts',(2.79554123232871,-30.6106762477312,53.0368014781913));
#86856=CARTESIAN_POINT('Ctrl Pts',(2.79940454072427,-30.5419506494363,53.0180093198818));
#86857=CARTESIAN_POINT('Ctrl Pts',(2.80326331721695,-30.4733056705754,52.9992392059517));
#86858=CARTESIAN_POINT('Ctrl Pts',(2.80712209370964,-30.4036068687027,52.9840182856126));
#86859=CARTESIAN_POINT('Ctrl Pts',(2.81098087020232,-30.3332541692799,52.9724548781451));
#86860=CARTESIAN_POINT('Ctrl Pts',(2.81483721579029,-30.2629457897881,52.9608987552513));
#86861=CARTESIAN_POINT('Ctrl Pts',(2.81869356137827,-30.1919848082382,52.9529956525039));
#86862=CARTESIAN_POINT('Ctrl Pts',(2.82254990696625,-30.1207821102618,52.948802972813));
#86863=CARTESIAN_POINT('Ctrl Pts',(2.82640511321135,-30.0496004488561,52.9446115318336));
#86864=CARTESIAN_POINT('Ctrl Pts',(2.83026031945645,-29.9781776974827,52.9441283661294));
#86865=CARTESIAN_POINT('Ctrl Pts',(2.83411552570155,-29.9069289167445,52.9473589364037));
#86866=CARTESIAN_POINT('Ctrl Pts',(2.83797088255257,-29.8356773526305,52.9505896328822));
#86867=CARTESIAN_POINT('Ctrl Pts',(2.84182623940359,-29.7646002578324,52.9575343291709));
#86868=CARTESIAN_POINT('Ctrl Pts',(2.84568159625461,-29.6941100056602,52.968146443795));
#86869=CARTESIAN_POINT('Ctrl Pts',(2.84954098872294,-29.6235459674045,52.9787696667122));
#86870=CARTESIAN_POINT('Ctrl Pts',(2.85340038119128,-29.5535704793747,52.9930678987881));
#86871=CARTESIAN_POINT('Ctrl Pts',(2.85725977365961,-29.484587224989,53.0109431295573));
#86872=CARTESIAN_POINT('Ctrl Pts',(2.86112135126282,-29.4155649132344,53.028828481036));
#86873=CARTESIAN_POINT('Ctrl Pts',(2.86498292886603,-29.3475364169614,53.0502947165981));
#86874=CARTESIAN_POINT('Ctrl Pts',(2.86884450646924,-29.2808890742504,53.0751942853972));
#86875=CARTESIAN_POINT('Ctrl Pts',(2.87271284058389,-29.2141251202527,53.1001374203857));
#86876=CARTESIAN_POINT('Ctrl Pts',(2.87658117469855,-29.1487475903056,53.1285256886587));
#86877=CARTESIAN_POINT('Ctrl Pts',(2.8804495088132,-29.085122062944,53.1601641587391));
#86878=CARTESIAN_POINT('Ctrl Pts',(2.8827472279862,-29.047329672272,53.1789568268887));
#86879=CARTESIAN_POINT('Ctrl Pts',(2.8850449471592,-29.010154926613,53.1988953386928));
#86880=CARTESIAN_POINT('Ctrl Pts',(2.8873426663322,-28.9736695586947,53.2199316339674));
#86881=CARTESIAN_POINT('Ctrl Pts',(2.89121173968022,-28.9122327363604,53.2553541391823));
#86882=CARTESIAN_POINT('Ctrl Pts',(2.89508081302825,-28.8525115731673,53.2940303836906));
#86883=CARTESIAN_POINT('Ctrl Pts',(2.89894988637628,-28.7948719569891,53.3357692580508));
#86884=CARTESIAN_POINT('Ctrl Pts',(2.90281319477187,-28.7373182243329,53.3774459411307));
#86885=CARTESIAN_POINT('Ctrl Pts',(2.90667650316746,-28.6818402725092,53.4221759133552));
#86886=CARTESIAN_POINT('Ctrl Pts',(2.91053981156305,-28.6287778654904,53.4697230903098));
#86887=CARTESIAN_POINT('Ctrl Pts',(2.91439858805576,-28.5757777040006,53.5172144914459));
#86888=CARTESIAN_POINT('Ctrl Pts',(2.91825736454848,-28.52518781889,53.5675162103332));
#86889=CARTESIAN_POINT('Ctrl Pts',(2.92211614104119,-28.4773161191118,53.6203510006588));
#86890=CARTESIAN_POINT('Ctrl Pts',(2.9259724866292,-28.42947457696,53.6731525067709));
#86891=CARTESIAN_POINT('Ctrl Pts',(2.9298288322172,-28.3843481482349,53.7284835592293));
#86892=CARTESIAN_POINT('Ctrl Pts',(2.9336851778052,-28.3422079092312,53.7860300883941));
#86893=CARTESIAN_POINT('Ctrl Pts',(2.93754038405033,-28.3000801204035,53.8435596156521));
#86894=CARTESIAN_POINT('Ctrl Pts',(2.94139559029546,-28.2609370566215,53.9033029284216));
#86895=CARTESIAN_POINT('Ctrl Pts',(2.94525079654059,-28.2250084196241,53.9649142779003));
#86896=CARTESIAN_POINT('Ctrl Pts',(2.94910615339164,-28.1890783790533,54.0265280342628));
#86897=CARTESIAN_POINT('Ctrl Pts',(2.95296151024268,-28.1563632573901,54.0900095514638));
#86898=CARTESIAN_POINT('Ctrl Pts',(2.95681686709372,-28.1270475759819,54.1549871126044));
#86899=CARTESIAN_POINT('Ctrl Pts',(2.96067625956207,-28.0977012082128,54.2200326893867));
#86900=CARTESIAN_POINT('Ctrl Pts',(2.96453565203042,-28.0717615842208,54.2865769924694));
#86901=CARTESIAN_POINT('Ctrl Pts',(2.96839504449877,-28.0493653045325,54.3542277124725));
#86902=CARTESIAN_POINT('Ctrl Pts',(2.97225662210199,-28.0269563443791,54.4219167353818));
#86903=CARTESIAN_POINT('Ctrl Pts',(2.97611819970521,-28.0080948507467,54.4907129535368));
#86904=CARTESIAN_POINT('Ctrl Pts',(2.97997977730844,-27.992866938006,54.5602109210647));
#86905=CARTESIAN_POINT('Ctrl Pts',(2.9838481114231,-27.9776123813449,54.6298304875504));
#86906=CARTESIAN_POINT('Ctrl Pts',(2.98771644553776,-27.9660041778331,54.7001537753637));
#86907=CARTESIAN_POINT('Ctrl Pts',(2.99158477965242,-27.9580768337136,54.7707679222213));
#86908=CARTESIAN_POINT('Ctrl Pts',(2.99388249882519,-27.9533681374033,54.8127114240737));
#86909=CARTESIAN_POINT('Ctrl Pts',(2.99618021799797,-27.9499571027309,54.8547574798927));
#86910=CARTESIAN_POINT('Ctrl Pts',(2.99847793717075,-27.9478422574973,54.8968197577716));
#86911=CARTESIAN_POINT('Ctrl Pts',(3.00034353126794,-27.9461251447923,54.9309715106293));
#86912=CARTESIAN_POINT('Ctrl Pts',(3.00220912536513,-27.945260491498,54.9651664828388));
#86913=CARTESIAN_POINT('Ctrl Pts',(3.00407471946232,-27.9452500948921,54.999375532939));
#86914=CARTESIAN_POINT('Ctrl Pts',(3.00407471949931,-27.9452500948919,54.9993755336174));
#86915=CARTESIAN_POINT('Ctrl Pts',(3.00791348792943,-27.9452287021789,55.0697663124844));
#86916=CARTESIAN_POINT('Ctrl Pts',(3.01175225635953,-27.9488287016156,55.1403032604115));
#86917=CARTESIAN_POINT('Ctrl Pts',(3.01559102478965,-27.9560689985433,55.2105792577255));
#86918=CARTESIAN_POINT('Ctrl Pts',(3.01950861575713,-27.9634579625723,55.2822982523251));
#86919=CARTESIAN_POINT('Ctrl Pts',(3.02342620672462,-27.9746384824612,55.3537449447915));
#86920=CARTESIAN_POINT('Ctrl Pts',(3.02734379769211,-27.9895745963596,55.4244846980723));
#86921=CARTESIAN_POINT('Ctrl Pts',(3.03117271153813,-28.0041726219795,55.4936232127996));
#86922=CARTESIAN_POINT('Ctrl Pts',(3.03500162538416,-28.0223579037011,55.5620859435652));
#86923=CARTESIAN_POINT('Ctrl Pts',(3.03883053923018,-28.0440446045511,55.6294728377892));
#86924=CARTESIAN_POINT('Ctrl Pts',(3.04265730106962,-28.0657191165859,55.6968218578154));
#86925=CARTESIAN_POINT('Ctrl Pts',(3.04648406290905,-28.0908909937632,55.763095771083));
#86926=CARTESIAN_POINT('Ctrl Pts',(3.05031082474849,-28.1194241368905,55.8279081987697));
#86927=CARTESIAN_POINT('Ctrl Pts',(3.05413676563533,-28.1479511588223,55.8927067222909));
#86928=CARTESIAN_POINT('Ctrl Pts',(3.05796270652218,-28.1798378159302,55.9560439306859));
#86929=CARTESIAN_POINT('Ctrl Pts',(3.06178864740903,-28.2149000053524,56.0175537192744));
#86930=CARTESIAN_POINT('Ctrl Pts',(3.06577402745905,-28.2514233480716,56.0816268169964));
#86931=CARTESIAN_POINT('Ctrl Pts',(3.06975940750908,-28.2913924556521,56.1437163194019));
#86932=CARTESIAN_POINT('Ctrl Pts',(3.0737447875591,-28.3345476417928,56.2034392402785));
#86933=CARTESIAN_POINT('Ctrl Pts',(3.07757550004275,-28.3760280296626,56.2608443900235));
#86934=CARTESIAN_POINT('Ctrl Pts',(3.08140621252639,-28.4204513813226,56.3160629059914));
#86935=CARTESIAN_POINT('Ctrl Pts',(3.08523692501004,-28.467545737203,56.3687883309465));
#86936=CARTESIAN_POINT('Ctrl Pts',(3.0890702692227,-28.514672447269,56.421549978675));
#86937=CARTESIAN_POINT('Ctrl Pts',(3.09290361343535,-28.5644734622282,56.4718147802386));
#86938=CARTESIAN_POINT('Ctrl Pts',(3.09673695764801,-28.6166409204184,56.5193140621475));
#86939=CARTESIAN_POINT('Ctrl Pts',(3.10057644985478,-28.6688920458213,56.5668895243547));
#86940=CARTESIAN_POINT('Ctrl Pts',(3.10441594206155,-28.7235167987091,56.6116903146885));
#86941=CARTESIAN_POINT('Ctrl Pts',(3.10825543426832,-28.78017627537,56.6534895352949));
#86942=CARTESIAN_POINT('Ctrl Pts',(3.10870802551532,-28.7868551750304,56.6584167392997));
#86943=CARTESIAN_POINT('Ctrl Pts',(3.10916061676232,-28.793562318163,56.6633022876481));
#86944=CARTESIAN_POINT('Ctrl Pts',(3.10961320800932,-28.8002971269466,56.668145850604));
#86945=CARTESIAN_POINT('Ctrl Pts',(3.11348228135749,-28.8578710843358,56.7095520873956));
#86946=CARTESIAN_POINT('Ctrl Pts',(3.11735135470566,-28.9177039567794,56.7480552898337));
#86947=CARTESIAN_POINT('Ctrl Pts',(3.12122042805384,-28.9794709514127,56.783400690672));
#86948=CARTESIAN_POINT('Ctrl Pts',(3.12508373644957,-29.0411459126947,56.8186934265603));
#86949=CARTESIAN_POINT('Ctrl Pts',(3.12894704484531,-29.1047488575599,56.8508374611335));
#86950=CARTESIAN_POINT('Ctrl Pts',(3.13281035324104,-29.1699247609691,56.879620349977));
#86951=CARTESIAN_POINT('Ctrl Pts',(3.13666912973391,-29.2350242089589,56.9083694746881));
#86952=CARTESIAN_POINT('Ctrl Pts',(3.14052790622678,-29.3016925081184,56.9337650901779));
#86953=CARTESIAN_POINT('Ctrl Pts',(3.14438668271965,-29.3695502355939,56.9556407280123));
#86954=CARTESIAN_POINT('Ctrl Pts',(3.14824302830782,-29.4373652148903,56.9775025849005));
#86955=CARTESIAN_POINT('Ctrl Pts',(3.15209937389599,-29.5063676746395,56.9958487148634));
#86956=CARTESIAN_POINT('Ctrl Pts',(3.15595571948416,-29.5761597972383,57.0105613755921));
#86957=CARTESIAN_POINT('Ctrl Pts',(3.15981092572945,-29.6459313000157,57.0252696895203));
#86958=CARTESIAN_POINT('Ctrl Pts',(3.16366613197474,-29.7164915273919,57.0363465652489));
#86959=CARTESIAN_POINT('Ctrl Pts',(3.16752133822003,-29.7874308248523,57.0437250079884));
#86960=CARTESIAN_POINT('Ctrl Pts',(3.17137669507123,-29.8583728935984,57.0511037389711));
#86961=CARTESIAN_POINT('Ctrl Pts',(3.17523205192243,-29.9296935784217,57.0547837020508));
#86962=CARTESIAN_POINT('Ctrl Pts',(3.17908740877364,-30.0009781593421,57.0547497671747));
#86963=CARTESIAN_POINT('Ctrl Pts',(3.18294680124216,-30.0723373578141,57.054715796777));
#86964=CARTESIAN_POINT('Ctrl Pts',(3.18680619371068,-30.1436598901606,57.0509601682432));
#86965=CARTESIAN_POINT('Ctrl Pts',(3.1906655861792,-30.2145319980673,57.0435199006384));
#86966=CARTESIAN_POINT('Ctrl Pts',(3.19452716378259,-30.2854442327858,57.0360754204565));
#86967=CARTESIAN_POINT('Ctrl Pts',(3.19838874138599,-30.3559050553296,57.0249422240914));
#86968=CARTESIAN_POINT('Ctrl Pts',(3.20225031898938,-30.4255095200008,57.0102087480878));
#86969=CARTESIAN_POINT('Ctrl Pts',(3.20611865310422,-30.4952357699654,56.9954494932681));
#86970=CARTESIAN_POINT('Ctrl Pts',(3.20998698721905,-30.5641022010401,56.9770775072827));
#86971=CARTESIAN_POINT('Ctrl Pts',(3.21385532133388,-30.6317183549069,56.9552313117822));
#86972=CARTESIAN_POINT('Ctrl Pts',(3.21615304050521,-30.6718811041471,56.9422550742774));
#86973=CARTESIAN_POINT('Ctrl Pts',(3.21845075967654,-30.7116030891717,56.9280540225237));
#86974=CARTESIAN_POINT('Ctrl Pts',(3.22074847884787,-30.7508062394283,56.9126650395026));
#86975=CARTESIAN_POINT('Ctrl Pts',(3.22461723638002,-30.8168140809136,56.8867540209945));
#86976=CARTESIAN_POINT('Ctrl Pts',(3.22848599391216,-30.8816083095328,56.8573712555002));
#86977=CARTESIAN_POINT('Ctrl Pts',(3.23235475144431,-30.9447988231827,56.8246514040256));
#86978=CARTESIAN_POINT('Ctrl Pts',(3.23621738593945,-31.0078893259504,56.7919833378748));
#86979=CARTESIAN_POINT('Ctrl Pts',(3.24008002043459,-31.069380726473,56.755988895384));
#86980=CARTESIAN_POINT('Ctrl Pts',(3.24394265492973,-31.1289021786639,56.7168510225142));
#86981=CARTESIAN_POINT('Ctrl Pts',(3.24667302071913,-31.1709758817289,56.6891857828214));
#86982=CARTESIAN_POINT('Ctrl Pts',(3.24940338650853,-31.2120656351482,56.6599509300902));
#86983=CARTESIAN_POINT('Ctrl Pts',(3.25213375229793,-31.2520475724682,56.6292251037768));
#86984=CARTESIAN_POINT('',(2.94592528057331,-27.9452500017688,55.0000852584629));
#86985=CARTESIAN_POINT('Ctrl Pts',(2.94592528057331,-27.9452500017688,55.0000852584629));
#86986=CARTESIAN_POINT('Ctrl Pts',(2.94997591064045,-27.9452531186631,55.075203179736));
#86987=CARTESIAN_POINT('Ctrl Pts',(2.95402654070758,-27.9493797866683,55.1502363805526));
#86988=CARTESIAN_POINT('Ctrl Pts',(2.95807717077472,-27.9575765752355,55.2247312093882));
#86989=CARTESIAN_POINT('Ctrl Pts',(2.96213971867074,-27.9657974805257,55.2994452181063));
#86990=CARTESIAN_POINT('Ctrl Pts',(2.96620226656675,-27.9781123929304,55.3736172816542));
#86991=CARTESIAN_POINT('Ctrl Pts',(2.97026481446277,-27.9944163846147,55.4468018847295));
#86992=CARTESIAN_POINT('Ctrl Pts',(2.97433371205507,-28.0107458591727,55.5201008741491));
#86993=CARTESIAN_POINT('Ctrl Pts',(2.97840260964737,-28.0310767338397,55.5924089327701));
#86994=CARTESIAN_POINT('Ctrl Pts',(2.98247150723968,-28.0552544358868,55.6632965048618));
#86995=CARTESIAN_POINT('Ctrl Pts',(2.98655160384029,-28.0794986833015,55.7343791839796));
#86996=CARTESIAN_POINT('Ctrl Pts',(2.99063170044091,-28.1076107675264,55.804033182481));
#86997=CARTESIAN_POINT('Ctrl Pts',(2.99471179704152,-28.13938810136,55.8718491412735));
#86998=CARTESIAN_POINT('Ctrl Pts',(2.99669196890805,-28.1548104279885,55.9047619045846));
#86999=CARTESIAN_POINT('Ctrl Pts',(2.99867214077457,-28.1710953858869,55.9372421261635));
#87000=CARTESIAN_POINT('Ctrl Pts',(3.0006523126411,-28.1882160943968,55.9692453981822));
#87001=CARTESIAN_POINT('Ctrl Pts',(3.00452138598909,-28.2216683810969,56.0317768425021));
#87002=CARTESIAN_POINT('Ctrl Pts',(3.00839045933707,-28.2584272837304,56.0926968909224));
#87003=CARTESIAN_POINT('Ctrl Pts',(3.01225953268506,-28.2983134164957,56.1516337673156));
#87004=CARTESIAN_POINT('Ctrl Pts',(3.01612284108062,-28.3381401185816,56.2104828272582));
#87005=CARTESIAN_POINT('Ctrl Pts',(3.01998614947617,-28.3810845315726,56.2673541816168));
#87006=CARTESIAN_POINT('Ctrl Pts',(3.02384945787173,-28.4269214872472,56.3219007357647));
#87007=CARTESIAN_POINT('Ctrl Pts',(3.02770823436442,-28.4727046733,56.3763833033861));
#87008=CARTESIAN_POINT('Ctrl Pts',(3.0315670108571,-28.5213733511166,56.4285461177086));
#87009=CARTESIAN_POINT('Ctrl Pts',(3.03542578734979,-28.5726601990824,56.4780726150012));
#87010=CARTESIAN_POINT('Ctrl Pts',(3.03928213293776,-28.6239147379885,56.5275679121983));
#87011=CARTESIAN_POINT('Ctrl Pts',(3.04313847852574,-28.6777838261136,56.5744298507));
#87012=CARTESIAN_POINT('Ctrl Pts',(3.04699482411372,-28.7339621666515,56.6183775106663));
#87013=CARTESIAN_POINT('Ctrl Pts',(3.05085003035882,-28.790123909509,56.6623121864608));
#87014=CARTESIAN_POINT('Ctrl Pts',(3.05470523660392,-28.8485931678945,56.7033339939136));
#87015=CARTESIAN_POINT('Ctrl Pts',(3.05856044284903,-28.9090316670453,56.7412023601495));
#87016=CARTESIAN_POINT('Ctrl Pts',(3.06241579970005,-28.9694725272619,56.7790722057355));
#87017=CARTESIAN_POINT('Ctrl Pts',(3.06627115655107,-29.0318823681512,56.8137881094636));
#87018=CARTESIAN_POINT('Ctrl Pts',(3.07012651340209,-29.0958955242342,56.8451538308229));
#87019=CARTESIAN_POINT('Ctrl Pts',(3.07398590587042,-29.1599756864626,56.8765523844343));
#87020=CARTESIAN_POINT('Ctrl Pts',(3.07784529833876,-29.2256620769808,56.904593541083));
#87021=CARTESIAN_POINT('Ctrl Pts',(3.08170469080709,-29.2925669254098,56.9291283024921));
#87022=CARTESIAN_POINT('Ctrl Pts',(3.08556626841031,-29.3595096544428,56.9536769551452));
#87023=CARTESIAN_POINT('Ctrl Pts',(3.08942784601352,-29.4276717503139,56.9747151171569));
#87024=CARTESIAN_POINT('Ctrl Pts',(3.09328942361673,-29.496650708445,56.9921438334596));
#87025=CARTESIAN_POINT('Ctrl Pts',(3.09715775773139,-29.5657503574356,57.009603044377));
#87026=CARTESIAN_POINT('Ctrl Pts',(3.10102609184604,-29.6356692455197,57.0234401064427));
#87027=CARTESIAN_POINT('Ctrl Pts',(3.10489442596069,-29.7059958154604,57.0336074109752));
#87028=CARTESIAN_POINT('Ctrl Pts',(3.10719214513368,-29.747768501928,57.0396466024901));
#87029=CARTESIAN_POINT('Ctrl Pts',(3.10948986430668,-29.7896849274336,57.0443920466834));
#87030=CARTESIAN_POINT('Ctrl Pts',(3.11178758347967,-29.8316587568884,57.0478424715704));
#87031=CARTESIAN_POINT('Ctrl Pts',(3.11565566451452,-29.9023193387308,57.0536510678621));
#87032=CARTESIAN_POINT('Ctrl Pts',(3.11952374554936,-29.9734192805823,57.0558095440457));
#87033=CARTESIAN_POINT('Ctrl Pts',(3.12339182658421,-30.0445492609425,57.0542670045175));
#87034=CARTESIAN_POINT('Ctrl Pts',(3.1272546011206,-30.1155816603244,57.0527265811507));
#87035=CARTESIAN_POINT('Ctrl Pts',(3.13111737565698,-30.1866435352803,57.0474952245094));
#87036=CARTESIAN_POINT('Ctrl Pts',(3.13498015019336,-30.2573213255353,57.0385738392133));
#87037=CARTESIAN_POINT('Ctrl Pts',(3.13883891816664,-30.3279258070782,57.0296617073935));
#87038=CARTESIAN_POINT('Ctrl Pts',(3.14269768613993,-30.3981465150949,57.0170672030046));
#87039=CARTESIAN_POINT('Ctrl Pts',(3.14655645411321,-30.4675725057126,57.0008432008535));
#87040=CARTESIAN_POINT('Ctrl Pts',(3.15049843878983,-30.538495710494,56.9842693181231));
#87041=CARTESIAN_POINT('Ctrl Pts',(3.15444042346644,-30.6085889994615,56.9639075857685));
#87042=CARTESIAN_POINT('Ctrl Pts',(3.15838240814305,-30.6774235720076,56.9398698066078));
#87043=CARTESIAN_POINT('Ctrl Pts',(3.16223780659657,-30.7447461839188,56.9163600204961));
#87044=CARTESIAN_POINT('Ctrl Pts',(3.1660932050501,-30.8108643475105,56.8893342390793));
#87045=CARTESIAN_POINT('Ctrl Pts',(3.16994860350362,-30.8753928403272,56.8589472659556));
#87046=CARTESIAN_POINT('Ctrl Pts',(3.17393388129178,-30.9420951467751,56.8275366269519));
#87047=CARTESIAN_POINT('Ctrl Pts',(3.17791915907993,-31.0070982448223,56.792534472704));
#87048=CARTESIAN_POINT('Ctrl Pts',(3.18190443686809,-31.0700020867776,56.7541645010636));
#87049=CARTESIAN_POINT('Ctrl Pts',(3.18588971465625,-31.1329059287328,56.7157945294232));
#87050=CARTESIAN_POINT('Ctrl Pts',(3.1898749924444,-31.1937100444688,56.6740570672336));
#87051=CARTESIAN_POINT('Ctrl Pts',(3.19386027023256,-31.2520475724682,56.6292251037768));
#87052=CARTESIAN_POINT('Ctrl Pts',(2.4939437805615,-31.2520475724682,56.6292251037768));
#87053=CARTESIAN_POINT('Ctrl Pts',(2.4977989078397,-31.3085916391625,56.5857714022116));
#87054=CARTESIAN_POINT('Ctrl Pts',(2.5016540351179,-31.3628837135078,56.539360769282));
#87055=CARTESIAN_POINT('Ctrl Pts',(2.5055091623961,-31.4146078579625,56.490262450272));
#87056=CARTESIAN_POINT('Ctrl Pts',(2.50936473298036,-31.4663379502433,56.441158485383));
#87057=CARTESIAN_POINT('Ctrl Pts',(2.51322030356461,-31.5154991758658,56.3893665571315));
#87058=CARTESIAN_POINT('Ctrl Pts',(2.51707587414886,-31.5618119435276,56.3351932502655));
#87059=CARTESIAN_POINT('Ctrl Pts',(2.52093566056926,-31.6081753514347,56.2809607081241));
#87060=CARTESIAN_POINT('Ctrl Pts',(2.52479544698966,-31.6516837706464,56.2243419617214));
#87061=CARTESIAN_POINT('Ctrl Pts',(2.52865523341006,-31.6920980780379,56.1656764803325));
#87062=CARTESIAN_POINT('Ctrl Pts',(2.53251746798286,-31.7325380190715,56.1069737891027));
#87063=CARTESIAN_POINT('Ctrl Pts',(2.53637970255566,-31.7698796889665,56.0462221933922));
#87064=CARTESIAN_POINT('Ctrl Pts',(2.54024193712846,-31.8039289149859,55.9837875950518));
#87065=CARTESIAN_POINT('Ctrl Pts',(2.54411066551593,-31.838035390082,55.9212480215467));
#87066=CARTESIAN_POINT('Ctrl Pts',(2.5479793939034,-31.8688381659839,55.8570202365651));
#87067=CARTESIAN_POINT('Ctrl Pts',(2.55184812229087,-31.8961907114886,55.7914912179957));
#87068=CARTESIAN_POINT('Ctrl Pts',(2.5532691579562,-31.9062376671823,55.7674215332891));
#87069=CARTESIAN_POINT('Ctrl Pts',(2.55469019362154,-31.9158196056307,55.7431764396063));
#87070=CARTESIAN_POINT('Ctrl Pts',(2.55611122928687,-31.9249309694336,55.718775573747));
#87071=CARTESIAN_POINT('Ctrl Pts',(2.55998030264425,-31.9497386050189,55.6523390005514));
#87072=CARTESIAN_POINT('Ctrl Pts',(2.56384937600163,-31.9711513322486,55.5844864813544));
#87073=CARTESIAN_POINT('Ctrl Pts',(2.56771844935902,-31.9890087674208,55.5155983762805));
#87074=CARTESIAN_POINT('Ctrl Pts',(2.57158175776409,-32.0068395948623,55.4468129150708));
#87075=CARTESIAN_POINT('Ctrl Pts',(2.57544506616916,-32.021125524562,55.3769953972711));
#87076=CARTESIAN_POINT('Ctrl Pts',(2.57930837457424,-32.0317549564942,55.3065442207271));
#87077=CARTESIAN_POINT('Ctrl Pts',(2.58316715107659,-32.0423719194371,55.2361756878255));
#87078=CARTESIAN_POINT('Ctrl Pts',(2.58702592757895,-32.0493408324931,55.1651754506854));
#87079=CARTESIAN_POINT('Ctrl Pts',(2.5908847040813,-32.05260086952,55.0939533551597));
#87080=CARTESIAN_POINT('Ctrl Pts',(2.59474104967903,-32.0558588528288,55.0227761272549));
#87081=CARTESIAN_POINT('Ctrl Pts',(2.59859739527676,-32.0554125734715,54.951377802384));
#87082=CARTESIAN_POINT('Ctrl Pts',(2.6024537408745,-32.0512530538119,54.8801731594036));
#87083=CARTESIAN_POINT('Ctrl Pts',(2.60630894712943,-32.0470947630668,54.8089895535672));
#87084=CARTESIAN_POINT('Ctrl Pts',(2.61016415338436,-32.039225438307,54.7380000007136));
#87085=CARTESIAN_POINT('Ctrl Pts',(2.61401935963929,-32.0276881760292,54.6676173541059));
#87086=CARTESIAN_POINT('Ctrl Pts',(2.61787471650019,-32.0161504630412,54.5972319579573));
#87087=CARTESIAN_POINT('Ctrl Pts',(2.62173007336109,-32.000944608807,54.5274539941576));
#87088=CARTESIAN_POINT('Ctrl Pts',(2.625585430222,-31.9821650810571,54.458687563474));
#87089=CARTESIAN_POINT('Ctrl Pts',(2.62944482270023,-31.9633658957268,54.389849151127));
#87090=CARTESIAN_POINT('Ctrl Pts',(2.63330421517847,-31.9409856977157,54.3220248551406));
#87091=CARTESIAN_POINT('Ctrl Pts',(2.63716360765671,-31.9151690153129,54.2556041340218));
#87092=CARTESIAN_POINT('Ctrl Pts',(2.64102518526984,-31.8893377158598,54.189145806405));
#87093=CARTESIAN_POINT('Ctrl Pts',(2.64488676288298,-31.8600662581771,54.1240930788425));
#87094=CARTESIAN_POINT('Ctrl Pts',(2.64874834049612,-31.8275464605445,54.0608133853961));
#87095=CARTESIAN_POINT('Ctrl Pts',(2.65261667462063,-31.7949697637881,53.9974229729609));
#87096=CARTESIAN_POINT('Ctrl Pts',(2.65648500874514,-31.7591336240462,53.9358122083976));
#87097=CARTESIAN_POINT('Ctrl Pts',(2.66035334286965,-31.7202743717362,53.8763213767061));
#87098=CARTESIAN_POINT('Ctrl Pts',(2.66265106195491,-31.6971926929572,53.8409849205015));
#87099=CARTESIAN_POINT('Ctrl Pts',(2.66494878104017,-31.6730452280721,53.8063958214799));
#87100=CARTESIAN_POINT('Ctrl Pts',(2.66724650012543,-31.6478880931675,53.7726197024162));
#87101=CARTESIAN_POINT('Ctrl Pts',(2.67111557347257,-31.6055266048661,53.7157449160781));
#87102=CARTESIAN_POINT('Ctrl Pts',(2.67498464681972,-31.5601342423003,53.6609543818503));
#87103=CARTESIAN_POINT('Ctrl Pts',(2.67885372016687,-31.511943576216,53.6085891387375));
#87104=CARTESIAN_POINT('Ctrl Pts',(2.68271702856159,-31.4638247146368,53.5563019202854));
#87105=CARTESIAN_POINT('Ctrl Pts',(2.68658033695631,-31.4129161521506,53.5064331743893));
#87106=CARTESIAN_POINT('Ctrl Pts',(2.69044364535103,-31.3594920722925,53.4592927377747));
#87107=CARTESIAN_POINT('Ctrl Pts',(2.69430242184289,-31.3061306622283,53.4122075998466));
#87108=CARTESIAN_POINT('Ctrl Pts',(2.69816119833475,-31.2502599586848,53.367844733821));
#87109=CARTESIAN_POINT('Ctrl Pts',(2.70201997482661,-31.1921913010982,53.3264775280607));
#87110=CARTESIAN_POINT('Ctrl Pts',(2.70587632041377,-31.1341592248924,53.2851363823054));
#87111=CARTESIAN_POINT('Ctrl Pts',(2.70973266600094,-31.0739323364675,53.2467874338947));
#87112=CARTESIAN_POINT('Ctrl Pts',(2.7135890115881,-31.0118542404584,53.2116631864868));
#87113=CARTESIAN_POINT('Ctrl Pts',(2.7174442178324,-30.9497944851904,53.1765493164064));
#87114=CARTESIAN_POINT('Ctrl Pts',(2.72129942407669,-30.8858850307203,53.1446584949976));
#87115=CARTESIAN_POINT('Ctrl Pts',(2.72515463032099,-30.8204961070475,53.1161784317988));
#87116=CARTESIAN_POINT('Ctrl Pts',(2.72900998717122,-30.7551046289172,53.0876972560093));
#87117=CARTESIAN_POINT('Ctrl Pts',(2.73286534402146,-30.6882340130916,53.0626272949301));
#87118=CARTESIAN_POINT('Ctrl Pts',(2.73672070087169,-30.6202749981291,53.0411083518489));
#87119=CARTESIAN_POINT('Ctrl Pts',(2.74058009333926,-30.5522448466702,53.0195668836883));
#87120=CARTESIAN_POINT('Ctrl Pts',(2.74443948580683,-30.4831244858713,53.0015840005369));
#87121=CARTESIAN_POINT('Ctrl Pts',(2.7482988782744,-30.4133195037398,52.987249506191));
#87122=CARTESIAN_POINT('Ctrl Pts',(2.75216045587686,-30.3434749989882,52.9729068958518));
#87123=CARTESIAN_POINT('Ctrl Pts',(2.75602203347932,-30.2729455817938,52.9622168592576));
#87124=CARTESIAN_POINT('Ctrl Pts',(2.75988361108177,-30.2021439848606,52.9552175245556));
#87125=CARTESIAN_POINT('Ctrl Pts',(2.7637519451957,-30.1312185080393,52.9482059432823));
#87126=CARTESIAN_POINT('Ctrl Pts',(2.76762027930962,-30.0600203860959,52.9448979791087));
#87127=CARTESIAN_POINT('Ctrl Pts',(2.77148861342355,-29.9889636844098,52.9452796389196));
#87128=CARTESIAN_POINT('Ctrl Pts',(2.7737863326037,-29.9467573130019,52.9455063378143));
#87129=CARTESIAN_POINT('Ctrl Pts',(2.77608405178384,-29.9046007848128,52.9470337898437));
#87130=CARTESIAN_POINT('Ctrl Pts',(2.77838177096399,-29.8625796677549,52.9498504408737));
#87131=CARTESIAN_POINT('Ctrl Pts',(2.78225084431046,-29.7918213325315,52.9545933309191));
#87132=CARTESIAN_POINT('Ctrl Pts',(2.78611991765693,-29.7211702309432,52.9630130139421));
#87133=CARTESIAN_POINT('Ctrl Pts',(2.7899889910034,-29.6510390227326,52.9750990644368));
#87134=CARTESIAN_POINT('Ctrl Pts',(2.79385229939739,-29.5810123106239,52.9871671066127));
#87135=CARTESIAN_POINT('Ctrl Pts',(2.79771560779139,-29.5115044290717,53.0028905906901));
#87136=CARTESIAN_POINT('Ctrl Pts',(2.80157891618538,-29.4429243927077,53.0222072074507));
#87137=CARTESIAN_POINT('Ctrl Pts',(2.80543769267647,-29.3744248050251,53.0415011646091));
#87138=CARTESIAN_POINT('Ctrl Pts',(2.80929646916756,-29.3068513658813,53.0643797510297));
#87139=CARTESIAN_POINT('Ctrl Pts',(2.81315524565865,-29.2406026200768,53.0907296729206));
#87140=CARTESIAN_POINT('Ctrl Pts',(2.817011591245,-29.1743956088454,53.1170629952106));
#87141=CARTESIAN_POINT('Ctrl Pts',(2.82086793683135,-29.1095120856153,53.1468631352237));
#87142=CARTESIAN_POINT('Ctrl Pts',(2.8247242824177,-29.0463337456507,53.1799675173736));
#87143=CARTESIAN_POINT('Ctrl Pts',(2.82857948866115,-28.9831740714906,53.2130621189574));
#87144=CARTESIAN_POINT('Ctrl Pts',(2.83243469490461,-28.9217190104928,53.2494587992553));
#87145=CARTESIAN_POINT('Ctrl Pts',(2.83628990114806,-28.862327065072,53.2889483188307));
#87146=CARTESIAN_POINT('Ctrl Pts',(2.84014525799741,-28.8029327994699,53.3284393810874));
#87147=CARTESIAN_POINT('Ctrl Pts',(2.84400061484677,-28.745602212768,53.371023251697));
#87148=CARTESIAN_POINT('Ctrl Pts',(2.84785597169612,-28.6906646823592,53.4164474784591));
#87149=CARTESIAN_POINT('Ctrl Pts',(2.85171536416276,-28.6356696457698,53.4619192532957));
#87150=CARTESIAN_POINT('Ctrl Pts',(2.85557475662939,-28.5830730410599,53.5102370091905));
#87151=CARTESIAN_POINT('Ctrl Pts',(2.85943414909603,-28.5331702926792,53.5611087003456));
#87152=CARTESIAN_POINT('Ctrl Pts',(2.86329572669754,-28.4832392900495,53.6120091943517));
#87153=CARTESIAN_POINT('Ctrl Pts',(2.86715730429904,-28.4360055018113,53.6654661379536));
#87154=CARTESIAN_POINT('Ctrl Pts',(2.87101888190054,-28.3917248124773,53.7211534557661));
#87155=CARTESIAN_POINT('Ctrl Pts',(2.87488721601348,-28.3473666462636,53.7769382083678));
#87156=CARTESIAN_POINT('Ctrl Pts',(2.87875555012642,-28.3059721771753,53.8349607309138));
#87157=CARTESIAN_POINT('Ctrl Pts',(2.88262388423935,-28.2677542231778,53.8948655596799));
#87158=CARTESIAN_POINT('Ctrl Pts',(2.88492160342708,-28.2450534626819,53.9304479242005));
#87159=CARTESIAN_POINT('Ctrl Pts',(2.88721932261481,-28.2234725547324,53.9666938950509));
#87160=CARTESIAN_POINT('Ctrl Pts',(2.88951704180255,-28.2030482011612,54.0035253163528));
#87161=CARTESIAN_POINT('Ctrl Pts',(2.89357123056583,-28.167010644793,54.0685121673027));
#87162=CARTESIAN_POINT('Ctrl Pts',(2.89762541932912,-28.1344462576373,54.1355570099439));
#87163=CARTESIAN_POINT('Ctrl Pts',(2.90167960809241,-28.1055831555683,54.2042724197104));
#87164=CARTESIAN_POINT('Ctrl Pts',(2.9057224180279,-28.0768010631136,54.2727949670179));
#87165=CARTESIAN_POINT('Ctrl Pts',(2.9097652279634,-28.0516997313481,54.3429783611871));
#87166=CARTESIAN_POINT('Ctrl Pts',(2.9138080378989,-28.0304609873698,54.4144117144035));
#87167=CARTESIAN_POINT('Ctrl Pts',(2.91784402707854,-28.0092580759659,54.4857245500912));
#87168=CARTESIAN_POINT('Ctrl Pts',(2.92188001625818,-27.9919049146791,54.5582827532555));
#87169=CARTESIAN_POINT('Ctrl Pts',(2.92591600543781,-27.9785350595101,54.6316563332019));
#87170=CARTESIAN_POINT('Ctrl Pts',(2.92994364806252,-27.96519285363,54.7048781742343));
#87171=CARTESIAN_POINT('Ctrl Pts',(2.93397129068723,-27.9558176275774,54.7789116245549));
#87172=CARTESIAN_POINT('Ctrl Pts',(2.93799893331193,-27.9504925475353,54.8533140606889));
#87173=CARTESIAN_POINT('Ctrl Pts',(2.94064104905385,-27.9469993185879,54.9021217296069));
#87174=CARTESIAN_POINT('Ctrl Pts',(2.94328316479576,-27.9452479687193,54.9510878823304));
#87175=CARTESIAN_POINT('Ctrl Pts',(2.94592528053768,-27.9452500017688,55.0000852578022));
#87176=CARTESIAN_POINT('Origin',(-1.54592528053767,-30.,55.));
#87177=CARTESIAN_POINT('',(1.79398371971565,-31.2520475724682,56.6292251037768));
#87178=CARTESIAN_POINT('',(1.85198267751189,-31.2510897925305,56.6279533612582));
#87179=CARTESIAN_POINT('',(-1.54592528053767,-31.2520475724682,56.6292251037768));
#87180=CARTESIAN_POINT('',(2.30407472893164,-27.94525085778,55.0018775106036));
#87181=CARTESIAN_POINT('Ctrl Pts',(1.85198267751188,-31.2510897925303,56.6279533612584));
#87182=CARTESIAN_POINT('Ctrl Pts',(1.86369686126964,-31.4238148888446,56.4975418353466));
#87183=CARTESIAN_POINT('Ctrl Pts',(1.91245613530692,-32.0571540930741,55.8463606150952));
#87184=CARTESIAN_POINT('Ctrl Pts',(1.99826049962372,-32.2401039315954,54.0618361945102));
#87185=CARTESIAN_POINT('Ctrl Pts',(2.10939577046228,-30.4267596474104,52.6091647644781));
#87186=CARTESIAN_POINT('Ctrl Pts',(2.21133384374181,-28.4052057105241,53.2838821759632));
#87187=CARTESIAN_POINT('Ctrl Pts',(2.27622682674183,-27.9501900713887,54.4882110047797));
#87188=CARTESIAN_POINT('Ctrl Pts',(2.30407471946232,-27.9455375406346,55.0018770739853));
#87189=CARTESIAN_POINT('Ctrl Pts',(2.30407472893164,-27.94525085778,55.0018775106036));
#87190=CARTESIAN_POINT('Ctrl Pts',(2.30909837625683,-27.9453355391577,55.094552879717));
#87191=CARTESIAN_POINT('Ctrl Pts',(2.31412202358202,-27.951693882386,55.1869490611887));
#87192=CARTESIAN_POINT('Ctrl Pts',(2.3191456709072,-27.9641908887325,55.278350184085));
#87193=CARTESIAN_POINT('Ctrl Pts',(2.3233192179846,-27.9745731550298,55.354284433574));
#87194=CARTESIAN_POINT('Ctrl Pts',(2.327492765062,-27.9891913884281,55.4295325551457));
#87195=CARTESIAN_POINT('Ctrl Pts',(2.3316663121394,-28.0079438906639,55.5036963567039));
#87196=CARTESIAN_POINT('Ctrl Pts',(2.33553538549683,-28.0253283373804,55.5724496697427));
#87197=CARTESIAN_POINT('Ctrl Pts',(2.33940445885427,-28.0463104154775,55.6404365923651));
#87198=CARTESIAN_POINT('Ctrl Pts',(2.3432735322117,-28.070805693686,55.707253060075));
#87199=CARTESIAN_POINT('Ctrl Pts',(2.34713684061684,-28.095264473721,55.7739699706783));
#87200=CARTESIAN_POINT('Ctrl Pts',(2.35100014902197,-28.1232258972913,55.83951943575));
#87201=CARTESIAN_POINT('Ctrl Pts',(2.35486345742711,-28.1545551496884,55.9035103026299));
#87202=CARTESIAN_POINT('Ctrl Pts',(2.35872223392952,-28.1858476509101,55.9674261042151));
#87203=CARTESIAN_POINT('Ctrl Pts',(2.36258101043192,-28.2204999210114,56.0297865051127));
#87204=CARTESIAN_POINT('Ctrl Pts',(2.36643978693433,-28.2583288730812,56.0902198164395));
#87205=CARTESIAN_POINT('Ctrl Pts',(2.37029613253212,-28.2961339941324,56.1506150567312));
#87206=CARTESIAN_POINT('Ctrl Pts',(2.37415247812991,-28.3371115696483,56.2090852052227));
#87207=CARTESIAN_POINT('Ctrl Pts',(2.3780088237277,-28.3810330623122,56.2652840065273));
#87208=CARTESIAN_POINT('Ctrl Pts',(2.38186402998269,-28.4249415785363,56.3214662041075));
#87209=CARTESIAN_POINT('Ctrl Pts',(2.38571923623769,-28.4717919861991,56.3753780041934));
#87210=CARTESIAN_POINT('Ctrl Pts',(2.38957444249268,-28.5213140130926,56.4267043543158));
#87211=CARTESIAN_POINT('Ctrl Pts',(2.39342979935363,-28.5708379745941,56.4780327095331));
#87212=CARTESIAN_POINT('Ctrl Pts',(2.39728515621459,-28.6230334236482,56.5267750661973));
#87213=CARTESIAN_POINT('Ctrl Pts',(2.40114051307555,-28.6775928143398,56.5726527899744));
#87214=CARTESIAN_POINT('Ctrl Pts',(2.40499990555384,-28.7322093153926,56.6185785365271));
#87215=CARTESIAN_POINT('Ctrl Pts',(2.40885929803214,-28.7891943251104,56.6616333510855));
#87216=CARTESIAN_POINT('Ctrl Pts',(2.41271869051043,-28.848207451908,56.7015791161917));
#87217=CARTESIAN_POINT('Ctrl Pts',(2.41658026812362,-28.9072539911257,56.7415474980403));
#87218=CARTESIAN_POINT('Ctrl Pts',(2.42044184573681,-28.9683305171944,56.7784030751178));
#87219=CARTESIAN_POINT('Ctrl Pts',(2.42430342335001,-29.0310702705056,56.8119527427066));
#87220=CARTESIAN_POINT('Ctrl Pts',(2.42817175747458,-29.0939197980851,56.8455611113584));
#87221=CARTESIAN_POINT('Ctrl Pts',(2.43204009159915,-29.1584379231518,56.8758518155378));
#87222=CARTESIAN_POINT('Ctrl Pts',(2.43590842572371,-29.2242367176355,56.9026793981738));
#87223=CARTESIAN_POINT('Ctrl Pts',(2.43820614480846,-29.2633199873247,56.9186144871902));
#87224=CARTESIAN_POINT('Ctrl Pts',(2.44050386389321,-29.3028547612633,56.9333286803494));
#87225=CARTESIAN_POINT('Ctrl Pts',(2.44280158297796,-29.3427575594089,56.946799922125));
#87226=CARTESIAN_POINT('Ctrl Pts',(2.44667069995754,-29.4099496695596,56.9694840746987));
#87227=CARTESIAN_POINT('Ctrl Pts',(2.45053981693712,-29.4784491573178,56.9887299601906));
#87228=CARTESIAN_POINT('Ctrl Pts',(2.4544089339167,-29.5478707448616,57.0043893581707));
#87229=CARTESIAN_POINT('Ctrl Pts',(2.45827227321816,-29.6171886664814,57.0200253722724));
#87230=CARTESIAN_POINT('Ctrl Pts',(2.46213561251963,-29.6874254845863,57.032085423783));
#87231=CARTESIAN_POINT('Ctrl Pts',(2.4659989518211,-29.7581794462689,57.0404706276477));
#87232=CARTESIAN_POINT('Ctrl Pts',(2.46985771066891,-29.8288495206153,57.0488458898442));
#87233=CARTESIAN_POINT('Ctrl Pts',(2.47371646951672,-29.9000350404802,57.0535549025545));
#87234=CARTESIAN_POINT('Ctrl Pts',(2.47757522836452,-29.9713244395928,57.0545498958982));
#87235=CARTESIAN_POINT('Ctrl Pts',(2.48143153828646,-30.0425685955429,57.0555442577785));
#87236=CARTESIAN_POINT('Ctrl Pts',(2.4852878482084,-30.1139160153628,57.052829270212));
#87237=CARTESIAN_POINT('Ctrl Pts',(2.48914415813034,-30.1849518558916,57.046409141277));
#87238=CARTESIAN_POINT('Ctrl Pts',(2.49299931069925,-30.2559663771938,57.0399909391467));
#87239=CARTESIAN_POINT('Ctrl Pts',(2.49685446326816,-30.3266690213528,57.0298698472306));
#87240=CARTESIAN_POINT('Ctrl Pts',(2.50070961583707,-30.3966485302921,57.016102057416));
#87241=CARTESIAN_POINT('Ctrl Pts',(2.50456490098836,-30.4666304458936,57.0023337941139));
#87242=CARTESIAN_POINT('Ctrl Pts',(2.50842018613966,-30.5358887007757,56.9849186801404));
#87243=CARTESIAN_POINT('Ctrl Pts',(2.51227547129095,-30.6040224223521,56.963963970086));
#87244=CARTESIAN_POINT('Ctrl Pts',(2.51613458294686,-30.6722237690172,56.942988461753));
#87245=CARTESIAN_POINT('Ctrl Pts',(2.51999369460276,-30.7392978896813,56.9184664888671));
#87246=CARTESIAN_POINT('Ctrl Pts',(2.52385280625866,-30.8048601979397,56.8905548456135));
#87247=CARTESIAN_POINT('Ctrl Pts',(2.52771409565969,-30.8704595038312,56.8626274514693));
#87248=CARTESIAN_POINT('Ctrl Pts',(2.53157538506072,-30.934544862529,56.8313067925013));
#87249=CARTESIAN_POINT('Ctrl Pts',(2.53543667446175,-30.996755198201,56.7967962147554));
#87250=CARTESIAN_POINT('Ctrl Pts',(2.539304243646,-31.0590667092529,56.762229510953));
#87251=CARTESIAN_POINT('Ctrl Pts',(2.54317181283025,-31.1194966994414,56.7244627914467));
#87252=CARTESIAN_POINT('Ctrl Pts',(2.5470393820145,-31.1777127538234,56.683742923365));
#87253=CARTESIAN_POINT('Ctrl Pts',(2.54871360662626,-31.2029137900305,56.666115777713));
#87254=CARTESIAN_POINT('Ctrl Pts',(2.55038783123802,-31.2277003728419,56.6479357485599));
#87255=CARTESIAN_POINT('Ctrl Pts',(2.55206205584979,-31.2520475724682,56.6292251037768));
#87256=CARTESIAN_POINT('',(2.24592528056623,-27.9452508239567,54.9981598779332));
#87257=CARTESIAN_POINT('Ctrl Pts',(2.24592528056623,-27.9452508239567,54.9981598779332));
#87258=CARTESIAN_POINT('Ctrl Pts',(2.24973199312503,-27.9451880223023,55.0682865558788));
#87259=CARTESIAN_POINT('Ctrl Pts',(2.25353870568382,-27.9487194886746,55.1385255805472));
#87260=CARTESIAN_POINT('Ctrl Pts',(2.25734541824262,-27.9558530803982,55.2084728605418));
#87261=CARTESIAN_POINT('Ctrl Pts',(2.26114901960389,-27.962980841891,55.2783629731508));
#87262=CARTESIAN_POINT('Ctrl Pts',(2.26495262096516,-27.9737048438551,55.3479613175438));
#87263=CARTESIAN_POINT('Ctrl Pts',(2.26875622232642,-27.9879809101615,55.4168653794998));
#87264=CARTESIAN_POINT('Ctrl Pts',(2.27255807195645,-28.0022504016908,55.4857377080047));
#87265=CARTESIAN_POINT('Ctrl Pts',(2.27635992158647,-28.0200686123143,55.5539158983948));
#87266=CARTESIAN_POINT('Ctrl Pts',(2.2801617712165,-28.0413399868185,55.6210060509077));
#87267=CARTESIAN_POINT('Ctrl Pts',(2.28396322602616,-28.0626091523002,55.6880892361387));
#87268=CARTESIAN_POINT('Ctrl Pts',(2.28776468083582,-28.0873306169522,55.7540841309453));
#87269=CARTESIAN_POINT('Ctrl Pts',(2.29156613564548,-28.115359074996,55.8186123296774));
#87270=CARTESIAN_POINT('Ctrl Pts',(2.295371110743,-28.1434134884292,55.8832002839099));
#87271=CARTESIAN_POINT('Ctrl Pts',(2.29917608584051,-28.1747808101523,55.9463183697255));
#87272=CARTESIAN_POINT('Ctrl Pts',(2.30298106093803,-28.209268150215,56.0076095497095));
#87273=CARTESIAN_POINT('Ctrl Pts',(2.3067878558536,-28.2437719846523,56.0689300436293));
#87274=CARTESIAN_POINT('Ctrl Pts',(2.31059465076918,-28.281398538287,56.1284214698724));
#87275=CARTESIAN_POINT('Ctrl Pts',(2.31440144568475,-28.3219111830263,56.1857552381701));
#87276=CARTESIAN_POINT('Ctrl Pts',(2.31821492477245,-28.3624949620128,56.2431896761346));
#87277=CARTESIAN_POINT('Ctrl Pts',(2.32202840386014,-28.4059746382782,56.2984584996802));
#87278=CARTESIAN_POINT('Ctrl Pts',(2.32584188294784,-28.4520733984623,56.3512663685417));
#87279=CARTESIAN_POINT('Ctrl Pts',(2.32850815116848,-28.4843042450103,56.3881880191675));
#87280=CARTESIAN_POINT('Ctrl Pts',(2.33117441938912,-28.517814575004,56.4239073940283));
#87281=CARTESIAN_POINT('Ctrl Pts',(2.33384068760975,-28.5524999386103,56.458335055732));
#87282=CARTESIAN_POINT('Ctrl Pts',(2.33770976095524,-28.6028325400977,56.508293701008));
#87283=CARTESIAN_POINT('Ctrl Pts',(2.34157883430073,-28.6558531559513,56.5557413933927));
#87284=CARTESIAN_POINT('Ctrl Pts',(2.34544790764622,-28.7112811807228,56.6003753832588));
#87285=CARTESIAN_POINT('Ctrl Pts',(2.34931121603942,-28.7666266172646,56.6449428680993));
#87286=CARTESIAN_POINT('Ctrl Pts',(2.35317452443262,-28.8243719672316,56.6867046701006));
#87287=CARTESIAN_POINT('Ctrl Pts',(2.35703783282581,-28.8842001035252,56.7253950717232));
#87288=CARTESIAN_POINT('Ctrl Pts',(2.36089660931638,-28.943958057669,56.7640400870823));
#87289=CARTESIAN_POINT('Ctrl Pts',(2.36475538580694,-29.0057935391012,56.799620596212));
#87290=CARTESIAN_POINT('Ctrl Pts',(2.3686141622975,-29.0693580851263,56.8319124402602));
#87291=CARTESIAN_POINT('Ctrl Pts',(2.3724705078835,-29.1328825875402,56.8641839414896));
#87292=CARTESIAN_POINT('Ctrl Pts',(2.3763268534695,-29.1981335614045,56.8931706684583));
#87293=CARTESIAN_POINT('Ctrl Pts',(2.3801831990555,-29.264736703325,56.9186936824472));
#87294=CARTESIAN_POINT('Ctrl Pts',(2.38403840529877,-29.331320167599,56.944209155758));
#87295=CARTESIAN_POINT('Ctrl Pts',(2.38789361154204,-29.3992545534528,56.9662627739669));
#87296=CARTESIAN_POINT('Ctrl Pts',(2.39174881778531,-29.4681458743348,56.9847238476707));
#87297=CARTESIAN_POINT('Ctrl Pts',(2.39560417463466,-29.5370398864998,57.0031856425681));
#87298=CARTESIAN_POINT('Ctrl Pts',(2.399459531484,-29.6068904381121,57.0180544907098));
#87299=CARTESIAN_POINT('Ctrl Pts',(2.40331488833334,-29.6772903703766,57.0292501219535));
#87300=CARTESIAN_POINT('Ctrl Pts',(2.40717428080024,-29.747763994186,57.0404574722903));
#87301=CARTESIAN_POINT('Ctrl Pts',(2.41103367326713,-29.818787665871,57.0479838538703));
#87302=CARTESIAN_POINT('Ctrl Pts',(2.41489306573403,-29.8899469614783,57.0518006460697));
#87303=CARTESIAN_POINT('Ctrl Pts',(2.41875464333594,-29.9611465465016,57.0556195992845));
#87304=CARTESIAN_POINT('Ctrl Pts',(2.42261622093785,-30.0324814222935,57.0557247813156));
#87305=CARTESIAN_POINT('Ctrl Pts',(2.42647779853975,-30.103537767924,57.0521397352796));
#87306=CARTESIAN_POINT('Ctrl Pts',(2.43034613265333,-30.1747184391743,57.0485484165726));
#87307=CARTESIAN_POINT('Ctrl Pts',(2.43421446676691,-30.2456191238906,57.0412540285306));
#87308=CARTESIAN_POINT('Ctrl Pts',(2.43808280088049,-30.3158324179635,57.0303318561908));
#87309=CARTESIAN_POINT('Ctrl Pts',(2.44038052006976,-30.3575378209603,57.0238442870624));
#87310=CARTESIAN_POINT('Ctrl Pts',(2.44267823925904,-30.3990009022484,57.0160777639563));
#87311=CARTESIAN_POINT('Ctrl Pts',(2.44497595844831,-30.4401387559793,57.0070564112613));
#87312=CARTESIAN_POINT('Ctrl Pts',(2.44884535137329,-30.5094155069934,56.9918643205764));
#87313=CARTESIAN_POINT('Ctrl Pts',(2.45271474429828,-30.5780404718284,56.9730514624935));
#87314=CARTESIAN_POINT('Ctrl Pts',(2.45658413722326,-30.6456070065421,56.9506894052113));
#87315=CARTESIAN_POINT('Ctrl Pts',(2.46044683547002,-30.7130566401767,56.9283660379203));
#87316=CARTESIAN_POINT('Ctrl Pts',(2.46430953371679,-30.7794510248455,56.9025058240084));
#87317=CARTESIAN_POINT('Ctrl Pts',(2.46817223196355,-30.8443951085459,56.8732310223685));
#87318=CARTESIAN_POINT('Ctrl Pts',(2.4720310850811,-30.9092745435532,56.8439853623772));
#87319=CARTESIAN_POINT('Ctrl Pts',(2.47588993819866,-30.9727061011769,56.8113320565288));
#87320=CARTESIAN_POINT('Ctrl Pts',(2.47974879131621,-31.0343124383689,56.7754422948481));
#87321=CARTESIAN_POINT('Ctrl Pts',(2.48360488003591,-31.0958746421304,56.7395782438064));
#87322=CARTESIAN_POINT('Ctrl Pts',(2.48746096875562,-31.1556138035919,56.7004825855342));
#87323=CARTESIAN_POINT('Ctrl Pts',(2.49131705747533,-31.2131766480482,56.6583726912641));
#87324=CARTESIAN_POINT('Ctrl Pts',(2.49219263183739,-31.2262470295867,56.6488111001048));
#87325=CARTESIAN_POINT('Ctrl Pts',(2.49306820619944,-31.2392053155072,56.6390942842944));
#87326=CARTESIAN_POINT('Ctrl Pts',(2.4939437805615,-31.2520475724682,56.6292251037768));
#87327=CARTESIAN_POINT('Ctrl Pts',(1.79398371971565,-31.2520475724682,56.6292251037768));
#87328=CARTESIAN_POINT('Ctrl Pts',(1.79795521490481,-31.3100301074008,56.5846659498946));
#87329=CARTESIAN_POINT('Ctrl Pts',(1.80192671009397,-31.365713925972,56.5369438826613));
#87330=CARTESIAN_POINT('Ctrl Pts',(1.80589820528314,-31.4187392548253,56.4863298723089));
#87331=CARTESIAN_POINT('Ctrl Pts',(1.80975587414567,-31.4702448340343,56.4371665012244));
#87332=CARTESIAN_POINT('Ctrl Pts',(1.8136135430082,-31.5192418864264,56.3852750899823));
#87333=CARTESIAN_POINT('Ctrl Pts',(1.81747121187074,-31.565433662945,56.3309451564278));
#87334=CARTESIAN_POINT('Ctrl Pts',(1.82132695612579,-31.6116023941888,56.2766423283094));
#87335=CARTESIAN_POINT('Ctrl Pts',(1.82518270038085,-31.6549683125772,56.2199037615503));
#87336=CARTESIAN_POINT('Ctrl Pts',(1.8290384446359,-31.6952730400049,56.1610542116252));
#87337=CARTESIAN_POINT('Ctrl Pts',(1.83289355506024,-31.735571141896,56.1022143357474));
#87338=CARTESIAN_POINT('Ctrl Pts',(1.83674866548457,-31.7728087781897,56.0412645668965));
#87339=CARTESIAN_POINT('Ctrl Pts',(1.84060377590891,-31.8067702540875,55.9785595594773));
#87340=CARTESIAN_POINT('Ctrl Pts',(1.84466176160446,-31.8425189534045,55.912554699658));
#87341=CARTESIAN_POINT('Ctrl Pts',(1.84871974730001,-31.874636879848,55.8446052843981));
#87342=CARTESIAN_POINT('Ctrl Pts',(1.85277773299556,-31.902927962765,55.7751533596825));
#87343=CARTESIAN_POINT('Ctrl Pts',(1.85663795119261,-31.929840268841,55.7090862013134));
#87344=CARTESIAN_POINT('Ctrl Pts',(1.86049816938967,-31.953289919347,55.6416600649415));
#87345=CARTESIAN_POINT('Ctrl Pts',(1.86435838758672,-31.9731588391813,55.5732728476571));
#87346=CARTESIAN_POINT('Ctrl Pts',(1.8682213057675,-31.9930416560953,55.5048377977465));
#87347=CARTESIAN_POINT('Ctrl Pts',(1.87208422394829,-32.0093386495623,55.4354408020274));
#87348=CARTESIAN_POINT('Ctrl Pts',(1.87594714212907,-32.021982778969,55.3654903610944));
#87349=CARTESIAN_POINT('Ctrl Pts',(1.8798163155915,-32.034647383205,55.2954266483577));
#87350=CARTESIAN_POINT('Ctrl Pts',(1.88368548905393,-32.0436472670316,55.2248081835591));
#87351=CARTESIAN_POINT('Ctrl Pts',(1.88755466251637,-32.0489672479301,55.1540479776236));
#87352=CARTESIAN_POINT('Ctrl Pts',(1.88813630976275,-32.0497669929584,55.1434106982834));
#87353=CARTESIAN_POINT('Ctrl Pts',(1.88871795700913,-32.0504836729769,55.132770212495));
#87354=CARTESIAN_POINT('Ctrl Pts',(1.88929960425551,-32.0511173379966,55.1221279176511));
#87355=CARTESIAN_POINT('Ctrl Pts',(1.89316867807618,-32.0553324301403,55.05133617123));
#87356=CARTESIAN_POINT('Ctrl Pts',(1.89703775189685,-32.0558865433756,54.9801872886027));
#87357=CARTESIAN_POINT('Ctrl Pts',(1.90090682571751,-32.0527379982001,54.9090919517021));
#87358=CARTESIAN_POINT('Ctrl Pts',(1.90477013459152,-32.0495941443787,54.8381025473437));
#87359=CARTESIAN_POINT('Ctrl Pts',(1.90863344346552,-32.0427586045275,54.7671670117002));
#87360=CARTESIAN_POINT('Ctrl Pts',(1.91249675233952,-32.0322416284498,54.696698951377));
#87361=CARTESIAN_POINT('Ctrl Pts',(1.91635552931687,-32.0217369894257,54.6263135543812));
#87362=CARTESIAN_POINT('Ctrl Pts',(1.92021430629422,-32.0075595636329,54.5563950215758));
#87363=CARTESIAN_POINT('Ctrl Pts',(1.92407308327157,-31.9897714985709,54.4873530006183));
#87364=CARTESIAN_POINT('Ctrl Pts',(1.92792942934779,-31.9719946393981,54.4183544738372));
#87365=CARTESIAN_POINT('Ctrl Pts',(1.93178577542401,-31.9506117746052,54.3502318327127));
#87366=CARTESIAN_POINT('Ctrl Pts',(1.93564212150022,-31.9257360644493,54.2833842224878));
#87367=CARTESIAN_POINT('Ctrl Pts',(1.93949732823641,-31.9008677037095,54.2165563620875));
#87368=CARTESIAN_POINT('Ctrl Pts',(1.9433525349726,-31.8725087156346,54.1510032397652));
#87369=CARTESIAN_POINT('Ctrl Pts',(1.94720774170879,-31.8408214758495,54.087106875614));
#87370=CARTESIAN_POINT('Ctrl Pts',(1.95106309905301,-31.8091329981664,54.0232080152788));
#87371=CARTESIAN_POINT('Ctrl Pts',(1.95491845639722,-31.7741162284318,53.9609664758441));
#87372=CARTESIAN_POINT('Ctrl Pts',(1.95877381374144,-31.7359800819237,53.9007408323493));
#87373=CARTESIAN_POINT('Ctrl Pts',(1.9626332067028,-31.6978040161882,53.8404521473209));
#87374=CARTESIAN_POINT('Ctrl Pts',(1.96649259966416,-31.6565023159761,53.7821839818299));
#87375=CARTESIAN_POINT('Ctrl Pts',(1.97035199262551,-31.6123274545571,53.7262662202087));
#87376=CARTESIAN_POINT('Ctrl Pts',(1.97421357072239,-31.5681275819356,53.6703167987156));
#87377=CARTESIAN_POINT('Ctrl Pts',(1.97807514881927,-31.5210516304962,53.6167207953959));
#87378=CARTESIAN_POINT('Ctrl Pts',(1.98193672691615,-31.4713908162051,53.565773160031));
#87379=CARTESIAN_POINT('Ctrl Pts',(1.98580506152013,-31.421643111623,53.5147363828564));
#87380=CARTESIAN_POINT('Ctrl Pts',(1.9896733961241,-31.3693018714003,53.4663575549583));
#87381=CARTESIAN_POINT('Ctrl Pts',(1.99354173072807,-31.3146928945613,53.4208926079933));
#87382=CARTESIAN_POINT('Ctrl Pts',(1.99583944551674,-31.2822562347263,53.3938873223337));
#87383=CARTESIAN_POINT('Ctrl Pts',(1.99813716030541,-31.2490200918453,53.3679092936663));
#87384=CARTESIAN_POINT('Ctrl Pts',(2.00043487509407,-31.215057371021,53.3430047834627));
#87385=CARTESIAN_POINT('Ctrl Pts',(2.00430394846561,-31.1578682632107,53.3010686050758));
#87386=CARTESIAN_POINT('Ctrl Pts',(2.00817302183714,-31.0983935265725,53.262014475793));
#87387=CARTESIAN_POINT('Ctrl Pts',(2.01204209520867,-31.0369555873072,53.2261001515158));
#87388=CARTESIAN_POINT('Ctrl Pts',(2.01590540362962,-30.9756091910679,53.1902393398719));
#87389=CARTESIAN_POINT('Ctrl Pts',(2.01976871205056,-30.9123058145872,53.157509290031));
#87390=CARTESIAN_POINT('Ctrl Pts',(2.02363202047151,-30.8473985058096,53.1281257160665));
#87391=CARTESIAN_POINT('Ctrl Pts',(2.02749079699221,-30.7825673373284,53.0987766108555));
#87392=CARTESIAN_POINT('Ctrl Pts',(2.03134957351291,-30.7161364142718,53.0727663832749));
#87393=CARTESIAN_POINT('Ctrl Pts',(2.03520835003361,-30.6484836059538,53.0502649986962));
#87394=CARTESIAN_POINT('Ctrl Pts',(2.03906469565122,-30.5808734166941,53.0277777892544));
#87395=CARTESIAN_POINT('Ctrl Pts',(2.04292104126883,-30.5120433292085,53.0087951902573));
#87396=CARTESIAN_POINT('Ctrl Pts',(2.04677738688643,-30.44239005677,52.9934386129074));
#87397=CARTESIAN_POINT('Ctrl Pts',(2.05063259316274,-30.3727573631016,52.9780865725944));
#87398=CARTESIAN_POINT('Ctrl Pts',(2.05448779943904,-30.3023024414472,52.9663585316487));
#87399=CARTESIAN_POINT('Ctrl Pts',(2.05834300571534,-30.2314343101485,52.958325265233));
#87400=CARTESIAN_POINT('Ctrl Pts',(2.06219836259909,-30.160563410316,52.9502916849897));
#87401=CARTESIAN_POINT('Ctrl Pts',(2.06605371948284,-30.0892797517333,52.945953218372));
#87402=CARTESIAN_POINT('Ctrl Pts',(2.06990907636659,-30.0179978969706,52.9453288247983));
#87403=CARTESIAN_POINT('Ctrl Pts',(2.07376846886978,-29.9466414274711,52.9447037776366));
#87404=CARTESIAN_POINT('Ctrl Pts',(2.07762786137298,-29.8752872523237,52.9478005685648));
#87405=CARTESIAN_POINT('Ctrl Pts',(2.08148725387617,-29.8043494540794,52.9545860012259));
#87406=CARTESIAN_POINT('Ctrl Pts',(2.0853488315155,-29.7333714918078,52.9613752757078));
#87407=CARTESIAN_POINT('Ctrl Pts',(2.08921040915483,-29.6628108564796,52.9718572779855));
#87408=CARTESIAN_POINT('Ctrl Pts',(2.09307198679416,-29.5930732932551,52.9859473150293));
#87409=CARTESIAN_POINT('Ctrl Pts',(2.09694032094654,-29.5232137118297,53.0000620050849));
#87410=CARTESIAN_POINT('Ctrl Pts',(2.10080865509892,-29.454180548386,53.0177972128689));
#87411=CARTESIAN_POINT('Ctrl Pts',(2.1046769892513,-29.3863655238667,53.0390180285886));
#87412=CARTESIAN_POINT('Ctrl Pts',(2.10697470814507,-29.3460846543808,53.0516228003843));
#87413=CARTESIAN_POINT('Ctrl Pts',(2.10927242703885,-29.3062332188164,53.065456404428));
#87414=CARTESIAN_POINT('Ctrl Pts',(2.11157014593263,-29.2668896249878,53.0804826803205));
#87415=CARTESIAN_POINT('Ctrl Pts',(2.11543921914794,-29.2006398998848,53.1057850624959));
#87416=CARTESIAN_POINT('Ctrl Pts',(2.11930829236326,-29.1355718665169,53.1345708206531));
#87417=CARTESIAN_POINT('Ctrl Pts',(2.12317736557858,-29.0720769492189,53.1667088680929));
#87418=CARTESIAN_POINT('Ctrl Pts',(2.12704067383899,-29.0086766399354,53.1987990295446));
#87419=CARTESIAN_POINT('Ctrl Pts',(2.1309039820994,-28.9468452239291,53.2342313478661));
#87420=CARTESIAN_POINT('Ctrl Pts',(2.13476729035982,-28.8869554125041,53.2728262077179));
#87421=CARTESIAN_POINT('Ctrl Pts',(2.13862606671434,-28.8271358556305,53.3113757933485));
#87422=CARTESIAN_POINT('Ctrl Pts',(2.14248484306886,-28.7692537855618,53.3530802895987));
#87423=CARTESIAN_POINT('Ctrl Pts',(2.14634361942338,-28.7136569403488,53.3977144151597));
#87424=CARTESIAN_POINT('Ctrl Pts',(2.1501999648714,-28.6580951193817,53.4423204226397));
#87425=CARTESIAN_POINT('Ctrl Pts',(2.15405631031943,-28.6048160450079,53.4898520944433));
#87426=CARTESIAN_POINT('Ctrl Pts',(2.15791265576745,-28.5541368830964,53.5400419835906));
#87427=CARTESIAN_POINT('Ctrl Pts',(2.16176786187102,-28.5034726941752,53.5902170443018));
#87428=CARTESIAN_POINT('Ctrl Pts',(2.16562306797458,-28.4554072377314,53.6430484215505));
#87429=CARTESIAN_POINT('Ctrl Pts',(2.16947827407815,-28.4102218119229,53.6982308671603));
#87430=CARTESIAN_POINT('Ctrl Pts',(2.17333363078626,-28.365034620935,53.7534154684853));
#87431=CARTESIAN_POINT('Ctrl Pts',(2.17718898749436,-28.3227279900157,53.8109509432653));
#87432=CARTESIAN_POINT('Ctrl Pts',(2.18104434420247,-28.2835426916522,53.8704992823733));
#87433=CARTESIAN_POINT('Ctrl Pts',(2.18490373652677,-28.2443163758585,53.9301099540381));
#87434=CARTESIAN_POINT('Ctrl Pts',(2.18876312885106,-28.208218182415,53.9917372893924));
#87435=CARTESIAN_POINT('Ctrl Pts',(2.19262252117536,-28.1754448051268,54.0550153951724));
#87436=CARTESIAN_POINT('Ctrl Pts',(2.19648409863368,-28.1426528720102,54.1183293281319));
#87437=CARTESIAN_POINT('Ctrl Pts',(2.200345676092,-28.1131897031921,54.1832954494789));
#87438=CARTESIAN_POINT('Ctrl Pts',(2.20420725355032,-28.0872042059791,54.2495269406062));
#87439=CARTESIAN_POINT('Ctrl Pts',(2.2080755875203,-28.0611732425501,54.3158743154227));
#87440=CARTESIAN_POINT('Ctrl Pts',(2.21194392149028,-28.0386322528878,54.3834910193113));
#87441=CARTESIAN_POINT('Ctrl Pts',(2.21581225546026,-28.0196803487775,54.4519747802499));
#87442=CARTESIAN_POINT('Ctrl Pts',(2.21810997589723,-28.0084232603948,54.4926528960308));
#87443=CARTESIAN_POINT('Ctrl Pts',(2.22040769633421,-27.9984314787575,54.5336367006076));
#87444=CARTESIAN_POINT('Ctrl Pts',(2.22270541677119,-27.9897171495473,54.5748407078804));
#87445=CARTESIAN_POINT('Ctrl Pts',(2.22812785170408,-27.9691520353733,54.6720788421699));
#87446=CARTESIAN_POINT('Ctrl Pts',(2.23355028663696,-27.9556362036303,54.7708559975689));
#87447=CARTESIAN_POINT('Ctrl Pts',(2.23897272156985,-27.9493462554379,54.8703204626261));
#87448=CARTESIAN_POINT('Ctrl Pts',(2.24129024122579,-27.94665796526,54.9128310424102));
#87449=CARTESIAN_POINT('Ctrl Pts',(2.24360776088173,-27.9452890575006,54.9554668839035));
#87450=CARTESIAN_POINT('Ctrl Pts',(2.24592528053768,-27.9452508239571,54.9981598774073));
#87451=CARTESIAN_POINT('Origin',(-1.54592528053767,-30.,55.));
#87452=CARTESIAN_POINT('',(1.09386116309789,-31.2520475724682,56.6292251037768));
#87453=CARTESIAN_POINT('',(1.1521101573493,-31.2520475724682,56.6292251037768));
#87454=CARTESIAN_POINT('',(-1.54592528053767,-31.2520475724682,56.6292251037768));
#87455=CARTESIAN_POINT('',(1.60407469463954,-27.9455255624714,54.9994775006002));
#87456=CARTESIAN_POINT('Ctrl Pts',(1.15211015734929,-31.2520475724682,56.6292251037768));
#87457=CARTESIAN_POINT('Ctrl Pts',(1.15596557278302,-31.3085761712459,56.5857832891923));
#87458=CARTESIAN_POINT('Ctrl Pts',(1.15982098821674,-31.3628659140609,56.5393770070728));
#87459=CARTESIAN_POINT('Ctrl Pts',(1.16367640365046,-31.4145978871033,56.4902719148876));
#87460=CARTESIAN_POINT('Ctrl Pts',(1.1675315895544,-31.4663267803145,56.441169746144));
#87461=CARTESIAN_POINT('Ctrl Pts',(1.17138677545833,-31.5154978548606,56.3893694219266));
#87462=CARTESIAN_POINT('Ctrl Pts',(1.17524196136226,-31.5618280037784,56.3351744639236));
#87463=CARTESIAN_POINT('Ctrl Pts',(1.17910093874514,-31.6082037172392,56.2809262065344));
#87464=CARTESIAN_POINT('Ctrl Pts',(1.18295991612802,-31.6517326074729,56.2242789811046));
#87465=CARTESIAN_POINT('Ctrl Pts',(1.1868188935109,-31.6921715266186,56.1655698550501));
#87466=CARTESIAN_POINT('Ctrl Pts',(1.19067971455899,-31.7326297658641,56.1068326801208));
#87467=CARTESIAN_POINT('Ctrl Pts',(1.19454053560709,-31.7699948382545,56.0460320565788));
#87468=CARTESIAN_POINT('Ctrl Pts',(1.19840135665518,-31.8040681871318,55.9835321747045));
#87469=CARTESIAN_POINT('Ctrl Pts',(1.20226929615544,-31.8382043593054,55.9209170576472));
#87470=CARTESIAN_POINT('Ctrl Pts',(1.20613723565571,-31.869036471134,55.8565968616065));
#87471=CARTESIAN_POINT('Ctrl Pts',(1.21000517515597,-31.8964132111337,55.790957960411));
#87472=CARTESIAN_POINT('Ctrl Pts',(1.21344131802192,-31.9207337543677,55.7326466445138));
#87473=CARTESIAN_POINT('Ctrl Pts',(1.21687746088786,-31.9423279731226,55.6732951182633));
#87474=CARTESIAN_POINT('Ctrl Pts',(1.2203136037538,-31.961123148466,55.6131831366329));
#87475=CARTESIAN_POINT('Ctrl Pts',(1.22418266806599,-31.9822863378325,55.5454976148327));
#87476=CARTESIAN_POINT('Ctrl Pts',(1.22805173237817,-31.9999827568448,55.476582593894));
#87477=CARTESIAN_POINT('Ctrl Pts',(1.23192079669036,-32.0140729123918,55.4068265798466));
#87478=CARTESIAN_POINT('Ctrl Pts',(1.23578409589712,-32.0281420728801,55.3371745058588));
#87479=CARTESIAN_POINT('Ctrl Pts',(1.23964739510388,-32.0386155407856,55.266684398468));
#87480=CARTESIAN_POINT('Ctrl Pts',(1.24351069431064,-32.0454035141265,55.1957601259168));
#87481=CARTESIAN_POINT('Ctrl Pts',(1.2473694614317,-32.052183524409,55.1249190555366));
#87482=CARTESIAN_POINT('Ctrl Pts',(1.25122822855277,-32.0552865820036,55.0536453129186));
#87483=CARTESIAN_POINT('Ctrl Pts',(1.25508699567383,-32.0546742055237,54.9823514404111));
#87484=CARTESIAN_POINT('Ctrl Pts',(1.2589433317824,-32.0540622148393,54.9111024828439));
#87485=CARTESIAN_POINT('Ctrl Pts',(1.26279966789097,-32.0497394381791,54.8398339051697));
#87486=CARTESIAN_POINT('Ctrl Pts',(1.26665600399954,-32.0417194340277,54.7689603600819));
#87487=CARTESIAN_POINT('Ctrl Pts',(1.27051120067154,-32.0337017995573,54.6981077560912));
#87488=CARTESIAN_POINT('Ctrl Pts',(1.27436639734354,-32.0219891609535,54.6276504354089));
#87489=CARTESIAN_POINT('Ctrl Pts',(1.27822159401553,-32.0066469694416,54.5579983003076));
#87490=CARTESIAN_POINT('Ctrl Pts',(1.28207694121374,-31.9913041788936,54.4883434456378));
#87491=CARTESIAN_POINT('Ctrl Pts',(1.28593228841194,-31.9723316607293,54.4194943129083));
#87492=CARTESIAN_POINT('Ctrl Pts',(1.28978763561014,-31.9498456863397,54.3518492752742));
#87493=CARTESIAN_POINT('Ctrl Pts',(1.29364701837012,-31.92733617489,54.2841334305988));
#87494=CARTESIAN_POINT('Ctrl Pts',(1.29750640113009,-31.9013060192717,54.2176246589508));
#87495=CARTESIAN_POINT('Ctrl Pts',(1.30136578389007,-31.8719206824674,54.1527039944324));
#87496=CARTESIAN_POINT('Ctrl Pts',(1.30522735173892,-31.8425187083984,54.0877465734089));
#87497=CARTESIAN_POINT('Ctrl Pts',(1.30908891958777,-31.8097579947878,54.0243794811739));
#87498=CARTESIAN_POINT('Ctrl Pts',(1.31295048743662,-31.773850028845,53.962959191899));
#87499=CARTESIAN_POINT('Ctrl Pts',(1.31681881182973,-31.7378792351154,53.9014314361962));
#87500=CARTESIAN_POINT('Ctrl Pts',(1.32068713622285,-31.6987504615151,53.8418576903979));
#87501=CARTESIAN_POINT('Ctrl Pts',(1.32455546061596,-31.6567181674367,53.7845649025204));
#87502=CARTESIAN_POINT('Ctrl Pts',(1.32685326527476,-31.6317507677724,53.7505326907609));
#87503=CARTESIAN_POINT('Ctrl Pts',(1.32915106993356,-31.6057596613866,53.7173046689099));
#87504=CARTESIAN_POINT('Ctrl Pts',(1.33144887459237,-31.5788044520992,53.6849433226922));
#87505=CARTESIAN_POINT('Ctrl Pts',(1.33531795118106,-31.5334168823606,53.6304528217048));
#87506=CARTESIAN_POINT('Ctrl Pts',(1.33918702776976,-31.4851160905946,53.5782080927003));
#87507=CARTESIAN_POINT('Ctrl Pts',(1.34305610435845,-31.4341528251068,53.5285370420095));
#87508=CARTESIAN_POINT('Ctrl Pts',(1.34691941602998,-31.3832654947929,53.4789400010949));
#87509=CARTESIAN_POINT('Ctrl Pts',(1.35078272770152,-31.3297239103519,53.4319093628715));
#87510=CARTESIAN_POINT('Ctrl Pts',(1.35464603937305,-31.2738186770057,53.387739617614));
#87511=CARTESIAN_POINT('Ctrl Pts',(1.35850481917804,-31.2179790234208,53.3436216857768));
#87512=CARTESIAN_POINT('Ctrl Pts',(1.36236359898302,-31.1597816077401,53.3023582804948));
#87513=CARTESIAN_POINT('Ctrl Pts',(1.36622237878801,-31.0995521569077,53.2642054796896));
#87514=CARTESIAN_POINT('Ctrl Pts',(1.37007872770888,-31.0393606483322,53.2260767136938));
#87515=CARTESIAN_POINT('Ctrl Pts',(1.37393507662976,-30.9771400537194,53.191054923777));
#87516=CARTESIAN_POINT('Ctrl Pts',(1.37779142555063,-30.9132460973394,53.1593536113109));
#87517=CARTESIAN_POINT('Ctrl Pts',(1.38164663514423,-30.8493710179151,53.1276616647425));
#87518=CARTESIAN_POINT('Ctrl Pts',(1.38550184473782,-30.7838239931369,53.099288463844));
#87519=CARTESIAN_POINT('Ctrl Pts',(1.38935705433142,-30.7169849007977,53.0744013360702));
#87520=CARTESIAN_POINT('Ctrl Pts',(1.39321241454153,-30.6501431971683,53.0495132359985));
#87521=CARTESIAN_POINT('Ctrl Pts',(1.39706777475164,-30.5820097817782,53.0281116468946));
#87522=CARTESIAN_POINT('Ctrl Pts',(1.40092313496175,-30.512982409171,53.0103149469373));
#87523=CARTESIAN_POINT('Ctrl Pts',(1.40478253078214,-30.4438827819471,52.9924996182291));
#87524=CARTESIAN_POINT('Ctrl Pts',(1.40864192660254,-30.3738878009,52.9782968328076));
#87525=CARTESIAN_POINT('Ctrl Pts',(1.41250132242293,-30.3034073328994,52.9677742367437));
#87526=CARTESIAN_POINT('Ctrl Pts',(1.41636290337928,-30.2328869598431,52.9572456829329));
#87527=CARTESIAN_POINT('Ctrl Pts',(1.42022448433563,-30.1618810364133,52.9504015130578));
#87528=CARTESIAN_POINT('Ctrl Pts',(1.42408606529199,-30.0908037574162,52.9472573858033));
#87529=CARTESIAN_POINT('Ctrl Pts',(1.42795440272499,-30.0196021169253,52.9441077573764));
#87530=CARTESIAN_POINT('Ctrl Pts',(1.431822740158,-29.9483293575278,52.944671092936));
#87531=CARTESIAN_POINT('Ctrl Pts',(1.435691077591,-29.8773981743257,52.9489109344445));
#87532=CARTESIAN_POINT('Ctrl Pts',(1.43798876687098,-29.8352669429939,52.9514292872386));
#87533=CARTESIAN_POINT('Ctrl Pts',(1.44028645615095,-29.7932561152423,52.9552437332563));
#87534=CARTESIAN_POINT('Ctrl Pts',(1.44258414543093,-29.7514505018919,52.9603380894153));
#87535=CARTESIAN_POINT('Ctrl Pts',(1.44645321930508,-29.6810541224437,52.968916464434));
#87536=CARTESIAN_POINT('Ctrl Pts',(1.45032229317924,-29.6109644848074,52.9811603850238));
#87537=CARTESIAN_POINT('Ctrl Pts',(1.4541913670534,-29.5415930737697,52.9970370316743));
#87538=CARTESIAN_POINT('Ctrl Pts',(1.45805467599476,-29.4723250263626,53.012890022069));
#87539=CARTESIAN_POINT('Ctrl Pts',(1.46191798493612,-29.4037735510006,53.0323648868264));
#87540=CARTESIAN_POINT('Ctrl Pts',(1.46578129387748,-29.3363436752025,53.0553771972292));
#87541=CARTESIAN_POINT('Ctrl Pts',(1.4696400709426,-29.2689928983985,53.0783625129121));
#87542=CARTESIAN_POINT('Ctrl Pts',(1.47349884800773,-29.2027615652538,53.1048768755501));
#87543=CARTESIAN_POINT('Ctrl Pts',(1.47735762507285,-29.1380414802018,53.1347855156451));
#87544=CARTESIAN_POINT('Ctrl Pts',(1.48121397124943,-29.0733621664385,53.1646753143898));
#87545=CARTESIAN_POINT('Ctrl Pts',(1.48507031742601,-29.0101926518868,53.1979549449937));
#87546=CARTESIAN_POINT('Ctrl Pts',(1.48892666360258,-28.9489052400723,53.2344413438935));
#87547=CARTESIAN_POINT('Ctrl Pts',(1.49278187045159,-28.8876359351484,53.2709169631697));
#87548=CARTESIAN_POINT('Ctrl Pts',(1.4966370773006,-28.8282480462308,53.3105972214957));
#87549=CARTESIAN_POINT('Ctrl Pts',(1.50049228414961,-28.7710881841521,53.3532537197949));
#87550=CARTESIAN_POINT('Ctrl Pts',(1.50434764161902,-28.7139260888751,53.3959118846554));
#87551=CARTESIAN_POINT('Ctrl Pts',(1.50820299908843,-28.6589925812664,53.4415462280417));
#87552=CARTESIAN_POINT('Ctrl Pts',(1.51205835655784,-28.6066028434589,53.4898867835016));
#87553=CARTESIAN_POINT('Ctrl Pts',(1.51591774966253,-28.5541582661519,53.5382779399375));
#87554=CARTESIAN_POINT('Ctrl Pts',(1.51977714276722,-28.5042631317822,53.5893806331602));
#87555=CARTESIAN_POINT('Ctrl Pts',(1.52363653587191,-28.457196569526,53.6428872053445));
#87556=CARTESIAN_POINT('Ctrl Pts',(1.52749811412259,-28.4101033586993,53.6964240723622));
#87557=CARTESIAN_POINT('Ctrl Pts',(1.53135969237328,-28.3658422096494,53.7523671466232));
#87558=CARTESIAN_POINT('Ctrl Pts',(1.53522127062396,-28.3246509219981,53.8103769381279));
#87559=CARTESIAN_POINT('Ctrl Pts',(1.53908960539675,-28.2833875628186,53.8684882281426));
#87560=CARTESIAN_POINT('Ctrl Pts',(1.54295794016954,-28.2452050492593,53.9286730447033));
#87561=CARTESIAN_POINT('Ctrl Pts',(1.54682627494233,-28.2102965820227,53.9905648915457));
#87562=CARTESIAN_POINT('Ctrl Pts',(1.54912398871805,-28.1895616480602,54.0273274153309));
#87563=CARTESIAN_POINT('Ctrl Pts',(1.55142170249376,-28.1699809454479,54.0646917503864));
#87564=CARTESIAN_POINT('Ctrl Pts',(1.55371941626947,-28.1515868774171,54.1025778636766));
#87565=CARTESIAN_POINT('Ctrl Pts',(1.55791568927332,-28.1179941245144,54.1717685853846));
#87566=CARTESIAN_POINT('Ctrl Pts',(1.56211196227716,-28.0882444852697,54.242941908556));
#87567=CARTESIAN_POINT('Ctrl Pts',(1.56630823528101,-28.062557410543,54.3156654509246));
#87568=CARTESIAN_POINT('Ctrl Pts',(1.57045671771971,-28.0371628810861,54.3875607585274));
#87569=CARTESIAN_POINT('Ctrl Pts',(1.57460520015842,-28.0157390341105,54.4609708158));
#87570=CARTESIAN_POINT('Ctrl Pts',(1.57875368259713,-27.9984521149186,54.5354533110372));
#87571=CARTESIAN_POINT('Ctrl Pts',(1.58297385088354,-27.9808664774665,54.6112228650698));
#87572=CARTESIAN_POINT('Ctrl Pts',(1.58719401916996,-27.9675623121118,54.6881019450977));
#87573=CARTESIAN_POINT('Ctrl Pts',(1.59141418745637,-27.9586631451064,54.7656041652397));
#87574=CARTESIAN_POINT('Ctrl Pts',(1.59563435574278,-27.949763978101,54.8431063853816));
#87575=CARTESIAN_POINT('Ctrl Pts',(1.59985452402919,-27.9452699678385,54.9212313568782));
#87576=CARTESIAN_POINT('Ctrl Pts',(1.6040746923156,-27.9452500664616,54.9994773875089));
#87577=CARTESIAN_POINT('Ctrl Pts',(1.60407471946232,-27.94846822613,54.9994787085655));
#87578=CARTESIAN_POINT('Ctrl Pts',(1.62433470867756,-27.9493198488661,55.3745305565027));
#87579=CARTESIAN_POINT('Ctrl Pts',(1.68163978817232,-28.2273233735254,56.4365344918066));
#87580=CARTESIAN_POINT('Ctrl Pts',(1.76427577418884,-29.7210216460611,57.3046347470521));
#87581=CARTESIAN_POINT('Ctrl Pts',(1.82665177099012,-30.8775867504766,56.9099569767507));
#87582=CARTESIAN_POINT('Ctrl Pts',(1.85198267751188,-31.2510897925303,56.6279533612584));
#87583=CARTESIAN_POINT('',(1.54592528048776,-27.9452502738004,55.0010607462675));
#87584=CARTESIAN_POINT('Ctrl Pts',(1.54592528053768,-27.9452502738009,55.0010607471837));
#87585=CARTESIAN_POINT('Ctrl Pts',(1.54924811760506,-27.9452817536834,55.0620397260039));
#87586=CARTESIAN_POINT('Ctrl Pts',(1.55257095467244,-27.948027507084,55.1229466290489));
#87587=CARTESIAN_POINT('Ctrl Pts',(1.55589379173983,-27.9534698488702,55.1836080145764));
#87588=CARTESIAN_POINT('Ctrl Pts',(1.5597628683149,-27.9598068544746,55.2542414946407));
#87589=CARTESIAN_POINT('Ctrl Pts',(1.56363194488996,-27.9698173072335,55.3246848690047));
#87590=CARTESIAN_POINT('Ctrl Pts',(1.56750102146503,-27.9834814798758,55.3945258172747));
#87591=CARTESIAN_POINT('Ctrl Pts',(1.57136433312278,-27.9971252929249,55.4642627026542));
#87592=CARTESIAN_POINT('Ctrl Pts',(1.57522764478053,-28.0144119270837,55.5333984708159));
#87593=CARTESIAN_POINT('Ctrl Pts',(1.57909095643828,-28.0352698667458,55.6015256154004));
#87594=CARTESIAN_POINT('Ctrl Pts',(1.5829497362293,-28.0561033389532,55.6695728432794));
#87595=CARTESIAN_POINT('Ctrl Pts',(1.58680851602031,-28.0804996537178,55.7366133355057));
#87596=CARTESIAN_POINT('Ctrl Pts',(1.59066729581133,-28.1083365598858,55.8022512024517));
#87597=CARTESIAN_POINT('Ctrl Pts',(1.59452364471814,-28.1361559298637,55.867847720043));
#87598=CARTESIAN_POINT('Ctrl Pts',(1.59837999362495,-28.1674114018557,55.9320429192325));
#87599=CARTESIAN_POINT('Ctrl Pts',(1.60223634253175,-28.2019318353487,55.9944588668053));
#87600=CARTESIAN_POINT('Ctrl Pts',(1.6060915521112,-28.2364420700565,56.0568563740869));
#87601=CARTESIAN_POINT('Ctrl Pts',(1.60994676169065,-28.2742151162716,56.117475248475));
#87602=CARTESIAN_POINT('Ctrl Pts',(1.6138019712701,-28.315033704418,56.1759617958305));
#87603=CARTESIAN_POINT('Ctrl Pts',(1.61765733146601,-28.3558538872771,56.2344506281556));
#87604=CARTESIAN_POINT('Ctrl Pts',(1.62151269166191,-28.3997195684674,56.2908065709542));
#87605=CARTESIAN_POINT('Ctrl Pts',(1.62536805185782,-28.4463709333038,56.344706022005));
#87606=CARTESIAN_POINT('Ctrl Pts',(1.62922744766402,-28.4930711306015,56.3986618924741));
#87607=CARTESIAN_POINT('Ctrl Pts',(1.63308684347022,-28.5425625138155,56.4501557701598));
#87608=CARTESIAN_POINT('Ctrl Pts',(1.63694623927641,-28.5945464502454,56.4988988898462));
#87609=CARTESIAN_POINT('Ctrl Pts',(1.64080782021855,-28.6465598192532,56.5476696072054));
#87610=CARTESIAN_POINT('Ctrl Pts',(1.64466940116069,-28.7010681794651,56.593686152664));
#87611=CARTESIAN_POINT('Ctrl Pts',(1.64853098210283,-28.757739768715,56.6367000581254));
#87612=CARTESIAN_POINT('Ctrl Pts',(1.65239931952175,-28.8145105143163,56.6797892235536));
#87613=CARTESIAN_POINT('Ctrl Pts',(1.65626765694067,-28.8734516438254,56.7198649867566));
#87614=CARTESIAN_POINT('Ctrl Pts',(1.66013599435959,-28.9342029851873,56.7567225978271));
#87615=CARTESIAN_POINT('Ctrl Pts',(1.66243368376586,-28.9702876640422,56.7786150372205));
#87616=CARTESIAN_POINT('Ctrl Pts',(1.66473137317212,-29.0070105153468,56.799372976299));
#87617=CARTESIAN_POINT('Ctrl Pts',(1.66702906257839,-29.0442925787914,56.8189614859988));
#87618=CARTESIAN_POINT('Ctrl Pts',(1.67089813645202,-29.1070717591432,56.8519465321481));
#87619=CARTESIAN_POINT('Ctrl Pts',(1.67476721032565,-29.1716835679484,56.8817422542605));
#87620=CARTESIAN_POINT('Ctrl Pts',(1.67863628419928,-29.2377708981664,56.9081415982096));
#87621=CARTESIAN_POINT('Ctrl Pts',(1.68249959314005,-29.3037597580441,56.934501607049));
#87622=CARTESIAN_POINT('Ctrl Pts',(1.68636290208083,-29.3712193278617,56.9574751041645));
#87623=CARTESIAN_POINT('Ctrl Pts',(1.6902262110216,-29.4397684568758,56.9769011559986));
#87624=CARTESIAN_POINT('Ctrl Pts',(1.69408498808608,-29.5082371739482,56.9963044199933));
#87625=CARTESIAN_POINT('Ctrl Pts',(1.69794376515055,-29.5777924463391,57.012168372749));
#87626=CARTESIAN_POINT('Ctrl Pts',(1.70180254221503,-29.6480353658451,57.0243810063336));
#87627=CARTESIAN_POINT('Ctrl Pts',(1.70565888839091,-29.7182340348777,57.0365859464051));
#87628=CARTESIAN_POINT('Ctrl Pts',(1.70951523456679,-29.789119014104,57.0451440478454));
#87629=CARTESIAN_POINT('Ctrl Pts',(1.71337158074267,-29.8602799654172,57.0499941157077));
#87630=CARTESIAN_POINT('Ctrl Pts',(1.71722678759094,-29.9314198927785,57.054842750655));
#87631=CARTESIAN_POINT('Ctrl Pts',(1.7210819944392,-30.002835145962,57.0559854938997));
#87632=CARTESIAN_POINT('Ctrl Pts',(1.72493720128747,-30.0741107323921,57.0534130519319));
#87633=CARTESIAN_POINT('Ctrl Pts',(1.72879255875609,-30.1453891035115,57.0508405094605));
#87634=CARTESIAN_POINT('Ctrl Pts',(1.7326479162247,-30.2165273116536,57.0445525133233));
#87635=CARTESIAN_POINT('Ctrl Pts',(1.73650327369332,-30.2871125708193,57.0345918347859));
#87636=CARTESIAN_POINT('Ctrl Pts',(1.74036266679717,-30.3577717158337,57.0246207298055));
#87637=CARTESIAN_POINT('Ctrl Pts',(1.74422205990101,-30.4278762744413,57.0109693361209));
#87638=CARTESIAN_POINT('Ctrl Pts',(1.74808145300486,-30.4970216752217,56.993731932046));
#87639=CARTESIAN_POINT('Ctrl Pts',(1.75194303125466,-30.566206225368,56.9764847683423));
#87640=CARTESIAN_POINT('Ctrl Pts',(1.75580460950447,-30.6344300717935,56.9556476943948));
#87641=CARTESIAN_POINT('Ctrl Pts',(1.75966618775427,-30.7013045302177,56.9313646777334));
#87642=CARTESIAN_POINT('Ctrl Pts',(1.76353452252614,-30.7682959974722,56.9070391735895));
#87643=CARTESIAN_POINT('Ctrl Pts',(1.76740285729801,-30.8339329154279,56.8792558784943));
#87644=CARTESIAN_POINT('Ctrl Pts',(1.77127119206988,-30.8978479208636,56.8482063395359));
#87645=CARTESIAN_POINT('Ctrl Pts',(1.77356890585224,-30.9358121606592,56.8297635320212));
#87646=CARTESIAN_POINT('Ctrl Pts',(1.77586661963459,-30.9731693666111,56.8101692312376));
#87647=CARTESIAN_POINT('Ctrl Pts',(1.77816433341695,-31.0098473657377,56.7894708325124));
#87648=CARTESIAN_POINT('Ctrl Pts',(1.78203306890693,-31.0716033068006,56.7546202648094));
#87649=CARTESIAN_POINT('Ctrl Pts',(1.78590180439691,-31.1316740064266,56.7165008235736));
#87650=CARTESIAN_POINT('Ctrl Pts',(1.78977053988689,-31.1896919225454,56.6753001796485));
#87651=CARTESIAN_POINT('Ctrl Pts',(1.79117493316314,-31.210753060354,56.6603438954942));
#87652=CARTESIAN_POINT('Ctrl Pts',(1.7925793264394,-31.2315438885102,56.6449820348889));
#87653=CARTESIAN_POINT('Ctrl Pts',(1.79398371971565,-31.2520475724682,56.6292251037768));
#87654=CARTESIAN_POINT('Ctrl Pts',(1.09386116309789,-31.2520475724682,56.6292251037768));
#87655=CARTESIAN_POINT('Ctrl Pts',(1.09772972046203,-31.3085492190033,56.5858040017936));
#87656=CARTESIAN_POINT('Ctrl Pts',(1.10159827782616,-31.3627137126113,56.53949850154));
#87657=CARTESIAN_POINT('Ctrl Pts',(1.10546683519029,-31.4142494145056,56.4906026150757));
#87658=CARTESIAN_POINT('Ctrl Pts',(1.10742879292206,-31.4403859970288,56.4658048278205));
#87659=CARTESIAN_POINT('Ctrl Pts',(1.10939075065382,-31.4658470525731,56.4403413415681));
#87660=CARTESIAN_POINT('Ctrl Pts',(1.11135270838559,-31.4905985265509,56.4142537237512));
#87661=CARTESIAN_POINT('Ctrl Pts',(1.11522171018827,-31.5394087001283,56.3628086601157));
#87662=CARTESIAN_POINT('Ctrl Pts',(1.11909071199094,-31.5856481018848,56.3087329449302));
#87663=CARTESIAN_POINT('Ctrl Pts',(1.12295971379362,-31.6290203852074,56.2523139171465));
#87664=CARTESIAN_POINT('Ctrl Pts',(1.12682294948606,-31.672328029282,56.1959789726354));
#87665=CARTESIAN_POINT('Ctrl Pts',(1.1306861851785,-31.7127767429601,56.1373080296882));
#87666=CARTESIAN_POINT('Ctrl Pts',(1.13454942087094,-31.750108024177,56.0766241062745));
#87667=CARTESIAN_POINT('Ctrl Pts',(1.13840812329285,-31.7873954994213,56.016011391729));
#87668=CARTESIAN_POINT('Ctrl Pts',(1.14226682571477,-31.8215725551428,55.9533908004313));
#87669=CARTESIAN_POINT('Ctrl Pts',(1.14612552813668,-31.852422942802,55.8891157424547));
#87670=CARTESIAN_POINT('Ctrl Pts',(1.14998179884972,-31.8832538889098,55.8248811898634));
#87671=CARTESIAN_POINT('Ctrl Pts',(1.15383806956276,-31.9107621165093,55.7589946760764));
#87672=CARTESIAN_POINT('Ctrl Pts',(1.15769434027581,-31.934777167482,55.6918344272225));
#87673=CARTESIAN_POINT('Ctrl Pts',(1.16154947095325,-31.9587851188461,55.6246940330625));
#87674=CARTESIAN_POINT('Ctrl Pts',(1.16540460163069,-31.9793017802805,55.5562811085952));
#87675=CARTESIAN_POINT('Ctrl Pts',(1.16925973230813,-31.9962053739874,55.486992471568));
#87676=CARTESIAN_POINT('Ctrl Pts',(1.17311501300943,-32.013109625504,55.4177011381475));
#87677=CARTESIAN_POINT('Ctrl Pts',(1.17697029371072,-32.0264004171426,55.3475344969958));
#87678=CARTESIAN_POINT('Ctrl Pts',(1.18082557441202,-32.0360066742742,55.276901399077));
#87679=CARTESIAN_POINT('Ctrl Pts',(1.18468489036429,-32.0456229860975,55.2061943708015));
#87680=CARTESIAN_POINT('Ctrl Pts',(1.18854420631656,-32.0515469993018,55.1350203935007));
#87681=CARTESIAN_POINT('Ctrl Pts',(1.19240352226884,-32.0537594393593,55.0637944178004));
#87682=CARTESIAN_POINT('Ctrl Pts',(1.19626502303373,-32.05597313191,54.9925281200812));
#87683=CARTESIAN_POINT('Ctrl Pts',(1.20012652379863,-32.0544710787649,54.921210251292));
#87684=CARTESIAN_POINT('Ctrl Pts',(1.20398802456352,-32.0492861423162,54.8502539836562));
#87685=CARTESIAN_POINT('Ctrl Pts',(1.20785628216241,-32.0440921332926,54.7791735571116));
#87686=CARTESIAN_POINT('Ctrl Pts',(1.21172453976131,-32.0352024353683,54.7084564771461));
#87687=CARTESIAN_POINT('Ctrl Pts',(1.2155927973602,-32.0227014951234,54.638508334639));
#87688=CARTESIAN_POINT('Ctrl Pts',(1.21789119131485,-32.0152738394537,54.596947403453));
#87689=CARTESIAN_POINT('Ctrl Pts',(1.2201895852695,-32.0065722627379,54.5556577129014));
#87690=CARTESIAN_POINT('Ctrl Pts',(1.22248797922415,-31.9966227768528,54.514721678361));
#87691=CARTESIAN_POINT('Ctrl Pts',(1.22635707361176,-31.9798739075304,54.445810349574));
#87692=CARTESIAN_POINT('Ctrl Pts',(1.23022616799936,-31.9595204436173,54.3776321757481));
#87693=CARTESIAN_POINT('Ctrl Pts',(1.23409526238696,-31.9356430854709,54.3105919871595));
#87694=CARTESIAN_POINT('Ctrl Pts',(1.23795859201317,-31.9118013034203,54.2436516851728));
#87695=CARTESIAN_POINT('Ctrl Pts',(1.24182192163938,-31.8844462107573,54.1778464567112));
#87696=CARTESIAN_POINT('Ctrl Pts',(1.24568525126559,-31.8537090082601,54.1135686855739));
#87697=CARTESIAN_POINT('Ctrl Pts',(1.24954404916813,-31.8230078608041,54.0493663128948));
#87698=CARTESIAN_POINT('Ctrl Pts',(1.25340284707066,-31.7889326923645,53.9866882746953));
#87699=CARTESIAN_POINT('Ctrl Pts',(1.25726164497319,-31.7516631534684,53.9259079372413));
#87700=CARTESIAN_POINT('Ctrl Pts',(1.26111801206976,-31.7144170920955,53.8651658876715));
#87701=CARTESIAN_POINT('Ctrl Pts',(1.26497437916632,-31.6739809058884,53.8063195802681));
#87702=CARTESIAN_POINT('Ctrl Pts',(1.26883074626288,-31.6305799285602,53.7497173683216));
#87703=CARTESIAN_POINT('Ctrl Pts',(1.27268597408294,-31.5871917730699,53.6931318782195));
#87704=CARTESIAN_POINT('Ctrl Pts',(1.276541201903,-31.5408408607529,53.6387895526885));
#87705=CARTESIAN_POINT('Ctrl Pts',(1.28039642972305,-31.4917945464425,53.5870079286477));
#87706=CARTESIAN_POINT('Ctrl Pts',(1.28425180818311,-31.4427463156858,53.5352242812806));
#87707=CARTESIAN_POINT('Ctrl Pts',(1.28810718664316,-31.3910028094911,53.486001885227));
#87708=CARTESIAN_POINT('Ctrl Pts',(1.29196256510322,-31.3368689910113,53.4396222049221));
#87709=CARTESIAN_POINT('Ctrl Pts',(1.29582197908265,-31.2826785093335,53.393193977866));
#87710=CARTESIAN_POINT('Ctrl Pts',(1.29968139306208,-31.2260930904763,53.3496147231137));
#87711=CARTESIAN_POINT('Ctrl Pts',(1.30354080704151,-31.1674509159418,53.3091256932088));
#87712=CARTESIAN_POINT('Ctrl Pts',(1.30740240613298,-31.1087755395475,53.26861373934));
#87713=CARTESIAN_POINT('Ctrl Pts',(1.31126400522446,-31.0480415031214,53.2311957481936));
#87714=CARTESIAN_POINT('Ctrl Pts',(1.31512560431593,-30.9856137707499,53.1970682050038));
#87715=CARTESIAN_POINT('Ctrl Pts',(1.31899395964842,-30.9230768150242,53.1628809523773));
#87716=CARTESIAN_POINT('Ctrl Pts',(1.3228623149809,-30.8588406850115,53.1319958522056));
#87717=CARTESIAN_POINT('Ctrl Pts',(1.32673067031339,-30.7932919523926,53.1045619396116));
#87718=CARTESIAN_POINT('Ctrl Pts',(1.32902819689649,-30.7543606902058,53.0882681563249));
#87719=CARTESIAN_POINT('Ctrl Pts',(1.3313257234796,-30.7149667486081,53.0731908442583));
#87720=CARTESIAN_POINT('Ctrl Pts',(1.33362325006271,-30.6751933787958,53.0593528234812));
#87721=CARTESIAN_POINT('Ctrl Pts',(1.33749233009677,-30.608214240378,53.0360493238424));
#87722=CARTESIAN_POINT('Ctrl Pts',(1.34136141013084,-30.5398960582951,53.0161718100595));
#87723=CARTESIAN_POINT('Ctrl Pts',(1.3452304901649,-30.4706227140094,52.9998720482033));
#87724=CARTESIAN_POINT('Ctrl Pts',(1.34909380543655,-30.4014525840197,52.9835965722894));
#87725=CARTESIAN_POINT('Ctrl Pts',(1.35295712070819,-30.3313305857591,52.9708883773768));
#87726=CARTESIAN_POINT('Ctrl Pts',(1.35682043597984,-30.2606575336868,52.9618500514848));
#87727=CARTESIAN_POINT('Ctrl Pts',(1.36067921959847,-30.1900673808155,52.9528223275122));
#87728=CARTESIAN_POINT('Ctrl Pts',(1.3645380032171,-30.1189279375903,52.9474559832131));
#87729=CARTESIAN_POINT('Ctrl Pts',(1.36839678683573,-30.0476503185958,52.9458025874718));
#87730=CARTESIAN_POINT('Ctrl Pts',(1.37225313970019,-29.9764175993383,52.9441502332499));
#87731=CARTESIAN_POINT('Ctrl Pts',(1.37610949256465,-29.9050473615041,52.9462061985068));
#87732=CARTESIAN_POINT('Ctrl Pts',(1.37996584542911,-29.8339544822215,52.9519701055586));
#87733=CARTESIAN_POINT('Ctrl Pts',(1.38382105909059,-29.7628826044456,52.9577323098979));
#87734=CARTESIAN_POINT('Ctrl Pts',(1.38767627275206,-29.6920884064903,52.9672002422019));
#87735=CARTESIAN_POINT('Ctrl Pts',(1.39153148641353,-29.621983666113,52.9803215073149));
#87736=CARTESIAN_POINT('Ctrl Pts',(1.39538685081032,-29.5518761847048,52.9934432854573));
#87737=CARTESIAN_POINT('Ctrl Pts',(1.3992422152071,-29.4824586914817,53.010218588467));
#87738=CARTESIAN_POINT('Ctrl Pts',(1.40309757960388,-29.4141330555407,53.0305438603792));
#87739=CARTESIAN_POINT('Ctrl Pts',(1.40695697976471,-29.3457358968804,53.0508904086206));
#87740=CARTESIAN_POINT('Ctrl Pts',(1.41081637992554,-29.2784333436547,53.0747942050973));
#87741=CARTESIAN_POINT('Ctrl Pts',(1.41467578008637,-29.2126114976239,53.1021019761784));
#87742=CARTESIAN_POINT('Ctrl Pts',(1.41853736547651,-29.1467523826339,53.1294252091809));
#87743=CARTESIAN_POINT('Ctrl Pts',(1.42239895086665,-29.0823760824192,53.1601560442001));
#87744=CARTESIAN_POINT('Ctrl Pts',(1.42626053625679,-29.0198456135793,53.1940944262558));
#87745=CARTESIAN_POINT('Ctrl Pts',(1.43012887822424,-28.9572057358038,53.2280921899591));
#87746=CARTESIAN_POINT('Ctrl Pts',(1.43399722019169,-28.8964185518926,53.2653084519122));
#87747=CARTESIAN_POINT('Ctrl Pts',(1.43786556215914,-28.8378189326264,53.3054992684751));
#87748=CARTESIAN_POINT('Ctrl Pts',(1.44016321507319,-28.8030129131221,53.3293711359497));
#87749=CARTESIAN_POINT('Ctrl Pts',(1.44246086798723,-28.768978046545,53.3542916063209));
#87750=CARTESIAN_POINT('Ctrl Pts',(1.44475852090127,-28.7357786680281,53.3802031033839));
#87751=CARTESIAN_POINT('Ctrl Pts',(1.44858235440861,-28.6805271131827,53.423325913661));
#87752=CARTESIAN_POINT('Ctrl Pts',(1.45240618791595,-28.6273639390351,53.4693732488752));
#87753=CARTESIAN_POINT('Ctrl Pts',(1.45623002142328,-28.5766206997893,53.5181130507925));
#87754=CARTESIAN_POINT('Ctrl Pts',(1.4600473499653,-28.525963783081,53.5667699383463));
#87755=CARTESIAN_POINT('Ctrl Pts',(1.46386467850732,-28.4777189834451,53.6181098561307));
#87756=CARTESIAN_POINT('Ctrl Pts',(1.46768200704934,-28.4321859584129,53.6718596860639));
#87757=CARTESIAN_POINT('Ctrl Pts',(1.47149570176107,-28.3866962776419,53.7255583499112));
#87758=CARTESIAN_POINT('Ctrl Pts',(1.47530939647279,-28.3439135753923,53.7816620009685));
#87759=CARTESIAN_POINT('Ctrl Pts',(1.47912309118452,-28.3041006756,53.839860765253));
#87760=CARTESIAN_POINT('Ctrl Pts',(1.48293450371858,-28.2643116005019,53.8980247024393));
#87761=CARTESIAN_POINT('Ctrl Pts',(1.48674591625265,-28.2274890845337,53.958280856368));
#87762=CARTESIAN_POINT('Ctrl Pts',(1.49055732878671,-28.1938544633214,54.020287867363));
#87763=CARTESIAN_POINT('Ctrl Pts',(1.49436780766194,-28.1602280813803,54.0822796888729));
#87764=CARTESIAN_POINT('Ctrl Pts',(1.49817828653717,-28.1297882811194,54.1460210780293));
#87765=CARTESIAN_POINT('Ctrl Pts',(1.5019887654124,-28.1027110288688,54.2111450560945));
#87766=CARTESIAN_POINT('Ctrl Pts',(1.50580205935471,-28.0756137727595,54.2763171457942));
#87767=CARTESIAN_POINT('Ctrl Pts',(1.50961535329702,-28.0518842218103,54.3428734049702));
#87768=CARTESIAN_POINT('Ctrl Pts',(1.51342864723933,-28.031650167987,54.4104268482075));
#87769=CARTESIAN_POINT('Ctrl Pts',(1.51724327680651,-28.0114090270874,54.4780039523691));
#87770=CARTESIAN_POINT('Ctrl Pts',(1.5210579063737,-27.9946659420835,54.5465784518758));
#87771=CARTESIAN_POINT('Ctrl Pts',(1.52487253594088,-27.9814980324821,54.6157509015935));
#87772=CARTESIAN_POINT('Ctrl Pts',(1.52869346817071,-27.9683083664059,54.6850376404203));
#87773=CARTESIAN_POINT('Ctrl Pts',(1.53251440040054,-27.9587057437019,54.7549238082747));
#87774=CARTESIAN_POINT('Ctrl Pts',(1.53633533263036,-27.9527155258906,54.8250033012576));
#87775=CARTESIAN_POINT('Ctrl Pts',(1.53953198191616,-27.9477040197093,54.8836328575328));
#87776=CARTESIAN_POINT('Ctrl Pts',(1.54272863120196,-27.9452199894214,54.9423975000279));
#87777=CARTESIAN_POINT('Ctrl Pts',(1.54592528048776,-27.9452502738004,55.0010607462675));
#87778=CARTESIAN_POINT('Origin',(-1.54592528053767,-30.,55.));
#87779=CARTESIAN_POINT('',(0.393903215690563,-31.2520475724682,56.6292251037768));
#87780=CARTESIAN_POINT('',(0.452117492759457,-31.2520475724682,56.6292251037768));
#87781=CARTESIAN_POINT('',(-1.54592528053767,-31.2520475724682,56.6292251037768));
#87782=CARTESIAN_POINT('',(0.145925152667093,-27.9455328192711,54.9976432278968));
#87783=CARTESIAN_POINT('Ctrl Pts',(0.145925280537677,-27.9452513492555,
54.9976452678552));
#87784=CARTESIAN_POINT('Ctrl Pts',(0.149739558055857,-27.9451705070726,
55.0681884787126));
#87785=CARTESIAN_POINT('Ctrl Pts',(0.153553835574038,-27.9487267508694,
55.1387974637158));
#87786=CARTESIAN_POINT('Ctrl Pts',(0.157368113092218,-27.9559135127653,
55.209064571854));
#87787=CARTESIAN_POINT('Ctrl Pts',(0.161181088392145,-27.9630978210556,
55.279307690361));
#87788=CARTESIAN_POINT('Ctrl Pts',(0.164994063692073,-27.9739101382345,
55.3492086695877));
#87789=CARTESIAN_POINT('Ctrl Pts',(0.168807038992,-27.9882919346166,55.4183637438539));
#87790=CARTESIAN_POINT('Ctrl Pts',(0.172620052583361,-28.0026738754265,
55.4875195126033));
#87791=CARTESIAN_POINT('Ctrl Pts',(0.176433066174722,-28.0206252631438,
55.5559288755018));
#87792=CARTESIAN_POINT('Ctrl Pts',(0.180246079766083,-28.0420365947538,
55.6231988977981));
#87793=CARTESIAN_POINT('Ctrl Pts',(0.184063186873329,-28.0634709128085,
55.6905411387998));
#87794=CARTESIAN_POINT('Ctrl Pts',(0.187880293980576,-28.0883724380495,
55.7567411231829));
#87795=CARTESIAN_POINT('Ctrl Pts',(0.191697401087823,-28.1165822768063,
55.8214226941471));
#87796=CARTESIAN_POINT('Ctrl Pts',(0.195516676866285,-28.1448081428486,
55.8861410136376));
#87797=CARTESIAN_POINT('Ctrl Pts',(0.199335952644747,-28.1763458387153,
55.9493387592996));
#87798=CARTESIAN_POINT('Ctrl Pts',(0.203155228423209,-28.2109902488435,
56.0106639761894));
#87799=CARTESIAN_POINT('Ctrl Pts',(0.206981583712272,-28.2456988767667,
56.0721028671232));
#87800=CARTESIAN_POINT('Ctrl Pts',(0.210807939001335,-28.283525447051,56.1316618817862));
#87801=CARTESIAN_POINT('Ctrl Pts',(0.214634294290398,-28.324221670915,56.1890183153631));
#87802=CARTESIAN_POINT('Ctrl Pts',(0.217179710085972,-28.3512941206009,
56.2271736775747));
#87803=CARTESIAN_POINT('Ctrl Pts',(0.219725125881546,-28.3796356264345,
56.264354979052));
#87804=CARTESIAN_POINT('Ctrl Pts',(0.22227054167712,-28.4091638996304,56.3004760913838));
#87805=CARTESIAN_POINT('Ctrl Pts',(0.226143006984167,-28.4540867030981,
56.3554289028655));
#87806=CARTESIAN_POINT('Ctrl Pts',(0.230015472291213,-28.5019476711101,
56.4081582801573));
#87807=CARTESIAN_POINT('Ctrl Pts',(0.23388793759826,-28.5524985386363,56.4583336661581));
#87808=CARTESIAN_POINT('Ctrl Pts',(0.237754613392442,-28.602973830302,56.5084340376604));
#87809=CARTESIAN_POINT('Ctrl Pts',(0.241621289186625,-28.6561306971562,
56.5559876587984));
#87810=CARTESIAN_POINT('Ctrl Pts',(0.245487964980807,-28.7116807291363,
56.6006970415482));
#87811=CARTESIAN_POINT('Ctrl Pts',(0.249350054695347,-28.7671648758744,
56.6453533966327));
#87812=CARTESIAN_POINT('Ctrl Pts',(0.253212144409888,-28.8250361733924,
56.6871719121174));
#87813=CARTESIAN_POINT('Ctrl Pts',(0.257074234124429,-28.884970754992,56.7258932021643));
#87814=CARTESIAN_POINT('Ctrl Pts',(0.260933857400563,-28.9448670606931,
56.7645897637133));
#87815=CARTESIAN_POINT('Ctrl Pts',(0.264793480676698,-29.0068236298311,
56.8001927619133));
#87816=CARTESIAN_POINT('Ctrl Pts',(0.268653103952832,-29.070486209859,56.8324851094723));
#87817=CARTESIAN_POINT('Ctrl Pts',(0.272511547105436,-29.134129324332,56.8647675832803));
#87818=CARTESIAN_POINT('Ctrl Pts',(0.27636999025804,-29.1994769819466,56.8937411970124));
#87819=CARTESIAN_POINT('Ctrl Pts',(0.280228433410645,-29.2661503428946,
56.9192348067046));
#87820=CARTESIAN_POINT('Ctrl Pts',(0.284086981101935,-29.3328255102566,
56.9447291071076));
#87821=CARTESIAN_POINT('Ctrl Pts',(0.287945528793224,-29.4008259986621,
56.9667430451765));
#87822=CARTESIAN_POINT('Ctrl Pts',(0.291804076484514,-29.4697546186279,
56.9851542504384));
#87823=CARTESIAN_POINT('Ctrl Pts',(0.295666566280546,-29.5387536598665,
57.0035842656011));
#87824=CARTESIAN_POINT('Ctrl Pts',(0.299529056076578,-29.6086822562916,
57.0184040747128));
#87825=CARTESIAN_POINT('Ctrl Pts',(0.30339154587261,-29.679130615291,57.0295419188715));
#87826=CARTESIAN_POINT('Ctrl Pts',(0.307256172571424,-29.7496179494858,
57.0406859249856));
#87827=CARTESIAN_POINT('Ctrl Pts',(0.311120799270237,-29.8206251363632,
57.0481438597316));
#87828=CARTESIAN_POINT('Ctrl Pts',(0.31498542596905,-29.8917375229701,57.0518959034433));
#87829=CARTESIAN_POINT('Ctrl Pts',(0.318856698894589,-29.962972205747,57.0556543997661));
#87830=CARTESIAN_POINT('Ctrl Pts',(0.322727971820127,-30.0343119644734,
57.0556942799084));
#87831=CARTESIAN_POINT('Ctrl Pts',(0.326599244745665,-30.1053431155557,
57.0520478528789));
#87832=CARTESIAN_POINT('Ctrl Pts',(0.328868100669004,-30.1469726908851,
57.0499107734934));
#87833=CARTESIAN_POINT('Ctrl Pts',(0.331136956592343,-30.1884963605189,
57.0465084894332));
#87834=CARTESIAN_POINT('Ctrl Pts',(0.333405812515682,-30.2298323520304,
57.0418556884511));
#87835=CARTESIAN_POINT('Ctrl Pts',(0.337281012319212,-30.3004341141503,
57.0339087169108));
#87836=CARTESIAN_POINT('Ctrl Pts',(0.341156212122742,-30.3707563721026,
57.0222806500465));
#87837=CARTESIAN_POINT('Ctrl Pts',(0.345031411926271,-30.4403862442338,
57.0070021221687));
#87838=CARTESIAN_POINT('Ctrl Pts',(0.349104062239962,-30.5135639215033,
56.9909451174957));
#87839=CARTESIAN_POINT('Ctrl Pts',(0.353176712553653,-30.5859762357596,
56.9708557003268));
#87840=CARTESIAN_POINT('Ctrl Pts',(0.357249362867344,-30.6571493257187,
56.9468313553586));
#87841=CARTESIAN_POINT('Ctrl Pts',(0.361114528254948,-30.7246964369731,
56.9240309528004));
#87842=CARTESIAN_POINT('Ctrl Pts',(0.364979693642552,-30.7911269703477,
56.897686913658));
#87843=CARTESIAN_POINT('Ctrl Pts',(0.368844859030155,-30.8560479883579,
56.8679345288656));
#87844=CARTESIAN_POINT('Ctrl Pts',(0.372707534701384,-30.9209271879967,
56.8382013088417));
#87845=CARTESIAN_POINT('Ctrl Pts',(0.376570210372613,-30.9842983642662,
56.8050643040583));
#87846=CARTESIAN_POINT('Ctrl Pts',(0.380432886043842,-31.0457881929967,
56.7687070469381));
#87847=CARTESIAN_POINT('Ctrl Pts',(0.384294620004037,-31.107263030655,56.7323586536297));
#87848=CARTESIAN_POINT('Ctrl Pts',(0.388156353964232,-31.1668570150223,
56.692791812487));
#87849=CARTESIAN_POINT('Ctrl Pts',(0.392018087924427,-31.2242225181329,
56.6502353736956));
#87850=CARTESIAN_POINT('Ctrl Pts',(0.392646463846472,-31.2335569521676,
56.6433106497917));
#87851=CARTESIAN_POINT('Ctrl Pts',(0.393274839768517,-31.2428324444266,
56.6363068622567));
#87852=CARTESIAN_POINT('Ctrl Pts',(0.393903215690563,-31.2520475724682,
56.6292251037768));
#87853=CARTESIAN_POINT('',(0.,-29.4698297828114,53.0148256743283));
#87854=CARTESIAN_POINT('Ctrl Pts',(-2.77555756156289E-16,-29.4698297828114,
53.0148256743283));
#87855=CARTESIAN_POINT('Ctrl Pts',(0.0370450902795195,-28.8097276504722,
53.1911157292334));
#87856=CARTESIAN_POINT('Ctrl Pts',(0.085686536603176,-28.0750579168316,
53.887168576849));
#87857=CARTESIAN_POINT('Ctrl Pts',(0.134327982926832,-27.9457073141171,
54.7833755124352));
#87858=CARTESIAN_POINT('Ctrl Pts',(0.145924338970969,-27.9473239353676,
54.9976302467543));
#87859=CARTESIAN_POINT('',(5.31147209548166E-9,-30.5303401832825,53.0148710740871));
#87860=CARTESIAN_POINT('Origin',(0.,-30.,55.));
#87861=CARTESIAN_POINT('',(0.204074719418397,-27.9452505428834,55.0014936462286));
#87862=CARTESIAN_POINT('Ctrl Pts',(5.31147215099281E-9,-30.5303401832825,
53.0148710740871));
#87863=CARTESIAN_POINT('Ctrl Pts',(0.00385890060565744,-30.4620053990835,
52.9966149893042));
#87864=CARTESIAN_POINT('Ctrl Pts',(0.00771779589984257,-30.3925893645069,
52.9818548053524));
#87865=CARTESIAN_POINT('Ctrl Pts',(0.0115766911940278,-30.322484042902,
52.9707140160703));
#87866=CARTESIAN_POINT('Ctrl Pts',(0.0154298196873703,-30.2524834879199,
52.9595898757792));
#87867=CARTESIAN_POINT('Ctrl Pts',(0.0192829481807127,-30.1817961688685,
52.952074471318));
#87868=CARTESIAN_POINT('Ctrl Pts',(0.0231360766740552,-30.1108274410599,
52.9482410373516));
#87869=CARTESIAN_POINT('Ctrl Pts',(0.0269846844776238,-30.0399419774359,
52.9444121009683));
#87870=CARTESIAN_POINT('Ctrl Pts',(0.0308332922811925,-29.9687762463427,
52.9442565816047));
#87871=CARTESIAN_POINT('Ctrl Pts',(0.0346819000847611,-29.8977422088653,
52.947796085509));
#87872=CARTESIAN_POINT('Ctrl Pts',(0.0385281035507021,-29.8267525484244,
52.9513333781819));
#87873=CARTESIAN_POINT('Ctrl Pts',(0.042374307016643,-29.7558949052976,
52.9585610906355));
#87874=CARTESIAN_POINT('Ctrl Pts',(0.0462205104825839,-29.6855812197391,
52.9694487464929));
#87875=CARTESIAN_POINT('Ctrl Pts',(0.0500656158362666,-29.6152876091248,
52.9803332938646));
#87876=CARTESIAN_POINT('Ctrl Pts',(0.0539107211899489,-29.5455381304157,
52.9948756354664));
#87877=CARTESIAN_POINT('Ctrl Pts',(0.0577558265436315,-29.4767378155319,
53.012993646511));
#87878=CARTESIAN_POINT('Ctrl Pts',(0.0616011384233991,-29.4079338052853,
53.0311126306998));
#87879=CARTESIAN_POINT('Ctrl Pts',(0.0654464503031668,-29.3400795319328,
53.0528075386411));
#87880=CARTESIAN_POINT('Ctrl Pts',(0.0692917621829343,-29.2735663538694,
53.0779459632286));
#87881=CARTESIAN_POINT('Ctrl Pts',(0.0731410484831663,-29.2069844294093,
53.1031103702778));
#87882=CARTESIAN_POINT('Ctrl Pts',(0.0769903347833989,-29.1417468242309,
53.1317252233557));
#87883=CARTESIAN_POINT('Ctrl Pts',(0.0808396210836309,-29.0782254133911,
53.1636097435507));
#87884=CARTESIAN_POINT('Ctrl Pts',(0.0846911736894365,-29.0146666036892,
53.1955130360739));
#87885=CARTESIAN_POINT('Ctrl Pts',(0.0885427262952419,-28.9528264236558,
53.2306895847781));
#87886=CARTESIAN_POINT('Ctrl Pts',(0.0923942789010475,-28.8930501979511,
53.2689137230502));
#87887=CARTESIAN_POINT('Ctrl Pts',(0.0962522709070446,-28.8331740325393,
53.3072017681538));
#87888=CARTESIAN_POINT('Ctrl Pts',(0.100110262913041,-28.7753691044501,
53.3485472865186));
#87889=CARTESIAN_POINT('Ctrl Pts',(0.103968254919039,-28.719949233271,53.3926831061995));
#87890=CARTESIAN_POINT('Ctrl Pts',(0.105632468402095,-28.696042885953,53.4117218771676));
#87891=CARTESIAN_POINT('Ctrl Pts',(0.107296681885152,-28.6725798933521,
53.4312793816445));
#87892=CARTESIAN_POINT('Ctrl Pts',(0.108960895368209,-28.6495832862577,
53.4513321008862));
#87893=CARTESIAN_POINT('Ctrl Pts',(0.1129239713703,-28.594820299037,53.4990846586035));
#87894=CARTESIAN_POINT('Ctrl Pts',(0.116887047372392,-28.5424701409817,
53.549853287079));
#87895=CARTESIAN_POINT('Ctrl Pts',(0.120850123374483,-28.4928872821031,
53.6033580208037));
#87896=CARTESIAN_POINT('Ctrl Pts',(0.124661299720926,-28.4452048710549,
53.6548119862302));
#87897=CARTESIAN_POINT('Ctrl Pts',(0.128472476067368,-28.4000818931433,
53.708795745255));
#87898=CARTESIAN_POINT('Ctrl Pts',(0.132283652413811,-28.3578002588971,
53.7650192014361));
#87899=CARTESIAN_POINT('Ctrl Pts',(0.136091341654092,-28.3155573110128,
53.8211912149279));
#87900=CARTESIAN_POINT('Ctrl Pts',(0.139899030894372,-28.276150852727,53.879598466174));
#87901=CARTESIAN_POINT('Ctrl Pts',(0.143706720134652,-28.2398237521968,
53.939916447081));
#87902=CARTESIAN_POINT('Ctrl Pts',(0.147512279870369,-28.2035169681162,
54.0002006942961));
#87903=CARTESIAN_POINT('Ctrl Pts',(0.151317839606087,-28.1702863835626,
54.0623931243556));
#87904=CARTESIAN_POINT('Ctrl Pts',(0.155123399341804,-28.1403314967629,
54.1261403885246));
#87905=CARTESIAN_POINT('Ctrl Pts',(0.158928184118078,-28.1103827099391,
54.1898746712801));
#87906=CARTESIAN_POINT('Ctrl Pts',(0.162732968894353,-28.0837085076307,
54.2551627066053));
#87907=CARTESIAN_POINT('Ctrl Pts',(0.166537753670627,-28.0604615061024,
54.3216284254264));
#87908=CARTESIAN_POINT('Ctrl Pts',(0.170345033971954,-28.0371992570692,
54.3881377385311));
#87909=CARTESIAN_POINT('Ctrl Pts',(0.17415231427328,-28.0173688617457,54.4558258046817));
#87910=CARTESIAN_POINT('Ctrl Pts',(0.177959594574607,-28.001073570741,54.5242997867252));
#87911=CARTESIAN_POINT('Ctrl Pts',(0.181768385432865,-27.9847718145004,
54.5928009361533));
#87912=CARTESIAN_POINT('Ctrl Pts',(0.185577176291123,-27.9720080458716,
54.6620881305532));
#87913=CARTESIAN_POINT('Ctrl Pts',(0.189385967149382,-27.9628341983099,
54.7317593264916));
#87914=CARTESIAN_POINT('Ctrl Pts',(0.193199808147877,-27.9536481869885,
54.8015229006474));
#87915=CARTESIAN_POINT('Ctrl Pts',(0.197013649146372,-27.9480616306873,
54.8716709942671));
#87916=CARTESIAN_POINT('Ctrl Pts',(0.200827490144868,-27.9460744487514,
54.9417986904941));
#87917=CARTESIAN_POINT('Ctrl Pts',(0.201909899902711,-27.9455104647996,
54.9617016971274));
#87918=CARTESIAN_POINT('Ctrl Pts',(0.202992309660554,-27.945236083957,54.9816030786799));
#87919=CARTESIAN_POINT('Ctrl Pts',(0.204074719418397,-27.9452505428834,
55.0014936462286));
#87920=CARTESIAN_POINT('Ctrl Pts',(0.204074719462322,-27.945250542884,55.0014936470358));
#87921=CARTESIAN_POINT('Ctrl Pts',(0.209415201710472,-27.9453218815624,
55.0996313644095));
#87922=CARTESIAN_POINT('Ctrl Pts',(0.214755683958621,-27.9524246358466,
55.1975148488935));
#87923=CARTESIAN_POINT('Ctrl Pts',(0.22009616620677,-27.9664469146436,55.2943797063953));
#87924=CARTESIAN_POINT('Ctrl Pts',(0.223961020165476,-27.9765946985329,
55.3644798416603));
#87925=CARTESIAN_POINT('Ctrl Pts',(0.227825874124181,-27.9903917548322,
55.4341948503752));
#87926=CARTESIAN_POINT('Ctrl Pts',(0.231690728082887,-28.0077969414506,
55.5031148338168));
#87927=CARTESIAN_POINT('Ctrl Pts',(0.235549755777647,-28.0251758897655,
55.5719309204439));
#87928=CARTESIAN_POINT('Ctrl Pts',(0.239408783472407,-28.0461520542666,
55.6399538923791));
#87929=CARTESIAN_POINT('Ctrl Pts',(0.243267811167167,-28.0706328265759,
55.7067813471035));
#87930=CARTESIAN_POINT('Ctrl Pts',(0.247122236420484,-28.0950844020693,
55.7735291005479));
#87931=CARTESIAN_POINT('Ctrl Pts',(0.250976661673801,-28.1230321167656,
55.8390837137948));
#87932=CARTESIAN_POINT('Ctrl Pts',(0.254831086927118,-28.1543333061832,
55.9030570401892));
#87933=CARTESIAN_POINT('Ctrl Pts',(0.258683039994727,-28.1856144193642,
55.9669893348));
#87934=CARTESIAN_POINT('Ctrl Pts',(0.262534993062336,-28.220244526808,56.0293419181982));
#87935=CARTESIAN_POINT('Ctrl Pts',(0.266386946129945,-28.2580330866495,
56.0897471428235));
#87936=CARTESIAN_POINT('Ctrl Pts',(0.270237725008371,-28.2958101274207,
56.1501339541504));
#87937=CARTESIAN_POINT('Ctrl Pts',(0.274088503886798,-28.3367434512255,
56.2085741724364));
#87938=CARTESIAN_POINT('Ctrl Pts',(0.277939282765224,-28.3805977331326,
56.2647267928547));
#87939=CARTESIAN_POINT('Ctrl Pts',(0.281790183797984,-28.4244534061843,
56.3208811945454));
#87940=CARTESIAN_POINT('Ctrl Pts',(0.285641084830744,-28.4712299197825,
56.3747474718326));
#87941=CARTESIAN_POINT('Ctrl Pts',(0.289491985863504,-28.5206510640933,
56.4260169312921));
#87942=CARTESIAN_POINT('Ctrl Pts',(0.293346909493499,-28.5701238330386,
56.4773399461102));
#87943=CARTESIAN_POINT('Ctrl Pts',(0.297201833123494,-28.6222464086909,
56.5260603767546));
#87944=CARTESIAN_POINT('Ctrl Pts',(0.30105675675349,-28.6767056801163,56.5719063920805));
#87945=CARTESIAN_POINT('Ctrl Pts',(0.30491385131992,-28.7311956207916,56.6177782260203));
#87946=CARTESIAN_POINT('Ctrl Pts',(0.308770945886351,-28.7880244880892,
56.6607721284675));
#87947=CARTESIAN_POINT('Ctrl Pts',(0.312628040452781,-28.8468482568665,
56.7006582901359));
#87948=CARTESIAN_POINT('Ctrl Pts',(0.316491917659155,-28.9057754663131,
56.7406145909904));
#87949=CARTESIAN_POINT('Ctrl Pts',(0.320355794865529,-28.9667041640678,
56.7774519883196));
#87950=CARTESIAN_POINT('Ctrl Pts',(0.324219672071903,-29.0292643129354,
56.8109858608944));
#87951=CARTESIAN_POINT('Ctrl Pts',(0.326556927063046,-29.0671068768622,
56.8312704628269));
#87952=CARTESIAN_POINT('Ctrl Pts',(0.328894182054188,-29.1055459530557,
56.8503472123624));
#87953=CARTESIAN_POINT('Ctrl Pts',(0.33123143704533,-29.1444964052382,56.868183920777));
#87954=CARTESIAN_POINT('Ctrl Pts',(0.335101212232454,-29.208986370584,56.8977160222825));
#87955=CARTESIAN_POINT('Ctrl Pts',(0.338970987419577,-29.2751333583356,
56.9239626235659));
#87956=CARTESIAN_POINT('Ctrl Pts',(0.342840762606701,-29.3425693897772,
56.9467363856573));
#87957=CARTESIAN_POINT('Ctrl Pts',(0.346704773776642,-29.4099049754758,
56.9694762263063));
#87958=CARTESIAN_POINT('Ctrl Pts',(0.350568784946584,-29.4785253373009,
56.9887533416089));
#87959=CARTESIAN_POINT('Ctrl Pts',(0.354432796116526,-29.5480410034477,
57.0044277557287));
#87960=CARTESIAN_POINT('Ctrl Pts',(0.358292273241919,-29.6174750996629,
57.0200837774347));
#87961=CARTESIAN_POINT('Ctrl Pts',(0.362151750367312,-29.6878019420199,
57.0321453888722));
#87962=CARTESIAN_POINT('Ctrl Pts',(0.366011227492706,-29.7586169935523,
57.0405224347451));
#87963=CARTESIAN_POINT('Ctrl Pts',(0.369868271988589,-29.8293874103378,
57.0488942005637));
#87964=CARTESIAN_POINT('Ctrl Pts',(0.373725316484471,-29.9006449446999,
57.053585951543));
#87965=CARTESIAN_POINT('Ctrl Pts',(0.377582360980354,-29.9719764123368,
57.0545588920823));
#87966=CARTESIAN_POINT('Ctrl Pts',(0.381438263340815,-30.0432867575323,
57.0555315445176));
#87967=CARTESIAN_POINT('Ctrl Pts',(0.385294165701275,-30.1146705072659,
57.0527875661136));
#87968=CARTESIAN_POINT('Ctrl Pts',(0.389150068061736,-30.1857126517967,
57.0463402389296));
#87969=CARTESIAN_POINT('Ctrl Pts',(0.393006117165451,-30.2567574999633,
57.0398926663811));
#87970=CARTESIAN_POINT('Ctrl Pts',(0.396862166269167,-30.3274602337197,
57.0297415113169));
#87971=CARTESIAN_POINT('Ctrl Pts',(0.400718215372883,-30.3974108749329,
57.0159519237782));
#87972=CARTESIAN_POINT('Ctrl Pts',(0.404578289322704,-30.4674345288485,
57.0021479430184));
#87973=CARTESIAN_POINT('Ctrl Pts',(0.408438363272525,-30.5367040457586,
56.9846980427912));
#87974=CARTESIAN_POINT('Ctrl Pts',(0.412298437222346,-30.6048204469937,
56.9637183579623));
#87975=CARTESIAN_POINT('Ctrl Pts',(0.41616069125129,-30.6729753187727,56.9427268243002));
#87976=CARTESIAN_POINT('Ctrl Pts',(0.420022945280233,-30.7399753221862,
56.9182017044133));
#87977=CARTESIAN_POINT('Ctrl Pts',(0.423885199309177,-30.8054400360123,
56.8903078878555));
#87978=CARTESIAN_POINT('Ctrl Pts',(0.427754194419916,-30.8710190103161,
56.8623653861264));
#87979=CARTESIAN_POINT('Ctrl Pts',(0.431623189530655,-30.9350569086456,
56.8310426622144));
#87980=CARTESIAN_POINT('Ctrl Pts',(0.435492184641395,-30.9971971788319,
56.7965509592076));
#87981=CARTESIAN_POINT('Ctrl Pts',(0.437783692388893,-31.0340012859677,
56.7761223976813));
#87982=CARTESIAN_POINT('Ctrl Pts',(0.440075200136391,-31.070140249418,56.7545830404281));
#87983=CARTESIAN_POINT('Ctrl Pts',(0.44236670788389,-31.1055451381042,56.7319836922195));
#87984=CARTESIAN_POINT('Ctrl Pts',(0.445616969509079,-31.1557632319189,
56.6999289045728));
#87985=CARTESIAN_POINT('Ctrl Pts',(0.448867231134268,-31.204668249553,56.6656357667991));
#87986=CARTESIAN_POINT('Ctrl Pts',(0.452117492759457,-31.2520475724682,
56.6292251037768));
#87987=CARTESIAN_POINT('Origin',(-1.54592528053767,30.,55.));
#87988=CARTESIAN_POINT('',(9.49394873882619,28.7479524050421,56.6292250864936));
#87989=CARTESIAN_POINT('',(9.55204617709054,28.7459570691003,56.6318367151304));
#87990=CARTESIAN_POINT('',(-1.54592528053767,28.7479524050421,56.6292250864936));
#87991=CARTESIAN_POINT('',(10.,32.0533758325287,54.9248651020699));
#87992=CARTESIAN_POINT('Ctrl Pts',(9.55204617709054,28.7459570691003,56.6318367151304));
#87993=CARTESIAN_POINT('Ctrl Pts',(9.55318375694229,28.7293604144358,56.6191575145376));
#87994=CARTESIAN_POINT('Ctrl Pts',(9.59136642707355,28.1793878778151,56.1844488346597));
#87995=CARTESIAN_POINT('Ctrl Pts',(9.66659418748432,27.5871748102564,54.7282396850668));
#87996=CARTESIAN_POINT('Ctrl Pts',(9.77772945832289,28.9189493130402,52.8236099253744));
#87997=CARTESIAN_POINT('Ctrl Pts',(9.88886472916144,31.2437676373092,52.9151786827749));
#87998=CARTESIAN_POINT('Ctrl Pts',(9.96295490972048,32.0283922803563,54.2420848806971));
#87999=CARTESIAN_POINT('Ctrl Pts',(10.,32.0533758325287,54.92486510207));
#88000=CARTESIAN_POINT('',(9.99999281908575,31.8181858731057,55.9591737972435));
#88001=CARTESIAN_POINT('Origin',(10.,30.,55.));
#88002=CARTESIAN_POINT('',(9.94592528058885,32.054749999972,55.0000107214664));
#88003=CARTESIAN_POINT('Ctrl Pts',(9.94592528058884,32.054749999972,55.0000107214664));
#88004=CARTESIAN_POINT('Ctrl Pts',(9.94992923499555,32.0547496125334,55.0742626500147));
#88005=CARTESIAN_POINT('Ctrl Pts',(9.95393318940226,32.0507200896955,55.1484433401657));
#88006=CARTESIAN_POINT('Ctrl Pts',(9.95793714380898,32.0427102750594,55.2221087451377));
#88007=CARTESIAN_POINT('Ctrl Pts',(9.96195105284767,32.0346805464212,55.2959572970492));
#88008=CARTESIAN_POINT('Ctrl Pts',(9.96596496188636,32.0226508056886,55.3692875772289));
#88009=CARTESIAN_POINT('Ctrl Pts',(9.96997887092505,32.0067214128151,55.4416635980576));
#88010=CARTESIAN_POINT('Ctrl Pts',(9.97399818909952,31.9907705535238,55.514137152667));
#88011=CARTESIAN_POINT('Ctrl Pts',(9.978017507274,31.9709096843372,55.5856534725178));
#88012=CARTESIAN_POINT('Ctrl Pts',(9.98203682544847,31.9472888596583,55.6557923905861));
#88013=CARTESIAN_POINT('Ctrl Pts',(9.98606643459486,31.9236075567508,55.726110890764));
#88014=CARTESIAN_POINT('Ctrl Pts',(9.99009604374126,31.896147221868,55.7950445439403));
#88015=CARTESIAN_POINT('Ctrl Pts',(9.99412565288765,31.86510586548,55.8621935241303));
#88016=CARTESIAN_POINT('Ctrl Pts',(9.99608057294537,31.8500464966883,55.8947701049995));
#88017=CARTESIAN_POINT('Ctrl Pts',(9.99803549300309,31.8341449817694,55.9269270350611));
#88018=CARTESIAN_POINT('Ctrl Pts',(9.9999904130608,31.8174276447438,55.9586210505831));
#88019=CARTESIAN_POINT('Ctrl Pts',(9.49394873882619,28.7479524050421,56.6292250864936));
#88020=CARTESIAN_POINT('Ctrl Pts',(9.4978046533836,28.691402000007,56.5857665127182));
#88021=CARTESIAN_POINT('Ctrl Pts',(9.50166056794101,28.6371010084152,56.5393479750722));
#88022=CARTESIAN_POINT('Ctrl Pts',(9.50551648249842,28.5853662515599,56.4902378737216));
#88023=CARTESIAN_POINT('Ctrl Pts',(9.50937266247207,28.5336279336182,56.441124391949));
#88024=CARTESIAN_POINT('Ctrl Pts',(9.51322884244571,28.4844565516489,56.3893193146642));
#88025=CARTESIAN_POINT('Ctrl Pts',(9.51708502241936,28.4381327212654,56.3351285204497));
#88026=CARTESIAN_POINT('Ctrl Pts',(9.52094529771214,28.3917596943012,56.2808801748247));
#88027=CARTESIAN_POINT('Ctrl Pts',(9.52480557300492,28.3482405707212,56.2242414252943));
#88028=CARTESIAN_POINT('Ctrl Pts',(9.5286658482977,28.3078156308828,56.1655512101214));
#88029=CARTESIAN_POINT('Ctrl Pts',(9.53252841044457,28.2673667430272,56.1068262264544));
#88030=CARTESIAN_POINT('Ctrl Pts',(9.53639097259144,28.2300159415455,56.0460477720046));
#88031=CARTESIAN_POINT('Ctrl Pts',(9.54025353473831,28.1959586525825,55.9835814045152));
#88032=CARTESIAN_POINT('Ctrl Pts',(9.54412272140385,28.1618429533888,55.9210079035736));
#88033=CARTESIAN_POINT('Ctrl Pts',(9.54799190806938,28.1310322513002,55.8567411489902));
#88034=CARTESIAN_POINT('Ctrl Pts',(9.55186109473492,28.1036744331779,55.791168065026));
#88035=CARTESIAN_POINT('Ctrl Pts',(9.55378516052864,28.0900699610782,55.7585599386287));
#88036=CARTESIAN_POINT('Ctrl Pts',(9.55570922632237,28.0773185709614,55.7256290338948));
#88037=CARTESIAN_POINT('Ctrl Pts',(9.55763329211609,28.0654338157958,55.6924241773895));
#88038=CARTESIAN_POINT('Ctrl Pts',(9.56150302050322,28.0415309042693,55.6256417543415));
#88039=CARTESIAN_POINT('Ctrl Pts',(9.56537274889035,28.0210434541086,55.5574898205418));
#88040=CARTESIAN_POINT('Ctrl Pts',(9.56924247727748,28.0041265586444,55.4883510710455));
#88041=CARTESIAN_POINT('Ctrl Pts',(9.5731064517937,27.9872348167886,55.4193151234515));
#88042=CARTESIAN_POINT('Ctrl Pts',(9.57697042630992,27.9739032056838,55.3492957405771));
#88043=CARTESIAN_POINT('Ctrl Pts',(9.58083440082614,27.9642377859759,55.2786929680703));
#88044=CARTESIAN_POINT('Ctrl Pts',(9.58469385650073,27.9545836697849,55.2081727641071));
#88045=CARTESIAN_POINT('Ctrl Pts',(9.58855331217531,27.9485872939616,55.1370710045039));
#88046=CARTESIAN_POINT('Ctrl Pts',(9.5924127678499,27.9463037898525,55.0657984720641));
#88047=CARTESIAN_POINT('Ctrl Pts',(9.59626980028674,27.944021719488,54.9945706895333));
#88048=CARTESIAN_POINT('Ctrl Pts',(9.60012683272359,27.9454479112186,54.9231728310949));
#88049=CARTESIAN_POINT('Ctrl Pts',(9.60398386516044,27.9505855838444,54.8520198886547));
#88050=CARTESIAN_POINT('Ctrl Pts',(9.60783976484055,27.9557217476073,54.7808878428433));
#88051=CARTESIAN_POINT('Ctrl Pts',(9.61169566452066,27.9645671933069,54.7100010542932));
#88052=CARTESIAN_POINT('Ctrl Pts',(9.61555156420076,27.9770730972883,54.6397718656387));
#88053=CARTESIAN_POINT('Ctrl Pts',(9.6194076199994,27.9895795076116,54.5695398335291));
#88054=CARTESIAN_POINT('Ctrl Pts',(9.62326367579804,28.0057465831644,54.4999659318545));
#88055=CARTESIAN_POINT('Ctrl Pts',(9.62711973159668,28.0254742551705,54.4314530401933));
#88056=CARTESIAN_POINT('Ctrl Pts',(9.63097982647678,28.0452225912122,54.362868383712));
#88057=CARTESIAN_POINT('Ctrl Pts',(9.63483992135688,28.0685388341787,54.2953474233671));
#88058=CARTESIAN_POINT('Ctrl Pts',(9.63870001623698,28.0952730616512,54.229277707064));
#88059=CARTESIAN_POINT('Ctrl Pts',(9.64256229925823,28.1220224437418,54.1631705383484));
#88060=CARTESIAN_POINT('Ctrl Pts',(9.64642458227949,28.152193461956,54.098516691584));
#88061=CARTESIAN_POINT('Ctrl Pts',(9.65028686530075,28.185589211249,54.0356810423082));
#88062=CARTESIAN_POINT('Ctrl Pts',(9.65415590181592,28.2190433555348,53.9727355201483));
#88063=CARTESIAN_POINT('Ctrl Pts',(9.65802493833108,28.2557332387271,53.9116149594333));
#88064=CARTESIAN_POINT('Ctrl Pts',(9.66189397484625,28.2954178206257,53.8526564785299));
#88065=CARTESIAN_POINT('Ctrl Pts',(9.66418550421571,28.3189219629564,53.8177369087509));
#88066=CARTESIAN_POINT('Ctrl Pts',(9.66647703358517,28.3434758107717,53.7835751766599));
#88067=CARTESIAN_POINT('Ctrl Pts',(9.66876856295463,28.3690228362396,53.7502356006862));
#88068=CARTESIAN_POINT('Ctrl Pts',(9.67263319854557,28.4121075748347,53.6940088232283));
#88069=CARTESIAN_POINT('Ctrl Pts',(9.67649783413651,28.4581888703725,53.639900970039));
#88070=CARTESIAN_POINT('Ctrl Pts',(9.68036246972745,28.5070304189907,53.5882495288894));
#88071=CARTESIAN_POINT('Ctrl Pts',(9.68422132903282,28.5557989664874,53.5366752886731));
#88072=CARTESIAN_POINT('Ctrl Pts',(9.68808018833819,28.6073192465963,53.4875505241705));
#88073=CARTESIAN_POINT('Ctrl Pts',(9.69193904764356,28.6613137277076,53.4411810153594));
#88074=CARTESIAN_POINT('Ctrl Pts',(9.69579337937049,28.7152448573906,53.3948659116385));
#88075=CARTESIAN_POINT('Ctrl Pts',(9.69964771109743,28.7716440546169,53.3512999585715));
#88076=CARTESIAN_POINT('Ctrl Pts',(9.70350204282436,28.8301970897572,53.3107520271768));
#88077=CARTESIAN_POINT('Ctrl Pts',(9.70735394857745,28.8887132707444,53.2702296172545));
#88078=CARTESIAN_POINT('Ctrl Pts',(9.71120585433055,28.9493802008428,53.2327217371875));
#88079=CARTESIAN_POINT('Ctrl Pts',(9.71505776008364,29.0118519125401,53.1984559623064));
#88080=CARTESIAN_POINT('Ctrl Pts',(9.71890853777658,29.0743053289173,53.1642002224204));
#88081=CARTESIAN_POINT('Ctrl Pts',(9.72275931546952,29.1385620508987,53.133184936992));
#88082=CARTESIAN_POINT('Ctrl Pts',(9.72661009316246,29.2042500770591,53.105592540492));
#88083=CARTESIAN_POINT('Ctrl Pts',(9.73046103910404,29.2699409732687,53.0779989384217));
#88084=CARTESIAN_POINT('Ctrl Pts',(9.73431198504562,29.3370628479334,53.0538287087524));
#88085=CARTESIAN_POINT('Ctrl Pts',(9.7381629309872,29.4052238384774,53.0332161074016));
#88086=CARTESIAN_POINT('Ctrl Pts',(9.74201796951611,29.4734572670173,53.012581600038));
#88087=CARTESIAN_POINT('Ctrl Pts',(9.74587300804502,29.5427315487197,52.9955124095462));
#88088=CARTESIAN_POINT('Ctrl Pts',(9.74972804657392,29.6126406530814,52.982092594083));
#88089=CARTESIAN_POINT('Ctrl Pts',(9.75358529565015,29.6825898445608,52.9686650834601));
#88090=CARTESIAN_POINT('Ctrl Pts',(9.75744254472639,29.7531741006322,52.9588911798621));
#88091=CARTESIAN_POINT('Ctrl Pts',(9.76129979380262,29.8239809778604,52.9528031686364));
#88092=CARTESIAN_POINT('Ctrl Pts',(9.76516388654014,29.8949134830361,52.9467043558561));
#88093=CARTESIAN_POINT('Ctrl Pts',(9.76902797927766,29.966068911074,52.9443045080096));
#88094=CARTESIAN_POINT('Ctrl Pts',(9.77289207201518,30.0370342234693,52.9455837742093));
#88095=CARTESIAN_POINT('Ctrl Pts',(9.77522932594121,30.0799586474608,52.9463575573845));
#88096=CARTESIAN_POINT('Ctrl Pts',(9.77756657986724,30.1228135799402,52.9484763725428));
#88097=CARTESIAN_POINT('Ctrl Pts',(9.77990383379327,30.1655090399434,52.9519266809518));
#88098=CARTESIAN_POINT('Ctrl Pts',(9.78377991976378,30.2363148996234,52.9576486488858));
#88099=CARTESIAN_POINT('Ctrl Pts',(9.78765600573429,30.3069601528984,52.9670577856244));
#88100=CARTESIAN_POINT('Ctrl Pts',(9.79153209170481,30.3770311499455,52.9801373624747));
#88101=CARTESIAN_POINT('Ctrl Pts',(9.79540239402569,30.4469975914953,52.99319742281));
#88102=CARTESIAN_POINT('Ctrl Pts',(9.79927269634657,30.5163910059807,53.0099169627378));
#88103=CARTESIAN_POINT('Ctrl Pts',(9.80314299866746,30.5848021793035,53.0302274310007));
#88104=CARTESIAN_POINT('Ctrl Pts',(9.80700870784549,30.653132164578,53.0505137954924));
#88105=CARTESIAN_POINT('Ctrl Pts',(9.81087441702353,30.7204817628165,53.0743824851228));
#88106=CARTESIAN_POINT('Ctrl Pts',(9.81474012620157,30.7864529913537,53.1017141271951));
#88107=CARTESIAN_POINT('Ctrl Pts',(9.81860336270708,30.8523820218784,53.1290282867829));
#88108=CARTESIAN_POINT('Ctrl Pts',(9.82246659921258,30.9169339861647,53.1598008188452));
#88109=CARTESIAN_POINT('Ctrl Pts',(9.82632983571809,30.9797284531328,53.1938633161851));
#88110=CARTESIAN_POINT('Ctrl Pts',(9.83019188108792,31.0425035589435,53.2279153111765));
#88111=CARTESIAN_POINT('Ctrl Pts',(9.83405392645776,31.1035218182551,53.2652550267964));
#88112=CARTESIAN_POINT('Ctrl Pts',(9.83791597182759,31.1624266341236,53.3056677177189));
#88113=CARTESIAN_POINT('Ctrl Pts',(9.8417781059365,31.2213328034613,53.3460813372127));
#88114=CARTESIAN_POINT('Ctrl Pts',(9.84564024004541,31.2781250351691,53.3895677966547));
#88115=CARTESIAN_POINT('Ctrl Pts',(9.84950237415431,31.3324764296357,53.4358695300694));
#88116=CARTESIAN_POINT('Ctrl Pts',(9.85336840341607,31.386882640166,53.4822179610674));
#88117=CARTESIAN_POINT('Ctrl Pts',(9.85723443267783,31.43884272998,53.5313870198914));
#88118=CARTESIAN_POINT('Ctrl Pts',(9.86110046193959,31.4880642720665,53.5830800006002));
#88119=CARTESIAN_POINT('Ctrl Pts',(9.86496860676023,31.5373127490423,53.6348012686128));
#88120=CARTESIAN_POINT('Ctrl Pts',(9.86883675158086,31.5838193791356,53.6890488410715));
#88121=CARTESIAN_POINT('Ctrl Pts',(9.87270489640149,31.6273316876262,53.7454924707489));
#88122=CARTESIAN_POINT('Ctrl Pts',(9.87657961756178,31.6709179725922,53.8020320617973));
#88123=CARTESIAN_POINT('Ctrl Pts',(9.88045433872207,31.7114994963422,53.8607747664305));
#88124=CARTESIAN_POINT('Ctrl Pts',(9.88432905988236,31.7488672088626,53.9213614839692));
#88125=CARTESIAN_POINT('Ctrl Pts',(9.88656574146552,31.7704377092784,53.9563351478012));
#88126=CARTESIAN_POINT('Ctrl Pts',(9.88880242304867,31.7909381626963,53.991922797583));
#88127=CARTESIAN_POINT('Ctrl Pts',(9.89103910463183,31.8103355640854,54.0280521063824));
#88128=CARTESIAN_POINT('Ctrl Pts',(9.89510093122654,31.8455613563589,54.0936631385629));
#88129=CARTESIAN_POINT('Ctrl Pts',(9.89916275782125,31.8772702128551,54.1612912793214));
#88130=CARTESIAN_POINT('Ctrl Pts',(9.90322458441596,31.9052388984376,54.2305441517669));
#88131=CARTESIAN_POINT('Ctrl Pts',(9.90727491714547,31.9331284402423,54.2996010574072));
#88132=CARTESIAN_POINT('Ctrl Pts',(9.91132524987497,31.9572987321473,54.3702731564436));
#88133=CARTESIAN_POINT('Ctrl Pts',(9.91537558260448,31.9775731898177,54.4421453223156));
#88134=CARTESIAN_POINT('Ctrl Pts',(9.9194189682171,31.9978128728074,54.5138942132937));
#88135=CARTESIAN_POINT('Ctrl Pts',(9.92346235382972,32.0141698957701,54.5868386811531));
#88136=CARTESIAN_POINT('Ctrl Pts',(9.92750573944234,32.0265162219192,54.660545194763));
#88137=CARTESIAN_POINT('Ctrl Pts',(9.93154060036725,32.0388365182544,54.7340963126055));
#88138=CARTESIAN_POINT('Ctrl Pts',(9.93557546129217,32.0471628851546,54.8084058693907));
#88139=CARTESIAN_POINT('Ctrl Pts',(9.93961032221709,32.0514178528905,54.8830283994199));
#88140=CARTESIAN_POINT('Ctrl Pts',(9.94171530832395,32.0536376686749,54.9219589578441));
#88141=CARTESIAN_POINT('Ctrl Pts',(9.94382029443082,32.0547502036409,54.9609744922976));
#88142=CARTESIAN_POINT('Ctrl Pts',(9.94592528053769,32.054749999972,55.0000107205177));
#88143=CARTESIAN_POINT('Origin',(-1.54592528053767,30.,55.));
#88144=CARTESIAN_POINT('',(8.79398090709402,28.7479524050421,56.6292250864936));
#88145=CARTESIAN_POINT('',(8.85202117008686,28.7479524050421,56.6292250864936));
#88146=CARTESIAN_POINT('',(-1.54592528053767,28.7479524050421,56.6292250864936));
#88147=CARTESIAN_POINT('',(9.30407471946233,32.0547491756286,55.0018405851164));
#88148=CARTESIAN_POINT('Ctrl Pts',(8.85202117008686,28.7479524050421,56.6292250864936));
#88149=CARTESIAN_POINT('Ctrl Pts',(8.85588129653178,28.6913884584482,56.5857561061291));
#88150=CARTESIAN_POINT('Ctrl Pts',(8.8597414229767,28.6371285515222,56.5393669217963));
#88151=CARTESIAN_POINT('Ctrl Pts',(8.86360154942161,28.5854753989256,56.4903414761239));
#88152=CARTESIAN_POINT('Ctrl Pts',(8.86746436612079,28.5337862474788,56.4412818629403));
#88153=CARTESIAN_POINT('Ctrl Pts',(8.87132718281997,28.4847077982068,56.3895826855296));
#88154=CARTESIAN_POINT('Ctrl Pts',(8.87518999951914,28.4385040565871,56.3355627956802));
#88155=CARTESIAN_POINT('Ctrl Pts',(8.87905908249684,28.3922253630511,56.2814552745238));
#88156=CARTESIAN_POINT('Ctrl Pts',(8.88292816547454,28.3488309715686,56.2250199175821));
#88157=CARTESIAN_POINT('Ctrl Pts',(8.88679724845224,28.3085423954682,56.1666056465539));
#88158=CARTESIAN_POINT('Ctrl Pts',(8.8874139295063,28.3021209251303,56.1572951783015));
#88159=CARTESIAN_POINT('Ctrl Pts',(8.88803061056035,28.2957782608037,56.1479344884688));
#88160=CARTESIAN_POINT('Ctrl Pts',(8.88864729161441,28.2895151905841,56.1385250455118));
#88161=CARTESIAN_POINT('Ctrl Pts',(8.89251644614069,28.2502196968614,56.0794887113036));
#88162=CARTESIAN_POINT('Ctrl Pts',(8.89638560066697,28.2139072368597,56.0182999790416));
#88163=CARTESIAN_POINT('Ctrl Pts',(8.90025475519325,28.1808206560891,55.9552926657251));
#88164=CARTESIAN_POINT('Ctrl Pts',(8.90411814428605,28.1477833776866,55.8923792397089));
#88165=CARTESIAN_POINT('Ctrl Pts',(8.90798153337886,28.1179626609685,55.8276530382313));
#88166=CARTESIAN_POINT('Ctrl Pts',(8.91184492247166,28.091557961512,55.7614765579004));
#88167=CARTESIAN_POINT('Ctrl Pts',(8.91570377857263,28.0651842432186,55.69537772376));
#88168=CARTESIAN_POINT('Ctrl Pts',(8.91956263467359,28.0422187599149,55.6278324397933));
#88169=CARTESIAN_POINT('Ctrl Pts',(8.92342149077455,28.0228141378531,55.5592259194872));
#88170=CARTESIAN_POINT('Ctrl Pts',(8.92727791525774,28.0034217434107,55.4906626308618));
#88171=CARTESIAN_POINT('Ctrl Pts',(8.93113433974092,27.9875858903567,55.4210398989647));
#88172=CARTESIAN_POINT('Ctrl Pts',(8.9349907642241,27.9754098448151,55.3507595558618));
#88173=CARTESIAN_POINT('Ctrl Pts',(8.938846048542,27.9632373991636,55.2804999913863));
#88174=CARTESIAN_POINT('Ctrl Pts',(8.94270133285991,27.9547226957614,55.2095836800666));
#88175=CARTESIAN_POINT('Ctrl Pts',(8.94655661717781,27.9499178580085,55.1384224461116));
#88176=CARTESIAN_POINT('Ctrl Pts',(8.95041205116911,27.9451128337178,55.0672584494697));
#88177=CARTESIAN_POINT('Ctrl Pts',(8.95426748516041,27.9440179915521,54.9958499961239));
#88178=CARTESIAN_POINT('Ctrl Pts',(8.95812291915171,27.9466334408295,54.924612095266));
#88179=CARTESIAN_POINT('Ctrl Pts',(8.96198238682083,27.9492516264732,54.8532996630475));
#88180=CARTESIAN_POINT('Ctrl Pts',(8.96584185448996,27.9555878347017,54.7821586259505));
#88181=CARTESIAN_POINT('Ctrl Pts',(8.96970132215909,27.965590094707,54.7116011446873));
#88182=CARTESIAN_POINT('Ctrl Pts',(8.97356297398307,27.975598015204,54.6410037334444));
#88183=CARTESIAN_POINT('Ctrl Pts',(8.97742462580706,27.9892760243878,54.5709910124351));
#88184=CARTESIAN_POINT('Ctrl Pts',(8.98128627763105,28.0065210865127,54.5019644751812));
#88185=CARTESIAN_POINT('Ctrl Pts',(8.98515468362329,28.0237963108729,54.4328172080253));
#88186=CARTESIAN_POINT('Ctrl Pts',(8.98902308961553,28.044650902163,54.3646600330377));
#88187=CARTESIAN_POINT('Ctrl Pts',(8.99289149560777,28.0689322965427,54.29787815362));
#88188=CARTESIAN_POINT('Ctrl Pts',(8.9951885178895,28.0833503550488,54.2582237157596));
#88189=CARTESIAN_POINT('Ctrl Pts',(8.99748554017123,28.0989757375881,54.2190538044965));
#88190=CARTESIAN_POINT('Ctrl Pts',(8.99978256245296,28.1157687985927,54.1804450340928));
#88191=CARTESIAN_POINT('Ctrl Pts',(9.00365176201357,28.1440557267504,54.1154108205942));
#88192=CARTESIAN_POINT('Ctrl Pts',(9.00752096157417,28.1757689648771,54.0517154981927));
#88193=CARTESIAN_POINT('Ctrl Pts',(9.01139016113478,28.2107597494939,53.9897441470257));
#88194=CARTESIAN_POINT('Ctrl Pts',(9.01525359714625,28.2456984119333,53.9278651082145));
#88195=CARTESIAN_POINT('Ctrl Pts',(9.01911703315772,28.2839046928784,53.8677053627107));
#88196=CARTESIAN_POINT('Ctrl Pts',(9.02298046916919,28.3251822016714,53.8096290893584));
#88197=CARTESIAN_POINT('Ctrl Pts',(9.02683937472661,28.3664113064385,53.7516209190849));
#88198=CARTESIAN_POINT('Ctrl Pts',(9.03069828028404,28.4107042052559,53.6956917619807));
#88199=CARTESIAN_POINT('Ctrl Pts',(9.03455718584146,28.4578200244877,53.6421787725812));
#88200=CARTESIAN_POINT('Ctrl Pts',(9.03841366131584,28.5049061732982,53.5886994821171));
#88201=CARTESIAN_POINT('Ctrl Pts',(9.04227013679021,28.5548113953747,53.537633704349));
#88202=CARTESIAN_POINT('Ctrl Pts',(9.04612661226458,28.6072540851992,53.4892861358597));
#88203=CARTESIAN_POINT('Ctrl Pts',(9.04998194901956,28.6596812900275,53.4409528431812));
#88204=CARTESIAN_POINT('Ctrl Pts',(9.05383728577453,28.7146441181887,53.3953364954274));
#88205=CARTESIAN_POINT('Ctrl Pts',(9.05769262252951,28.771824832693,53.3527042400011));
#88206=CARTESIAN_POINT('Ctrl Pts',(9.06154811031643,28.8290077872388,53.3100703144658));
#88207=CARTESIAN_POINT('Ctrl Pts',(9.06540359810335,28.8884084098854,53.2704210019285));
#88208=CARTESIAN_POINT('Ctrl Pts',(9.06925908589027,28.9496780785689,53.2339814769201));
#88209=CARTESIAN_POINT('Ctrl Pts',(9.07311860903011,29.0110118752564,53.1975038124202));
#88210=CARTESIAN_POINT('Ctrl Pts',(9.07697813216994,29.0742182047295,53.1642428906337));
#88211=CARTESIAN_POINT('Ctrl Pts',(9.08083765530977,29.1389225928098,53.1343785857451));
#88212=CARTESIAN_POINT('Ctrl Pts',(9.08469936363192,29.2036636151786,53.1044973723037));
#88213=CARTESIAN_POINT('Ctrl Pts',(9.08856107195407,29.2699039333472,53.0780167844557));
#88214=CARTESIAN_POINT('Ctrl Pts',(9.09242278027622,29.3372503405294,53.0550680085485));
#88215=CARTESIAN_POINT('Ctrl Pts',(9.0962912437545,29.4047145545103,53.0320790891216));
#88216=CARTESIAN_POINT('Ctrl Pts',(9.10015970723278,29.4732882530069,53.0126344489143));
#88217=CARTESIAN_POINT('Ctrl Pts',(9.10402817071106,29.5425650540414,52.996814828151));
#88218=CARTESIAN_POINT('Ctrl Pts',(9.10632472490455,29.5836919585141,52.9874233432352));
#88219=CARTESIAN_POINT('Ctrl Pts',(9.10862127909803,29.6250664825843,52.9793084509649));
#88220=CARTESIAN_POINT('Ctrl Pts',(9.11091783329152,29.6666028112324,52.972478390492));
#88221=CARTESIAN_POINT('Ctrl Pts',(9.11478631643122,29.7365696282645,52.9609733392037));
#88222=CARTESIAN_POINT('Ctrl Pts',(9.11865479957092,29.8072699698205,52.9530716445104));
#88223=CARTESIAN_POINT('Ctrl Pts',(9.12252328271062,29.8782997758385,52.9488572409657));
#88224=CARTESIAN_POINT('Ctrl Pts',(9.1263859997762,29.9492237100945,52.9446491190983));
#88225=CARTESIAN_POINT('Ctrl Pts',(9.13024871684178,30.0204756529167,52.9441174076207));
#88226=CARTESIAN_POINT('Ctrl Pts',(9.13411143390736,30.0916432604721,52.9472946935057));
#88227=CARTESIAN_POINT('Ctrl Pts',(9.1379696202359,30.1627273926627,52.9504682526236));
#88228=CARTESIAN_POINT('Ctrl Pts',(9.14182780656444,30.2337269029682,52.957342146198));
#88229=CARTESIAN_POINT('Ctrl Pts',(9.14568599289298,30.3042280154203,52.9678969324531));
#88230=CARTESIAN_POINT('Ctrl Pts',(9.14954174935052,30.3746847265414,52.9784450713442));
#88231=CARTESIAN_POINT('Ctrl Pts',(9.15339750580807,30.4446431830962,52.9926694318933));
#88232=CARTESIAN_POINT('Ctrl Pts',(9.15725326226561,30.5136947794281,53.0104987468995));
#88233=CARTESIAN_POINT('Ctrl Pts',(9.16110788126701,30.5827260053959,53.0283228022209));
#88234=CARTESIAN_POINT('Ctrl Pts',(9.16496250026841,30.6508504319847,53.0497495793187));
#88235=CARTESIAN_POINT('Ctrl Pts',(9.1688171192698,30.7176713991228,53.0746570888849));
#88236=CARTESIAN_POINT('Ctrl Pts',(9.17267189161837,30.7844950245797,53.0995655893392));
#88237=CARTESIAN_POINT('Ctrl Pts',(9.17652666396692,30.8500146330596,53.1279549253845));
#88238=CARTESIAN_POINT('Ctrl Pts',(9.18038143631549,30.9138520748046,53.1596543944478));
#88239=CARTESIAN_POINT('Ctrl Pts',(9.18424025245614,30.9777564842764,53.1913871173716));
#88240=CARTESIAN_POINT('Ctrl Pts',(9.18809906859679,31.0399747682461,53.2264366885038));
#88241=CARTESIAN_POINT('Ctrl Pts',(9.19195788473744,31.1001528137344,53.2645861159561));
#88242=CARTESIAN_POINT('Ctrl Pts',(9.19581888975065,31.1603649945814,53.3027571832669));
#88243=CARTESIAN_POINT('Ctrl Pts',(9.19967989476387,31.2185342366537,53.3440313258441));
#88244=CARTESIAN_POINT('Ctrl Pts',(9.20354089977709,31.2743371748439,53.3881494091229));
#88245=CARTESIAN_POINT('Ctrl Pts',(9.20740867340654,31.3302379395512,53.4323448345376));
#88246=CARTESIAN_POINT('Ctrl Pts',(9.21127644703598,31.3837637531121,53.4793938336401));
#88247=CARTESIAN_POINT('Ctrl Pts',(9.21514422066542,31.4346264894879,53.5289988449496));
#88248=CARTESIAN_POINT('Ctrl Pts',(9.21744718182031,31.4649113296381,53.5585348067401));
#88249=CARTESIAN_POINT('Ctrl Pts',(9.2197501429752,31.4942527651073,53.5889762636244));
#88250=CARTESIAN_POINT('Ctrl Pts',(9.22205310413008,31.5225968865233,53.6202549932508));
#88251=CARTESIAN_POINT('Ctrl Pts',(9.2258818694665,31.5697201258097,53.6722571364507));
#88252=CARTESIAN_POINT('Ctrl Pts',(9.22971063480291,31.6142781779404,53.7267889663082));
#88253=CARTESIAN_POINT('Ctrl Pts',(9.23353940013933,31.6559837342967,53.7835644553677));
#88254=CARTESIAN_POINT('Ctrl Pts',(9.23736291548182,31.6976321040933,53.8402620940116));
#88255=CARTESIAN_POINT('Ctrl Pts',(9.24118643082432,31.7364354404661,53.8991968972038));
#88256=CARTESIAN_POINT('Ctrl Pts',(9.24500994616681,31.7721446014219,53.9600475615918));
#88257=CARTESIAN_POINT('Ctrl Pts',(9.24882956237847,31.8078173470169,54.0208361719064));
#88258=CARTESIAN_POINT('Ctrl Pts',(9.25264917859012,31.8404019248255,54.0835363428967));
#88259=CARTESIAN_POINT('Ctrl Pts',(9.25646879480177,31.8696918061671,54.1477969065701));
#88260=CARTESIAN_POINT('Ctrl Pts',(9.26043595519015,31.900113097365,54.2145397279986));
#88261=CARTESIAN_POINT('Ctrl Pts',(9.26440311557854,31.9269796377569,54.2829654981407));
#88262=CARTESIAN_POINT('Ctrl Pts',(9.26837027596692,31.9501125700655,54.3526527001891));
#88263=CARTESIAN_POINT('Ctrl Pts',(9.27218707210809,31.9723687125265,54.4196986014959));
#88264=CARTESIAN_POINT('Ctrl Pts',(9.27600386824927,31.991169053742,54.4879115124635));
#88265=CARTESIAN_POINT('Ctrl Pts',(9.27982066439045,32.0064043053609,54.5568980637264));
#88266=CARTESIAN_POINT('Ctrl Pts',(9.28363748065307,32.0216396372972,54.6258849786738));
#88267=CARTESIAN_POINT('Ctrl Pts',(9.2874542969157,32.0333097454008,54.6956450548262));
#88268=CARTESIAN_POINT('Ctrl Pts',(9.29127111317833,32.0413564087979,54.7657745215404));
#88269=CARTESIAN_POINT('Ctrl Pts',(9.29509049992236,32.0494084913186,54.8359512177981));
#88270=CARTESIAN_POINT('Ctrl Pts',(9.29890988666638,32.0538322209711,54.9064973060252));
#88271=CARTESIAN_POINT('Ctrl Pts',(9.30272927341042,32.0546213278406,54.9770051814002));
#88272=CARTESIAN_POINT('Ctrl Pts',(9.30317775542772,32.054713986758,54.9852843938245));
#88273=CARTESIAN_POINT('Ctrl Pts',(9.30362623744502,32.0547565903784,54.9935630809628));
#88274=CARTESIAN_POINT('Ctrl Pts',(9.30407471946233,32.0547491756286,55.0018405851164));
#88275=CARTESIAN_POINT('Ctrl Pts',(9.3040750081896,32.0541656181102,55.0018453898296));
#88276=CARTESIAN_POINT('Ctrl Pts',(9.31377946378262,32.0557552315022,55.1809084352921));
#88277=CARTESIAN_POINT('Ctrl Pts',(9.36052900965515,31.9523257255288,56.0417158650899));
#88278=CARTESIAN_POINT('Ctrl Pts',(9.44318606595545,30.7618299889055,57.2943384729));
#88279=CARTESIAN_POINT('Ctrl Pts',(9.51613866666276,29.2698275908187,57.0320534795199));
#88280=CARTESIAN_POINT('Ctrl Pts',(9.55204617709054,28.7459570691003,56.6318367151304));
#88281=CARTESIAN_POINT('',(9.24592528058114,32.0547492110797,54.998199425793));
#88282=CARTESIAN_POINT('Ctrl Pts',(9.24592528058114,32.0547492110797,54.998199425793));
#88283=CARTESIAN_POINT('Ctrl Pts',(9.2497310207861,32.0548106172635,55.0682739094095));
#88284=CARTESIAN_POINT('Ctrl Pts',(9.25353676099106,32.0512831032295,55.1384663101287));
#88285=CARTESIAN_POINT('Ctrl Pts',(9.25734250119601,32.0441571007588,55.2083730066908));
#88286=CARTESIAN_POINT('Ctrl Pts',(9.26114492485008,32.0370373083152,55.2782187823534));
#88287=CARTESIAN_POINT('Ctrl Pts',(9.26494734850415,32.0263252921618,55.3477788510323));
#88288=CARTESIAN_POINT('Ctrl Pts',(9.26874977215822,32.0120635168845,55.4166508928618));
#88289=CARTESIAN_POINT('Ctrl Pts',(9.27255024081877,31.9978090742142,55.4854875245403));
#88290=CARTESIAN_POINT('Ctrl Pts',(9.27635070947932,31.9800085923165,55.5536363407389));
#88291=CARTESIAN_POINT('Ctrl Pts',(9.28015117813986,31.9587559546279,55.6207033693399));
#88292=CARTESIAN_POINT('Ctrl Pts',(9.2839510505265,31.9375066513683,55.6877598754703));
#88293=CARTESIAN_POINT('Ctrl Pts',(9.28775092291313,31.9128064196875,55.753734453472));
#88294=CARTESIAN_POINT('Ctrl Pts',(9.29155079529976,31.8847989711826,55.8182483734961));
#88295=CARTESIAN_POINT('Ctrl Pts',(9.29535403990283,31.8567666673224,55.8828195467328));
#88296=CARTESIAN_POINT('Ctrl Pts',(9.29915728450591,31.825421483627,55.9459270116931));
#88297=CARTESIAN_POINT('Ctrl Pts',(9.30296052910898,31.7909548332783,56.0072131589972));
#88298=CARTESIAN_POINT('Ctrl Pts',(9.30676541564393,31.7564733030316,56.068525764678));
#88299=CARTESIAN_POINT('Ctrl Pts',(9.31057030217887,31.7188678920193,56.1280150634692));
#88300=CARTESIAN_POINT('Ctrl Pts',(9.31437518871381,31.6783739012035,56.1853516821007));
#88301=CARTESIAN_POINT('Ctrl Pts',(9.31818690566785,31.6378072167803,56.2427912297239));
#88302=CARTESIAN_POINT('Ctrl Pts',(9.32199862262189,31.5943419074146,56.2980699853191));
#88303=CARTESIAN_POINT('Ctrl Pts',(9.32581033957593,31.5482537046868,56.3508915679742));
#88304=CARTESIAN_POINT('Ctrl Pts',(9.32899447653029,31.5097536924258,56.3950163430684));
#88305=CARTESIAN_POINT('Ctrl Pts',(9.33217861348464,31.4694241869326,56.4374269880513));
#88306=CARTESIAN_POINT('Ctrl Pts',(9.335362750439,31.427444051006,56.4779719360487));
#88307=CARTESIAN_POINT('Ctrl Pts',(9.33923123464619,31.3764413789553,56.5272309639291));
#88308=CARTESIAN_POINT('Ctrl Pts',(9.34309971885338,31.3227858472138,56.5739435066278));
#88309=CARTESIAN_POINT('Ctrl Pts',(9.34696820306057,31.2667620480004,56.6178107047012));
#88310=CARTESIAN_POINT('Ctrl Pts',(9.35083092119519,31.2108217536625,56.6616125176175));
#88311=CARTESIAN_POINT('Ctrl Pts',(9.3546936393298,31.1525205781485,56.7025771070642));
#88312=CARTESIAN_POINT('Ctrl Pts',(9.35855635746442,31.0921791328281,56.7404431344675));
#88313=CARTESIAN_POINT('Ctrl Pts',(9.36241454485926,31.0319084644519,56.7782647472616));
#88314=CARTESIAN_POINT('Ctrl Pts',(9.3662727322541,30.9696026893691,56.8129947600966));
#88315=CARTESIAN_POINT('Ctrl Pts',(9.37013091964894,30.90561319018,56.844413812644));
#88316=CARTESIAN_POINT('Ctrl Pts',(9.37398667717055,30.8416639913588,56.8758130775795));
#88317=CARTESIAN_POINT('Ctrl Pts',(9.37784243469217,30.7760336074036,56.9039053055744));
#88318=CARTESIAN_POINT('Ctrl Pts',(9.38169819221378,30.709098646093,56.9285167027042));
#88319=CARTESIAN_POINT('Ctrl Pts',(9.38555281227549,30.6421834307945,56.9531208393988));
#88320=CARTESIAN_POINT('Ctrl Pts',(9.38940743233721,30.5739648580217,56.9742460161874));
#88321=CARTESIAN_POINT('Ctrl Pts',(9.39326205239892,30.5048385606257,56.9917669517806));
#88322=CARTESIAN_POINT('Ctrl Pts',(9.39711682580255,30.4357095132936,57.0092885843799));
#88323=CARTESIAN_POINT('Ctrl Pts',(9.40097159920618,30.3656731412421,57.0232055738624));
#88324=CARTESIAN_POINT('Ctrl Pts',(9.40482637260981,30.2951375604076,57.0334432332713));
#88325=CARTESIAN_POINT('Ctrl Pts',(9.40868518979036,30.2245279855601,57.0436916323025));
#88326=CARTESIAN_POINT('Ctrl Pts',(9.4125440069709,30.1534186384365,57.05025292645));
#88327=CARTESIAN_POINT('Ctrl Pts',(9.41640282415145,30.082224193917,57.0531041728161));
#88328=CARTESIAN_POINT('Ctrl Pts',(9.42026383019759,30.0109893652428,57.0559570365159));
#88329=CARTESIAN_POINT('Ctrl Pts',(9.42412483624374,29.939669829223,57.0550956690197));
#88330=CARTESIAN_POINT('Ctrl Pts',(9.42798584228988,29.8686789413621,57.0505492781346));
#88331=CARTESIAN_POINT('Ctrl Pts',(9.43185361693012,29.797563601869,57.0459949171313));
#88332=CARTESIAN_POINT('Ctrl Pts',(9.43572139157036,29.7267785436418,57.0377426913391));
#88333=CARTESIAN_POINT('Ctrl Pts',(9.4395891662106,29.6567299953908,57.0258734576561));
#88334=CARTESIAN_POINT('Ctrl Pts',(9.44189211789959,29.615021665017,57.0188062745083));
#88335=CARTESIAN_POINT('Ctrl Pts',(9.44419506958858,29.5735742331112,57.0104577492287));
#88336=CARTESIAN_POINT('Ctrl Pts',(9.44649802127757,29.5324708422954,57.0008533302559));
#88337=CARTESIAN_POINT('Ctrl Pts',(9.45045224773995,29.4618952777124,56.9843622992717));
#88338=CARTESIAN_POINT('Ctrl Pts',(9.45440647420234,29.3920522645419,56.9640996457197));
#88339=CARTESIAN_POINT('Ctrl Pts',(9.45836070066472,29.3233744778301,56.9401483101166));
#88340=CARTESIAN_POINT('Ctrl Pts',(9.46222412370766,29.2562737828537,56.91674698428));
#88341=CARTESIAN_POINT('Ctrl Pts',(9.4660875467506,29.1902858677679,56.8898247211004));
#88342=CARTESIAN_POINT('Ctrl Pts',(9.46995096979354,29.1258038704839,56.8595103359861));
#88343=CARTESIAN_POINT('Ctrl Pts',(9.47395059796565,29.0590485578855,56.8281272160492));
#88344=CARTESIAN_POINT('Ctrl Pts',(9.47795022613776,28.9939078532244,56.7931084315634));
#88345=CARTESIAN_POINT('Ctrl Pts',(9.48194985430987,28.9307982082082,56.7546524131375));
#88346=CARTESIAN_POINT('Ctrl Pts',(9.48594948248198,28.867688563192,56.7161963947116));
#88347=CARTESIAN_POINT('Ctrl Pts',(9.48994911065408,28.8066104976308,56.6743034027799));
#88348=CARTESIAN_POINT('Ctrl Pts',(9.49394873882619,28.7479524050421,56.6292250864936));
#88349=CARTESIAN_POINT('Ctrl Pts',(8.79398090709402,28.7479524050421,56.6292250864936));
#88350=CARTESIAN_POINT('Ctrl Pts',(8.7980159387603,28.6890642014229,56.5839699315589));
#88351=CARTESIAN_POINT('Ctrl Pts',(8.80205097042658,28.632543821309,56.5354495734022));
#88352=CARTESIAN_POINT('Ctrl Pts',(8.80608600209286,28.5787688567674,56.4839473036486));
#88353=CARTESIAN_POINT('Ctrl Pts',(8.80994398458318,28.5273534308732,56.4347048512085));
#88354=CARTESIAN_POINT('Ctrl Pts',(8.8138019670735,28.4784479420345,56.3827370556703));
#88355=CARTESIAN_POINT('Ctrl Pts',(8.81765994956382,28.4323493299988,56.328333143208));
#88356=CARTESIAN_POINT('Ctrl Pts',(8.82151585847565,28.3862754949263,56.2739584716203));
#88357=CARTESIAN_POINT('Ctrl Pts',(8.82537176738749,28.3430058566912,56.2171506511486));
#88358=CARTESIAN_POINT('Ctrl Pts',(8.82922767629933,28.3027990407137,56.1582342018338));
#88359=CARTESIAN_POINT('Ctrl Pts',(8.83308280260811,28.2626003851927,56.0993297103205));
#88360=CARTESIAN_POINT('Ctrl Pts',(8.8369379289169,28.2254635909987,56.0383178411421));
#88361=CARTESIAN_POINT('Ctrl Pts',(8.84079305522569,28.1916046465441,55.9755530780533));
#88362=CARTESIAN_POINT('Ctrl Pts',(8.84464868865254,28.1577412481544,55.9127800586474));
#88363=CARTESIAN_POINT('Ctrl Pts',(8.84850432207939,28.1271567838051,55.8482541163248));
#88364=CARTESIAN_POINT('Ctrl Pts',(8.85235995550625,28.1000210416728,55.7823538332582));
#88365=CARTESIAN_POINT('Ctrl Pts',(8.85621984300843,28.0728553595856,55.7163808397606));
#88366=CARTESIAN_POINT('Ctrl Pts',(8.8600797305106,28.0491461764957,55.6490309301374));
#88367=CARTESIAN_POINT('Ctrl Pts',(8.86393961801278,28.0290145576689,55.5807012559129));
#88368=CARTESIAN_POINT('Ctrl Pts',(8.86780201100793,28.0088698711997,55.512327228189));
#88369=CARTESIAN_POINT('Ctrl Pts',(8.87166440400307,27.9923074822234,55.4429726426712));
#88370=CARTESIAN_POINT('Ctrl Pts',(8.87552679699821,27.9793974979391,55.3730456958136));
#88371=CARTESIAN_POINT('Ctrl Pts',(8.87939562802961,27.9664659946257,55.3030021911072));
#88372=CARTESIAN_POINT('Ctrl Pts',(8.88326445906101,27.9571991048352,55.2323849024254));
#88373=CARTESIAN_POINT('Ctrl Pts',(8.8871332900924,27.9516150981964,55.161607105546));
#88374=CARTESIAN_POINT('Ctrl Pts',(8.88836274908986,27.9498405809977,55.1391149371139));
#88375=CARTESIAN_POINT('Ctrl Pts',(8.88959220808731,27.948437594808,55.1166065523314));
#88376=CARTESIAN_POINT('Ctrl Pts',(8.89082166708476,27.9474056259948,55.0940951555716));
#88377=CARTESIAN_POINT('Ctrl Pts',(8.89469076157756,27.9441580310279,55.0232520274891));
#88378=CARTESIAN_POINT('Ctrl Pts',(8.89855985607037,27.9445759946267,54.9521018198761));
#88379=CARTESIAN_POINT('Ctrl Pts',(8.90242895056317,27.948695578934,54.8810557499698));
#88380=CARTESIAN_POINT('Ctrl Pts',(8.90629228027677,27.9528090252435,54.8101155355569));
#88381=CARTESIAN_POINT('Ctrl Pts',(8.91015560999037,27.960613116748,54.7392796318758));
#88382=CARTESIAN_POINT('Ctrl Pts',(8.91401893970397,27.9720919511485,54.6689614706666));
#88383=CARTESIAN_POINT('Ctrl Pts',(8.91787773766708,27.9835573206839,54.5987257938387));
#88384=CARTESIAN_POINT('Ctrl Pts',(8.9217365356302,27.9986887930481,54.5290071302452));
#88385=CARTESIAN_POINT('Ctrl Pts',(8.92559533359331,28.0174186272033,54.4602142436673));
#88386=CARTESIAN_POINT('Ctrl Pts',(8.92945170073389,28.0361366626317,54.3914646926827));
#88387=CARTESIAN_POINT('Ctrl Pts',(8.93330806787446,28.0584484353156,54.3236402292901));
#88388=CARTESIAN_POINT('Ctrl Pts',(8.93716443501504,28.0842353397634,54.2571384186213));
#88389=CARTESIAN_POINT('Ctrl Pts',(8.94101966286253,28.1100146259423,54.1906562546951));
#88390=CARTESIAN_POINT('Ctrl Pts',(8.94487489071002,28.1392668301418,54.1254964204129));
#88391=CARTESIAN_POINT('Ctrl Pts',(8.94873011855751,28.1718243701289,54.0620386847821));
#88392=CARTESIAN_POINT('Ctrl Pts',(8.95258549702839,28.204383182136,53.9985784698635));
#88393=CARTESIAN_POINT('Ctrl Pts',(8.95644087549927,28.2402473626092,53.9368209168332));
#88394=CARTESIAN_POINT('Ctrl Pts',(8.96029625397015,28.2792031143695,53.8771217158995));
#88395=CARTESIAN_POINT('Ctrl Pts',(8.96415566793503,28.318199641816,53.8173600267382));
#88396=CARTESIAN_POINT('Ctrl Pts',(8.9680150818999,28.3602939343272,53.7596613982291));
#88397=CARTESIAN_POINT('Ctrl Pts',(8.97187449586478,28.4052290328142,53.7043522374035));
#88398=CARTESIAN_POINT('Ctrl Pts',(8.97573609492737,28.4501895723608,53.6490117619997));
#88399=CARTESIAN_POINT('Ctrl Pts',(8.97959769398996,28.4979937939993,53.5960638081306));
#88400=CARTESIAN_POINT('Ctrl Pts',(8.98345929305254,28.5483464768113,53.5457993222688));
#88401=CARTESIAN_POINT('Ctrl Pts',(8.98732764833382,28.5987872562203,53.4954468941186));
#88402=CARTESIAN_POINT('Ctrl Pts',(8.99119600361509,28.6517850375334,53.4477876325501));
#88403=CARTESIAN_POINT('Ctrl Pts',(8.99506435889637,28.7070105530286,53.4030729971221));
#88404=CARTESIAN_POINT('Ctrl Pts',(8.99736188523869,28.7398105590757,53.3765157020153));
#88405=CARTESIAN_POINT('Ctrl Pts',(8.999659411581,28.773395808489,53.3509963215848));
#88406=CARTESIAN_POINT('Ctrl Pts',(9.00195693792332,28.8076927897776,53.3265601059639));
#88407=CARTESIAN_POINT('Ctrl Pts',(9.00582593492974,28.8654483486545,53.2854099161514));
#88408=CARTESIAN_POINT('Ctrl Pts',(9.00969493193617,28.9254498910936,53.2471725992289));
#88409=CARTESIAN_POINT('Ctrl Pts',(9.0135639289426,28.9873715156788,53.2121014807206));
#88410=CARTESIAN_POINT('Ctrl Pts',(9.01742716090311,29.0492008731963,53.1770826203578));
#88411=CARTESIAN_POINT('Ctrl Pts',(9.02129039286362,29.1129442145097,53.1452208311218));
#88412=CARTESIAN_POINT('Ctrl Pts',(9.02515362482413,29.1782455927105,53.1167269829894));
#88413=CARTESIAN_POINT('Ctrl Pts',(9.02901232510842,29.2434703706178,53.0882665589162));
#88414=CARTESIAN_POINT('Ctrl Pts',(9.03287102539272,29.310249112044,53.063166421903));
#88415=CARTESIAN_POINT('Ctrl Pts',(9.03672972567701,29.3782016751627,53.0415913588504));
#88416=CARTESIAN_POINT('Ctrl Pts',(9.04058599523718,29.4461114326933,53.0200298866502));
#88417=CARTESIAN_POINT('Ctrl Pts',(9.04444226479734,29.5151930829683,53.0019892295235));
#88418=CARTESIAN_POINT('Ctrl Pts',(9.0482985343575,29.5850483046845,52.9875853675113));
#88419=CARTESIAN_POINT('Ctrl Pts',(9.05215366486527,29.6548828927918,52.9731857600651));
#88420=CARTESIAN_POINT('Ctrl Pts',(9.05600879537304,29.7254901231765,52.962420913157));
#88421=CARTESIAN_POINT('Ctrl Pts',(9.0598639258808,29.7964600620339,52.9553560074789));
#88422=CARTESIAN_POINT('Ctrl Pts',(9.06371920739509,29.8674327808034,52.9482908250664));
#88423=CARTESIAN_POINT('Ctrl Pts',(9.06757448890938,29.9387677526166,52.9449259175499));
#88424=CARTESIAN_POINT('Ctrl Pts',(9.07142977042368,30.0100502077706,52.9452745789708));
#88425=CARTESIAN_POINT('Ctrl Pts',(9.07528908868052,30.0814073005145,52.9456236054639));
#88426=CARTESIAN_POINT('Ctrl Pts',(9.07914840693737,30.1527112800329,52.9496939605497));
#88427=CARTESIAN_POINT('Ctrl Pts',(9.08300772519421,30.223548569157,52.9574467939053));
#88428=CARTESIAN_POINT('Ctrl Pts',(9.08686922910844,30.2944259757404,52.9652040179423));
#88429=CARTESIAN_POINT('Ctrl Pts',(9.09073073302266,30.3648356860456,52.9766477938668));
#88430=CARTESIAN_POINT('Ctrl Pts',(9.09459223693689,30.4343731635707,52.9916878934614));
#88431=CARTESIAN_POINT('Ctrl Pts',(9.098460498985,30.504032340722,53.0067543151856));
#88432=CARTESIAN_POINT('Ctrl Pts',(9.10232876103311,30.5728157683698,53.0254294994618));
#88433=CARTESIAN_POINT('Ctrl Pts',(9.10619702308123,30.6403336194645,53.0475731977143));
#88434=CARTESIAN_POINT('Ctrl Pts',(9.10849541830811,30.6804505259085,53.0607302614644));
#88435=CARTESIAN_POINT('Ctrl Pts',(9.11079381353499,30.7201209950869,53.0751108971256));
#88436=CARTESIAN_POINT('Ctrl Pts',(9.11309220876187,30.7592670510234,53.0906778407691));
#88437=CARTESIAN_POINT('Ctrl Pts',(9.11696136318876,30.8251661330657,53.1168834768612));
#88438=CARTESIAN_POINT('Ctrl Pts',(9.12083051761564,30.8898359757849,53.1465561400865));
#88439=CARTESIAN_POINT('Ctrl Pts',(9.12469967204252,30.9528869714854,53.1795593989165));
#88440=CARTESIAN_POINT('Ctrl Pts',(9.12856306103708,31.0158440148106,53.2125134795451));
#88441=CARTESIAN_POINT('Ctrl Pts',(9.13242645003163,31.0771865724978,53.2487880810627));
#88442=CARTESIAN_POINT('Ctrl Pts',(9.13628983902619,31.1365444117604,53.2881985037405));
#88443=CARTESIAN_POINT('Ctrl Pts',(9.14014869503105,31.195832605312,53.3275626854004));
#88444=CARTESIAN_POINT('Ctrl Pts',(9.14400755103591,31.2531403033267,53.3700551124467));
#88445=CARTESIAN_POINT('Ctrl Pts',(9.14786640704078,31.3081228683027,53.4154457649158));
#88446=CARTESIAN_POINT('Ctrl Pts',(9.15172283142924,31.3630707866097,53.4608078149557));
#88447=CARTESIAN_POINT('Ctrl Pts',(9.15557925581769,31.4156961050115,53.5090641585697));
#88448=CARTESIAN_POINT('Ctrl Pts',(9.15943568020615,31.4656853314769,53.5599430318236));
#88449=CARTESIAN_POINT('Ctrl Pts',(9.16329096443082,31.5156597784731,53.6108068625815));
#88450=CARTESIAN_POINT('Ctrl Pts',(9.1671462486555,31.5629993405386,53.6642913373607));
#88451=CARTESIAN_POINT('Ctrl Pts',(9.17100153288017,31.6074269063078,53.7200873844759));
#88452=CARTESIAN_POINT('Ctrl Pts',(9.17485696677985,31.6518561969035,53.77588559778));
#88453=CARTESIAN_POINT('Ctrl Pts',(9.17871240067954,31.693372965888,53.8339951802086));
#88454=CARTESIAN_POINT('Ctrl Pts',(9.18256783457922,31.7317410710717,53.8940748554882));
#88455=CARTESIAN_POINT('Ctrl Pts',(9.1864273021598,31.7701493182205,53.9542173880868));
#88456=CARTESIAN_POINT('Ctrl Pts',(9.19028676974038,31.8054020635424,54.0163337178684));
#88457=CARTESIAN_POINT('Ctrl Pts',(9.19414623732096,31.8373076201051,54.0800552888333));
#88458=CARTESIAN_POINT('Ctrl Pts',(9.198007889058,31.8692312327147,54.1438129212179));
#88459=CARTESIAN_POINT('Ctrl Pts',(9.20186954079504,31.8978036910347,54.2091771579076));
#88460=CARTESIAN_POINT('Ctrl Pts',(9.20573119253207,31.9228813756042,54.27575917137));
#88461=CARTESIAN_POINT('Ctrl Pts',(9.2095995984408,31.9480029219713,54.3424576392361));
#88462=CARTESIAN_POINT('Ctrl Pts',(9.21346800434952,31.9696173434629,54.4103776733197));
#88463=CARTESIAN_POINT('Ctrl Pts',(9.21733641025824,31.987631022315,54.4791156734637));
#88464=CARTESIAN_POINT('Ctrl Pts',(9.21963343337231,31.9983273757145,54.5199316526734));
#88465=CARTESIAN_POINT('Ctrl Pts',(9.22193045648637,32.0077551304157,54.5610358282184));
#88466=CARTESIAN_POINT('Ctrl Pts',(9.22422747960044,32.015903316979,54.6023426360634));
#88467=CARTESIAN_POINT('Ctrl Pts',(9.22983463068173,32.0357934577526,54.7031746698618));
#88468=CARTESIAN_POINT('Ctrl Pts',(9.23544178176301,32.0481232837319,54.8055436168192));
#88469=CARTESIAN_POINT('Ctrl Pts',(9.2410489328443,32.0527124830813,54.9085176284622));
#88470=CARTESIAN_POINT('Ctrl Pts',(9.24267438207543,32.0540428397002,54.9383686215289));
#88471=CARTESIAN_POINT('Ctrl Pts',(9.24429983130656,32.0547229842024,54.9682702891664));
#88472=CARTESIAN_POINT('Ctrl Pts',(9.24592528053769,32.054749211079,54.998199424993));
#88473=CARTESIAN_POINT('Origin',(-1.54592528053767,30.,55.));
#88474=CARTESIAN_POINT('',(8.09385946234359,28.7479524050421,56.6292250864936));
#88475=CARTESIAN_POINT('',(8.1521140472482,28.7479524050421,56.6292250864936));
#88476=CARTESIAN_POINT('',(-1.54592528053767,28.7479524050421,56.6292250864936));
#88477=CARTESIAN_POINT('',(8.60407471942946,32.0547498911142,54.9993310707398));
#88478=CARTESIAN_POINT('Ctrl Pts',(8.1521140472482,28.7479524050421,56.6292250864936));
#88479=CARTESIAN_POINT('Ctrl Pts',(8.15596957998729,28.6914289717662,56.5857872403185));
#88480=CARTESIAN_POINT('Ctrl Pts',(8.15982511272638,28.6371409837604,56.5393831604098));
#88481=CARTESIAN_POINT('Ctrl Pts',(8.16368064546547,28.5854080864135,56.4902775850545));
#88482=CARTESIAN_POINT('Ctrl Pts',(8.16753577929291,28.5336805415967,56.441177090394));
#88483=CARTESIAN_POINT('Ctrl Pts',(8.17139091312036,28.4845079139827,56.3893759905912));
#88484=CARTESIAN_POINT('Ctrl Pts',(8.17524604694781,28.4381741799003,56.33517701829));
#88485=CARTESIAN_POINT('Ctrl Pts',(8.17912851525075,28.3915119206939,56.2805937531091));
#88486=CARTESIAN_POINT('Ctrl Pts',(8.18301098355368,28.347729313344,56.2235788417456));
#88487=CARTESIAN_POINT('Ctrl Pts',(8.18689345185662,28.3070748871319,56.1644750425494));
#88488=CARTESIAN_POINT('Ctrl Pts',(8.19075397014214,28.2666503057745,56.1057053940328));
#88489=CARTESIAN_POINT('Ctrl Pts',(8.19461448842766,28.2293188353886,56.0448708633677));
#88490=CARTESIAN_POINT('Ctrl Pts',(8.19847500671318,28.1952798414538,55.9823353357366));
#88491=CARTESIAN_POINT('Ctrl Pts',(8.20236845002482,28.1609505407047,55.919266464205));
#88492=CARTESIAN_POINT('Ctrl Pts',(8.20626189333647,28.1299703652479,55.8544678955933));
#88493=CARTESIAN_POINT('Ctrl Pts',(8.21015533664811,28.1024944009687,55.7883337263779));
#88494=CARTESIAN_POINT('Ctrl Pts',(8.21404877995976,28.0750184366895,55.7221995571625));
#88495=CARTESIAN_POINT('Ctrl Pts',(8.2179422232714,28.0510467901622,55.6547302798665));
#88496=CARTESIAN_POINT('Ctrl Pts',(8.22183566658305,28.0306827583382,55.5863336628522));
#88497=CARTESIAN_POINT('Ctrl Pts',(8.22570474058982,28.0104461862614,55.5183651445359));
#88498=CARTESIAN_POINT('Ctrl Pts',(8.22957381459659,27.9936928793508,55.4492146040001));
#88499=CARTESIAN_POINT('Ctrl Pts',(8.23344288860335,27.9805570088349,55.3792724191582));
#88500=CARTESIAN_POINT('Ctrl Pts',(8.23730619764755,27.9674407109097,55.3094344489365));
#88501=CARTESIAN_POINT('Ctrl Pts',(8.24116950669174,27.9579312392786,55.2388076493481));
#88502=CARTESIAN_POINT('Ctrl Pts',(8.24503281573593,27.9521128687209,55.167797079955));
#88503=CARTESIAN_POINT('Ctrl Pts',(8.2488915928593,27.9463013235024,55.0968698107262));
#88504=CARTESIAN_POINT('Ctrl Pts',(8.25275036998267,27.9441723181709,55.0255601477312));
#88505=CARTESIAN_POINT('Ctrl Pts',(8.25660914710603,27.9457586931575,54.9542811224769));
#88506=CARTESIAN_POINT('Ctrl Pts',(8.26046549331331,27.9473440687745,54.8830470009119));
#88507=CARTESIAN_POINT('Ctrl Pts',(8.26432183952059,27.9526401702527,54.8118439633125));
#88508=CARTESIAN_POINT('Ctrl Pts',(8.26817818572786,27.9616277741692,54.7410864401745));
#88509=CARTESIAN_POINT('Ctrl Pts',(8.27203339258008,27.9706127227037,54.6703498223022));
#88510=CARTESIAN_POINT('Ctrl Pts',(8.27588859943229,27.983286947251,54.6000589392268));
#88511=CARTESIAN_POINT('Ctrl Pts',(8.27974380628451,27.9995794014052,54.5306227623565));
#88512=CARTESIAN_POINT('Ctrl Pts',(8.28359916372963,28.0158724919788,54.4611838731557));
#88513=CARTESIAN_POINT('Ctrl Pts',(8.28745452117475,28.0357839796486,54.392600228883));
#88514=CARTESIAN_POINT('Ctrl Pts',(8.29130987861986,28.0591921601236,54.325268578489));
#88515=CARTESIAN_POINT('Ctrl Pts',(8.29516927165858,28.0826248431004,54.2578664487216));
#88516=CARTESIAN_POINT('Ctrl Pts',(8.29902866469729,28.1095613655399,54.191719388721));
#88517=CARTESIAN_POINT('Ctrl Pts',(8.30288805773601,28.139831073066,54.1272061378716));
#88518=CARTESIAN_POINT('Ctrl Pts',(8.30674963589709,28.170117918783,54.0626563607222));
#88519=CARTESIAN_POINT('Ctrl Pts',(8.31061121405816,28.2037414773222,53.9997426628237));
#88520=CARTESIAN_POINT('Ctrl Pts',(8.31447279221924,28.2404854099351,53.9388185971057));
#88521=CARTESIAN_POINT('Ctrl Pts',(8.31834112686611,28.2772936322886,53.8777879344039));
#88522=CARTESIAN_POINT('Ctrl Pts',(8.32220946151299,28.3172328567141,53.8187542566786));
#88523=CARTESIAN_POINT('Ctrl Pts',(8.32607779615985,28.3600441796943,53.7620410063555));
#88524=CARTESIAN_POINT('Ctrl Pts',(8.32837550991377,28.3854732530849,53.7283544649385));
#88525=CARTESIAN_POINT('Ctrl Pts',(8.33067322366769,28.4119148693543,53.6954859602599));
#88526=CARTESIAN_POINT('Ctrl Pts',(8.3329709374216,28.4393085840758,53.6634971504855));
#88527=CARTESIAN_POINT('Ctrl Pts',(8.33684001407724,28.485436341269,53.6096317997955));
#88528=CARTESIAN_POINT('Ctrl Pts',(8.34070909073287,28.5344463679899,53.5580518102964));
#88529=CARTESIAN_POINT('Ctrl Pts',(8.3445781673885,28.5860834597022,53.5090816321568));
#88530=CARTESIAN_POINT('Ctrl Pts',(8.34844147911268,28.6376436120513,53.4601844196741));
#88531=CARTESIAN_POINT('Ctrl Pts',(8.35230479083687,28.691822709941,53.4138896312969));
#88532=CARTESIAN_POINT('Ctrl Pts',(8.35616810256105,28.7483261521441,53.3704877597595));
#88533=CARTESIAN_POINT('Ctrl Pts',(8.36002688239727,28.8047633125435,53.3271368011262));
#88534=CARTESIAN_POINT('Ctrl Pts',(8.36388566223349,28.8635190179454,53.286672313062));
#88535=CARTESIAN_POINT('Ctrl Pts',(8.36774444206971,28.9242640734426,53.2493458997239));
#88536=CARTESIAN_POINT('Ctrl Pts',(8.37160079100859,28.9849708616635,53.2120430007304));
#88537=CARTESIAN_POINT('Ctrl Pts',(8.37545713994746,29.0476641006963,53.1778745080932));
#88538=CARTESIAN_POINT('Ctrl Pts',(8.37931348888634,29.1119851827573,53.1470490435909));
#88539=CARTESIAN_POINT('Ctrl Pts',(8.38316869848472,29.1762872614515,53.1162326863298));
#88540=CARTESIAN_POINT('Ctrl Pts',(8.3870239080831,29.2422157905404,53.0887576062114));
#88541=CARTESIAN_POINT('Ctrl Pts',(8.39087911768149,29.3093886417666,53.064785925439));
#88542=CARTESIAN_POINT('Ctrl Pts',(8.39473447788319,29.3765641170926,53.0408133082155));
#88543=CARTESIAN_POINT('Ctrl Pts',(8.3985898380849,29.4449835527988,53.0203445232556));
#88544=CARTESIAN_POINT('Ctrl Pts',(8.40244519828661,29.514247614255,53.003492503835));
#88545=CARTESIAN_POINT('Ctrl Pts',(8.40630459407851,29.5835841777222,52.9866228445984));
#88546=CARTESIAN_POINT('Ctrl Pts',(8.41016398987041,29.6537666588396,52.9733776233692));
#88547=CARTESIAN_POINT('Ctrl Pts',(8.41402338566231,29.7243843048492,52.963818880579));
#88548=CARTESIAN_POINT('Ctrl Pts',(8.41788496657881,29.7950419333751,52.9542547257903));
#88549=CARTESIAN_POINT('Ctrl Pts',(8.42174654749532,29.8661347329007,52.9483812444725));
#88550=CARTESIAN_POINT('Ctrl Pts',(8.42560812841182,29.9372483333486,52.9462084353975));
#88551=CARTESIAN_POINT('Ctrl Pts',(8.42947646578746,30.0084863585194,52.9440318246423));
#88552=CARTESIAN_POINT('Ctrl Pts',(8.4333448031631,30.079744771449,52.945568803024));
#88553=CARTESIAN_POINT('Ctrl Pts',(8.43721314053875,30.1506114136066,52.9507772779438));
#88554=CARTESIAN_POINT('Ctrl Pts',(8.43951082977922,30.1927043091796,52.9538709731468));
#88555=CARTESIAN_POINT('Ctrl Pts',(8.44180851901969,30.2346591058783,52.958258995766));
#88556=CARTESIAN_POINT('Ctrl Pts',(8.44410620826017,30.2763912218767,52.9639240056006));
#88557=CARTESIAN_POINT('Ctrl Pts',(8.44797527190787,30.3466636547658,52.9734632780265));
#88558=CARTESIAN_POINT('Ctrl Pts',(8.45184433555557,30.4165793040417,52.9866635449544));
#88559=CARTESIAN_POINT('Ctrl Pts',(8.45571339920327,30.4857271733883,53.0034863698106));
#88560=CARTESIAN_POINT('Ctrl Pts',(8.45957669789329,30.5547720114652,53.0202841284279));
#88561=CARTESIAN_POINT('Ctrl Pts',(8.46343999658332,30.6230508722509,53.040693616869));
#88562=CARTESIAN_POINT('Ctrl Pts',(8.46730329527334,30.6901599209877,53.0646248823646));
#88563=CARTESIAN_POINT('Ctrl Pts',(8.471162062099,30.7571902470757,53.088528075154));
#88564=CARTESIAN_POINT('Ctrl Pts',(8.47502082892466,30.8230530315313,53.1159446765813));
#88565=CARTESIAN_POINT('Ctrl Pts',(8.47887959575032,30.887358349047,53.1467345784058));
#88566=CARTESIAN_POINT('Ctrl Pts',(8.48273593170018,30.9516231566673,53.1775050837675));
#88567=CARTESIAN_POINT('Ctrl Pts',(8.48659226765004,31.0143320068052,53.2116444641662));
#88568=CARTESIAN_POINT('Ctrl Pts',(8.4904486035999,31.0751151329243,53.2489645881773));
#88569=CARTESIAN_POINT('Ctrl Pts',(8.49430380024967,31.1358803015259,53.286273686484));
#88570=CARTESIAN_POINT('Ctrl Pts',(8.49815899689945,31.1947204618297,53.3267614087846));
#88571=CARTESIAN_POINT('Ctrl Pts',(8.50201419354923,31.2512921568985,53.3701946433441));
#88572=CARTESIAN_POINT('Ctrl Pts',(8.50586954086163,31.3078660628118,53.4136295752918));
#88573=CARTESIAN_POINT('Ctrl Pts',(8.50972488817404,31.362170943501,53.4600099504573));
#88574=CARTESIAN_POINT('Ctrl Pts',(8.51358023548644,31.4138953356547,53.5090615229615));
#88575=CARTESIAN_POINT('Ctrl Pts',(8.51743961856765,31.4656738727846,53.5581644425403));
#88576=CARTESIAN_POINT('Ctrl Pts',(8.52129900164886,31.5148661758648,53.6099438063461));
#88577=CARTESIAN_POINT('Ctrl Pts',(8.52515838473007,31.5611973460965,53.6640881731786));
#88578=CARTESIAN_POINT('Ctrl Pts',(8.52901995301741,31.6075547493181,53.7182631968803));
#88579=CARTESIAN_POINT('Ctrl Pts',(8.53288152130476,31.6510474984651,53.7748055040666));
#88580=CARTESIAN_POINT('Ctrl Pts',(8.5367430895921,31.6914424553517,53.8333723890059));
#88581=CARTESIAN_POINT('Ctrl Pts',(8.54061141460413,31.7319080927448,53.8920417505266));
#88582=CARTESIAN_POINT('Ctrl Pts',(8.54447973961616,31.7692648613614,53.9527423486073));
#88583=CARTESIAN_POINT('Ctrl Pts',(8.54834806462818,31.8033245867531,54.0151050831121));
#88584=CARTESIAN_POINT('Ctrl Pts',(8.5506458694517,31.8235562376743,54.0521488660691));
#88585=CARTESIAN_POINT('Ctrl Pts',(8.55294367427521,31.8426254516933,54.0897786828393));
#88586=CARTESIAN_POINT('Ctrl Pts',(8.55524147909873,31.8605009184363,54.1279140552688));
#88587=CARTESIAN_POINT('Ctrl Pts',(8.5594321115992,31.8931013861208,54.1974636225275));
#88588=CARTESIAN_POINT('Ctrl Pts',(8.56362274409967,31.9218405243209,54.2689335422176));
#88589=CARTESIAN_POINT('Ctrl Pts',(8.56781337660014,31.9465079265243,54.3418932803274));
#88590=CARTESIAN_POINT('Ctrl Pts',(8.57199339313536,31.9711128397633,54.414668192389));
#88591=CARTESIAN_POINT('Ctrl Pts',(8.57617340967057,31.9916664358248,54.4889250781403));
#88592=CARTESIAN_POINT('Ctrl Pts',(8.58035342620579,32.0080057339108,54.5642127410291));
#88593=CARTESIAN_POINT('Ctrl Pts',(8.5845163948271,32.0242783932778,54.6391933482917));
#88594=CARTESIAN_POINT('Ctrl Pts',(8.58867936344842,32.0363709182544,54.7151960144015));
#88595=CARTESIAN_POINT('Ctrl Pts',(8.59284233206974,32.0441702493645,54.7917560226244));
#88596=CARTESIAN_POINT('Ctrl Pts',(8.59658646118964,32.0511848837231,54.860613269047));
#88597=CARTESIAN_POINT('Ctrl Pts',(8.60033059030956,32.0547272944609,54.92992093489));
#88598=CARTESIAN_POINT('Ctrl Pts',(8.60407471942946,32.0547498911142,54.9993310707398));
#88599=CARTESIAN_POINT('Ctrl Pts',(8.60407471946233,32.0547498911144,54.9993310713492));
#88600=CARTESIAN_POINT('Ctrl Pts',(8.60802536615502,32.0547737341254,55.0725697110582));
#88601=CARTESIAN_POINT('Ctrl Pts',(8.61197601284772,32.0508775057908,55.1457764205272));
#88602=CARTESIAN_POINT('Ctrl Pts',(8.61592665954042,32.0430975996036,55.2185171869532));
#88603=CARTESIAN_POINT('Ctrl Pts',(8.61988032369122,32.0353117512143,55.2913135119326));
#88604=CARTESIAN_POINT('Ctrl Pts',(8.62383398784202,32.0236363737173,55.3636427378917));
#88605=CARTESIAN_POINT('Ctrl Pts',(8.62778765199282,32.0081593529454,55.435078815478));
#88606=CARTESIAN_POINT('Ctrl Pts',(8.63174855413826,31.9926539983069,55.5066456714832));
#88607=CARTESIAN_POINT('Ctrl Pts',(8.6357094562837,31.9733332044954,55.5773156739349));
#88608=CARTESIAN_POINT('Ctrl Pts',(8.63967035842913,31.9503352789342,55.6466760102591));
#88609=CARTESIAN_POINT('Ctrl Pts',(8.64363545516164,31.927312998618,55.7161097990342));
#88610=CARTESIAN_POINT('Ctrl Pts',(8.64760055189415,31.9006059955549,55.784230740216));
#88611=CARTESIAN_POINT('Ctrl Pts',(8.65156564862666,31.870400467028,55.850646610198));
#88612=CARTESIAN_POINT('Ctrl Pts',(8.65553891540463,31.8401327002866,55.917199329471));
#88613=CARTESIAN_POINT('Ctrl Pts',(8.6595121821826,31.8063522248623,55.9820395644455));
#88614=CARTESIAN_POINT('Ctrl Pts',(8.66348544896057,31.7692906356216,56.0448005595335));
#88615=CARTESIAN_POINT('Ctrl Pts',(8.66444921595281,31.7603008701752,56.0600240466151));
#88616=CARTESIAN_POINT('Ctrl Pts',(8.66541298294505,31.7511182482559,56.0751253411417));
#88617=CARTESIAN_POINT('Ctrl Pts',(8.66637674993729,31.7417464389131,56.0900994931811));
#88618=CARTESIAN_POINT('Ctrl Pts',(8.67024584450429,31.704122804878,56.1502140341101));
#88619=CARTESIAN_POINT('Ctrl Pts',(8.67411493907129,31.6633096439208,56.2084962168561));
#88620=CARTESIAN_POINT('Ctrl Pts',(8.6779840336383,31.6195111909914,56.2645873100556));
#88621=CARTESIAN_POINT('Ctrl Pts',(8.68184736342655,31.5757779958081,56.320594830022));
#88622=CARTESIAN_POINT('Ctrl Pts',(8.6857106932148,31.5290686342519,56.3744173608726));
#88623=CARTESIAN_POINT('Ctrl Pts',(8.68957402300305,31.479631340782,56.4257239066088));
#88624=CARTESIAN_POINT('Ctrl Pts',(8.69343282104112,31.4302520380805,56.4769702689124));
#88625=CARTESIAN_POINT('Ctrl Pts',(8.69729161907919,31.3781514950012,56.5257061602548));
#88626=CARTESIAN_POINT('Ctrl Pts',(8.70115041711727,31.3236179274611,56.5716339092179));
#88627=CARTESIAN_POINT('Ctrl Pts',(8.70500678433295,31.2691187129541,56.6175327263221));
#88628=CARTESIAN_POINT('Ctrl Pts',(8.70886315154863,31.2121898854573,56.6606265984677));
#88629=CARTESIAN_POINT('Ctrl Pts',(8.71271951876431,31.1531551264326,56.7006559960445));
#88630=CARTESIAN_POINT('Ctrl Pts',(8.71657474668694,31.0941378081461,56.7406735676691));
#88631=CARTESIAN_POINT('Ctrl Pts',(8.72042997460958,31.0330161953365,56.7776281896037));
#88632=CARTESIAN_POINT('Ctrl Pts',(8.72428520253221,30.9701441298328,56.8113028266557));
#88633=CARTESIAN_POINT('Ctrl Pts',(8.72814058107816,30.9072696079246,56.8449787793719));
#88634=CARTESIAN_POINT('Ctrl Pts',(8.73199595962412,30.8426449268075,56.8753742653652));
#88635=CARTESIAN_POINT('Ctrl Pts',(8.73585133817007,30.7766482436334,56.902318340384));
#88636=CARTESIAN_POINT('Ctrl Pts',(8.73971075220939,30.7105824805558,56.9292906182458));
#88637=CARTESIAN_POINT('Ctrl Pts',(8.74357016624872,30.6431422993087,56.9528040894751));
#88638=CARTESIAN_POINT('Ctrl Pts',(8.74742958028804,30.5747247011059,56.9727364447484));
#88639=CARTESIAN_POINT('Ctrl Pts',(8.75129117942483,30.5062683666808,56.9926800851906));
#88640=CARTESIAN_POINT('Ctrl Pts',(8.75515277856163,30.4368339867346,57.0090384620328));
#88641=CARTESIAN_POINT('Ctrl Pts',(8.75901437769842,30.3668298626838,57.0217401945709));
#88642=CARTESIAN_POINT('Ctrl Pts',(8.76288273305271,30.2967032600766,57.0344641499406));
#88643=CARTESIAN_POINT('Ctrl Pts',(8.766751088407,30.2260054051838,57.043518626219));
#88644=CARTESIAN_POINT('Ctrl Pts',(8.77061944376129,30.15515014269,57.0488840854776));
#88645=CARTESIAN_POINT('Ctrl Pts',(8.77291696943281,30.1130671979675,57.0520707835074));
#88646=CARTESIAN_POINT('Ctrl Pts',(8.77521449510433,30.0709287566252,57.0539571768937));
#88647=CARTESIAN_POINT('Ctrl Pts',(8.77751202077585,30.0288210183556,57.0545478605769));
#88648=CARTESIAN_POINT('Ctrl Pts',(8.78138026090062,29.9579261227046,57.0555423679953));
#88649=CARTESIAN_POINT('Ctrl Pts',(8.78524850102539,29.8868408233463,57.0528650337751));
#88650=CARTESIAN_POINT('Ctrl Pts',(8.78911674115016,29.8159770152335,57.0464928789462));
#88651=CARTESIAN_POINT('Ctrl Pts',(8.79297960130612,29.7452117648795,57.040129586544));
#88652=CARTESIAN_POINT('Ctrl Pts',(8.79684246146208,29.6746678741339,57.0300817116751));
#88653=CARTESIAN_POINT('Ctrl Pts',(8.80070532161804,29.6047579252208,57.0163782544017));
#88654=CARTESIAN_POINT('Ctrl Pts',(8.80456410221453,29.5349218080752,57.0026892693242));
#88655=CARTESIAN_POINT('Ctrl Pts',(8.80842288281104,29.465718778231,56.9853524574742));
#88656=CARTESIAN_POINT('Ctrl Pts',(8.81228166340753,29.3975552529139,56.9644484949238));
#88657=CARTESIAN_POINT('Ctrl Pts',(8.81613799763461,29.3294349415502,56.9435577849576));
#88658=CARTESIAN_POINT('Ctrl Pts',(8.81999433186168,29.2623532905634,56.9191045533825));
#88659=CARTESIAN_POINT('Ctrl Pts',(8.82385066608875,29.1967039048842,56.8912199623713));
#88660=CARTESIAN_POINT('Ctrl Pts',(8.82770557291724,29.1310788189245,56.8633456926713));
#88661=CARTESIAN_POINT('Ctrl Pts',(8.83156047974573,29.0668853908702,56.8320427790204));
#88662=CARTESIAN_POINT('Ctrl Pts',(8.83541538657421,29.0044978000164,56.7974907321952));
#88663=CARTESIAN_POINT('Ctrl Pts',(8.83927123820595,28.9420949185209,56.7629302169718));
#88664=CARTESIAN_POINT('Ctrl Pts',(8.84312708983769,28.8814991834627,56.7251192134167));
#88665=CARTESIAN_POINT('Ctrl Pts',(8.84698294146943,28.8230594593807,56.6842827928666));
#88666=CARTESIAN_POINT('Ctrl Pts',(8.84866235100857,28.7976061381791,56.6664965602088));
#88667=CARTESIAN_POINT('Ctrl Pts',(8.85034176054771,28.7725614516204,56.648136959284));
#88668=CARTESIAN_POINT('Ctrl Pts',(8.85202117008686,28.7479524050421,56.6292250864936));
#88669=CARTESIAN_POINT('',(8.54592528048675,32.0547496520916,55.001195712928));
#88670=CARTESIAN_POINT('Ctrl Pts',(8.54592528053768,32.0547496520911,55.001195713863));
#88671=CARTESIAN_POINT('Ctrl Pts',(8.54975547188148,32.0547087341851,55.0715102394462));
#88672=CARTESIAN_POINT('Ctrl Pts',(8.55358566322528,32.0510587897108,55.141718266117));
#88673=CARTESIAN_POINT('Ctrl Pts',(8.55741585456908,32.0438307944968,55.2115496300313));
#88674=CARTESIAN_POINT('Ctrl Pts',(8.56128493121179,32.0365294184178,55.2820899437643));
#88675=CARTESIAN_POINT('Ctrl Pts',(8.56515400785449,32.0255575352495,55.3523899848868));
#88676=CARTESIAN_POINT('Ctrl Pts',(8.5690230844972,32.0109405032667,55.422037740992));
#88677=CARTESIAN_POINT('Ctrl Pts',(8.57288639620839,31.9963452506891,55.4915817218089));
#88678=CARTESIAN_POINT('Ctrl Pts',(8.57674970791958,31.9781157291987,55.5604748752605));
#88679=CARTESIAN_POINT('Ctrl Pts',(8.58061301963077,31.9563290148064,55.6283107100206));
#88680=CARTESIAN_POINT('Ctrl Pts',(8.58447179945396,31.9345678574898,55.6960669694243));
#88681=CARTESIAN_POINT('Ctrl Pts',(8.58833057927715,31.9092579436745,55.7627679135125));
#88682=CARTESIAN_POINT('Ctrl Pts',(8.59218935910033,31.880526921484,55.8280193597217));
#88683=CARTESIAN_POINT('Ctrl Pts',(8.59604570802616,31.8518139988403,55.8932296997845));
#88684=CARTESIAN_POINT('Ctrl Pts',(8.59990205695198,31.8196844389608,55.9569919100661));
#88685=CARTESIAN_POINT('Ctrl Pts',(8.60375840587781,31.7843145294576,56.0189304306313));
#88686=CARTESIAN_POINT('Ctrl Pts',(8.60761361546314,31.7489550698309,56.0808506517465));
#88687=CARTESIAN_POINT('Ctrl Pts',(8.61146882504848,31.710357401943,56.140947831195));
#88688=CARTESIAN_POINT('Ctrl Pts',(8.61532403463381,31.6687436070267,56.1988712760374));
#88689=CARTESIAN_POINT('Ctrl Pts',(8.61917939482249,31.6271281864722,56.2567969836527));
#88690=CARTESIAN_POINT('Ctrl Pts',(8.62303475501116,31.5824966901905,56.3125483948307));
#88691=CARTESIAN_POINT('Ctrl Pts',(8.62689011519983,31.5351133294593,56.3658054869623));
#88692=CARTESIAN_POINT('Ctrl Pts',(8.63074951097883,31.487680370293,56.4191183258452));
#88693=CARTESIAN_POINT('Ctrl Pts',(8.63460890675783,31.4374901201012,56.4699312700161));
#88694=CARTESIAN_POINT('Ctrl Pts',(8.63846830253683,31.3848451286348,56.5179596609253));
#88695=CARTESIAN_POINT('Ctrl Pts',(8.64232988344048,31.3321703304641,56.5660152446976));
#88696=CARTESIAN_POINT('Ctrl Pts',(8.64619146434413,31.2770383999112,56.6112828283351));
#88697=CARTESIAN_POINT('Ctrl Pts',(8.65005304524778,31.2197844625913,56.6535184992375));
#88698=CARTESIAN_POINT('Ctrl Pts',(8.65392138261079,31.1624303502627,56.6958280682665));
#88699=CARTESIAN_POINT('Ctrl Pts',(8.6577897199738,31.1029472240117,56.7350948656177));
#88700=CARTESIAN_POINT('Ctrl Pts',(8.66165805733681,31.0416980194437,56.7711190809167));
#88701=CARTESIAN_POINT('Ctrl Pts',(8.66395574669375,31.0053176233586,56.7925165052665));
#88702=CARTESIAN_POINT('Ctrl Pts',(8.6662534360507,30.9683146132999,56.8127708167859));
#88703=CARTESIAN_POINT('Ctrl Pts',(8.66855112540764,30.9307684193872,56.831848168373));
#88704=CARTESIAN_POINT('Ctrl Pts',(8.67242018908383,30.8675446356291,56.8639723925812));
#88705=CARTESIAN_POINT('Ctrl Pts',(8.67628925276001,30.8025319705833,56.8928825727001));
#88706=CARTESIAN_POINT('Ctrl Pts',(8.6801583164362,30.7360903244563,56.9183765523853));
#88707=CARTESIAN_POINT('Ctrl Pts',(8.68402161515472,30.6697476772885,56.9438325456929));
#88708=CARTESIAN_POINT('Ctrl Pts',(8.68788491387324,30.6019807252953,56.9658822698298));
#88709=CARTESIAN_POINT('Ctrl Pts',(8.69174821259176,30.5331727802138,56.9843700131122));
#88710=CARTESIAN_POINT('Ctrl Pts',(8.69560697944579,30.4644455506829,57.0028360692425));
#88711=CARTESIAN_POINT('Ctrl Pts',(8.69946574629982,30.3946802205381,57.0177483187944));
#88712=CARTESIAN_POINT('Ctrl Pts',(8.70332451315385,30.3242771890504,57.0290002136919));
#88713=CARTESIAN_POINT('Ctrl Pts',(8.707180849132,30.2539185087863,57.0402450203249));
#88714=CARTESIAN_POINT('Ctrl Pts',(8.71103718511014,30.1829234027668,57.0478339706537));
#88715=CARTESIAN_POINT('Ctrl Pts',(8.71489352108828,30.1117030050094,57.0517114809768));
#88716=CARTESIAN_POINT('Ctrl Pts',(8.71874871776621,30.0405036483167,57.055587845744));
#88717=CARTESIAN_POINT('Ctrl Pts',(8.72260391444415,29.9690796168307,57.055754920952));
#88718=CARTESIAN_POINT('Ctrl Pts',(8.72645911112208,29.8978459896077,57.0522090830763));
#88719=CARTESIAN_POINT('Ctrl Pts',(8.73031445846246,29.8266095785493,57.048663106628));
#88720=CARTESIAN_POINT('Ctrl Pts',(8.73416980580284,29.7555640716055,57.0414039553665));
#88721=CARTESIAN_POINT('Ctrl Pts',(8.73802515314322,29.6851216301961,57.0304800355408));
#88722=CARTESIAN_POINT('Ctrl Pts',(8.74188453625196,29.6146054498077,57.0195446805819));
#88723=CARTESIAN_POINT('Ctrl Pts',(8.74574391936071,29.5446940761796,57.0049369735972));
#88724=CARTESIAN_POINT('Ctrl Pts',(8.74960330246945,29.4757907532576,56.9867567108556));
#88725=CARTESIAN_POINT('Ctrl Pts',(8.75346487078411,29.4068484168599,56.9685661543399));
#88726=CARTESIAN_POINT('Ctrl Pts',(8.75732643909878,29.3389157302231,56.9467991635959));
#88727=CARTESIAN_POINT('Ctrl Pts',(8.76118800741344,29.2723793727463,56.921605002412));
#88728=CARTESIAN_POINT('Ctrl Pts',(8.76505633245216,29.2057265942276,56.8963667581042));
#88729=CARTESIAN_POINT('Ctrl Pts',(8.76892465749088,29.1404754676766,56.8676895664043));
#88730=CARTESIAN_POINT('Ctrl Pts',(8.7727929825296,29.0769907033567,56.8357699749179));
#88731=CARTESIAN_POINT('Ctrl Pts',(8.7750907871018,29.0392804333409,56.8168095766768));
#88732=CARTESIAN_POINT('Ctrl Pts',(8.777388591674,29.0021929199974,56.7967059949121));
#88733=CARTESIAN_POINT('Ctrl Pts',(8.77968639624619,28.965799690604,56.7755076126407));
#88734=CARTESIAN_POINT('Ctrl Pts',(8.7835554038458,28.9045213369959,56.7398141062826));
#88735=CARTESIAN_POINT('Ctrl Pts',(8.78742441144541,28.8449729706854,56.7008746005939));
#88736=CARTESIAN_POINT('Ctrl Pts',(8.79129341904501,28.787519610286,56.6588818122636));
#88737=CARTESIAN_POINT('Ctrl Pts',(8.79218924839468,28.7742168691676,56.649158809325));
#88738=CARTESIAN_POINT('Ctrl Pts',(8.79308507774435,28.7610263498124,56.6392723176847));
#88739=CARTESIAN_POINT('Ctrl Pts',(8.79398090709402,28.7479524050421,56.6292250864936));
#88740=CARTESIAN_POINT('Ctrl Pts',(8.09385946234359,28.7479524050421,56.6292250864936));
#88741=CARTESIAN_POINT('Ctrl Pts',(8.09772772740314,28.6914355148067,56.5857922685974));
#88742=CARTESIAN_POINT('Ctrl Pts',(8.10159599246268,28.6372539723095,56.5394711345916));
#88743=CARTESIAN_POINT('Ctrl Pts',(8.10546425752223,28.5857004584289,56.4905550540694));
#88744=CARTESIAN_POINT('Ctrl Pts',(8.1079344287531,28.5527797549927,56.4593185454608));
#88745=CARTESIAN_POINT('Ctrl Pts',(8.11040459998397,28.5209299459321,56.4270246259437));
#88746=CARTESIAN_POINT('Ctrl Pts',(8.11287477121484,28.4902185814113,56.3937566611802));
#88747=CARTESIAN_POINT('Ctrl Pts',(8.11674384460076,28.4421148217901,56.3416484528659));
#88748=CARTESIAN_POINT('Ctrl Pts',(8.12061291798667,28.3966176804652,56.2869448935148));
#88749=CARTESIAN_POINT('Ctrl Pts',(8.12448199137259,28.3540195501558,56.2299373647591));
#88750=CARTESIAN_POINT('Ctrl Pts',(8.12834529980468,28.3114848914401,56.1730147777293));
#88751=CARTESIAN_POINT('Ctrl Pts',(8.13220860823678,28.271840957964,56.1137954215481));
#88752=CARTESIAN_POINT('Ctrl Pts',(8.13607191666887,28.23534181248,56.0526058349252));
#88753=CARTESIAN_POINT('Ctrl Pts',(8.13993069319587,28.1988854828017,55.9914880275569));
#88754=CARTESIAN_POINT('Ctrl Pts',(8.14378946972286,28.1655668610939,55.9284049957587));
#88755=CARTESIAN_POINT('Ctrl Pts',(8.14764824624986,28.135597344255,55.8637130887922));
#88756=CARTESIAN_POINT('Ctrl Pts',(8.15150459187077,28.1056467072554,55.7990619356629));
#88757=CARTESIAN_POINT('Ctrl Pts',(8.15536093749167,28.0790411929748,55.7328043579541));
#88758=CARTESIAN_POINT('Ctrl Pts',(8.15921728311258,28.0559460723379,55.6653208916317));
#88759=CARTESIAN_POINT('Ctrl Pts',(8.16307248938919,28.0328577750764,55.5978573630716));
#88760=CARTESIAN_POINT('Ctrl Pts',(8.16692769566581,28.0132779696707,55.5291691242994));
#88761=CARTESIAN_POINT('Ctrl Pts',(8.17078290194242,27.9973229967891,55.4596546348186));
#88762=CARTESIAN_POINT('Ctrl Pts',(8.17463825882349,27.9813674006231,55.3901374297395));
#88763=CARTESIAN_POINT('Ctrl Pts',(8.17849361570457,27.9690370246441,55.3197943838363));
#88764=CARTESIAN_POINT('Ctrl Pts',(8.18234897258564,27.9603973464495,55.2490352949481));
#88765=CARTESIAN_POINT('Ctrl Pts',(8.18620836508162,27.9517486246267,55.1782021386148));
#88766=CARTESIAN_POINT('Ctrl Pts',(8.1900677575776,27.9467983715154,55.1069525531432));
#88767=CARTESIAN_POINT('Ctrl Pts',(8.19392715007359,27.945560186038,55.0357017269566));
#88768=CARTESIAN_POINT('Ctrl Pts',(8.19778872770313,27.9443212995174,54.9644105595578));
#88769=CARTESIAN_POINT('Ctrl Pts',(8.20165030533268,27.9467986476289,54.8931186357687));
#88770=CARTESIAN_POINT('Ctrl Pts',(8.20551188296223,27.9529537215789,54.8222386529578));
#88771=CARTESIAN_POINT('Ctrl Pts',(8.20938021710087,27.9591195649131,54.7512346531531));
#88772=CARTESIAN_POINT('Ctrl Pts',(8.21324855123952,27.9689759142079,54.6806445146228));
#88773=CARTESIAN_POINT('Ctrl Pts',(8.21711688537817,27.9824327849669,54.6108726489648));
#88774=CARTESIAN_POINT('Ctrl Pts',(8.21941460426991,27.9904259171676,54.5694294519481));
#88775=CARTESIAN_POINT('Ctrl Pts',(8.22171232316166,27.9996883921494,54.5282747183294));
#88776=CARTESIAN_POINT('Ctrl Pts',(8.2240100420534,28.0101930999981,54.487490426231));
#88777=CARTESIAN_POINT('Ctrl Pts',(8.22787911588953,28.0278817260697,54.418814733112));
#88778=CARTESIAN_POINT('Ctrl Pts',(8.23174818972565,28.0491645565733,54.350921348827));
#88779=CARTESIAN_POINT('Ctrl Pts',(8.23561726356177,28.0739553723287,54.2842139602376));
#88780=CARTESIAN_POINT('Ctrl Pts',(8.23948057244793,28.0987092495767,54.2176059661738));
#88781=CARTESIAN_POINT('Ctrl Pts',(8.24334388133408,28.1269605689286,54.152180911724));
#88782=CARTESIAN_POINT('Ctrl Pts',(8.24720719022022,28.1585727854168,54.0883293490013));
#88783=CARTESIAN_POINT('Ctrl Pts',(8.25106596720477,28.1901479188089,54.024552688133));
#88784=CARTESIAN_POINT('Ctrl Pts',(8.25492474418931,28.2250759036248,53.9623462858401));
#88785=CARTESIAN_POINT('Ctrl Pts',(8.25878352117385,28.2631720093297,53.902081016958));
#88786=CARTESIAN_POINT('Ctrl Pts',(8.2626398672542,28.301244115725,53.8418537132383));
#88787=CARTESIAN_POINT('Ctrl Pts',(8.26649621333455,28.3424801243909,53.7835655264644));
#88788=CARTESIAN_POINT('Ctrl Pts',(8.2703525594149,28.3866499674206,53.7275616970258));
#88789=CARTESIAN_POINT('Ctrl Pts',(8.27420776615216,28.4308067606346,53.67157441371));
#88790=CARTESIAN_POINT('Ctrl Pts',(8.27806297288942,28.4778953667262,53.6178705290785));
#88791=CARTESIAN_POINT('Ctrl Pts',(8.28191817962669,28.5276441214334,53.56676389616));
#88792=CARTESIAN_POINT('Ctrl Pts',(8.28577353696892,28.5773948195928,53.5156552667433));
#88793=CARTESIAN_POINT('Ctrl Pts',(8.28962889431116,28.6298055322612,53.4671444370395));
#88794=CARTESIAN_POINT('Ctrl Pts',(8.29348425165339,28.6845674830464,53.4215086772994));
#88795=CARTESIAN_POINT('Ctrl Pts',(8.29734364460812,28.7393867561478,53.3758251481242));
#88796=CARTESIAN_POINT('Ctrl Pts',(8.30120303756285,28.7965618064593,53.3330230081686));
#88797=CARTESIAN_POINT('Ctrl Pts',(8.30506243051757,28.8557511915957,53.2933388658069));
#88798=CARTESIAN_POINT('Ctrl Pts',(8.3089240086052,28.9149740889123,53.2536322548534));
#88799=CARTESIAN_POINT('Ctrl Pts',(8.31278558669282,28.9762131741812,53.2170474050503));
#88800=CARTESIAN_POINT('Ctrl Pts',(8.31664716478044,29.039100836507,53.1837757957514));
#88801=CARTESIAN_POINT('Ctrl Pts',(8.3205154993711,29.1020985317447,53.1504459719806));
#88802=CARTESIAN_POINT('Ctrl Pts',(8.32438383396176,29.1667501221892,53.120441167342));
#88803=CARTESIAN_POINT('Ctrl Pts',(8.32825216855243,29.2326670396085,53.0939051203057));
#88804=CARTESIAN_POINT('Ctrl Pts',(8.33054988333227,29.271820394068,53.0781432294855));
#88805=CARTESIAN_POINT('Ctrl Pts',(8.33284759811211,29.3114198421419,53.0636042166553));
#88806=CARTESIAN_POINT('Ctrl Pts',(8.33514531289195,29.3513818074579,53.050309767475));
#88807=CARTESIAN_POINT('Ctrl Pts',(8.33901438504249,29.4186728952993,53.0279235324507));
#88808=CARTESIAN_POINT('Ctrl Pts',(8.34288345719303,29.4872560984358,53.0089812381622));
#88809=CARTESIAN_POINT('Ctrl Pts',(8.34675252934356,29.5567455001129,52.9936293934495));
#88810=CARTESIAN_POINT('Ctrl Pts',(8.35061583654187,29.6261313619579,52.9783004231232));
#88811=CARTESIAN_POINT('Ctrl Pts',(8.35447914374019,29.6964202716635,52.966551387107));
#88812=CARTESIAN_POINT('Ctrl Pts',(8.3583424509385,29.767210052625,52.9584793895478));
#88813=CARTESIAN_POINT('Ctrl Pts',(8.36220122623995,29.8379167928212,52.950416860938));
#88814=CARTESIAN_POINT('Ctrl Pts',(8.3660600015414,29.9091227568787,52.9460228576987));
#88815=CARTESIAN_POINT('Ctrl Pts',(8.36991877684285,29.9804161657888,52.9453433289385));
#88816=CARTESIAN_POINT('Ctrl Pts',(8.37377512124393,30.0516646622176,52.9446642282588));
#88817=CARTESIAN_POINT('Ctrl Pts',(8.37763146564502,30.1230000095906,52.9476949641638));
#88818=CARTESIAN_POINT('Ctrl Pts',(8.3814878100461,30.194007376137,52.9544294926587));
#88819=CARTESIAN_POINT('Ctrl Pts',(8.38534301511035,30.2649937639273,52.9611620314723));
#88820=CARTESIAN_POINT('Ctrl Pts',(8.3891982201746,30.3356518799121,52.9715961446121));
#88821=CARTESIAN_POINT('Ctrl Pts',(8.39305342523885,30.405570701832,52.9856738177953));
#88822=CARTESIAN_POINT('Ctrl Pts',(8.39690878091677,30.4754922553135,52.9997520409595));
#88823=CARTESIAN_POINT('Ctrl Pts',(8.40076413659469,30.5446739815933,53.0174740087301));
#88824=CARTESIAN_POINT('Ctrl Pts',(8.40461949227261,30.6127154649093,53.0387306861216));
#88825=CARTESIAN_POINT('Ctrl Pts',(8.40847888358764,30.6808281714167,53.0600096141804));
#88826=CARTESIAN_POINT('Ctrl Pts',(8.41233827490267,30.7477977877063,53.0848304927303));
#88827=CARTESIAN_POINT('Ctrl Pts',(8.41619766621771,30.8132403429686,53.1130347891208));
#88828=CARTESIAN_POINT('Ctrl Pts',(8.42005924267704,30.8787199510757,53.1412550544693));
#88829=CARTESIAN_POINT('Ctrl Pts',(8.42392081913638,30.9426703412895,53.1728623357878));
#88830=CARTESIAN_POINT('Ctrl Pts',(8.42778239559572,31.0047312648068,53.2076516387656));
#88831=CARTESIAN_POINT('Ctrl Pts',(8.43165072859373,31.0669007753313,53.2425018120314));
#88832=CARTESIAN_POINT('Ctrl Pts',(8.43551906159174,31.1271738077633,53.2805448633252));
#88833=CARTESIAN_POINT('Ctrl Pts',(8.43938739458976,31.1852188559992,53.3215322982303));
#88834=CARTESIAN_POINT('Ctrl Pts',(8.44168512430334,31.2196967130313,53.3458781979017));
#88835=CARTESIAN_POINT('Ctrl Pts',(8.44398285401693,31.2533891120851,53.3712621389149));
#88836=CARTESIAN_POINT('Ctrl Pts',(8.44628058373051,31.2862325040358,53.3976256654384));
#88837=CARTESIAN_POINT('Ctrl Pts',(8.45010049356877,31.3408337024676,53.441454273191));
#88838=CARTESIAN_POINT('Ctrl Pts',(8.45392040340703,31.3933122653082,53.488173590139));
#88839=CARTESIAN_POINT('Ctrl Pts',(8.45774031324528,31.4433401967307,53.5375477310348));
#88840=CARTESIAN_POINT('Ctrl Pts',(8.46155371487817,31.49328289262,53.5868377502989));
#88841=CARTESIAN_POINT('Ctrl Pts',(8.46536711651106,31.5407828948695,53.6387732653233));
#88842=CARTESIAN_POINT('Ctrl Pts',(8.46918051814395,31.585544633233,53.693077745799));
#88843=CARTESIAN_POINT('Ctrl Pts',(8.47299028959825,31.6302637605316,53.747330530969));
#88844=CARTESIAN_POINT('Ctrl Pts',(8.47680006105254,31.6722494743745,53.8039474289001));
#88845=CARTESIAN_POINT('Ctrl Pts',(8.48060983250683,31.7112435202134,53.8626156423496));
#88846=CARTESIAN_POINT('Ctrl Pts',(8.48441732946353,31.7502142859515,53.9212488298896));
#88847=CARTESIAN_POINT('Ctrl Pts',(8.48822482642023,31.7861966495347,53.9819304895735));
#88848=CARTESIAN_POINT('Ctrl Pts',(8.49203232337693,31.8189742648894,54.0443169007616));
#88849=CARTESIAN_POINT('Ctrl Pts',(8.49583889833161,31.8517439430014,54.1066882048078));
#88850=CARTESIAN_POINT('Ctrl Pts',(8.4996454732863,31.8813101817803,54.1707629987572));
#88851=CARTESIAN_POINT('Ctrl Pts',(8.50345204824098,31.9075023513006,54.236172570352));
#88852=CARTESIAN_POINT('Ctrl Pts',(8.50726133449443,31.9337131766461,54.301628731044));
#88853=CARTESIAN_POINT('Ctrl Pts',(8.51107062074788,31.9565449440846,54.3684211048419));
#88854=CARTESIAN_POINT('Ctrl Pts',(8.51487990700134,31.9758754824593,54.4361616895632));
#88855=CARTESIAN_POINT('Ctrl Pts',(8.51869055156213,31.995212913677,54.5039264290807));
#88856=CARTESIAN_POINT('Ctrl Pts',(8.52250119612292,32.0110465156929,54.5726395660196));
#88857=CARTESIAN_POINT('Ctrl Pts',(8.52631184068371,32.0233049526314,54.6419013667199));
#88858=CARTESIAN_POINT('Ctrl Pts',(8.53012846729214,32.035582633179,54.7112718963729));
#88859=CARTESIAN_POINT('Ctrl Pts',(8.53394509390057,32.0442738790978,54.7811923136052));
#88860=CARTESIAN_POINT('Ctrl Pts',(8.537761720509,32.0493591950676,54.8512570939779));
#88861=CARTESIAN_POINT('Ctrl Pts',(8.54048290716825,32.0529849346001,54.9012120319884));
#88862=CARTESIAN_POINT('Ctrl Pts',(8.5432040938275,32.0547787224859,54.9512402585401));
#88863=CARTESIAN_POINT('Ctrl Pts',(8.54592528048675,32.0547496520916,55.001195712928));
#88864=CARTESIAN_POINT('Origin',(-1.54592528053767,30.,55.));
#88865=CARTESIAN_POINT('',(7.39391310532386,28.7479524050421,56.6292250864936));
#88866=CARTESIAN_POINT('',(7.45211324799747,28.7479524050421,56.6292250864936));
#88867=CARTESIAN_POINT('',(-1.54592528053767,28.7479524050421,56.6292250864936));
#88868=CARTESIAN_POINT('',(7.9040747195078,32.0547494456334,54.9984906394957));
#88869=CARTESIAN_POINT('Ctrl Pts',(7.45211324799746,28.7479524050421,56.6292250864936));
#88870=CARTESIAN_POINT('Ctrl Pts',(7.45597808883343,28.6916394093406,56.5859489600594));
#88871=CARTESIAN_POINT('Ctrl Pts',(7.45984292966939,28.6374791542456,56.5396778427251));
#88872=CARTESIAN_POINT('Ctrl Pts',(7.46370777050535,28.585805915676,56.4906551091258));
#88873=CARTESIAN_POINT('Ctrl Pts',(7.4675674996065,28.5342010214195,56.4416972142158));
#88874=CARTESIAN_POINT('Ctrl Pts',(7.47142722870764,28.4850769597258,56.3899952649857));
#88875=CARTESIAN_POINT('Ctrl Pts',(7.47528695780879,28.4387352829959,56.3358330905986));
#88876=CARTESIAN_POINT('Ctrl Pts',(7.47914387883221,28.3924273213345,56.2817103209448));
#88877=CARTESIAN_POINT('Ctrl Pts',(7.48300079985563,28.3488980437697,56.2251312448299));
#88878=CARTESIAN_POINT('Ctrl Pts',(7.48685772087905,28.3084114391004,56.166415750551));
#88879=CARTESIAN_POINT('Ctrl Pts',(7.49071312610269,28.2679407459796,56.1077233319152));
#88880=CARTESIAN_POINT('Ctrl Pts',(7.49456853132634,28.2305106279276,56.0468965611038));
#88881=CARTESIAN_POINT('Ctrl Pts',(7.49842393654998,28.1963430684199,55.9842861553751));
#88882=CARTESIAN_POINT('Ctrl Pts',(7.50227911625905,28.1621775074785,55.9216794119227));
#88883=CARTESIAN_POINT('Ctrl Pts',(7.50613429596812,28.1312743574825,55.8572896678745));
#88884=CARTESIAN_POINT('Ctrl Pts',(7.5099894756772,28.1038099013592,55.7914926862055));
#88885=CARTESIAN_POINT('Ctrl Pts',(7.51384844943747,28.0763184162619,55.725630950845));
#88886=CARTESIAN_POINT('Ctrl Pts',(7.51770742319774,28.0522725726796,55.6583596607912));
#88887=CARTESIAN_POINT('Ctrl Pts',(7.52156639695801,28.0318003266534,55.5900742396838));
#88888=CARTESIAN_POINT('Ctrl Pts',(7.52542721801123,28.0113182805513,55.5217561303062));
#88889=CARTESIAN_POINT('Ctrl Pts',(7.52928803906444,27.9944133552572,55.4524233954285));
#88890=CARTESIAN_POINT('Ctrl Pts',(7.53314886011766,27.9811627431385,55.3824835850177));
#88891=CARTESIAN_POINT('Ctrl Pts',(7.53701679547944,27.9678877142075,55.3124148969963));
#88892=CARTESIAN_POINT('Ctrl Pts',(7.54088473084123,27.9582805181449,55.2417373809803));
#88893=CARTESIAN_POINT('Ctrl Pts',(7.54475266620301,27.9523665739296,55.1708651952251));
#88894=CARTESIAN_POINT('Ctrl Pts',(7.54817645798591,27.9471317104392,55.1081310529687));
#88895=CARTESIAN_POINT('Ctrl Pts',(7.5516002497688,27.9447898576055,55.0452446609213));
#88896=CARTESIAN_POINT('Ctrl Pts',(7.5550240415517,27.945324596287,54.9824914912983));
#88897=CARTESIAN_POINT('Ctrl Pts',(7.55889311489863,27.9459288804584,54.911576952267));
#88898=CARTESIAN_POINT('Ctrl Pts',(7.56276218824556,27.950209947427,54.840554831208));
#88899=CARTESIAN_POINT('Ctrl Pts',(7.56663126159248,27.9581814784797,54.7698376927546));
#88900=CARTESIAN_POINT('Ctrl Pts',(7.57049456998679,27.9661411318824,54.6992259234468));
#88901=CARTESIAN_POINT('Ctrl Pts',(7.5743578783811,27.9777802803876,54.628918713516));
#88902=CARTESIAN_POINT('Ctrl Pts',(7.57822118677541,27.993060597262,54.5593280174123));
#88903=CARTESIAN_POINT('Ctrl Pts',(7.58207996326658,28.0083229893661,54.4898189555615));
#88904=CARTESIAN_POINT('Ctrl Pts',(7.58593873975774,28.0272179618767,54.4210252101689));
#88905=CARTESIAN_POINT('Ctrl Pts',(7.58979751624891,28.0496556792535,54.3533512599318));
#88906=CARTESIAN_POINT('Ctrl Pts',(7.5936538618352,28.0720792615912,54.2857199421031));
#88907=CARTESIAN_POINT('Ctrl Pts',(7.5975102074215,28.0980410083899,54.2192074798708));
#88908=CARTESIAN_POINT('Ctrl Pts',(7.60136655300779,28.1274009027621,54.1542044079544));
#88909=CARTESIAN_POINT('Ctrl Pts',(7.60522175925105,28.1567521228621,54.0892205409551));
#88910=CARTESIAN_POINT('Ctrl Pts',(7.60907696549432,28.189499297522,54.0257456214304));
#88911=CARTESIAN_POINT('Ctrl Pts',(7.61293217173758,28.2254544716958,53.9641497548026));
#88912=CARTESIAN_POINT('Ctrl Pts',(7.6167875285866,28.2614110504783,53.9025514818982));
#88913=CARTESIAN_POINT('Ctrl Pts',(7.62064288543561,28.3005756307868,53.8428328260587));
#88914=CARTESIAN_POINT('Ctrl Pts',(7.62449824228463,28.3427154183277,53.7853373398959));
#88915=CARTESIAN_POINT('Ctrl Pts',(7.62835763475074,28.3848993159351,53.7277816700002));
#88916=CARTESIAN_POINT('Ctrl Pts',(7.63221702721685,28.430064349888,53.6724542078469));
#88917=CARTESIAN_POINT('Ctrl Pts',(7.63607641968296,28.4779362178107,53.6196669222801));
#88918=CARTESIAN_POINT('Ctrl Pts',(7.63993799728382,28.5258351901243,53.5668497492808));
#88919=CARTESIAN_POINT('Ctrl Pts',(7.64379957488468,28.576443702482,53.5165759584295));
#88920=CARTESIAN_POINT('Ctrl Pts',(7.64766115248553,28.6294511728063,53.4691200325375));
#88921=CARTESIAN_POINT('Ctrl Pts',(7.65152948659766,28.6825513890514,53.421581074131));
#88922=CARTESIAN_POINT('Ctrl Pts',(7.65539782070978,28.738058565056,53.376870129106));
#88923=CARTESIAN_POINT('Ctrl Pts',(7.6592661548219,28.7956302665086,53.3352204027109));
#88924=CARTESIAN_POINT('Ctrl Pts',(7.66156387401135,28.8298267964264,53.3104812326187));
#88925=CARTESIAN_POINT('Ctrl Pts',(7.6638615932008,28.86475117244,53.2868212673977));
#88926=CARTESIAN_POINT('Ctrl Pts',(7.66615931239025,28.9003275144172,53.2642817086427));
#88927=CARTESIAN_POINT('Ctrl Pts',(7.67002838580839,28.9602336507679,53.2263278942534));
#88928=CARTESIAN_POINT('Ctrl Pts',(7.67389745922652,29.0222243264519,53.1914047567569));
#88929=CARTESIAN_POINT('Ctrl Pts',(7.67776653264466,29.0859603481719,53.1597475506371));
#88930=CARTESIAN_POINT('Ctrl Pts',(7.68162984111065,29.14960140268,53.1281375140225));
#88931=CARTESIAN_POINT('Ctrl Pts',(7.68549314957663,29.2149822096154,53.099783963722));
#88932=CARTESIAN_POINT('Ctrl Pts',(7.68935645804262,29.2817358810413,53.0748781290743));
#88933=CARTESIAN_POINT('Ctrl Pts',(7.69321523460581,29.3484112462298,53.0500015105305));
#88934=CARTESIAN_POINT('Ctrl Pts',(7.69707401116899,29.4164558240683,53.0285647431085));
#88935=CARTESIAN_POINT('Ctrl Pts',(7.70093278773218,29.4854810707992,53.0107117267741));
#88936=CARTESIAN_POINT('Ctrl Pts',(7.70478913339068,29.5544628338524,52.9928699572638));
#88937=CARTESIAN_POINT('Ctrl Pts',(7.70864547904917,29.6244235709156,52.9786075810603));
#88938=CARTESIAN_POINT('Ctrl Pts',(7.71250182470766,29.6949592366148,52.9680187758807));
#88939=CARTESIAN_POINT('Ctrl Pts',(7.71635703102319,29.7654740628141,52.9574330991242));
#88940=CARTESIAN_POINT('Ctrl Pts',(7.72021223733871,29.836563000288,52.9505189107643));
#88941=CARTESIAN_POINT('Ctrl Pts',(7.72406744365423,29.9078131672703,52.9473190334659));
#88942=CARTESIAN_POINT('Ctrl Pts',(7.72792280057547,29.9790661176788,52.9441190311626));
#88943=CARTESIAN_POINT('Ctrl Pts',(7.73177815749672,30.0504798247049,52.9446336475956));
#88944=CARTESIAN_POINT('Ctrl Pts',(7.73563351441796,30.1216393955579,52.948853632734));
#88945=CARTESIAN_POINT('Ctrl Pts',(7.73949290695573,30.1928734530918,52.9530780351657));
#88946=CARTESIAN_POINT('Ctrl Pts',(7.7433522994935,30.2638523574922,52.961015520074));
#88947=CARTESIAN_POINT('Ctrl Pts',(7.74721169203127,30.3341652383747,52.9726048347789));
#88948=CARTESIAN_POINT('Ctrl Pts',(7.75107326970358,30.4045179294353,52.984200711193));
#88949=CARTESIAN_POINT('Ctrl Pts',(7.7549348473759,30.4742033715237,52.9994524294759));
#88950=CARTESIAN_POINT('Ctrl Pts',(7.75879642504821,30.5428225110972,53.0182479257117));
#88951=CARTESIAN_POINT('Ctrl Pts',(7.76266475923068,30.611561711939,53.037076307978));
#88952=CARTESIAN_POINT('Ctrl Pts',(7.76653309341314,30.6792304240199,53.0594606949899));
#88953=CARTESIAN_POINT('Ctrl Pts',(7.77040142759561,30.7454469973676,53.085239874915));
#88954=CARTESIAN_POINT('Ctrl Pts',(7.77269914614001,30.7847784101543,53.100552228238));
#88955=CARTESIAN_POINT('Ctrl Pts',(7.77499686468441,30.8235978937815,53.1170613980573));
#88956=CARTESIAN_POINT('Ctrl Pts',(7.77729458322882,30.8618296784007,53.1347259804716));
#88957=CARTESIAN_POINT('Ctrl Pts',(7.78116365643173,30.9262072644763,53.1644709475503));
#88958=CARTESIAN_POINT('Ctrl Pts',(7.78503272963465,30.9891692263907,53.1976109568967));
#88959=CARTESIAN_POINT('Ctrl Pts',(7.78890180283756,31.0503339503682,53.233988631066));
#88960=CARTESIAN_POINT('Ctrl Pts',(7.79276511108818,31.1114075383818,53.2703121021886));
#88961=CARTESIAN_POINT('Ctrl Pts',(7.79662841933881,31.1706887898942,53.3098634160372));
#88962=CARTESIAN_POINT('Ctrl Pts',(7.80049172758943,31.2278180579912,53.3524380500356));
#88963=CARTESIAN_POINT('Ctrl Pts',(7.80435050393808,31.284880309887,53.3949627413279));
#88964=CARTESIAN_POINT('Ctrl Pts',(7.80820928028672,31.3397952050739,53.4405034192621));
#88965=CARTESIAN_POINT('Ctrl Pts',(7.81206805663537,31.3922311147639,53.4888116975098));
#88966=CARTESIAN_POINT('Ctrl Pts',(7.81592440207993,31.4446339915296,53.5370895431073));
#88967=CARTESIAN_POINT('Ctrl Pts',(7.8197807475245,31.4945606247154,53.588131201571));
#88968=CARTESIAN_POINT('Ctrl Pts',(7.82363709296907,31.5417127518387,53.6416482954265));
#88969=CARTESIAN_POINT('Ctrl Pts',(7.8274922990716,31.5888509480522,53.6951495778678));
#88970=CARTESIAN_POINT('Ctrl Pts',(7.83134750517413,31.6332159446003,53.7511244794588));
#88971=CARTESIAN_POINT('Ctrl Pts',(7.83520271127665,31.6745478320743,53.8092493457506));
#88972=CARTESIAN_POINT('Ctrl Pts',(7.83905806798614,31.7158813342142,53.8673764827406));
#88973=CARTESIAN_POINT('Ctrl Pts',(7.84291342469562,31.7541812123083,53.9276533540082));
#88974=CARTESIAN_POINT('Ctrl Pts',(7.8467687814051,31.7892302147803,53.9897263731952));
#88975=CARTESIAN_POINT('Ctrl Pts',(7.85062817373444,31.824315905025,54.0518643677213));
#88976=CARTESIAN_POINT('Ctrl Pts',(7.85448756606379,31.8561436874045,54.1158018394496));
#88977=CARTESIAN_POINT('Ctrl Pts',(7.85834695839314,31.8845421816423,54.1811603770512));
#88978=CARTESIAN_POINT('Ctrl Pts',(7.86220853585858,31.9129567547261,54.246555919779));
#88979=CARTESIAN_POINT('Ctrl Pts',(7.86607011332404,31.9379380043066,54.3133736748274));
#88980=CARTESIAN_POINT('Ctrl Pts',(7.86993169078948,31.9593636478709,54.3812176005234));
#88981=CARTESIAN_POINT('Ctrl Pts',(7.8738000247698,31.9808267793997,54.4491802312037));
#88982=CARTESIAN_POINT('Ctrl Pts',(7.87766835875011,31.9987217621738,54.5181721468595));
#88983=CARTESIAN_POINT('Ctrl Pts',(7.88153669273042,32.0129770440577,54.587785271252));
#88984=CARTESIAN_POINT('Ctrl Pts',(7.88383441317607,32.0214444237642,54.6291342085506));
#88985=CARTESIAN_POINT('Ctrl Pts',(7.88613213362173,32.0286286516942,54.6707021625283));
#88986=CARTESIAN_POINT('Ctrl Pts',(7.88842985406738,32.0345234182149,54.7124030194264));
#88987=CARTESIAN_POINT('Ctrl Pts',(7.89364480919903,32.047902305527,54.8070481700526));
#88988=CARTESIAN_POINT('Ctrl Pts',(7.89885976433068,32.0546790423547,54.9026480509711));
#88989=CARTESIAN_POINT('Ctrl Pts',(7.90407471946233,32.0547494456328,54.99849063866));
#88990=CARTESIAN_POINT('Ctrl Pts',(7.9040747195078,32.0547494456334,54.9984906394957));
#88991=CARTESIAN_POINT('Ctrl Pts',(7.90805348639939,32.0548031600125,55.0716140518894));
#88992=CARTESIAN_POINT('Ctrl Pts',(7.91203225329098,32.050948418131,55.1448858516356));
#88993=CARTESIAN_POINT('Ctrl Pts',(7.91601102018257,32.0431692286174,55.2178464269408));
#88994=CARTESIAN_POINT('Ctrl Pts',(7.9198148683539,32.0357320359866,55.2875994329639));
#88995=CARTESIAN_POINT('Ctrl Pts',(7.92361871652522,32.0247082537432,55.3570674381738));
#88996=CARTESIAN_POINT('Ctrl Pts',(7.92742256469655,32.0101370404031,55.4258481434733));
#88997=CARTESIAN_POINT('Ctrl Pts',(7.93122379837268,31.9955758422806,55.4945815737987));
#88998=CARTESIAN_POINT('Ctrl Pts',(7.93502503204882,31.9774721493163,55.562628151676));
#88999=CARTESIAN_POINT('Ctrl Pts',(7.93882626572496,31.9559166148128,55.6295933277913));
#89000=CARTESIAN_POINT('Ctrl Pts',(7.94262624479613,31.9343681947576,55.6965364019132));
#89001=CARTESIAN_POINT('Ctrl Pts',(7.94642622386731,31.9093703466155,55.7623983055163));
#89002=CARTESIAN_POINT('Ctrl Pts',(7.95022620293848,31.881063720918,55.8267991535712));
#89003=CARTESIAN_POINT('Ctrl Pts',(7.95402628536076,31.8527563253424,55.891201753188));
#89004=CARTESIAN_POINT('Ctrl Pts',(7.95782636778304,31.821140178272,55.9541427608864));
#89005=CARTESIAN_POINT('Ctrl Pts',(7.96162645020532,31.7864034803868,56.0152635952116));
#89006=CARTESIAN_POINT('Ctrl Pts',(7.96543037542157,31.7516316553758,56.0764462373471));
#89007=CARTESIAN_POINT('Ctrl Pts',(7.96923430063783,31.7137332332642,56.1358045982852));
#89008=CARTESIAN_POINT('Ctrl Pts',(7.97303822585408,31.6729410672239,56.1930070192986));
#89009=CARTESIAN_POINT('Ctrl Pts',(7.97684442147971,31.6321245539866,56.2502435821276));
#89010=CARTESIAN_POINT('Ctrl Pts',(7.98065061710535,31.5884111753275,56.305321255317));
#89011=CARTESIAN_POINT('Ctrl Pts',(7.98445681273098,31.5420737815355,56.3579418304187));
#89012=CARTESIAN_POINT('Ctrl Pts',(7.98826926304291,31.4956602419301,56.4106488764279));
#89013=CARTESIAN_POINT('Ctrl Pts',(7.99208171335483,31.4466144388796,56.460890416329));
#89014=CARTESIAN_POINT('Ctrl Pts',(7.99589416366676,31.3952448863443,56.5084062018004));
#89015=CARTESIAN_POINT('Ctrl Pts',(7.99711781741315,31.3787571841404,56.5236569891282));
#89016=CARTESIAN_POINT('Ctrl Pts',(7.99834147115954,31.3620303358886,56.5386273004867));
#89017=CARTESIAN_POINT('Ctrl Pts',(7.99956512490593,31.3450751859396,56.5533094690593));
#89018=CARTESIAN_POINT('Ctrl Pts',(8.00343419874421,31.2914646549499,56.5997330545558));
#89019=CARTESIAN_POINT('Ctrl Pts',(8.00730327258249,31.2353429159238,56.6434688627475));
#89020=CARTESIAN_POINT('Ctrl Pts',(8.01117234642077,31.1770104950513,56.6842339080541));
#89021=CARTESIAN_POINT('Ctrl Pts',(8.01503565530908,31.1187649899374,56.7249382131276));
#89022=CARTESIAN_POINT('Ctrl Pts',(8.01889896419739,31.0583157362857,56.7626802657115));
#89023=CARTESIAN_POINT('Ctrl Pts',(8.0227622730857,30.9959971815572,56.7972165080563));
#89024=CARTESIAN_POINT('Ctrl Pts',(8.02662105007241,30.9337517303693,56.8317122372409));
#89025=CARTESIAN_POINT('Ctrl Pts',(8.03047982705912,30.8696417565971,56.8630093917077));
#89026=CARTESIAN_POINT('Ctrl Pts',(8.03433860404583,30.8040301473627,56.8909080053329));
#89027=CARTESIAN_POINT('Ctrl Pts',(8.03819495012834,30.7384598713115,56.9187890437374));
#89028=CARTESIAN_POINT('Ctrl Pts',(8.04205129621086,30.6713902826035,56.9432755993105));
#89029=CARTESIAN_POINT('Ctrl Pts',(8.04590764229338,30.6032069770608,56.9642145772102));
#89030=CARTESIAN_POINT('Ctrl Pts',(8.04976284903281,30.5350438160218,56.9851473687669));
#89031=CARTESIAN_POINT('Ctrl Pts',(8.05361805577223,30.4657680555189,57.0025345209226));
#89032=CARTESIAN_POINT('Ctrl Pts',(8.05747326251165,30.3957816509574,57.0162724139524));
#89033=CARTESIAN_POINT('Ctrl Pts',(8.06132861985604,30.3257925123531,57.0300108436577));
#89034=CARTESIAN_POINT('Ctrl Pts',(8.06518397720043,30.2550931516865,57.0400996397943));
#89035=CARTESIAN_POINT('Ctrl Pts',(8.06903933454482,30.184095240651,57.0464863803284));
#89036=CARTESIAN_POINT('Ctrl Pts',(8.07289872750168,30.1130230122358,57.0528798062116));
#89037=CARTESIAN_POINT('Ctrl Pts',(8.07675812045855,30.0416520944371,57.0555633972228));
#89038=CARTESIAN_POINT('Ctrl Pts',(8.08061751341541,29.9703978982166,57.0545367551032));
#89039=CARTESIAN_POINT('Ctrl Pts',(8.08447909150516,29.899103358893,57.0535095317136));
#89040=CARTESIAN_POINT('Ctrl Pts',(8.08834066959491,29.8279261576458,57.0487679256912));
#89041=CARTESIAN_POINT('Ctrl Pts',(8.09220224768466,29.75727755977,57.0403635410164));
#89042=CARTESIAN_POINT('Ctrl Pts',(8.09607058227741,29.6865053498754,57.0319444514077));
#89043=CARTESIAN_POINT('Ctrl Pts',(8.09993891687017,29.6162640688021,57.0198498705121));
#89044=CARTESIAN_POINT('Ctrl Pts',(8.10380725146292,29.546955064474,57.0041825887115));
#89045=CARTESIAN_POINT('Ctrl Pts',(8.10610496622344,29.5057868773735,56.9948765310819));
#89046=CARTESIAN_POINT('Ctrl Pts',(8.10840268098397,29.4649473438168,56.984310943031));
#89047=CARTESIAN_POINT('Ctrl Pts',(8.11070039574449,29.4245175385844,56.9725155256938));
#89048=CARTESIAN_POINT('Ctrl Pts',(8.11456845415719,29.356456502054,56.9526586818217));
#89049=CARTESIAN_POINT('Ctrl Pts',(8.11843651256988,29.2892911237888,56.9292361830943));
#89050=CARTESIAN_POINT('Ctrl Pts',(8.12230457098257,29.2234218330817,56.9023469486836));
#89051=CARTESIAN_POINT('Ctrl Pts',(8.12616758929226,29.1576383704503,56.8754927511046));
#89052=CARTESIAN_POINT('Ctrl Pts',(8.13003060760194,29.0931480923012,56.8451809568028));
#89053=CARTESIAN_POINT('Ctrl Pts',(8.13389362591162,29.0303369325548,56.8115604042186));
#89054=CARTESIAN_POINT('Ctrl Pts',(8.13775232708187,28.9675959677993,56.777977424486));
#89055=CARTESIAN_POINT('Ctrl Pts',(8.14161102825211,28.9065308214457,56.7410932569561));
#89056=CARTESIAN_POINT('Ctrl Pts',(8.14546972942235,28.8475062975245,56.7011042967009));
#89057=CARTESIAN_POINT('Ctrl Pts',(8.14768450203097,28.8136280848697,56.678151896421));
#89058=CARTESIAN_POINT('Ctrl Pts',(8.14989927463959,28.7804217316529,56.6541775271539));
#89059=CARTESIAN_POINT('Ctrl Pts',(8.1521140472482,28.7479524050421,56.6292250864936));
#89060=CARTESIAN_POINT('',(7.84592528058377,32.0547497348706,55.0010438147506));
#89061=CARTESIAN_POINT('Ctrl Pts',(7.84592528058377,32.0547497348706,55.0010438147506));
#89062=CARTESIAN_POINT('Ctrl Pts',(7.85018308153819,32.054709658985,55.0799332108663));
#89063=CARTESIAN_POINT('Ctrl Pts',(7.85444088249261,32.0501221476688,55.1586663192241));
#89064=CARTESIAN_POINT('Ctrl Pts',(7.85869868344703,32.0410657724735,55.2367447463771));
#89065=CARTESIAN_POINT('Ctrl Pts',(7.86297170270139,32.0319770278378,55.3151022426871));
#89066=CARTESIAN_POINT('Ctrl Pts',(7.86724472195574,32.0183875525732,55.3928000839848));
#89067=CARTESIAN_POINT('Ctrl Pts',(7.8715177412101,32.0004267215885,55.4693511415292));
#89068=CARTESIAN_POINT('Ctrl Pts',(7.87581130775081,31.9823795239587,55.5462703033123));
#89069=CARTESIAN_POINT('Ctrl Pts',(7.88010487429152,31.9599189709612,55.6220313489285));
#89070=CARTESIAN_POINT('Ctrl Pts',(7.88439844083223,31.9332245845972,55.6961610934325));
#89071=CARTESIAN_POINT('Ctrl Pts',(7.8864670370674,31.92036350358,55.7318760425174));
#89072=CARTESIAN_POINT('Ctrl Pts',(7.88853563330255,31.9065203612943,55.7672126691331));
#89073=CARTESIAN_POINT('Ctrl Pts',(7.89060422953771,31.8917190493863,55.802120066255));
#89074=CARTESIAN_POINT('Ctrl Pts',(7.89447330295551,31.8640348829558,55.8674103727891));
#89075=CARTESIAN_POINT('Ctrl Pts',(7.8983423763733,31.832912403107,55.9313936569463));
#89076=CARTESIAN_POINT('Ctrl Pts',(7.90221144979109,31.7984967809814,55.9936834965419));
#89077=CARTESIAN_POINT('Ctrl Pts',(7.90607475825673,31.7641324384241,56.055880523749));
#89078=CARTESIAN_POINT('Ctrl Pts',(7.90993806672237,31.7264849264835,56.1163886932305));
#89079=CARTESIAN_POINT('Ctrl Pts',(7.91380137518801,31.6857472356805,56.1748420404018));
#89080=CARTESIAN_POINT('Ctrl Pts',(7.91766015175086,31.6450573327403,56.233226818136));
#89081=CARTESIAN_POINT('Ctrl Pts',(7.9215189283137,31.6012847277701,56.2895611648883));
#89082=CARTESIAN_POINT('Ctrl Pts',(7.92537770487655,31.5546671432434,56.343505726158));
#89083=CARTESIAN_POINT('Ctrl Pts',(7.9292340505347,31.5080789262906,56.3974163040951));
#89084=CARTESIAN_POINT('Ctrl Pts',(7.93309039619284,31.4586496024489,56.4489397167259));
#89085=CARTESIAN_POINT('Ctrl Pts',(7.93694674185099,31.4066579254486,56.4977686881734));
#89086=CARTESIAN_POINT('Ctrl Pts',(7.94080194816617,31.3546816091956,56.5465832332832));
#89087=CARTESIAN_POINT('Ctrl Pts',(7.94465715448135,31.3001447966244,56.5927045852321));
#89088=CARTESIAN_POINT('Ctrl Pts',(7.94851236079653,31.2433627193998,56.6358626808222));
#89089=CARTESIAN_POINT('Ctrl Pts',(7.95236771771743,31.1865784239527,56.6790224624065));
#89090=CARTESIAN_POINT('Ctrl Pts',(7.95622307463832,31.1275490777957,56.7192184656));
#89091=CARTESIAN_POINT('Ctrl Pts',(7.96007843155922,31.066621184959,56.7562223123217));
#89092=CARTESIAN_POINT('Ctrl Pts',(7.96393782409665,31.0056295155079,56.7932648930281));
#89093=CARTESIAN_POINT('Ctrl Pts',(7.96779721663408,30.9427357483097,56.8271083943739));
#89094=CARTESIAN_POINT('Ctrl Pts',(7.97165660917151,30.8783126575179,56.8575694975273));
#89095=CARTESIAN_POINT('Ctrl Pts',(7.97551818684348,30.8138530912655,56.8880478473349));
#89096=CARTESIAN_POINT('Ctrl Pts',(7.97937976451545,30.7478629273174,56.9151398020609));
#89097=CARTESIAN_POINT('Ctrl Pts',(7.98324134218742,30.6807341214891,56.938710555586));
#89098=CARTESIAN_POINT('Ctrl Pts',(7.98710967636956,30.6134878619935,56.9623225502952));
#89099=CARTESIAN_POINT('Ctrl Pts',(7.9909780105517,30.5450994492843,56.982400906374));
#89100=CARTESIAN_POINT('Ctrl Pts',(7.99484634473384,30.4759744797673,56.998861140027));
#89101=CARTESIAN_POINT('Ctrl Pts',(7.99714406328132,30.4349155337004,57.0086382126324));
#89102=CARTESIAN_POINT('Ctrl Pts',(7.9994417818288,30.3935969062403,57.0171397434808));
#89103=CARTESIAN_POINT('Ctrl Pts',(8.00173950037628,30.3521044669293,57.0243566896346));
#89104=CARTESIAN_POINT('Ctrl Pts',(8.00560732707783,30.2822588520887,57.0365052171677));
#89105=CARTESIAN_POINT('Ctrl Pts',(8.00947515377938,30.2116470006334,57.0450585066231));
#89106=CARTESIAN_POINT('Ctrl Pts',(8.01334298048093,30.1406719063312,57.0499290176172));
#89107=CARTESIAN_POINT('Ctrl Pts',(8.01720559809914,30.0697923993474,57.0547929691402));
#89108=CARTESIAN_POINT('Ctrl Pts',(8.02106821571735,29.998551099857,57.0559839468317));
#89109=CARTESIAN_POINT('Ctrl Pts',(8.02493083333555,29.9273599179333,57.0534656025795));
#89110=CARTESIAN_POINT('Ctrl Pts',(8.02878954136263,29.8562407929515,57.0509498072973));
#89111=CARTESIAN_POINT('Ctrl Pts',(8.0326482493897,29.7851721677428,57.044732156475));
#89112=CARTESIAN_POINT('Ctrl Pts',(8.03650695741678,29.7145680590569,57.0348282899521));
#89113=CARTESIAN_POINT('Ctrl Pts',(8.04036305078054,29.6440117917654,57.0249311342962));
#89114=CARTESIAN_POINT('Ctrl Pts',(8.04421914414431,29.5739198959833,57.0113527887946));
#89115=CARTESIAN_POINT('Ctrl Pts',(8.04807523750807,29.5047016374595,56.9941607494294));
#89116=CARTESIAN_POINT('Ctrl Pts',(8.05193146499039,29.4354809714595,56.9769681121088));
#89117=CARTESIAN_POINT('Ctrl Pts',(8.05578769247272,29.3671344794266,56.9561616284492));
#89118=CARTESIAN_POINT('Ctrl Pts',(8.05964391995505,29.3000603463786,56.9318597370897));
#89119=CARTESIAN_POINT('Ctrl Pts',(8.0634999438389,29.2329897546648,56.9075591288049));
#89120=CARTESIAN_POINT('Ctrl Pts',(8.06735596772276,29.1671918430208,56.87976365237));
#89121=CARTESIAN_POINT('Ctrl Pts',(8.07121199160661,29.1030466153127,56.8486406325184));
#89122=CARTESIAN_POINT('Ctrl Pts',(8.07507195419949,29.0388358669038,56.8174858222726));
#89123=CARTESIAN_POINT('Ctrl Pts',(8.07893191679236,28.9762816102448,56.7829968969987));
#89124=CARTESIAN_POINT('Ctrl Pts',(8.08279187938524,28.9157401986791,56.745387706425));
#89125=CARTESIAN_POINT('Ctrl Pts',(8.08648107370469,28.8578771945009,56.7094423808202));
#89126=CARTESIAN_POINT('Ctrl Pts',(8.09017026802414,28.8018530005804,56.6706473009991));
#89127=CARTESIAN_POINT('Ctrl Pts',(8.09385946234359,28.7479524050421,56.6292250864936));
#89128=CARTESIAN_POINT('Ctrl Pts',(7.39391310532386,28.7479524050421,56.6292250864936));
#89129=CARTESIAN_POINT('Ctrl Pts',(7.39776854184031,28.6913983985599,56.5857637450324));
#89130=CARTESIAN_POINT('Ctrl Pts',(7.40162397835676,28.6371169242198,56.5393596194705));
#89131=CARTESIAN_POINT('Ctrl Pts',(7.40547941487322,28.5854187500326,56.4902877070354));
#89132=CARTESIAN_POINT('Ctrl Pts',(7.40933896177683,28.5336654589967,56.4411634776816));
#89133=CARTESIAN_POINT('Ctrl Pts',(7.41319850868044,28.4845013178865,56.3893661199868));
#89134=CARTESIAN_POINT('Ctrl Pts',(7.41705805558405,28.4382004105911,56.3352077010795));
#89135=CARTESIAN_POINT('Ctrl Pts',(7.42091989553231,28.3918719948729,56.2810171054231));
#89136=CARTESIAN_POINT('Ctrl Pts',(7.42478173548057,28.3484104947549,56.2244630418472));
#89137=CARTESIAN_POINT('Ctrl Pts',(7.42864357542883,28.30804814303,56.1658887066078));
#89138=CARTESIAN_POINT('Ctrl Pts',(7.43251206243218,28.2676163190382,56.1072135523706));
#89139=CARTESIAN_POINT('Ctrl Pts',(7.43638054943553,28.2302945452081,56.0465115992591));
#89140=CARTESIAN_POINT('Ctrl Pts',(7.44024903643888,28.1962699885805,55.9841522282678));
#89141=CARTESIAN_POINT('Ctrl Pts',(7.44218707302041,28.1792243489395,55.9529113989518));
#89142=CARTESIAN_POINT('Ctrl Pts',(7.44412510960195,28.163005503771,55.92125493001));
#89143=CARTESIAN_POINT('Ctrl Pts',(7.44606314618349,28.1476323957765,55.8892310280929));
#89144=CARTESIAN_POINT('Ctrl Pts',(7.44993221953076,28.1169417044999,55.8252988884398));
#89145=CARTESIAN_POINT('Ctrl Pts',(7.45380129287804,28.089504589936,55.7596507813514));
#89146=CARTESIAN_POINT('Ctrl Pts',(7.45767036622531,28.0655150426256,55.6926510753562));
#89147=CARTESIAN_POINT('Ctrl Pts',(7.46153367462014,28.0415612399463,55.6257511994971));
#89148=CARTESIAN_POINT('Ctrl Pts',(7.46539698301496,28.021044970332,55.5575041758807));
#89149=CARTESIAN_POINT('Ctrl Pts',(7.46926029140978,28.0041132635704,55.4882967313474));
#89150=CARTESIAN_POINT('Ctrl Pts',(7.4731190679017,27.9872014187622,55.4191704714845));
#89151=CARTESIAN_POINT('Ctrl Pts',(7.47697784439362,27.9738658993027,55.34908649816));
#89152=CARTESIAN_POINT('Ctrl Pts',(7.48083662088554,27.9642041985783,55.2784475128523));
#89153=CARTESIAN_POINT('Ctrl Pts',(7.48469296647273,27.9545485844137,55.2078530278271));
#89154=CARTESIAN_POINT('Ctrl Pts',(7.48854931205992,27.9485622629525,55.136704704665));
#89155=CARTESIAN_POINT('Ctrl Pts',(7.49240565764711,27.9462915341241,55.0654148277497));
#89156=CARTESIAN_POINT('Ctrl Pts',(7.49626086389141,27.944021476174,54.9941460131621));
#89157=CARTESIAN_POINT('Ctrl Pts',(7.50011607013571,27.9454648469601,54.9227362131237));
#89158=CARTESIAN_POINT('Ctrl Pts',(7.50397127638,27.9506159104974,54.8516004845243));
#89159=CARTESIAN_POINT('Ctrl Pts',(7.5078266332302,27.9557671752639,54.7804619769658));
#89160=CARTESIAN_POINT('Ctrl Pts',(7.51168199008039,27.964626383067,54.7095980464614));
#89161=CARTESIAN_POINT('Ctrl Pts',(7.51553734693059,27.9771358471552,54.639419659943));
#89162=CARTESIAN_POINT('Ctrl Pts',(7.51939673939808,27.9896584055981,54.5691678137887));
#89163=CARTESIAN_POINT('Ctrl Pts',(7.52325613186558,28.0058387623317,54.499603423333));
#89164=CARTESIAN_POINT('Ctrl Pts',(7.52711552433307,28.0255680547007,54.4311273816736));
#89165=CARTESIAN_POINT('Ctrl Pts',(7.53097710193543,28.0453085175232,54.3626125698226));
#89166=CARTESIAN_POINT('Ctrl Pts',(7.53483867953779,28.0686017572935,54.2951877928236));
#89167=CARTESIAN_POINT('Ctrl Pts',(7.53870025714014,28.0952898298514,54.2292362682168));
#89168=CARTESIAN_POINT('Ctrl Pts',(7.54256859125393,28.1220245979017,54.1631693497797));
#89169=CARTESIAN_POINT('Ctrl Pts',(7.54643692536773,28.1521658523427,54.0985812705681));
#89170=CARTESIAN_POINT('Ctrl Pts',(7.55030525948152,28.1855088725025,54.0358322185776));
#89171=CARTESIAN_POINT('Ctrl Pts',(7.5526029786617,28.2053140120516,53.9985604379984));
#89172=CARTESIAN_POINT('Ctrl Pts',(7.55490069784187,28.2262479197591,53.9619369825761));
#89173=CARTESIAN_POINT('Ctrl Pts',(7.55719841702204,28.2482606182029,53.9260322627001));
#89174=CARTESIAN_POINT('Ctrl Pts',(7.56106749037988,28.2853272649097,53.8655731794964));
#89175=CARTESIAN_POINT('Ctrl Pts',(7.56493656373772,28.3256001937771,53.8069168887159));
#89176=CARTESIAN_POINT('Ctrl Pts',(7.56880563709556,28.368878496433,53.7504239906667));
#89177=CARTESIAN_POINT('Ctrl Pts',(7.57266894550101,28.4120923140477,53.6940152675189));
#89178=CARTESIAN_POINT('Ctrl Pts',(7.57653225390645,28.458302323663,53.6397639210872));
#89179=CARTESIAN_POINT('Ctrl Pts',(7.58039556231189,28.507263362889,53.5880032242506));
#89180=CARTESIAN_POINT('Ctrl Pts',(7.58425433881445,28.5561669677477,53.5363032459553));
#89181=CARTESIAN_POINT('Ctrl Pts',(7.58811311531702,28.6078148598398,53.4870884649957));
#89182=CARTESIAN_POINT('Ctrl Pts',(7.59197189181958,28.6619215890214,53.4406592006322));
#89183=CARTESIAN_POINT('Ctrl Pts',(7.59582823741744,28.7159942327092,53.3942591852074));
#89184=CARTESIAN_POINT('Ctrl Pts',(7.5996845830153,28.7725222725302,53.3506415205144));
#89185=CARTESIAN_POINT('Ctrl Pts',(7.60354092861316,28.8311844418321,53.3100687133837));
#89186=CARTESIAN_POINT('Ctrl Pts',(7.60739613486812,28.8898292796153,53.2695078933373));
#89187=CARTESIAN_POINT('Ctrl Pts',(7.61125134112308,28.950606595804,53.2319904210965));
#89188=CARTESIAN_POINT('Ctrl Pts',(7.61510654737804,29.0131645720318,53.1977365895611));
#89189=CARTESIAN_POINT('Ctrl Pts',(7.61896190423888,29.0757249921232,53.1634814198799));
#89190=CARTESIAN_POINT('Ctrl Pts',(7.62281726109971,29.1400657832103,53.1324903754074));
#89191=CARTESIAN_POINT('Ctrl Pts',(7.62667261796054,29.2058103868482,53.1049378846956));
#89192=CARTESIAN_POINT('Ctrl Pts',(7.63053201043858,29.2716238090321,53.0773565532541));
#89193=CARTESIAN_POINT('Ctrl Pts',(7.63439140291661,29.3388435281668,53.053221148785));
#89194=CARTESIAN_POINT('Ctrl Pts',(7.63825079539464,29.4070736933023,53.0326576410483));
#89195=CARTESIAN_POINT('Ctrl Pts',(7.64211237300751,29.475342489417,53.0120824905368));
#89196=CARTESIAN_POINT('Ctrl Pts',(7.64597395062037,29.5446223983934,52.9950833784676));
#89197=CARTESIAN_POINT('Ctrl Pts',(7.64983552823323,29.6145057992422,52.9817354525033));
#89198=CARTESIAN_POINT('Ctrl Pts',(7.65370386235734,29.6845114734286,52.9683641719878));
#89199=CARTESIAN_POINT('Ctrl Pts',(7.65757219648145,29.7551222662411,52.9586568983741));
#89200=CARTESIAN_POINT('Ctrl Pts',(7.66144053060556,29.8259245349132,52.9526369899417));
#89201=CARTESIAN_POINT('Ctrl Pts',(7.66373824969057,29.8679797759474,52.9490612754219));
#89202=CARTESIAN_POINT('Ctrl Pts',(7.66603596877559,29.9101025340802,52.9467855163726));
#89203=CARTESIAN_POINT('Ctrl Pts',(7.6683336878606,29.9522065485288,52.9458059126518));
#89204=CARTESIAN_POINT('Ctrl Pts',(7.6722027611918,30.0231044753042,52.9441563817512));
#89205=CARTESIAN_POINT('Ctrl Pts',(7.676071834523,30.094226769938,52.9461783579694));
#89206=CARTESIAN_POINT('Ctrl Pts',(7.6799409078542,30.1651615109235,52.9518986260906));
#89207=CARTESIAN_POINT('Ctrl Pts',(7.68380421623302,30.2359905585378,52.9576103709633));
#89208=CARTESIAN_POINT('Ctrl Pts',(7.68766752461183,30.3066321269481,52.9670094308485));
#89209=CARTESIAN_POINT('Ctrl Pts',(7.69153083299065,30.3766732518212,52.9800705893863));
#89210=CARTESIAN_POINT('Ctrl Pts',(7.69538960946671,30.4466322140671,52.9931164263668));
#89211=CARTESIAN_POINT('Ctrl Pts',(7.69924838594278,30.5159916566329,53.0098157403258));
#89212=CARTESIAN_POINT('Ctrl Pts',(7.70310716241884,30.5843444503246,53.0300915945469));
#89213=CARTESIAN_POINT('Ctrl Pts',(7.70696350799029,30.6526541839626,53.0503546756343));
#89214=CARTESIAN_POINT('Ctrl Pts',(7.71081985356173,30.7199580622556,53.0741896890356));
#89215=CARTESIAN_POINT('Ctrl Pts',(7.71467619913318,30.7858612982909,53.1014690989219));
#89216=CARTESIAN_POINT('Ctrl Pts',(7.71853140536186,30.8517450634636,53.1287404492093));
#89217=CARTESIAN_POINT('Ctrl Pts',(7.72238661159054,30.9162285593068,53.1594539900038));
#89218=CARTESIAN_POINT('Ctrl Pts',(7.72624181781923,30.9789358945171,53.1934336223305));
#89219=CARTESIAN_POINT('Ctrl Pts',(7.73009717465397,31.0416456794291,53.2274145820929));
#89220=CARTESIAN_POINT('Ctrl Pts',(7.73395253148872,31.1025787398888,53.264661653327));
#89221=CARTESIAN_POINT('Ctrl Pts',(7.73780788832346,31.1613842990994,53.3049530766656));
#89222=CARTESIAN_POINT('Ctrl Pts',(7.74166728077582,31.2202514133776,53.3452866752904));
#89223=CARTESIAN_POINT('Ctrl Pts',(7.74552667322819,31.2769861792992,53.388670712238));
#89224=CARTESIAN_POINT('Ctrl Pts',(7.74938606568054,31.3312680688472,53.4348409373588));
#89225=CARTESIAN_POINT('Ctrl Pts',(7.75324764326794,31.3855806920561,53.4810373034274));
#89226=CARTESIAN_POINT('Ctrl Pts',(7.75710922085533,31.4374373209418,53.5300226642431));
#89227=CARTESIAN_POINT('Ctrl Pts',(7.76097079844273,31.4865537416984,53.5814953170531));
#89228=CARTESIAN_POINT('Ctrl Pts',(7.76483913254197,31.535756100306,53.633058030358));
#89229=CARTESIAN_POINT('Ctrl Pts',(7.76870746664122,31.5822083617667,53.6871163559044));
#89230=CARTESIAN_POINT('Ctrl Pts',(7.77257580074047,31.6256665567958,53.7433354430813));
#89231=CARTESIAN_POINT('Ctrl Pts',(7.77487352006003,31.6514799254838,53.7767285470431));
#89232=CARTESIAN_POINT('Ctrl Pts',(7.7771712393796,31.6762377635927,53.8108834243772));
#89233=CARTESIAN_POINT('Ctrl Pts',(7.77946895869917,31.6998964790238,53.8457255425582));
#89234=CARTESIAN_POINT('Ctrl Pts',(7.78339694508646,31.740341415602,53.9052886775131));
#89235=CARTESIAN_POINT('Ctrl Pts',(7.78732493147376,31.7777270931469,53.9670902448251));
#89236=CARTESIAN_POINT('Ctrl Pts',(7.79125291786106,31.811802195853,54.0307887920571));
#89237=CARTESIAN_POINT('Ctrl Pts',(7.79517455595466,31.845822227401,54.094384391609));
#89238=CARTESIAN_POINT('Ctrl Pts',(7.79909619404826,31.8765420917977,54.1598704747647));
#89239=CARTESIAN_POINT('Ctrl Pts',(7.80301783214186,31.9037535793997,54.2268765483943));
#89240=CARTESIAN_POINT('Ctrl Pts',(7.80693336842903,31.930922727748,54.2937783650575));
#89241=CARTESIAN_POINT('Ctrl Pts',(7.8108489047162,31.9545941801382,54.3621950395487));
#89242=CARTESIAN_POINT('Ctrl Pts',(7.81476444100337,31.9746063348883,54.4317329987417));
#89243=CARTESIAN_POINT('Ctrl Pts',(7.81867638568829,31.994600133098,54.5012071728815));
#89244=CARTESIAN_POINT('Ctrl Pts',(7.8225883303732,32.0109411715262,54.5718001425371));
#89245=CARTESIAN_POINT('Ctrl Pts',(7.82650027505812,32.0235168926669,54.643100928004));
#89246=CARTESIAN_POINT('Ctrl Pts',(7.83040988908265,32.0360851214381,54.7143592338528));
#89247=CARTESIAN_POINT('Ctrl Pts',(7.83431950310718,32.0448924077463,54.7863240593764));
#89248=CARTESIAN_POINT('Ctrl Pts',(7.83822911713171,32.0498770841231,54.8585733317694));
#89249=CARTESIAN_POINT('Ctrl Pts',(7.8407945049337,32.0531479000896,54.9059814393055));
#89250=CARTESIAN_POINT('Ctrl Pts',(7.84335989273569,32.0547738811628,54.9535117905185));
#89251=CARTESIAN_POINT('Ctrl Pts',(7.84592528053768,32.054749734871,55.0010438138966));
#89252=CARTESIAN_POINT('Origin',(-1.54592528053767,30.,55.));
#89253=CARTESIAN_POINT('',(6.69398930495604,28.7479524050421,56.6292250864936));
#89254=CARTESIAN_POINT('',(6.75200712216955,28.7479524050421,56.6292250864936));
#89255=CARTESIAN_POINT('',(-1.54592528053767,28.7479524050421,56.6292250864936));
#89256=CARTESIAN_POINT('',(7.20407471942299,32.054749359036,55.0016229729599));
#89257=CARTESIAN_POINT('Ctrl Pts',(6.75200712216955,28.7479524050421,56.6292250864936));
#89258=CARTESIAN_POINT('Ctrl Pts',(6.75587000514611,28.6914451856499,56.5857997005698));
#89259=CARTESIAN_POINT('Ctrl Pts',(6.75973288812266,28.6372603557193,56.5394776390901));
#89260=CARTESIAN_POINT('Ctrl Pts',(6.76359577109921,28.5856936487085,56.4905485926988));
#89261=CARTESIAN_POINT('Ctrl Pts',(6.76746492126687,28.5340432792079,56.4415401631923));
#89262=CARTESIAN_POINT('Ctrl Pts',(6.77133407143453,28.4850198364317,56.3899166654894));
#89263=CARTESIAN_POINT('Ctrl Pts',(6.77520322160219,28.4388799193048,56.336002116821));
#89264=CARTESIAN_POINT('Ctrl Pts',(6.77582786296206,28.4314310224336,56.3272980718661));
#89265=CARTESIAN_POINT('Ctrl Pts',(6.77645250432192,28.4240571888272,56.318534376648));
#89266=CARTESIAN_POINT('Ctrl Pts',(6.77707714568178,28.4167593915148,56.3097124639185));
#89267=CARTESIAN_POINT('Ctrl Pts',(6.78094621902979,28.3715563119641,56.2550689042481));
#89268=CARTESIAN_POINT('Ctrl Pts',(6.78481529237779,28.3290969431629,56.1979753737612));
#89269=CARTESIAN_POINT('Ctrl Pts',(6.78868436572579,28.2896574231043,56.1387387023184));
#89270=CARTESIAN_POINT('Ctrl Pts',(6.79254767412137,28.2502766682685,56.0795902940234));
#89271=CARTESIAN_POINT('Ctrl Pts',(6.79641098251694,28.2139070976231,56.0183054844465));
#89272=CARTESIAN_POINT('Ctrl Pts',(6.80027429091252,28.1807846665721,55.9552241271664));
#89273=CARTESIAN_POINT('Ctrl Pts',(6.80413306740522,28.1477010902086,55.8922167682719));
#89274=CARTESIAN_POINT('Ctrl Pts',(6.80799184389793,28.1178573120209,55.8274174758217));
#89275=CARTESIAN_POINT('Ctrl Pts',(6.81185062039063,28.0914450656736,55.7611935530194));
#89276=CARTESIAN_POINT('Ctrl Pts',(6.81570696597863,28.0650494581894,55.6950113491521));
#89277=CARTESIAN_POINT('Ctrl Pts',(6.81956331156663,28.0420812731967,55.6274067456564));
#89278=CARTESIAN_POINT('Ctrl Pts',(6.82341965715463,28.022684873006,55.5587686919118));
#89279=CARTESIAN_POINT('Ctrl Pts',(6.82727486339976,28.0032942034092,55.4901509170234));
#89280=CARTESIAN_POINT('Ctrl Pts',(6.83113006964489,27.9874733556432,55.4205007652727));
#89281=CARTESIAN_POINT('Ctrl Pts',(6.83498527589001,27.9753168606364,55.3502224260051));
#89282=CARTESIAN_POINT('Ctrl Pts',(6.83884063274106,27.963159890729,55.2799413412725));
#89283=CARTESIAN_POINT('Ctrl Pts',(6.8426959895921,27.9546676384162,55.209032499354));
#89284=CARTESIAN_POINT('Ctrl Pts',(6.84655134644315,27.9498832308868,55.1379086491153));
#89285=CARTESIAN_POINT('Ctrl Pts',(6.85041073891151,27.9450938152508,55.0667103495707));
#89286=CARTESIAN_POINT('Ctrl Pts',(6.85427013137987,27.9440200248333,54.9952970781169));
#89287=CARTESIAN_POINT('Ctrl Pts',(6.85812952384823,27.9466528919666,54.9240841490138));
#89288=CARTESIAN_POINT('Ctrl Pts',(6.86199110145147,27.9492872497931,54.8528309001307));
#89289=CARTESIAN_POINT('Ctrl Pts',(6.86585267905471,27.9556323997215,54.7817787034945));
#89290=CARTESIAN_POINT('Ctrl Pts',(6.86971425665795,27.9656274785321,54.7113375563115));
#89291=CARTESIAN_POINT('Ctrl Pts',(6.87358259077263,27.9756400454968,54.6407731599112));
#89292=CARTESIAN_POINT('Ctrl Pts',(6.87745092488731,27.9893151983316,54.570822424443));
#89293=CARTESIAN_POINT('Ctrl Pts',(6.881319259002,28.006541124023,54.5018842782159));
#89294=CARTESIAN_POINT('Ctrl Pts',(6.88361697817478,28.016773006419,54.4609362898504));
#89295=CARTESIAN_POINT('Ctrl Pts',(6.88591469734756,28.0282566940931,54.4203452700944));
#89296=CARTESIAN_POINT('Ctrl Pts',(6.88821241652034,28.0409606653552,54.3801916039498));
#89297=CARTESIAN_POINT('Ctrl Pts',(6.89208148986834,28.0623525731244,54.3125778235781));
#89298=CARTESIAN_POINT('Ctrl Pts',(6.89595056321633,28.0872908982648,54.2459403779374));
#89299=CARTESIAN_POINT('Ctrl Pts',(6.89981963656433,28.1156676269756,54.1806776760809));
#89300=CARTESIAN_POINT('Ctrl Pts',(6.90368294495989,28.1440020741175,54.1155122162092));
#89301=CARTESIAN_POINT('Ctrl Pts',(6.90754625335546,28.1757645631943,54.051717876011));
#89302=CARTESIAN_POINT('Ctrl Pts',(6.91140956175102,28.2107975421477,53.9896772162743));
#89303=CARTESIAN_POINT('Ctrl Pts',(6.9152683382437,28.2457894252211,53.9277093341199));
#89304=CARTESIAN_POINT('Ctrl Pts',(6.91912711473639,28.284043939903,53.8674914671293));
#89305=CARTESIAN_POINT('Ctrl Pts',(6.92298589122907,28.3253564882268,53.8093839111721));
#89306=CARTESIAN_POINT('Ctrl Pts',(6.92684223681705,28.3666430109778,53.7513129611006));
#89307=CARTESIAN_POINT('Ctrl Pts',(6.93069858240503,28.4109834644791,53.6953500794837));
#89308=CARTESIAN_POINT('Ctrl Pts',(6.93455492799301,28.4581293723475,53.6418275035614));
#89309=CARTESIAN_POINT('Ctrl Pts',(6.93841013423811,28.5052613511338,53.5883207406838));
#89310=CARTESIAN_POINT('Ctrl Pts',(6.94226534048321,28.5551968178432,53.5372532164894));
#89311=CARTESIAN_POINT('Ctrl Pts',(6.94612054672832,28.6076474655815,53.4889235683135));
#89312=CARTESIAN_POINT('Ctrl Pts',(6.94997590357933,28.6601001623354,53.4405920321113));
#89313=CARTESIAN_POINT('Ctrl Pts',(6.95383126043035,28.715067876452,53.3949989118376));
#89314=CARTESIAN_POINT('Ctrl Pts',(6.95768661728136,28.7722272302686,53.3524043006835));
#89315=CARTESIAN_POINT('Ctrl Pts',(6.96154600974969,28.8294464159729,53.3097651033713));
#89316=CARTESIAN_POINT('Ctrl Pts',(6.96540540221802,28.8888614306154,53.2701309716089));
#89317=CARTESIAN_POINT('Ctrl Pts',(6.96926479468635,28.950118486855,53.2337196228072));
#89318=CARTESIAN_POINT('Ctrl Pts',(6.97312637228955,29.0114102259965,53.1972876584011));
#89319=CARTESIAN_POINT('Ctrl Pts',(6.97698794989275,29.0745456527526,53.1640823355941));
#89320=CARTESIAN_POINT('Ctrl Pts',(6.98084952749596,29.1391473005867,53.1342748883041));
#89321=CARTESIAN_POINT('Ctrl Pts',(6.9847178616106,29.2038619804034,53.1044152876251));
#89322=CARTESIAN_POINT('Ctrl Pts',(6.98858619572524,29.2700475519769,53.0779656125225));
#89323=CARTESIAN_POINT('Ctrl Pts',(6.99245452983988,29.337308214895,53.0550482884004));
#89324=CARTESIAN_POINT('Ctrl Pts',(6.99475224901289,29.3772598090944,53.0414358202245));
#89325=CARTESIAN_POINT('Ctrl Pts',(6.99704996818589,29.4175904326409,53.029068655143));
#89326=CARTESIAN_POINT('Ctrl Pts',(6.9993476873589,29.4582154543603,53.0179639083493));
#89327=CARTESIAN_POINT('Ctrl Pts',(7.00321676070842,29.5266229389234,52.9992648957034));
#89328=CARTESIAN_POINT('Ctrl Pts',(7.00708583405794,29.5961336115655,52.984074911664));
#89329=CARTESIAN_POINT('Ctrl Pts',(7.01095490740746,29.6663541686804,52.9725192918937));
#89330=CARTESIAN_POINT('Ctrl Pts',(7.01481821580455,29.7364700965639,52.9609808900959));
#89331=CARTESIAN_POINT('Ctrl Pts',(7.01868152420164,29.8072933339145,52.9530661817184));
#89332=CARTESIAN_POINT('Ctrl Pts',(7.02254483259873,29.8784170241721,52.9488502876463));
#89333=CARTESIAN_POINT('Ctrl Pts',(7.02640360909295,29.9494572818834,52.9446393390821));
#89334=CARTESIAN_POINT('Ctrl Pts',(7.03026238558717,30.0207968098355,52.9441186148241));
#89335=CARTESIAN_POINT('Ctrl Pts',(7.03412116208139,30.0920219411853,52.9473116347481));
#89336=CARTESIAN_POINT('Ctrl Pts',(7.0379775076709,30.163202203,52.9505026431725));
#89337=CARTESIAN_POINT('Ctrl Pts',(7.04183385326041,30.2342677270393,52.9574027324669));
#89338=CARTESIAN_POINT('Ctrl Pts',(7.04569019884992,30.3048046216598,52.9679833403451));
#89339=CARTESIAN_POINT('Ctrl Pts',(7.04954540509655,30.3753206764185,52.9785608222224));
#89340=CARTESIAN_POINT('Ctrl Pts',(7.05340061134318,30.4453079316725,52.9928165918795));
#89341=CARTESIAN_POINT('Ctrl Pts',(7.05725581758981,30.5143591218829,53.0106704003017));
#89342=CARTESIAN_POINT('Ctrl Pts',(7.06111117444235,30.5834130096188,53.0285249061934));
#89343=CARTESIAN_POINT('Ctrl Pts',(7.0649665312949,30.6515302899424,53.0499776061749));
#89344=CARTESIAN_POINT('Ctrl Pts',(7.06882188814744,30.7183170588043,53.0748978817915));
#89345=CARTESIAN_POINT('Ctrl Pts',(7.07268128061728,30.7851737371063,53.0998442428521));
#89346=CARTESIAN_POINT('Ctrl Pts',(7.07654067308711,30.8506966676963,53.1282652550816));
#89347=CARTESIAN_POINT('Ctrl Pts',(7.08040006555695,30.914511055146,53.1599817684284));
#89348=CARTESIAN_POINT('Ctrl Pts',(7.08426164316165,30.978361573423,53.1917162392284));
#89349=CARTESIAN_POINT('Ctrl Pts',(7.08812322076636,31.0405011994903,53.2267496868237));
#89350=CARTESIAN_POINT('Ctrl Pts',(7.09198479837106,31.1005813479816,53.2648578562622));
#89351=CARTESIAN_POINT('Ctrl Pts',(7.09585313248718,31.1607666172941,53.3030327026675));
#89352=CARTESIAN_POINT('Ctrl Pts',(7.09972146660329,31.2188848184593,53.344292730476));
#89353=CARTESIAN_POINT('Ctrl Pts',(7.10358980071941,31.2746184286335,53.3883718096634));
#89354=CARTESIAN_POINT('Ctrl Pts',(7.10588751987876,31.3077231657305,53.4145539701839));
#89355=CARTESIAN_POINT('Ctrl Pts',(7.10818523903811,31.3399872413693,53.4417299774308));
#89356=CARTESIAN_POINT('Ctrl Pts',(7.11048295819746,31.3713503754222,53.4698380117356));
#89357=CARTESIAN_POINT('Ctrl Pts',(7.11438261491519,31.4245794464778,53.5175425731711));
#89358=CARTESIAN_POINT('Ctrl Pts',(7.11828227163292,31.475438208622,53.5681375184189));
#89359=CARTESIAN_POINT('Ctrl Pts',(7.12218192835065,31.523590769643,53.6213525725703));
#89360=CARTESIAN_POINT('Ctrl Pts',(7.12598698948115,31.5705752740591,53.6732767671252));
#89361=CARTESIAN_POINT('Ctrl Pts',(7.12979205061164,31.6149830001411,53.7276950180236));
#89362=CARTESIAN_POINT('Ctrl Pts',(7.13359711174214,31.6565353095011,53.7843156944025));
#89363=CARTESIAN_POINT('Ctrl Pts',(7.13739855500299,31.6980481107339,53.8408825355814));
#89364=CARTESIAN_POINT('Ctrl Pts',(7.14119999826383,31.7367105809646,53.8996472498017));
#89365=CARTESIAN_POINT('Ctrl Pts',(7.14500144152468,31.7722833964258,53.9602841132052));
#89366=CARTESIAN_POINT('Ctrl Pts',(7.14880063065913,31.8078351184189,54.0208850210137));
#89367=CARTESIAN_POINT('Ctrl Pts',(7.15259981979358,31.8403005656675,54.0833554448163));
#89368=CARTESIAN_POINT('Ctrl Pts',(7.15639900892804,31.8694840246935,54.1473411913808));
#89369=CARTESIAN_POINT('Ctrl Pts',(7.16037198480262,31.9000024260006,54.2142538452185));
#89370=CARTESIAN_POINT('Ctrl Pts',(7.16434496067719,31.9269310579137,54.2828232869357));
#89371=CARTESIAN_POINT('Ctrl Pts',(7.16831793655177,31.9501011079919,54.3526181720895));
#89372=CARTESIAN_POINT('Ctrl Pts',(7.1721185069018,31.9722657040316,54.4193843391825));
#89373=CARTESIAN_POINT('Ctrl Pts',(7.17591907725182,31.9909910752409,54.4872712685952));
#89374=CARTESIAN_POINT('Ctrl Pts',(7.17971964760184,32.0061804532204,54.5558856547957));
#89375=CARTESIAN_POINT('Ctrl Pts',(7.18352169694533,32.0213757421524,54.6245267423119));
#89376=CARTESIAN_POINT('Ctrl Pts',(7.18732374628882,32.0330322152166,54.6938953556266));
#89377=CARTESIAN_POINT('Ctrl Pts',(7.19112579563232,32.0411045496009,54.7635898054263));
#89378=CARTESIAN_POINT('Ctrl Pts',(7.19493249872834,32.0491867646163,54.8333695620416));
#89379=CARTESIAN_POINT('Ctrl Pts',(7.19873920182436,32.053676062702,54.9034754508831));
#89380=CARTESIAN_POINT('Ctrl Pts',(7.20254590492038,32.0545791584104,54.973503880934));
#89381=CARTESIAN_POINT('Ctrl Pts',(7.20305550975458,32.0547000561866,54.9828786142887));
#89382=CARTESIAN_POINT('Ctrl Pts',(7.20356511458878,32.0547567608594,54.9922519653911));
#89383=CARTESIAN_POINT('Ctrl Pts',(7.20407471942298,32.054749359036,55.0016229729599));
#89384=CARTESIAN_POINT('Ctrl Pts',(7.20407471946233,32.0547493590354,55.0016229736834));
#89385=CARTESIAN_POINT('Ctrl Pts',(7.20992255598689,32.0546644213158,55.1091575115331));
#89386=CARTESIAN_POINT('Ctrl Pts',(7.21577039251145,32.046135906768,55.2163661668599));
#89387=CARTESIAN_POINT('Ctrl Pts',(7.22161822903602,32.0293269300152,55.3222262770401));
#89388=CARTESIAN_POINT('Ctrl Pts',(7.22548730238329,32.0182056950634,55.3922659454058));
#89389=CARTESIAN_POINT('Ctrl Pts',(7.22935637573056,32.0034324231375,55.461866373971));
#89390=CARTESIAN_POINT('Ctrl Pts',(7.23322544907782,31.9850548085864,55.5306175359031));
#89391=CARTESIAN_POINT('Ctrl Pts',(7.23708875747264,31.9667045768386,55.5992662580145));
#89392=CARTESIAN_POINT('Ctrl Pts',(7.24095206586746,31.9447607871872,55.6670677598202));
#89393=CARTESIAN_POINT('Ctrl Pts',(7.24481537426228,31.9193224755962,55.733620335849));
#89394=CARTESIAN_POINT('Ctrl Pts',(7.24867415075418,31.8939140047392,55.8000948415345));
#89395=CARTESIAN_POINT('Ctrl Pts',(7.25253292724609,31.865019327127,55.8653228799985));
#89396=CARTESIAN_POINT('Ctrl Pts',(7.256391703738,31.83278730781,55.9289177826001));
#89397=CARTESIAN_POINT('Ctrl Pts',(7.26024804932519,31.8005755936255,55.9924726224643));
#89398=CARTESIAN_POINT('Ctrl Pts',(7.26410439491237,31.7650309279952,56.054395935349));
#89399=CARTESIAN_POINT('Ctrl Pts',(7.26796074049956,31.7263497324162,56.1143222890557));
#89400=CARTESIAN_POINT('Ctrl Pts',(7.27181594674385,31.687679965052,56.1742309377452));
#89401=CARTESIAN_POINT('Ctrl Pts',(7.27567115298815,31.6458757707532,56.2321433906354));
#89402=CARTESIAN_POINT('Ctrl Pts',(7.27952635923244,31.6011779466979,56.2877215325948));
#89403=CARTESIAN_POINT('Ctrl Pts',(7.28338171608263,31.5564783764959,56.3433018457469));
#89404=CARTESIAN_POINT('Ctrl Pts',(7.28723707293281,31.5088852582695,56.3965472897482));
#89405=CARTESIAN_POINT('Ctrl Pts',(7.291092429783,31.4586797915564,56.4471526623701));
#89406=CARTESIAN_POINT('Ctrl Pts',(7.29495182225048,31.4084217719779,56.4978110064613));
#89407=CARTESIAN_POINT('Ctrl Pts',(7.29881121471797,31.3555462880924,56.5458234170168));
#89408=CARTESIAN_POINT('Ctrl Pts',(7.30267060718546,31.300370900928,56.5909220856219));
#89409=CARTESIAN_POINT('Ctrl Pts',(7.30653218478781,31.2451642742193,56.6360462884721));
#89410=CARTESIAN_POINT('Ctrl Pts',(7.31039376239016,31.1876555438217,56.6782531777251));
#89411=CARTESIAN_POINT('Ctrl Pts',(7.31425533999251,31.1281925858735,56.717317399807));
#89412=CARTESIAN_POINT('Ctrl Pts',(7.31812367410629,31.0686255869876,56.7564499716388));
#89413=CARTESIAN_POINT('Ctrl Pts',(7.32199200822008,31.0070979533721,56.7924286527873));
#89414=CARTESIAN_POINT('Ctrl Pts',(7.32586034233386,30.9439829351717,56.8250736370362));
#89415=CARTESIAN_POINT('Ctrl Pts',(7.3281580615141,30.9064937774064,56.8444641561179));
#89416=CARTESIAN_POINT('Ctrl Pts',(7.33045578069434,30.8684449854165,56.8626794081664));
#89417=CARTESIAN_POINT('Ctrl Pts',(7.33275349987458,30.8299177134289,56.8796899083192));
#89418=CARTESIAN_POINT('Ctrl Pts',(7.33662257323247,30.7650425786077,56.9083334751708));
#89419=CARTESIAN_POINT('Ctrl Pts',(7.34049164659037,30.698555734578,56.9336705787696));
#89420=CARTESIAN_POINT('Ctrl Pts',(7.34436071994826,30.6308275304466,56.9555189053882));
#89421=CARTESIAN_POINT('Ctrl Pts',(7.34822402835375,30.5632002419187,56.9773346778132));
#89422=CARTESIAN_POINT('Ctrl Pts',(7.35208733675924,30.494335723326,56.9956718438268));
#89423=CARTESIAN_POINT('Ctrl Pts',(7.35595064516473,30.4246251784845,57.0103957372361));
#89424=CARTESIAN_POINT('Ctrl Pts',(7.35980942166735,30.3549964084809,57.0251023585957));
#89425=CARTESIAN_POINT('Ctrl Pts',(7.36366819816997,30.2845240565464,57.0362040267317));
#89426=CARTESIAN_POINT('Ctrl Pts',(7.36752697467258,30.2136137189081,57.0436160944743));
#89427=CARTESIAN_POINT('Ctrl Pts',(7.37138332027049,30.1427480524949,57.0510234928532));
#89428=CARTESIAN_POINT('Ctrl Pts',(7.37523966586839,30.0714454298039,57.0547458518868));
#89429=CARTESIAN_POINT('Ctrl Pts',(7.3790960114663,30.0001193983105,57.054749996531));
#89430=CARTESIAN_POINT('Ctrl Pts',(7.38295121772131,29.9288144398266,57.0547541399507));
#89431=CARTESIAN_POINT('Ctrl Pts',(7.38680642397632,29.8574865717917,57.051042249844));
#89432=CARTESIAN_POINT('Ctrl Pts',(7.39066163023133,29.786550459199,57.0436332489055));
#89433=CARTESIAN_POINT('Ctrl Pts',(7.39451698709222,29.7156115754456,57.03622395853));
#89434=CARTESIAN_POINT('Ctrl Pts',(7.39837234395311,29.6450649604476,57.0251173232309));
#89435=CARTESIAN_POINT('Ctrl Pts',(7.402227700814,29.5753195404234,57.0103840602616));
#89436=CARTESIAN_POINT('Ctrl Pts',(7.40608709329209,29.5055011139756,56.9956353751636));
#89437=CARTESIAN_POINT('Ctrl Pts',(7.40994648577017,29.4364860329173,56.977252584949));
#89438=CARTESIAN_POINT('Ctrl Pts',(7.41380587824825,29.3686715284612,56.9553572368047));
#89439=CARTESIAN_POINT('Ctrl Pts',(7.41766745586116,29.3008186283674,56.933449491816));
#89440=CARTESIAN_POINT('Ctrl Pts',(7.42152903347407,29.2341681121487,56.9080254031045));
#89441=CARTESIAN_POINT('Ctrl Pts',(7.42539061108697,29.1690979846837,56.8792550128823));
#89442=CARTESIAN_POINT('Ctrl Pts',(7.42925894521113,29.1039140055518,56.8504342837871));
#89443=CARTESIAN_POINT('Ctrl Pts',(7.43312727933529,29.0403163695113,56.8182557830016));
#89444=CARTESIAN_POINT('Ctrl Pts',(7.43699561345945,28.9786585770717,56.782935573797));
#89445=CARTESIAN_POINT('Ctrl Pts',(7.43929333254401,28.9420349861788,56.761956021319));
#89446=CARTESIAN_POINT('Ctrl Pts',(7.44159105162857,28.906095262753,56.7398688732154));
#89447=CARTESIAN_POINT('Ctrl Pts',(7.44388877071313,28.8709081934411,56.7167263191498));
#89448=CARTESIAN_POINT('Ctrl Pts',(7.44663026314124,28.8289252179179,56.6891140939806));
#89449=CARTESIAN_POINT('Ctrl Pts',(7.44937175556935,28.7878975561809,56.659922643773));
#89450=CARTESIAN_POINT('Ctrl Pts',(7.45211324799746,28.7479524050421,56.6292250864936));
#89451=CARTESIAN_POINT('',(7.1459252805008,32.0547492461588,54.9982399120147));
#89452=CARTESIAN_POINT('Ctrl Pts',(7.14592528053769,32.0547492461594,54.9982399126965));
#89453=CARTESIAN_POINT('Ctrl Pts',(7.14975890798128,32.0548099310451,55.0690842525566));
#89454=CARTESIAN_POINT('Ctrl Pts',(7.15359253542487,32.051202432858,55.1399937211669));
#89455=CARTESIAN_POINT('Ctrl Pts',(7.15742616286845,32.0439332342796,55.2105575843025));
#89456=CARTESIAN_POINT('Ctrl Pts',(7.16125834634856,32.0366667736974,55.2810948690491));
#89457=CARTESIAN_POINT('Ctrl Pts',(7.16509052982867,32.0257413995781,55.3512863175634));
#89458=CARTESIAN_POINT('Ctrl Pts',(7.16892271330877,32.0112155594184,55.4207250123931));
#89459=CARTESIAN_POINT('Ctrl Pts',(7.17275477349921,31.9966901865866,55.4901614732292));
#89460=CARTESIAN_POINT('Ctrl Pts',(7.17658683368964,31.9785646802737,55.5588447472066));
#89461=CARTESIAN_POINT('Ctrl Pts',(7.18041889388008,31.9569484900965,55.6263786152232));
#89462=CARTESIAN_POINT('Ctrl Pts',(7.184254856409,31.9353102872978,55.6939812556491));
#89463=CARTESIAN_POINT('Ctrl Pts',(7.18809081893792,31.910174452913,55.7604316831496));
#89464=CARTESIAN_POINT('Ctrl Pts',(7.19192678146684,31.8816998964897,55.8253502662812));
#89465=CARTESIAN_POINT('Ctrl Pts',(7.19576473620229,31.8532105518101,55.8903025648688));
#89466=CARTESIAN_POINT('Ctrl Pts',(7.19960269093774,31.8213792547125,55.9537209954185));
#89467=CARTESIAN_POINT('Ctrl Pts',(7.20344064567319,31.7864112720573,56.0152498852828));
#89468=CARTESIAN_POINT('Ctrl Pts',(7.20728565488565,31.751379015369,56.076891870316));
#89469=CARTESIAN_POINT('Ctrl Pts',(7.21113066409811,31.7131988248763,56.1366369637702));
#89470=CARTESIAN_POINT('Ctrl Pts',(7.21497567331057,31.672119382911,56.1941584198897));
#89471=CARTESIAN_POINT('Ctrl Pts',(7.21791465037584,31.6407198384317,56.2381256072108));
#89472=CARTESIAN_POINT('Ctrl Pts',(7.2208536274411,31.6076273168153,56.2807942302441));
#89473=CARTESIAN_POINT('Ctrl Pts',(7.22379260450636,31.5729677245609,56.3220325638916));
#89474=CARTESIAN_POINT('Ctrl Pts',(7.22766167785587,31.527339432227,56.3763215679058));
#89475=CARTESIAN_POINT('Ctrl Pts',(7.23153075120538,31.478807891512,56.4283519319452));
#89476=CARTESIAN_POINT('Ctrl Pts',(7.23539982455489,31.4276252989438,56.4777968630078));
#89477=CARTESIAN_POINT('Ctrl Pts',(7.23926313295197,31.3765189688769,56.5271681206996));
#89478=CARTESIAN_POINT('Ctrl Pts',(7.24312644134905,31.3227697743101,56.5739612573854));
#89479=CARTESIAN_POINT('Ctrl Pts',(7.24698974974612,31.2666696204287,56.6178830721603));
#89480=CARTESIAN_POINT('Ctrl Pts',(7.25084852624033,31.2106352755437,56.6617533638939));
#89481=CARTESIAN_POINT('Ctrl Pts',(7.25470730273454,31.1522558299576,56.7027587261679));
#89482=CARTESIAN_POINT('Ctrl Pts',(7.25856607922875,31.0918581402454,56.740644525479));
#89483=CARTESIAN_POINT('Ctrl Pts',(7.26242242481826,31.0314984991293,56.7785064579587));
#89484=CARTESIAN_POINT('Ctrl Pts',(7.26627877040776,30.969123546933,56.8132524689203));
#89485=CARTESIAN_POINT('Ctrl Pts',(7.27013511599726,30.9050899488404,56.8446706337469));
#89486=CARTESIAN_POINT('Ctrl Pts',(7.27399032224388,30.8410752692349,56.8760795161941));
#89487=CARTESIAN_POINT('Ctrl Pts',(7.27784552849051,30.7754033524808,56.9041622905641));
#89488=CARTESIAN_POINT('Ctrl Pts',(7.28170073473713,30.7084548126927,56.9287533126018));
#89489=CARTESIAN_POINT('Ctrl Pts',(7.28555609158966,30.6415036575203,56.9533452953024));
#89490=CARTESIAN_POINT('Ctrl Pts',(7.2894114484422,30.5732762370567,56.9744450894259));
#89491=CARTESIAN_POINT('Ctrl Pts',(7.29326680529474,30.5041708253421,56.9919360786365));
#89492=CARTESIAN_POINT('Ctrl Pts',(7.29712619776457,30.4349930771345,57.0094453766422));
#89493=CARTESIAN_POINT('Ctrl Pts',(7.30098559023439,30.364935974961,57.0233382094805));
#89494=CARTESIAN_POINT('Ctrl Pts',(7.30484498270422,30.2944096805196,57.0335487460389));
#89495=CARTESIAN_POINT('Ctrl Pts',(7.30870656030892,30.2238434550615,57.0437650636625));
#89496=CARTESIAN_POINT('Ctrl Pts',(7.31256813791362,30.1528079924837,57.0502948901935));
#89497=CARTESIAN_POINT('Ctrl Pts',(7.31642971551831,30.0817175522559,57.0531244005548));
#89498=CARTESIAN_POINT('Ctrl Pts',(7.32029804963442,30.0105027267586,57.0559588616436));
#89499=CARTESIAN_POINT('Ctrl Pts',(7.32416638375053,29.9392332174624,57.0550800863142));
#89500=CARTESIAN_POINT('Ctrl Pts',(7.32803471786664,29.8683215534489,57.0505263590634));
#89501=CARTESIAN_POINT('Ctrl Pts',(7.33033243702606,29.8262013321494,57.047821529016));
#89502=CARTESIAN_POINT('Ctrl Pts',(7.33263015618549,29.7842072533363,57.0438211176024));
#89503=CARTESIAN_POINT('Ctrl Pts',(7.33492787534492,29.7424240587483,57.0385416838977));
#89504=CARTESIAN_POINT('Ctrl Pts',(7.33879679455239,29.6720691577032,57.0296521281915));
#89505=CARTESIAN_POINT('Ctrl Pts',(7.34266571375985,29.6020371950836,57.0170987141508));
#89506=CARTESIAN_POINT('Ctrl Pts',(7.34653463296732,29.5327394571435,57.000916077098));
#89507=CARTESIAN_POINT('Ctrl Pts',(7.35048283899703,29.462021581657,56.9844018048266));
#89508=CARTESIAN_POINT('Ctrl Pts',(7.35443104502674,29.3920688738398,56.9641078751369));
#89509=CARTESIAN_POINT('Ctrl Pts',(7.35837925105645,29.3233131428259,56.9401269184844));
#89510=CARTESIAN_POINT('Ctrl Pts',(7.36223788239855,29.2561173033377,56.9166900283484));
#89511=CARTESIAN_POINT('Ctrl Pts',(7.36609651374064,29.1900651880705,56.889731810428));
#89512=CARTESIAN_POINT('Ctrl Pts',(7.36995514508274,29.1255476136902,56.8593898425497));
#89513=CARTESIAN_POINT('Ctrl Pts',(7.37394813845626,29.0587834623276,56.8279913320583));
#89514=CARTESIAN_POINT('Ctrl Pts',(7.37794113182978,28.9936632172819,56.7929692017413));
#89515=CARTESIAN_POINT('Ctrl Pts',(7.3819341252033,28.9305982714506,56.7545305655575));
#89516=CARTESIAN_POINT('Ctrl Pts',(7.38592711857682,28.8675333256194,56.7160919293738));
#89517=CARTESIAN_POINT('Ctrl Pts',(7.38992011195034,28.8065241834037,56.674237070926));
#89518=CARTESIAN_POINT('Ctrl Pts',(7.39391310532386,28.7479524050421,56.6292250864936));
#89519=CARTESIAN_POINT('Ctrl Pts',(6.69398930495604,28.7479524050421,56.6292250864936));
#89520=CARTESIAN_POINT('Ctrl Pts',(6.69784740484003,28.6915069530229,56.5858471683454));
#89521=CARTESIAN_POINT('Ctrl Pts',(6.70170550472402,28.6372599899261,56.5394875233192));
#89522=CARTESIAN_POINT('Ctrl Pts',(6.70556360460801,28.5855382786981,56.4904011545458));
#89523=CARTESIAN_POINT('Ctrl Pts',(6.70941957225292,28.5338451522805,56.4413419141198));
#89524=CARTESIAN_POINT('Ctrl Pts',(6.71327553989783,28.4846748602865,56.3895592738365));
#89525=CARTESIAN_POINT('Ctrl Pts',(6.71713150754274,28.4383199524028,56.3353475171044));
#89526=CARTESIAN_POINT('Ctrl Pts',(6.72098663402215,28.3919751566759,56.2811475864723));
#89527=CARTESIAN_POINT('Ctrl Pts',(6.72484176050156,28.3484448409394,56.2245199608754));
#89528=CARTESIAN_POINT('Ctrl Pts',(6.72869688698097,28.3079824598838,56.1657933806808));
#89529=CARTESIAN_POINT('Ctrl Pts',(6.73255246205531,28.2675153704954,56.1070599668723));
#89530=CARTESIAN_POINT('Ctrl Pts',(6.73640803712965,28.2301171979976,56.0462275150466));
#89531=CARTESIAN_POINT('Ctrl Pts',(6.74026361220398,28.1959981164053,55.9836537838522));
#89532=CARTESIAN_POINT('Ctrl Pts',(6.74412340630836,28.1618416994149,55.9210115802648));
#89533=CARTESIAN_POINT('Ctrl Pts',(6.74798320041274,28.1309717656873,55.8566247226886));
#89534=CARTESIAN_POINT('Ctrl Pts',(6.75184299451711,28.1035520965734,55.7908747764904));
#89535=CARTESIAN_POINT('Ctrl Pts',(6.75570524152721,28.076115002213,55.7250830460894));
#89536=CARTESIAN_POINT('Ctrl Pts',(6.75956748853731,28.052132698729,55.6579269606755));
#89537=CARTESIAN_POINT('Ctrl Pts',(6.76342973554741,28.0317195237508,55.5898046535219));
#89538=CARTESIAN_POINT('Ctrl Pts',(6.76729847175235,28.0112720513625,55.5215678899592));
#89539=CARTESIAN_POINT('Ctrl Pts',(6.77116720795728,27.9944057874356,55.4523621367241));
#89540=CARTESIAN_POINT('Ctrl Pts',(6.77503594416221,27.9811841000988,55.3825962948147));
#89541=CARTESIAN_POINT('Ctrl Pts',(6.77644113649218,27.9763817531175,55.3572561266689));
#89542=CARTESIAN_POINT('Ctrl Pts',(6.77784632882215,27.9720597274933,55.3318421154545));
#89543=CARTESIAN_POINT('Ctrl Pts',(6.77925152115212,27.9682193607167,55.3063739485233));
#89544=CARTESIAN_POINT('Ctrl Pts',(6.7831205945003,27.957645248956,55.2362495934447));
#89545=CARTESIAN_POINT('Ctrl Pts',(6.78698966784848,27.9506850681283,55.1654398123005));
#89546=CARTESIAN_POINT('Ctrl Pts',(6.79085874119666,27.9474173181755,55.094349863667));
#89547=CARTESIAN_POINT('Ctrl Pts',(6.79472204959241,27.9441544371981,55.023365839666));
#89548=CARTESIAN_POINT('Ctrl Pts',(6.79858535798816,27.9445730883938,54.952102958126));
#89549=CARTESIAN_POINT('Ctrl Pts',(6.80244866638391,27.9487003168898,54.8809740676499));
#89550=CARTESIAN_POINT('Ctrl Pts',(6.80630744287678,27.952822703888,54.8099286158204));
#89551=CARTESIAN_POINT('Ctrl Pts',(6.81016621936966,27.9606449988298,54.7390173254585));
#89552=CARTESIAN_POINT('Ctrl Pts',(6.81402499586253,27.9721422035047,54.668653776703));
#89553=CARTESIAN_POINT('Ctrl Pts',(6.8178813414507,27.9836321653116,54.5983345547132));
#89554=CARTESIAN_POINT('Ctrl Pts',(6.82173768703886,27.9987923656292,54.5285628680318));
#89555=CARTESIAN_POINT('Ctrl Pts',(6.82559403262703,28.0175460548859,54.4597464317549));
#89556=CARTESIAN_POINT('Ctrl Pts',(6.82944923887232,28.0362942034353,54.3909503270368));
#89557=CARTESIAN_POINT('Ctrl Pts',(6.83330444511761,28.0586336055317,54.3231093808666));
#89558=CARTESIAN_POINT('Ctrl Pts',(6.8371596513629,28.0844369538214,54.2566186855892));
#89559=CARTESIAN_POINT('Ctrl Pts',(6.84101500821412,28.1102413101343,54.1901253928131));
#89560=CARTESIAN_POINT('Ctrl Pts',(6.84487036506534,28.1395097034985,54.1249829077371));
#89561=CARTESIAN_POINT('Ctrl Pts',(6.84872572191656,28.1720663643886,54.0615671647367));
#89562=CARTESIAN_POINT('Ctrl Pts',(6.85258511438508,28.2046571041536,53.9980850409369));
#89563=CARTESIAN_POINT('Ctrl Pts',(6.8564445068536,28.2405427601566,53.936333700391));
#89564=CARTESIAN_POINT('Ctrl Pts',(6.86030389932212,28.2795015977718,53.8766644266159));
#89565=CARTESIAN_POINT('Ctrl Pts',(6.86416547692552,28.3184824933445,53.8169613689194));
#89566=CARTESIAN_POINT('Ctrl Pts',(6.86802705452891,28.3605397477762,53.7593431172579));
#89567=CARTESIAN_POINT('Ctrl Pts',(6.87188863213231,28.405409894687,53.704129652111));
#89568=CARTESIAN_POINT('Ctrl Pts',(6.87575696624714,28.4503585498376,53.648819581264));
#89569=CARTESIAN_POINT('Ctrl Pts',(6.87962530036197,28.4981295979932,53.5959230581633));
#89570=CARTESIAN_POINT('Ctrl Pts',(6.8834936344768,28.5484216159474,53.5457243186207));
#89571=CARTESIAN_POINT('Ctrl Pts',(6.8857913536481,28.5782941477366,53.5159071924889));
#89572=CARTESIAN_POINT('Ctrl Pts',(6.88808907281939,28.6090554407189,53.4870411428942));
#89573=CARTESIAN_POINT('Ctrl Pts',(6.89038679199069,28.6406370524378,53.4591788100837));
#89574=CARTESIAN_POINT('Ctrl Pts',(6.89425586533907,28.693816559197,53.4122621064901));
#89575=CARTESIAN_POINT('Ctrl Pts',(6.89812493868745,28.7495319885956,53.3680098732096));
#89576=CARTESIAN_POINT('Ctrl Pts',(6.90199401203584,28.8074854408002,53.3267078591601));
#89577=CARTESIAN_POINT('Ctrl Pts',(6.90585732043179,28.8653525418647,53.2854673854653));
#89578=CARTESIAN_POINT('Ctrl Pts',(6.90972062882775,28.9254506541244,53.2471686849973));
#89579=CARTESIAN_POINT('Ctrl Pts',(6.91358393722371,28.9874475937907,53.2120583938004));
#89580=CARTESIAN_POINT('Ctrl Pts',(6.91744271371679,29.0493718071612,53.1769892891755));
#89581=CARTESIAN_POINT('Ctrl Pts',(6.92130149020988,29.1131900028269,53.1451014027384));
#89582=CARTESIAN_POINT('Ctrl Pts',(6.92516026670296,29.1785411559669,53.1165980434172));
#89583=CARTESIAN_POINT('Ctrl Pts',(6.92901661229134,29.2438511399886,53.088112640293));
#89584=CARTESIAN_POINT('Ctrl Pts',(6.93287295787971,29.3106917213013,53.0630077278986));
#89585=CARTESIAN_POINT('Ctrl Pts',(6.93672930346809,29.3786787344817,53.0414399556014));
#89586=CARTESIAN_POINT('Ctrl Pts',(6.94058450971359,29.4466456611536,53.0198785554217));
#89587=CARTESIAN_POINT('Ctrl Pts',(6.9444397159591,29.5157578844699,53.0018523674691));
#89588=CARTESIAN_POINT('Ctrl Pts',(6.9482949222046,29.5856144232053,52.9874687191886));
#89589=CARTESIAN_POINT('Ctrl Pts',(6.95215027905601,29.6554736909276,52.9730845090023));
#89590=CARTESIAN_POINT('Ctrl Pts',(6.95600563590742,29.7260768555491,52.9623432168142));
#89591=CARTESIAN_POINT('Ctrl Pts',(6.95986099275883,29.7970127471481,52.9553010642934));
#89592=CARTESIAN_POINT('Ctrl Pts',(6.96372038522755,29.8680228913061,52.9482515403584));
#89593=CARTESIAN_POINT('Ctrl Pts',(6.96757977769628,29.9393659732943,52.9449089337533));
#89594=CARTESIAN_POINT('Ctrl Pts',(6.971439170165,30.0106266036311,52.9452774791239));
#89595=CARTESIAN_POINT('Ctrl Pts',(6.9753007477686,30.0819275807557,52.9456462331599));
#89596=CARTESIAN_POINT('Ctrl Pts',(6.9791623253722,30.1531455280784,52.9497302941936));
#89597=CARTESIAN_POINT('Ctrl Pts',(6.9830239029758,30.2238687213579,52.9574818585634));
#89598=CARTESIAN_POINT('Ctrl Pts',(6.98689223709084,30.294715657344,52.9652469856629));
#89599=CARTESIAN_POINT('Ctrl Pts',(6.99076057120587,30.3650656313385,52.9766923496815));
#89600=CARTESIAN_POINT('Ctrl Pts',(6.9946289053209,30.4345163633338,52.99171887115));
#89601=CARTESIAN_POINT('Ctrl Pts',(6.99692662449035,30.4757688181354,53.0006443479577));
#89602=CARTESIAN_POINT('Ctrl Pts',(6.9992243436598,30.5167042642628,53.0108323415111));
#89603=CARTESIAN_POINT('Ctrl Pts',(7.00152206282925,30.5572413556216,53.0222539005006));
#89604=CARTESIAN_POINT('Ctrl Pts',(7.00539113617725,30.6255007764713,53.0414863855086));
#89605=CARTESIAN_POINT('Ctrl Pts',(7.00926020952525,30.692897053114,53.0642945225908));
#89606=CARTESIAN_POINT('Ctrl Pts',(7.01312928287326,30.7590285452664,53.0905830130716));
#89607=CARTESIAN_POINT('Ctrl Pts',(7.01699259126884,30.8250615009292,53.1168323334765));
#89608=CARTESIAN_POINT('Ctrl Pts',(7.02085589966442,30.889832965112,53.146551535711));
#89609=CARTESIAN_POINT('Ctrl Pts',(7.02471920806,30.952955563574,53.1795953042377));
#89610=CARTESIAN_POINT('Ctrl Pts',(7.02857798455271,31.0160041152719,53.2126003103529));
#89611=CARTESIAN_POINT('Ctrl Pts',(7.03243676104541,31.0774072149769,53.2489219119856));
#89612=CARTESIAN_POINT('Ctrl Pts',(7.03629553753811,31.1367982471061,53.2883670639192));
#89613=CARTESIAN_POINT('Ctrl Pts',(7.04015188312611,31.196151864801,53.3277873666796));
#89614=CARTESIAN_POINT('Ctrl Pts',(7.04400822871411,31.2534955259851,53.3703270476572));
#89615=CARTESIAN_POINT('Ctrl Pts',(7.04786457430211,31.3084892651732,53.4157483137372));
#89616=CARTESIAN_POINT('Ctrl Pts',(7.05171978054724,31.3634667566669,53.4611561602741));
#89617=CARTESIAN_POINT('Ctrl Pts',(7.05557498679237,31.4160953301477,53.5094435925552));
#89618=CARTESIAN_POINT('Ctrl Pts',(7.0594301930375,31.4660673373388,53.5603319393387));
#89619=CARTESIAN_POINT('Ctrl Pts',(7.06328554988854,31.516041296716,53.6112222741056));
#89620=CARTESIAN_POINT('Ctrl Pts',(7.06714090673959,31.563358144965,53.6647133769486));
#89621=CARTESIAN_POINT('Ctrl Pts',(7.07099626359064,31.607747644014,53.7204902987208));
#89622=CARTESIAN_POINT('Ctrl Pts',(7.074855656059,31.6521836080304,53.7763256053117));
#89623=CARTESIAN_POINT('Ctrl Pts',(7.07871504852737,31.6936858028527,53.8344511263032));
#89624=CARTESIAN_POINT('Ctrl Pts',(7.08257444099573,31.7320253784342,53.8945201716178));
#89625=CARTESIAN_POINT('Ctrl Pts',(7.08643601859897,31.7703866613556,53.954623227199));
#89626=CARTESIAN_POINT('Ctrl Pts',(7.09029759620222,31.8055815206531,54.0166715749086));
#89627=CARTESIAN_POINT('Ctrl Pts',(7.09415917380546,31.8374268138238,54.0802933802883));
#89628=CARTESIAN_POINT('Ctrl Pts',(7.09802750792014,31.8693278259543,54.1440265032434));
#89629=CARTESIAN_POINT('Ctrl Pts',(7.10189584203482,31.8978673764082,54.2093381351131));
#89630=CARTESIAN_POINT('Ctrl Pts',(7.1057641761495,31.922910523935,54.2758365657946));
#89631=CARTESIAN_POINT('Ctrl Pts',(7.10806189532227,31.9377856920338,54.3153354080884));
#89632=CARTESIAN_POINT('Ctrl Pts',(7.11035961449504,31.9514282306982,54.355252661328));
#89633=CARTESIAN_POINT('Ctrl Pts',(7.1126573336678,31.9638183439841,54.3955042809652));
#89634=CARTESIAN_POINT('Ctrl Pts',(7.11737359945988,31.9892501148215,54.4781241846597));
#89635=CARTESIAN_POINT('Ctrl Pts',(7.12208986525197,32.0094837420675,54.562414597967));
#89636=CARTESIAN_POINT('Ctrl Pts',(7.12680613104405,32.024337058198,54.647782684545));
#89637=CARTESIAN_POINT('Ctrl Pts',(7.13145774528214,32.0389867619766,54.7319805276077));
#89638=CARTESIAN_POINT('Ctrl Pts',(7.13610935952022,32.0484026072855,54.8172267077028));
#89639=CARTESIAN_POINT('Ctrl Pts',(7.1407609737583,32.0524559155886,54.9029315856441));
#89640=CARTESIAN_POINT('Ctrl Pts',(7.14248240933913,32.0539559344585,54.9346486238136));
#89641=CARTESIAN_POINT('Ctrl Pts',(7.14420384491996,32.0547219964682,54.966428274309));
#89642=CARTESIAN_POINT('Ctrl Pts',(7.1459252805008,32.0547492461588,54.9982399120147));
#89643=CARTESIAN_POINT('Origin',(-1.54592528053767,30.,55.));
#89644=CARTESIAN_POINT('',(5.99388650947633,28.7479524050421,56.6292250864936));
#89645=CARTESIAN_POINT('',(6.05208116311818,28.7479524050421,56.6292250864936));
#89646=CARTESIAN_POINT('',(-1.54592528053767,28.7479524050421,56.6292250864936));
#89647=CARTESIAN_POINT('',(6.50407471951138,32.0547499427048,55.0004852364685));
#89648=CARTESIAN_POINT('Ctrl Pts',(6.05208116311818,28.7479524050421,56.6292250864936));
#89649=CARTESIAN_POINT('Ctrl Pts',(6.05593629750659,28.6914020110631,56.5857665212147));
#89650=CARTESIAN_POINT('Ctrl Pts',(6.059791431895,28.6371119664565,56.5393564016427));
#89651=CARTESIAN_POINT('Ctrl Pts',(6.06364656628342,28.5853961878313,56.4902662906668));
#89652=CARTESIAN_POINT('Ctrl Pts',(6.06753147914733,28.5332809375167,56.4407969896238));
#89653=CARTESIAN_POINT('Ctrl Pts',(6.07141639201125,28.4837802730513,56.388606443096));
#89654=CARTESIAN_POINT('Ctrl Pts',(6.07530130487517,28.4371775409704,56.3340103163217));
#89655=CARTESIAN_POINT('Ctrl Pts',(6.07916181998135,28.3908674801041,56.2797570603196));
#89656=CARTESIAN_POINT('Ctrl Pts',(6.08302233508754,28.3474193099307,56.2231287771434));
#89657=CARTESIAN_POINT('Ctrl Pts',(6.08688285019373,28.3070691274068,56.1644666689608));
#89658=CARTESIAN_POINT('Ctrl Pts',(6.09077996193651,28.2663364360917,56.1052484598963));
#89659=CARTESIAN_POINT('Ctrl Pts',(6.09467707367929,28.2287610480401,56.0439580900017));
#89660=CARTESIAN_POINT('Ctrl Pts',(6.09857418542207,28.1945386894449,55.9809724861527));
#89661=CARTESIAN_POINT('Ctrl Pts',(6.10247129716486,28.1603163308497,55.9179868823037));
#89662=CARTESIAN_POINT('Ctrl Pts',(6.10636840890764,28.1294471595806,55.8533065255599));
#89663=CARTESIAN_POINT('Ctrl Pts',(6.11026552065042,28.1020766226353,55.7873273881637));
#89664=CARTESIAN_POINT('Ctrl Pts',(6.11413459399864,28.0749030074016,55.7218229482382));
#89665=CARTESIAN_POINT('Ctrl Pts',(6.11800366734685,28.0510713524173,55.6547817560974));
#89666=CARTESIAN_POINT('Ctrl Pts',(6.12187274069507,28.0307555752006,55.5865781771397));
#89667=CARTESIAN_POINT('Ctrl Pts',(6.12573604909085,28.010470068666,55.5184762220988));
#89668=CARTESIAN_POINT('Ctrl Pts',(6.12959935748664,27.9936901788,55.449215779923));
#89669=CARTESIAN_POINT('Ctrl Pts',(6.13346266588243,27.9805417175088,55.3791909911608));
#89670=CARTESIAN_POINT('Ctrl Pts',(6.13732144237534,27.9674086801867,55.3092483458646));
#89671=CARTESIAN_POINT('Ctrl Pts',(6.14118021886825,27.957898699064,55.2385436101104));
#89672=CARTESIAN_POINT('Ctrl Pts',(6.14503899536116,27.9520872552484,55.1674841854739));
#89673=CARTESIAN_POINT('Ctrl Pts',(6.14889534094936,27.9462794724548,55.0964695259824));
#89674=CARTESIAN_POINT('Ctrl Pts',(6.15275168653757,27.9441656438702,55.0251011039398));
#89675=CARTESIAN_POINT('Ctrl Pts',(6.15660803212577,27.9457696122914,54.9537931096617));
#89676=CARTESIAN_POINT('Ctrl Pts',(6.16046323837111,27.9473731068262,54.8825061830636));
#89677=CARTESIAN_POINT('Ctrl Pts',(6.16431844461644,27.9526922068022,54.811280134185));
#89678=CARTESIAN_POINT('Ctrl Pts',(6.16817365086178,27.9616986453253,54.7405290959828));
#89679=CARTESIAN_POINT('Ctrl Pts',(6.17202900771301,27.9707054356903,54.6697752938497));
#89680=CARTESIAN_POINT('Ctrl Pts',(6.17588436456425,27.9833997870615,54.5994970208538));
#89681=CARTESIAN_POINT('Ctrl Pts',(6.17973972141549,27.9997017805379,54.5301015048795));
#89682=CARTESIAN_POINT('Ctrl Pts',(6.18359911388405,28.0160208382212,54.4606333487431));
#89683=CARTESIAN_POINT('Ctrl Pts',(6.1874585063526,28.0359549650723,54.3920502680835));
#89684=CARTESIAN_POINT('Ctrl Pts',(6.19131789882116,28.0593736888521,54.3247466527438));
#89685=CARTESIAN_POINT('Ctrl Pts',(6.19517947642459,28.0828056719909,54.2574049310238));
#89686=CARTESIAN_POINT('Ctrl Pts',(6.19904105402803,28.1097259961425,54.1913445667913));
#89687=CARTESIAN_POINT('Ctrl Pts',(6.20290263163146,28.139956139845,54.1269396350769));
#89688=CARTESIAN_POINT('Ctrl Pts',(6.20677096574633,28.1702391765183,54.0624220155695));
#89689=CARTESIAN_POINT('Ctrl Pts',(6.2106392998612,28.2038433657608,53.9995660400105));
#89690=CARTESIAN_POINT('Ctrl Pts',(6.21450763397607,28.2405447292237,53.9387202477021));
#89691=CARTESIAN_POINT('Ctrl Pts',(6.21680535314704,28.2623446627159,53.9025789684567));
#89692=CARTESIAN_POINT('Ctrl Pts',(6.21910307231801,28.2852364919427,53.8671463546764));
#89693=CARTESIAN_POINT('Ctrl Pts',(6.22140079148898,28.3091664896412,53.832489998866));
#89694=CARTESIAN_POINT('Ctrl Pts',(6.22526986483719,28.3494616299212,53.7741330054152));
#89695=CARTESIAN_POINT('Ctrl Pts',(6.2291389381854,28.3928604218901,53.7177502591308));
#89696=CARTESIAN_POINT('Ctrl Pts',(6.23300801153361,28.4391426714855,53.6636909180423));
#89697=CARTESIAN_POINT('Ctrl Pts',(6.23687131992938,28.4853559601326,53.6097121258351));
#89698=CARTESIAN_POINT('Ctrl Pts',(6.24073462832516,28.534443864862,53.5580502330751));
#89699=CARTESIAN_POINT('Ctrl Pts',(6.24459793672093,28.5861434868901,53.5090247075029));
#89700=CARTESIAN_POINT('Ctrl Pts',(6.24845671321384,28.6377824620215,53.4600566919447));
#89701=CARTESIAN_POINT('Ctrl Pts',(6.25231548970675,28.6920267181043,53.4137192332201));
#89702=CARTESIAN_POINT('Ctrl Pts',(6.25617426619966,28.7485749175707,53.3702967062784));
#89703=CARTESIAN_POINT('Ctrl Pts',(6.26003061178786,28.8050874934958,53.3269015341279));
#89704=CARTESIAN_POINT('Ctrl Pts',(6.26388695737606,28.8639007488455,53.2864179457088));
#89705=CARTESIAN_POINT('Ctrl Pts',(6.26774330296426,28.9246796357711,53.249090614345));
#89706=CARTESIAN_POINT('Ctrl Pts',(6.27159850920958,28.985440565802,53.2117743112017));
#89707=CARTESIAN_POINT('Ctrl Pts',(6.2754537154549,29.0481655607558,53.1776126679242));
#89708=CARTESIAN_POINT('Ctrl Pts',(6.27930892170022,29.1124913585484,53.1468065471061));
#89709=CARTESIAN_POINT('Ctrl Pts',(6.28316427855145,29.1768196692663,53.1159992228287));
#89710=CARTESIAN_POINT('Ctrl Pts',(6.28701963540268,29.2427484678953,53.0885478891027));
#89711=CARTESIAN_POINT('Ctrl Pts',(6.29087499225391,29.3098922794099,53.0646062683573));
#89712=CARTESIAN_POINT('Ctrl Pts',(6.29473438472246,29.3771063741018,53.0406395865804));
#89713=CARTESIAN_POINT('Ctrl Pts',(6.29859377719101,29.4455375620161,53.0201901150297));
#89714=CARTESIAN_POINT('Ctrl Pts',(6.30245316965956,29.5147837356099,53.0033621411805));
#89715=CARTESIAN_POINT('Ctrl Pts',(6.306314747263,29.584069115434,52.9865246395642));
#89716=CARTESIAN_POINT('Ctrl Pts',(6.31017632486643,29.6541699219019,52.9733128074614));
#89717=CARTESIAN_POINT('Ctrl Pts',(6.31403790246987,29.7246750546569,52.9637795460776));
#89718=CARTESIAN_POINT('Ctrl Pts',(6.31790623658473,29.7953035485829,52.9542296045709));
#89719=CARTESIAN_POINT('Ctrl Pts',(6.3217745706996,29.8663372969251,52.9483711240021));
#89720=CARTESIAN_POINT('Ctrl Pts',(6.32564290481447,29.9373619988214,52.9462049656043));
#89721=CARTESIAN_POINT('Ctrl Pts',(6.32794062398549,29.9795493627661,52.9449183074382));
#89722=CARTESIAN_POINT('Ctrl Pts',(6.33023834315651,30.0217335510167,52.9449333531371));
#89723=CARTESIAN_POINT('Ctrl Pts',(6.33253606232754,30.0638286364279,52.9462416238341));
#89724=CARTESIAN_POINT('Ctrl Pts',(6.33640513567577,30.1347115254729,52.948444588996));
#89725=CARTESIAN_POINT('Ctrl Pts',(6.34027420902401,30.205619072688,52.9543258278911));
#89726=CARTESIAN_POINT('Ctrl Pts',(6.34414328237225,30.2761385098526,52.9638897166714));
#89727=CARTESIAN_POINT('Ctrl Pts',(6.34800659076804,30.3465528724515,52.9734393551755));
#89728=CARTESIAN_POINT('Ctrl Pts',(6.35186989916384,30.4165797954267,52.986660686914));
#89729=CARTESIAN_POINT('Ctrl Pts',(6.35573320755963,30.4858082931554,53.0035061069962));
#89730=CARTESIAN_POINT('Ctrl Pts',(6.35959198405257,30.5549555815178,53.020331766345));
#89731=CARTESIAN_POINT('Ctrl Pts',(6.3634507605455,30.6233058353217,53.0407729552543));
#89732=CARTESIAN_POINT('Ctrl Pts',(6.36730953703843,30.690456704111,53.0647307416672));
#89733=CARTESIAN_POINT('Ctrl Pts',(6.37116588262667,30.7575652700194,53.0886734354475));
#89734=CARTESIAN_POINT('Ctrl Pts',(6.3750222282149,30.8234754935029,53.1161281686742));
#89735=CARTESIAN_POINT('Ctrl Pts',(6.37887857380313,30.8878000959244,53.146946155079));
#89736=CARTESIAN_POINT('Ctrl Pts',(6.38273378004849,30.9521056938828,53.177755036425));
#89737=CARTESIAN_POINT('Ctrl Pts',(6.38658898629385,31.0148261629514,53.2119249884776));
#89738=CARTESIAN_POINT('Ctrl Pts',(6.3904441925392,31.0755957294081,53.2492597595934));
#89739=CARTESIAN_POINT('Ctrl Pts',(6.39429954939046,31.1363676698636,53.286595989214));
#89740=CARTESIAN_POINT('Ctrl Pts',(6.39815490624172,31.1951881436373,53.3270970271897));
#89741=CARTESIAN_POINT('Ctrl Pts',(6.40201026309298,31.2517189340107,53.3705223926856));
#89742=CARTESIAN_POINT('Ctrl Pts',(6.40586965556155,31.3083088983194,53.4139932139367));
#89743=CARTESIAN_POINT('Ctrl Pts',(6.40972904803013,31.3626040087653,53.4603941767263));
#89744=CARTESIAN_POINT('Ctrl Pts',(6.41358844049871,31.4142985602079,53.5094440147737));
#89745=CARTESIAN_POINT('Ctrl Pts',(6.41745001810216,31.4660223803936,53.5585216241639));
#89746=CARTESIAN_POINT('Ctrl Pts',(6.4213115957056,31.5151423758184,53.6102507419261));
#89747=CARTESIAN_POINT('Ctrl Pts',(6.42517317330905,31.5613911358061,53.6643146764577));
#89748=CARTESIAN_POINT('Ctrl Pts',(6.42904150742394,31.6077208161606,53.7184732053831));
#89749=CARTESIAN_POINT('Ctrl Pts',(6.43290984153884,31.6511689348274,53.7749743220313));
#89750=CARTESIAN_POINT('Ctrl Pts',(6.43677817565373,31.6915100663392,53.8334704213038));
#89751=CARTESIAN_POINT('Ctrl Pts',(6.43907589482452,31.7154719549696,53.8682160261877));
#89752=CARTESIAN_POINT('Ctrl Pts',(6.44137361399532,31.7383385031005,53.9036649604587));
#89753=CARTESIAN_POINT('Ctrl Pts',(6.44367133316611,31.7600702303999,53.9397404343464));
#89754=CARTESIAN_POINT('Ctrl Pts',(6.44766818401097,31.7978722706671,54.0024932242084));
#89755=CARTESIAN_POINT('Ctrl Pts',(6.45166503485583,31.8323780045915,54.067375195746));
#89756=CARTESIAN_POINT('Ctrl Pts',(6.4556618857007,31.863350142198,54.134018585609));
#89757=CARTESIAN_POINT('Ctrl Pts',(6.45969628851417,31.8946132750867,54.2012881160465));
#89758=CARTESIAN_POINT('Ctrl Pts',(6.46373069132764,31.9222757546574,54.2703519944482));
#89759=CARTESIAN_POINT('Ctrl Pts',(6.46776509414111,31.9461388143958,54.3408025503675));
#89760=CARTESIAN_POINT('Ctrl Pts',(6.47174648699992,31.9696883259406,54.4103274226236));
#89761=CARTESIAN_POINT('Ctrl Pts',(6.47572787985874,31.9895374936084,54.4812023266619));
#89762=CARTESIAN_POINT('Ctrl Pts',(6.47970927271755,32.0055423268114,54.5530128213608));
#89763=CARTESIAN_POINT('Ctrl Pts',(6.48377018050835,32.0218668027296,54.6262574891754));
#89764=CARTESIAN_POINT('Ctrl Pts',(6.48783108829915,32.0341915119555,54.7004751038008));
#89765=CARTESIAN_POINT('Ctrl Pts',(6.49189199608994,32.0424167700165,54.7752083185361));
#89766=CARTESIAN_POINT('Ctrl Pts',(6.49595290388074,32.0506420280775,54.8499415332714));
#89767=CARTESIAN_POINT('Ctrl Pts',(6.50001381167153,32.0547677239393,54.9251898673997));
#89768=CARTESIAN_POINT('Ctrl Pts',(6.50407471946233,32.0547499427051,55.0004852355591));
#89769=CARTESIAN_POINT('Ctrl Pts',(6.50407471951138,32.0547499427048,55.0004852364685));
#89770=CARTESIAN_POINT('Ctrl Pts',(6.50830237655249,32.0547314313017,55.078872387755));
#89771=CARTESIAN_POINT('Ctrl Pts',(6.51253003359359,32.0502226030005,55.1571404354878));
#89772=CARTESIAN_POINT('Ctrl Pts',(6.51675769063469,32.0412922454997,55.2347840091714));
#89773=CARTESIAN_POINT('Ctrl Pts',(6.52089243721875,32.0325581488567,55.3107212240261));
#89774=CARTESIAN_POINT('Ctrl Pts',(6.52502718380281,32.0195950692558,55.3860607936641));
#89775=CARTESIAN_POINT('Ctrl Pts',(6.52916193038686,32.0025186272055,55.4603441214952));
#89776=CARTESIAN_POINT('Ctrl Pts',(6.53343604265649,31.9848666069413,55.5371312416868));
#89777=CARTESIAN_POINT('Ctrl Pts',(6.53771015492612,31.9628191668442,55.6127892221114));
#89778=CARTESIAN_POINT('Ctrl Pts',(6.54198426719576,31.9365582108483,55.6868332100999));
#89779=CARTESIAN_POINT('Ctrl Pts',(6.54625837946539,31.9102972548523,55.7608771980884));
#89780=CARTESIAN_POINT('Ctrl Pts',(6.55053249173502,31.8798230313502,55.833306828919));
#89781=CARTESIAN_POINT('Ctrl Pts',(6.55480660400465,31.8453691251967,55.9036649568678));
#89782=CARTESIAN_POINT('Ctrl Pts',(6.55867567735283,31.8141802650007,55.9673555528329));
#89783=CARTESIAN_POINT('Ctrl Pts',(6.56254475070101,31.7796291418862,56.029554339914));
#89784=CARTESIAN_POINT('Ctrl Pts',(6.56641382404918,31.7418816971565,56.0898833495431));
#89785=CARTESIAN_POINT('Ctrl Pts',(6.57027713244493,31.7041904964427,56.1501224684311));
#89786=CARTESIAN_POINT('Ctrl Pts',(6.57414044084068,31.6633126832068,56.2084969315057));
#89787=CARTESIAN_POINT('Ctrl Pts',(6.57800374923642,31.6194608366359,56.2646517944093));
#89788=CARTESIAN_POINT('Ctrl Pts',(6.58186252572929,31.5756604310293,56.3207407841393));
#89789=CARTESIAN_POINT('Ctrl Pts',(6.58572130222216,31.5288932194195,56.3746149645708));
#89790=CARTESIAN_POINT('Ctrl Pts',(6.58958007871504,31.4794150018997,56.4259483913011));
#89791=CARTESIAN_POINT('Ctrl Pts',(6.5934364243032,31.4299679540608,56.4772494796286));
#89792=CARTESIAN_POINT('Ctrl Pts',(6.59729276989137,31.3778136249783,56.5260126408673));
#89793=CARTESIAN_POINT('Ctrl Pts',(6.60114911547953,31.3232470434511,56.5719461900771));
#89794=CARTESIAN_POINT('Ctrl Pts',(6.60500432172482,31.2686965834163,56.6178661683916));
#89795=CARTESIAN_POINT('Ctrl Pts',(6.60885952797012,31.2117356572642,56.6609578816924));
#89796=CARTESIAN_POINT('Ctrl Pts',(6.61271473421541,31.1526936970947,56.7009687837166));
#89797=CARTESIAN_POINT('Ctrl Pts',(6.61657009106661,31.0936494304161,56.7409812487903));
#89798=CARTESIAN_POINT('Ctrl Pts',(6.62042544791781,31.0325243716964,56.7779123929433));
#89799=CARTESIAN_POINT('Ctrl Pts',(6.62428080476902,30.9696769155757,56.8115529917448));
#89800=CARTESIAN_POINT('Ctrl Pts',(6.62814019723753,30.906763673513,56.8452288040397));
#89801=CARTESIAN_POINT('Ctrl Pts',(6.63199958970605,30.8421248641636,56.8756069654698));
#89802=CARTESIAN_POINT('Ctrl Pts',(6.63585898217457,30.7761426666169,56.9025246709457));
#89803=CARTESIAN_POINT('Ctrl Pts',(6.63972055977796,30.7101231108584,56.9294576168557));
#89804=CARTESIAN_POINT('Ctrl Pts',(6.64358213738136,30.6427591117286,56.9529260466303));
#89805=CARTESIAN_POINT('Ctrl Pts',(6.64744371498475,30.5744493672258,56.9728166379555));
#89806=CARTESIAN_POINT('Ctrl Pts',(6.65131204909958,30.5060201027709,56.9927420313801));
#89807=CARTESIAN_POINT('Ctrl Pts',(6.65518038321441,30.4366422621961,57.0090769765954));
#89808=CARTESIAN_POINT('Ctrl Pts',(6.65904871732924,30.3667254312438,57.0217591401003));
#89809=CARTESIAN_POINT('Ctrl Pts',(6.66134643650057,30.325196122216,57.0292921114916));
#89810=CARTESIAN_POINT('Ctrl Pts',(6.66364415567189,30.2834767822597,57.0355373207603));
#89811=CARTESIAN_POINT('Ctrl Pts',(6.66594187484322,30.2416536453535,57.0404904013956));
#89812=CARTESIAN_POINT('Ctrl Pts',(6.6698098468366,30.1712487306679,57.0488283991009));
#89813=CARTESIAN_POINT('Ctrl Pts',(6.67367781882998,30.1002739040565,57.053534580653));
#89814=CARTESIAN_POINT('Ctrl Pts',(6.67754579082335,30.029136364528,57.0545434127227));
#89815=CARTESIAN_POINT('Ctrl Pts',(6.68140849503884,29.9580957069726,57.0555508708674));
#89816=CARTESIAN_POINT('Ctrl Pts',(6.68527119925432,29.8868932572574,57.0528709610102));
#89817=CARTESIAN_POINT('Ctrl Pts',(6.68913390346981,29.8159423194845,57.0464897587682));
#89818=CARTESIAN_POINT('Ctrl Pts',(6.69299263966132,29.7450642671841,57.0401151117171));
#89819=CARTESIAN_POINT('Ctrl Pts',(6.69685137585284,29.6744376953771,57.0300467605922));
#89820=CARTESIAN_POINT('Ctrl Pts',(6.70071011204435,29.6044751694042,57.0163228091955));
#89821=CARTESIAN_POINT('Ctrl Pts',(6.70456617531102,29.5345611060793,57.0026083643027));
#89822=CARTESIAN_POINT('Ctrl Pts',(6.70842223857769,29.4653106507555,56.9852434401794));
#89823=CARTESIAN_POINT('Ctrl Pts',(6.71227830184436,29.3971287898033,56.9643176592435));
#89824=CARTESIAN_POINT('Ctrl Pts',(6.71613400849578,29.328953234425,56.9433938135593));
#89825=CARTESIAN_POINT('Ctrl Pts',(6.71998971514719,29.2618465451175,56.9189098952704));
#89826=CARTESIAN_POINT('Ctrl Pts',(6.72384542179861,29.1961997293143,56.8910057343503));
#89827=CARTESIAN_POINT('Ctrl Pts',(6.72770090164963,29.1305567749884,56.8631032148088));
#89828=CARTESIAN_POINT('Ctrl Pts',(6.73155638150064,29.0663739676047,56.8317810498464));
#89829=CARTESIAN_POINT('Ctrl Pts',(6.73541186135166,29.0040215106627,56.7972268669474));
#89830=CARTESIAN_POINT('Ctrl Pts',(6.73927005832253,28.941625111305,56.762648332253));
#89831=CARTESIAN_POINT('Ctrl Pts',(6.7431282552934,28.8810620577117,56.7248334770607));
#89832=CARTESIAN_POINT('Ctrl Pts',(6.74698645226427,28.8226761059155,56.6840148487818));
#89833=CARTESIAN_POINT('Ctrl Pts',(6.74866000889936,28.7973502353695,56.6663090948487));
#89834=CARTESIAN_POINT('Ctrl Pts',(6.75033356553446,28.7724336105351,56.6480387143424));
#89835=CARTESIAN_POINT('Ctrl Pts',(6.75200712216955,28.7479524050421,56.6292250864936));
#89836=CARTESIAN_POINT('',(6.44592528053626,32.0547499999799,54.9999909154181));
#89837=CARTESIAN_POINT('Ctrl Pts',(6.44592528053768,32.0547499999799,54.9999909154441));
#89838=CARTESIAN_POINT('Ctrl Pts',(6.44979385259827,32.0547503134813,55.0708988474441));
#89839=CARTESIAN_POINT('Ctrl Pts',(6.45366242465885,32.0510758456684,55.1419458653844));
#89840=CARTESIAN_POINT('Ctrl Pts',(6.45753099671943,32.0437093535415,55.2127196294353));
#89841=CARTESIAN_POINT('Ctrl Pts',(6.46139380423281,32.0363538382016,55.2833879337203));
#89842=CARTESIAN_POINT('Ctrl Pts',(6.46525661174618,32.0253172686326,55.353783312964));
#89843=CARTESIAN_POINT('Ctrl Pts',(6.46911941925955,32.0106344132235,55.4234935877453));
#89844=CARTESIAN_POINT('Ctrl Pts',(6.47297769671015,31.9959687769631,55.4931221106092));
#89845=CARTESIAN_POINT('Ctrl Pts',(6.47683597416075,31.9776654483257,55.5620666517314));
#89846=CARTESIAN_POINT('Ctrl Pts',(6.48069425161135,31.9558107670499,55.6299220634268));
#89847=CARTESIAN_POINT('Ctrl Pts',(6.48455010010935,31.9339698442415,55.6977347572043));
#89848=CARTESIAN_POINT('Ctrl Pts',(6.48840594860734,31.9085821530333,55.7644592204329));
#89849=CARTESIAN_POINT('Ctrl Pts',(6.49226179710534,31.8797843322488,55.8297038186798));
#89850=CARTESIAN_POINT('Ctrl Pts',(6.49611650897051,31.8509950005293,55.8949291840257));
#89851=CARTESIAN_POINT('Ctrl Pts',(6.49997122083568,31.8187977310234,55.9586751061272));
#89852=CARTESIAN_POINT('Ctrl Pts',(6.50382593270085,31.7833772733351,56.0205699698953));
#89853=CARTESIAN_POINT('Ctrl Pts',(6.50768079864212,31.7479553998611,56.0824673076534));
#89854=CARTESIAN_POINT('Ctrl Pts',(6.51153566458339,31.7093103257034,56.1425130195337));
#89855=CARTESIAN_POINT('Ctrl Pts',(6.51539053052465,31.6676718636708,56.2003616611758));
#89856=CARTESIAN_POINT('Ctrl Pts',(6.51924943297202,31.6259898011841,56.2582708772706));
#89857=CARTESIAN_POINT('Ctrl Pts',(6.52310833541939,31.5813083783211,56.3139780354879));
#89858=CARTESIAN_POINT('Ctrl Pts',(6.52696723786676,31.5338991807724,56.367168923625));
#89859=CARTESIAN_POINT('Ctrl Pts',(6.53082833001041,31.4864630813403,56.4203899944089));
#89860=CARTESIAN_POINT('Ctrl Pts',(6.53468942215406,31.4362964679263,56.4710916072193));
#89861=CARTESIAN_POINT('Ctrl Pts',(6.53855051429771,31.3837075199634,56.5189967286656));
#89862=CARTESIAN_POINT('Ctrl Pts',(6.54241835505558,31.3310266543489,56.5669855811321));
#89863=CARTESIAN_POINT('Ctrl Pts',(6.54628619581346,31.2759153771656,56.612167875523));
#89864=CARTESIAN_POINT('Ctrl Pts',(6.55015403657133,31.2187140609575,56.6543075893329));
#89865=CARTESIAN_POINT('Ctrl Pts',(6.55242968420589,31.1850596144405,56.6791005283538));
#89866=CARTESIAN_POINT('Ctrl Pts',(6.55470533184045,31.1506822350117,56.7028410824422));
#89867=CARTESIAN_POINT('Ctrl Pts',(6.556980979475,31.1156552945759,56.7254885760806));
#89868=CARTESIAN_POINT('Ctrl Pts',(6.56085005282324,31.0561022250882,56.7639940163387));
#89869=CARTESIAN_POINT('Ctrl Pts',(6.56471912617149,30.9944367163045,56.7994881602145));
#89870=CARTESIAN_POINT('Ctrl Pts',(6.56858819951973,30.9309957744197,56.8317326307386));
#89871=CARTESIAN_POINT('Ctrl Pts',(6.57245150791554,30.8676493600817,56.8639290567255));
#89872=CARTESIAN_POINT('Ctrl Pts',(6.57631481631135,30.8025331932397,56.8928852023628));
#89873=CARTESIAN_POINT('Ctrl Pts',(6.58017812470716,30.7360123801288,56.9184064581827));
#89874=CARTESIAN_POINT('Ctrl Pts',(6.58403690120009,30.6695696001007,56.9438977759701));
#89875=CARTESIAN_POINT('Ctrl Pts',(6.58789567769302,30.6017258981191,56.9659620344101));
#89876=CARTESIAN_POINT('Ctrl Pts',(6.59175445418596,30.5328684724132,56.9844517513933));
#89877=CARTESIAN_POINT('Ctrl Pts',(6.59561079977419,30.4640544246641,57.0029298204514));
#89878=CARTESIAN_POINT('Ctrl Pts',(6.59946714536242,30.394228388246,57.0178376899948));
#89879=CARTESIAN_POINT('Ctrl Pts',(6.60332349095064,30.3237935215392,57.0290774548817));
#89880=CARTESIAN_POINT('Ctrl Pts',(6.607178697196,30.2533794645501,57.0403138990221));
#89881=CARTESIAN_POINT('Ctrl Pts',(6.61103390344136,30.1823574138323,57.0478843134958));
#89882=CARTESIAN_POINT('Ctrl Pts',(6.61488910968672,30.1111398380561,57.0517420644167));
#89883=CARTESIAN_POINT('Ctrl Pts',(6.61874446653799,30.0399194801232,57.0555999660429));
#89884=CARTESIAN_POINT('Ctrl Pts',(6.62259982338926,29.9685040671611,57.0557448920874));
#89885=CARTESIAN_POINT('Ctrl Pts',(6.62645518024052,29.8973085596809,57.0521822605668));
#89886=CARTESIAN_POINT('Ctrl Pts',(6.63031457270911,29.8260385278871,57.0486158998409));
#89887=CARTESIAN_POINT('Ctrl Pts',(6.63417396517768,29.7549893472539,57.0413342587147));
#89888=CARTESIAN_POINT('Ctrl Pts',(6.63803335764626,29.6845724363127,57.0303947927845));
#89889=CARTESIAN_POINT('Ctrl Pts',(6.64189493524972,29.6141156562862,57.0194491330793));
#89890=CARTESIAN_POINT('Ctrl Pts',(6.64575651285318,29.5442923343014,57.0048416253512));
#89891=CARTESIAN_POINT('Ctrl Pts',(6.64961809045664,29.4755025418036,56.9866806433963));
#89892=CARTESIAN_POINT('Ctrl Pts',(6.65348642457153,29.406592389425,56.9684878855987));
#89893=CARTESIAN_POINT('Ctrl Pts',(6.65735475868643,29.3387198396845,56.94672938864));
#89894=CARTESIAN_POINT('Ctrl Pts',(6.66122309280132,29.2722680150892,56.9215628328623));
#89895=CARTESIAN_POINT('Ctrl Pts',(6.66352081197207,29.2327968559886,56.9066143625506));
#89896=CARTESIAN_POINT('Ctrl Pts',(6.66581853114281,29.1938265516427,56.8904643983559));
#89897=CARTESIAN_POINT('Ctrl Pts',(6.66811625031356,29.1554332511048,56.8731536427001));
#89898=CARTESIAN_POINT('Ctrl Pts',(6.67198550519559,29.0907806741342,56.844003115218));
#89899=CARTESIAN_POINT('Ctrl Pts',(6.67585476007762,29.0275124372444,56.8114442962693));
#89900=CARTESIAN_POINT('Ctrl Pts',(6.67972401495966,28.9660116448843,56.7756310551421));
#89901=CARTESIAN_POINT('Ctrl Pts',(6.68358710202818,28.9046088883035,56.7398749023689));
#89902=CARTESIAN_POINT('Ctrl Pts',(6.6874501890967,28.8449683975511,56.7008748722515));
#89903=CARTESIAN_POINT('Ctrl Pts',(6.69131327616523,28.7874516304901,56.6588321235432));
#89904=CARTESIAN_POINT('Ctrl Pts',(6.69220528576216,28.7741706696179,56.6491242048077));
#89905=CARTESIAN_POINT('Ctrl Pts',(6.6930972953591,28.7610028408573,56.6392542512241));
#89906=CARTESIAN_POINT('Ctrl Pts',(6.69398930495604,28.7479524050421,56.6292250864936));
#89907=CARTESIAN_POINT('Ctrl Pts',(5.99388650947633,28.7479524050421,56.6292250864936));
#89908=CARTESIAN_POINT('Ctrl Pts',(5.99635921474496,28.7119320134646,56.6015436783089));
#89909=CARTESIAN_POINT('Ctrl Pts',(5.99883192001359,28.6768690092049,56.5726970773672));
#89910=CARTESIAN_POINT('Ctrl Pts',(6.00130462528221,28.6428394576484,56.5427614283434));
#89911=CARTESIAN_POINT('Ctrl Pts',(6.00517369863043,28.5895929860008,56.4959207379994));
#89912=CARTESIAN_POINT('Ctrl Pts',(6.00904277197864,28.5386700366479,56.4462284604087));
#89913=CARTESIAN_POINT('Ctrl Pts',(6.01291184532686,28.490391633517,56.3939440958463));
#89914=CARTESIAN_POINT('Ctrl Pts',(6.01677515372265,28.4421851656204,56.3417376354349));
#89915=CARTESIAN_POINT('Ctrl Pts',(6.02063846211843,28.3966157492419,56.2869471084689));
#89916=CARTESIAN_POINT('Ctrl Pts',(6.02450177051421,28.3539699294818,56.2298709564218));
#89917=CARTESIAN_POINT('Ctrl Pts',(6.02836054700713,28.3113741359411,56.1728617582783));
#89918=CARTESIAN_POINT('Ctrl Pts',(6.03221932350004,28.2716954161044,56.1135726480542));
#89919=CARTESIAN_POINT('Ctrl Pts',(6.03607809999295,28.2351809694622,56.0523361401907));
#89920=CARTESIAN_POINT('Ctrl Pts',(6.03993444558116,28.1986895257433,55.9911382093516));
#89921=CARTESIAN_POINT('Ctrl Pts',(6.04379079116937,28.1653586485714,55.9279957310736));
#89922=CARTESIAN_POINT('Ctrl Pts',(6.04764713675757,28.1353921673438,55.8632700579176));
#89923=CARTESIAN_POINT('Ctrl Pts',(6.05150234300291,28.1054345396009,55.7985635077194));
#89924=CARTESIAN_POINT('Ctrl Pts',(6.05535754924824,28.0788395384246,55.7322751318467));
#89925=CARTESIAN_POINT('Ctrl Pts',(6.05921275549357,28.0557641846634,55.6647891822695));
#89926=CARTESIAN_POINT('Ctrl Pts',(6.06306811234482,28.0326879294499,55.5973005963137));
#89927=CARTESIAN_POINT('Ctrl Pts',(6.06692346919607,28.0131317497197,55.5286148041409));
#89928=CARTESIAN_POINT('Ctrl Pts',(6.07077882604731,27.9972032527049,55.4591326077772));
#89929=CARTESIAN_POINT('Ctrl Pts',(6.07463821851587,27.9812580824428,55.3895776805184));
#89930=CARTESIAN_POINT('Ctrl Pts',(6.07849761098443,27.9689482839272,55.319225159408));
#89931=CARTESIAN_POINT('Ctrl Pts',(6.08235700345299,27.9603304240577,55.2484865861078));
#89932=CARTESIAN_POINT('Ctrl Pts',(6.08621858105643,27.9517076848747,55.1777079616014));
#89933=CARTESIAN_POINT('Ctrl Pts',(6.09008015865986,27.9467810790953,55.1065433346407));
#89934=CARTESIAN_POINT('Ctrl Pts',(6.0939417362633,27.9455550884156,55.0354071710931));
#89935=CARTESIAN_POINT('Ctrl Pts',(6.09781007037817,27.9443269526488,54.9641465422746));
#89936=CARTESIAN_POINT('Ctrl Pts',(6.10167840449304,27.9468123423208,54.8929149619447));
#89937=CARTESIAN_POINT('Ctrl Pts',(6.10554673860792,27.9529636818121,54.8221239911635));
#89938=CARTESIAN_POINT('Ctrl Pts',(6.10784445777887,27.9566174641009,54.7800754591949));
#89939=CARTESIAN_POINT('Ctrl Pts',(6.11014217694982,27.9615636544422,54.7381822477433));
#89940=CARTESIAN_POINT('Ctrl Pts',(6.11243989612077,27.9677837873881,54.6965287036682));
#89941=CARTESIAN_POINT('Ctrl Pts',(6.11630896946899,27.9782577177568,54.626389315323));
#89942=CARTESIAN_POINT('Ctrl Pts',(6.1201780428172,27.9923875858267,54.5566554207574));
#89943=CARTESIAN_POINT('Ctrl Pts',(6.12404711616542,28.0101294859619,54.4877374697856));
#89944=CARTESIAN_POINT('Ctrl Pts',(6.1279104245612,28.0278449505139,54.4189222071511));
#89945=CARTESIAN_POINT('Ctrl Pts',(6.13177373295699,28.0491616439714,54.3509209414692));
#89946=CARTESIAN_POINT('Ctrl Pts',(6.13563704135277,28.0739842444239,54.2841362756972));
#89947=CARTESIAN_POINT('Ctrl Pts',(6.13949581784568,28.0987777264104,54.2174299525237));
#89948=CARTESIAN_POINT('Ctrl Pts',(6.14335459433859,28.1270687778568,54.151937847602));
#89949=CARTESIAN_POINT('Ctrl Pts',(6.14721337083151,28.1587121110229,54.0880479878819));
#89950=CARTESIAN_POINT('Ctrl Pts',(6.15106971641971,28.1903355099099,54.0241983767124));
#89951=CARTESIAN_POINT('Ctrl Pts',(6.15492606200792,28.2253067855866,53.9619494424751));
#89952=CARTESIAN_POINT('Ctrl Pts',(6.15878240759612,28.2634328997712,53.9016684157764));
#89953=CARTESIAN_POINT('Ctrl Pts',(6.16263761384145,28.3015477497381,53.8414051988815));
#89954=CARTESIAN_POINT('Ctrl Pts',(6.16649282008678,28.3428153282386,53.7831091456008));
#89955=CARTESIAN_POINT('Ctrl Pts',(6.17034802633211,28.3869979709239,53.7271205804568));
#89956=CARTESIAN_POINT('Ctrl Pts',(6.17420338318336,28.4311823396304,53.6711298280865));
#89957=CARTESIAN_POINT('Ctrl Pts',(6.17805874003461,28.4782816959485,53.6174471228038));
#89958=CARTESIAN_POINT('Ctrl Pts',(6.18191409688585,28.5280176709357,53.566380250756));
#89959=CARTESIAN_POINT('Ctrl Pts',(6.18577348935441,28.5778057073453,53.5152599241615));
#89960=CARTESIAN_POINT('Ctrl Pts',(6.18963288182297,28.6302355321642,53.4667612454625));
#89961=CARTESIAN_POINT('Ctrl Pts',(6.19349227429153,28.6849920711708,53.4211549443925));
#89962=CARTESIAN_POINT('Ctrl Pts',(6.19735385189496,28.7397796125759,53.3755228216627));
#89963=CARTESIAN_POINT('Ctrl Pts',(6.20121542949839,28.7968961014696,53.3327866277352));
#89964=CARTESIAN_POINT('Ctrl Pts',(6.20507700710183,28.8559957577342,53.2931749192791));
#89965=CARTESIAN_POINT('Ctrl Pts',(6.2089453412167,28.9151988192763,53.2534939031491));
#89966=CARTESIAN_POINT('Ctrl Pts',(6.21281367533157,28.9763915587461,53.2169485363525));
#89967=CARTESIAN_POINT('Ctrl Pts',(6.21668200944644,29.0392024024628,53.1837220644773));
#89968=CARTESIAN_POINT('Ctrl Pts',(6.2189797286174,29.0765108860287,53.1639861525462));
#89969=CARTESIAN_POINT('Ctrl Pts',(6.22127744778836,29.1143898337741,53.1454202891854));
#89970=CARTESIAN_POINT('Ctrl Pts',(6.22357516695932,29.1527583672327,53.1280547074752));
#89971=CARTESIAN_POINT('Ctrl Pts',(6.22744424030754,29.2173662062111,53.0988132273934));
#89972=CARTESIAN_POINT('Ctrl Pts',(6.23131331365576,29.2836162215101,53.0728631850844));
#89973=CARTESIAN_POINT('Ctrl Pts',(6.23518238700398,29.3511397635225,53.050390306749));
#89974=CARTESIAN_POINT('Ctrl Pts',(6.23904569539977,29.4185626948788,53.0279509131948));
#89975=CARTESIAN_POINT('Ctrl Pts',(6.24290900379556,29.4872549291605,53.008978551621));
#89976=CARTESIAN_POINT('Ctrl Pts',(6.24677231219134,29.5568265229057,52.993611495323));
#89977=CARTESIAN_POINT('Ctrl Pts',(6.25063108868426,29.6263165048112,52.9782624655451));
#89978=CARTESIAN_POINT('Ctrl Pts',(6.25448986517717,29.6966833251353,52.9665104445909));
#89979=CARTESIAN_POINT('Ctrl Pts',(6.25834864167009,29.7675221866831,52.9584438217831));
#89980=CARTESIAN_POINT('Ctrl Pts',(6.26220498725829,29.8383164220334,52.9503822806875));
#89981=CARTESIAN_POINT('Ctrl Pts',(6.2660613328465,29.9095816271032,52.9460015863917));
#89982=CARTESIAN_POINT('Ctrl Pts',(6.26991767843471,29.9809045784327,52.9453387317187));
#89983=CARTESIAN_POINT('Ctrl Pts',(6.27377288468005,30.0522064576632,52.9446760728837));
#89984=CARTESIAN_POINT('Ctrl Pts',(6.27762809092538,30.1235655637825,52.9477290775123));
#89985=CARTESIAN_POINT('Ctrl Pts',(6.28148329717072,30.1945670747281,52.9544826532313));
#89986=CARTESIAN_POINT('Ctrl Pts',(6.28533865402196,30.2655713593897,52.9612364927827));
#89987=CARTESIAN_POINT('Ctrl Pts',(6.28919401087321,30.3362175377481,52.971691142247));
#89988=CARTESIAN_POINT('Ctrl Pts',(6.29304936772446,30.4060960479372,52.9857796639022));
#89989=CARTESIAN_POINT('Ctrl Pts',(6.29690876019302,30.4760477038651,52.9998829327998));
#89990=CARTESIAN_POINT('Ctrl Pts',(6.30076815266158,30.5452296103556,53.0176275708755));
#89991=CARTESIAN_POINT('Ctrl Pts',(6.30462754513014,30.6132434306249,53.0388957046359));
#89992=CARTESIAN_POINT('Ctrl Pts',(6.30848912273358,30.6812957593829,53.0601758801208));
#89993=CARTESIAN_POINT('Ctrl Pts',(6.31235070033702,30.7481782296865,53.0849833536127));
#89994=CARTESIAN_POINT('Ctrl Pts',(6.31621227794046,30.8135112824052,53.1131515811016));
#89995=CARTESIAN_POINT('Ctrl Pts',(6.32008061205533,30.8789586468285,53.1413690938751));
#89996=CARTESIAN_POINT('Ctrl Pts',(6.3239489461702,30.9428507455122,53.1729588853261));
#89997=CARTESIAN_POINT('Ctrl Pts',(6.32781728028508,31.0048320976366,53.2077081660457));
#89998=CARTESIAN_POINT('Ctrl Pts',(6.33011499945601,31.0416478784836,53.2283485983647));
#89999=CARTESIAN_POINT('Ctrl Pts',(6.33241271862695,31.0777900498443,53.2501028948123));
#90000=CARTESIAN_POINT('Ctrl Pts',(6.33471043779788,31.1131893460155,53.2729195032027));
#90001=CARTESIAN_POINT('Ctrl Pts',(6.3385795111461,31.1727973586455,53.3113398343453));
#90002=CARTESIAN_POINT('Ctrl Pts',(6.34244858449431,31.230530748491,53.352924986983));
#90003=CARTESIAN_POINT('Ctrl Pts',(6.34631765784252,31.2860335365734,53.3974659737439));
#90004=CARTESIAN_POINT('Ctrl Pts',(6.35018096623831,31.3414536250262,53.441940594053));
#90005=CARTESIAN_POINT('Ctrl Pts',(6.3540442746341,31.394649333214,53.4893620046678));
#90006=CARTESIAN_POINT('Ctrl Pts',(6.35790758302988,31.4452930003892,53.53947759157));
#90007=CARTESIAN_POINT('Ctrl Pts',(6.36176635952279,31.4958772593688,53.5895343897479));
#90008=CARTESIAN_POINT('Ctrl Pts',(6.3656251360157,31.5439150802224,53.642278746476));
#90009=CARTESIAN_POINT('Ctrl Pts',(6.36948391250862,31.5891126557695,53.6974185131927));
#90010=CARTESIAN_POINT('Ctrl Pts',(6.37334025809682,31.6342817583021,53.7525235436352));
#90011=CARTESIAN_POINT('Ctrl Pts',(6.37719660368503,31.6766138581673,53.8100206153618));
#90012=CARTESIAN_POINT('Ctrl Pts',(6.38105294927323,31.7158537585194,53.8695826249235));
#90013=CARTESIAN_POINT('Ctrl Pts',(6.38490815551856,31.7550820655897,53.9291270371123));
#90014=CARTESIAN_POINT('Ctrl Pts',(6.38876336176389,31.7912197197449,53.9907347705194));
#90015=CARTESIAN_POINT('Ctrl Pts',(6.39261856800922,31.8240544161565,54.0540491294998));
#90016=CARTESIAN_POINT('Ctrl Pts',(6.39647392486046,31.8568903952749,54.1173659618931));
#90017=CARTESIAN_POINT('Ctrl Pts',(6.40032928171171,31.8864229387863,54.1823891199662));
#90018=CARTESIAN_POINT('Ctrl Pts',(6.40418463856296,31.9124861523396,54.2487382083393));
#90019=CARTESIAN_POINT('Ctrl Pts',(6.40804403103151,31.938576647714,54.3151567480083));
#90020=CARTESIAN_POINT('Ctrl Pts',(6.41190342350007,31.9611903857798,54.3829035355099));
#90021=CARTESIAN_POINT('Ctrl Pts',(6.41576281596863,31.9802103536278,54.4515799804116));
#90022=CARTESIAN_POINT('Ctrl Pts',(6.41962439357206,31.9992410903197,54.5202953089708));
#90023=CARTESIAN_POINT('Ctrl Pts',(6.4234859711755,32.0146739011016,54.5899408682429));
#90024=CARTESIAN_POINT('Ctrl Pts',(6.42734754877893,32.0264428476099,54.6601074465797));
#90025=CARTESIAN_POINT('Ctrl Pts',(6.4312158828938,32.0382323859669,54.7303967937269));
#90026=CARTESIAN_POINT('Ctrl Pts',(6.43508421700867,32.0463452058353,54.8012084972222));
#90027=CARTESIAN_POINT('Ctrl Pts',(6.43895255112354,32.0507672808364,54.8721284928113));
#90028=CARTESIAN_POINT('Ctrl Pts',(6.44125027029451,32.0533939118884,54.9142536631382));
#90029=CARTESIAN_POINT('Ctrl Pts',(6.44354798946548,32.0547193955748,54.9564170246935));
#90030=CARTESIAN_POINT('Ctrl Pts',(6.44584570863644,32.0547494759025,54.9985324242889));
#90031=CARTESIAN_POINT('Ctrl Pts',(6.44587223260258,32.054749823138,54.9990185878927));
#90032=CARTESIAN_POINT('Ctrl Pts',(6.44589875656871,32.0547499978305,54.9995047516197));
#90033=CARTESIAN_POINT('Ctrl Pts',(6.44592528053485,32.0547499999799,54.9999909153921));
#90034=CARTESIAN_POINT('Origin',(-1.54592528053767,30.,55.));
#90035=CARTESIAN_POINT('',(5.29388070767824,28.7479524050421,56.6292250864936));
#90036=CARTESIAN_POINT('',(5.35213793390276,28.7479524050421,56.6292250864936));
#90037=CARTESIAN_POINT('',(-1.54592528053767,28.7479524050421,56.6292250864936));
#90038=CARTESIAN_POINT('',(5.80407471943462,32.0547491412314,54.9981214077884));
#90039=CARTESIAN_POINT('Ctrl Pts',(5.35213793390276,28.7479524050421,56.6292250864936));
#90040=CARTESIAN_POINT('Ctrl Pts',(5.35599766292863,28.6915503629408,56.5858805285507));
#90041=CARTESIAN_POINT('Ctrl Pts',(5.35985739195449,28.6373313286563,56.5395495273057));
#90042=CARTESIAN_POINT('Ctrl Pts',(5.36371712098035,28.5856246526876,56.4904831228213));
#90043=CARTESIAN_POINT('Ctrl Pts',(5.36757404196294,28.5339555945369,56.4414524152955));
#90044=CARTESIAN_POINT('Ctrl Pts',(5.37143096294552,28.484795620045,56.3896905857117));
#90045=CARTESIAN_POINT('Ctrl Pts',(5.3752878839281,28.4384404564927,56.3354884329642));
#90046=CARTESIAN_POINT('Ctrl Pts',(5.37914328914527,28.3921035104651,56.281307581599));
#90047=CARTESIAN_POINT('Ctrl Pts',(5.38299869436244,28.3485695030702,56.2246886793533));
#90048=CARTESIAN_POINT('Ctrl Pts',(5.38685409957961,28.3080955784032,56.1659575424007));
#90049=CARTESIAN_POINT('Ctrl Pts',(5.39070927931651,28.267624020821,56.1072298402915));
#90050=CARTESIAN_POINT('Ctrl Pts',(5.39456445905341,28.2302124649732,56.0463905496428));
#90051=CARTESIAN_POINT('Ctrl Pts',(5.39841963879031,28.196075196942,55.9837951348793));
#90052=CARTESIAN_POINT('Ctrl Pts',(5.40227861260071,28.161904332733,55.921138116865));
#90053=CARTESIAN_POINT('Ctrl Pts',(5.40613758641111,28.1310144263927,55.8567219499077));
#90054=CARTESIAN_POINT('Ctrl Pts',(5.40999656022151,28.1035737355695,55.7909266628949));
#90055=CARTESIAN_POINT('Ctrl Pts',(5.41385738135562,28.0761199086532,55.7250998791164));
#90056=CARTESIAN_POINT('Ctrl Pts',(5.41771820248974,28.0521187503223,55.6578931182441));
#90057=CARTESIAN_POINT('Ctrl Pts',(5.42157902362385,28.0316892851007,55.5897037324901));
#90058=CARTESIAN_POINT('Ctrl Pts',(5.42544695903229,28.0112221748252,55.5213886952283));
#90059=CARTESIAN_POINT('Ctrl Pts',(5.42931489444074,27.9943400227808,55.4520878885795));
#90060=CARTESIAN_POINT('Ctrl Pts',(5.43318282984919,27.9811110440717,55.3822106044194));
#90061=CARTESIAN_POINT('Ctrl Pts',(5.43660651843915,27.9694014629437,55.3203589871577));
#90062=CARTESIAN_POINT('Ctrl Pts',(5.44003020702911,27.9605533501439,55.2580560670572));
#90063=CARTESIAN_POINT('Ctrl Pts',(5.44345389561907,27.9545799673091,55.1955874545234));
#90064=CARTESIAN_POINT('Ctrl Pts',(5.44732296896728,27.9478295121444,55.1249923529236));
#90065=CARTESIAN_POINT('Ctrl Pts',(5.45119204231549,27.9447248768961,55.053909088628));
#90066=CARTESIAN_POINT('Ctrl Pts',(5.45506111566371,27.9453224383922,54.9827465851109));
#90067=CARTESIAN_POINT('Ctrl Pts',(5.4589244240595,27.9459191095165,54.9116901143336));
#90068=CARTESIAN_POINT('Ctrl Pts',(5.46278773245528,27.9502070236293,54.8405551205059));
#90069=CARTESIAN_POINT('Ctrl Pts',(5.46665104085107,27.9581907664978,54.7697553117116));
#90070=CARTESIAN_POINT('Ctrl Pts',(5.47050981734398,27.9661651439355,54.6990385555302));
#90071=CARTESIAN_POINT('Ctrl Pts',(5.47436859383689,27.9778266843106,54.6286566837512));
#90072=CARTESIAN_POINT('Ctrl Pts',(5.47822737032981,27.9931279671208,54.5590213087377));
#90073=CARTESIAN_POINT('Ctrl Pts',(5.48208371591801,28.0084196106165,54.489429801764));
#90074=CARTESIAN_POINT('Ctrl Pts',(5.48594006150622,28.0273463434204,54.4205843318948));
#90075=CARTESIAN_POINT('Ctrl Pts',(5.48979640709442,28.0498093885285,54.352887844784));
#90076=CARTESIAN_POINT('Ctrl Pts',(5.49365161333976,28.0722657970139,54.285211358347));
#90077=CARTESIAN_POINT('Ctrl Pts',(5.49750681958509,28.0982562906982,54.2186836415558));
#90078=CARTESIAN_POINT('Ctrl Pts',(5.50136202583042,28.127632294866,54.1536922904337));
#90079=CARTESIAN_POINT('Ctrl Pts',(5.50521738268167,28.1570094466249,54.0886984003861));
#90080=CARTESIAN_POINT('Ctrl Pts',(5.50907273953292,28.1897721693541,54.0252414369272));
#90081=CARTESIAN_POINT('Ctrl Pts',(5.51292809638416,28.2257245380364,53.9636872346758));
#90082=CARTESIAN_POINT('Ctrl Pts',(5.51678748885272,28.2617145400707,53.9020686002035));
#90083=CARTESIAN_POINT('Ctrl Pts',(5.52064688132128,28.3009006075061,53.8423571232076));
#90084=CARTESIAN_POINT('Ctrl Pts',(5.52450627378984,28.3430422566967,53.7848915277198));
#90085=CARTESIAN_POINT('Ctrl Pts',(5.52836785139328,28.3852077659088,53.727393396003));
#90086=CARTESIAN_POINT('Ctrl Pts',(5.53222942899671,28.4303318806809,53.6721440535545));
#90087=CARTESIAN_POINT('Ctrl Pts',(5.53609100660015,28.4781341470806,53.6194487013451));
#90088=CARTESIAN_POINT('Ctrl Pts',(5.53995934071502,28.5260200519805,53.5666611493183));
#90089=CARTESIAN_POINT('Ctrl Pts',(5.54382767482989,28.5765931192425,53.5164368517539));
#90090=CARTESIAN_POINT('Ctrl Pts',(5.54769600894476,28.6295369352046,53.4690432564793));
#90091=CARTESIAN_POINT('Ctrl Pts',(5.54999372811572,28.6609845861332,53.4408923343487));
#90092=CARTESIAN_POINT('Ctrl Pts',(5.55229144728667,28.6932680392855,53.4137393489293));
#90093=CARTESIAN_POINT('Ctrl Pts',(5.55458916645763,28.7263160946049,53.3876331460745));
#90094=CARTESIAN_POINT('Ctrl Pts',(5.55845823980585,28.7819649100315,53.3436735469358));
#90095=CARTESIAN_POINT('Ctrl Pts',(5.56232731315406,28.8400012139871,53.302512198001));
#90096=CARTESIAN_POINT('Ctrl Pts',(5.56619638650228,28.9001120288156,53.2644182493055));
#90097=CARTESIAN_POINT('Ctrl Pts',(5.57005969489807,28.9601332780151,53.2263810609198));
#90098=CARTESIAN_POINT('Ctrl Pts',(5.57392300329385,29.022222495477,53.1914024584711));
#90099=CARTESIAN_POINT('Ctrl Pts',(5.57778631168964,29.0860345941754,53.1597106750688));
#90100=CARTESIAN_POINT('Ctrl Pts',(5.58164508818255,29.1497718372826,53.1280560681146));
#90101=CARTESIAN_POINT('Ctrl Pts',(5.58550386467546,29.2152275141708,53.0996808366239));
#90102=CARTESIAN_POINT('Ctrl Pts',(5.58936264116837,29.282030092187,53.0747683843301));
#90103=CARTESIAN_POINT('Ctrl Pts',(5.59321898675658,29.3487905867342,53.0498716260775));
#90104=CARTESIAN_POINT('Ctrl Pts',(5.59707533234478,29.4168958449017,53.0284334884235));
#90105=CARTESIAN_POINT('Ctrl Pts',(5.60093167793299,29.4859537613947,53.0105895277556));
#90106=CARTESIAN_POINT('Ctrl Pts',(5.60478688417832,29.5549912749846,52.9927508390191));
#90107=CARTESIAN_POINT('Ctrl Pts',(5.60864209042365,29.6249804180432,52.9785043405957));
#90108=CARTESIAN_POINT('Ctrl Pts',(5.61249729666899,29.6955149726785,52.9679354265582));
#90109=CARTESIAN_POINT('Ctrl Pts',(5.61635265352023,29.766052282788,52.9573660996399));
#90110=CARTESIAN_POINT('Ctrl Pts',(5.62020801037148,29.8371345660271,52.9504747121478));
#90111=CARTESIAN_POINT('Ctrl Pts',(5.62406336722272,29.9083482061046,52.9472950744991));
#90112=CARTESIAN_POINT('Ctrl Pts',(5.62792275969128,29.9796363894761,52.944112108546));
#90113=CARTESIAN_POINT('Ctrl Pts',(5.63178215215984,30.051055717867,52.9446486700726));
#90114=CARTESIAN_POINT('Ctrl Pts',(5.6356415446284,30.1221911847715,52.9488864300424));
#90115=CARTESIAN_POINT('Ctrl Pts',(5.63950312223183,30.1933669275979,52.9531265893736));
#90116=CARTESIAN_POINT('Ctrl Pts',(5.64336469983527,30.2642580060049,52.9610720646429));
#90117=CARTESIAN_POINT('Ctrl Pts',(5.6472262774387,30.3344558992222,52.9726527643308));
#90118=CARTESIAN_POINT('Ctrl Pts',(5.65109461155358,30.4047766160409,52.9842537264964));
#90119=CARTESIAN_POINT('Ctrl Pts',(5.65496294566845,30.4744012514912,52.9995025079733));
#90120=CARTESIAN_POINT('Ctrl Pts',(5.65883127978332,30.5429334995974,53.0182783299578));
#90121=CARTESIAN_POINT('Ctrl Pts',(5.66112899895427,30.5836403919252,53.0294308221787));
#90122=CARTESIAN_POINT('Ctrl Pts',(5.66342671812523,30.623962183262,53.0418267532859));
#90123=CARTESIAN_POINT('Ctrl Pts',(5.66572443729618,30.6638192197251,53.0554327972468));
#90124=CARTESIAN_POINT('Ctrl Pts',(5.6695935106444,30.7309335126586,53.0783436832806));
#90125=CARTESIAN_POINT('Ctrl Pts',(5.67346258399261,30.7969917617407,53.1047780728358));
#90126=CARTESIAN_POINT('Ctrl Pts',(5.67733165734083,30.861598094463,53.1346189970631));
#90127=CARTESIAN_POINT('Ctrl Pts',(5.68119496573661,30.9261081631961,53.1644154580578));
#90128=CARTESIAN_POINT('Ctrl Pts',(5.6850582741324,30.9891701723715,53.1976081764317));
#90129=CARTESIAN_POINT('Ctrl Pts',(5.68892158252818,31.0504052106035,53.2340310149844));
#90130=CARTESIAN_POINT('Ctrl Pts',(5.69278035902109,31.1115684162978,53.2704111272648));
#90131=CARTESIAN_POINT('Ctrl Pts',(5.69663913551401,31.1709084925866,53.3100135860908));
#90132=CARTESIAN_POINT('Ctrl Pts',(5.70049791200692,31.2280698480373,53.3526257222958));
#90133=CARTESIAN_POINT('Ctrl Pts',(5.70435425759513,31.2851951936782,53.3952110142295));
#90134=CARTESIAN_POINT('Ctrl Pts',(5.70821060318333,31.340144152993,53.4408019322545));
#90135=CARTESIAN_POINT('Ctrl Pts',(5.71206694877154,31.3925901753264,53.4891425725489));
#90136=CARTESIAN_POINT('Ctrl Pts',(5.71592215501687,31.4450207026788,53.537468930782));
#90137=CARTESIAN_POINT('Ctrl Pts',(5.71977736126221,31.4949494041253,53.5885430693971));
#90138=CARTESIAN_POINT('Ctrl Pts',(5.72363256750754,31.5420842183902,53.6420700217273));
#90139=CARTESIAN_POINT('Ctrl Pts',(5.72748792435879,31.5892208740046,53.6955990651195));
#90140=CARTESIAN_POINT('Ctrl Pts',(5.73134328121004,31.6335631063546,53.7515807464294));
#90141=CARTESIAN_POINT('Ctrl Pts',(5.73519863806129,31.6748581792146,53.80968590615));
#90142=CARTESIAN_POINT('Ctrl Pts',(5.73905803052985,31.7161964779335,53.8678518877861));
#90143=CARTESIAN_POINT('Ctrl Pts',(5.74291742299841,31.7544809679483,53.9281453881853));
#90144=CARTESIAN_POINT('Ctrl Pts',(5.74677681546697,31.789501963657,53.9902078012939));
#90145=CARTESIAN_POINT('Ctrl Pts',(5.75063839307041,31.8245427877712,54.0523053532862));
#90146=CARTESIAN_POINT('Ctrl Pts',(5.75449997067384,31.8563162228105,54.1161733765902));
#90147=CARTESIAN_POINT('Ctrl Pts',(5.75836154827727,31.8846595887194,54.1814306399895));
#90148=CARTESIAN_POINT('Ctrl Pts',(5.76222988239215,31.9130525463485,54.2468020824865));
#90149=CARTESIAN_POINT('Ctrl Pts',(5.76609821650702,31.938003282546,54.3135671628902));
#90150=CARTESIAN_POINT('Ctrl Pts',(5.76996655062189,31.9593983267177,54.3813274212027));
#90151=CARTESIAN_POINT('Ctrl Pts',(5.77226426979284,31.9721065886457,54.4215757658208));
#90152=CARTESIAN_POINT('Ctrl Pts',(5.77456198896379,31.9835613184563,54.4621749669161));
#90153=CARTESIAN_POINT('Ctrl Pts',(5.77685970813474,31.9937473133959,54.5030400289493));
#90154=CARTESIAN_POINT('Ctrl Pts',(5.78191177765076,32.0161435901798,54.5928913636023));
#90155=CARTESIAN_POINT('Ctrl Pts',(5.78696384716678,32.0324751044773,54.6843103064811));
#90156=CARTESIAN_POINT('Ctrl Pts',(5.79201591668279,32.0425683991214,54.7765902924879));
#90157=CARTESIAN_POINT('Ctrl Pts',(5.79603551760007,32.0505989727865,54.8500114350955));
#90158=CARTESIAN_POINT('Ctrl Pts',(5.80005511851734,32.0546813537135,54.9239774059945));
#90159=CARTESIAN_POINT('Ctrl Pts',(5.80407471943462,32.0547491412314,54.9981214077884));
#90160=CARTESIAN_POINT('Ctrl Pts',(5.80407471946232,32.0547491412319,54.9981214082994));
#90161=CARTESIAN_POINT('Ctrl Pts',(5.80788808427067,32.0548134507169,55.0684612587007));
#90162=CARTESIAN_POINT('Ctrl Pts',(5.81170144907902,32.0512616122162,55.1388965966684));
#90163=CARTESIAN_POINT('Ctrl Pts',(5.81551481388736,32.0440909046793,55.2090213766761));
#90164=CARTESIAN_POINT('Ctrl Pts',(5.81932566294072,32.0369249278052,55.2790998939279));
#90165=CARTESIAN_POINT('Ctrl Pts',(5.82313651199408,32.0261448653966,55.3488677648101));
#90166=CARTESIAN_POINT('Ctrl Pts',(5.82694736104743,32.0118000195855,55.4179213367317));
#90167=CARTESIAN_POINT('Ctrl Pts',(5.83075704398262,31.9974595632911,55.4869537782901));
#90168=CARTESIAN_POINT('Ctrl Pts',(5.83456672691781,31.9795565892295,55.5552718667561));
#90169=CARTESIAN_POINT('Ctrl Pts',(5.838376409853,31.9581916522916,55.6224813373874));
#90170=CARTESIAN_POINT('Ctrl Pts',(5.84218627454133,31.9368256960708,55.6896940144621));
#90171=CARTESIAN_POINT('Ctrl Pts',(5.84599613922967,31.9119976032424,55.7557974946331));
#90172=CARTESIAN_POINT('Ctrl Pts',(5.849806003918,31.8838574485778,55.8204137224217));
#90173=CARTESIAN_POINT('Ctrl Pts',(5.85361981396675,31.8556881529696,55.8850968644785));
#90174=CARTESIAN_POINT('Ctrl Pts',(5.8574336240155,31.8242001532049,55.9482892241745));
#90175=CARTESIAN_POINT('Ctrl Pts',(5.86124743406425,31.7895907717139,56.0096348014487));
#90176=CARTESIAN_POINT('Ctrl Pts',(5.86506356527389,31.7549603262628,56.0710177148652));
#90177=CARTESIAN_POINT('Ctrl Pts',(5.86887969648353,31.7172049893169,56.130551190873));
#90178=CARTESIAN_POINT('Ctrl Pts',(5.87269582769317,31.6765654040821,56.1879082491232));
#90179=CARTESIAN_POINT('Ctrl Pts',(5.87651830066253,31.6358582827825,56.2453606250294));
#90180=CARTESIAN_POINT('Ctrl Pts',(5.88034077363189,31.5922576630937,56.3006289805395));
#90181=CARTESIAN_POINT('Ctrl Pts',(5.88416324660125,31.5460437137662,56.3534202590563));
#90182=CARTESIAN_POINT('Ctrl Pts',(5.88544049072526,31.5306017483947,56.3710599783756));
#90183=CARTESIAN_POINT('Ctrl Pts',(5.88671773484928,31.5148682976371,56.3884234488371));
#90184=CARTESIAN_POINT('Ctrl Pts',(5.8879949789733,31.4988546567116,56.4055007223598));
#90185=CARTESIAN_POINT('Ctrl Pts',(5.89186405232151,31.450345565812,56.4572318069697));
#90186=CARTESIAN_POINT('Ctrl Pts',(5.89573312566973,31.3990601643256,56.5065499255199));
#90187=CARTESIAN_POINT('Ctrl Pts',(5.89960219901794,31.3452680229111,56.5531424625683));
#90188=CARTESIAN_POINT('Ctrl Pts',(5.90346550741372,31.2915560322483,56.5996655763374));
#90189=CARTESIAN_POINT('Ctrl Pts',(5.9073288158095,31.2353450798583,56.6434708543948));
#90190=CARTESIAN_POINT('Ctrl Pts',(5.91119212420528,31.1769425622696,56.6842813801791));
#90191=CARTESIAN_POINT('Ctrl Pts',(5.91505090069819,31.1186085544943,56.725044032659));
#90192=CARTESIAN_POINT('Ctrl Pts',(5.9189096771911,31.0580884843514,56.7628186340324));
#90193=CARTESIAN_POINT('Ctrl Pts',(5.92276845368401,30.9957225538102,56.7973686762414));
#90194=CARTESIAN_POINT('Ctrl Pts',(5.92662479927221,30.9333959117934,56.8318969530383));
#90195=CARTESIAN_POINT('Ctrl Pts',(5.93048114486042,30.8692261403501,56.8632044660194));
#90196=CARTESIAN_POINT('Ctrl Pts',(5.93433749044863,30.8035808867981,56.8910989717285));
#90197=CARTESIAN_POINT('Ctrl Pts',(5.93819269669395,30.7379550278906,56.9189852361103));
#90198=CARTESIAN_POINT('Ctrl Pts',(5.94204790293928,30.6708549991593,56.9434603052145));
#90199=CARTESIAN_POINT('Ctrl Pts',(5.94590310918461,30.6026698482918,56.9643794481871));
#90200=CARTESIAN_POINT('Ctrl Pts',(5.94975846603586,30.534482033731,56.9852994083784));
#90201=CARTESIAN_POINT('Ctrl Pts',(5.9536138228871,30.4652094779389,57.0026630262639));
#90202=CARTESIAN_POINT('Ctrl Pts',(5.95746917973835,30.3952562000434,57.0163754855748));
#90203=CARTESIAN_POINT('Ctrl Pts',(5.9613285722069,30.3252296981456,57.0301022984827));
#90204=CARTESIAN_POINT('Ctrl Pts',(5.96518796467546,30.2545215294252,57.0401702298633));
#90205=CARTESIAN_POINT('Ctrl Pts',(5.96904735714402,30.1835448252711,57.0465358192849));
#90206=CARTESIAN_POINT('Ctrl Pts',(5.97290893474745,30.1125279350842,57.0529050128157));
#90207=CARTESIAN_POINT('Ctrl Pts',(5.97677051235089,30.0412426924744,57.0555676733289));
#90208=CARTESIAN_POINT('Ctrl Pts',(5.98063208995432,29.9701034964045,57.0545324922164));
#90209=CARTESIAN_POINT('Ctrl Pts',(5.98450042406919,29.8988398297577,57.0534954998718));
#90210=CARTESIAN_POINT('Ctrl Pts',(5.98836875818406,29.8277232046934,57.048747780675));
#90211=CARTESIAN_POINT('Ctrl Pts',(5.99223709229893,29.757163462566,57.0403499647333));
#90212=CARTESIAN_POINT('Ctrl Pts',(5.99453481146991,29.7152522761558,57.0353618168353));
#90213=CARTESIAN_POINT('Ctrl Pts',(5.99683253064088,29.673537401737,57.0290868493545));
#90214=CARTESIAN_POINT('Ctrl Pts',(5.99913024981186,29.6321025567787,57.0215461987724));
#90215=CARTESIAN_POINT('Ctrl Pts',(6.00299944641644,29.5623292078643,57.0088482764167));
#90216=CARTESIAN_POINT('Ctrl Pts',(6.00686864302101,29.4930773589399,56.992508916201));
#90217=CARTESIAN_POINT('Ctrl Pts',(6.01073783962559,29.424755896298,56.9725850510576));
#90218=CARTESIAN_POINT('Ctrl Pts',(6.01460043061965,29.3565510741421,56.9526952005449));
#90219=CARTESIAN_POINT('Ctrl Pts',(6.0184630216137,29.2892739449733,56.9292331382224));
#90220=CARTESIAN_POINT('Ctrl Pts',(6.02232561260776,29.2233236576029,56.902306868426));
#90221=CARTESIAN_POINT('Ctrl Pts',(6.02618437399501,29.1574387573444,56.8754072949653));
#90222=CARTESIAN_POINT('Ctrl Pts',(6.03004313538226,29.0928785364837,56.8450505102895));
#90223=CARTESIAN_POINT('Ctrl Pts',(6.03390189676951,29.0300262074176,56.8113940499525));
#90224=CARTESIAN_POINT('Ctrl Pts',(6.03775817547493,28.9672143168031,56.7777592437875));
#90225=CARTESIAN_POINT('Ctrl Pts',(6.04161445418034,28.9061085647321,56.7408292034265));
#90226=CARTESIAN_POINT('Ctrl Pts',(6.04547073288576,28.8470698473807,56.7008085211691));
#90227=CARTESIAN_POINT('Ctrl Pts',(6.0476742096299,28.8133351381894,56.6779407127518));
#90228=CARTESIAN_POINT('Ctrl Pts',(6.04987768637404,28.7802748782558,56.6540646713894));
#90229=CARTESIAN_POINT('Ctrl Pts',(6.05208116311818,28.7479524050421,56.6292250864936));
#90230=CARTESIAN_POINT('',(5.74592528057397,32.0547492412561,55.0017658022556));
#90231=CARTESIAN_POINT('Ctrl Pts',(5.74592528057397,32.0547492412561,55.0017658022556));
#90232=CARTESIAN_POINT('Ctrl Pts',(5.75057817989353,32.0546753518278,55.0877461243741));
#90233=CARTESIAN_POINT('Ctrl Pts',(5.7552310792131,32.0492009128718,55.1734909003204));
#90234=CARTESIAN_POINT('Ctrl Pts',(5.75988397853267,32.0384370230129,55.25840291351));
#90235=CARTESIAN_POINT('Ctrl Pts',(5.76460377517735,32.027518374714,55.3445357540079));
#90236=CARTESIAN_POINT('Ctrl Pts',(5.76932357182203,32.0111571571895,55.4298117228975));
#90237=CARTESIAN_POINT('Ctrl Pts',(5.77404336846671,31.9895181111646,55.5136294849872));
#90238=CARTESIAN_POINT('Ctrl Pts',(5.7757069401795,31.9818910654317,55.543172465022));
#90239=CARTESIAN_POINT('Ctrl Pts',(5.7773705118923,31.9736087726772,55.5725344842986));
#90240=CARTESIAN_POINT('Ctrl Pts',(5.77903408360509,31.9646798449385,55.6016898448475));
#90241=CARTESIAN_POINT('Ctrl Pts',(5.78290315695331,31.9439132761899,55.669498300347));
#90242=CARTESIAN_POINT('Ctrl Pts',(5.78677223030153,31.919591424662,55.7363632146236));
#90243=CARTESIAN_POINT('Ctrl Pts',(5.79064130364974,31.891818620162,55.8018851980854));
#90244=CARTESIAN_POINT('Ctrl Pts',(5.79450461204553,31.8640871973786,55.8673095532306));
#90245=CARTESIAN_POINT('Ctrl Pts',(5.79836792044131,31.8329152162863,55.9313945058254));
#90246=CARTESIAN_POINT('Ctrl Pts',(5.80223122883709,31.7984566891992,55.9937560563713));
#90247=CARTESIAN_POINT('Ctrl Pts',(5.80609000533,31.764038584124,56.05604445291));
#90248=CARTESIAN_POINT('Ctrl Pts',(5.80994878182292,31.7263418248368,56.1166130399686));
#90249=CARTESIAN_POINT('Ctrl Pts',(5.81380755831583,31.6855676731749,56.1750996475396));
#90250=CARTESIAN_POINT('Ctrl Pts',(5.81766390390404,31.6448192079132,56.2335494104346));
#90251=CARTESIAN_POINT('Ctrl Pts',(5.82152024949224,31.600997473704,56.2899193984339));
#90252=CARTESIAN_POINT('Ctrl Pts',(5.82537659508045,31.554347868057,56.3438750937371));
#90253=CARTESIAN_POINT('Ctrl Pts',(5.82923180132578,31.5077120448613,56.3978148480319));
#90254=CARTESIAN_POINT('Ctrl Pts',(5.83308700757112,31.4582503264421,56.449341358436));
#90255=CARTESIAN_POINT('Ctrl Pts',(5.83694221381645,31.4062482494231,56.4981533377777));
#90256=CARTESIAN_POINT('Ctrl Pts',(5.8407975706677,31.3542441409122,56.5469672239883));
#90257=CARTESIAN_POINT('Ctrl Pts',(5.84465292751894,31.2996998324747,56.5930660377379));
#90258=CARTESIAN_POINT('Ctrl Pts',(5.84850828437019,31.2429362859699,56.6361867104702));
#90259=CARTESIAN_POINT('Ctrl Pts',(5.85236767683875,31.1861133218912,56.6793525200186));
#90260=CARTESIAN_POINT('Ctrl Pts',(5.85622706930731,31.127066870136,56.7195336710873));
#90261=CARTESIAN_POINT('Ctrl Pts',(5.86008646177587,31.0661486922942,56.7565091882536));
#90262=CARTESIAN_POINT('Ctrl Pts',(5.86394803937931,31.0051960234189,56.7935056404486));
#90263=CARTESIAN_POINT('Ctrl Pts',(5.86780961698274,30.9423699468744,56.8272926154684));
#90264=CARTESIAN_POINT('Ctrl Pts',(5.87167119458618,30.8780463317208,56.8576954007188));
#90265=CARTESIAN_POINT('Ctrl Pts',(5.87553952870105,30.8136101710518,56.8881513810069));
#90266=CARTESIAN_POINT('Ctrl Pts',(5.87940786281593,30.7476716900095,56.9152111651147));
#90267=CARTESIAN_POINT('Ctrl Pts',(5.8832761969308,30.6806255415039,56.938748677563));
#90268=CARTESIAN_POINT('Ctrl Pts',(5.88557391610175,30.6408013649502,56.9527295261617));
#90269=CARTESIAN_POINT('Ctrl Pts',(5.8878716352727,30.6005866745913,56.9654686251862));
#90270=CARTESIAN_POINT('Ctrl Pts',(5.89016935444365,30.5600659399301,56.9769480785873));
#90271=CARTESIAN_POINT('Ctrl Pts',(5.89403860384475,30.4918309570381,56.9962789301375));
#90272=CARTESIAN_POINT('Ctrl Pts',(5.89790785324585,30.4224603230496,57.0121107721138));
#90273=CARTESIAN_POINT('Ctrl Pts',(5.90177710264696,30.352346221252,57.0243146254645));
#90274=CARTESIAN_POINT('Ctrl Pts',(5.90563962090602,30.2823540934936,57.0364972483744));
#90275=CARTESIAN_POINT('Ctrl Pts',(5.90950213916508,30.2116215424782,57.0450643409051));
#90276=CARTESIAN_POINT('Ctrl Pts',(5.91336465742414,30.1405544638856,57.0499370734688));
#90277=CARTESIAN_POINT('Ctrl Pts',(5.91722337851842,30.0695572499225,57.0548050157462));
#90278=CARTESIAN_POINT('Ctrl Pts',(5.9210820996127,29.9982266427402,57.0559857693842));
#90279=CARTESIAN_POINT('Ctrl Pts',(5.92494082070698,29.9269760556761,57.0534519877648));
#90280=CARTESIAN_POINT('Ctrl Pts',(5.92879703927701,29.8557716772699,57.0509198493972));
#90281=CARTESIAN_POINT('Ctrl Pts',(5.93265325784704,29.7846477002684,57.0446779736162));
#90282=CARTESIAN_POINT('Ctrl Pts',(5.93650947641706,29.7140182219434,57.0347510867719));
#90283=CARTESIAN_POINT('Ctrl Pts',(5.94036448407722,29.6434109223231,57.0248273171175));
#90284=CARTESIAN_POINT('Ctrl Pts',(5.94421949173738,29.5732982936435,57.0112209023425));
#90285=CARTESIAN_POINT('Ctrl Pts',(5.94807449939753,29.5040882643472,56.9940083031276));
#90286=CARTESIAN_POINT('Ctrl Pts',(5.95193183773653,29.4348363917225,56.9767852974377));
#90287=CARTESIAN_POINT('Ctrl Pts',(5.95578917607553,29.3664886826125,56.9559518624032));
#90288=CARTESIAN_POINT('Ctrl Pts',(5.95964651441454,29.2994408398931,56.9316351688894));
#90289=CARTESIAN_POINT('Ctrl Pts',(5.96350485094092,29.2323756467872,56.9073121827938));
#90290=CARTESIAN_POINT('Ctrl Pts',(5.96736318746731,29.1666114412787,56.8795043250355));
#90291=CARTESIAN_POINT('Ctrl Pts',(5.97122152399369,29.1025243457336,56.8483871381556));
#90292=CARTESIAN_POINT('Ctrl Pts',(5.97508578920756,29.038338774496,56.8172221368678));
#90293=CARTESIAN_POINT('Ctrl Pts',(5.97895005442143,28.9758358925275,56.7827378749951));
#90294=CARTESIAN_POINT('Ctrl Pts',(5.98281431963531,28.9153670640459,56.745155854571));
#90295=CARTESIAN_POINT('Ctrl Pts',(5.98650504958231,28.8576137516344,56.7092615562837));
#90296=CARTESIAN_POINT('Ctrl Pts',(5.99019577952932,28.8017160054131,56.6705420212124));
#90297=CARTESIAN_POINT('Ctrl Pts',(5.99388650947633,28.7479524050421,56.6292250864936));
#90298=CARTESIAN_POINT('Ctrl Pts',(5.29388070767824,28.7479524050421,56.6292250864936));
#90299=CARTESIAN_POINT('Ctrl Pts',(5.29774025035993,28.6913741458772,56.5857451070227));
#90300=CARTESIAN_POINT('Ctrl Pts',(5.30159979304163,28.6370931697353,56.5393373503055));
#90301=CARTESIAN_POINT('Ctrl Pts',(5.30545933572333,28.5854145236434,56.4902836953348));
#90302=CARTESIAN_POINT('Ctrl Pts',(5.30932116858873,28.5337052123657,56.4412009328013));
#90303=CARTESIAN_POINT('Ctrl Pts',(5.31318300145413,28.4846016390198,56.3894694995279));
#90304=CARTESIAN_POINT('Ctrl Pts',(5.31704483431953,28.4383704634804,56.3354065872121));
#90305=CARTESIAN_POINT('Ctrl Pts',(5.32091331711177,28.3920596796446,56.2812505806521));
#90306=CARTESIAN_POINT('Ctrl Pts',(5.32478179990401,28.3486314623212,56.2247554664636));
#90307=CARTESIAN_POINT('Ctrl Pts',(5.32865028269625,28.3083103737035,56.1662691673799));
#90308=CARTESIAN_POINT('Ctrl Pts',(5.33059785521445,28.2880108794798,56.1368244690565));
#90309=CARTESIAN_POINT('Ctrl Pts',(5.33254542773266,28.2684982009073,56.1068755093954));
#90310=CARTESIAN_POINT('Ctrl Pts',(5.33449300025086,28.2497965371344,56.0764689503526));
#90311=CARTESIAN_POINT('Ctrl Pts',(5.33836207359907,28.2126435642953,56.0160628776113));
#90312=CARTESIAN_POINT('Ctrl Pts',(5.34223114694728,28.1785487493108,55.9536127950323));
#90313=CARTESIAN_POINT('Ctrl Pts',(5.3461002202955,28.147742810437,55.8894609975778));
#90314=CARTESIAN_POINT('Ctrl Pts',(5.34996352869129,28.1169827726758,55.8254047868508));
#90315=CARTESIAN_POINT('Ctrl Pts',(5.35382683708707,28.0895020923366,55.7596523286275));
#90316=CARTESIAN_POINT('Ctrl Pts',(5.35769014548286,28.0654870977573,55.6925730239884));
#90317=CARTESIAN_POINT('Ctrl Pts',(5.36154892197578,28.0415002742717,55.6255724075777));
#90318=CARTESIAN_POINT('Ctrl Pts',(5.36540769846869,28.0209712240983,55.5572484915745));
#90319=CARTESIAN_POINT('Ctrl Pts',(5.3692664749616,28.0040386621116,55.4879917009076));
#90320=CARTESIAN_POINT('Ctrl Pts',(5.37312282054981,27.9871167670927,55.4187785397847));
#90321=CARTESIAN_POINT('Ctrl Pts',(5.37697916613801,27.9737869803035,55.348634140719));
#90322=CARTESIAN_POINT('Ctrl Pts',(5.38083551172622,27.9641380924165,55.2779637669743));
#90323=CARTESIAN_POINT('Ctrl Pts',(5.38469071797155,27.9544920552574,55.2073142725271));
#90324=CARTESIAN_POINT('Ctrl Pts',(5.38854592421688,27.9485248236772,55.1361395929656));
#90325=CARTESIAN_POINT('Ctrl Pts',(5.39240113046221,27.9462737202159,55.0648531435187));
#90326=CARTESIAN_POINT('Ctrl Pts',(5.39625648731345,27.944022528814,54.9935639092246));
#90327=CARTESIAN_POINT('Ctrl Pts',(5.40011184416469,27.9454877668835,54.9221633819897));
#90328=CARTESIAN_POINT('Ctrl Pts',(5.40396720101593,27.9506546621121,54.851066294691));
#90329=CARTESIAN_POINT('Ctrl Pts',(5.40782659348449,27.9558269658185,54.7798947861007));
#90330=CARTESIAN_POINT('Ctrl Pts',(5.41168598595305,27.9647086262349,54.7090278370035));
#90331=CARTESIAN_POINT('Ctrl Pts',(5.41554537842161,27.9772329265544,54.6388754659617));
#90332=CARTESIAN_POINT('Ctrl Pts',(5.41940695602504,27.9897643179602,54.5686833756135));
#90333=CARTESIAN_POINT('Ctrl Pts',(5.42326853362847,28.0059423446728,54.4992071420754));
#90334=CARTESIAN_POINT('Ctrl Pts',(5.4271301112319,28.0256496404589,54.4308442917092));
#90335=CARTESIAN_POINT('Ctrl Pts',(5.43099844534677,28.0453914176367,54.3623618284728));
#90336=CARTESIAN_POINT('Ctrl Pts',(5.43486677946164,28.0686746338715,54.2949970970483));
#90337=CARTESIAN_POINT('Ctrl Pts',(5.43873511357652,28.0953330110473,54.2291295675058));
#90338=CARTESIAN_POINT('Ctrl Pts',(5.44103283274748,28.1111675957767,54.1900054688939));
#90339=CARTESIAN_POINT('Ctrl Pts',(5.44333055191844,28.1281920767405,54.151409186527));
#90340=CARTESIAN_POINT('Ctrl Pts',(5.44562827108941,28.1463640450114,54.1134159324275));
#90341=CARTESIAN_POINT('Ctrl Pts',(5.44949734443762,28.1769633797821,54.0494400172219));
#90342=CARTESIAN_POINT('Ctrl Pts',(5.45336641778584,28.2109386112393,53.9869247961123));
#90343=CARTESIAN_POINT('Ctrl Pts',(5.45723549113405,28.2481272957714,53.9262497540495));
#90344=CARTESIAN_POINT('Ctrl Pts',(5.46109879952983,28.285260568845,53.8656651183191));
#90345=CARTESIAN_POINT('Ctrl Pts',(5.46496210792562,28.3255975390151,53.8069156298805));
#90346=CARTESIAN_POINT('Ctrl Pts',(5.4688254163214,28.3689289141422,53.750358181166));
#90347=CARTESIAN_POINT('Ctrl Pts',(5.47268419281431,28.4122094588506,53.6938670778834));
#90348=CARTESIAN_POINT('Ctrl Pts',(5.47654296930722,28.4584771372476,53.6395632904025));
#90349=CARTESIAN_POINT('Ctrl Pts',(5.48040174580014,28.5074791703103,53.5877751115908));
#90350=CARTESIAN_POINT('Ctrl Pts',(5.48425809138834,28.556450333673,53.5360195576611));
#90351=CARTESIAN_POINT('Ctrl Pts',(5.48811443697655,28.6081521010895,53.4867768203067));
#90352=CARTESIAN_POINT('Ctrl Pts',(5.49197078256476,28.6622921501111,53.4403412966788));
#90353=CARTESIAN_POINT('Ctrl Pts',(5.49582598881009,28.716416203658,53.3939194922524));
#90354=CARTESIAN_POINT('Ctrl Pts',(5.49968119505543,28.7729767401188,53.3503035710919));
#90355=CARTESIAN_POINT('Ctrl Pts',(5.50353640130077,28.8316466737575,53.3097491110613));
#90356=CARTESIAN_POINT('Ctrl Pts',(5.50739175815202,28.8903188993719,53.2691930667466));
#90357=CARTESIAN_POINT('Ctrl Pts',(5.51124711500326,28.9511002849051,53.2316989954189));
#90358=CARTESIAN_POINT('Ctrl Pts',(5.51510247185451,29.01363438323,53.1974794224326));
#90359=CARTESIAN_POINT('Ctrl Pts',(5.51896186432308,29.0762339394878,53.1632240299083));
#90360=CARTESIAN_POINT('Ctrl Pts',(5.52282125679163,29.1405894439088,53.132250211661));
#90361=CARTESIAN_POINT('Ctrl Pts',(5.5266806492602,29.2063202372391,53.1047242953375));
#90362=CARTESIAN_POINT('Ctrl Pts',(5.53054222686363,29.2720882464395,53.0771827942192));
#90363=CARTESIAN_POINT('Ctrl Pts',(5.53440380446706,29.3392326371751,53.0530932452881));
#90364=CARTESIAN_POINT('Ctrl Pts',(5.53826538207049,29.4073557750041,53.032572648081));
#90365=CARTESIAN_POINT('Ctrl Pts',(5.54213371618536,29.4755981062838,53.012016146468));
#90366=CARTESIAN_POINT('Ctrl Pts',(5.54600205030023,29.5448221317369,52.9950411796585));
#90367=CARTESIAN_POINT('Ctrl Pts',(5.5498703844151,29.6146188587501,52.9817138611017));
#90368=CARTESIAN_POINT('Ctrl Pts',(5.55216810358606,29.6560768282445,52.973797679501));
#90369=CARTESIAN_POINT('Ctrl Pts',(5.55446582275701,29.6977367133036,52.9671674501319));
#90370=CARTESIAN_POINT('Ctrl Pts',(5.55676354192797,29.739512323952,52.9618283357069));
#90371=CARTESIAN_POINT('Ctrl Pts',(5.56063261527619,29.8098572572268,52.9528379309675));
#90372=CARTESIAN_POINT('Ctrl Pts',(5.5645016886244,29.8808059628848,52.9474759921008));
#90373=CARTESIAN_POINT('Ctrl Pts',(5.56837076197262,29.9519515155083,52.9458118621611));
#90374=CARTESIAN_POINT('Ctrl Pts',(5.57223407036841,30.0229910606491,52.9441502117893));
#90375=CARTESIAN_POINT('Ctrl Pts',(5.5760973787642,30.0942263888595,52.946175444879));
#90376=CARTESIAN_POINT('Ctrl Pts',(5.57996068715999,30.1652441467217,52.9519052916249));
#90377=CARTESIAN_POINT('Ctrl Pts',(5.5838194636529,30.2361785963031,52.9576284169014));
#90378=CARTESIAN_POINT('Ctrl Pts',(5.58767824014582,30.3068955006345,52.9670474848391));
#90379=CARTESIAN_POINT('Ctrl Pts',(5.59153701663873,30.3769819483143,52.9801281790309));
#90380=CARTESIAN_POINT('Ctrl Pts',(5.59539336222694,30.4470242437931,52.9932006328073));
#90381=CARTESIAN_POINT('Ctrl Pts',(5.59924970781515,30.5164363941828,53.0099300474541));
#90382=CARTESIAN_POINT('Ctrl Pts',(5.60310605340336,30.5848125184159,53.0302305005905));
#90383=CARTESIAN_POINT('Ctrl Pts',(5.60696125964869,30.6531684411789,53.0505249560339));
#90384=CARTESIAN_POINT('Ctrl Pts',(5.61081646589403,30.7204884800177,53.0743882172142));
#90385=CARTESIAN_POINT('Ctrl Pts',(5.61467167213936,30.7863805132799,53.1016841014116));
#90386=CARTESIAN_POINT('Ctrl Pts',(5.61852702899061,30.8522751206535,53.1289810519388));
#90387=CARTESIAN_POINT('Ctrl Pts',(5.62238238584187,30.9167411637363,53.1597107037642));
#90388=CARTESIAN_POINT('Ctrl Pts',(5.62623774269312,30.9794067666008,53.1936888562497));
#90389=CARTESIAN_POINT('Ctrl Pts',(5.63009713516168,31.0421379650511,53.2277025755648));
#90390=CARTESIAN_POINT('Ctrl Pts',(5.63395652763024,31.1030645332306,53.2649713514497));
#90391=CARTESIAN_POINT('Ctrl Pts',(5.6378159200988,31.1618402761301,53.3052655856265));
#90392=CARTESIAN_POINT('Ctrl Pts',(5.64167749770225,31.2206492970461,53.3455826338439));
#90393=CARTESIAN_POINT('Ctrl Pts',(5.64553907530569,31.2773046824805,53.388928255033));
#90394=CARTESIAN_POINT('Ctrl Pts',(5.64940065290914,31.3314924733856,53.4350318355259));
#90395=CARTESIAN_POINT('Ctrl Pts',(5.65326898702401,31.3857750753928,53.4812160823682));
#90396=CARTESIAN_POINT('Ctrl Pts',(5.65713732113888,31.437581109668,53.5301675890948));
#90397=CARTESIAN_POINT('Ctrl Pts',(5.66100565525375,31.486633208518,53.5815786007566));
#90398=CARTESIAN_POINT('Ctrl Pts',(5.66330337442468,31.5157692512058,53.61211579418));
#90399=CARTESIAN_POINT('Ctrl Pts',(5.66560109359561,31.5439344211605,53.6435200799704));
#90400=CARTESIAN_POINT('Ctrl Pts',(5.66789881276654,31.571077634615,53.6757218462451));
#90401=CARTESIAN_POINT('Ctrl Pts',(5.67174314546748,31.6164911666132,53.7295988842593));
#90402=CARTESIAN_POINT('Ctrl Pts',(5.67558747816843,31.6592258384195,53.7859284481417));
#90403=CARTESIAN_POINT('Ctrl Pts',(5.67943181086938,31.6990035717013,53.8444116538117));
#90404=CARTESIAN_POINT('Ctrl Pts',(5.68327073565045,31.7387253486413,53.9028125896796));
#90405=CARTESIAN_POINT('Ctrl Pts',(5.68710966043152,31.7754981613696,53.9633607567449));
#90406=CARTESIAN_POINT('Ctrl Pts',(5.69094858521259,31.8090834220944,54.02572348155));
#90407=CARTESIAN_POINT('Ctrl Pts',(5.69478343427784,31.8426330259658,54.0880199969972));
#90408=CARTESIAN_POINT('Ctrl Pts',(5.69861828334308,31.8730015594206,54.1521268173281));
#90409=CARTESIAN_POINT('Ctrl Pts',(5.70245313240832,31.899994128269,54.2176830085934));
#90410=CARTESIAN_POINT('Ctrl Pts',(5.7062858215248,31.9269714937639,54.2832022758464));
#90411=CARTESIAN_POINT('Ctrl Pts',(5.71011851064129,31.9505764742473,54.3501688427883));
#90412=CARTESIAN_POINT('Ctrl Pts',(5.71395119975777,31.970661212502,54.4181993915093));
#90413=CARTESIAN_POINT('Ctrl Pts',(5.71778249936705,31.9907386692143,54.4862052763627));
#90414=CARTESIAN_POINT('Ctrl Pts',(5.72161379897633,32.007298281549,54.555273904177));
#90415=CARTESIAN_POINT('Ctrl Pts',(5.72544509858562,32.0202418689665,54.6250061955517));
#90416=CARTESIAN_POINT('Ctrl Pts',(5.72927810286536,32.0331912154093,54.6947695131027));
#90417=CARTESIAN_POINT('Ctrl Pts',(5.7331111071451,32.0425212306723,54.7651965997985));
#90418=CARTESIAN_POINT('Ctrl Pts',(5.73694411142483,32.048185000157,54.8358788020031));
#90419=CARTESIAN_POINT('Ctrl Pts',(5.73993783446245,32.0526086208859,54.8910843070446));
#90420=CARTESIAN_POINT('Ctrl Pts',(5.74293155750006,32.0547967824529,54.9464451824544));
#90421=CARTESIAN_POINT('Ctrl Pts',(5.74592528053768,32.0547492412566,55.0017658015851));
#90422=CARTESIAN_POINT('Origin',(-1.54592528053767,30.,55.));
#90423=CARTESIAN_POINT('',(4.59397380484682,28.7479524050421,56.6292250864936));
#90424=CARTESIAN_POINT('',(4.6520175253044,28.7479524050421,56.6292250864936));
#90425=CARTESIAN_POINT('',(-1.54592528053767,28.7479524050421,56.6292250864936));
#90426=CARTESIAN_POINT('',(5.10407471942445,32.0547498925786,55.0006644157262));
#90427=CARTESIAN_POINT('Ctrl Pts',(4.6520175253044,28.7479524050421,56.6292250864936));
#90428=CARTESIAN_POINT('Ctrl Pts',(4.65588667393895,28.6914965352496,56.5858391623626));
#90429=CARTESIAN_POINT('Ctrl Pts',(4.6597558225735,28.6373821256713,56.5395797426843));
#90430=CARTESIAN_POINT('Ctrl Pts',(4.66362497120805,28.5858980096712,56.4907424738862));
#90431=CARTESIAN_POINT('Ctrl Pts',(4.66425231405508,28.577550387246,56.482824010642));
#90432=CARTESIAN_POINT('Ctrl Pts',(4.66487965690211,28.5692718285588,56.474837849469));
#90433=CARTESIAN_POINT('Ctrl Pts',(4.66550699974914,28.5610634645336,56.4667853317374));
#90434=CARTESIAN_POINT('Ctrl Pts',(4.66937607309736,28.5104392123682,56.417122245773));
#90435=CARTESIAN_POINT('Ctrl Pts',(4.67324514644557,28.4622899074248,56.3647379575138));
#90436=CARTESIAN_POINT('Ctrl Pts',(4.67711421979379,28.4169220079584,56.3099090173037));
#90437=CARTESIAN_POINT('Ctrl Pts',(4.68097752818958,28.3716217070508,56.2551617726841));
#90438=CARTESIAN_POINT('Ctrl Pts',(4.68484083658536,28.3290948924322,56.1979774777012));
#90439=CARTESIAN_POINT('Ctrl Pts',(4.68870414498115,28.289611479732,56.1386696940885));
#90440=CARTESIAN_POINT('Ctrl Pts',(4.69256292147406,28.2501743835495,56.0794314822229));
#90441=CARTESIAN_POINT('Ctrl Pts',(4.69642169796697,28.2137738657556,56.0180751320759));
#90442=CARTESIAN_POINT('Ctrl Pts',(4.70028047445989,28.1806387041183,55.9549460914354));
#90443=CARTESIAN_POINT('Ctrl Pts',(4.70413682004809,28.1475244165639,55.891856820054));
#90444=CARTESIAN_POINT('Ctrl Pts',(4.7079931656363,28.11767162921,55.8269975028873));
#90445=CARTESIAN_POINT('Ctrl Pts',(4.71184951122451,28.0912642476933,55.7607400281082));
#90446=CARTESIAN_POINT('Ctrl Pts',(4.71570471746984,28.0648646681386,55.6945021288521));
#90447=CARTESIAN_POINT('Ctrl Pts',(4.71955992371517,28.0419086533007,55.626867343082));
#90448=CARTESIAN_POINT('Ctrl Pts',(4.7234151299605,28.0225321258001,55.5582278826853));
#90449=CARTESIAN_POINT('Ctrl Pts',(4.72727048681175,28.003154841344,55.4895857408473));
#90450=CARTESIAN_POINT('Ctrl Pts',(4.731125843663,27.9873574517059,55.4199393145738));
#90451=CARTESIAN_POINT('Ctrl Pts',(4.73498120051424,27.9752256400638,55.3496946580158));
#90452=CARTESIAN_POINT('Ctrl Pts',(4.7388405929828,27.9630811293769,55.279376472453));
#90453=CARTESIAN_POINT('Ctrl Pts',(4.74269998545136,27.9546099389754,55.2084592862478));
#90454=CARTESIAN_POINT('Ctrl Pts',(4.74655937791992,27.9498462038099,55.1373571056304));
#90455=CARTESIAN_POINT('Ctrl Pts',(4.75042095552336,27.9450797714831,55.0662146679373));
#90456=CARTESIAN_POINT('Ctrl Pts',(4.75428253312679,27.9440249802595,54.9948875132875));
#90457=CARTESIAN_POINT('Ctrl Pts',(4.75814411073023,27.9466637979444,54.9237897393517));
#90458=CARTESIAN_POINT('Ctrl Pts',(4.7620124448451,27.9493072327066,54.8525675673143));
#90459=CARTESIAN_POINT('Ctrl Pts',(4.76588077895997,27.9556571358943,54.7815760612898));
#90460=CARTESIAN_POINT('Ctrl Pts',(4.76974911307484,27.9656436525551,54.7112235914919));
#90461=CARTESIAN_POINT('Ctrl Pts',(4.7720468322458,27.9715754594005,54.6694355210258));
#90462=CARTESIAN_POINT('Ctrl Pts',(4.77434455141675,27.9787893326922,54.6278727252012));
#90463=CARTESIAN_POINT('Ctrl Pts',(4.77664227058771,27.9872622538327,54.586618423665));
#90464=CARTESIAN_POINT('Ctrl Pts',(4.78051134393593,28.0015295993727,54.5171513101072));
#90465=CARTESIAN_POINT('Ctrl Pts',(4.78438041728414,28.0194254679784,54.4482876251215));
#90466=CARTESIAN_POINT('Ctrl Pts',(4.78824949063236,28.0408837296112,54.3804348286113));
#90467=CARTESIAN_POINT('Ctrl Pts',(4.79211279902815,28.0623100182504,54.312683133349));
#90468=CARTESIAN_POINT('Ctrl Pts',(4.79597610742393,28.0872880184086,54.2459397961355));
#90469=CARTESIAN_POINT('Ctrl Pts',(4.79983941581972,28.1157006857587,54.1806016494709));
#90470=CARTESIAN_POINT('Ctrl Pts',(4.80369819231263,28.1440800232693,54.1153401485473));
#90471=CARTESIAN_POINT('Ctrl Pts',(4.80755696880555,28.1758858320737,54.0514810072649));
#90472=CARTESIAN_POINT('Ctrl Pts',(4.81141574529846,28.2109519672827,53.9894037902653));
#90473=CARTESIAN_POINT('Ctrl Pts',(4.81527209088667,28.2459960119577,53.9273656799098));
#90474=CARTESIAN_POINT('Ctrl Pts',(4.81912843647487,28.2842960697709,53.867107688675));
#90475=CARTESIAN_POINT('Ctrl Pts',(4.82298478206308,28.3256394450817,53.808986022486));
#90476=CARTESIAN_POINT('Ctrl Pts',(4.82683998830841,28.3669706056469,53.7508815281258));
#90477=CARTESIAN_POINT('Ctrl Pts',(4.83069519455375,28.411343017247,53.6949125014039));
#90478=CARTESIAN_POINT('Ctrl Pts',(4.83455040079908,28.4585008851392,53.641405858476));
#90479=CARTESIAN_POINT('Ctrl Pts',(4.83840575765033,28.5056605952813,53.5878971252795));
#90480=CARTESIAN_POINT('Ctrl Pts',(4.84226111450158,28.5556056549018,53.5368513298448));
#90481=CARTESIAN_POINT('Ctrl Pts',(4.84611647135282,28.6080413916997,53.4885606875304));
#90482=CARTESIAN_POINT('Ctrl Pts',(4.84997586382138,28.6605320159115,53.4402194967039));
#90483=CARTESIAN_POINT('Ctrl Pts',(4.85383525628994,28.7155181636516,53.3946395458177));
#90484=CARTESIAN_POINT('Ctrl Pts',(4.8576946487585,28.7726705238238,53.3520740552412));
#90485=CARTESIAN_POINT('Ctrl Pts',(4.86155622636194,28.8298552428755,53.30948446467));
#90486=CARTESIAN_POINT('Ctrl Pts',(4.86541780396537,28.8892082115208,53.2699130016197));
#90487=CARTESIAN_POINT('Ctrl Pts',(4.86927938156881,28.9503717482546,53.2335691081625));
#90488=CARTESIAN_POINT('Ctrl Pts',(4.87314771568368,29.0116423013889,53.1971616246504));
#90489=CARTESIAN_POINT('Ctrl Pts',(4.87701604979855,29.0747293173161,53.1639932116718));
#90490=CARTESIAN_POINT('Ctrl Pts',(4.88088438391342,29.1392518196144,53.1342266663759));
#90491=CARTESIAN_POINT('Ctrl Pts',(4.88318210308437,29.1775769968317,53.1165458870667));
#90492=CARTESIAN_POINT('Ctrl Pts',(4.88547982225532,29.2164082578056,53.1000644084989));
#90493=CARTESIAN_POINT('Ctrl Pts',(4.88777754142626,29.2556632016253,53.0848080270935));
#90494=CARTESIAN_POINT('Ctrl Pts',(4.89164661477447,29.3217636454215,53.0591181780328));
#90495=CARTESIAN_POINT('Ctrl Pts',(4.89551568812269,29.3893251031837,53.0368040872381));
#90496=CARTESIAN_POINT('Ctrl Pts',(4.8993847614709,29.4579693835411,53.0180311876013));
#90497=CARTESIAN_POINT('Ctrl Pts',(4.90324806986669,29.5265113833328,52.9992862597457));
#90498=CARTESIAN_POINT('Ctrl Pts',(4.90711137826247,29.596132538375,52.9840721766353));
#90499=CARTESIAN_POINT('Ctrl Pts',(4.91097468665826,29.6664359717593,52.9725058319285));
#90500=CARTESIAN_POINT('Ctrl Pts',(4.91483346315117,29.7366569348102,52.960953055269));
#90501=CARTESIAN_POINT('Ctrl Pts',(4.91869223964408,29.8075581094114,52.9530395958994));
#90502=CARTESIAN_POINT('Ctrl Pts',(4.922551016137,29.8787304957534,52.9488317304912));
#90503=CARTESIAN_POINT('Ctrl Pts',(4.9264073617252,29.9498580457881,52.9446265159024));
#90504=CARTESIAN_POINT('Ctrl Pts',(4.93026370731341,30.0212559847979,52.9441222924568));
#90505=CARTESIAN_POINT('Ctrl Pts',(4.93412005290161,30.0925096901931,52.9473335585828));
#90506=CARTESIAN_POINT('Ctrl Pts',(4.93797525914695,30.1637423439476,52.9505438759522));
#90507=CARTESIAN_POINT('Ctrl Pts',(4.94183046539228,30.2348303636575,52.9574674817409));
#90508=CARTESIAN_POINT('Ctrl Pts',(4.94568567163761,30.3053603589388,52.9680667792251));
#90509=CARTESIAN_POINT('Ctrl Pts',(4.94954102848885,30.3758931095161,52.9786664907771));
#90510=CARTESIAN_POINT('Ctrl Pts',(4.9533963853401,30.4458673123203,52.9929421047382));
#90511=CARTESIAN_POINT('Ctrl Pts',(4.95725174219134,30.5148776448274,53.0108045411883));
#90512=CARTESIAN_POINT('Ctrl Pts',(4.9611111346599,30.5839602143033,53.0286856752482));
#90513=CARTESIAN_POINT('Ctrl Pts',(4.96497052712846,30.6520764281661,53.0501610047003));
#90514=CARTESIAN_POINT('Ctrl Pts',(4.96882991959702,30.7188349384421,53.0750911985824));
#90515=CARTESIAN_POINT('Ctrl Pts',(4.97269149720045,30.7856312464675,53.1000355075971));
#90516=CARTESIAN_POINT('Ctrl Pts',(4.97655307480389,30.8510678748055,53.1284383815136));
#90517=CARTESIAN_POINT('Ctrl Pts',(4.98041465240732,30.9147748684456,53.1601129103773));
#90518=CARTESIAN_POINT('Ctrl Pts',(4.98428298652219,30.978593328713,53.1918428594186));
#90519=CARTESIAN_POINT('Ctrl Pts',(4.98815132063707,31.0406756889177,53.2268556535021));
#90520=CARTESIAN_POINT('Ctrl Pts',(4.99201965475194,31.1006785481548,53.2649195130681));
#90521=CARTESIAN_POINT('Ctrl Pts',(4.9943173739229,31.1363191406909,53.2875287441346));
#90522=CARTESIAN_POINT('Ctrl Pts',(4.99661509309386,31.1712266300883,53.311213615859));
#90523=CARTESIAN_POINT('Ctrl Pts',(4.99891281226483,31.2053346523553,53.3359188906993));
#90524=CARTESIAN_POINT('Ctrl Pts',(5.00275064676246,31.26230460158,53.3771836184579));
#90525=CARTESIAN_POINT('Ctrl Pts',(5.00658848126009,31.3172734889281,53.4214646825556));
#90526=CARTESIAN_POINT('Ctrl Pts',(5.01042631575773,31.3699002709869,53.4685396479014));
#90527=CARTESIAN_POINT('Ctrl Pts',(5.01432833257717,31.4234071611025,53.5164018750681));
#90528=CARTESIAN_POINT('Ctrl Pts',(5.01823034939662,31.4744924192996,53.5671520862871));
#90529=CARTESIAN_POINT('Ctrl Pts',(5.02213236621606,31.522828336926,53.6205104499289));
#90530=CARTESIAN_POINT('Ctrl Pts',(5.02595997436977,31.5702425232262,53.6728513077966));
#90531=CARTESIAN_POINT('Ctrl Pts',(5.02978758252348,31.6150109502794,53.7277013416823));
#90532=CARTESIAN_POINT('Ctrl Pts',(5.03361519067719,31.6568593683213,53.7847573920792));
#90533=CARTESIAN_POINT('Ctrl Pts',(5.03744050268938,31.6986826819412,53.8417792151569));
#90534=CARTESIAN_POINT('Ctrl Pts',(5.04126581470158,31.7375891686526,53.901004032373));
#90535=CARTESIAN_POINT('Ctrl Pts',(5.04509112671377,31.7733450235497,53.9620958666853));
#90536=CARTESIAN_POINT('Ctrl Pts',(5.04891547573736,31.8090918772253,54.0231723216665));
#90537=CARTESIAN_POINT('Ctrl Pts',(5.05273982476095,31.8416894240058,54.0861144340417));
#90538=CARTESIAN_POINT('Ctrl Pts',(5.05656417378454,31.8709483479536,54.1505591004728));
#90539=CARTESIAN_POINT('Ctrl Pts',(5.0605233859212,31.901239068305,54.2172763650066));
#90540=CARTESIAN_POINT('Ctrl Pts',(5.06448259805786,31.9279510192921,54.2856036450338));
#90541=CARTESIAN_POINT('Ctrl Pts',(5.06844181019452,31.9509280911055,54.3551146258167));
#90542=CARTESIAN_POINT('Ctrl Pts',(5.07227054686683,31.9731479556739,54.4223348787524));
#90543=CARTESIAN_POINT('Ctrl Pts',(5.07609928353915,31.9918752129524,54.490661515234));
#90544=CARTESIAN_POINT('Ctrl Pts',(5.07992802021147,32.0070199603936,54.5596950589858));
#90545=CARTESIAN_POINT('Ctrl Pts',(5.0839524700803,32.0229388605609,54.6322573843359));
#90546=CARTESIAN_POINT('Ctrl Pts',(5.08797691994912,32.0348990846252,54.7056002068221));
#90547=CARTESIAN_POINT('Ctrl Pts',(5.09200136981795,32.0428577974627,54.779252221198));
#90548=CARTESIAN_POINT('Ctrl Pts',(5.09602581968678,32.0508165103001,54.8529042355738));
#90549=CARTESIAN_POINT('Ctrl Pts',(5.10005026955561,32.0547737561238,54.9268648126138));
#90550=CARTESIAN_POINT('Ctrl Pts',(5.10407471942444,32.0547498925786,55.0006644157262));
#90551=CARTESIAN_POINT('Ctrl Pts',(5.10407471946233,32.0547498925784,55.0006644164209));
#90552=CARTESIAN_POINT('Ctrl Pts',(5.10606584067601,32.0547380859309,55.0371772219239));
#90553=CARTESIAN_POINT('Ctrl Pts',(5.1080569618897,32.0537530962652,55.0736730530944));
#90554=CARTESIAN_POINT('Ctrl Pts',(5.11004808310338,32.0517972511101,55.1101163150356));
#90555=CARTESIAN_POINT('Ctrl Pts',(5.1139171564516,32.0479967248986,55.1809315183137));
#90556=CARTESIAN_POINT('Ctrl Pts',(5.11778622979981,32.040518304,55.2516884433728));
#90557=CARTESIAN_POINT('Ctrl Pts',(5.12165530314803,32.02936691962,55.3219743282499));
#90558=CARTESIAN_POINT('Ctrl Pts',(5.12551861154381,32.0182321508982,55.3921554865566));
#90559=CARTESIAN_POINT('Ctrl Pts',(5.1293819199396,32.0034353574455,55.4618665219658));
#90560=CARTESIAN_POINT('Ctrl Pts',(5.13324522833539,31.9850333981067,55.5306976266206));
#90561=CARTESIAN_POINT('Ctrl Pts',(5.1371040048283,31.9666530254196,55.5994479880758));
#90562=CARTESIAN_POINT('Ctrl Pts',(5.14096278132121,31.9446760120999,55.667320002077));
#90563=CARTESIAN_POINT('Ctrl Pts',(5.14482155781412,31.9192103364242,55.733913650958));
#90564=CARTESIAN_POINT('Ctrl Pts',(5.14867790340233,31.8937607033027,55.8004653479885));
#90565=CARTESIAN_POINT('Ctrl Pts',(5.15253424899053,31.8648269412174,55.8657398249892));
#90566=CARTESIAN_POINT('Ctrl Pts',(5.15639059457873,31.8325665301756,55.9293532562918));
#90567=CARTESIAN_POINT('Ctrl Pts',(5.16024580082406,31.8003156503515,55.9929478932441));
#90568=CARTESIAN_POINT('Ctrl Pts',(5.1641010070694,31.7647402923912,56.054882025751));
#90569=CARTESIAN_POINT('Ctrl Pts',(5.16795621331473,31.726044904763,56.1147943977442));
#90570=CARTESIAN_POINT('Ctrl Pts',(5.17181157016597,31.6873480054765,56.1747091102496));
#90571=CARTESIAN_POINT('Ctrl Pts',(5.17566692701722,31.645531099945,56.232601498556));
#90572=CARTESIAN_POINT('Ctrl Pts',(5.17952228386847,31.6008422332874,56.2881388537823));
#90573=CARTESIAN_POINT('Ctrl Pts',(5.18338167633703,31.5561065882974,56.3437343430597));
#90574=CARTESIAN_POINT('Ctrl Pts',(5.18724106880558,31.5084932862138,56.3969694990261));
#90575=CARTESIAN_POINT('Ctrl Pts',(5.19110046127414,31.45829041423,56.4475450356604));
#90576=CARTESIAN_POINT('Ctrl Pts',(5.19496203887757,31.4080591180712,56.4981492074672));
#90577=CARTESIAN_POINT('Ctrl Pts',(5.198823616481,31.3552356931969,56.5460904356481));
#90578=CARTESIAN_POINT('Ctrl Pts',(5.20268519408444,31.3001427797329,56.5911085176092));
#90579=CARTESIAN_POINT('Ctrl Pts',(5.20655352819931,31.244953471495,56.6362053666486));
#90580=CARTESIAN_POINT('Ctrl Pts',(5.21042186231418,31.1874871385044,56.6783685706389));
#90581=CARTESIAN_POINT('Ctrl Pts',(5.21429019642905,31.1280963799291,56.7173805984961));
#90582=CARTESIAN_POINT('Ctrl Pts',(5.21658791560001,31.0928193639051,56.7405530240529));
#90583=CARTESIAN_POINT('Ctrl Pts',(5.21888563477098,31.0568638927504,56.762614530318));
#90584=CARTESIAN_POINT('Ctrl Pts',(5.22118335394194,31.0203076268373,56.7835273782921));
#90585=CARTESIAN_POINT('Ctrl Pts',(5.22505242729016,30.9587514210389,56.8187420136377));
#90586=CARTESIAN_POINT('Ctrl Pts',(5.22892150063837,30.8952494193225,56.8508350814401));
#90587=CARTESIAN_POINT('Ctrl Pts',(5.23279057398659,30.8301510755014,56.8795868573556));
#90588=CARTESIAN_POINT('Ctrl Pts',(5.23665388238237,30.7651497287701,56.9082957928788));
#90589=CARTESIAN_POINT('Ctrl Pts',(5.24051719077816,30.6985572020688,56.9336731241379));
#90590=CARTESIAN_POINT('Ctrl Pts',(5.24438049917394,30.6307486310241,56.9555443556619));
#90591=CARTESIAN_POINT('Ctrl Pts',(5.24823927566685,30.563019603683,56.9773899308606));
#90592=CARTESIAN_POINT('Ctrl Pts',(5.25209805215977,30.4940778255901,56.9957374274862));
#90593=CARTESIAN_POINT('Ctrl Pts',(5.25595682865268,30.4243179325502,57.0104606075764));
#90594=CARTESIAN_POINT('Ctrl Pts',(5.25981317424089,30.3546019859924,57.0251745125381));
#90595=CARTESIAN_POINT('Ctrl Pts',(5.26366951982909,30.2840694211964,57.0362685307208));
#90596=CARTESIAN_POINT('Ctrl Pts',(5.2675258654173,30.2131281183253,57.0436667946804));
#90597=CARTESIAN_POINT('Ctrl Pts',(5.27138107166263,30.1422077747966,57.0510628728505));
#90598=CARTESIAN_POINT('Ctrl Pts',(5.27523627790797,30.0708794158375,57.0547653141544));
#90599=CARTESIAN_POINT('Ctrl Pts',(5.2790914841533,29.9995574339136,57.0547499523385));
#90600=CARTESIAN_POINT('Ctrl Pts',(5.28294684100455,29.9282326657542,57.0547345899226));
#90601=CARTESIAN_POINT('Ctrl Pts',(5.28680219785579,29.8569147609101,57.0510011383427));
#90602=CARTESIAN_POINT('Ctrl Pts',(5.29065755470704,29.7860177733686,57.04357754176));
#90603=CARTESIAN_POINT('Ctrl Pts',(5.2945169471756,29.7150465739912,57.0361461744842));
#90604=CARTESIAN_POINT('Ctrl Pts',(5.29837633964416,29.6444976555829,57.02501700212));
#90605=CARTESIAN_POINT('Ctrl Pts',(5.30223573211272,29.5747787095139,57.0102697372784));
#90606=CARTESIAN_POINT('Ctrl Pts',(5.30609730971616,29.5050202895377,56.9955141227385));
#90607=CARTESIAN_POINT('Ctrl Pts',(5.30995888731959,29.436093246975,56.9771364629712));
#90608=CARTESIAN_POINT('Ctrl Pts',(5.31382046492302,29.3683911777761,56.9552666974582));
#90609=CARTESIAN_POINT('Ctrl Pts',(5.3176887990379,29.3005706518603,56.9333586669312));
#90610=CARTESIAN_POINT('Ctrl Pts',(5.32155713315277,29.2339798324878,56.9079465050117));
#90611=CARTESIAN_POINT('Ctrl Pts',(5.32542546726764,29.168992714123,56.8792084645721));
#90612=CARTESIAN_POINT('Ctrl Pts',(5.32772318643859,29.1303915635248,56.8621385981921));
#90613=CARTESIAN_POINT('Ctrl Pts',(5.33002090560955,29.0923557749171,56.8438962093788));
#90614=CARTESIAN_POINT('Ctrl Pts',(5.33231862478051,29.0549591746737,56.8245260757157));
#90615=CARTESIAN_POINT('Ctrl Pts',(5.33618678846678,28.9920027555951,56.7919168480168));
#90616=CARTESIAN_POINT('Ctrl Pts',(5.34005495215306,28.930612833919,56.7559814127838));
#90617=CARTESIAN_POINT('Ctrl Pts',(5.34392311583933,28.8711632793371,56.7168940621317));
#90618=CARTESIAN_POINT('Ctrl Pts',(5.34666138852714,28.8290789455763,56.6892241305025));
#90619=CARTESIAN_POINT('Ctrl Pts',(5.34939966121495,28.7879666574385,56.6599757475854));
#90620=CARTESIAN_POINT('Ctrl Pts',(5.35213793390276,28.7479524050421,56.6292250864936));
#90621=CARTESIAN_POINT('',(5.04592528049196,32.0547497417017,54.9989697199742));
#90622=CARTESIAN_POINT('Ctrl Pts',(5.04592528053768,32.0547497417021,54.9989697208213));
#90623=CARTESIAN_POINT('Ctrl Pts',(5.04983580638859,32.0547860725486,55.0714265840048));
#90624=CARTESIAN_POINT('Ctrl Pts',(5.0537463322395,32.0509854787254,55.1438783326772));
#90625=CARTESIAN_POINT('Ctrl Pts',(5.05765685809041,32.0433759542005,55.2158987547329));
#90626=CARTESIAN_POINT('Ctrl Pts',(5.06156889758461,32.0357634842646,55.2879470536605));
#90627=CARTESIAN_POINT('Ctrl Pts',(5.0654809370788,32.0243392038328,55.3595632307956));
#90628=CARTESIAN_POINT('Ctrl Pts',(5.069392976573,32.0091827682212,55.4303279753663));
#90629=CARTESIAN_POINT('Ctrl Pts',(5.07331083119321,31.9940038030357,55.5011979095466));
#90630=CARTESIAN_POINT('Ctrl Pts',(5.07722868581341,31.9750817055291,55.5712134277556));
#90631=CARTESIAN_POINT('Ctrl Pts',(5.08114654043362,31.9525468000705,55.6399676210829));
#90632=CARTESIAN_POINT('Ctrl Pts',(5.08506751736912,31.9299939355279,55.708776607732));
#90633=CARTESIAN_POINT('Ctrl Pts',(5.08898849430461,31.9038226982931,55.7763218332456));
#90634=CARTESIAN_POINT('Ctrl Pts',(5.09290947124011,31.8742116465852,55.8422162823791));
#90635=CARTESIAN_POINT('Ctrl Pts',(5.0968384919827,31.8445398483868,55.9082459126795));
#90636=CARTESIAN_POINT('Ctrl Pts',(5.10076751272528,31.8114143545489,55.9726175877549));
#90637=CARTESIAN_POINT('Ctrl Pts',(5.10469653346786,31.7750596081185,56.0349690575694));
#90638=CARTESIAN_POINT('Ctrl Pts',(5.10720517516982,31.7518474545224,56.0747798673368));
#90639=CARTESIAN_POINT('Ctrl Pts',(5.10971381687178,31.7273197264889,56.1137676684778));
#90640=CARTESIAN_POINT('Ctrl Pts',(5.11222245857374,31.7015435920207,56.1518450273163));
#90641=CARTESIAN_POINT('Ctrl Pts',(5.11609153192196,31.6617891086231,56.2105716657746));
#90642=CARTESIAN_POINT('Ctrl Pts',(5.11996060527018,31.6189128733263,56.2673528041018));
#90643=CARTESIAN_POINT('Ctrl Pts',(5.12382967861839,31.5731318462584,56.3218372656223));
#90644=CARTESIAN_POINT('Ctrl Pts',(5.12769298701418,31.5274190333129,56.3762405448283));
#90645=CARTESIAN_POINT('Ctrl Pts',(5.13155629540997,31.4788103298453,56.4283535710454));
#90646=CARTESIAN_POINT('Ctrl Pts',(5.13541960380576,31.4275656730795,56.477854462234));
#90647=CARTESIAN_POINT('Ctrl Pts',(5.13927838029867,31.3763811295078,56.5272972857749));
#90648=CARTESIAN_POINT('Ctrl Pts',(5.14313715679158,31.3225671223705,56.5741337249527));
#90649=CARTESIAN_POINT('Ctrl Pts',(5.1469959332845,31.2664223501252,56.6180766340329));
#90650=CARTESIAN_POINT('Ctrl Pts',(5.1508522788727,31.2103129472751,56.6619918604981));
#90651=CARTESIAN_POINT('Ctrl Pts',(5.15470862446091,31.1518760740568,56.7030168746311));
#90652=CARTESIAN_POINT('Ctrl Pts',(5.15856497004912,31.0914445044239,56.7409039193083));
#90653=CARTESIAN_POINT('Ctrl Pts',(5.16242017629445,31.0310307890721,56.7787797703999));
#90654=CARTESIAN_POINT('Ctrl Pts',(5.16627538253979,30.968623958642,56.8135192346888));
#90655=CARTESIAN_POINT('Ctrl Pts',(5.17013058878512,30.9045854047204,56.8449181033495));
#90656=CARTESIAN_POINT('Ctrl Pts',(5.17398594563637,30.8405443490947,56.8763181986257));
#90657=CARTESIAN_POINT('Ctrl Pts',(5.17784130248762,30.7748718805687,56.9043772272931));
#90658=CARTESIAN_POINT('Ctrl Pts',(5.18169665933887,30.7079520380719,56.9289379135394));
#90659=CARTESIAN_POINT('Ctrl Pts',(5.18555605180743,30.640962146839,56.9535243088276));
#90660=CARTESIAN_POINT('Ctrl Pts',(5.18941544427599,30.5727227321486,56.974604883981));
#90661=CARTESIAN_POINT('Ctrl Pts',(5.19327483674455,30.5036349212799,56.9920716424284));
#90662=CARTESIAN_POINT('Ctrl Pts',(5.19713641434798,30.4345079938441,57.0095482903139));
#90663=CARTESIAN_POINT('Ctrl Pts',(5.20099799195142,30.364532190757,57.0234069539317));
#90664=CARTESIAN_POINT('Ctrl Pts',(5.20485956955485,30.2941181062907,57.0335909377385));
#90665=CARTESIAN_POINT('Ctrl Pts',(5.20872790366972,30.2235808199582,57.0437927402219));
#90666=CARTESIAN_POINT('Ctrl Pts',(5.21259623778459,30.1526042051134,57.0503069817965));
#90667=CARTESIAN_POINT('Ctrl Pts',(5.21646457189946,30.0816025369965,57.0531289751147));
#90668=CARTESIAN_POINT('Ctrl Pts',(5.21876229107041,30.0394288546937,57.0548051871365));
#90669=CARTESIAN_POINT('Ctrl Pts',(5.22106001024135,29.9972463264547,57.0551797214769));
#90670=CARTESIAN_POINT('Ctrl Pts',(5.2233577294123,29.9551409540643,57.0542602630869));
#90671=CARTESIAN_POINT('Ctrl Pts',(5.2272261855104,29.8842520540425,57.052712256498));
#90672=CARTESIAN_POINT('Ctrl Pts',(5.23109464160851,29.8133045461066,57.0474875355493));
#90673=CARTESIAN_POINT('Ctrl Pts',(5.23496309770662,29.7427109426911,57.0385779120478));
#90674=CARTESIAN_POINT('Ctrl Pts',(5.23882613522175,29.6722162204024,57.02968076834));
#90675=CARTESIAN_POINT('Ctrl Pts',(5.24268917273688,29.6020748968272,57.0171090230153));
#90676=CARTESIAN_POINT('Ctrl Pts',(5.24655221025201,29.5326982937989,57.0009064640511));
#90677=CARTESIAN_POINT('Ctrl Pts',(5.2504962517042,29.4618669345165,56.9843641540332));
#90678=CARTESIAN_POINT('Ctrl Pts',(5.25444029315638,29.3918332494984,56.9640370254787));
#90679=CARTESIAN_POINT('Ctrl Pts',(5.25838433460857,29.323027683322,56.9400273309806));
#90680=CARTESIAN_POINT('Ctrl Pts',(5.26224054865168,29.2557543055571,56.9165522934546));
#90681=CARTESIAN_POINT('Ctrl Pts',(5.26609676269479,29.1896553918124,56.8895571900547));
#90682=CARTESIAN_POINT('Ctrl Pts',(5.26995297673789,29.1251191575739,56.8591882836485));
#90683=CARTESIAN_POINT('Ctrl Pts',(5.27394093189462,29.0583781506563,56.8277818742655));
#90684=CARTESIAN_POINT('Ctrl Pts',(5.27792888705134,28.9933090523761,56.7927671232011));
#90685=CARTESIAN_POINT('Ctrl Pts',(5.28191684220807,28.9303176686924,56.7543595049443));
#90686=CARTESIAN_POINT('Ctrl Pts',(5.28590479736479,28.8673262850087,56.7159518866875));
#90687=CARTESIAN_POINT('Ctrl Pts',(5.28989275252152,28.8064131033691,56.6741517067297));
#90688=CARTESIAN_POINT('Ctrl Pts',(5.29388070767824,28.7479524050421,56.6292250864936));
#90689=CARTESIAN_POINT('Ctrl Pts',(4.59397380484682,28.7479524050421,56.6292250864936));
#90690=CARTESIAN_POINT('Ctrl Pts',(4.5978297750184,28.6914443882701,56.5857990877893));
#90691=CARTESIAN_POINT('Ctrl Pts',(4.60168574518998,28.6371627163018,56.5394024137685));
#90692=CARTESIAN_POINT('Ctrl Pts',(4.60554171536156,28.5854289256007,56.4902973656196));
#90693=CARTESIAN_POINT('Ctrl Pts',(4.60939684217606,28.5337064498362,56.441203057463));
#90694=CARTESIAN_POINT('Ctrl Pts',(4.61325196899057,28.4845311008614,56.3894018859296));
#90695=CARTESIAN_POINT('Ctrl Pts',(4.61710709580507,28.4381891114174,56.3351944842624));
#90696=CARTESIAN_POINT('Ctrl Pts',(4.62096266902407,28.3918417558017,56.280980805648));
#90697=CARTESIAN_POINT('Ctrl Pts',(4.62481824224307,28.3483287247538,56.2243607146393));
#90698=CARTESIAN_POINT('Ctrl Pts',(4.62867381546206,28.3078962192091,56.1656682021626));
#90699=CARTESIAN_POINT('Ctrl Pts',(4.63253360638861,28.2674194835398,56.1069114844851));
#90700=CARTESIAN_POINT('Ctrl Pts',(4.63639339731515,28.2300302732144,56.0460782226223));
#90701=CARTESIAN_POINT('Ctrl Pts',(4.6402531882417,28.1959311208761,55.9835309053999));
#90702=CARTESIAN_POINT('Ctrl Pts',(4.64411543010531,28.1618103158427,55.9209438711201));
#90703=CARTESIAN_POINT('Ctrl Pts',(4.64797767196891,28.1309839357524,55.8566410535872));
#90704=CARTESIAN_POINT('Ctrl Pts',(4.65183991383252,28.1036070581878,55.7910065567016));
#90705=CARTESIAN_POINT('Ctrl Pts',(4.65570864680383,28.0761841694549,55.7252617506735));
#90706=CARTESIAN_POINT('Ctrl Pts',(4.65957737977513,28.0522225139632,55.6581812563938));
#90707=CARTESIAN_POINT('Ctrl Pts',(4.66344611274644,28.0318275943512,55.5901651837772));
#90708=CARTESIAN_POINT('Ctrl Pts',(4.66485786690413,28.024385206166,55.56534517836));
#90709=CARTESIAN_POINT('Ctrl Pts',(4.66626962106181,28.0174172795207,55.5404006892119));
#90710=CARTESIAN_POINT('Ctrl Pts',(4.66768137521949,28.0109272352027,55.515351432366));
#90711=CARTESIAN_POINT('Ctrl Pts',(4.67155044856771,27.9931405282447,55.4467010858963));
#90712=CARTESIAN_POINT('Ctrl Pts',(4.67541952191593,27.9788772247288,55.3769943617172));
#90713=CARTESIAN_POINT('Ctrl Pts',(4.67928859526415,27.9682574135064,55.3066261970675));
#90714=CARTESIAN_POINT('Ctrl Pts',(4.68315190365994,27.9576534258936,55.2363628815859));
#90715=CARTESIAN_POINT('Ctrl Pts',(4.68701521205573,27.9506822263921,55.1654405583595));
#90716=CARTESIAN_POINT('Ctrl Pts',(4.69087852045152,27.9474135131066,55.0942670479151));
#90717=CARTESIAN_POINT('Ctrl Pts',(4.69473729694444,27.9441486342267,55.0231770284592));
#90718=CARTESIAN_POINT('Ctrl Pts',(4.69859607343735,27.9445776365808,54.9518368899955));
#90719=CARTESIAN_POINT('Ctrl Pts',(4.70245484993026,27.9487185311776,54.8806605758113));
#90720=CARTESIAN_POINT('Ctrl Pts',(4.70631119551847,27.9528568171443,54.8095291004089));
#90721=CARTESIAN_POINT('Ctrl Pts',(4.71016754110668,27.960702327913,54.7385617283502));
#90722=CARTESIAN_POINT('Ctrl Pts',(4.71402388669489,27.9722209939527,54.6681719343788));
#90723=CARTESIAN_POINT('Ctrl Pts',(4.71787909294022,27.9837362568457,54.5978029368086));
#90724=CARTESIAN_POINT('Ctrl Pts',(4.72173429918555,27.9989224421392,54.5280116576999));
#90725=CARTESIAN_POINT('Ctrl Pts',(4.72558950543088,28.0176938863608,54.4592042582187));
#90726=CARTESIAN_POINT('Ctrl Pts',(4.72944486228214,28.0364660639002,54.3903941707354));
#90727=CARTESIAN_POINT('Ctrl Pts',(4.73330021913339,28.0588236484586,54.3225685072681));
#90728=CARTESIAN_POINT('Ctrl Pts',(4.73715557598465,28.0846307894571,54.2561193981531));
#90729=CARTESIAN_POINT('Ctrl Pts',(4.74101496845321,28.1104649442312,54.1896007330449));
#90730=CARTESIAN_POINT('Ctrl Pts',(4.74487436092177,28.1397556872707,54.1244619524432));
#90731=CARTESIAN_POINT('Ctrl Pts',(4.74873375339033,28.1723188950766,54.0610754336977));
#90732=CARTESIAN_POINT('Ctrl Pts',(4.75259533099376,28.2049005397224,53.9976530263781));
#90733=CARTESIAN_POINT('Ctrl Pts',(4.7564569085972,28.2407580932333,53.9359852760448));
#90734=CARTESIAN_POINT('Ctrl Pts',(4.76031848620064,28.2796626801179,53.8764177518664));
#90735=CARTESIAN_POINT('Ctrl Pts',(4.76418682031551,28.3186353374425,53.816746003793));
#90736=CARTESIAN_POINT('Ctrl Pts',(4.76805515443038,28.3606653857271,53.7591822110122));
#90737=CARTESIAN_POINT('Ctrl Pts',(4.77192348854526,28.4054824916269,53.7040403254763));
#90738=CARTESIAN_POINT('Ctrl Pts',(4.77422120771619,28.4321030265532,53.6712870617315));
#90739=CARTESIAN_POINT('Ctrl Pts',(4.77651892688712,28.4597061291633,53.6393876151707));
#90740=CARTESIAN_POINT('Ctrl Pts',(4.77881664605806,28.4882291828091,53.6084014376301));
#90741=CARTESIAN_POINT('Ctrl Pts',(4.78268571940627,28.5362584581298,53.5562245679752));
#90742=CARTESIAN_POINT('Ctrl Pts',(4.78655479275449,28.5870862098638,53.5064349216959));
#90743=CARTESIAN_POINT('Ctrl Pts',(4.79042386610271,28.6404457659141,53.4593475904412));
#90744=CARTESIAN_POINT('Ctrl Pts',(4.79428717449849,28.6937258157687,53.4123304197136));
#90745=CARTESIAN_POINT('Ctrl Pts',(4.79815048289427,28.7495298205365,53.3680078903842));
#90746=CARTESIAN_POINT('Ctrl Pts',(4.80201379129005,28.8075529541779,53.3266597460737));
#90747=CARTESIAN_POINT('Ctrl Pts',(4.80587256778296,28.8655080230471,53.2853601057278));
#90748=CARTESIAN_POINT('Ctrl Pts',(4.80973134427587,28.9256766563068,53.2470282003395));
#90749=CARTESIAN_POINT('Ctrl Pts',(4.81359012076878,28.9877208506948,53.2119036697141));
#90750=CARTESIAN_POINT('Ctrl Pts',(4.81744646635699,29.0497259592418,53.1768012664098));
#90751=CARTESIAN_POINT('Ctrl Pts',(4.82130281194519,29.1136038630109,53.1449024679027));
#90752=CARTESIAN_POINT('Ctrl Pts',(4.8251591575334,29.1789887057697,53.1164029047468));
#90753=CARTESIAN_POINT('Ctrl Pts',(4.82901436377873,29.2443542308214,53.0879117616802));
#90754=CARTESIAN_POINT('Ctrl Pts',(4.83286957002406,29.3112253658996,53.062818054167));
#90755=CARTESIAN_POINT('Ctrl Pts',(4.83672477626939,29.379214416526,53.0412700998221));
#90756=CARTESIAN_POINT('Ctrl Pts',(4.84058013312063,29.4472061231849,53.0197213036937));
#90757=CARTESIAN_POINT('Ctrl Pts',(4.84443548997187,29.5163153683469,53.0017186804078));
#90758=CARTESIAN_POINT('Ctrl Pts',(4.84829084682311,29.5861390257607,52.9873607733869));
#90759=CARTESIAN_POINT('Ctrl Pts',(4.85215023929167,29.6560357714959,52.972987837143));
#90760=CARTESIAN_POINT('Ctrl Pts',(4.85600963176022,29.726647945485,52.9622673310629));
#90761=CARTESIAN_POINT('Ctrl Pts',(4.85986902422878,29.7975628353229,52.9552465290756));
#90762=CARTESIAN_POINT('Ctrl Pts',(4.86373060183221,29.868517876195,52.9482217520069));
#90763=CARTESIAN_POINT('Ctrl Pts',(4.86759217943564,29.9397754886184,52.944900871601));
#90764=CARTESIAN_POINT('Ctrl Pts',(4.87145375703907,30.0109212110354,52.9452790238941));
#90765=CARTESIAN_POINT('Ctrl Pts',(4.87532209115394,30.0821914154484,52.9456578378314));
#90766=CARTESIAN_POINT('Ctrl Pts',(4.87919042526881,30.1533488538527,52.9497485783339));
#90767=CARTESIAN_POINT('Ctrl Pts',(4.88305875938368,30.2239831424404,52.9574944028467));
#90768=CARTESIAN_POINT('Ctrl Pts',(4.88535647855466,30.2659386080742,52.962095279852));
#90769=CARTESIAN_POINT('Ctrl Pts',(4.88765419772564,30.307709654124,52.9679847345438));
#90770=CARTESIAN_POINT('Ctrl Pts',(4.88995191689661,30.3492123714913,52.9751424044893));
#90771=CARTESIAN_POINT('Ctrl Pts',(4.89382099024483,30.4190977864161,52.9871950305765));
#90772=CARTESIAN_POINT('Ctrl Pts',(4.89769006359304,30.4884953840999,53.0028935228187));
#90773=CARTESIAN_POINT('Ctrl Pts',(4.90155913694125,30.5569958089551,53.0221847327654));
#90774=CARTESIAN_POINT('Ctrl Pts',(4.90542244533704,30.6253941675906,53.041447198644));
#90775=CARTESIAN_POINT('Ctrl Pts',(4.90928575373283,30.6928975431113,53.0642916257024));
#90776=CARTESIAN_POINT('Ctrl Pts',(4.91314906212862,30.7591055840198,53.0906136391998));
#90777=CARTESIAN_POINT('Ctrl Pts',(4.91700783862153,30.8252359587469,53.1169047753256));
#90778=CARTESIAN_POINT('Ctrl Pts',(4.92086661511444,30.8900735678922,53.1466652161715));
#90779=CARTESIAN_POINT('Ctrl Pts',(4.92472539160735,30.953233758787,53.1797409624977));
#90780=CARTESIAN_POINT('Ctrl Pts',(4.92858173719555,31.0163541607992,53.2127958721708));
#90781=CARTESIAN_POINT('Ctrl Pts',(4.93243808278376,31.0777988117451,53.2491617188719));
#90782=CARTESIAN_POINT('Ctrl Pts',(4.93629442837197,31.1372049265938,53.2886372338306));
#90783=CARTESIAN_POINT('Ctrl Pts',(4.94014963461732,31.1965934901283,53.3281010858963));
#90784=CARTESIAN_POINT('Ctrl Pts',(4.94400484086266,31.2539443088724,53.3706725135541));
#90785=CARTESIAN_POINT('Ctrl Pts',(4.947860047108,31.3089225031761,53.416106239933));
#90786=CARTESIAN_POINT('Ctrl Pts',(4.95171540395928,31.3639028452357,53.4615417412075));
#90787=CARTESIAN_POINT('Ctrl Pts',(4.95557076081055,31.4165100057726,53.5098394520472));
#90788=CARTESIAN_POINT('Ctrl Pts',(4.95942611766182,31.4664425529645,53.5607141349422));
#90789=CARTESIAN_POINT('Ctrl Pts',(4.96328551013038,31.5164273673416,53.6116420712085));
#90790=CARTESIAN_POINT('Ctrl Pts',(4.96714490259894,31.5637316386344,53.6651520168592));
#90791=CARTESIAN_POINT('Ctrl Pts',(4.9710042950675,31.6080918095699,53.7209228739071));
#90792=CARTESIAN_POINT('Ctrl Pts',(4.97486587267093,31.6524770966234,53.7767253076463));
#90793=CARTESIAN_POINT('Ctrl Pts',(4.97872745027436,31.693914682697,53.8347908054513));
#90794=CARTESIAN_POINT('Ctrl Pts',(4.9825890278778,31.7321838651551,53.894768522075));
#90795=CARTESIAN_POINT('Ctrl Pts',(4.98645736199267,31.770520006301,53.9548511802977));
#90796=CARTESIAN_POINT('Ctrl Pts',(4.99032569610754,31.8056764360204,54.0168523145415));
#90797=CARTESIAN_POINT('Ctrl Pts',(4.99419403022242,31.8374783327811,54.0803963141331));
#90798=CARTESIAN_POINT('Ctrl Pts',(4.99649174939334,31.8563680733487,54.118140278776));
#90799=CARTESIAN_POINT('Ctrl Pts',(4.99878946856425,31.8740752011145,54.1564281827517));
#90800=CARTESIAN_POINT('Ctrl Pts',(5.00108718773517,31.8905713141638,54.1951784865195));
#90801=CARTESIAN_POINT('Ctrl Pts',(5.00537446195649,31.9213511244745,54.2674820040749));
#90802=CARTESIAN_POINT('Ctrl Pts',(5.00966173617781,31.9480150746282,54.3416372137357));
#90803=CARTESIAN_POINT('Ctrl Pts',(5.01394901039913,31.9703612656978,54.4171843815255));
#90804=CARTESIAN_POINT('Ctrl Pts',(5.01822262075583,31.9926362377798,54.4924907748231));
#90805=CARTESIAN_POINT('Ctrl Pts',(5.02249623111252,32.0106207692059,54.5691800046967));
#90806=CARTESIAN_POINT('Ctrl Pts',(5.02676984146922,32.024161307071,54.6467740589132));
#90807=CARTESIAN_POINT('Ctrl Pts',(5.03102083155032,32.0376301746917,54.7239574067843));
#90808=CARTESIAN_POINT('Ctrl Pts',(5.03527182163142,32.0467018415724,54.8020357440816));
#90809=CARTESIAN_POINT('Ctrl Pts',(5.03952281171252,32.0512732988444,54.8805202278706));
#90810=CARTESIAN_POINT('Ctrl Pts',(5.04165696797233,32.0535683416385,54.9199223787064));
#90811=CARTESIAN_POINT('Ctrl Pts',(5.04379112423215,32.0547299142487,54.9594266319029));
#90812=CARTESIAN_POINT('Ctrl Pts',(5.04592528049197,32.0547497417017,54.9989697199742));
#90813=CARTESIAN_POINT('Origin',(-1.54592528053767,30.,55.));
#90814=CARTESIAN_POINT('',(3.89394682837563,28.7479524050421,56.6292250864936));
#90815=CARTESIAN_POINT('',(3.95204618956481,28.7479524050421,56.6292250864936));
#90816=CARTESIAN_POINT('',(-1.54592528053767,28.7479524050421,56.6292250864936));
#90817=CARTESIAN_POINT('',(4.40407471951261,32.0547494817011,55.0014594345582));
#90818=CARTESIAN_POINT('Ctrl Pts',(3.95204618956481,28.7479524050421,56.6292250864936));
#90819=CARTESIAN_POINT('Ctrl Pts',(3.95593362166089,28.6909406676674,56.5854119821803));
#90820=CARTESIAN_POINT('Ctrl Pts',(3.95982105375698,28.6362494734195,56.5386166933452));
#90821=CARTESIAN_POINT('Ctrl Pts',(3.96370848585306,28.5841940618756,56.4891242755632));
#90822=CARTESIAN_POINT('Ctrl Pts',(3.96756899650448,28.5324991471446,56.4399746052181));
#90823=CARTESIAN_POINT('Ctrl Pts',(3.9714295071559,28.4834039172625,56.3881654430581));
#90824=CARTESIAN_POINT('Ctrl Pts',(3.97529001780731,28.4371786472169,56.3340116123127));
#90825=CARTESIAN_POINT('Ctrl Pts',(3.97919091062573,28.3904698461716,56.2792913153057));
#90826=CARTESIAN_POINT('Ctrl Pts',(3.98309180344414,28.3466917103696,56.2221774112299));
#90827=CARTESIAN_POINT('Ctrl Pts',(3.98699269626255,28.3060787348042,56.1630254983523));
#90828=CARTESIAN_POINT('Ctrl Pts',(3.99089358908096,28.2654657592389,56.1038735854746));
#90829=CARTESIAN_POINT('Ctrl Pts',(3.99479448189937,28.2280181518745,56.0426841281137));
#90830=CARTESIAN_POINT('Ctrl Pts',(3.99869537471779,28.1939221902578,55.9798369801436));
#90831=CARTESIAN_POINT('Ctrl Pts',(4.002564448066,28.1601043484166,55.9175024745467));
#90832=CARTESIAN_POINT('Ctrl Pts',(4.00643352141422,28.12945115043,55.8532930462971));
#90833=CARTESIAN_POINT('Ctrl Pts',(4.01030259476243,28.1021743860266,55.7875630142703));
#90834=CARTESIAN_POINT('Ctrl Pts',(4.01416590315822,28.0749382642358,55.7219309205542));
#90835=CARTESIAN_POINT('Ctrl Pts',(4.01802921155401,28.0510687744827,55.6547831654671));
#90836=CARTESIAN_POINT('Ctrl Pts',(4.02189251994979,28.0307319100996,55.5864987234428));
#90837=CARTESIAN_POINT('Ctrl Pts',(4.02575129644271,28.010418902133,55.5182943833486));
#90838=CARTESIAN_POINT('Ctrl Pts',(4.02961007293562,27.9936304261562,55.448956468227));
#90839=CARTESIAN_POINT('Ctrl Pts',(4.03346884942853,27.9804837906095,55.3788823597224));
#90840=CARTESIAN_POINT('Ctrl Pts',(4.03732519501674,27.967345437019,55.3088523956456));
#90841=CARTESIAN_POINT('Ctrl Pts',(4.04118154060495,27.9578444614835,55.2380876346411));
#90842=CARTESIAN_POINT('Ctrl Pts',(4.04503788619316,27.9520475161225,55.1669975636947));
#90843=CARTESIAN_POINT('Ctrl Pts',(4.0488930924385,27.9462522834473,55.0959284960438));
#90844=CARTESIAN_POINT('Ctrl Pts',(4.05274829868383,27.9441589478354,55.0245347931742));
#90845=CARTESIAN_POINT('Ctrl Pts',(4.05660350492917,27.9457823265314,54.9532312870671));
#90846=CARTESIAN_POINT('Ctrl Pts',(4.06045886178042,27.9474057686458,54.8819249954463));
#90847=CARTESIAN_POINT('Ctrl Pts',(4.06431421863168,27.9527462000759,54.8107093931937));
#90848=CARTESIAN_POINT('Ctrl Pts',(4.06816957548293,27.9617663485298,54.7399977990202));
#90849=CARTESIAN_POINT('Ctrl Pts',(4.07202896795149,27.9707959388767,54.6692121870724));
#90850=CARTESIAN_POINT('Ctrl Pts',(4.07588836042004,27.9835128736404,54.5989321192273));
#90851=CARTESIAN_POINT('Ctrl Pts',(4.0797477528886,27.9998282686893,54.529563386028));
#90852=CARTESIAN_POINT('Ctrl Pts',(4.08360933049203,28.0161529012901,54.4601553772072));
#90853=CARTESIAN_POINT('Ctrl Pts',(4.08747090809547,28.0360799142424,54.3916601968676));
#90854=CARTESIAN_POINT('Ctrl Pts',(4.0913324856989,28.0594705271053,54.3244684113035));
#90855=CARTESIAN_POINT('Ctrl Pts',(4.09520081981377,28.0829020659729,54.2571590618537));
#90856=CARTESIAN_POINT('Ctrl Pts',(4.09906915392864,28.1098091206272,54.1911581102851));
#90857=CARTESIAN_POINT('Ctrl Pts',(4.10293748804351,28.1400050514512,54.1268354371181));
#90858=CARTESIAN_POINT('Ctrl Pts',(4.10523520721446,28.1579408778505,54.0886289547219));
#90859=CARTESIAN_POINT('Ctrl Pts',(4.1075329263854,28.1770361820226,54.0510141262206));
#90860=CARTESIAN_POINT('Ctrl Pts',(4.10983064555635,28.1972445332813,54.0140637496694));
#90861=CARTESIAN_POINT('Ctrl Pts',(4.11369971890457,28.2312728837671,53.9518439105661));
#90862=CARTESIAN_POINT('Ctrl Pts',(4.11756879225278,28.2685928276122,53.8912659359023));
#90863=CARTESIAN_POINT('Ctrl Pts',(4.121437865601,28.3090215532379,53.8326999292872));
#90864=CARTESIAN_POINT('Ctrl Pts',(4.12530117399678,28.3493900397161,53.7742211865238));
#90865=CARTESIAN_POINT('Ctrl Pts',(4.12916448239255,28.3928578396379,53.7177488576873));
#90866=CARTESIAN_POINT('Ctrl Pts',(4.13302779078832,28.4391965888961,53.6636279431287));
#90867=CARTESIAN_POINT('Ctrl Pts',(4.13688656728124,28.4854809798974,53.6095705157946));
#90868=CARTESIAN_POINT('Ctrl Pts',(4.14074534377415,28.5346293162252,53.5578593909253));
#90869=CARTESIAN_POINT('Ctrl Pts',(4.14460412026706,28.5863713641356,53.5088086499834));
#90870=CARTESIAN_POINT('Ctrl Pts',(4.14846046585527,28.6380808162251,53.459788809426));
#90871=CARTESIAN_POINT('Ctrl Pts',(4.15231681144348,28.6923803864422,53.4134263611475));
#90872=CARTESIAN_POINT('Ctrl Pts',(4.15617315703168,28.7489621966495,53.3699993935314));
#90873=CARTESIAN_POINT('Ctrl Pts',(4.16002836327702,28.8055272899728,53.3265852562503));
#90874=CARTESIAN_POINT('Ctrl Pts',(4.16388356952235,28.8643728994989,53.2861051734575));
#90875=CARTESIAN_POINT('Ctrl Pts',(4.16773877576769,28.9251585431525,53.2487965837339));
#90876=CARTESIAN_POINT('Ctrl Pts',(4.17159413261893,28.9859465614332,53.2114865365282));
#90877=CARTESIAN_POINT('Ctrl Pts',(4.17544948947017,29.0486743491362,53.1773484806093));
#90878=CARTESIAN_POINT('Ctrl Pts',(4.17930484632141,29.1129744440563,53.1465752711257));
#90879=CARTESIAN_POINT('Ctrl Pts',(4.18316423878997,29.1773418454766,53.1157698496052));
#90880=CARTESIAN_POINT('Ctrl Pts',(4.18702363125853,29.2432844004578,53.0883365157092));
#90881=CARTESIAN_POINT('Ctrl Pts',(4.19088302372709,29.3104129791282,53.0644206802238));
#90882=CARTESIAN_POINT('Ctrl Pts',(4.19474460133053,29.3775795650757,53.0404913039216));
#90883=CARTESIAN_POINT('Ctrl Pts',(4.19860617893397,29.4459330457793,53.0200835296513));
#90884=CARTESIAN_POINT('Ctrl Pts',(4.20246775653741,29.5150700199561,53.0032925910503));
#90885=CARTESIAN_POINT('Ctrl Pts',(4.20633609065228,29.5843279614691,52.9864722737393));
#90886=CARTESIAN_POINT('Ctrl Pts',(4.21020442476715,29.6543716558712,52.973281516649));
#90887=CARTESIAN_POINT('Ctrl Pts',(4.21407275888202,29.724789123801,52.9637641256176));
#90888=CARTESIAN_POINT('Ctrl Pts',(4.21637047805298,29.7666158019596,52.9581109707502));
#90889=CARTESIAN_POINT('Ctrl Pts',(4.21866819722395,29.8085742650115,52.9537528354883));
#90890=CARTESIAN_POINT('Ctrl Pts',(4.22096591639491,29.8505781698028,52.9506901944409));
#90891=CARTESIAN_POINT('Ctrl Pts',(4.22483498974313,29.9213075220241,52.9455330877756));
#90892=CARTESIAN_POINT('Ctrl Pts',(4.22870406309134,29.9924427144347,52.9440318803733));
#90893=CARTESIAN_POINT('Ctrl Pts',(4.23257313643955,30.0635736564367,52.9462337151693));
#90894=CARTESIAN_POINT('Ctrl Pts',(4.23643644483534,30.1345986127257,52.9484322692126));
#90895=CARTESIAN_POINT('Ctrl Pts',(4.24029975323112,30.2056188495799,52.9543228983359));
#90896=CARTESIAN_POINT('Ctrl Pts',(4.2441630616269,30.2762206606864,52.963900859705));
#90897=CARTESIAN_POINT('Ctrl Pts',(4.24802183811981,30.3467396514436,52.9734675855252));
#90898=CARTESIAN_POINT('Ctrl Pts',(4.25188061461272,30.4168407123865,52.9867129867538));
#90899=CARTESIAN_POINT('Ctrl Pts',(4.25573939110564,30.4861134049202,53.0035803747566));
#90900=CARTESIAN_POINT('Ctrl Pts',(4.25959573669384,30.5553424578924,53.0204371368492));
#90901=CARTESIAN_POINT('Ctrl Pts',(4.26345208228205,30.6237437069085,53.0409112441355));
#90902=CARTESIAN_POINT('Ctrl Pts',(4.26730842787026,30.6909165357602,53.0648948599332));
#90903=CARTESIAN_POINT('Ctrl Pts',(4.27116363411559,30.7580695186511,53.0888713898613));
#90904=CARTESIAN_POINT('Ctrl Pts',(4.27501884036093,30.8239943446481,53.1163552065664));
#90905=CARTESIAN_POINT('Ctrl Pts',(4.27887404660627,30.8883068660076,53.1471890343849));
#90906=CARTESIAN_POINT('Ctrl Pts',(4.28272940345752,30.9526218997738,53.178024066745));
#90907=CARTESIAN_POINT('Ctrl Pts',(4.28658476030876,31.0153240667616,53.2122091580435));
#90908=CARTESIAN_POINT('Ctrl Pts',(4.29044011716001,31.0760520426574,53.249540184982));
#90909=CARTESIAN_POINT('Ctrl Pts',(4.29429950962857,31.1368435859168,53.286910288391));
#90910=CARTESIAN_POINT('Ctrl Pts',(4.29815890209713,31.1956563982002,53.3274326461382));
#90911=CARTESIAN_POINT('Ctrl Pts',(4.30201829456569,31.2521572635057,53.3708591988567));
#90912=CARTESIAN_POINT('Ctrl Pts',(4.30587987216913,31.3086901188233,53.4143103390915));
#90913=CARTESIAN_POINT('Ctrl Pts',(4.30974144977257,31.3629080519673,53.4606686317754));
#90914=CARTESIAN_POINT('Ctrl Pts',(4.31360302737602,31.4145122626426,53.5096468132239));
#90915=CARTESIAN_POINT('Ctrl Pts',(4.31747136149089,31.4662067639906,53.5587106906435));
#90916=CARTESIAN_POINT('Ctrl Pts',(4.32133969560576,31.5152780778462,53.6104032564012));
#90917=CARTESIAN_POINT('Ctrl Pts',(4.32520802972063,31.5614659582069,53.6644021474033));
#90918=CARTESIAN_POINT('Ctrl Pts',(4.32750574889158,31.5889007078999,53.6964764934606));
#90919=CARTESIAN_POINT('Ctrl Pts',(4.32980346806252,31.6153189306063,53.729363929871));
#90920=CARTESIAN_POINT('Ctrl Pts',(4.33210118723347,31.6406733981608,53.7629921734008));
#90921=CARTESIAN_POINT('Ctrl Pts',(4.33598223894954,31.6834993453246,53.8197932628943));
#90922=CARTESIAN_POINT('Ctrl Pts',(4.3398632906656,31.723457290319,53.8789338902988));
#90923=CARTESIAN_POINT('Ctrl Pts',(4.34374434238167,31.7602831217971,53.9400939222665));
#90924=CARTESIAN_POINT('Ctrl Pts',(4.34761960540842,31.7970540265922,54.0011627324601));
#90925=CARTESIAN_POINT('Ctrl Pts',(4.35149486843518,31.8307018422724,54.0642445616435));
#90926=CARTESIAN_POINT('Ctrl Pts',(4.35537013146193,31.8610038890175,54.1289878947099));
#90927=CARTESIAN_POINT('Ctrl Pts',(4.35942884712863,31.8927404165791,54.1967961385419));
#90928=CARTESIAN_POINT('Ctrl Pts',(4.36348756279533,31.920806196447,54.2664266821933));
#90929=CARTESIAN_POINT('Ctrl Pts',(4.36754627846203,31.9449979565058,54.3374439558133));
#90930=CARTESIAN_POINT('Ctrl Pts',(4.37141366678506,31.9680493200522,54.4051134841285));
#90931=CARTESIAN_POINT('Ctrl Pts',(4.37528105510808,31.9875834868991,54.4740414408063));
#90932=CARTESIAN_POINT('Ctrl Pts',(4.3791484434311,32.0034736409941,54.543830149679));
#90933=CARTESIAN_POINT('Ctrl Pts',(4.38301406018565,32.0193565161468,54.6135868898258));
#90934=CARTESIAN_POINT('Ctrl Pts',(4.38687967694019,32.0315985897945,54.6842031295411));
#90935=CARTESIAN_POINT('Ctrl Pts',(4.39074529369473,32.040123513712,54.7552682870991));
#90936=CARTESIAN_POINT('Ctrl Pts',(4.39461092103566,32.0486484609759,54.8263336392762));
#90937=CARTESIAN_POINT('Ctrl Pts',(4.39847654837658,32.0534561785917,54.8978474341116));
#90938=CARTESIAN_POINT('Ctrl Pts',(4.40234217571751,32.0545220261428,54.9693927035783));
#90939=CARTESIAN_POINT('Ctrl Pts',(4.40291969029912,32.0546812609702,54.980081379107));
#90940=CARTESIAN_POINT('Ctrl Pts',(4.40349720488072,32.0547570735857,54.9907707532352));
#90941=CARTESIAN_POINT('Ctrl Pts',(4.40407471946233,32.0547494817017,55.0014594336275));
#90942=CARTESIAN_POINT('Ctrl Pts',(4.40407471951261,32.0547494817011,55.0014594345582));
#90943=CARTESIAN_POINT('Ctrl Pts',(4.40849095806831,32.0546914267306,55.0831954875701));
#90944=CARTESIAN_POINT('Ctrl Pts',(4.41290719662402,32.0497522762913,55.1647368982365));
#90945=CARTESIAN_POINT('Ctrl Pts',(4.41732343517972,32.0400254037017,55.2455481923201));
#90946=CARTESIAN_POINT('Ctrl Pts',(4.4217797159885,32.030210337078,55.327092206398));
#90947=CARTESIAN_POINT('Ctrl Pts',(4.42623599679728,32.0155204432684,55.4078926142023));
#90948=CARTESIAN_POINT('Ctrl Pts',(4.43069227760607,31.9961013728872,55.4874185795163));
#90949=CARTESIAN_POINT('Ctrl Pts',(4.43487367109472,31.9778801750024,55.5620389564206));
#90950=CARTESIAN_POINT('Ctrl Pts',(4.43905506458338,31.9554957935063,55.6355373428861));
#90951=CARTESIAN_POINT('Ctrl Pts',(4.44323645807203,31.9291064843791,55.7074925684604));
#90952=CARTESIAN_POINT('Ctrl Pts',(4.44710553142025,31.9046882676053,55.7740732541313));
#90953=CARTESIAN_POINT('Ctrl Pts',(4.45097460476847,31.8767712524526,55.8395187237066));
#90954=CARTESIAN_POINT('Ctrl Pts',(4.45484367811669,31.8454813033535,55.9034358424772));
#90955=CARTESIAN_POINT('Ctrl Pts',(4.45870698651247,31.8142379765466,55.9672577241934));
#90956=CARTESIAN_POINT('Ctrl Pts',(4.46257029490826,31.7796319035185,56.029555342638));
#90957=CARTESIAN_POINT('Ctrl Pts',(4.46643360330405,31.7418377221506,56.08995362846));
#90958=CARTESIAN_POINT('Ctrl Pts',(4.47029237979696,31.7040878757261,56.1502810633074));
#90959=CARTESIAN_POINT('Ctrl Pts',(4.47415115628987,31.6631576060078,56.2087131813575));
#90960=CARTESIAN_POINT('Ctrl Pts',(4.47800993278278,31.6192675452452,56.2648992763914));
#90961=CARTESIAN_POINT('Ctrl Pts',(4.48186627837099,31.575405133805,56.3210499759981));
#90962=CARTESIAN_POINT('Ctrl Pts',(4.48572262395919,31.5285869289446,56.3749570778473));
#90963=CARTESIAN_POINT('Ctrl Pts',(4.4895789695474,31.4790761318269,56.4262998838813));
#90964=CARTESIAN_POINT('Ctrl Pts',(4.49343417579273,31.429579962489,56.4776275208754));
#90965=CARTESIAN_POINT('Ctrl Pts',(4.49728938203806,31.3773931172375,56.5263920166289));
#90966=CARTESIAN_POINT('Ctrl Pts',(4.5011445882834,31.3228170725557,56.5723080344052));
#90967=CARTESIAN_POINT('Ctrl Pts',(4.50499994513464,31.2682388958285,56.6182258459179));
#90968=CARTESIAN_POINT('Ctrl Pts',(4.50885530198588,31.2112717075104,56.6612946474703));
#90969=CARTESIAN_POINT('Ctrl Pts',(4.51271065883712,31.152250281613,56.7012691882894));
#90970=CARTESIAN_POINT('Ctrl Pts',(4.51657005130568,31.0931670746931,56.7412855726927));
#90971=CARTESIAN_POINT('Ctrl Pts',(4.52042944377424,31.0320257407813,56.7782009577452));
#90972=CARTESIAN_POINT('Ctrl Pts',(4.52428883624279,30.9691895223348,56.811813796254));
#90973=CARTESIAN_POINT('Ctrl Pts',(4.52815041384623,30.9063177268866,56.8454456658892));
#90974=CARTESIAN_POINT('Ctrl Pts',(4.53201199144966,30.8417495765086,56.8757710600617));
#90975=CARTESIAN_POINT('Ctrl Pts',(4.5358735690531,30.7758698732853,56.9026359352825));
#90976=CARTESIAN_POINT('Ctrl Pts',(4.53974190316797,30.7098749018961,56.929547815343));
#90977=CARTESIAN_POINT('Ctrl Pts',(4.54361023728284,30.6425642549529,56.9529869280869));
#90978=CARTESIAN_POINT('Ctrl Pts',(4.54747857139771,30.5743388494694,56.9728488154165));
#90979=CARTESIAN_POINT('Ctrl Pts',(4.54977629056867,30.5338142160043,56.9846464104362));
#90980=CARTESIAN_POINT('Ctrl Pts',(4.55207400973963,30.4929670773006,56.995182881589));
#90981=CARTESIAN_POINT('Ctrl Pts',(4.55437172891059,30.4518827500531,57.0044449462892));
#90982=CARTESIAN_POINT('Ctrl Pts',(4.55844030376033,30.3791346689688,57.0208452984178));
#90983=CARTESIAN_POINT('Ctrl Pts',(4.56250887861007,30.3053427076324,57.0333138865847));
#90984=CARTESIAN_POINT('Ctrl Pts',(4.56657745345982,30.2309707793399,57.0417272250698));
#90985=CARTESIAN_POINT('Ctrl Pts',(4.57043978118483,30.1603689663671,57.0497140685447));
#90986=CARTESIAN_POINT('Ctrl Pts',(4.57430210890985,30.0892451145857,57.0540466922945));
#90987=CARTESIAN_POINT('Ctrl Pts',(4.57816443663487,30.01800922301,57.05467107596));
#90988=CARTESIAN_POINT('Ctrl Pts',(4.58202297547393,29.9468432127825,57.0552948471144));
#90989=CARTESIAN_POINT('Ctrl Pts',(4.585881514313,29.8755658640219,57.052217591045));
#90990=CARTESIAN_POINT('Ctrl Pts',(4.58974005315206,29.8045915154746,57.045437138285));
#90991=CARTESIAN_POINT('Ctrl Pts',(4.59359609769486,29.7336630472617,57.0386610686499));
#90992=CARTESIAN_POINT('Ctrl Pts',(4.59745214223766,29.6630376728841,57.0281866000545));
#90993=CARTESIAN_POINT('Ctrl Pts',(4.60130818678046,29.5931272137334,57.0140635785137));
#90994=CARTESIAN_POINT('Ctrl Pts',(4.60516302857667,29.5232385604942,56.999944962113));
#90995=CARTESIAN_POINT('Ctrl Pts',(4.60901787037287,29.4540648551168,56.9821801503313));
#90996=CARTESIAN_POINT('Ctrl Pts',(4.61287271216908,29.3860085838065,56.9608702413318));
#90997=CARTESIAN_POINT('Ctrl Pts',(4.61672933980179,29.3179207839976,56.9395504600689));
#90998=CARTESIAN_POINT('Ctrl Pts',(4.62058596743451,29.2509519173612,56.9146824432169));
#90999=CARTESIAN_POINT('Ctrl Pts',(4.62444259506723,29.1854889899216,56.8864170739688));
#91000=CARTESIAN_POINT('Ctrl Pts',(4.62830025698201,29.1200085064361,56.8581441244286));
#91001=CARTESIAN_POINT('Ctrl Pts',(4.63215791889679,29.0560352053134,56.8264722170175));
#91002=CARTESIAN_POINT('Ctrl Pts',(4.63601558081158,28.9939336051439,56.7915992776403));
#91003=CARTESIAN_POINT('Ctrl Pts',(4.63987770210721,28.9317602167531,56.7566860258351));
#91004=CARTESIAN_POINT('Ctrl Pts',(4.64373982340285,28.8714632614709,56.718564611389));
#91005=CARTESIAN_POINT('Ctrl Pts',(4.64760194469848,28.813379370413,56.6774769876033));
#91006=CARTESIAN_POINT('Ctrl Pts',(4.64907380490046,28.7912435126604,56.6618184327277));
#91007=CARTESIAN_POINT('Ctrl Pts',(4.65054566510243,28.7694287440933,56.6457294964002));
#91008=CARTESIAN_POINT('Ctrl Pts',(4.6520175253044,28.7479524050421,56.6292250864936));
#91009=CARTESIAN_POINT('',(4.34592528058805,32.054749644159,54.9987907322124));
#91010=CARTESIAN_POINT('Ctrl Pts',(4.34592528058805,32.054749644159,54.9987907322123));
#91011=CARTESIAN_POINT('Ctrl Pts',(4.34974237135586,32.0547908859483,55.0688674784532));
#91012=CARTESIAN_POINT('Ctrl Pts',(4.35355946212367,32.0512429716119,55.1390874484566));
#91013=CARTESIAN_POINT('Ctrl Pts',(4.35737655289148,32.0440883161928,55.2090466888139));
#91014=CARTESIAN_POINT('Ctrl Pts',(4.36118805254388,32.0369441406146,55.2789034557928));
#91015=CARTESIAN_POINT('Ctrl Pts',(4.36499955219628,32.0262037618752,55.3484997581352));
#91016=CARTESIAN_POINT('Ctrl Pts',(4.36881105184869,32.0119016127208,55.4174319863538));
#91017=CARTESIAN_POINT('Ctrl Pts',(4.37261948474162,31.9976109711765,55.4863087512158));
#91018=CARTESIAN_POINT('Ctrl Pts',(4.37642791763454,31.9797643402277,55.554522013904));
#91019=CARTESIAN_POINT('Ctrl Pts',(4.38023635052747,31.958447737978,55.6216751725047));
#91020=CARTESIAN_POINT('Ctrl Pts',(4.38404307118795,31.9371407194545,55.6887981397326));
#91021=CARTESIAN_POINT('Ctrl Pts',(4.38784979184843,31.9123669743003,55.754861472588));
#91022=CARTESIAN_POINT('Ctrl Pts',(4.39165651250891,31.8842627237978,55.8194824892614));
#91023=CARTESIAN_POINT('Ctrl Pts',(4.39546287300827,31.8561611322921,55.884097392017));
#91024=CARTESIAN_POINT('Ctrl Pts',(4.39926923350764,31.82472986167,55.9472697921498));
#91025=CARTESIAN_POINT('Ctrl Pts',(4.403075594007,31.7901530068413,56.0086375833753));
#91026=CARTESIAN_POINT('Ctrl Pts',(4.40688551322988,31.755543824684,56.0700627498813));
#91027=CARTESIAN_POINT('Ctrl Pts',(4.41069543245276,31.7177834317607,56.129679502477));
#91028=CARTESIAN_POINT('Ctrl Pts',(4.41450535167564,31.6771010428824,56.1871519087558));
#91029=CARTESIAN_POINT('Ctrl Pts',(4.41831711300166,31.6363989839922,56.2446521030517));
#91030=CARTESIAN_POINT('Ctrl Pts',(4.42212887432769,31.5927724276063,56.3000054956356));
#91031=CARTESIAN_POINT('Ctrl Pts',(4.42594063565372,31.546491159843,56.3529089603619));
#91032=CARTESIAN_POINT('Ctrl Pts',(4.42975910316213,31.5001284676157,56.405905500245));
#91033=CARTESIAN_POINT('Ctrl Pts',(4.43357757067055,31.4511020881627,56.4564431490457));
#91034=CARTESIAN_POINT('Ctrl Pts',(4.43739603817897,31.3997183644062,56.5042559831505));
#91035=CARTESIAN_POINT('Ctrl Pts',(4.44006763663344,31.3637676389724,56.5377083284741));
#91036=CARTESIAN_POINT('Ctrl Pts',(4.44273923508791,31.3266637077791,56.5698276548949));
#91037=CARTESIAN_POINT('Ctrl Pts',(4.44541083354238,31.288520118375,56.6005353688822));
#91038=CARTESIAN_POINT('Ctrl Pts',(4.44927990689059,31.2332796517841,56.6450070212647));
#91039=CARTESIAN_POINT('Ctrl Pts',(4.45314898023881,31.1756259560803,56.6867025917087));
#91040=CARTESIAN_POINT('Ctrl Pts',(4.45701805358702,31.1158695099185,56.7253500512459));
#91041=CARTESIAN_POINT('Ctrl Pts',(4.46088136198281,31.0562021013733,56.7639399257374));
#91042=CARTESIAN_POINT('Ctrl Pts',(4.46474467037861,30.9944385661033,56.7994904428259));
#91043=CARTESIAN_POINT('Ctrl Pts',(4.4686079787744,30.93092186864,56.8317701921878));
#91044=CARTESIAN_POINT('Ctrl Pts',(4.47246675526731,30.8674796802436,56.8640120753806));
#91045=CARTESIAN_POINT('Ctrl Pts',(4.47632553176022,30.8022888456627,56.892990593039));
#91046=CARTESIAN_POINT('Ctrl Pts',(4.48018430825314,30.7357191879358,56.9185189180728));
#91047=CARTESIAN_POINT('Ctrl Pts',(4.48404065384134,30.6691914669457,56.9440311610853));
#91048=CARTESIAN_POINT('Ctrl Pts',(4.48789699942955,30.6012870986316,56.9660973501538));
#91049=CARTESIAN_POINT('Ctrl Pts',(4.49175334501776,30.5323969196768,56.984578313501));
#91050=CARTESIAN_POINT('Ctrl Pts',(4.49560855126309,30.4635270940676,57.0030538167168));
#91051=CARTESIAN_POINT('Ctrl Pts',(4.49946375750842,30.3936725049778,57.0179460712978));
#91052=CARTESIAN_POINT('Ctrl Pts',(4.50331896375375,30.3232385643448,57.0291659353095));
#91053=CARTESIAN_POINT('Ctrl Pts',(4.50717432060499,30.2528018721683,57.0403862376318));
#91054=CARTESIAN_POINT('Ctrl Pts',(4.51102967745623,30.1817862635981,57.0479337903105));
#91055=CARTESIAN_POINT('Ctrl Pts',(4.51488503430747,30.1106050250406,57.0517709645415));
#91056=CARTESIAN_POINT('Ctrl Pts',(4.51874442677603,30.0393492771056,57.0556121553571));
#91057=CARTESIAN_POINT('Ctrl Pts',(4.52260381924459,29.9679280391652,57.0557351884641));
#91058=CARTESIAN_POINT('Ctrl Pts',(4.52646321171315,29.8967564692996,57.0521545594493));
#91059=CARTESIAN_POINT('Ctrl Pts',(4.53032478931658,29.8255446030712,57.0485719031317));
#91060=CARTESIAN_POINT('Ctrl Pts',(4.53418636692,29.7545831697904,57.0412814599578));
#91061=CARTESIAN_POINT('Ctrl Pts',(4.53804794452343,29.6842813201151,57.0303495456871));
#91062=CARTESIAN_POINT('Ctrl Pts',(4.5419162786383,29.6138564649481,57.0193985041033));
#91063=CARTESIAN_POINT('Ctrl Pts',(4.54578461275318,29.5440939731254,57.0047933703205));
#91064=CARTESIAN_POINT('Ctrl Pts',(4.54965294686805,29.4753912491385,56.9866512580268));
#91065=CARTESIAN_POINT('Ctrl Pts',(4.55195066603901,29.4345830972794,56.9758751776829));
#91066=CARTESIAN_POINT('Ctrl Pts',(4.55424838520997,29.3941485465822,56.9638521549952));
#91067=CARTESIAN_POINT('Ctrl Pts',(4.55654610438093,29.3541675553053,56.9506147789555));
#91068=CARTESIAN_POINT('Ctrl Pts',(4.56041440940474,29.2868579069515,56.9283291102439));
#91069=CARTESIAN_POINT('Ctrl Pts',(4.56428271442855,29.2205713103213,56.9025117402514));
#91070=CARTESIAN_POINT('Ctrl Pts',(4.56815101945236,29.1557044660339,56.8732759043518));
#91071=CARTESIAN_POINT('Ctrl Pts',(4.57201426849238,29.0909224045418,56.8440782805144));
#91072=CARTESIAN_POINT('Ctrl Pts',(4.57587751753241,29.0275568547142,56.8114712484247));
#91073=CARTESIAN_POINT('Ctrl Pts',(4.57974076657243,28.9659882323256,56.7756174212963));
#91074=CARTESIAN_POINT('Ctrl Pts',(4.58359955333986,28.9044907252013,56.7398050073796));
#91075=CARTESIAN_POINT('Ctrl Pts',(4.58745834010729,28.844786440948,56.7007534901179));
#91076=CARTESIAN_POINT('Ctrl Pts',(4.59131712687472,28.7872329280312,56.6586722375587));
#91077=CARTESIAN_POINT('Ctrl Pts',(4.59220268619875,28.7740248776604,56.6490149416736));
#91078=CARTESIAN_POINT('Ctrl Pts',(4.59308824552279,28.7609299953523,56.6391982699849));
#91079=CARTESIAN_POINT('Ctrl Pts',(4.59397380484682,28.7479524050421,56.6292250864936));
#91080=CARTESIAN_POINT('Ctrl Pts',(3.89394682837563,28.7479524050421,56.6292250864936));
#91081=CARTESIAN_POINT('Ctrl Pts',(3.89781364428523,28.6916779684571,56.5859785924591));
#91082=CARTESIAN_POINT('Ctrl Pts',(3.90168046019482,28.6375451445928,56.539734920853));
#91083=CARTESIAN_POINT('Ctrl Pts',(3.90554727610442,28.5858898030596,56.4907346891413));
#91084=CARTESIAN_POINT('Ctrl Pts',(3.90951904585791,28.5328324225418,56.4404044839347));
#91085=CARTESIAN_POINT('Ctrl Pts',(3.91349081561139,28.4823894318975,56.3871661480069));
#91086=CARTESIAN_POINT('Ctrl Pts',(3.91746258536488,28.434890663223,56.3313265288551));
#91087=CARTESIAN_POINT('Ctrl Pts',(3.92132025666669,28.3887564086816,56.2770910344343));
#91088=CARTESIAN_POINT('Ctrl Pts',(3.9251779279685,28.3453998344527,56.2204020964724));
#91089=CARTESIAN_POINT('Ctrl Pts',(3.9290355992703,28.3050860971334,56.16157841938));
#91090=CARTESIAN_POINT('Ctrl Pts',(3.93289134533374,28.2647924790902,56.1027840992732));
#91091=CARTESIAN_POINT('Ctrl Pts',(3.93674709139717,28.227538958787,56.04185755422));
#91092=CARTESIAN_POINT('Ctrl Pts',(3.9406028374606,28.1935488776755,55.979148561329));
#91093=CARTESIAN_POINT('Ctrl Pts',(3.94445794906157,28.1595643896271,55.9164498871939));
#91094=CARTESIAN_POINT('Ctrl Pts',(3.94831306066253,28.1288425052922,55.8519697749701));
#91095=CARTESIAN_POINT('Ctrl Pts',(3.9521681722635,28.1015610149185,55.786083317736));
#91096=CARTESIAN_POINT('Ctrl Pts',(3.95622663709055,28.0728404536037,55.7167214167221));
#91097=CARTESIAN_POINT('Ctrl Pts',(3.96028510191761,28.0479335052111,55.6458012472298));
#91098=CARTESIAN_POINT('Ctrl Pts',(3.96434356674466,28.0269894365152,55.5737829545024));
#91099=CARTESIAN_POINT('Ctrl Pts',(3.96820378534732,28.0070684350922,55.505282581784));
#91100=CARTESIAN_POINT('Ctrl Pts',(3.97206400394997,27.9907322761517,55.4357893650098));
#91101=CARTESIAN_POINT('Ctrl Pts',(3.97592422255263,27.9780571691284,55.3657112948582));
#91102=CARTESIAN_POINT('Ctrl Pts',(3.97978714071035,27.9653731980606,55.2955842172206));
#91103=CARTESIAN_POINT('Ctrl Pts',(3.98365005886806,27.9563554330937,55.2248719538347));
#91104=CARTESIAN_POINT('Ctrl Pts',(3.98751297702578,27.9510282251341,55.1539877537434));
#91105=CARTESIAN_POINT('Ctrl Pts',(3.99138215086262,27.9456923901982,55.0829887625039));
#91106=CARTESIAN_POINT('Ctrl Pts',(3.99525132469946,27.944059041005,55.0118177633292));
#91107=CARTESIAN_POINT('Ctrl Pts',(3.9991204985363,27.9461004820823,54.940887118177));
#91108=CARTESIAN_POINT('Ctrl Pts',(3.99970358242024,27.9464081269291,54.9301978811951));
#91109=CARTESIAN_POINT('Ctrl Pts',(4.00028666630419,27.9467991323694,54.9195140894891));
#91110=CARTESIAN_POINT('Ctrl Pts',(4.00086975018814,27.947273302386,54.9088371380301));
#91111=CARTESIAN_POINT('Ctrl Pts',(4.00473882353635,27.9504196739869,54.8379898560741));
#91112=CARTESIAN_POINT('Ctrl Pts',(4.00860789688457,27.9572443216408,54.7671668837603));
#91113=CARTESIAN_POINT('Ctrl Pts',(4.01247697023278,27.9677461262914,54.69678101099));
#91114=CARTESIAN_POINT('Ctrl Pts',(4.01634027862857,27.978232283163,54.6265000137731));
#91115=CARTESIAN_POINT('Ctrl Pts',(4.02020358702435,27.992384650276,54.5566552998758));
#91116=CARTESIAN_POINT('Ctrl Pts',(4.02406689542013,28.0101501558676,54.4876571847814));
#91117=CARTESIAN_POINT('Ctrl Pts',(4.02792567191305,28.0278948214076,54.4187400088003));
#91118=CARTESIAN_POINT('Ctrl Pts',(4.03178444840596,28.0492440859143,54.3506679271217));
#91119=CARTESIAN_POINT('Ctrl Pts',(4.03564322489887,28.0740936699586,54.2838419375538));
#91120=CARTESIAN_POINT('Ctrl Pts',(4.03949957048707,28.0989275995667,54.2170580462036));
#91121=CARTESIAN_POINT('Ctrl Pts',(4.04335591607528,28.1272573049385,54.1515191437892));
#91122=CARTESIAN_POINT('Ctrl Pts',(4.04721226166348,28.1589288574891,54.0876104939701));
#91123=CARTESIAN_POINT('Ctrl Pts',(4.05106746790881,28.190591052798,54.0237207257224));
#91124=CARTESIAN_POINT('Ctrl Pts',(4.05492267415414,28.2255929195596,53.9614606888882));
#91125=CARTESIAN_POINT('Ctrl Pts',(4.05877788039947,28.2637333542961,53.9011935122524));
#91126=CARTESIAN_POINT('Ctrl Pts',(4.06263323725072,28.3018752790113,53.8409239812437));
#91127=CARTESIAN_POINT('Ctrl Pts',(4.06648859410196,28.3431557534853,53.7826478743109));
#91128=CARTESIAN_POINT('Ctrl Pts',(4.07034395095321,28.3873298158101,53.7267001768927));
#91129=CARTESIAN_POINT('Ctrl Pts',(4.07420334342177,28.4315501175928,53.6706939158954));
#91130=CARTESIAN_POINT('Ctrl Pts',(4.07806273589032,28.4786697518997,53.6170213118141));
#91131=CARTESIAN_POINT('Ctrl Pts',(4.08192212835888,28.528403407789,53.5659842984497));
#91132=CARTESIAN_POINT('Ctrl Pts',(4.08578370596231,28.5781652221894,53.514918388631));
#91133=CARTESIAN_POINT('Ctrl Pts',(4.08964528356575,28.6305436475791,53.4664913700499));
#91134=CARTESIAN_POINT('Ctrl Pts',(4.09350686116918,28.685218460614,53.42096641385));
#91135=CARTESIAN_POINT('Ctrl Pts',(4.09737519528405,28.7399889368823,53.3753618037058));
#91136=CARTESIAN_POINT('Ctrl Pts',(4.10124352939892,28.7970634335964,53.3326696847263));
#91137=CARTESIAN_POINT('Ctrl Pts',(4.10511186351379,28.8560913755677,53.2931108350425));
#91138=CARTESIAN_POINT('Ctrl Pts',(4.10740958268476,28.8911528852157,53.2696136073985));
#91139=CARTESIAN_POINT('Ctrl Pts',(4.10970730185573,28.9269030806228,53.2472209860022));
#91140=CARTESIAN_POINT('Ctrl Pts',(4.1120050210267,28.9632646532559,53.2259714254524));
#91141=CARTESIAN_POINT('Ctrl Pts',(4.11587409437492,29.0244930197819,53.1901898080018));
#91142=CARTESIAN_POINT('Ctrl Pts',(4.11974316772313,29.0876959275459,53.1575116551603));
#91143=CARTESIAN_POINT('Ctrl Pts',(4.12361224107135,29.1525259668356,53.1281599091771));
#91144=CARTESIAN_POINT('Ctrl Pts',(4.12747554946714,29.2172594088114,53.0988518975468));
#91145=CARTESIAN_POINT('Ctrl Pts',(4.13133885786292,29.2836147309311,53.0728606532385));
#91146=CARTESIAN_POINT('Ctrl Pts',(4.13520216625871,29.3512184250663,53.0503641287341));
#91147=CARTESIAN_POINT('Ctrl Pts',(4.13906094275162,29.4187428158314,53.027893994063));
#91148=CARTESIAN_POINT('Ctrl Pts',(4.14291971924454,29.4875122110839,53.008910588793));
#91149=CARTESIAN_POINT('Ctrl Pts',(4.14677849573745,29.5571331576811,52.9935437900431));
#91150=CARTESIAN_POINT('Ctrl Pts',(4.15063484132565,29.6267102453279,52.9781866718808));
#91151=CARTESIAN_POINT('Ctrl Pts',(4.15449118691386,29.6971373467649,52.9664417444936));
#91152=CARTESIAN_POINT('Ctrl Pts',(4.15834753250207,29.768007299874,52.9583886389451));
#91153=CARTESIAN_POINT('Ctrl Pts',(4.1622027387474,29.8388563147208,52.9503379126565));
#91154=CARTESIAN_POINT('Ctrl Pts',(4.16605794499273,29.9101474390716,52.9459768976138));
#91155=CARTESIAN_POINT('Ctrl Pts',(4.16991315123806,29.981466521313,52.945333586037));
#91156=CARTESIAN_POINT('Ctrl Pts',(4.17376850808931,30.0527883896766,52.9446902493287));
#91157=CARTESIAN_POINT('Ctrl Pts',(4.17762386494056,30.1241377323131,52.9477649066092));
#91158=CARTESIAN_POINT('Ctrl Pts',(4.18147922179181,30.1951002548227,52.9545334387803));
#91159=CARTESIAN_POINT('Ctrl Pts',(4.18533861426037,30.2661370577674,52.9613090559519));
#91160=CARTESIAN_POINT('Ctrl Pts',(4.18919800672893,30.3367857477192,52.9717862203667));
#91161=CARTESIAN_POINT('Ctrl Pts',(4.19305739919749,30.4066379145324,52.9858889879243));
#91162=CARTESIAN_POINT('Ctrl Pts',(4.19691897680092,30.4765296306807,52.9999997402747));
#91163=CARTESIAN_POINT('Ctrl Pts',(4.20078055440436,30.5456234551803,53.0177400613253));
#91164=CARTESIAN_POINT('Ctrl Pts',(4.20464213200779,30.613524608849,53.0389836520731));
#91165=CARTESIAN_POINT('Ctrl Pts',(4.20851046612266,30.6815445675681,53.0602644122315));
#91166=CARTESIAN_POINT('Ctrl Pts',(4.21237880023754,30.7483672335379,53.0850605109329));
#91167=CARTESIAN_POINT('Ctrl Pts',(4.21624713435241,30.8136169820425,53.11319715682));
#91168=CARTESIAN_POINT('Ctrl Pts',(4.21854485352336,30.8523741301032,53.1299098059194));
#91169=CARTESIAN_POINT('Ctrl Pts',(4.2208425726943,30.8905767687622,53.1478001486802));
#91170=CARTESIAN_POINT('Ctrl Pts',(4.22314029186525,30.9281506612641,53.1668240912299));
#91171=CARTESIAN_POINT('Ctrl Pts',(4.22700936521347,30.9914204236902,53.1988580447381));
#91172=CARTESIAN_POINT('Ctrl Pts',(4.23087843856169,31.0531537505688,53.2342341040927));
#91173=CARTESIAN_POINT('Ctrl Pts',(4.2347475119099,31.1129749158544,53.2727813111308));
#91174=CARTESIAN_POINT('Ctrl Pts',(4.23861082030568,31.1727069470912,53.3112710825002));
#91175=CARTESIAN_POINT('Ctrl Pts',(4.24247412870147,31.2305320671684,53.3529223615003));
#91176=CARTESIAN_POINT('Ctrl Pts',(4.24633743709725,31.2860981930602,53.3975178627182));
#91177=CARTESIAN_POINT('Ctrl Pts',(4.25019621359016,31.3415991364039,53.4420610506182));
#91178=CARTESIAN_POINT('Ctrl Pts',(4.25405499008307,31.3948459722212,53.4895412978214));
#91179=CARTESIAN_POINT('Ctrl Pts',(4.25791376657599,31.4455161902335,53.5396984878892));
#91180=CARTESIAN_POINT('Ctrl Pts',(4.26177011216419,31.496154487643,53.5898240805454));
#91181=CARTESIAN_POINT('Ctrl Pts',(4.2656264577524,31.5442190431926,53.6426229293582));
#91182=CARTESIAN_POINT('Ctrl Pts',(4.26948280334061,31.5894221252477,53.6977961487259));
#91183=CARTESIAN_POINT('Ctrl Pts',(4.27333800958594,31.6346118522213,53.7529530673723));
#91184=CARTESIAN_POINT('Ctrl Pts',(4.27719321583127,31.676941476376,53.8104825883361));
#91185=CARTESIAN_POINT('Ctrl Pts',(4.2810484220766,31.7161628592673,53.8700519467818));
#91186=CARTESIAN_POINT('Ctrl Pts',(4.28490377892785,31.7553857743651,53.9296236323398));
#91187=CARTESIAN_POINT('Ctrl Pts',(4.28875913577909,31.7914999418219,53.9912349066404));
#91188=CARTESIAN_POINT('Ctrl Pts',(4.29261449263034,31.8243009267392,54.05452462158));
#91189=CARTESIAN_POINT('Ctrl Pts',(4.2964738850989,31.8571362462791,54.1178805853985));
#91190=CARTESIAN_POINT('Ctrl Pts',(4.30033327756746,31.886651236198,54.1829180648712));
#91191=CARTESIAN_POINT('Ctrl Pts',(4.30419267003602,31.9126881934473,54.2492527474926));
#91192=CARTESIAN_POINT('Ctrl Pts',(4.30805424763945,31.9387398924632,54.3156249878979));
#91193=CARTESIAN_POINT('Ctrl Pts',(4.31191582524288,31.9613094849413,54.3832954324829));
#91194=CARTESIAN_POINT('Ctrl Pts',(4.31577740284632,31.9802889661255,54.4518639100173));
#91195=CARTESIAN_POINT('Ctrl Pts',(4.31964573696119,31.9993016552611,54.5205523602028));
#91196=CARTESIAN_POINT('Ctrl Pts',(4.32351407107606,32.0147115867772,54.5901415059713));
#91197=CARTESIAN_POINT('Ctrl Pts',(4.32738240519093,32.0264618851509,54.6602209680826));
#91198=CARTESIAN_POINT('Ctrl Pts',(4.32968012436189,32.0334413458272,54.7018468770145));
#91199=CARTESIAN_POINT('Ctrl Pts',(4.33197784353285,32.0391306287755,54.7436456571901));
#91200=CARTESIAN_POINT('Ctrl Pts',(4.33427556270382,32.0435265158288,54.7855310241446));
#91201=CARTESIAN_POINT('Ctrl Pts',(4.33815880198177,32.0509557445539,54.8563190056285));
#91202=CARTESIAN_POINT('Ctrl Pts',(4.34204204125973,32.0547076876349,54.9274995857473));
#91203=CARTESIAN_POINT('Ctrl Pts',(4.34592528053768,32.0547496441584,54.9987907312877));
#91204=CARTESIAN_POINT('Origin',(-1.54592528053767,30.,55.));
#91205=CARTESIAN_POINT('',(3.19386027176893,28.7479524050421,56.6292250864936));
#91206=CARTESIAN_POINT('',(3.25213375383374,28.7479524050421,56.6292250864936));
#91207=CARTESIAN_POINT('',(-1.54592528053767,28.7479524050421,56.6292250864936));
#91208=CARTESIAN_POINT('',(3.70407471941232,32.0547494644754,54.9985165115458));
#91209=CARTESIAN_POINT('Ctrl Pts',(3.25213375383374,28.7479524050421,56.6292250864936));
#91210=CARTESIAN_POINT('Ctrl Pts',(3.25599067728616,28.6914737930115,56.5858216851185));
#91211=CARTESIAN_POINT('Ctrl Pts',(3.25984760073858,28.6372072335646,56.5394414926044));
#91212=CARTESIAN_POINT('Ctrl Pts',(3.263704524191,28.5854770435146,56.4903430370475));
#91213=CARTESIAN_POINT('Ctrl Pts',(3.26755993040323,28.5337672031355,56.4412638958872));
#91214=CARTESIAN_POINT('Ctrl Pts',(3.27141533661547,28.484592103884,56.3894689480892));
#91215=CARTESIAN_POINT('Ctrl Pts',(3.2752707428277,28.4382413232633,56.3352555553667));
#91216=CARTESIAN_POINT('Ctrl Pts',(3.27912592208643,28.3918932711416,56.2810453539862));
#91217=CARTESIAN_POINT('Ctrl Pts',(3.28298110134515,28.3483695220187,56.2244173606011));
#91218=CARTESIAN_POINT('Ctrl Pts',(3.28683628060388,28.3079201049453,56.1657028743431));
#91219=CARTESIAN_POINT('Ctrl Pts',(3.29069525296784,28.2674308897497,56.106930618988));
#91220=CARTESIAN_POINT('Ctrl Pts',(3.2945542253318,28.2300223251508,56.0460681709911));
#91221=CARTESIAN_POINT('Ctrl Pts',(3.29841319769576,28.1959012107259,55.983476039891));
#91222=CARTESIAN_POINT('Ctrl Pts',(3.30227401606044,28.1617637739239,55.9208539668508));
#91223=CARTESIAN_POINT('Ctrl Pts',(3.30613483442512,28.1309171305301,55.856501001065));
#91224=CARTESIAN_POINT('Ctrl Pts',(3.30999565278981,28.1035209114166,55.7907999930867));
#91225=CARTESIAN_POINT('Ctrl Pts',(3.313863586875,28.0760741994231,55.7249778941981));
#91226=CARTESIAN_POINT('Ctrl Pts',(3.3177315209602,28.0520907814756,55.6578032477188));
#91227=CARTESIAN_POINT('Ctrl Pts',(3.3215994550454,28.0316809932176,55.5896760551685));
#91228=CARTESIAN_POINT('Ctrl Pts',(3.32502755325908,28.0135920710364,55.5292958361833));
#91229=CARTESIAN_POINT('Ctrl Pts',(3.32845565147276,27.9983095611418,55.4681678213857));
#91230=CARTESIAN_POINT('Ctrl Pts',(3.33188374968643,27.985876448174,55.4065757991813));
#91231=CARTESIAN_POINT('Ctrl Pts',(3.33575282303467,27.9718439954784,55.3370608562825));
#91232=CARTESIAN_POINT('Ctrl Pts',(3.33962189638291,27.9613871130557,55.2666824303764));
#91233=CARTESIAN_POINT('Ctrl Pts',(3.34349096973115,27.9546042657693,55.195841397286));
#91234=CARTESIAN_POINT('Ctrl Pts',(3.34735427812696,27.9478315249834,55.1251059179417));
#91235=CARTESIAN_POINT('Ctrl Pts',(3.35121758652277,27.9447219988389,55.0539096792663));
#91236=CARTESIAN_POINT('Ctrl Pts',(3.35508089491858,27.9453231361891,54.9826636849266));
#91237=CARTESIAN_POINT('Ctrl Pts',(3.35893967141151,27.9459235683676,54.9115012666035));
#91238=CARTESIAN_POINT('Ctrl Pts',(3.36279844790444,27.950226013748,54.8402896919626));
#91239=CARTESIAN_POINT('Ctrl Pts',(3.36665722439738,27.958225977863,54.7694432715653));
#91240=CARTESIAN_POINT('Ctrl Pts',(3.37051356998561,27.9662209022587,54.6986414821272));
#91241=CARTESIAN_POINT('Ctrl Pts',(3.37436991557383,27.9779086696814,54.6282048721231));
#91242=CARTESIAN_POINT('Ctrl Pts',(3.37822626116206,27.9932328074166,54.558544456065));
#91243=CARTESIAN_POINT('Ctrl Pts',(3.38208146740741,28.0085524176927,54.4889046209161));
#91244=CARTESIAN_POINT('Ctrl Pts',(3.38593667365277,28.0275061610827,54.4200409986257));
#91245=CARTESIAN_POINT('Ctrl Pts',(3.38979187989812,28.0499864442201,54.3523544991473));
#91246=CARTESIAN_POINT('Ctrl Pts',(3.39364723674939,28.0724676055632,54.2846653554555));
#91247=CARTESIAN_POINT('Ctrl Pts',(3.39750259360066,28.0984754249632,54.2181538862027));
#91248=CARTESIAN_POINT('Ctrl Pts',(3.40135795045193,28.1278529579359,54.1532042658406));
#91249=CARTESIAN_POINT('Ctrl Pts',(3.40521734292052,28.1572612420128,54.088186659084));
#91250=CARTESIAN_POINT('Ctrl Pts',(3.4090767353891,28.19004608027,54.0247346083166));
#91251=CARTESIAN_POINT('Ctrl Pts',(3.41293612785768,28.2260033992049,53.9632099427235));
#91252=CARTESIAN_POINT('Ctrl Pts',(3.41679770546114,28.2619810766787,53.9016504427119));
#91253=CARTESIAN_POINT('Ctrl Pts',(3.42065928306459,28.3011345437811,53.8420209064998));
#91254=CARTESIAN_POINT('Ctrl Pts',(3.42452086066805,28.343216496851,53.7846539644227));
#91255=CARTESIAN_POINT('Ctrl Pts',(3.42838919478294,28.3853720797237,53.7271866487574));
#91256=CARTESIAN_POINT('Ctrl Pts',(3.43225752889784,28.4304660711418,53.6719902074214));
#91257=CARTESIAN_POINT('Ctrl Pts',(3.43612586301273,28.4782114877151,53.6193634488477));
#91258=CARTESIAN_POINT('Ctrl Pts',(3.43842358218348,28.5065713852105,53.5881041241673));
#91259=CARTESIAN_POINT('Ctrl Pts',(3.44072130135424,28.5358660346034,53.5577507144534));
#91260=CARTESIAN_POINT('Ctrl Pts',(3.44301902052499,28.5660296831505,53.528359183464));
#91261=CARTESIAN_POINT('Ctrl Pts',(3.4468880938732,28.6168215162709,53.4788675002934));
#91262=CARTESIAN_POINT('Ctrl Pts',(3.45075716722141,28.6702780599787,53.4319114872838));
#91263=CARTESIAN_POINT('Ctrl Pts',(3.45462624056962,28.726115924839,53.387791289705));
#91264=CARTESIAN_POINT('Ctrl Pts',(3.4584895489654,28.7818705908022,53.3437368315986));
#91265=CARTESIAN_POINT('Ctrl Pts',(3.46235285736117,28.8399991568081,53.302510100363));
#91266=CARTESIAN_POINT('Ctrl Pts',(3.46621616575694,28.9001820553276,53.2643738734749));
#91267=CARTESIAN_POINT('Ctrl Pts',(3.47007494224985,28.9602943555354,53.2262823827709));
#91268=CARTESIAN_POINT('Ctrl Pts',(3.47393371874276,29.0224557931115,53.1912744539904));
#91269=CARTESIAN_POINT('Ctrl Pts',(3.47779249523567,29.0863158500689,53.1595710183045));
#91270=CARTESIAN_POINT('Ctrl Pts',(3.48164884082387,29.1501356772506,53.1278875547603));
#91271=CARTESIAN_POINT('Ctrl Pts',(3.48550518641207,29.215651566714,53.0995046697073));
#91272=CARTESIAN_POINT('Ctrl Pts',(3.48936153200027,29.2824875784926,53.0745978374681));
#91273=CARTESIAN_POINT('Ctrl Pts',(3.49321673824559,29.3493038438215,53.0496983638593));
#91274=CARTESIAN_POINT('Ctrl Pts',(3.49707194449091,29.4174390022002,53.0282730737539));
#91275=CARTESIAN_POINT('Ctrl Pts',(3.50092715073624,29.4864978769356,53.0104490124381));
#91276=CARTESIAN_POINT('Ctrl Pts',(3.50478250758748,29.555559449497,52.9926242548149));
#91277=CARTESIAN_POINT('Ctrl Pts',(3.50863786443872,29.6255443391362,52.9784011245611));
#91278=CARTESIAN_POINT('Ctrl Pts',(3.51249322128996,29.6960446631106,52.9678561282044));
#91279=CARTESIAN_POINT('Ctrl Pts',(3.51635261375851,29.7666187837111,52.9573000938111));
#91280=CARTESIAN_POINT('Ctrl Pts',(3.52021200622706,29.8377089342517,52.9504299510045));
#91281=CARTESIAN_POINT('Ctrl Pts',(3.52407139869561,29.9089004441347,52.9472704919008));
#91282=CARTESIAN_POINT('Ctrl Pts',(3.52793297629904,29.9801322616705,52.9441092439549));
#91283=CARTESIAN_POINT('Ctrl Pts',(3.53179455390247,30.0514650667895,52.9446628582596));
#91284=CARTESIAN_POINT('Ctrl Pts',(3.5356561315059,30.122485273634,52.9489039709846));
#91285=CARTESIAN_POINT('Ctrl Pts',(3.53952446562076,30.1936297428628,52.9531525042847));
#91286=CARTESIAN_POINT('Ctrl Pts',(3.54339279973563,30.2644600389151,52.9611013632751));
#91287=CARTESIAN_POINT('Ctrl Pts',(3.54726113385049,30.3345694703267,52.9726715036716));
#91288=CARTESIAN_POINT('Ctrl Pts',(3.54955885302151,30.3762131804719,52.97954395383));
#91289=CARTESIAN_POINT('Ctrl Pts',(3.55185657219254,30.4176027678515,52.9876930655164));
#91290=CARTESIAN_POINT('Ctrl Pts',(3.55415429136356,30.4586555529481,52.9970939497196));
#91291=CARTESIAN_POINT('Ctrl Pts',(3.55802336471177,30.5277833378795,53.0129238696588));
#91292=CARTESIAN_POINT('Ctrl Pts',(3.56189243805998,30.5962260391793,53.0323677854611));
#91293=CARTESIAN_POINT('Ctrl Pts',(3.56576151140819,30.6635777914809,53.0553503973329));
#91294=CARTESIAN_POINT('Ctrl Pts',(3.56962481980397,30.7308291890946,53.0782987649161));
#91295=CARTESIAN_POINT('Ctrl Pts',(3.57348812819975,30.7969924083183,53.1047752068268));
#91296=CARTESIAN_POINT('Ctrl Pts',(3.57735143659553,30.8616733563969,53.1346537615296));
#91297=CARTESIAN_POINT('Ctrl Pts',(3.58121021308843,30.9262784296698,53.1644972668152));
#91298=CARTESIAN_POINT('Ctrl Pts',(3.58506898958134,30.9894042467702,53.1977347549037));
#91299=CARTESIAN_POINT('Ctrl Pts',(3.58892776607425,31.0506750854305,53.2341915654988));
#91300=CARTESIAN_POINT('Ctrl Pts',(3.59278411166246,31.111907325439,53.2706254094793));
#91301=CARTESIAN_POINT('Ctrl Pts',(3.59664045725066,31.1712864889574,53.3102743044954));
#91302=CARTESIAN_POINT('Ctrl Pts',(3.60049680283886,31.2284612560273,53.3529175779762));
#91303=CARTESIAN_POINT('Ctrl Pts',(3.60435200908419,31.2856191310263,53.3955482526614));
#91304=CARTESIAN_POINT('Ctrl Pts',(3.60820721532952,31.3405735133567,53.4411712592051));
#91305=CARTESIAN_POINT('Ctrl Pts',(3.61206242157485,31.3930033370939,53.4895234972549));
#91306=CARTESIAN_POINT('Ctrl Pts',(3.6159177784261,31.4454352090333,53.5378776242134));
#91307=CARTESIAN_POINT('Ctrl Pts',(3.61977313527734,31.4953419709606,53.5889608634017));
#91308=CARTESIAN_POINT('Ctrl Pts',(3.62362849212858,31.542438125459,53.6424720291536));
#91309=CARTESIAN_POINT('Ctrl Pts',(3.62748788459715,31.5895835781324,53.696039208031));
#91310=CARTESIAN_POINT('Ctrl Pts',(3.63134727706571,31.6339122288386,53.7520390213581));
#91311=CARTESIAN_POINT('Ctrl Pts',(3.63520666953427,31.6751783462013,53.8101365326567));
#91312=CARTESIAN_POINT('Ctrl Pts',(3.6390682471377,31.7164678278714,53.8682669379662));
#91313=CARTESIAN_POINT('Ctrl Pts',(3.64292982474114,31.7546910639894,53.9284969952103));
#91314=CARTESIAN_POINT('Ctrl Pts',(3.64679140234457,31.7896467299854,53.9904643917361));
#91315=CARTESIAN_POINT('Ctrl Pts',(3.65065973645944,31.8246635570874,54.052540211157));
#91316=CARTESIAN_POINT('Ctrl Pts',(3.65452807057431,31.8564011831489,54.1163590037662));
#91317=CARTESIAN_POINT('Ctrl Pts',(3.65839640468919,31.8847054418722,54.1815362195691));
#91318=CARTESIAN_POINT('Ctrl Pts',(3.66069412386016,31.9015176499074,54.2202502845423));
#91319=CARTESIAN_POINT('Ctrl Pts',(3.66299184303114,31.9171194519221,54.2594432652729));
#91320=CARTESIAN_POINT('Ctrl Pts',(3.66528956220212,31.9314869158582,54.2990322001912));
#91321=CARTESIAN_POINT('Ctrl Pts',(3.66976608681323,31.9594782851783,54.3761612261088));
#91322=CARTESIAN_POINT('Ctrl Pts',(3.67424261142434,31.982872578991,54.4550424288438));
#91323=CARTESIAN_POINT('Ctrl Pts',(3.67871913603545,32.0014795158374,54.5351588333815));
#91324=CARTESIAN_POINT('Ctrl Pts',(3.68315616207688,32.0199222745645,54.6145683316331));
#91325=CARTESIAN_POINT('Ctrl Pts',(3.6875931881183,32.033661696059,54.6951911642588));
#91326=CARTESIAN_POINT('Ctrl Pts',(3.69203021415973,32.0425588387469,54.7765029021285));
#91327=CARTESIAN_POINT('Ctrl Pts',(3.69604504924393,32.050609402408,54.850077682828));
#91328=CARTESIAN_POINT('Ctrl Pts',(3.70005988432813,32.0546958210966,54.9242161665668));
#91329=CARTESIAN_POINT('Ctrl Pts',(3.70407471941232,32.0547494644754,54.9985165115458));
#91330=CARTESIAN_POINT('Ctrl Pts',(3.70407471946232,32.0547494644761,54.998516512471));
#91331=CARTESIAN_POINT('Ctrl Pts',(3.70793830290605,32.0548010869056,55.0700177265207));
#91332=CARTESIAN_POINT('Ctrl Pts',(3.71180188634978,32.05111623467,55.1415522381299));
#91333=CARTESIAN_POINT('Ctrl Pts',(3.71566546979351,32.0437110737994,55.2127031013635));
#91334=CARTESIAN_POINT('Ctrl Pts',(3.71952882663495,32.0363063472475,55.2838497915415));
#91335=CARTESIAN_POINT('Ctrl Pts',(3.7233921834764,32.0251817962441,55.3546123983532));
#91336=CARTESIAN_POINT('Ctrl Pts',(3.72725554031784,32.0104054413667,55.4245792315022));
#91337=CARTESIAN_POINT('Ctrl Pts',(3.73111993974999,31.9956250988457,55.4945649463577));
#91338=CARTESIAN_POINT('Ctrl Pts',(3.73498433918215,31.9771910976799,55.563753989815));
#91339=CARTESIAN_POINT('Ctrl Pts',(3.7388487386143,31.9552221704314,55.6317466475999));
#91340=CARTESIAN_POINT('Ctrl Pts',(3.74271803189463,31.9332254218883,55.699825410807));
#91341=CARTESIAN_POINT('Ctrl Pts',(3.74658732517497,31.9076849661807,55.7667043065627));
#91342=CARTESIAN_POINT('Ctrl Pts',(3.7504566184553,31.87876856606,55.8320013447615));
#91343=CARTESIAN_POINT('Ctrl Pts',(3.75432884727622,31.8498302277557,55.897347922267));
#91344=CARTESIAN_POINT('Ctrl Pts',(3.75820107609715,31.8175110677505,55.9611098252564));
#91345=CARTESIAN_POINT('Ctrl Pts',(3.76207330491807,31.7820246506315,56.0229299619434));
#91346=CARTESIAN_POINT('Ctrl Pts',(3.76595231070725,31.7464761270789,56.0848582929349));
#91347=CARTESIAN_POINT('Ctrl Pts',(3.76983131649643,31.7077495507213,56.1448376751856));
#91348=CARTESIAN_POINT('Ctrl Pts',(3.7737103222856,31.6661010629529,56.2025409808098));
#91349=CARTESIAN_POINT('Ctrl Pts',(3.77461515920396,31.6563859216578,56.2160011518118));
#91350=CARTESIAN_POINT('Ctrl Pts',(3.77551999612232,31.6465119574723,56.2293376254161));
#91351=CARTESIAN_POINT('Ctrl Pts',(3.77642483304068,31.6364827163498,56.242546530955));
#91352=CARTESIAN_POINT('Ctrl Pts',(3.78029390638889,31.5935977845543,56.2990276750626));
#91353=CARTESIAN_POINT('Ctrl Pts',(3.7841629797371,31.5477013562299,56.3533966652134));
#91354=CARTESIAN_POINT('Ctrl Pts',(3.78803205308531,31.499029141768,56.4053146247835));
#91355=CARTESIAN_POINT('Ctrl Pts',(3.7918953614811,31.4504294493225,56.4571552261492));
#91356=CARTESIAN_POINT('Ctrl Pts',(3.79575866987688,31.3990625100132,56.5065516946494));
#91357=CARTESIAN_POINT('Ctrl Pts',(3.79962197827267,31.3452053570871,56.5531967389112));
#91358=CARTESIAN_POINT('Ctrl Pts',(3.80348075476558,31.2914113819766,56.5997870656127));
#91359=CARTESIAN_POINT('Ctrl Pts',(3.80733953125849,31.2351333611201,56.6436320626762));
#91360=CARTESIAN_POINT('Ctrl Pts',(3.8111983077514,31.1766851454725,56.6844612286795));
#91361=CARTESIAN_POINT('Ctrl Pts',(3.81505465333961,31.1182737503153,56.7252646736253));
#91362=CARTESIAN_POINT('Ctrl Pts',(3.81891099892781,31.0576952700763,56.7630557792994));
#91363=CARTESIAN_POINT('Ctrl Pts',(3.82276734451602,30.9952954419552,56.7976052252158));
#91364=CARTESIAN_POINT('Ctrl Pts',(3.82662255076135,30.9329140496299,56.8321444636277));
#91365=CARTESIAN_POINT('Ctrl Pts',(3.83047775700668,30.8687128024807,56.863443708473));
#91366=CARTESIAN_POINT('Ctrl Pts',(3.83433296325201,30.8030636482535,56.8913186773661));
#91367=CARTESIAN_POINT('Ctrl Pts',(3.83818832010326,30.7374119294031,56.9191947352114));
#91368=CARTESIAN_POINT('Ctrl Pts',(3.84204367695451,30.6703126391839,56.9436460636852));
#91369=CARTESIAN_POINT('Ctrl Pts',(3.84589903380576,30.6021577906026,56.9645364740102));
#91370=CARTESIAN_POINT('Ctrl Pts',(3.84975842627431,30.5339316005354,56.9854487514943));
#91371=CARTESIAN_POINT('Ctrl Pts',(3.85361781874287,30.4646481118632,57.0027925274235));
#91372=CARTESIAN_POINT('Ctrl Pts',(3.85747721121143,30.3947137246528,57.0164817475174));
#91373=CARTESIAN_POINT('Ctrl Pts',(3.86133878881486,30.3247397415552,57.0301787182592));
#91374=CARTESIAN_POINT('Ctrl Pts',(3.8652003664183,30.2541146074705,57.0402169457162));
#91375=CARTESIAN_POINT('Ctrl Pts',(3.86906194402173,30.183251389623,57.0465621150362));
#91376=CARTESIAN_POINT('Ctrl Pts',(3.8729302781366,30.1122641840712,57.0529183863495));
#91377=CARTESIAN_POINT('Ctrl Pts',(3.87679861225147,30.0410385486675,57.0555686805711));
#91378=CARTESIAN_POINT('Ctrl Pts',(3.88066694636634,29.9699884019044,57.0545308141957));
#91379=CARTESIAN_POINT('Ctrl Pts',(3.88296466553731,29.9277859241789,57.0539143406966));
#91380=CARTESIAN_POINT('Ctrl Pts',(3.88526238470827,29.885645300261,57.0519976298562));
#91381=CARTESIAN_POINT('Ctrl Pts',(3.88756010387923,29.8436519877082,57.0487930255525));
#91382=CARTESIAN_POINT('Ctrl Pts',(3.89142879126944,29.7729475253008,57.0433974087089));
#91383=CARTESIAN_POINT('Ctrl Pts',(3.89529747865965,29.7023842197183,57.0343268801619));
#91384=CARTESIAN_POINT('Ctrl Pts',(3.89916616604986,29.6323744933448,57.0215956691081));
#91385=CARTESIAN_POINT('Ctrl Pts',(3.90302937622933,29.5624638853508,57.0088824826499));
#91386=CARTESIAN_POINT('Ctrl Pts',(3.9068925864088,29.4931057753174,56.9925189834931));
#91387=CARTESIAN_POINT('Ctrl Pts',(3.91075579658827,29.424708554523,56.9725712446604));
#91388=CARTESIAN_POINT('Ctrl Pts',(3.91461452942191,29.3563906040755,56.9526466246644));
#91389=CARTESIAN_POINT('Ctrl Pts',(3.91847326225554,29.2890317950303,56.9291461509425));
#91390=CARTESIAN_POINT('Ctrl Pts',(3.92233199508918,29.2230295971289,56.9021867825117));
#91391=CARTESIAN_POINT('Ctrl Pts',(3.92618810381818,29.1570722835668,56.8752457476135));
#91392=CARTESIAN_POINT('Ctrl Pts',(3.93004421254717,29.0924701982269,56.8448506709057));
#91393=CARTESIAN_POINT('Ctrl Pts',(3.93390032127617,29.0296034520015,56.8111676074103));
#91394=CARTESIAN_POINT('Ctrl Pts',(3.93775577559101,28.9667473747926,56.7774902602148));
#91395=CARTESIAN_POINT('Ctrl Pts',(3.94161122990586,28.9056264836543,56.7405262564653));
#91396=CARTESIAN_POINT('Ctrl Pts',(3.9454666842207,28.8465974065651,56.7004881710725));
#91397=CARTESIAN_POINT('Ctrl Pts',(3.94765985266874,28.81301881924,56.6777125761796));
#91398=CARTESIAN_POINT('Ctrl Pts',(3.94985302111678,28.7801166565293,56.6539430791467));
#91399=CARTESIAN_POINT('Ctrl Pts',(3.95204618956481,28.7479524050421,56.6292250864936));
#91400=CARTESIAN_POINT('',(3.64592528049244,32.0547492155205,55.0017954993351));
#91401=CARTESIAN_POINT('Ctrl Pts',(3.64592528053768,32.0547492155198,55.001795500168));
#91402=CARTESIAN_POINT('Ctrl Pts',(3.65155534725615,32.0546586344092,55.1054554547564));
#91403=CARTESIAN_POINT('Ctrl Pts',(3.65718541397462,32.0467203700807,55.2087840266247));
#91404=CARTESIAN_POINT('Ctrl Pts',(3.66281548069309,32.0311035472159,55.3108310521601));
#91405=CARTESIAN_POINT('Ctrl Pts',(3.66436496635288,32.0268055443164,55.3389160484129));
#91406=CARTESIAN_POINT('Ctrl Pts',(3.66591445201267,32.0219261885247,55.3669041565549));
#91407=CARTESIAN_POINT('Ctrl Pts',(3.66746393767245,32.0164695735925,55.394775912735));
#91408=CARTESIAN_POINT('Ctrl Pts',(3.67133301102066,32.0028443791468,55.4643718256258));
#91409=CARTESIAN_POINT('Ctrl Pts',(3.67520208436887,31.9855852435917,55.5333978458126));
#91410=CARTESIAN_POINT('Ctrl Pts',(3.67907115771708,31.9647545311723,55.6014459200443));
#91411=CARTESIAN_POINT('Ctrl Pts',(3.68293446611286,31.9439548566929,55.6693926020625));
#91412=CARTESIAN_POINT('Ctrl Pts',(3.68679777450863,31.9195943097706,55.7363637697985));
#91413=CARTESIAN_POINT('Ctrl Pts',(3.69066108290441,31.8917862649139,55.8019615267474));
#91414=CARTESIAN_POINT('Ctrl Pts',(3.69451985939732,31.8640108406366,55.8674823334163));
#91415=CARTESIAN_POINT('Ctrl Pts',(3.69837863589022,31.8327961401176,55.9316324843945));
#91416=CARTESIAN_POINT('Ctrl Pts',(3.70223741238313,31.7983047958053,55.9940308968456));
#91417=CARTESIAN_POINT('Ctrl Pts',(3.70609375797133,31.7638351799272,56.0563900003099));
#91418=CARTESIAN_POINT('Ctrl Pts',(3.70995010355953,31.7260932500095,56.1169991304984));
#91419=CARTESIAN_POINT('Ctrl Pts',(3.71380644914773,31.6852884029895,56.1755001323901));
#91420=CARTESIAN_POINT('Ctrl Pts',(3.71766165539305,31.6444956116089,56.2339838503796));
#91421=CARTESIAN_POINT('Ctrl Pts',(3.72151686163838,31.6006419774188,56.2903602783589));
#91422=CARTESIAN_POINT('Ctrl Pts',(3.7253720678837,31.5539802651177,56.3443001517983));
#91423=CARTESIAN_POINT('Ctrl Pts',(3.72922742473494,31.5073167299491,56.3982421324307));
#91424=CARTESIAN_POINT('Ctrl Pts',(3.73308278158618,31.4578452183628,56.4497470035925));
#91425=CARTESIAN_POINT('Ctrl Pts',(3.73693813843742,31.4058576914259,56.4985198410294));
#91426=CARTESIAN_POINT('Ctrl Pts',(3.74079753090597,31.3538157462414,56.5473437317188));
#91427=CARTESIAN_POINT('Ctrl Pts',(3.74465692337453,31.2992528833491,56.59342954688));
#91428=CARTESIAN_POINT('Ctrl Pts',(3.74851631584308,31.2424960612611,56.6365210356884));
#91429=CARTESIAN_POINT('Ctrl Pts',(3.75237789344651,31.1857071042418,56.6796369223045));
#91430=CARTESIAN_POINT('Ctrl Pts',(3.75623947104993,31.1267221170847,56.7197548343266));
#91431=CARTESIAN_POINT('Ctrl Pts',(3.76010104865336,31.0658968318021,56.7566620353541));
#91432=CARTESIAN_POINT('Ctrl Pts',(3.76396938276822,31.0049651219496,56.7936338120424));
#91433=CARTESIAN_POINT('Ctrl Pts',(3.76783771688309,30.942187113305,56.8273834317251));
#91434=CARTESIAN_POINT('Ctrl Pts',(3.77170605099795,30.8779422625793,56.8577445858021));
#91435=CARTESIAN_POINT('Ctrl Pts',(3.77400377016897,30.8397820052776,56.8757785517693));
#91436=CARTESIAN_POINT('Ctrl Pts',(3.77630148934,30.8011046100197,56.8926179419242));
#91437=CARTESIAN_POINT('Ctrl Pts',(3.77859920851102,30.7619922359673,56.9082361999568));
#91438=CARTESIAN_POINT('Ctrl Pts',(3.78246828185923,30.696131861932,56.9345354042555));
#91439=CARTESIAN_POINT('Ctrl Pts',(3.78633735520744,30.6287793604348,56.957472487004));
#91440=CARTESIAN_POINT('Ctrl Pts',(3.79020642855566,30.5603113789127,56.976878529693));
#91441=CARTESIAN_POINT('Ctrl Pts',(3.79406973695144,30.4919454152695,56.996255657212));
#91442=CARTESIAN_POINT('Ctrl Pts',(3.79793304534723,30.4224677343409,57.0121120567743));
#91443=CARTESIAN_POINT('Ctrl Pts',(3.80179635374301,30.3522741165739,57.0243271744686));
#91444=CARTESIAN_POINT('Ctrl Pts',(3.80565513023592,30.2821628403199,57.0365279630643));
#91445=CARTESIAN_POINT('Ctrl Pts',(3.80951390672883,30.2113377717017,57.0450958714596));
#91446=CARTESIAN_POINT('Ctrl Pts',(3.81337268322174,30.140207281009,57.0499608486144));
#91447=CARTESIAN_POINT('Ctrl Pts',(3.81722902880995,30.0691216002307,57.0548227609906));
#91448=CARTESIAN_POINT('Ctrl Pts',(3.82108537439815,29.9977313626162,57.0559863371499));
#91449=CARTESIAN_POINT('Ctrl Pts',(3.82494171998636,29.9264510391778,57.0534332501598));
#91450=CARTESIAN_POINT('Ctrl Pts',(3.82879692623169,29.8551917752442,57.0508809174698));
#91451=CARTESIAN_POINT('Ctrl Pts',(3.83265213247702,29.7840428462275,57.0446141189907));
#91452=CARTESIAN_POINT('Ctrl Pts',(3.83650733872235,29.7134179720959,57.0346666321003));
#91453=CARTESIAN_POINT('Ctrl Pts',(3.8403626955736,29.6427903389618,57.0247187566055));
#91454=CARTESIAN_POINT('Ctrl Pts',(3.84421805242484,29.5726872820889,57.0110899771617));
#91455=CARTESIAN_POINT('Ctrl Pts',(3.84807340927609,29.503514929387,56.9938656266555));
#91456=CARTESIAN_POINT('Ctrl Pts',(3.85193280174465,29.4342701701207,56.9766232464598));
#91457=CARTESIAN_POINT('Ctrl Pts',(3.8557921942132,29.3659585321451,56.9557778996608));
#91458=CARTESIAN_POINT('Ctrl Pts',(3.85965158668176,29.298972633494,56.9314652971021));
#91459=CARTESIAN_POINT('Ctrl Pts',(3.8635131642852,29.2319488083494,56.9071389290825));
#91460=CARTESIAN_POINT('Ctrl Pts',(3.86737474188863,29.166252664371,56.8793415867396));
#91461=CARTESIAN_POINT('Ctrl Pts',(3.87123631949207,29.1022558669431,56.8482567554488));
#91462=CARTESIAN_POINT('Ctrl Pts',(3.87510465360694,29.0381470958252,56.8171175357603));
#91463=CARTESIAN_POINT('Ctrl Pts',(3.87897298772181,28.9757440330042,56.7826795777972));
#91464=CARTESIAN_POINT('Ctrl Pts',(3.88284132183667,28.915392205271,56.7451714798589));
#91465=CARTESIAN_POINT('Ctrl Pts',(3.88513904100764,28.8795443318796,56.7228923609566));
#91466=CARTESIAN_POINT('Ctrl Pts',(3.88743676017861,28.8444195966072,56.6995308769136));
#91467=CARTESIAN_POINT('Ctrl Pts',(3.88973447934958,28.8100848707453,56.6751416500317));
#91468=CARTESIAN_POINT('Ctrl Pts',(3.8911385956916,28.7891032162897,56.6602376041123));
#91469=CARTESIAN_POINT('Ctrl Pts',(3.89254271203362,28.7683867515158,56.644928732705));
#91470=CARTESIAN_POINT('Ctrl Pts',(3.89394682837563,28.7479524050421,56.6292250864936));
#91471=CARTESIAN_POINT('Ctrl Pts',(3.19386027176893,28.7479524050421,56.6292250864936));
#91472=CARTESIAN_POINT('Ctrl Pts',(3.19772209747134,28.6914220012474,56.5857818835256));
#91473=CARTESIAN_POINT('Ctrl Pts',(3.20158392317375,28.6372079170157,56.5394334898166));
#91474=CARTESIAN_POINT('Ctrl Pts',(3.20544574887617,28.5856083501764,56.4904676525874));
#91475=CARTESIAN_POINT('Ctrl Pts',(3.20931422741344,28.5339198918585,56.4414174610517));
#91476=CARTESIAN_POINT('Ctrl Pts',(3.21318270595072,28.4848552756939,56.3897411776724));
#91477=CARTESIAN_POINT('Ctrl Pts',(3.217051184488,28.4386740269193,56.3357614937868));
#91478=CARTESIAN_POINT('Ctrl Pts',(3.21900840776474,28.4153090232932,56.3084509393261));
#91479=CARTESIAN_POINT('Ctrl Pts',(3.22096563104148,28.3926814269665,56.2805512636196));
#91480=CARTESIAN_POINT('Ctrl Pts',(3.22292285431822,28.3708205831157,56.2521070202265));
#91481=CARTESIAN_POINT('Ctrl Pts',(3.2267919276666,28.3276056830472,56.195877940318));
#91482=CARTESIAN_POINT('Ctrl Pts',(3.23066100101498,28.2872205677673,56.1372988340834));
#91483=CARTESIAN_POINT('Ctrl Pts',(3.23453007436335,28.249930197065,56.076686234404));
#91484=CARTESIAN_POINT('Ctrl Pts',(3.2383933827593,28.2126953893345,56.0161639480173));
#91485=CARTESIAN_POINT('Ctrl Pts',(3.24225669115525,28.1785464255646,55.9536145928793));
#91486=CARTESIAN_POINT('Ctrl Pts',(3.2461199995512,28.1477069248002,55.8893862637049));
#91487=CARTESIAN_POINT('Ctrl Pts',(3.24997877604428,28.116903600703,55.8252332783859));
#91488=CARTESIAN_POINT('Ctrl Pts',(3.25383755253736,28.0894022374831,55.759405667002));
#91489=CARTESIAN_POINT('Ctrl Pts',(3.25769632903044,28.0653812767344,55.6922773707773));
#91490=CARTESIAN_POINT('Ctrl Pts',(3.26155267461882,28.0413754484161,55.6251913632135));
#91491=CARTESIAN_POINT('Ctrl Pts',(3.26540902020719,28.0208458358845,55.5568067527675));
#91492=CARTESIAN_POINT('Ctrl Pts',(3.26926536579557,28.003922763762,55.4875174145327));
#91493=CARTESIAN_POINT('Ctrl Pts',(3.27312057204107,27.9870046914979,55.4182485475735));
#91494=CARTESIAN_POINT('Ctrl Pts',(3.27697577828658,27.9736911594497,55.3480759551445));
#91495=CARTESIAN_POINT('Ctrl Pts',(3.28083098453208,27.9640621465015,55.2774069559186));
#91496=CARTESIAN_POINT('Ctrl Pts',(3.2846863413835,27.9544327573902,55.2067351959664));
#91497=CARTESIAN_POINT('Ctrl Pts',(3.28854169823492,27.9484882365511,55.135567472352));
#91498=CARTESIAN_POINT('Ctrl Pts',(3.29239705508633,27.9462568852949,55.0643178148045));
#91499=CARTESIAN_POINT('Ctrl Pts',(3.29625644755507,27.9440231983586,54.9929935762615));
#91500=CARTESIAN_POINT('Ctrl Pts',(3.3001158400238,27.9455104551327,54.9215877191223));
#91501=CARTESIAN_POINT('Ctrl Pts',(3.30397523249253,27.9506948035876,54.8505149691208));
#91502=CARTESIAN_POINT('Ctrl Pts',(3.30783681009614,27.9558820873492,54.7794019787068));
#91503=CARTESIAN_POINT('Ctrl Pts',(3.31169838769975,27.9647705692329,54.7086229531048));
#91504=CARTESIAN_POINT('Ctrl Pts',(3.31555996530335,27.977284725652,54.6385854438191));
#91505=CARTESIAN_POINT('Ctrl Pts',(3.3194282994184,27.989820777796,54.5684253915521));
#91506=CARTESIAN_POINT('Ctrl Pts',(3.32329663353344,28.0059950596976,54.4990099191882));
#91507=CARTESIAN_POINT('Ctrl Pts',(3.32716496764848,28.0256815275821,54.4307336897643));
#91508=CARTESIAN_POINT('Ctrl Pts',(3.32946268681792,28.0373749266762,54.3901788678441));
#91509=CARTESIAN_POINT('Ctrl Pts',(3.33176040598735,28.0503065279621,54.3500256656002));
#91510=CARTESIAN_POINT('Ctrl Pts',(3.33405812515678,28.0644419479984,54.310353286217));
#91511=CARTESIAN_POINT('Ctrl Pts',(3.33792719850495,28.0882442375276,54.2435499327991));
#91512=CARTESIAN_POINT('Ctrl Pts',(3.34179627185313,28.1155556601753,54.1778494349638));
#91513=CARTESIAN_POINT('Ctrl Pts',(3.34566534520131,28.1462539875542,54.1136460730379));
#91514=CARTESIAN_POINT('Ctrl Pts',(3.34952865359705,28.1769065741622,54.0495383746711));
#91515=CARTESIAN_POINT('Ctrl Pts',(3.35339196199279,28.2109358404614,53.9869238189406));
#91516=CARTESIAN_POINT('Ctrl Pts',(3.35725527038854,28.2481706198582,53.9261790720181));
#91517=CARTESIAN_POINT('Ctrl Pts',(3.36111404688141,28.2853617205251,53.8655055824908));
#91518=CARTESIAN_POINT('Ctrl Pts',(3.36497282337429,28.3257506124843,53.8066979570904));
#91519=CARTESIAN_POINT('Ctrl Pts',(3.36883159986716,28.3691199117373,53.7501089246625));
#91520=CARTESIAN_POINT('Ctrl Pts',(3.37268794545533,28.4124618897308,53.6935555414996));
#91521=CARTESIAN_POINT('Ctrl Pts',(3.37654429104349,28.4587802551666,53.6392183630728));
#91522=CARTESIAN_POINT('Ctrl Pts',(3.38040063663166,28.5078147798167,53.5874205044789));
#91523=CARTESIAN_POINT('Ctrl Pts',(3.38425584287695,28.5568348174,53.5356379493685));
#91524=CARTESIAN_POINT('Ctrl Pts',(3.38811104912224,28.608569087273,53.4863935772635));
#91525=CARTESIAN_POINT('Ctrl Pts',(3.39196625536753,28.6627187609505,53.4399754969277));
#91526=CARTESIAN_POINT('Ctrl Pts',(3.39582161221874,28.716870550017,53.393555603242));
#91527=CARTESIAN_POINT('Ctrl Pts',(3.39967696906994,28.7734375599698,53.3499625350206));
#91528=CARTESIAN_POINT('Ctrl Pts',(3.40353232592115,28.8320872960135,53.3094446242826));
#91529=CARTESIAN_POINT('Ctrl Pts',(3.40739171838967,28.8907984240112,53.2688843011848));
#91530=CARTESIAN_POINT('Ctrl Pts',(3.41125111085819,28.951596229579,53.2314058379809));
#91531=CARTESIAN_POINT('Ctrl Pts',(3.41511050332671,29.014119347079,53.1972141278854));
#91532=CARTESIAN_POINT('Ctrl Pts',(3.4189720809301,29.0766778643073,53.1630030589144));
#91533=CARTESIAN_POINT('Ctrl Pts',(3.4228336585335,29.1409632000845,53.1320826582238));
#91534=CARTESIAN_POINT('Ctrl Pts',(3.42669523613689,29.2065919913585,53.1046105164575));
#91535=CARTESIAN_POINT('Ctrl Pts',(3.43056357025173,29.2723356117837,53.0770903073314));
#91536=CARTESIAN_POINT('Ctrl Pts',(3.43443190436656,29.3394269233546,53.0530305668982));
#91537=CARTESIAN_POINT('Ctrl Pts',(3.43830023848139,29.4074659908464,53.0325394513495));
#91538=CARTESIAN_POINT('Ctrl Pts',(3.44059795765271,29.4478799429853,53.0203681063621));
#91539=CARTESIAN_POINT('Ctrl Pts',(3.44289567682402,29.4886280333401,53.0094548530609));
#91540=CARTESIAN_POINT('Ctrl Pts',(3.44519339599534,29.5296250715218,52.9998137613814));
#91541=CARTESIAN_POINT('Ctrl Pts',(3.44906246934354,29.5986589855718,52.9835793619256));
#91542=CARTESIAN_POINT('Ctrl Pts',(3.45293154269173,29.6686695703827,52.9708912873145));
#91543=CARTESIAN_POINT('Ctrl Pts',(3.45680061603993,29.7392592815901,52.9618606916447));
#91544=CARTESIAN_POINT('Ctrl Pts',(3.46066392443569,29.8097438135233,52.9528435516397));
#91545=CARTESIAN_POINT('Ctrl Pts',(3.46452723283146,29.8808052810812,52.9474731342666));
#91546=CARTESIAN_POINT('Ctrl Pts',(3.46839054122722,29.9520343959929,52.9458099252182));
#91547=CARTESIAN_POINT('Ctrl Pts',(3.47224931772011,30.0231799546887,52.9441486672182));
#91548=CARTESIAN_POINT('Ctrl Pts',(3.47610809421301,30.094492286807,52.9461859906645));
#91549=CARTESIAN_POINT('Ctrl Pts',(3.4799668707059,30.1655571482066,52.9519305692488));
#91550=CARTESIAN_POINT('Ctrl Pts',(3.48382321629408,30.2365772410361,52.9576715289339));
#91551=CARTESIAN_POINT('Ctrl Pts',(3.48767956188226,30.3073496893853,52.967115071211));
#91552=CARTESIAN_POINT('Ctrl Pts',(3.49153590747045,30.3774618917421,52.9802178130347));
#91553=CARTESIAN_POINT('Ctrl Pts',(3.49539111371576,30.4475533797111,52.9933166837023));
#91554=CARTESIAN_POINT('Ctrl Pts',(3.49924631996107,30.5169845316913,53.0100725184486));
#91555=CARTESIAN_POINT('Ctrl Pts',(3.50310152620637,30.5853512211227,53.030390518293));
#91556=CARTESIAN_POINT('Ctrl Pts',(3.5069568830576,30.6537205813393,53.050709311872));
#91557=CARTESIAN_POINT('Ctrl Pts',(3.51081223990882,30.7210249314183,53.0745904063286));
#91558=CARTESIAN_POINT('Ctrl Pts',(3.51466759676005,30.7868753035779,53.1018891446706));
#91559=CARTESIAN_POINT('Ctrl Pts',(3.51852698922858,30.8527946049993,53.1292164581265));
#91560=CARTESIAN_POINT('Ctrl Pts',(3.52238638169712,30.9172564406547,53.1599683704244));
#91561=CARTESIAN_POINT('Ctrl Pts',(3.52624577416566,30.9798926790859,53.1939524092722));
#91562=CARTESIAN_POINT('Ctrl Pts',(3.53010735176907,31.042564381293,53.2279556894149));
#91563=CARTESIAN_POINT('Ctrl Pts',(3.53396892937248,31.1034080141042,53.2651944853304));
#91564=CARTESIAN_POINT('Ctrl Pts',(3.53783050697589,31.162083256404,53.3054321885255));
#91565=CARTESIAN_POINT('Ctrl Pts',(3.54169884109074,31.2208611613942,53.3457402946828));
#91566=CARTESIAN_POINT('Ctrl Pts',(3.54556717520559,31.2774627151784,53.3890574888126));
#91567=CARTESIAN_POINT('Ctrl Pts',(3.54943550932044,31.3315801405265,53.4351064279462));
#91568=CARTESIAN_POINT('Ctrl Pts',(3.55173322849159,31.3637248938038,53.4624586491135));
#91569=CARTESIAN_POINT('Ctrl Pts',(3.55403094766275,31.3949938940229,53.4907739380971));
#91570=CARTESIAN_POINT('Ctrl Pts',(3.5563286668339,31.4253291162108,53.5199883537682));
#91571=CARTESIAN_POINT('Ctrl Pts',(3.56013990426076,31.4756462896958,53.5684464402949));
#91572=CARTESIAN_POINT('Ctrl Pts',(3.56395114168762,31.5236017843575,53.6195819833469));
#91573=CARTESIAN_POINT('Ctrl Pts',(3.56776237911448,31.5688910656209,53.6731321140691));
#91574=CARTESIAN_POINT('Ctrl Pts',(3.5715685505651,31.6141201474276,53.7266110648411));
#91575=CARTESIAN_POINT('Ctrl Pts',(3.57537472201571,31.6566897173767,53.7824978653989));
#91576=CARTESIAN_POINT('Ctrl Pts',(3.57918089346633,31.6963307948588,53.8404917434905));
#91577=CARTESIAN_POINT('Ctrl Pts',(3.58298336737587,31.7359333626432,53.8984292828836));
#91578=CARTESIAN_POINT('Ctrl Pts',(3.58678584128542,31.7726127957148,53.9584694309203));
#91579=CARTESIAN_POINT('Ctrl Pts',(3.59058831519496,31.8061405313258,54.0202786398154));
#91580=CARTESIAN_POINT('Ctrl Pts',(3.5943884546426,31.8396476831739,54.0820499020349));
#91581=CARTESIAN_POINT('Ctrl Pts',(3.59818859409023,31.870006736961,54.145587631284));
#91582=CARTESIAN_POINT('Ctrl Pts',(3.60198873353787,31.8970336522008,54.2105312641291));
#91583=CARTESIAN_POINT('Ctrl Pts',(3.60578956781207,31.9240655091063,54.275486771423));
#91584=CARTESIAN_POINT('Ctrl Pts',(3.60959040208628,31.9477638020177,54.3418482392775));
#91585=CARTESIAN_POINT('Ctrl Pts',(3.61339123636048,31.9679921061031,54.4092338594539));
#91586=CARTESIAN_POINT('Ctrl Pts',(3.61719222217702,31.9882212167074,54.4766221663494));
#91587=CARTESIAN_POINT('Ctrl Pts',(3.62099320799356,32.0049799299312,54.5450342228552));
#91588=CARTESIAN_POINT('Ctrl Pts',(3.62479419381009,32.0181820637142,54.6140742037614));
#91589=CARTESIAN_POINT('Ctrl Pts',(3.62859963984799,32.0313996893832,54.6831951988078));
#91590=CARTESIAN_POINT('Ctrl Pts',(3.63240508588588,32.0410523192832,54.7529450939127));
#91591=CARTESIAN_POINT('Ctrl Pts',(3.63621053192378,32.0471053357224,54.8229200548993));
#91592=CARTESIAN_POINT('Ctrl Pts',(3.63944878144667,32.0522561583595,54.8824653438806));
#91593=CARTESIAN_POINT('Ctrl Pts',(3.64268703096955,32.0548013150988,54.9421733287147));
#91594=CARTESIAN_POINT('Ctrl Pts',(3.64592528049244,32.0547492155205,55.0017954993351));
#91595=CARTESIAN_POINT('Origin',(-1.54592528053767,30.,55.));
#91596=CARTESIAN_POINT('',(2.49394378209486,28.7479524050421,56.6292250864936));
#91597=CARTESIAN_POINT('',(2.55206205739628,28.7479524050421,56.6292250864936));
#91598=CARTESIAN_POINT('',(-1.54592528053767,28.7479524050421,56.6292250864936));
#91599=CARTESIAN_POINT('',(3.00407471949931,32.0547499051081,54.9993755336174));
#91600=CARTESIAN_POINT('Ctrl Pts',(2.55206205739628,28.7479524050421,56.6292250864936));
#91601=CARTESIAN_POINT('Ctrl Pts',(2.55268698953636,28.7388644085502,56.6222410274799));
#91602=CARTESIAN_POINT('Ctrl Pts',(2.55331192167644,28.729837617433,56.615183051692));
#91603=CARTESIAN_POINT('Ctrl Pts',(2.55393685381652,28.720873281012,56.6080523621048));
#91604=CARTESIAN_POINT('Ctrl Pts',(2.55780592716298,28.6653733748771,56.5639049111191));
#91605=CARTESIAN_POINT('Ctrl Pts',(2.56167500050944,28.6120529828087,56.516794349591));
#91606=CARTESIAN_POINT('Ctrl Pts',(2.5655440738559,28.5612455809797,56.466963968286));
#91607=CARTESIAN_POINT('Ctrl Pts',(2.56940738224989,28.5105138826151,56.4172078346765));
#91608=CARTESIAN_POINT('Ctrl Pts',(2.57327069064389,28.4622880860022,56.3647402628779));
#91609=CARTESIAN_POINT('Ctrl Pts',(2.57713399903788,28.4168691584292,56.3098451438882));
#91610=CARTESIAN_POINT('Ctrl Pts',(2.58099277552896,28.3715035101054,56.2550144203142));
#91611=CARTESIAN_POINT('Ctrl Pts',(2.58485155202003,28.3289384987099,56.1977621784438));
#91612=CARTESIAN_POINT('Ctrl Pts',(2.58871032851111,28.2894374808424,56.1384082881608));
#91613=CARTESIAN_POINT('Ctrl Pts',(2.59256667409745,28.2499613473421,56.0790917889143));
#91614=CARTESIAN_POINT('Ctrl Pts',(2.59642301968379,28.2135456463576,56.0176766714484));
#91615=CARTESIAN_POINT('Ctrl Pts',(2.60027936527013,28.1804118451149,55.9545137553235));
#91616=CARTESIAN_POINT('Ctrl Pts',(2.60413457151358,28.14728783313,55.8913695004463));
#91617=CARTESIAN_POINT('Ctrl Pts',(2.60798977775702,28.117444021457,55.8264789020229));
#91618=CARTESIAN_POINT('Ctrl Pts',(2.61184498400046,28.0910562597286,55.7602179680715));
#91619=CARTESIAN_POINT('Ctrl Pts',(2.6157003408498,28.0646674671469,55.6939544455979));
#91620=CARTESIAN_POINT('Ctrl Pts',(2.61955569769913,28.0417351702449,55.6263209334428));
#91621=CARTESIAN_POINT('Ctrl Pts',(2.62341105454847,28.0223866848822,55.5577124154696));
#91622=CARTESIAN_POINT('Ctrl Pts',(2.62727044701509,28.0030179463795,55.4890320811296));
#91623=CARTESIAN_POINT('Ctrl Pts',(2.63112983948172,27.9872406401299,55.4193751721457));
#91624=CARTESIAN_POINT('Ctrl Pts',(2.63498923194835,27.97513163587,55.3491499254552));
#91625=CARTESIAN_POINT('Ctrl Pts',(2.63885080954984,27.9630157756586,55.2788849181971));
#91626=CARTESIAN_POINT('Ctrl Pts',(2.64271238715133,27.9545724095138,55.2080514152575));
#91627=CARTESIAN_POINT('Ctrl Pts',(2.64657396475282,27.9498265305783,55.1370631525225));
#91628=CARTESIAN_POINT('Ctrl Pts',(2.65044229886574,27.9450723478902,55.065950683295));
#91629=CARTESIAN_POINT('Ctrl Pts',(2.65431063297867,27.9440285758852,54.994683399541));
#91630=CARTESIAN_POINT('Ctrl Pts',(2.65817896709159,27.9466680704179,54.9236747128482));
#91631=CARTESIAN_POINT('Ctrl Pts',(2.66047668627942,27.9482358815369,54.8814968613096));
#91632=CARTESIAN_POINT('Ctrl Pts',(2.66277440546725,27.9511022049546,54.8394101629236));
#91633=CARTESIAN_POINT('Ctrl Pts',(2.66507212465507,27.95525277321,54.7974997752229));
#91634=CARTESIAN_POINT('Ctrl Pts',(2.66894119800453,27.9622418139541,54.726927894648));
#91635=CARTESIAN_POINT('Ctrl Pts',(2.67281027135398,27.972902383093,54.6565800340402));
#91636=CARTESIAN_POINT('Ctrl Pts',(2.67667934470343,27.987210946956,54.5868683134322));
#91637=CARTESIAN_POINT('Ctrl Pts',(2.68054265310047,28.0014981909364,54.5172604638847));
#91638=CARTESIAN_POINT('Ctrl Pts',(2.68440596149751,28.0194225433629,54.4482873448617));
#91639=CARTESIAN_POINT('Ctrl Pts',(2.68826926989455,28.0409087288895,54.3803557843741));
#91640=CARTESIAN_POINT('Ctrl Pts',(2.69212804638874,28.062369709774,54.312503911864));
#91641=CARTESIAN_POINT('Ctrl Pts',(2.69598682288293,28.0873840785482,54.2456916318765));
#91642=CARTESIAN_POINT('Ctrl Pts',(2.69984559937711,28.1158259337503,54.1803136876999));
#91643=CARTESIAN_POINT('Ctrl Pts',(2.70370194496661,28.1442498715013,54.1149769295188));
#91644=CARTESIAN_POINT('Ctrl Pts',(2.70755829055611,28.1760968185179,54.0510731588551));
#91645=CARTESIAN_POINT('Ctrl Pts',(2.7114146361456,28.211192151875,53.9889787119025));
#91646=CARTESIAN_POINT('Ctrl Pts',(2.71526984239223,28.2462771164472,53.9269026105218));
#91647=CARTESIAN_POINT('Ctrl Pts',(2.71912504863886,28.2846083231466,53.866635194288));
#91648=CARTESIAN_POINT('Ctrl Pts',(2.72298025488549,28.3259652457834,53.8085281353825));
#91649=CARTESIAN_POINT('Ctrl Pts',(2.72683561173805,28.367323784053,53.7504188064904));
#91650=CARTESIAN_POINT('Ctrl Pts',(2.7306909685906,28.4117079894499,53.6944703969827));
#91651=CARTESIAN_POINT('Ctrl Pts',(2.73454632544316,28.4588550703749,53.641004095521));
#91652=CARTESIAN_POINT('Ctrl Pts',(2.73840571791303,28.5060515027824,53.5874818278957));
#91653=CARTESIAN_POINT('Ctrl Pts',(2.7422651103829,28.5560162619583,53.5364472199352));
#91654=CARTESIAN_POINT('Ctrl Pts',(2.74612450285277,28.6084480616532,53.4881862663068));
#91655=CARTESIAN_POINT('Ctrl Pts',(2.74998608045752,28.6609095475113,53.439897987991));
#91656=CARTESIAN_POINT('Ctrl Pts',(2.75384765806227,28.7158404802419,53.3943868002737));
#91657=CARTESIAN_POINT('Ctrl Pts',(2.75770923566703,28.7729068176881,53.3518980964687));
#91658=CARTESIAN_POINT('Ctrl Pts',(2.76157756978321,28.8300730027615,53.3093350511788));
#91659=CARTESIAN_POINT('Ctrl Pts',(2.76544590389939,28.8893816477604,53.2698053176901));
#91660=CARTESIAN_POINT('Ctrl Pts',(2.76931423801557,28.9504707055922,53.2335103106217));
#91661=CARTESIAN_POINT('Ctrl Pts',(2.77161195717492,28.9867564798794,53.211951745455));
#91662=CARTESIAN_POINT('Ctrl Pts',(2.77390967633428,29.0236699388517,53.1915335551998));
#91663=CARTESIAN_POINT('Ctrl Pts',(2.77620739549364,29.0611317998012,53.1722899395267));
#91664=CARTESIAN_POINT('Ctrl Pts',(2.78007646884162,29.1242129153393,53.1398860836347));
#91665=CARTESIAN_POINT('Ctrl Pts',(2.78394554218961,29.1890971270844,53.1106883390549));
#91666=CARTESIAN_POINT('Ctrl Pts',(2.78781461553759,29.2554254312286,53.0849004532299));
#91667=CARTESIAN_POINT('Ctrl Pts',(2.79167792393314,29.3216549056314,53.0591509915758));
#91668=CARTESIAN_POINT('Ctrl Pts',(2.7955412323287,29.3893237522684,53.0368014781914));
#91669=CARTESIAN_POINT('Ctrl Pts',(2.79940454072425,29.4580493505633,53.0180093198819));
#91670=CARTESIAN_POINT('Ctrl Pts',(2.80326331721693,29.5266943294242,52.9992392059518));
#91671=CARTESIAN_POINT('Ctrl Pts',(2.80712209370961,29.5963931312968,52.9840182856127));
#91672=CARTESIAN_POINT('Ctrl Pts',(2.8109808702023,29.6667458307197,52.9724548781452));
#91673=CARTESIAN_POINT('Ctrl Pts',(2.81483721579027,29.7370542102115,52.9608987552513));
#91674=CARTESIAN_POINT('Ctrl Pts',(2.81869356137825,29.8080151917614,52.952995652504));
#91675=CARTESIAN_POINT('Ctrl Pts',(2.82254990696622,29.8792178897378,52.948802972813));
#91676=CARTESIAN_POINT('Ctrl Pts',(2.82640511321133,29.9503995511435,52.9446115318337));
#91677=CARTESIAN_POINT('Ctrl Pts',(2.83026031945643,30.0218223025168,52.9441283661294));
#91678=CARTESIAN_POINT('Ctrl Pts',(2.83411552570153,30.093071083255,52.9473589364037));
#91679=CARTESIAN_POINT('Ctrl Pts',(2.83797088255255,30.164322647369,52.9505896328822));
#91680=CARTESIAN_POINT('Ctrl Pts',(2.84182623940357,30.2353997421671,52.9575343291708));
#91681=CARTESIAN_POINT('Ctrl Pts',(2.84568159625458,30.3058899943393,52.968146443795));
#91682=CARTESIAN_POINT('Ctrl Pts',(2.84954098872291,30.376454032595,52.9787696667121));
#91683=CARTESIAN_POINT('Ctrl Pts',(2.85340038119125,30.4464295206248,52.9930678987879));
#91684=CARTESIAN_POINT('Ctrl Pts',(2.85725977365958,30.5154127750105,53.0109431295571));
#91685=CARTESIAN_POINT('Ctrl Pts',(2.86112135126279,30.5844350867651,53.0288284810359));
#91686=CARTESIAN_POINT('Ctrl Pts',(2.864982928866,30.6524635830381,53.0502947165979));
#91687=CARTESIAN_POINT('Ctrl Pts',(2.86884450646921,30.7191109257491,53.075194285397));
#91688=CARTESIAN_POINT('Ctrl Pts',(2.87271284058386,30.7858748797468,53.1001374203855));
#91689=CARTESIAN_POINT('Ctrl Pts',(2.87658117469851,30.8512524096939,53.1285256886584));
#91690=CARTESIAN_POINT('Ctrl Pts',(2.88044950881317,30.9148779370555,53.1601641587389));
#91691=CARTESIAN_POINT('Ctrl Pts',(2.88274722798618,30.9526703277277,53.1789568268885));
#91692=CARTESIAN_POINT('Ctrl Pts',(2.88504494715919,30.9898450733868,53.1988953386927));
#91693=CARTESIAN_POINT('Ctrl Pts',(2.8873426663322,31.0263304413053,53.2199316339674));
#91694=CARTESIAN_POINT('Ctrl Pts',(2.89121173968022,31.0877672636396,53.2553541391823));
#91695=CARTESIAN_POINT('Ctrl Pts',(2.89508081302825,31.1474884268327,53.2940303836905));
#91696=CARTESIAN_POINT('Ctrl Pts',(2.89894988637627,31.2051280430109,53.3357692580508));
#91697=CARTESIAN_POINT('Ctrl Pts',(2.90281319477187,31.2626817756671,53.3774459411307));
#91698=CARTESIAN_POINT('Ctrl Pts',(2.90667650316746,31.3181597274908,53.4221759133552));
#91699=CARTESIAN_POINT('Ctrl Pts',(2.91053981156305,31.3712221345096,53.4697230903099));
#91700=CARTESIAN_POINT('Ctrl Pts',(2.91439858805577,31.4242222959994,53.517214491446));
#91701=CARTESIAN_POINT('Ctrl Pts',(2.91825736454848,31.47481218111,53.5675162103333));
#91702=CARTESIAN_POINT('Ctrl Pts',(2.9221161410412,31.5226838808883,53.6203510006589));
#91703=CARTESIAN_POINT('Ctrl Pts',(2.9259724866292,31.5705254230401,53.673152506771));
#91704=CARTESIAN_POINT('Ctrl Pts',(2.92982883221721,31.6156518517652,53.7284835592295));
#91705=CARTESIAN_POINT('Ctrl Pts',(2.93368517780522,31.6577920907689,53.7860300883942));
#91706=CARTESIAN_POINT('Ctrl Pts',(2.93754038405034,31.6999198795965,53.8435596156521));
#91707=CARTESIAN_POINT('Ctrl Pts',(2.94139559029547,31.7390629433785,53.9033029284216));
#91708=CARTESIAN_POINT('Ctrl Pts',(2.94525079654059,31.7749915803759,53.9649142779002));
#91709=CARTESIAN_POINT('Ctrl Pts',(2.94910615339163,31.8109216209466,54.0265280342627));
#91710=CARTESIAN_POINT('Ctrl Pts',(2.95296151024267,31.8436367426098,54.0900095514636));
#91711=CARTESIAN_POINT('Ctrl Pts',(2.95681686709371,31.872952424018,54.1549871126042));
#91712=CARTESIAN_POINT('Ctrl Pts',(2.96067625956206,31.9022987917871,54.2200326893865));
#91713=CARTESIAN_POINT('Ctrl Pts',(2.96453565203041,31.9282384157792,54.2865769924692));
#91714=CARTESIAN_POINT('Ctrl Pts',(2.96839504449875,31.9506346954674,54.3542277124723));
#91715=CARTESIAN_POINT('Ctrl Pts',(2.97225662210198,31.9730436556208,54.4219167353815));
#91716=CARTESIAN_POINT('Ctrl Pts',(2.9761181997052,31.9919051492532,54.4907129535365));
#91717=CARTESIAN_POINT('Ctrl Pts',(2.97997977730842,32.0071330619939,54.5602109210643));
#91718=CARTESIAN_POINT('Ctrl Pts',(2.98384811142308,32.022387618655,54.6298304875501));
#91719=CARTESIAN_POINT('Ctrl Pts',(2.98771644553774,32.0339958221669,54.7001537753634));
#91720=CARTESIAN_POINT('Ctrl Pts',(2.9915847796524,32.0419231662864,54.770767922221));
#91721=CARTESIAN_POINT('Ctrl Pts',(2.99388249882518,32.0466318625967,54.8127114240735));
#91722=CARTESIAN_POINT('Ctrl Pts',(2.99618021799797,32.0500428972691,54.8547574798927));
#91723=CARTESIAN_POINT('Ctrl Pts',(2.99847793717075,32.0521577425027,54.8968197577717));
#91724=CARTESIAN_POINT('Ctrl Pts',(3.00034353126794,32.0538748552077,54.9309715106294));
#91725=CARTESIAN_POINT('Ctrl Pts',(3.00220912536513,32.054739508502,54.9651664828388));
#91726=CARTESIAN_POINT('Ctrl Pts',(3.00407471946232,32.0547499051079,54.9993755329391));
#91727=CARTESIAN_POINT('Ctrl Pts',(3.00407471949931,32.0547499051081,54.9993755336174));
#91728=CARTESIAN_POINT('Ctrl Pts',(3.00791348792943,32.0547712978211,55.0697663124845));
#91729=CARTESIAN_POINT('Ctrl Pts',(3.01175225635954,32.0511712983844,55.1403032604116));
#91730=CARTESIAN_POINT('Ctrl Pts',(3.01559102478966,32.0439310014567,55.2105792577257));
#91731=CARTESIAN_POINT('Ctrl Pts',(3.01950861575714,32.0365420374276,55.2822982523253));
#91732=CARTESIAN_POINT('Ctrl Pts',(3.02342620672463,32.0253615175388,55.3537449447917));
#91733=CARTESIAN_POINT('Ctrl Pts',(3.02734379769211,32.0104254036403,55.4244846980724));
#91734=CARTESIAN_POINT('Ctrl Pts',(3.03117271153814,31.9958273780204,55.4936232127998));
#91735=CARTESIAN_POINT('Ctrl Pts',(3.03500162538417,31.9776420962988,55.5620859435654));
#91736=CARTESIAN_POINT('Ctrl Pts',(3.03883053923019,31.9559553954488,55.6294728377895));
#91737=CARTESIAN_POINT('Ctrl Pts',(3.04265730106963,31.934280883414,55.6968218578157));
#91738=CARTESIAN_POINT('Ctrl Pts',(3.04648406290907,31.9091090062367,55.7630957710834));
#91739=CARTESIAN_POINT('Ctrl Pts',(3.05031082474851,31.8805758631093,55.8279081987701));
#91740=CARTESIAN_POINT('Ctrl Pts',(3.05413676563536,31.8520488411774,55.8927067222914));
#91741=CARTESIAN_POINT('Ctrl Pts',(3.05796270652221,31.8201621840695,55.9560439306865));
#91742=CARTESIAN_POINT('Ctrl Pts',(3.06178864740907,31.7850999946472,56.0175537192751));
#91743=CARTESIAN_POINT('Ctrl Pts',(3.06577402745909,31.7485766519281,56.081626816997));
#91744=CARTESIAN_POINT('Ctrl Pts',(3.06975940750911,31.7086075443476,56.1437163194024));
#91745=CARTESIAN_POINT('Ctrl Pts',(3.07374478755913,31.6654523582068,56.203439240279));
#91746=CARTESIAN_POINT('Ctrl Pts',(3.07757550004278,31.623971970337,56.2608443900239));
#91747=CARTESIAN_POINT('Ctrl Pts',(3.08140621252642,31.579548618677,56.3160629059919));
#91748=CARTESIAN_POINT('Ctrl Pts',(3.08523692501007,31.5324542627966,56.368788330947));
#91749=CARTESIAN_POINT('Ctrl Pts',(3.08907026922274,31.4853275527304,56.4215499786756));
#91750=CARTESIAN_POINT('Ctrl Pts',(3.0929036134354,31.4355265377711,56.4718147802392));
#91751=CARTESIAN_POINT('Ctrl Pts',(3.09673695764807,31.3833590795809,56.5193140621482));
#91752=CARTESIAN_POINT('Ctrl Pts',(3.10057644985484,31.3311079541779,56.5668895243553));
#91753=CARTESIAN_POINT('Ctrl Pts',(3.10441594206161,31.2764832012901,56.6116903146892));
#91754=CARTESIAN_POINT('Ctrl Pts',(3.10825543426838,31.2198237246292,56.6534895352955));
#91755=CARTESIAN_POINT('Ctrl Pts',(3.10870802551535,31.213144824969,56.6584167393001));
#91756=CARTESIAN_POINT('Ctrl Pts',(3.10916061676233,31.2064376818367,56.6633022876482));
#91757=CARTESIAN_POINT('Ctrl Pts',(3.10961320800931,31.1997028730535,56.6681458506039));
#91758=CARTESIAN_POINT('Ctrl Pts',(3.11348228135748,31.1421289156642,56.7095520873955));
#91759=CARTESIAN_POINT('Ctrl Pts',(3.11735135470566,31.0822960432207,56.7480552898336));
#91760=CARTESIAN_POINT('Ctrl Pts',(3.12122042805383,31.0205290485874,56.783400690672));
#91761=CARTESIAN_POINT('Ctrl Pts',(3.12508373644957,30.9588540873052,56.8186934265603));
#91762=CARTESIAN_POINT('Ctrl Pts',(3.12894704484532,30.8952511424399,56.8508374611336));
#91763=CARTESIAN_POINT('Ctrl Pts',(3.13281035324106,30.8300752390306,56.8796203499772));
#91764=CARTESIAN_POINT('Ctrl Pts',(3.13666912973393,30.7649757910408,56.9083694746882));
#91765=CARTESIAN_POINT('Ctrl Pts',(3.1405279062268,30.6983074918813,56.933765090178));
#91766=CARTESIAN_POINT('Ctrl Pts',(3.14438668271967,30.6304497644057,56.9556407280124));
#91767=CARTESIAN_POINT('Ctrl Pts',(3.14824302830784,30.5626347851093,56.9775025849006));
#91768=CARTESIAN_POINT('Ctrl Pts',(3.15209937389601,30.4936323253602,56.9958487148634));
#91769=CARTESIAN_POINT('Ctrl Pts',(3.15595571948418,30.4238402027613,57.0105613755922));
#91770=CARTESIAN_POINT('Ctrl Pts',(3.15981092572947,30.3540686999839,57.0252696895204));
#91771=CARTESIAN_POINT('Ctrl Pts',(3.16366613197476,30.2835084726075,57.0363465652489));
#91772=CARTESIAN_POINT('Ctrl Pts',(3.16752133822006,30.2125691751471,57.0437250079884));
#91773=CARTESIAN_POINT('Ctrl Pts',(3.17137669507126,30.141627106401,57.0511037389711));
#91774=CARTESIAN_POINT('Ctrl Pts',(3.17523205192246,30.0703064215777,57.0547837020508));
#91775=CARTESIAN_POINT('Ctrl Pts',(3.17908740877366,29.9990218406574,57.0547497671747));
#91776=CARTESIAN_POINT('Ctrl Pts',(3.18294680124218,29.9276626421854,57.054715796777));
#91777=CARTESIAN_POINT('Ctrl Pts',(3.1868061937107,29.856340109839,57.0509601682432));
#91778=CARTESIAN_POINT('Ctrl Pts',(3.19066558617921,29.7854680019323,57.0435199006384));
#91779=CARTESIAN_POINT('Ctrl Pts',(3.19452716378261,29.7145557672138,57.0360754204565));
#91780=CARTESIAN_POINT('Ctrl Pts',(3.198388741386,29.64409494467,57.0249422240913));
#91781=CARTESIAN_POINT('Ctrl Pts',(3.2022503189894,29.5744904799988,57.0102087480877));
#91782=CARTESIAN_POINT('Ctrl Pts',(3.20611865310423,29.5047642300343,56.995449493268));
#91783=CARTESIAN_POINT('Ctrl Pts',(3.20998698721906,29.4358977989596,56.9770775072826));
#91784=CARTESIAN_POINT('Ctrl Pts',(3.21385532133389,29.3682816450929,56.9552313117822));
#91785=CARTESIAN_POINT('Ctrl Pts',(3.21615304050522,29.3281188958527,56.9422550742774));
#91786=CARTESIAN_POINT('Ctrl Pts',(3.21845075967655,29.2883969108282,56.9280540225236));
#91787=CARTESIAN_POINT('Ctrl Pts',(3.22074847884788,29.2491937605716,56.9126650395026));
#91788=CARTESIAN_POINT('Ctrl Pts',(3.22461723637989,29.1831859190886,56.8867540209954));
#91789=CARTESIAN_POINT('Ctrl Pts',(3.2284859939119,29.1183916904716,56.8573712555023));
#91790=CARTESIAN_POINT('Ctrl Pts',(3.23235475144391,29.0552011768238,56.824651404029));
#91791=CARTESIAN_POINT('Ctrl Pts',(3.23621738593897,28.9921106740573,56.791983337879));
#91792=CARTESIAN_POINT('Ctrl Pts',(3.24008002043403,28.9306192735358,56.7559888953893));
#91793=CARTESIAN_POINT('Ctrl Pts',(3.24394265492909,28.8710978213459,56.7168510225206));
#91794=CARTESIAN_POINT('Ctrl Pts',(3.24667302123064,28.8290241103887,56.6891857776388));
#91795=CARTESIAN_POINT('Ctrl Pts',(3.24940338753219,28.7879343494465,56.6599509191292));
#91796=CARTESIAN_POINT('Ctrl Pts',(3.25213375383374,28.7479524050421,56.6292250864936));
#91797=CARTESIAN_POINT('',(2.94592528057331,32.0547499982312,55.000085258463));
#91798=CARTESIAN_POINT('Ctrl Pts',(2.94592528057331,32.0547499982312,55.000085258463));
#91799=CARTESIAN_POINT('Ctrl Pts',(2.94997591064043,32.0547468813369,55.0752031797358));
#91800=CARTESIAN_POINT('Ctrl Pts',(2.95402654070755,32.0506202133317,55.1502363805521));
#91801=CARTESIAN_POINT('Ctrl Pts',(2.95807717077467,32.0424234247646,55.2247312093873));
#91802=CARTESIAN_POINT('Ctrl Pts',(2.96213971867067,32.0342025194745,55.2994452181052));
#91803=CARTESIAN_POINT('Ctrl Pts',(2.96620226656668,32.0218876070698,55.3736172816528));
#91804=CARTESIAN_POINT('Ctrl Pts',(2.97026481446268,32.0055836153857,55.446801884728));
#91805=CARTESIAN_POINT('Ctrl Pts',(2.97433371205498,31.9892541408277,55.5201008741474));
#91806=CARTESIAN_POINT('Ctrl Pts',(2.97840260964727,31.9689232661609,55.5924089327683));
#91807=CARTESIAN_POINT('Ctrl Pts',(2.98247150723956,31.9447455641139,55.6632965048598));
#91808=CARTESIAN_POINT('Ctrl Pts',(2.98655160384017,31.9205013166993,55.7343791839775));
#91809=CARTESIAN_POINT('Ctrl Pts',(2.99063170044077,31.8923892324745,55.8040331824788));
#91810=CARTESIAN_POINT('Ctrl Pts',(2.99471179704137,31.8606118986411,55.8718491412711));
#91811=CARTESIAN_POINT('Ctrl Pts',(2.99669196890795,31.8451895720123,55.904761904583));
#91812=CARTESIAN_POINT('Ctrl Pts',(2.99867214077452,31.8289046141135,55.9372421261628));
#91813=CARTESIAN_POINT('Ctrl Pts',(3.0006523126411,31.8117839056032,55.9692453981822));
#91814=CARTESIAN_POINT('Ctrl Pts',(3.00452138598909,31.7783316189031,56.0317768425022));
#91815=CARTESIAN_POINT('Ctrl Pts',(3.00839045933708,31.7415727162695,56.0926968909224));
#91816=CARTESIAN_POINT('Ctrl Pts',(3.01225953268507,31.7016865835042,56.1516337673158));
#91817=CARTESIAN_POINT('Ctrl Pts',(3.01612284108062,31.6618598814184,56.2104828272583));
#91818=CARTESIAN_POINT('Ctrl Pts',(3.01998614947618,31.6189154684274,56.2673541816167));
#91819=CARTESIAN_POINT('Ctrl Pts',(3.02384945787173,31.5730785127529,56.3219007357647));
#91820=CARTESIAN_POINT('Ctrl Pts',(3.02770823436442,31.5272953267001,56.376383303386));
#91821=CARTESIAN_POINT('Ctrl Pts',(3.0315670108571,31.4786266488835,56.4285461177085));
#91822=CARTESIAN_POINT('Ctrl Pts',(3.03542578734978,31.4273398009177,56.4780726150012));
#91823=CARTESIAN_POINT('Ctrl Pts',(3.03928213293776,31.3760852620116,56.5275679121982));
#91824=CARTESIAN_POINT('Ctrl Pts',(3.04313847852574,31.3222161738864,56.5744298507));
#91825=CARTESIAN_POINT('Ctrl Pts',(3.04699482411372,31.2660378333485,56.6183775106662));
#91826=CARTESIAN_POINT('Ctrl Pts',(3.05085003035883,31.209876090491,56.6623121864608));
#91827=CARTESIAN_POINT('Ctrl Pts',(3.05470523660393,31.1514068321055,56.7033339939137));
#91828=CARTESIAN_POINT('Ctrl Pts',(3.05856044284904,31.0909683329546,56.7412023601495));
#91829=CARTESIAN_POINT('Ctrl Pts',(3.06241579970006,31.030527472738,56.7790722057355));
#91830=CARTESIAN_POINT('Ctrl Pts',(3.06627115655108,30.9681176318487,56.8137881094637));
#91831=CARTESIAN_POINT('Ctrl Pts',(3.0701265134021,30.9041044757656,56.845153830823));
#91832=CARTESIAN_POINT('Ctrl Pts',(3.07398590587044,30.8400243135373,56.8765523844344));
#91833=CARTESIAN_POINT('Ctrl Pts',(3.07784529833877,30.774337923019,56.9045935410831));
#91834=CARTESIAN_POINT('Ctrl Pts',(3.08170469080711,30.70743307459,56.9291283024921));
#91835=CARTESIAN_POINT('Ctrl Pts',(3.08556626841032,30.640490345557,56.9536769551453));
#91836=CARTESIAN_POINT('Ctrl Pts',(3.08942784601353,30.5723282496859,56.974715117157));
#91837=CARTESIAN_POINT('Ctrl Pts',(3.09328942361675,30.5033492915548,56.9921438334597));
#91838=CARTESIAN_POINT('Ctrl Pts',(3.0971577577314,30.4342496425641,57.009603044377));
#91839=CARTESIAN_POINT('Ctrl Pts',(3.10102609184606,30.36433075448,57.0234401064428));
#91840=CARTESIAN_POINT('Ctrl Pts',(3.10489442596071,30.2940041845394,57.0336074109752));
#91841=CARTESIAN_POINT('Ctrl Pts',(3.1071921451337,30.2522314980719,57.0396466024901));
#91842=CARTESIAN_POINT('Ctrl Pts',(3.10948986430668,30.2103150725664,57.0443920466834));
#91843=CARTESIAN_POINT('Ctrl Pts',(3.11178758347967,30.1683412431117,57.0478424715704));
#91844=CARTESIAN_POINT('Ctrl Pts',(3.11565566451447,30.0976806612701,57.053651067862));
#91845=CARTESIAN_POINT('Ctrl Pts',(3.11952374554928,30.0265807194194,57.0558095440457));
#91846=CARTESIAN_POINT('Ctrl Pts',(3.12339182658408,29.95545073906,57.0542670045176));
#91847=CARTESIAN_POINT('Ctrl Pts',(3.12725460112043,29.8844183396786,57.0527265811509));
#91848=CARTESIAN_POINT('Ctrl Pts',(3.13111737565678,29.8133564647233,57.0474952245098));
#91849=CARTESIAN_POINT('Ctrl Pts',(3.13498015019314,29.7426786744688,57.0385738392138));
#91850=CARTESIAN_POINT('Ctrl Pts',(3.13883891816641,29.6720741929262,57.0296617073942));
#91851=CARTESIAN_POINT('Ctrl Pts',(3.14269768613968,29.6018534849097,57.0170672030055));
#91852=CARTESIAN_POINT('Ctrl Pts',(3.14655645411294,29.5324274942923,57.0008432008546));
#91853=CARTESIAN_POINT('Ctrl Pts',(3.15049843891761,29.4615042872069,56.984269317586));
#91854=CARTESIAN_POINT('Ctrl Pts',(3.15444042372228,29.3914109959895,56.9639075844468));
#91855=CARTESIAN_POINT('Ctrl Pts',(3.15838240852694,29.322576421289,56.9398698042669));
#91856=CARTESIAN_POINT('Ctrl Pts',(3.16223780698054,29.2552538094563,56.9163600179216));
#91857=CARTESIAN_POINT('Ctrl Pts',(3.16609320543414,29.1891356459562,56.8893342362753));
#91858=CARTESIAN_POINT('Ctrl Pts',(3.16994860388774,29.1246071532437,56.8589472629281));
#91859=CARTESIAN_POINT('Ctrl Pts',(3.17393388186794,29.0579048436906,56.8275366221803));
#91860=CARTESIAN_POINT('Ctrl Pts',(3.17791915984814,28.9929017427155,56.7925344658481));
#91861=CARTESIAN_POINT('Ctrl Pts',(3.18190443782834,28.9299978980659,56.7541644918184));
#91862=CARTESIAN_POINT('Ctrl Pts',(3.18588971580853,28.8670940534163,56.7157945177888));
#91863=CARTESIAN_POINT('Ctrl Pts',(3.18987499378873,28.8062899352195,56.6740570529051));
#91864=CARTESIAN_POINT('Ctrl Pts',(3.19386027176893,28.7479524050421,56.6292250864936));
#91865=CARTESIAN_POINT('Ctrl Pts',(2.49394378209486,28.7479524050421,56.6292250864936));
#91866=CARTESIAN_POINT('Ctrl Pts',(2.49779890937301,28.6914083389449,56.5857713841458));
#91867=CARTESIAN_POINT('Ctrl Pts',(2.50165403665116,28.6371162652407,56.5393607504666));
#91868=CARTESIAN_POINT('Ctrl Pts',(2.50550916392931,28.5853921214667,56.4902624307455));
#91869=CARTESIAN_POINT('Ctrl Pts',(2.50936473451369,28.5336620298643,56.441158465143));
#91870=CARTESIAN_POINT('Ctrl Pts',(2.51322030509808,28.48450080496,56.3893665362161));
#91871=CARTESIAN_POINT('Ctrl Pts',(2.51707587568247,28.438188038051,56.3351932287175));
#91872=CARTESIAN_POINT('Ctrl Pts',(2.52093566210309,28.3918246308965,56.2809606859415));
#91873=CARTESIAN_POINT('Ctrl Pts',(2.52479544852371,28.3483162124722,56.2243419389469));
#91874=CARTESIAN_POINT('Ctrl Pts',(2.52865523494433,28.3079019058973,56.1656764570129));
#91875=CARTESIAN_POINT('Ctrl Pts',(2.5325174695175,28.2674619656793,56.1069737652352));
#91876=CARTESIAN_POINT('Ctrl Pts',(2.53637970409067,28.2301202966293,56.0462221690235));
#91877=CARTESIAN_POINT('Ctrl Pts',(2.54024193866385,28.1960710714782,55.9837875702315));
#91878=CARTESIAN_POINT('Ctrl Pts',(2.54411066705154,28.161964597253,55.9212479962764));
#91879=CARTESIAN_POINT('Ctrl Pts',(2.54797939543923,28.1311618222452,55.8570202108948));
#91880=CARTESIAN_POINT('Ctrl Pts',(2.55184812382693,28.103809277651,55.7914911919774));
#91881=CARTESIAN_POINT('Ctrl Pts',(2.55326915898024,28.0937623259125,55.7674215158171));
#91882=CARTESIAN_POINT('Ctrl Pts',(2.55469019413355,28.0841803910862,55.743176430814));
#91883=CARTESIAN_POINT('Ctrl Pts',(2.55611122928687,28.0750690305662,55.7187755737466));
#91884=CARTESIAN_POINT('Ctrl Pts',(2.55998030264427,28.0502613949809,55.6523390005508));
#91885=CARTESIAN_POINT('Ctrl Pts',(2.56384937600167,28.0288486677511,55.5844864813534));
#91886=CARTESIAN_POINT('Ctrl Pts',(2.56771844935906,28.0109912325788,55.5155983762792));
#91887=CARTESIAN_POINT('Ctrl Pts',(2.57158175776416,27.9931604051373,55.4468129150691));
#91888=CARTESIAN_POINT('Ctrl Pts',(2.57544506616926,27.9788744754376,55.3769953972689));
#91889=CARTESIAN_POINT('Ctrl Pts',(2.57930837457436,27.9682450435054,55.3065442207244));
#91890=CARTESIAN_POINT('Ctrl Pts',(2.58316715107673,27.9576280805626,55.2361756878225));
#91891=CARTESIAN_POINT('Ctrl Pts',(2.5870259275791,27.9506591675067,55.1651754506821));
#91892=CARTESIAN_POINT('Ctrl Pts',(2.59088470408147,27.9473991304798,55.0939533551561));
#91893=CARTESIAN_POINT('Ctrl Pts',(2.59474104967922,27.9441411471711,55.022776127251));
#91894=CARTESIAN_POINT('Ctrl Pts',(2.59859739527697,27.9445874265286,54.9513778023797));
#91895=CARTESIAN_POINT('Ctrl Pts',(2.60245374087473,27.9487469461884,54.880173159399));
#91896=CARTESIAN_POINT('Ctrl Pts',(2.60630894712967,27.9529052369337,54.8089895535622));
#91897=CARTESIAN_POINT('Ctrl Pts',(2.61016415338462,27.9607745616937,54.7380000007084));
#91898=CARTESIAN_POINT('Ctrl Pts',(2.61401935963957,27.9723118239717,54.6676173541004));
#91899=CARTESIAN_POINT('Ctrl Pts',(2.61787471650049,27.98384953696,54.5972319579517));
#91900=CARTESIAN_POINT('Ctrl Pts',(2.6217300733614,27.9990553911943,54.5274539941519));
#91901=CARTESIAN_POINT('Ctrl Pts',(2.62558543022232,28.0178349189445,54.458687563468));
#91902=CARTESIAN_POINT('Ctrl Pts',(2.62944482270057,28.0366341042751,54.3898491511208));
#91903=CARTESIAN_POINT('Ctrl Pts',(2.63330421517883,28.0590143022865,54.3220248551342));
#91904=CARTESIAN_POINT('Ctrl Pts',(2.63716360765709,28.0848309846897,54.2556041340152));
#91905=CARTESIAN_POINT('Ctrl Pts',(2.64102518527025,28.1106622841431,54.1891458063981));
#91906=CARTESIAN_POINT('Ctrl Pts',(2.64488676288341,28.1399337418262,54.1240930788353));
#91907=CARTESIAN_POINT('Ctrl Pts',(2.64874834049657,28.1724535394593,54.0608133853887));
#91908=CARTESIAN_POINT('Ctrl Pts',(2.6526166746211,28.2050302362161,53.9974229729533));
#91909=CARTESIAN_POINT('Ctrl Pts',(2.65648500874563,28.2408663759584,53.9358122083899));
#91910=CARTESIAN_POINT('Ctrl Pts',(2.66035334287016,28.2797256282689,53.8763213766983));
#91911=CARTESIAN_POINT('Ctrl Pts',(2.66265106195524,28.3028073070463,53.8409849204964));
#91912=CARTESIAN_POINT('Ctrl Pts',(2.66494878104033,28.3269547719297,53.8063958214775));
#91913=CARTESIAN_POINT('Ctrl Pts',(2.66724650012542,28.3521119068325,53.7726197024163));
#91914=CARTESIAN_POINT('Ctrl Pts',(2.67111557347256,28.3944733951337,53.7157449160783));
#91915=CARTESIAN_POINT('Ctrl Pts',(2.67498464681969,28.4398657576993,53.6609543818507));
#91916=CARTESIAN_POINT('Ctrl Pts',(2.67885372016682,28.4880564237835,53.6085891387381));
#91917=CARTESIAN_POINT('Ctrl Pts',(2.68271702856152,28.5361752853624,53.5563019202862));
#91918=CARTESIAN_POINT('Ctrl Pts',(2.68658033695623,28.5870838478484,53.5064331743903));
#91919=CARTESIAN_POINT('Ctrl Pts',(2.69044364535093,28.6405079277061,53.4592927377759));
#91920=CARTESIAN_POINT('Ctrl Pts',(2.69430242184279,28.6938693377704,53.4122075998477));
#91921=CARTESIAN_POINT('Ctrl Pts',(2.69816119833464,28.7497400413137,53.3678447338221));
#91922=CARTESIAN_POINT('Ctrl Pts',(2.7020199748265,28.8078086989003,53.3264775280618));
#91923=CARTESIAN_POINT('Ctrl Pts',(2.70587632041366,28.8658407751059,53.2851363823065));
#91924=CARTESIAN_POINT('Ctrl Pts',(2.70973266600082,28.9260676635307,53.2467874338958));
#91925=CARTESIAN_POINT('Ctrl Pts',(2.71358901158797,28.9881457595397,53.211663186488));
#91926=CARTESIAN_POINT('Ctrl Pts',(2.71744421783227,29.0502055148076,53.1765493164075));
#91927=CARTESIAN_POINT('Ctrl Pts',(2.72129942407657,29.1141149692776,53.1446584949986));
#91928=CARTESIAN_POINT('Ctrl Pts',(2.72515463032086,29.1795038929504,53.1161784317997));
#91929=CARTESIAN_POINT('Ctrl Pts',(2.72900998717109,29.2448953710806,53.0876972560102));
#91930=CARTESIAN_POINT('Ctrl Pts',(2.73286534402132,29.3117659869061,53.0626272949309));
#91931=CARTESIAN_POINT('Ctrl Pts',(2.73672070087155,29.3797250018685,53.0411083518497));
#91932=CARTESIAN_POINT('Ctrl Pts',(2.74058009333911,29.4477551533273,53.019566883689));
#91933=CARTESIAN_POINT('Ctrl Pts',(2.74443948580667,29.516875514126,53.0015840005375));
#91934=CARTESIAN_POINT('Ctrl Pts',(2.74829887827424,29.5866804962575,52.9872495061916));
#91935=CARTESIAN_POINT('Ctrl Pts',(2.7521604558767,29.656525001009,52.9729068958522));
#91936=CARTESIAN_POINT('Ctrl Pts',(2.75602203347916,29.7270544182035,52.962216859258));
#91937=CARTESIAN_POINT('Ctrl Pts',(2.75988361108161,29.7978560151366,52.9552175245558));
#91938=CARTESIAN_POINT('Ctrl Pts',(2.76375194519554,29.8687814919579,52.9482059432824));
#91939=CARTESIAN_POINT('Ctrl Pts',(2.76762027930946,29.9399796139013,52.9448979791088));
#91940=CARTESIAN_POINT('Ctrl Pts',(2.77148861342339,30.0110363155874,52.9452796389196));
#91941=CARTESIAN_POINT('Ctrl Pts',(2.77378633260359,30.0532426869962,52.9455063378143));
#91942=CARTESIAN_POINT('Ctrl Pts',(2.77608405178379,30.0953992151863,52.9470337898436));
#91943=CARTESIAN_POINT('Ctrl Pts',(2.77838177096398,30.1374203322452,52.9498504408737));
#91944=CARTESIAN_POINT('Ctrl Pts',(2.78225084431045,30.2081786674685,52.9545933309191));
#91945=CARTESIAN_POINT('Ctrl Pts',(2.78611991765693,30.2788297690568,52.9630130139421));
#91946=CARTESIAN_POINT('Ctrl Pts',(2.7899889910034,30.3489609772674,52.9750990644368));
#91947=CARTESIAN_POINT('Ctrl Pts',(2.7938522993974,30.4189876893763,52.9871671066127));
#91948=CARTESIAN_POINT('Ctrl Pts',(2.7977156077914,30.4884955709285,53.0028905906901));
#91949=CARTESIAN_POINT('Ctrl Pts',(2.80157891618539,30.5570756072926,53.0222072074508));
#91950=CARTESIAN_POINT('Ctrl Pts',(2.80543769267648,30.6255751949752,53.0415011646092));
#91951=CARTESIAN_POINT('Ctrl Pts',(2.80929646916757,30.6931486341189,53.0643797510298));
#91952=CARTESIAN_POINT('Ctrl Pts',(2.81315524565865,30.7593973799234,53.0907296729207));
#91953=CARTESIAN_POINT('Ctrl Pts',(2.817011591245,30.8256043911547,53.1170629952106));
#91954=CARTESIAN_POINT('Ctrl Pts',(2.82086793683135,30.8904879143848,53.1468631352238));
#91955=CARTESIAN_POINT('Ctrl Pts',(2.8247242824177,30.9536662543494,53.1799675173736));
#91956=CARTESIAN_POINT('Ctrl Pts',(2.82857948866116,31.0168259285095,53.2130621189575));
#91957=CARTESIAN_POINT('Ctrl Pts',(2.83243469490461,31.0782809895073,53.2494587992554));
#91958=CARTESIAN_POINT('Ctrl Pts',(2.83628990114807,31.1376729349282,53.2889483188308));
#91959=CARTESIAN_POINT('Ctrl Pts',(2.84014525799743,31.1970672005305,53.3284393810876));
#91960=CARTESIAN_POINT('Ctrl Pts',(2.8440006148468,31.2543977872325,53.3710232516974));
#91961=CARTESIAN_POINT('Ctrl Pts',(2.84785597169616,31.3093353176415,53.4164474784597));
#91962=CARTESIAN_POINT('Ctrl Pts',(2.8517153641628,31.3643303542309,53.4619192532963));
#91963=CARTESIAN_POINT('Ctrl Pts',(2.85557475662944,31.4169269589407,53.5102370091911));
#91964=CARTESIAN_POINT('Ctrl Pts',(2.85943414909608,31.4668297073214,53.5611087003462));
#91965=CARTESIAN_POINT('Ctrl Pts',(2.86329572669758,31.5167607099511,53.6120091943524));
#91966=CARTESIAN_POINT('Ctrl Pts',(2.86715730429908,31.5639944981892,53.6654661379542));
#91967=CARTESIAN_POINT('Ctrl Pts',(2.87101888190058,31.6082751875232,53.7211534557667));
#91968=CARTESIAN_POINT('Ctrl Pts',(2.87488721601352,31.6526333537369,53.7769382083685));
#91969=CARTESIAN_POINT('Ctrl Pts',(2.87875555012646,31.6940278228252,53.8349607309145));
#91970=CARTESIAN_POINT('Ctrl Pts',(2.8826238842394,31.7322457768227,53.8948655596807));
#91971=CARTESIAN_POINT('Ctrl Pts',(2.88492160342711,31.7549465373184,53.930447924201));
#91972=CARTESIAN_POINT('Ctrl Pts',(2.88721932261482,31.7765274452677,53.9666938950511));
#91973=CARTESIAN_POINT('Ctrl Pts',(2.88951704180254,31.7969517988388,54.0035253163527));
#91974=CARTESIAN_POINT('Ctrl Pts',(2.89357123056584,31.8329893552072,54.068512167303));
#91975=CARTESIAN_POINT('Ctrl Pts',(2.89762541932915,31.865553742363,54.1355570099445));
#91976=CARTESIAN_POINT('Ctrl Pts',(2.90167960809246,31.8944168444321,54.2042724197114));
#91977=CARTESIAN_POINT('Ctrl Pts',(2.90572241802795,31.9231989368867,54.2727949670188));
#91978=CARTESIAN_POINT('Ctrl Pts',(2.90976522796344,31.9483002686522,54.3429783611878));
#91979=CARTESIAN_POINT('Ctrl Pts',(2.91380803789893,31.9695390126303,54.4144117144042));
#91980=CARTESIAN_POINT('Ctrl Pts',(2.91784402707856,31.9907419240342,54.4857245500916));
#91981=CARTESIAN_POINT('Ctrl Pts',(2.92188001625818,32.0080950853209,54.5582827532557));
#91982=CARTESIAN_POINT('Ctrl Pts',(2.92591600543781,32.0214649404899,54.631656333202));
#91983=CARTESIAN_POINT('Ctrl Pts',(2.92994364806252,32.0348071463701,54.7048781742343));
#91984=CARTESIAN_POINT('Ctrl Pts',(2.93397129068723,32.0441823724226,54.778911624555));
#91985=CARTESIAN_POINT('Ctrl Pts',(2.93799893331194,32.0495074524647,54.853314060689));
#91986=CARTESIAN_POINT('Ctrl Pts',(2.94064104905385,32.0530006814121,54.902121729607));
#91987=CARTESIAN_POINT('Ctrl Pts',(2.94328316479577,32.0547520312807,54.9510878823305));
#91988=CARTESIAN_POINT('Ctrl Pts',(2.94592528053768,32.0547499982312,55.0000852578023));
#91989=CARTESIAN_POINT('Origin',(-1.54592528053767,30.,55.));
#91990=CARTESIAN_POINT('',(1.79398372125809,28.7479524050421,56.6292250864936));
#91991=CARTESIAN_POINT('',(1.85198267906976,28.7489102161968,56.6279533026672));
#91992=CARTESIAN_POINT('',(-1.54592528053767,28.7479524050421,56.6292250864936));
#91993=CARTESIAN_POINT('',(2.30407472893336,32.05474914222,55.0018775106353));
#91994=CARTESIAN_POINT('Ctrl Pts',(1.85198267906975,28.748910216197,56.6279533026674));
#91995=CARTESIAN_POINT('Ctrl Pts',(1.86369686230822,28.5761851337391,56.4975417835351));
#91996=CARTESIAN_POINT('Ctrl Pts',(1.91245613582621,27.9428459579379,55.8463605828614));
#91997=CARTESIAN_POINT('Ctrl Pts',(1.99826049962372,27.759896125161,54.0618362182718));
#91998=CARTESIAN_POINT('Ctrl Pts',(2.10939577046228,29.5732403634016,52.6091648250566));
#91999=CARTESIAN_POINT('Ctrl Pts',(2.21133384374181,31.5947942490703,53.2838822194413));
#92000=CARTESIAN_POINT('Ctrl Pts',(2.27622682674183,32.0498098766772,54.4882110177461));
#92001=CARTESIAN_POINT('Ctrl Pts',(2.30407471946232,32.0544624073133,55.0018770739377));
#92002=CARTESIAN_POINT('Ctrl Pts',(2.30407472893336,32.05474914222,55.0018775106353));
#92003=CARTESIAN_POINT('Ctrl Pts',(2.30909837625834,32.0546644608409,55.0945528797447));
#92004=CARTESIAN_POINT('Ctrl Pts',(2.31412202358331,32.0483061176117,55.1869490612125));
#92005=CARTESIAN_POINT('Ctrl Pts',(2.31914567090828,32.0358091112648,55.2783501841048));
#92006=CARTESIAN_POINT('Ctrl Pts',(2.32331921798532,32.0254268449677,55.3542844335871));
#92007=CARTESIAN_POINT('Ctrl Pts',(2.32749276506236,32.0108086115702,55.4295325551524));
#92008=CARTESIAN_POINT('Ctrl Pts',(2.3316663121394,31.992056109336,55.5036963567041));
#92009=CARTESIAN_POINT('Ctrl Pts',(2.33553538549684,31.9746716626195,55.5724496697432));
#92010=CARTESIAN_POINT('Ctrl Pts',(2.33940445885429,31.9536895845222,55.6404365923658));
#92011=CARTESIAN_POINT('Ctrl Pts',(2.34327353221173,31.9291943063137,55.7072530600759));
#92012=CARTESIAN_POINT('Ctrl Pts',(2.34713684061688,31.9047355262786,55.7739699706794));
#92013=CARTESIAN_POINT('Ctrl Pts',(2.35100014902202,31.8767741027081,55.8395194357512));
#92014=CARTESIAN_POINT('Ctrl Pts',(2.35486345742717,31.8454448503109,55.9035103026313));
#92015=CARTESIAN_POINT('Ctrl Pts',(2.35872223392959,31.814152349089,55.9674261042166));
#92016=CARTESIAN_POINT('Ctrl Pts',(2.36258101043202,31.7795000789876,56.0297865051145));
#92017=CARTESIAN_POINT('Ctrl Pts',(2.36643978693444,31.7416711269176,56.0902198164414));
#92018=CARTESIAN_POINT('Ctrl Pts',(2.37029613253224,31.7038660058662,56.1506150567333));
#92019=CARTESIAN_POINT('Ctrl Pts',(2.37415247813005,31.6628884303501,56.2090852052249));
#92020=CARTESIAN_POINT('Ctrl Pts',(2.37800882372785,31.6189669376859,56.2652840065297));
#92021=CARTESIAN_POINT('Ctrl Pts',(2.38186402998285,31.5750584214616,56.32146620411));
#92022=CARTESIAN_POINT('Ctrl Pts',(2.38571923623786,31.5282080137986,56.375378004196));
#92023=CARTESIAN_POINT('Ctrl Pts',(2.38957444249286,31.4786859869049,56.4267043543184));
#92024=CARTESIAN_POINT('Ctrl Pts',(2.39342979935383,31.4291620254032,56.4780327095358));
#92025=CARTESIAN_POINT('Ctrl Pts',(2.3972851562148,31.3769665763488,56.5267750662));
#92026=CARTESIAN_POINT('Ctrl Pts',(2.40114051307577,31.3224071856569,56.5726527899772));
#92027=CARTESIAN_POINT('Ctrl Pts',(2.40499990555408,31.2677906846039,56.6185785365299));
#92028=CARTESIAN_POINT('Ctrl Pts',(2.40885929803238,31.2108056748858,56.6616333510883));
#92029=CARTESIAN_POINT('Ctrl Pts',(2.41271869051069,31.1517925480879,56.7015791161945));
#92030=CARTESIAN_POINT('Ctrl Pts',(2.4165802681239,31.0927460088698,56.7415474980431));
#92031=CARTESIAN_POINT('Ctrl Pts',(2.42044184573711,31.0316694828008,56.7784030751206));
#92032=CARTESIAN_POINT('Ctrl Pts',(2.42430342335032,30.9689297294892,56.8119527427094));
#92033=CARTESIAN_POINT('Ctrl Pts',(2.42817175747491,30.9060802019094,56.8455611113611));
#92034=CARTESIAN_POINT('Ctrl Pts',(2.43204009159949,30.8415620768424,56.8758518155404));
#92035=CARTESIAN_POINT('Ctrl Pts',(2.43590842572407,30.7757632823584,56.9026793981763));
#92036=CARTESIAN_POINT('Ctrl Pts',(2.4382061448087,30.7366800126712,56.9186144871918));
#92037=CARTESIAN_POINT('Ctrl Pts',(2.44050386389333,30.6971452387346,56.9333286803501));
#92038=CARTESIAN_POINT('Ctrl Pts',(2.44280158297796,30.6572424405911,56.946799922125));
#92039=CARTESIAN_POINT('Ctrl Pts',(2.4466706999575,30.590050330441,56.9694840746985));
#92040=CARTESIAN_POINT('Ctrl Pts',(2.45053981693705,30.5215508426835,56.9887299601902));
#92041=CARTESIAN_POINT('Ctrl Pts',(2.45440893391659,30.4521292551403,57.0043893581703));
#92042=CARTESIAN_POINT('Ctrl Pts',(2.45827227321803,30.382811333521,57.020025372272));
#92043=CARTESIAN_POINT('Ctrl Pts',(2.46213561251947,30.3125745154167,57.0320854237826));
#92044=CARTESIAN_POINT('Ctrl Pts',(2.46599895182091,30.2418205537346,57.0404706276473));
#92045=CARTESIAN_POINT('Ctrl Pts',(2.46985771066873,30.1711504793881,57.0488458898439));
#92046=CARTESIAN_POINT('Ctrl Pts',(2.47371646951655,30.099964959523,57.0535549025544));
#92047=CARTESIAN_POINT('Ctrl Pts',(2.47757522836436,30.0286755604101,57.0545498958982));
#92048=CARTESIAN_POINT('Ctrl Pts',(2.48143153828633,29.9574314044596,57.0555442577785));
#92049=CARTESIAN_POINT('Ctrl Pts',(2.48528784820829,29.8860839846391,57.0528292702121));
#92050=CARTESIAN_POINT('Ctrl Pts',(2.48914415813026,29.8150481441099,57.0464091412772));
#92051=CARTESIAN_POINT('Ctrl Pts',(2.49299931069921,29.7440336228069,57.0399909391468));
#92052=CARTESIAN_POINT('Ctrl Pts',(2.49685446326816,29.6733309786471,57.0298698472307));
#92053=CARTESIAN_POINT('Ctrl Pts',(2.50070961583712,29.6033514697071,57.0161020574159));
#92054=CARTESIAN_POINT('Ctrl Pts',(2.50456490098847,29.5333695541045,57.0023337941135));
#92055=CARTESIAN_POINT('Ctrl Pts',(2.50842018613982,29.4641112992215,56.9849186801397));
#92056=CARTESIAN_POINT('Ctrl Pts',(2.51227547129117,29.3959775776441,56.9639639700848));
#92057=CARTESIAN_POINT('Ctrl Pts',(2.5161345829473,29.3277762309751,56.9429884617504));
#92058=CARTESIAN_POINT('Ctrl Pts',(2.51999369460343,29.2607021103072,56.9184664888628));
#92059=CARTESIAN_POINT('Ctrl Pts',(2.52385280625956,29.1951398020452,56.890554845607));
#92060=CARTESIAN_POINT('Ctrl Pts',(2.52771409566082,29.1295404961499,56.8626274514607));
#92061=CARTESIAN_POINT('Ctrl Pts',(2.53157538506208,29.0654551374486,56.83130679249));
#92062=CARTESIAN_POINT('Ctrl Pts',(2.53543667446335,29.0032448017733,56.7967962147411));
#92063=CARTESIAN_POINT('Ctrl Pts',(2.53930424364821,28.9409332907121,56.7622295109324));
#92064=CARTESIAN_POINT('Ctrl Pts',(2.54317181283307,28.8805033005149,56.7244627914188));
#92065=CARTESIAN_POINT('Ctrl Pts',(2.54703938201794,28.8222872461249,56.6837429233289));
#92066=CARTESIAN_POINT('Ctrl Pts',(2.54871360714405,28.7970862021761,56.6661157722607));
#92067=CARTESIAN_POINT('Ctrl Pts',(2.55038783227017,28.7722996118778,56.6479357373517));
#92068=CARTESIAN_POINT('Ctrl Pts',(2.55206205739628,28.7479524050421,56.6292250864936));
#92069=CARTESIAN_POINT('',(2.24592528056623,32.0547491760433,54.9981598779361));
#92070=CARTESIAN_POINT('Ctrl Pts',(2.24592528056623,32.0547491760433,54.9981598779361));
#92071=CARTESIAN_POINT('Ctrl Pts',(2.24973199312511,32.0548119776976,55.0682865558832));
#92072=CARTESIAN_POINT('Ctrl Pts',(2.25353870568399,32.0512805113251,55.1385255805531));
#92073=CARTESIAN_POINT('Ctrl Pts',(2.25734541824288,32.044146919601,55.2084728605491));
#92074=CARTESIAN_POINT('Ctrl Pts',(2.26114901960424,32.0370191581078,55.2783629731596));
#92075=CARTESIAN_POINT('Ctrl Pts',(2.26495262096559,32.0262951561432,55.3479613175541));
#92076=CARTESIAN_POINT('Ctrl Pts',(2.26875622232695,32.0120190898361,55.4168653795114));
#92077=CARTESIAN_POINT('Ctrl Pts',(2.27255807195707,31.9977495983061,55.4857377080177));
#92078=CARTESIAN_POINT('Ctrl Pts',(2.27635992158718,31.9799313876817,55.5539158984091));
#92079=CARTESIAN_POINT('Ctrl Pts',(2.2801617712173,31.9586600131765,55.6210060509233));
#92080=CARTESIAN_POINT('Ctrl Pts',(2.28396322602705,31.9373908476939,55.6880892361555));
#92081=CARTESIAN_POINT('Ctrl Pts',(2.28776468083681,31.9126693830407,55.7540841309633));
#92082=CARTESIAN_POINT('Ctrl Pts',(2.29156613564656,31.8846409249957,55.8186123296965));
#92083=CARTESIAN_POINT('Ctrl Pts',(2.29537111074416,31.8565865115612,55.8832002839301));
#92084=CARTESIAN_POINT('Ctrl Pts',(2.29917608584177,31.8252191898369,55.9463183697466));
#92085=CARTESIAN_POINT('Ctrl Pts',(2.30298106093937,31.7907318497726,56.0076095497314));
#92086=CARTESIAN_POINT('Ctrl Pts',(2.30678785585504,31.7562280153338,56.0689300436522));
#92087=CARTESIAN_POINT('Ctrl Pts',(2.3105946507707,31.7186014616975,56.1284214698961));
#92088=CARTESIAN_POINT('Ctrl Pts',(2.31440144568637,31.6780888169565,56.1857552381945));
#92089=CARTESIAN_POINT('Ctrl Pts',(2.31821492477416,31.6375050379683,56.2431896761596));
#92090=CARTESIAN_POINT('Ctrl Pts',(2.32202840386194,31.5940253617011,56.2984584997057));
#92091=CARTESIAN_POINT('Ctrl Pts',(2.32584188294973,31.5479266015151,56.3512663685676));
#92092=CARTESIAN_POINT('Ctrl Pts',(2.32850815116974,31.5156957549742,56.3881880191841));
#92093=CARTESIAN_POINT('Ctrl Pts',(2.33117441938974,31.4821854249881,56.4239073940361));
#92094=CARTESIAN_POINT('Ctrl Pts',(2.33384068760975,31.44750006139,56.4583350557317));
#92095=CARTESIAN_POINT('Ctrl Pts',(2.33770976095523,31.3971674599028,56.5082937010076));
#92096=CARTESIAN_POINT('Ctrl Pts',(2.34157883430071,31.3441468440493,56.5557413933921));
#92097=CARTESIAN_POINT('Ctrl Pts',(2.34544790764619,31.2887188192779,56.6003753832582));
#92098=CARTESIAN_POINT('Ctrl Pts',(2.34931121603938,31.2333733827363,56.6449428680987));
#92099=CARTESIAN_POINT('Ctrl Pts',(2.35317452443257,31.1756280327693,56.6867046701));
#92100=CARTESIAN_POINT('Ctrl Pts',(2.35703783282577,31.1157998964758,56.7253950717226));
#92101=CARTESIAN_POINT('Ctrl Pts',(2.36089660931632,31.0560419423322,56.7640400870816));
#92102=CARTESIAN_POINT('Ctrl Pts',(2.36475538580687,30.9942064609002,56.7996205962112));
#92103=CARTESIAN_POINT('Ctrl Pts',(2.36861416229742,30.9306419148754,56.8319124402594));
#92104=CARTESIAN_POINT('Ctrl Pts',(2.3724705078834,30.8671174124616,56.8641839414887));
#92105=CARTESIAN_POINT('Ctrl Pts',(2.37632685346939,30.8018664385975,56.8931706684575));
#92106=CARTESIAN_POINT('Ctrl Pts',(2.38018319905538,30.7352632966772,56.9186936824463));
#92107=CARTESIAN_POINT('Ctrl Pts',(2.38403840529864,30.6686798324034,56.9442091557572));
#92108=CARTESIAN_POINT('Ctrl Pts',(2.3878936115419,30.6007454465498,56.9662627739661));
#92109=CARTESIAN_POINT('Ctrl Pts',(2.39174881778516,30.531854125668,56.98472384767));
#92110=CARTESIAN_POINT('Ctrl Pts',(2.39560417463449,30.4629601135034,57.0031856425673));
#92111=CARTESIAN_POINT('Ctrl Pts',(2.39945953148381,30.3931095618915,57.0180544907091));
#92112=CARTESIAN_POINT('Ctrl Pts',(2.40331488833313,30.3227096296274,57.0292501219529));
#92113=CARTESIAN_POINT('Ctrl Pts',(2.40717428080002,30.2522360058182,57.0404574722898));
#92114=CARTESIAN_POINT('Ctrl Pts',(2.41103367326691,30.1812123341334,57.0479838538699));
#92115=CARTESIAN_POINT('Ctrl Pts',(2.41489306573379,30.1100530385263,57.0518006460695));
#92116=CARTESIAN_POINT('Ctrl Pts',(2.41875464333569,30.0388534535032,57.0556195992844));
#92117=CARTESIAN_POINT('Ctrl Pts',(2.4226162209376,29.9675185777114,57.0557247813157));
#92118=CARTESIAN_POINT('Ctrl Pts',(2.4264777985395,29.896462232081,57.0521397352798));
#92119=CARTESIAN_POINT('Ctrl Pts',(2.43034613265307,29.8252815608309,57.0485484165731));
#92120=CARTESIAN_POINT('Ctrl Pts',(2.43421446676664,29.7543808761147,57.0412540285312));
#92121=CARTESIAN_POINT('Ctrl Pts',(2.43808280088021,29.684167582042,57.0303318561917));
#92122=CARTESIAN_POINT('Ctrl Pts',(2.44038052006958,29.6424621790435,57.0238442870631));
#92123=CARTESIAN_POINT('Ctrl Pts',(2.44267823925894,29.6009990977538,57.0160777639568));
#92124=CARTESIAN_POINT('Ctrl Pts',(2.44497595844831,29.5598612440212,57.0070564112614));
#92125=CARTESIAN_POINT('Ctrl Pts',(2.4488453513732,29.4905844930089,56.9918643205769));
#92126=CARTESIAN_POINT('Ctrl Pts',(2.45271474429808,29.4219595281757,56.9730514624946));
#92127=CARTESIAN_POINT('Ctrl Pts',(2.45658413722297,29.3543929934636,56.9506894052132));
#92128=CARTESIAN_POINT('Ctrl Pts',(2.46044683546966,29.2869433598302,56.9283660379228));
#92129=CARTESIAN_POINT('Ctrl Pts',(2.46430953371635,29.2205489751626,56.9025058240117));
#92130=CARTESIAN_POINT('Ctrl Pts',(2.46817223196304,29.1556048914633,56.8732310223727));
#92131=CARTESIAN_POINT('Ctrl Pts',(2.47203108508053,29.090725456457,56.8439853623822));
#92132=CARTESIAN_POINT('Ctrl Pts',(2.47588993819801,29.0272938988342,56.8113320565347));
#92133=CARTESIAN_POINT('Ctrl Pts',(2.4797487913155,28.9656875616429,56.7754422948549));
#92134=CARTESIAN_POINT('Ctrl Pts',(2.48360488003521,28.9041253578811,56.7395782438137));
#92135=CARTESIAN_POINT('Ctrl Pts',(2.48746096875492,28.8443861964193,56.7004825855419));
#92136=CARTESIAN_POINT('Ctrl Pts',(2.49131705747463,28.7868233519627,56.6583726912721));
#92137=CARTESIAN_POINT('Ctrl Pts',(2.49219263234804,28.7737529627907,56.6488110945287));
#92138=CARTESIAN_POINT('Ctrl Pts',(2.49306820722145,28.7607946693678,56.6390942729529));
#92139=CARTESIAN_POINT('Ctrl Pts',(2.49394378209486,28.7479524050421,56.6292250864936));
#92140=CARTESIAN_POINT('Ctrl Pts',(1.79398372125809,28.7479524050421,56.6292250864936));
#92141=CARTESIAN_POINT('Ctrl Pts',(1.79795521638298,28.689969871642,56.5846659325161));
#92142=CARTESIAN_POINT('Ctrl Pts',(1.80192671150787,28.6342860545768,56.5369438653214));
#92143=CARTESIAN_POINT('Ctrl Pts',(1.80589820663276,28.5812607271816,56.486329855134));
#92144=CARTESIAN_POINT('Ctrl Pts',(1.80975587549361,28.5297551485781,56.4371664834359));
#92145=CARTESIAN_POINT('Ctrl Pts',(1.81361354435446,28.4807580968254,56.3852750716134));
#92146=CARTESIAN_POINT('Ctrl Pts',(1.81747121321531,28.4345663209761,56.3309451375161));
#92147=CARTESIAN_POINT('Ctrl Pts',(1.82132695746882,28.3883975903995,56.2766423088531));
#92148=CARTESIAN_POINT('Ctrl Pts',(1.82518270172232,28.3450316727083,56.2199037415867));
#92149=CARTESIAN_POINT('Ctrl Pts',(1.82903844597583,28.304726946003,56.1610541911951));
#92150=CARTESIAN_POINT('Ctrl Pts',(1.83289355639876,28.2644288448327,56.1022143148487));
#92151=CARTESIAN_POINT('Ctrl Pts',(1.83674866682168,28.2271912092852,56.04126454557));
#92152=CARTESIAN_POINT('Ctrl Pts',(1.84060377724461,28.1932297341536,55.9785595377663));
#92153=CARTESIAN_POINT('Ctrl Pts',(1.84466176282885,28.1574810366108,55.9125546793286));
#92154=CARTESIAN_POINT('Ctrl Pts',(1.84871974841309,28.125363111767,55.844605265604));
#92155=CARTESIAN_POINT('Ctrl Pts',(1.85277773399733,28.0970720302535,55.7751533425434));
#92156=CARTESIAN_POINT('Ctrl Pts',(1.85663795219314,28.0701597247831,55.7090861839579));
#92157=CARTESIAN_POINT('Ctrl Pts',(1.86049817038895,28.0467100748932,55.6416600474042));
#92158=CARTESIAN_POINT('Ctrl Pts',(1.86435838858476,28.026841155681,55.5732728299735));
#92159=CARTESIAN_POINT('Ctrl Pts',(1.86822130676439,28.006958339389,55.5048377799148));
#92160=CARTESIAN_POINT('Ctrl Pts',(1.87208422494403,27.9906613465503,55.4354407840832));
#92161=CARTESIAN_POINT('Ctrl Pts',(1.87594714312366,27.9780172177736,55.3654903430737));
#92162=CARTESIAN_POINT('Ctrl Pts',(1.87981631658485,27.9653526141689,55.2954266302621));
#92163=CARTESIAN_POINT('Ctrl Pts',(1.88368549004604,27.9563527309751,55.2248081654246));
#92164=CARTESIAN_POINT('Ctrl Pts',(1.88755466350723,27.9510327507063,55.1540479594862));
#92165=CARTESIAN_POINT('Ctrl Pts',(1.88813631042332,27.9502330062265,55.1434106861825));
#92166=CARTESIAN_POINT('Ctrl Pts',(1.88871795733942,27.9495163266622,55.132770206435));
#92167=CARTESIAN_POINT('Ctrl Pts',(1.88929960425551,27.9488826620024,55.1221279176341));
#92168=CARTESIAN_POINT('Ctrl Pts',(1.89316867807688,27.9446675698584,55.0513361711988));
#92169=CARTESIAN_POINT('Ctrl Pts',(1.89703775189826,27.9441134566244,54.9801872885577));
#92170=CARTESIAN_POINT('Ctrl Pts',(1.90090682571963,27.9472620018025,54.9090919516438));
#92171=CARTESIAN_POINT('Ctrl Pts',(1.90477013459435,27.9504058556265,54.8381025472719));
#92172=CARTESIAN_POINT('Ctrl Pts',(1.90863344346907,27.9572413954818,54.7671670116155));
#92173=CARTESIAN_POINT('Ctrl Pts',(1.91249675234378,27.9677583715647,54.69669895128));
#92174=CARTESIAN_POINT('Ctrl Pts',(1.91635552932186,27.9782630105941,54.6263135542717));
#92175=CARTESIAN_POINT('Ctrl Pts',(1.92021430629993,27.9924404363935,54.5563950214545));
#92176=CARTESIAN_POINT('Ctrl Pts',(1.92407308327801,28.0102285014632,54.4873530004859));
#92177=CARTESIAN_POINT('Ctrl Pts',(1.92792942935496,28.0280053606438,54.4183544736937));
#92178=CARTESIAN_POINT('Ctrl Pts',(1.93178577543191,28.0493882254456,54.3502318325588));
#92179=CARTESIAN_POINT('Ctrl Pts',(1.93564212150886,28.0742639356115,54.2833842223245));
#92180=CARTESIAN_POINT('Ctrl Pts',(1.93949732824578,28.0991322963613,54.2165563619146));
#92181=CARTESIAN_POINT('Ctrl Pts',(1.94335253498271,28.1274912844472,54.1510032395835));
#92182=CARTESIAN_POINT('Ctrl Pts',(1.94720774171963,28.1591785242444,54.0871068754246));
#92183=CARTESIAN_POINT('Ctrl Pts',(1.95106309906459,28.1908670019396,54.0232080150816));
#92184=CARTESIAN_POINT('Ctrl Pts',(1.95491845640955,28.2258837716872,53.9609664756402));
#92185=CARTESIAN_POINT('Ctrl Pts',(1.9587738137545,28.2640199182091,53.9007408321395));
#92186=CARTESIAN_POINT('Ctrl Pts',(1.9626332067166,28.3021959839585,53.8404521471054));
#92187=CARTESIAN_POINT('Ctrl Pts',(1.9664925996787,28.3434976841852,53.7821839816096));
#92188=CARTESIAN_POINT('Ctrl Pts',(1.97035199264079,28.3876725456196,53.726266219985));
#92189=CARTESIAN_POINT('Ctrl Pts',(1.97421357073841,28.4318724182566,53.6703167984883));
#92190=CARTESIAN_POINT('Ctrl Pts',(1.97807514883603,28.4789483697121,53.6167207951661));
#92191=CARTESIAN_POINT('Ctrl Pts',(1.98193672693366,28.5286091840201,53.5657731598));
#92192=CARTESIAN_POINT('Ctrl Pts',(1.98580506153836,28.5783568886189,53.5147363826243));
#92193=CARTESIAN_POINT('Ctrl Pts',(1.98967339614307,28.630698128859,53.4663575547262));
#92194=CARTESIAN_POINT('Ctrl Pts',(1.99354173074778,28.6853071057159,53.4208926077626));
#92195=CARTESIAN_POINT('Ctrl Pts',(1.99583944552988,28.7177437654626,53.3938873221861));
#92196=CARTESIAN_POINT('Ctrl Pts',(1.99813716031198,28.7509799082505,53.367909293596));
#92197=CARTESIAN_POINT('Ctrl Pts',(2.00043487509407,28.7849426289779,53.3430047834635));
#92198=CARTESIAN_POINT('Ctrl Pts',(2.00430394846558,28.8421317367879,53.3010686050767));
#92199=CARTESIAN_POINT('Ctrl Pts',(2.00817302183709,28.9016064734258,53.2620144757941));
#92200=CARTESIAN_POINT('Ctrl Pts',(2.01204209520859,28.9630444126907,53.226100151517));
#92201=CARTESIAN_POINT('Ctrl Pts',(2.01590540362951,29.0243908089297,53.1902393398732));
#92202=CARTESIAN_POINT('Ctrl Pts',(2.01976871205043,29.08769418541,53.1575092900324));
#92203=CARTESIAN_POINT('Ctrl Pts',(2.02363202047135,29.1526014941873,53.1281257160679));
#92204=CARTESIAN_POINT('Ctrl Pts',(2.02749079699203,29.2174326626681,53.098776610857));
#92205=CARTESIAN_POINT('Ctrl Pts',(2.03134957351271,29.2838635857244,53.0727663832764));
#92206=CARTESIAN_POINT('Ctrl Pts',(2.03520835003339,29.3515163940419,53.0502649986976));
#92207=CARTESIAN_POINT('Ctrl Pts',(2.03906469565097,29.4191265833013,53.0277777892558));
#92208=CARTESIAN_POINT('Ctrl Pts',(2.04292104126856,29.4879566707864,53.0087951902587));
#92209=CARTESIAN_POINT('Ctrl Pts',(2.04677738688614,29.5576099432245,52.9934386129086));
#92210=CARTESIAN_POINT('Ctrl Pts',(2.05063259316243,29.6272426368925,52.9780865725956));
#92211=CARTESIAN_POINT('Ctrl Pts',(2.05448779943871,29.6976975585464,52.9663585316496));
#92212=CARTESIAN_POINT('Ctrl Pts',(2.05834300571499,29.7685656898447,52.9583252652337));
#92213=CARTESIAN_POINT('Ctrl Pts',(2.06219836259872,29.8394365896767,52.9502916849903));
#92214=CARTESIAN_POINT('Ctrl Pts',(2.06605371948246,29.9107202482591,52.9459532183724));
#92215=CARTESIAN_POINT('Ctrl Pts',(2.06990907636619,29.9820021030213,52.9453288247984));
#92216=CARTESIAN_POINT('Ctrl Pts',(2.07376846886937,30.0533585725203,52.9447037776364));
#92217=CARTESIAN_POINT('Ctrl Pts',(2.07762786137254,30.1247127476673,52.9478005685642));
#92218=CARTESIAN_POINT('Ctrl Pts',(2.08148725387572,30.195650545911,52.954586001225));
#92219=CARTESIAN_POINT('Ctrl Pts',(2.08534883151504,30.2666285081821,52.9613752757065));
#92220=CARTESIAN_POINT('Ctrl Pts',(2.08921040915435,30.3371891435098,52.9718572779838));
#92221=CARTESIAN_POINT('Ctrl Pts',(2.09307198679367,30.4069267067339,52.9859473150271));
#92222=CARTESIAN_POINT('Ctrl Pts',(2.09694032094603,30.4767862881588,53.0000620050822));
#92223=CARTESIAN_POINT('Ctrl Pts',(2.1008086550984,30.5458194516021,53.0177972128657));
#92224=CARTESIAN_POINT('Ctrl Pts',(2.10467698925076,30.6136344761209,53.0390180285847));
#92225=CARTESIAN_POINT('Ctrl Pts',(2.10697470814472,30.6539153456098,53.0516228003811));
#92226=CARTESIAN_POINT('Ctrl Pts',(2.10927242703867,30.693766781177,53.0654564044256));
#92227=CARTESIAN_POINT('Ctrl Pts',(2.11157014593263,30.7331103750084,53.0804826803191));
#92228=CARTESIAN_POINT('Ctrl Pts',(2.11543921914776,30.7993601001079,53.1057850624929));
#92229=CARTESIAN_POINT('Ctrl Pts',(2.1193082923629,30.8644281334726,53.1345708206484));
#92230=CARTESIAN_POINT('Ctrl Pts',(2.12317736557803,30.9279230507677,53.1667088680862));
#92231=CARTESIAN_POINT('Ctrl Pts',(2.12704067383826,30.9913233600482,53.1987990295357));
#92232=CARTESIAN_POINT('Ctrl Pts',(2.13090398209848,31.0531547760517,53.2342313478549));
#92233=CARTESIAN_POINT('Ctrl Pts',(2.13476729035871,31.1130445874744,53.2728262077041));
#92234=CARTESIAN_POINT('Ctrl Pts',(2.13862606671304,31.1728641443455,53.311375793332));
#92235=CARTESIAN_POINT('Ctrl Pts',(2.14248484306737,31.2307462144121,53.3530802895793));
#92236=CARTESIAN_POINT('Ctrl Pts',(2.1463436194217,31.2863430596233,53.3977144151373));
#92237=CARTESIAN_POINT('Ctrl Pts',(2.15019996486953,31.3419048805885,53.4423204226142));
#92238=CARTESIAN_POINT('Ctrl Pts',(2.15405631031736,31.3951839549608,53.4898520944146));
#92239=CARTESIAN_POINT('Ctrl Pts',(2.15791265576519,31.445863116871,53.5400419835584));
#92240=CARTESIAN_POINT('Ctrl Pts',(2.16176786186857,31.4965273057911,53.5902170442662));
#92241=CARTESIAN_POINT('Ctrl Pts',(2.16562306797194,31.5445927622341,53.6430484215114));
#92242=CARTESIAN_POINT('Ctrl Pts',(2.16947827407531,31.5897781880421,53.6982308671175));
#92243=CARTESIAN_POINT('Ctrl Pts',(2.17333363078323,31.6349653790295,53.7534154684389));
#92244=CARTESIAN_POINT('Ctrl Pts',(2.17718898749114,31.6772720099486,53.8109509432151));
#92245=CARTESIAN_POINT('Ctrl Pts',(2.18104434419906,31.7164573083123,53.8704992823193));
#92246=CARTESIAN_POINT('Ctrl Pts',(2.18490373652315,31.7556836241061,53.9301099539802));
#92247=CARTESIAN_POINT('Ctrl Pts',(2.18876312884725,31.79178181755,53.9917372893305));
#92248=CARTESIAN_POINT('Ctrl Pts',(2.19262252117135,31.8245551948391,54.0550153951065));
#92249=CARTESIAN_POINT('Ctrl Pts',(2.19648409862947,31.8573471279565,54.118329328062));
#92250=CARTESIAN_POINT('Ctrl Pts',(2.20034567608759,31.8868102967758,54.1832954494049));
#92251=CARTESIAN_POINT('Ctrl Pts',(2.20420725354571,31.9127957939903,54.2495269405282));
#92252=CARTESIAN_POINT('Ctrl Pts',(2.20807558751549,31.9388267574208,54.3158743153406));
#92253=CARTESIAN_POINT('Ctrl Pts',(2.21194392148527,31.961367747085,54.3834910192252));
#92254=CARTESIAN_POINT('Ctrl Pts',(2.21581225545505,31.9803196511975,54.4519747801598));
#92255=CARTESIAN_POINT('Ctrl Pts',(2.21810997589376,31.9915767395906,54.4926528959711));
#92256=CARTESIAN_POINT('Ctrl Pts',(2.22040769633247,32.0015685212364,54.5336367005789));
#92257=CARTESIAN_POINT('Ctrl Pts',(2.22270541677119,32.0102828504532,54.5748407078828));
#92258=CARTESIAN_POINT('Ctrl Pts',(2.22812785170467,32.0308479646294,54.6720788421834));
#92259=CARTESIAN_POINT('Ctrl Pts',(2.23355028663815,32.044363796373,54.7708559975936));
#92260=CARTESIAN_POINT('Ctrl Pts',(2.23897272157163,32.0506537445644,54.870320462662));
#92261=CARTESIAN_POINT('Ctrl Pts',(2.24129024122698,32.0533420347409,54.9128310424351));
#92262=CARTESIAN_POINT('Ctrl Pts',(2.24360776088233,32.0547109424995,54.9554668839174));
#92263=CARTESIAN_POINT('Ctrl Pts',(2.24592528053768,32.0547491760429,54.9981598774102));
#92264=CARTESIAN_POINT('Origin',(-1.54592528053767,30.,55.));
#92265=CARTESIAN_POINT('',(1.0938611646792,28.7479524050421,56.6292250864936));
#92266=CARTESIAN_POINT('',(1.15211015888001,28.7479524050421,56.6292250864936));
#92267=CARTESIAN_POINT('',(-1.54592528053767,28.7479524050421,56.6292250864936));
#92268=CARTESIAN_POINT('',(1.60407469463907,32.0544744411595,54.9994775005687));
#92269=CARTESIAN_POINT('Ctrl Pts',(1.15211015888001,28.7479524050421,56.6292250864936));
#92270=CARTESIAN_POINT('Ctrl Pts',(1.15596557431626,28.6914238068245,56.5857832710984));
#92271=CARTESIAN_POINT('Ctrl Pts',(1.15982098975252,28.637134064618,56.5393769881983));
#92272=CARTESIAN_POINT('Ctrl Pts',(1.16367640518878,28.5854020922282,56.4902718952686));
#92273=CARTESIAN_POINT('Ctrl Pts',(1.16753159109547,28.5336731996664,56.4411697257776));
#92274=CARTESIAN_POINT('Ctrl Pts',(1.17138677700217,28.4845021258141,56.3893694008486));
#92275=CARTESIAN_POINT('Ctrl Pts',(1.17524196290887,28.4381719776294,56.3351744421752));
#92276=CARTESIAN_POINT('Ctrl Pts',(1.17910094029473,28.3917962648997,56.280926184112));
#92277=CARTESIAN_POINT('Ctrl Pts',(1.18295991768059,28.3482673754369,56.224278958049));
#92278=CARTESIAN_POINT('Ctrl Pts',(1.18681889506645,28.307828457096,56.1655698314069));
#92279=CARTESIAN_POINT('Ctrl Pts',(1.19067971611772,28.2673702186535,56.1068326558866));
#92280=CARTESIAN_POINT('Ctrl Pts',(1.194540537169,28.2300051471003,56.0460320317991));
#92281=CARTESIAN_POINT('Ctrl Pts',(1.19840135822027,28.1959317990882,55.9835321494282));
#92282=CARTESIAN_POINT('Ctrl Pts',(1.20226929772362,28.1617956277824,55.9209170318751));
#92283=CARTESIAN_POINT('Ctrl Pts',(1.20613723722698,28.1309635168494,55.856596835388));
#92284=CARTESIAN_POINT('Ctrl Pts',(1.21000517673033,28.1035867777666,55.7909579337982));
#92285=CARTESIAN_POINT('Ctrl Pts',(1.21344131907149,28.0792662390809,55.7326466265028));
#92286=CARTESIAN_POINT('Ctrl Pts',(1.21687746141264,28.0576720240531,55.6732951092148));
#92287=CARTESIAN_POINT('Ctrl Pts',(1.2203136037538,28.0388768515798,55.6131831367794));
#92288=CARTESIAN_POINT('Ctrl Pts',(1.22418266805922,28.0177136622499,55.545497615114));
#92289=CARTESIAN_POINT('Ctrl Pts',(1.22805173236463,28.0000172432589,55.4765825943095));
#92290=CARTESIAN_POINT('Ctrl Pts',(1.23192079667004,27.9859270877188,55.4068265803942));
#92291=CARTESIAN_POINT('Ctrl Pts',(1.23578409586991,27.9718579272379,55.3371745065406));
#92292=CARTESIAN_POINT('Ctrl Pts',(1.23964739506977,27.9613844593252,55.2666843992818));
#92293=CARTESIAN_POINT('Ctrl Pts',(1.24351069426964,27.9545964859637,55.1957601268589));
#92294=CARTESIAN_POINT('Ctrl Pts',(1.24736946138368,27.9478164756607,55.1249190566094));
#92295=CARTESIAN_POINT('Ctrl Pts',(1.25122822849772,27.944713418032,55.0536453141185));
#92296=CARTESIAN_POINT('Ctrl Pts',(1.25508699561175,27.9453257944649,54.982351441733));
#92297=CARTESIAN_POINT('Ctrl Pts',(1.25894333171321,27.9459377851025,54.9111024842893));
#92298=CARTESIAN_POINT('Ctrl Pts',(1.26279966781467,27.9502605617029,54.8398339067335));
#92299=CARTESIAN_POINT('Ctrl Pts',(1.26665600391613,27.9582805657826,54.7689603617579));
#92300=CARTESIAN_POINT('Ctrl Pts',(1.27051120058094,27.9662982001813,54.6981077578807));
#92301=CARTESIAN_POINT('Ctrl Pts',(1.27436639724576,27.9780108387014,54.6276504373054));
#92302=CARTESIAN_POINT('Ctrl Pts',(1.27822159391058,27.9933530301187,54.5579983023039));
#92303=CARTESIAN_POINT('Ctrl Pts',(1.28207694110156,28.0086958205719,54.4883434477345));
#92304=CARTESIAN_POINT('Ctrl Pts',(1.28593228829254,28.0276683386305,54.419494315098));
#92305=CARTESIAN_POINT('Ctrl Pts',(1.28978763548352,28.0501543129043,54.3518492775485));
#92306=CARTESIAN_POINT('Ctrl Pts',(1.29364701823621,28.0726638242378,54.2841334329587));
#92307=CARTESIAN_POINT('Ctrl Pts',(1.2975064009889,28.0986939797298,54.217624661388));
#92308=CARTESIAN_POINT('Ctrl Pts',(1.30136578374159,28.1280793163987,54.1527039969375));
#92309=CARTESIAN_POINT('Ctrl Pts',(1.30522735158312,28.157481290332,54.0877465759825));
#92310=CARTESIAN_POINT('Ctrl Pts',(1.30908891942465,28.1902420037978,54.0243794838064));
#92311=CARTESIAN_POINT('Ctrl Pts',(1.31295048726618,28.2261499695875,53.9629591945804));
#92312=CARTESIAN_POINT('Ctrl Pts',(1.31681881165199,28.2621207631639,53.9014314389258));
#92313=CARTESIAN_POINT('Ctrl Pts',(1.32068713603781,28.3012495366031,53.8418576931656));
#92314=CARTESIAN_POINT('Ctrl Pts',(1.32455546042362,28.343281830513,53.7845649053151));
#92315=CARTESIAN_POINT('Ctrl Pts',(1.32685326514654,28.3682492308209,53.7505326925579));
#92316=CARTESIAN_POINT('Ctrl Pts',(1.32915106986945,28.3942403379088,53.7173046697533));
#92317=CARTESIAN_POINT('Ctrl Pts',(1.33144887459236,28.4211955479515,53.6849433226313));
#92318=CARTESIAN_POINT('Ctrl Pts',(1.33531795118427,28.4665831177334,53.6304528215963));
#92319=CARTESIAN_POINT('Ctrl Pts',(1.33918702777618,28.5148839095463,53.5782080925501));
#92320=CARTESIAN_POINT('Ctrl Pts',(1.34305610436809,28.565847175084,53.5285370418235));
#92321=CARTESIAN_POINT('Ctrl Pts',(1.34691941604287,28.6167345054482,53.4789400008727));
#92322=CARTESIAN_POINT('Ctrl Pts',(1.35078272771764,28.6702760899426,53.4319093626192));
#92323=CARTESIAN_POINT('Ctrl Pts',(1.35464603939242,28.7261813233442,53.3877396173376));
#92324=CARTESIAN_POINT('Ctrl Pts',(1.35850481920069,28.7820209769852,53.3436216854757));
#92325=CARTESIAN_POINT('Ctrl Pts',(1.36236359900897,28.8402183927242,53.3023582801752));
#92326=CARTESIAN_POINT('Ctrl Pts',(1.36622237881724,28.9004478436164,53.2642054793576));
#92327=CARTESIAN_POINT('Ctrl Pts',(1.37007872774143,28.9606393522521,53.2260767133492));
#92328=CARTESIAN_POINT('Ctrl Pts',(1.37393507666562,29.0228599469266,53.1910549234259));
#92329=CARTESIAN_POINT('Ctrl Pts',(1.3777914255898,29.0867539033691,53.1593536109594));
#92330=CARTESIAN_POINT('Ctrl Pts',(1.38164663518673,29.1506289828561,53.1276616643905));
#92331=CARTESIAN_POINT('Ctrl Pts',(1.38550184478365,29.2161760076978,53.0992884634977));
#92332=CARTESIAN_POINT('Ctrl Pts',(1.38935705438057,29.2830151001007,53.0744013357357));
#92333=CARTESIAN_POINT('Ctrl Pts',(1.39321241459403,29.3498568037942,53.0495132356756));
#92334=CARTESIAN_POINT('Ctrl Pts',(1.39706777480749,29.4179902192486,53.0281116465895));
#92335=CARTESIAN_POINT('Ctrl Pts',(1.40092313502095,29.4870175919196,53.0103149466561));
#92336=CARTESIAN_POINT('Ctrl Pts',(1.40478253084469,29.5561172192072,52.9924996179719));
#92337=CARTESIAN_POINT('Ctrl Pts',(1.40864192666842,29.6261122003175,52.9782968325805));
#92338=CARTESIAN_POINT('Ctrl Pts',(1.41250132249215,29.6965926683802,52.9677742365526));
#92339=CARTESIAN_POINT('Ctrl Pts',(1.41636290345185,29.7671130414986,52.9572456827779));
#92340=CARTESIAN_POINT('Ctrl Pts',(1.42022448441154,29.8381189649896,52.9504015129451));
#92341=CARTESIAN_POINT('Ctrl Pts',(1.42408606537124,29.9091962440461,52.9472573857386));
#92342=CARTESIAN_POINT('Ctrl Pts',(1.42795440280756,29.9803978845959,52.9441077573599));
#92343=CARTESIAN_POINT('Ctrl Pts',(1.43182274024388,30.0516706440507,52.9446710929736));
#92344=CARTESIAN_POINT('Ctrl Pts',(1.4356910776802,30.122601827308,52.9489109345422));
#92345=CARTESIAN_POINT('Ctrl Pts',(1.43798876693044,30.1647330580912,52.9514292873371));
#92346=CARTESIAN_POINT('Ctrl Pts',(1.44028645618068,30.2067438852967,52.955243733322));
#92347=CARTESIAN_POINT('Ctrl Pts',(1.44258414543092,30.2485494981069,52.9603380894151));
#92348=CARTESIAN_POINT('Ctrl Pts',(1.4464532193052,30.3189458775589,52.9689164644343));
#92349=CARTESIAN_POINT('Ctrl Pts',(1.45032229317949,30.3890355151986,52.9811603850249));
#92350=CARTESIAN_POINT('Ctrl Pts',(1.45419136705377,30.4584069262394,52.9970370316764));
#92351=CARTESIAN_POINT('Ctrl Pts',(1.45805467599527,30.5276749736498,53.0128900220722));
#92352=CARTESIAN_POINT('Ctrl Pts',(1.46191798493676,30.5962264490148,53.0323648868309));
#92353=CARTESIAN_POINT('Ctrl Pts',(1.46578129387826,30.6636563248155,53.0553771972353));
#92354=CARTESIAN_POINT('Ctrl Pts',(1.46964007094354,30.7310071016223,53.0783625129199));
#92355=CARTESIAN_POINT('Ctrl Pts',(1.47349884800882,30.7972384347695,53.1048768755598));
#92356=CARTESIAN_POINT('Ctrl Pts',(1.4773576250741,30.8619585198236,53.1347855156568));
#92357=CARTESIAN_POINT('Ctrl Pts',(1.48121397125084,30.9266378335891,53.1646753144036));
#92358=CARTESIAN_POINT('Ctrl Pts',(1.48507031742757,30.9898073481427,53.1979549450098));
#92359=CARTESIAN_POINT('Ctrl Pts',(1.48892666360431,31.0510947599586,53.2344413439119));
#92360=CARTESIAN_POINT('Ctrl Pts',(1.49278187045349,31.1123640648841,53.2709169631905));
#92361=CARTESIAN_POINT('Ctrl Pts',(1.49663707730267,31.1717519538029,53.310597221519));
#92362=CARTESIAN_POINT('Ctrl Pts',(1.50049228415185,31.2289118158825,53.3532537198207));
#92363=CARTESIAN_POINT('Ctrl Pts',(1.50434764162142,31.2860739111603,53.3959118846837));
#92364=CARTESIAN_POINT('Ctrl Pts',(1.508202999091,31.3410074187695,53.4415462280725));
#92365=CARTESIAN_POINT('Ctrl Pts',(1.51205835656057,31.3933971565771,53.4898867835348));
#92366=CARTESIAN_POINT('Ctrl Pts',(1.51591774966546,31.4458417338846,53.5382779399735));
#92367=CARTESIAN_POINT('Ctrl Pts',(1.51977714277035,31.4957368682545,53.589380633199));
#92368=CARTESIAN_POINT('Ctrl Pts',(1.52363653587523,31.5428034305105,53.6428872053859));
#92369=CARTESIAN_POINT('Ctrl Pts',(1.52749811412611,31.5898966413371,53.6964240724064));
#92370=CARTESIAN_POINT('Ctrl Pts',(1.53135969237699,31.6341577903864,53.75236714667));
#92371=CARTESIAN_POINT('Ctrl Pts',(1.53522127062787,31.675349078037,53.8103769381772));
#92372=CARTESIAN_POINT('Ctrl Pts',(1.53908960540088,31.7166124372159,53.8684882281948));
#92373=CARTESIAN_POINT('Ctrl Pts',(1.54295794017389,31.7547949507744,53.9286730447583));
#92374=CARTESIAN_POINT('Ctrl Pts',(1.5468262749469,31.7897034180098,53.9905648916032));
#92375=CARTESIAN_POINT('Ctrl Pts',(1.54912398872109,31.8104383519567,54.0273274153636));
#92376=CARTESIAN_POINT('Ctrl Pts',(1.55142170249528,31.8300190545549,54.0646917503932));
#92377=CARTESIAN_POINT('Ctrl Pts',(1.55371941626948,31.8484131225733,54.1025778636568));
#92378=CARTESIAN_POINT('Ctrl Pts',(1.55791568927328,31.8820058754753,54.1717685853616));
#92379=CARTESIAN_POINT('Ctrl Pts',(1.56211196227709,31.9117555147201,54.2429419085303));
#92380=CARTESIAN_POINT('Ctrl Pts',(1.5663082352809,31.9374425894471,54.3156654508967));
#92381=CARTESIAN_POINT('Ctrl Pts',(1.57045671771888,31.9628371189002,54.3875607584855));
#92382=CARTESIAN_POINT('Ctrl Pts',(1.57460520015686,31.9842609658738,54.4609708157442));
#92383=CARTESIAN_POINT('Ctrl Pts',(1.57875368259484,32.0015478850653,54.5354533109678));
#92384=CARTESIAN_POINT('Ctrl Pts',(1.58297385088156,32.0191335225213,54.6112228650054));
#92385=CARTESIAN_POINT('Ctrl Pts',(1.58719401916828,32.0324376878795,54.6881019450392));
#92386=CARTESIAN_POINT('Ctrl Pts',(1.591414187455,32.0413368548877,54.7656041651877));
#92387=CARTESIAN_POINT('Ctrl Pts',(1.59563435574172,32.0502360218958,54.8431063853363));
#92388=CARTESIAN_POINT('Ctrl Pts',(1.59985452402844,32.0547300321603,54.9212313568403));
#92389=CARTESIAN_POINT('Ctrl Pts',(1.60407469231516,32.0547499335384,54.9994773874789));
#92390=CARTESIAN_POINT('Ctrl Pts',(1.60407471946232,32.0515317218955,54.9994787085569));
#92391=CARTESIAN_POINT('Ctrl Pts',(1.62433470867756,32.0506800991794,55.3745305470031));
#92392=CARTESIAN_POINT('Ctrl Pts',(1.68163978817232,31.7726765815566,56.4365344554507));
#92393=CARTESIAN_POINT('Ctrl Pts',(1.76427577470813,30.2789783374865,57.3046346940974));
#92394=CARTESIAN_POINT('Ctrl Pts',(1.8266517720287,29.1224132525016,56.909956921782));
#92395=CARTESIAN_POINT('Ctrl Pts',(1.85198267906975,28.748910216197,56.6279533026674));
#92396=CARTESIAN_POINT('',(1.54592528048776,32.0547497261996,55.0010607463466));
#92397=CARTESIAN_POINT('Ctrl Pts',(1.54592528053768,32.0547497261991,55.0010607472628));
#92398=CARTESIAN_POINT('Ctrl Pts',(1.54924811760506,32.0547182463142,55.0620397260944));
#92399=CARTESIAN_POINT('Ctrl Pts',(1.55257095467244,32.0519724929102,55.1229466291482));
#92400=CARTESIAN_POINT('Ctrl Pts',(1.55589379173983,32.0465301511204,55.1836080146816));
#92401=CARTESIAN_POINT('Ctrl Pts',(1.55976286831917,32.0401931455047,55.2542414948306));
#92402=CARTESIAN_POINT('Ctrl Pts',(1.56363194489852,32.030182692726,55.3246848692759));
#92403=CARTESIAN_POINT('Ctrl Pts',(1.56750102147786,32.016518520056,55.3945258176229));
#92404=CARTESIAN_POINT('Ctrl Pts',(1.57136433313993,32.0028747069793,55.4642627030801));
#92405=CARTESIAN_POINT('Ctrl Pts',(1.575227644802,31.985588072785,55.5333984713152));
#92406=CARTESIAN_POINT('Ctrl Pts',(1.57909095646407,31.9647301330804,55.6015256159682));
#92407=CARTESIAN_POINT('Ctrl Pts',(1.58294973625947,31.9438966608302,55.6695728439167));
#92408=CARTESIAN_POINT('Ctrl Pts',(1.58680851605488,31.9195003460157,55.7366133362076));
#92409=CARTESIAN_POINT('Ctrl Pts',(1.59066729585028,31.8916634397915,55.8022512032126));
#92410=CARTESIAN_POINT('Ctrl Pts',(1.5945236447615,31.8638440697572,55.8678477208634));
#92411=CARTESIAN_POINT('Ctrl Pts',(1.59837999367272,31.8325885977026,55.9320429201068));
#92412=CARTESIAN_POINT('Ctrl Pts',(1.60223634258394,31.7980681641413,55.9944588677273));
#92413=CARTESIAN_POINT('Ctrl Pts',(1.60609155216783,31.7635579293651,56.0568563750571));
#92414=CARTESIAN_POINT('Ctrl Pts',(1.60994676175171,31.7257848830761,56.1174752494872));
#92415=CARTESIAN_POINT('Ctrl Pts',(1.6138019713356,31.6849662948508,56.1759617968781));
#92416=CARTESIAN_POINT('Ctrl Pts',(1.61765733153597,31.6441461119126,56.234450629239));
#92417=CARTESIAN_POINT('Ctrl Pts',(1.62151269173635,31.6002804306385,56.2908065720668));
#92418=CARTESIAN_POINT('Ctrl Pts',(1.62536805193672,31.553629065714,56.3447060231398));
#92419=CARTESIAN_POINT('Ctrl Pts',(1.62922744774737,31.5069288683283,56.3986618936309));
#92420=CARTESIAN_POINT('Ctrl Pts',(1.63308684355802,31.4574374850222,56.4501557713316));
#92421=CARTESIAN_POINT('Ctrl Pts',(1.63694623936868,31.4054535484968,56.4988988910256));
#92422=CARTESIAN_POINT('Ctrl Pts',(1.64080782031528,31.3534401793933,56.5476696083925));
#92423=CARTESIAN_POINT('Ctrl Pts',(1.64466940126188,31.2989318190824,56.5936861538513));
#92424=CARTESIAN_POINT('Ctrl Pts',(1.64853098220848,31.2422602297307,56.6367000593052));
#92425=CARTESIAN_POINT('Ctrl Pts',(1.65239931963182,31.1854894840281,56.6797892247252));
#92426=CARTESIAN_POINT('Ctrl Pts',(1.65626765705516,31.1265483544151,56.7198649879123));
#92427=CARTESIAN_POINT('Ctrl Pts',(1.6601359944785,31.0657970129473,56.7567225989588));
#92428=CARTESIAN_POINT('Ctrl Pts',(1.66243368384513,31.0297123346933,56.7786150379353));
#92429=CARTESIAN_POINT('Ctrl Pts',(1.66473137321176,30.9929894840122,56.7993729766357));
#92430=CARTESIAN_POINT('Ctrl Pts',(1.66702906257839,30.9557074212098,56.8189614859981));
#92431=CARTESIAN_POINT('Ctrl Pts',(1.67089813645219,30.8929282408536,56.8519465321499));
#92432=CARTESIAN_POINT('Ctrl Pts',(1.67476721032598,30.8283164320441,56.881742254264));
#92433=CARTESIAN_POINT('Ctrl Pts',(1.67863628419978,30.7622291018219,56.9081415982143));
#92434=CARTESIAN_POINT('Ctrl Pts',(1.68249959314074,30.6962402419397,56.934501607055));
#92435=CARTESIAN_POINT('Ctrl Pts',(1.6863629020817,30.6287806721178,56.9574751041712));
#92436=CARTESIAN_POINT('Ctrl Pts',(1.69022621102266,30.5602315430996,56.9769011560056));
#92437=CARTESIAN_POINT('Ctrl Pts',(1.69408498808734,30.4917628260228,56.9963044200006));
#92438=CARTESIAN_POINT('Ctrl Pts',(1.69794376515202,30.4222075536278,57.0121683727561));
#92439=CARTESIAN_POINT('Ctrl Pts',(1.7018025422167,30.351964634118,57.02438100634));
#92440=CARTESIAN_POINT('Ctrl Pts',(1.7056588883928,30.2817659650812,57.0365859464109));
#92441=CARTESIAN_POINT('Ctrl Pts',(1.70951523456889,30.2108809858512,57.0451440478502));
#92442=CARTESIAN_POINT('Ctrl Pts',(1.71337158074499,30.1397200345346,57.049994115711));
#92443=CARTESIAN_POINT('Ctrl Pts',(1.71722678759349,30.0685801071696,57.0548427506568));
#92444=CARTESIAN_POINT('Ctrl Pts',(1.72108199444199,29.9971648539827,57.0559854938997));
#92445=CARTESIAN_POINT('Ctrl Pts',(1.7249372012905,29.9258892675496,57.0534130519298));
#92446=CARTESIAN_POINT('Ctrl Pts',(1.72879255875936,29.854610896427,57.0508405094563));
#92447=CARTESIAN_POINT('Ctrl Pts',(1.73264791622821,29.7834726882822,57.0445525133166));
#92448=CARTESIAN_POINT('Ctrl Pts',(1.73650327369707,29.7128874291141,57.0345918347765));
#92449=CARTESIAN_POINT('Ctrl Pts',(1.74036266680119,29.6422282840968,57.0246207297933));
#92450=CARTESIAN_POINT('Ctrl Pts',(1.7442220599053,29.572123725487,57.0109693361057));
#92451=CARTESIAN_POINT('Ctrl Pts',(1.74808145300941,29.5029783247046,56.9937319320276));
#92452=CARTESIAN_POINT('Ctrl Pts',(1.75194303125949,29.4337937745563,56.9764847683208));
#92453=CARTESIAN_POINT('Ctrl Pts',(1.75580460950957,29.3655699281291,56.9556476943698));
#92454=CARTESIAN_POINT('Ctrl Pts',(1.75966618775964,29.2986954697037,56.9313646777048));
#92455=CARTESIAN_POINT('Ctrl Pts',(1.7635345225318,29.2317040024477,56.9070391735573));
#92456=CARTESIAN_POINT('Ctrl Pts',(1.76740285730397,29.166067084491,56.8792558784584));
#92457=CARTESIAN_POINT('Ctrl Pts',(1.77127119207613,29.1021520790547,56.8482063394963));
#92458=CARTESIAN_POINT('Ctrl Pts',(1.7735689058564,29.0641878392959,56.8297635319973));
#92459=CARTESIAN_POINT('Ctrl Pts',(1.77586661963668,29.0268306333798,56.8101692312318));
#92460=CARTESIAN_POINT('Ctrl Pts',(1.77816433341695,28.9901526342878,56.7894708325268));
#92461=CARTESIAN_POINT('Ctrl Pts',(1.78203306890535,28.9283966932524,56.7546202648405));
#92462=CARTESIAN_POINT('Ctrl Pts',(1.78590180439376,28.8683259936513,56.7165008236237));
#92463=CARTESIAN_POINT('Ctrl Pts',(1.78977053988216,28.8103080775549,56.6753001797197));
#92464=CARTESIAN_POINT('Ctrl Pts',(1.79117493367413,28.7892469320117,56.6603438900747));
#92465=CARTESIAN_POINT('Ctrl Pts',(1.79257932746611,28.7684560963194,56.6449820236807));
#92466=CARTESIAN_POINT('Ctrl Pts',(1.79398372125809,28.7479524050421,56.6292250864936));
#92467=CARTESIAN_POINT('Ctrl Pts',(1.0938611646792,28.7479524050421,56.6292250864936));
#92468=CARTESIAN_POINT('Ctrl Pts',(1.0977297220774,28.6914507587339,56.5858039834442));
#92469=CARTESIAN_POINT('Ctrl Pts',(1.1015982794756,28.637286265427,56.5394984821215));
#92470=CARTESIAN_POINT('Ctrl Pts',(1.10546683687381,28.5857505639064,56.4906025945936));
#92471=CARTESIAN_POINT('Ctrl Pts',(1.1074287940444,28.5596139892786,56.4658048141101));
#92472=CARTESIAN_POINT('Ctrl Pts',(1.109390751215,28.53415294125,56.4403413350234));
#92473=CARTESIAN_POINT('Ctrl Pts',(1.1113527083856,28.509401474378,56.4142537247303));
#92474=CARTESIAN_POINT('Ctrl Pts',(1.11522171013032,28.4605913015836,56.3628086619877));
#92475=CARTESIAN_POINT('Ctrl Pts',(1.11909071187505,28.4143519004918,56.3087329477492));
#92476=CARTESIAN_POINT('Ctrl Pts',(1.12295971361977,28.3709796177163,56.2523139209496));
#92477=CARTESIAN_POINT('Ctrl Pts',(1.12682294925331,28.3276719741995,56.1959789774364));
#92478=CARTESIAN_POINT('Ctrl Pts',(1.13068618488685,28.2872232609604,56.1373080355254));
#92479=CARTESIAN_POINT('Ctrl Pts',(1.13454942052039,28.2498919800653,56.0766241131706));
#92480=CARTESIAN_POINT('Ctrl Pts',(1.13840812288228,28.2126045051539,56.0160113997015));
#92481=CARTESIAN_POINT('Ctrl Pts',(1.14226682524417,28.1784274496466,55.9533908095042));
#92482=CARTESIAN_POINT('Ctrl Pts',(1.14612552760606,28.1475770620854,55.8891157526373));
#92483=CARTESIAN_POINT('Ctrl Pts',(1.14998179825842,28.1167461160811,55.8248812011668));
#92484=CARTESIAN_POINT('Ctrl Pts',(1.15383806891078,28.0892378884678,55.7589946885105));
#92485=CARTESIAN_POINT('Ctrl Pts',(1.15769433956313,28.0652228373674,55.6918344407842));
#92486=CARTESIAN_POINT('Ctrl Pts',(1.16154947017932,28.0412148858793,55.6246940477617));
#92487=CARTESIAN_POINT('Ctrl Pts',(1.1654046007955,28.0206982242059,55.5562811244291));
#92488=CARTESIAN_POINT('Ctrl Pts',(1.16925973141168,28.0037946301486,55.4869924885217));
#92489=CARTESIAN_POINT('Ctrl Pts',(1.17311501205124,27.9868903782838,55.4177011562296));
#92490=CARTESIAN_POINT('Ctrl Pts',(1.17697029269079,27.9735995861848,55.3475345161915));
#92491=CARTESIAN_POINT('Ctrl Pts',(1.18082557333034,27.9639933284843,55.2769014193601));
#92492=CARTESIAN_POINT('Ctrl Pts',(1.18468488922055,27.9543770160923,55.2061943921779));
#92493=CARTESIAN_POINT('Ctrl Pts',(1.18854420511077,27.9484530022102,55.1350204159442));
#92494=CARTESIAN_POINT('Ctrl Pts',(1.19240352100098,27.9462405613698,55.0637944412743));
#92495=CARTESIAN_POINT('Ctrl Pts',(1.19626502170354,27.944026868036,54.9925281445905));
#92496=CARTESIAN_POINT('Ctrl Pts',(1.20012652240609,27.9455289202923,54.9212102767999));
#92497=CARTESIAN_POINT('Ctrl Pts',(1.20398802310865,27.9507138557503,54.8502540101159));
#92498=CARTESIAN_POINT('Ctrl Pts',(1.20785628064545,27.9559078637821,54.7791735845182));
#92499=CARTESIAN_POINT('Ctrl Pts',(1.21172453818225,27.9647975606131,54.7084565054525));
#92500=CARTESIAN_POINT('Ctrl Pts',(1.21559279571905,27.9772984996671,54.6385083637885));
#92501=CARTESIAN_POINT('Ctrl Pts',(1.21789119022075,27.9847261565163,54.5969474225441));
#92502=CARTESIAN_POINT('Ctrl Pts',(1.22018958472245,27.9934277350247,54.5556577220521));
#92503=CARTESIAN_POINT('Ctrl Pts',(1.22248797922415,28.0033772232959,54.5147216777495));
#92504=CARTESIAN_POINT('Ctrl Pts',(1.2263570736365,28.0201260927555,54.44581034849));
#92505=CARTESIAN_POINT('Ctrl Pts',(1.23022616804885,28.0404795568516,54.3776321742186));
#92506=CARTESIAN_POINT('Ctrl Pts',(1.2340952624612,28.0643569152215,54.3105919852154));
#92507=CARTESIAN_POINT('Ctrl Pts',(1.23795859211244,28.0881986974973,54.2436516828094));
#92508=CARTESIAN_POINT('Ctrl Pts',(1.24182192176367,28.1155537904264,54.1778464539593));
#92509=CARTESIAN_POINT('Ctrl Pts',(1.24568525141491,28.1462909932252,54.1135686824677));
#92510=CARTESIAN_POINT('Ctrl Pts',(1.24954404934275,28.1769921409852,54.0493663094295));
#92511=CARTESIAN_POINT('Ctrl Pts',(1.25340284727059,28.2110673097648,53.9866882709052));
#92512=CARTESIAN_POINT('Ctrl Pts',(1.25726164519843,28.2483368490322,53.9259079331634));
#92513=CARTESIAN_POINT('Ctrl Pts',(1.26111801232047,28.2855829107777,53.8651658833031));
#92514=CARTESIAN_POINT('Ctrl Pts',(1.2649743794425,28.3260190973889,53.8063195756463));
#92515=CARTESIAN_POINT('Ctrl Pts',(1.26883074656453,28.3694200751477,53.7497173634859));
#92516=CARTESIAN_POINT('Ctrl Pts',(1.27268597441018,28.41280823107,53.6931318731679));
#92517=CARTESIAN_POINT('Ctrl Pts',(1.27654120225583,28.4591591438457,53.6387895474606));
#92518=CARTESIAN_POINT('Ctrl Pts',(1.28039643010148,28.508205458637,53.587007923285));
#92519=CARTESIAN_POINT('Ctrl Pts',(1.28425180858722,28.5572536898756,53.5352242757819));
#92520=CARTESIAN_POINT('Ctrl Pts',(1.28810718707295,28.6089971965746,53.4860018796339));
#92521=CARTESIAN_POINT('Ctrl Pts',(1.29196256555869,28.6631310155764,53.439622199278));
#92522=CARTESIAN_POINT('Ctrl Pts',(1.29582197956375,28.7173214977758,53.3931939721718));
#92523=CARTESIAN_POINT('Ctrl Pts',(1.29968139356882,28.7739069171724,53.3496147174127));
#92524=CARTESIAN_POINT('Ctrl Pts',(1.30354080757388,28.8325490922598,53.3091256875461));
#92525=CARTESIAN_POINT('Ctrl Pts',(1.30740240669101,28.8912244692073,53.2686137337156));
#92526=CARTESIAN_POINT('Ctrl Pts',(1.31126400580813,28.9519585062001,53.2311957426527));
#92527=CARTESIAN_POINT('Ctrl Pts',(1.31512560492525,29.0143862391476,53.1970681995931));
#92528=CARTESIAN_POINT('Ctrl Pts',(1.31899396028313,29.0769231954454,53.1628809470997));
#92529=CARTESIAN_POINT('Ctrl Pts',(1.32286231564101,29.1411593260394,53.1319958471076));
#92530=CARTESIAN_POINT('Ctrl Pts',(1.32673067099888,29.2067080592444,53.1045619347411));
#92531=CARTESIAN_POINT('Ctrl Pts',(1.32902819735349,29.245639317652,53.0882681533171));
#92532=CARTESIAN_POINT('Ctrl Pts',(1.3313257237081,29.285033255374,53.073190842872));
#92533=CARTESIAN_POINT('Ctrl Pts',(1.33362325006271,29.32480662124,53.0593528234688));
#92534=CARTESIAN_POINT('Ctrl Pts',(1.33749233009983,29.3917857597262,53.0360493238075));
#92535=CARTESIAN_POINT('Ctrl Pts',(1.34136141013695,29.4601039418764,53.0161718100105));
#92536=CARTESIAN_POINT('Ctrl Pts',(1.34523049017407,29.5293772862274,52.9998720481476));
#92537=CARTESIAN_POINT('Ctrl Pts',(1.3490938054489,29.5985474162846,52.9835965722265));
#92538=CARTESIAN_POINT('Ctrl Pts',(1.35295712072372,29.6686694146107,52.9708883773142));
#92539=CARTESIAN_POINT('Ctrl Pts',(1.35682043599855,29.7393424667455,52.9618500514296));
#92540=CARTESIAN_POINT('Ctrl Pts',(1.36067921962054,29.8099326196826,52.9528223274637));
#92541=CARTESIAN_POINT('Ctrl Pts',(1.36453800324253,29.8810720629707,52.9474559831786));
#92542=CARTESIAN_POINT('Ctrl Pts',(1.36839678686451,29.9523496820247,52.9458025874574));
#92543=CARTESIAN_POINT('Ctrl Pts',(1.37225313973244,30.0235824013435,52.9441502332556));
#92544=CARTESIAN_POINT('Ctrl Pts',(1.37610949260036,30.0949526392354,52.9462061985391));
#92545=CARTESIAN_POINT('Ctrl Pts',(1.37996584546828,30.1660455185716,52.9519701056229));
#92546=CARTESIAN_POINT('Ctrl Pts',(1.38382105913332,30.2371173964031,52.9577323099944));
#92547=CARTESIAN_POINT('Ctrl Pts',(1.38767627279836,30.3079115944096,52.9672002423364));
#92548=CARTESIAN_POINT('Ctrl Pts',(1.3915314864634,30.3780163348335,52.9803215074921));
#92549=CARTESIAN_POINT('Ctrl Pts',(1.39538685086384,30.4481238162901,52.9934432856775));
#92550=CARTESIAN_POINT('Ctrl Pts',(1.39924221526429,30.5175413095568,53.0102185887353));
#92551=CARTESIAN_POINT('Ctrl Pts',(1.40309757966473,30.5858669455365,53.0305438606997));
#92552=CARTESIAN_POINT('Ctrl Pts',(1.40695697982935,30.6542641042375,53.0508904089938));
#92553=CARTESIAN_POINT('Ctrl Pts',(1.41081637999396,30.7215666574989,53.0747942055277));
#92554=CARTESIAN_POINT('Ctrl Pts',(1.41467578015858,30.7873885035599,53.1021019766695));
#92555=CARTESIAN_POINT('Ctrl Pts',(1.41853736555258,30.8532476185814,53.1294252097332));
#92556=CARTESIAN_POINT('Ctrl Pts',(1.42239895094658,30.9176239188223,53.1601560448173));
#92557=CARTESIAN_POINT('Ctrl Pts',(1.42626053634058,30.9801543876826,53.1940944269408));
#92558=CARTESIAN_POINT('Ctrl Pts',(1.43012887831197,31.0427942654798,53.2280921907124));
#92559=CARTESIAN_POINT('Ctrl Pts',(1.43399722028336,31.1035814494069,53.2653084527368));
#92560=CARTESIAN_POINT('Ctrl Pts',(1.43786556225475,31.1621810686832,53.3054992693733));
#92561=CARTESIAN_POINT('Ctrl Pts',(1.44016321513692,31.1969870876753,53.3293711365362));
#92562=CARTESIAN_POINT('Ctrl Pts',(1.4424608680191,31.2310219537611,53.3542916065651));
#92563=CARTESIAN_POINT('Ctrl Pts',(1.44475852090127,31.2642213318106,53.380203103258));
#92564=CARTESIAN_POINT('Ctrl Pts',(1.4485823544001,31.3194728865213,53.4233259134211));
#92565=CARTESIAN_POINT('Ctrl Pts',(1.45240618789893,31.3726360605504,53.4693732485111));
#92566=CARTESIAN_POINT('Ctrl Pts',(1.45623002139776,31.4233792996943,53.5181130502964));
#92567=CARTESIAN_POINT('Ctrl Pts',(1.46004734993108,31.4740362162981,53.566769937716));
#92568=CARTESIAN_POINT('Ctrl Pts',(1.4638646784644,31.5222810158461,53.618109855358));
#92569=CARTESIAN_POINT('Ctrl Pts',(1.46768200699772,31.5678140408072,53.6718596851432));
#92570=CARTESIAN_POINT('Ctrl Pts',(1.47149570170064,31.6133037215056,53.7255583488409));
#92571=CARTESIAN_POINT('Ctrl Pts',(1.47530939640356,31.6560864236995,53.7816619997429));
#92572=CARTESIAN_POINT('Ctrl Pts',(1.47912309110647,31.6958993234528,53.8398607638683));
#92573=CARTESIAN_POINT('Ctrl Pts',(1.48293450363163,31.7356883985107,53.898024700894));
#92574=CARTESIAN_POINT('Ctrl Pts',(1.48674591615678,31.7725109144556,53.9582808546584));
#92575=CARTESIAN_POINT('Ctrl Pts',(1.49055732868193,31.8061455356611,54.0202878654873));
#92576=CARTESIAN_POINT('Ctrl Pts',(1.49436780754815,31.8397719175946,54.0822796868295));
#92577=CARTESIAN_POINT('Ctrl Pts',(1.49817828641437,31.8702117178646,54.1460210758164));
#92578=CARTESIAN_POINT('Ctrl Pts',(1.50198876528059,31.8972889701406,54.2111450537121));
#92579=CARTESIAN_POINT('Ctrl Pts',(1.50580205921379,31.9243862262747,54.2763171432405));
#92580=CARTESIAN_POINT('Ctrl Pts',(1.509615353147,31.9481157772653,54.3428734022453));
#92581=CARTESIAN_POINT('Ctrl Pts',(1.5134286470802,31.968349831146,54.410426845313));
#92582=CARTESIAN_POINT('Ctrl Pts',(1.51724327663821,31.9885909721027,54.4780039493037));
#92583=CARTESIAN_POINT('Ctrl Pts',(1.52105790619622,32.00533405718,54.5465784486412));
#92584=CARTESIAN_POINT('Ctrl Pts',(1.52487253575423,32.0185019668706,54.6157508981929));
#92585=CARTESIAN_POINT('Ctrl Pts',(1.52869346797487,32.0316916330361,54.6850376368532));
#92586=CARTESIAN_POINT('Ctrl Pts',(1.5325144001955,32.0412942558452,54.7549238045444));
#92587=CARTESIAN_POINT('Ctrl Pts',(1.53633533241613,32.047284473777,54.8250032973687));
#92588=CARTESIAN_POINT('Ctrl Pts',(1.53953198177334,32.0522959801831,54.8836328549622));
#92589=CARTESIAN_POINT('Ctrl Pts',(1.54272863113055,32.0547800105815,54.9423974987856));
#92590=CARTESIAN_POINT('Ctrl Pts',(1.54592528048776,32.0547497261996,55.0010607463466));
#92591=CARTESIAN_POINT('Origin',(-1.54592528053767,30.,55.));
#92592=CARTESIAN_POINT('',(0.393903217269906,28.7479524050421,56.6292250864936));
#92593=CARTESIAN_POINT('',(0.452117494115148,28.7479524050421,56.6292250864936));
#92594=CARTESIAN_POINT('',(-1.54592528053767,28.7479524050421,56.6292250864936));
#92595=CARTESIAN_POINT('',(0.145925152720326,32.0544673062769,54.9976428107105));
#92596=CARTESIAN_POINT('Ctrl Pts',(0.145925280537679,32.0547486502654,54.9976448497734));
#92597=CARTESIAN_POINT('Ctrl Pts',(0.149739546941021,32.0548295065906,55.0681878763859));
#92598=CARTESIAN_POINT('Ctrl Pts',(0.153553813344363,32.0512732959282,55.1387966811012));
#92599=CARTESIAN_POINT('Ctrl Pts',(0.157368079747704,32.0440865851276,55.2090636147235));
#92600=CARTESIAN_POINT('Ctrl Pts',(0.16118104386731,32.0369023280457,55.2793065574979));
#92601=CARTESIAN_POINT('Ctrl Pts',(0.164994007986915,32.0260900801542,55.3492073667697));
#92602=CARTESIAN_POINT('Ctrl Pts',(0.168806972106521,32.0117083701161,55.4183622785397));
#92603=CARTESIAN_POINT('Ctrl Pts',(0.17261997446274,31.9973265158574,55.4875178837989));
#92604=CARTESIAN_POINT('Ctrl Pts',(0.17643297681896,31.9793752318499,55.5559270906845));
#92605=CARTESIAN_POINT('Ctrl Pts',(0.18024597917518,31.9579640201056,55.6231969660323));
#92606=CARTESIAN_POINT('Ctrl Pts',(0.184063075019275,31.9365298221349,55.6905390596463));
#92607=CARTESIAN_POINT('Ctrl Pts',(0.187880170863369,31.9116284331976,55.7567389057323));
#92608=CARTESIAN_POINT('Ctrl Pts',(0.191697266707464,31.8834187459821,55.8214203490195));
#92609=CARTESIAN_POINT('Ctrl Pts',(0.195516531191688,31.8551930317496,55.8861385403422));
#92610=CARTESIAN_POINT('Ctrl Pts',(0.199335795675912,31.8236555029915,55.9493361684856));
#92611=CARTESIAN_POINT('Ctrl Pts',(0.203155060160136,31.7890112742995,56.0106612800189));
#92612=CARTESIAN_POINT('Ctrl Pts',(0.206981404197841,31.7543028275699,56.0721000664256));
#92613=CARTESIAN_POINT('Ctrl Pts',(0.210807748235547,31.7164764527575,56.1316589887038));
#92614=CARTESIAN_POINT('Ctrl Pts',(0.214634092273253,31.6757804376753,56.1890153435531));
#92615=CARTESIAN_POINT('Ctrl Pts',(0.217179575407875,31.6487073310709,56.2271717749909));
#92616=CARTESIAN_POINT('Ctrl Pts',(0.219725058542498,31.6203650995654,56.2643540944347));
#92617=CARTESIAN_POINT('Ctrl Pts',(0.22227054167712,31.5908360390092,56.3004761664443));
#92618=CARTESIAN_POINT('Ctrl Pts',(0.226143011689853,31.5459131715374,56.355429050929));
#92619=CARTESIAN_POINT('Ctrl Pts',(0.230015481702586,31.4980521337605,56.4081584923707));
#92620=CARTESIAN_POINT('Ctrl Pts',(0.233887951715319,31.4475011920355,56.4583339334856));
#92621=CARTESIAN_POINT('Ctrl Pts',(0.237754632281614,31.397025825323,56.5084343609716));
#92622=CARTESIAN_POINT('Ctrl Pts',(0.241621312847911,31.3438688788997,56.5559880289897));
#92623=CARTESIAN_POINT('Ctrl Pts',(0.245487993414207,31.2883187640707,56.6006974494399));
#92624=CARTESIAN_POINT('Ctrl Pts',(0.249350087975477,31.2328345334288,56.6453538431081));
#92625=CARTESIAN_POINT('Ctrl Pts',(0.253212182536747,31.1749631486356,56.6871723879026));
#92626=CARTESIAN_POINT('Ctrl Pts',(0.257074277098017,31.1150284775513,56.7258936979865));
#92627=CARTESIAN_POINT('Ctrl Pts',(0.260933905263996,31.0551320817056,56.7645902800231));
#92628=CARTESIAN_POINT('Ctrl Pts',(0.264793533429976,30.9931754201667,56.8001932893774));
#92629=CARTESIAN_POINT('Ctrl Pts',(0.268653161595956,30.9295127465629,56.8324856388188));
#92630=CARTESIAN_POINT('Ctrl Pts',(0.272511609673873,30.8658695379329,56.8647681148178));
#92631=CARTESIAN_POINT('Ctrl Pts',(0.276370057751791,30.8005217849537,56.8937417214125));
#92632=CARTESIAN_POINT('Ctrl Pts',(0.280228505829709,30.7338483284433,56.9192353147389));
#92633=CARTESIAN_POINT('Ctrl Pts',(0.284087058474176,30.6671730650373,56.9447295989589));
#92634=CARTESIAN_POINT('Ctrl Pts',(0.287945611118644,30.59917248037,56.9667435115671));
#92635=CARTESIAN_POINT('Ctrl Pts',(0.291804163763111,30.5302437648765,56.9851546822124));
#92636=CARTESIAN_POINT('Ctrl Pts',(0.295666658520141,30.4612446279632,57.0035846627363));
#92637=CARTESIAN_POINT('Ctrl Pts',(0.299529153277172,30.3913159365964,57.0184044280303));
#92638=CARTESIAN_POINT('Ctrl Pts',(0.303391648034202,30.3208674842945,57.029542219325));
#92639=CARTESIAN_POINT('Ctrl Pts',(0.307256279705638,30.2503800565838,57.0406861725715));
#92640=CARTESIAN_POINT('Ctrl Pts',(0.311120911377074,30.1793727778278,57.0481440453768));
#92641=CARTESIAN_POINT('Ctrl Pts',(0.31498554304851,30.1082603018613,57.0518960182087));
#92642=CARTESIAN_POINT('Ctrl Pts',(0.31885682091095,30.0370255303856,57.0556544434869));
#92643=CARTESIAN_POINT('Ctrl Pts',(0.32272809877339,29.9656856854891,57.0556942436997));
#92644=CARTESIAN_POINT('Ctrl Pts',(0.326599376635829,29.8946544516291,57.0520477279874));
#92645=CARTESIAN_POINT('Ctrl Pts',(0.32886818859578,29.8530256875264,57.0499106407635));
#92646=CARTESIAN_POINT('Ctrl Pts',(0.331137000555731,29.8115028259049,57.0465083981366));
#92647=CARTESIAN_POINT('Ctrl Pts',(0.333405812515682,29.7701676343163,57.0418556869143));
#92648=CARTESIAN_POINT('Ctrl Pts',(0.337281013011975,29.699565857798,57.0339087132752));
#92649=CARTESIAN_POINT('Ctrl Pts',(0.341156213508268,29.6292435862739,57.0222806428858));
#92650=CARTESIAN_POINT('Ctrl Pts',(0.345031414004561,29.5596137015207,57.0070021102659));
#92651=CARTESIAN_POINT('Ctrl Pts',(0.349104064276673,29.4864360248151,56.9909451036435));
#92652=CARTESIAN_POINT('Ctrl Pts',(0.353176714548785,29.4140237118823,56.9708556847076));
#92653=CARTESIAN_POINT('Ctrl Pts',(0.357249364820897,29.3428506238397,56.9468313383321));
#92654=CARTESIAN_POINT('Ctrl Pts',(0.361114530947594,29.2753035007984,56.9240309298458));
#92655=CARTESIAN_POINT('Ctrl Pts',(0.364979697074291,29.2088729566203,56.8976868836698));
#92656=CARTESIAN_POINT('Ctrl Pts',(0.368844863200987,29.1439519288621,56.8679344909287));
#92657=CARTESIAN_POINT('Ctrl Pts',(0.372707539625806,29.0790727192302,56.838201262846));
#92658=CARTESIAN_POINT('Ctrl Pts',(0.376570216050625,29.0157015340332,56.8050642490638));
#92659=CARTESIAN_POINT('Ctrl Pts',(0.380432892475445,28.9542116974909,56.7687069821865));
#92660=CARTESIAN_POINT('Ctrl Pts',(0.384294627206833,28.8927368517396,56.7323585789559));
#92661=CARTESIAN_POINT('Ctrl Pts',(0.388156361938221,28.8331428604117,56.6927917271036));
#92662=CARTESIAN_POINT('Ctrl Pts',(0.39201809666961,28.7757773515059,56.6502352769875));
#92663=CARTESIAN_POINT('Ctrl Pts',(0.392646470203042,28.7664429538749,56.6433105789464));
#92664=CARTESIAN_POINT('Ctrl Pts',(0.393274843736474,28.7571674975787,56.6363068178906));
#92665=CARTESIAN_POINT('Ctrl Pts',(0.393903217269906,28.7479524050421,56.6292250864936));
#92666=CARTESIAN_POINT('',(0.,30.5301702171886,53.0148256743283));
#92667=CARTESIAN_POINT('Ctrl Pts',(-8.32667268468867E-16,30.5301702171886,
53.0148256743283));
#92668=CARTESIAN_POINT('Ctrl Pts',(0.037045090279519,31.1902723495278,53.1911157292334));
#92669=CARTESIAN_POINT('Ctrl Pts',(0.0856865365995149,31.9249421915379,
53.8871678923641));
#92670=CARTESIAN_POINT('Ctrl Pts',(0.13432798291951,32.0542927425914,54.7833750251074));
#92671=CARTESIAN_POINT('Ctrl Pts',(0.145924338959986,32.0526761052044,54.9976298288387));
#92672=CARTESIAN_POINT('',(5.304521544236E-9,29.4696598908744,53.0148710542757));
#92673=CARTESIAN_POINT('Origin',(0.,30.,55.));
#92674=CARTESIAN_POINT('',(0.204074719418398,32.0547494571313,55.0014936260708));
#92675=CARTESIAN_POINT('Ctrl Pts',(5.30452171076945E-9,29.4696598908744,
53.0148710542757));
#92676=CARTESIAN_POINT('Ctrl Pts',(0.00385890399912051,29.5379947425062,
52.9966149542125));
#92677=CARTESIAN_POINT('Ctrl Pts',(0.00771780269371889,29.6074108442032,
52.9818547624561));
#92678=CARTESIAN_POINT('Ctrl Pts',(0.0115767013883177,29.6775162317845,
52.9707139724185));
#92679=CARTESIAN_POINT('Ctrl Pts',(0.0154298333236881,29.7475168534927,
52.9595898312383));
#92680=CARTESIAN_POINT('Ctrl Pts',(0.0192829652590586,29.8182042381468,
52.9520744330023));
#92681=CARTESIAN_POINT('Ctrl Pts',(0.023136097194429,29.8891730296929,52.9482410119235));
#92682=CARTESIAN_POINT('Ctrl Pts',(0.0269847084857915,29.9600585578971,
52.9444120883633));
#92683=CARTESIAN_POINT('Ctrl Pts',(0.0308333197771542,30.0312243517176,
52.9442565885634));
#92684=CARTESIAN_POINT('Ctrl Pts',(0.0346819310685167,30.1022584494044,
52.9477961183095));
#92685=CARTESIAN_POINT('Ctrl Pts',(0.0385281380490834,30.1732481705524,
52.9513334368348));
#92686=CARTESIAN_POINT('Ctrl Pts',(0.0423743450296501,30.2441058718704,
52.9585611814656));
#92687=CARTESIAN_POINT('Ctrl Pts',(0.0462205520102168,30.3144196125068,
52.9694488753614));
#92688=CARTESIAN_POINT('Ctrl Pts',(0.0500656609004903,30.3847132786032,
52.9803334608257));
#92689=CARTESIAN_POINT('Ctrl Pts',(0.053910769790764,30.4544628096774,52.994875846421));
#92690=CARTESIAN_POINT('Ctrl Pts',(0.0577558786810375,30.5232631732663,
53.0129939069033));
#92691=CARTESIAN_POINT('Ctrl Pts',(0.0616011941145184,30.5920672325237,
53.0311129406122));
#92692=CARTESIAN_POINT('Ctrl Pts',(0.0654465095479991,30.6599215512192,
53.0528079035498));
#92693=CARTESIAN_POINT('Ctrl Pts',(0.06929182498148,30.7264347704545,53.0779463881633));
#92694=CARTESIAN_POINT('Ctrl Pts',(0.0731411148383938,30.793016736117,53.103110855296));
#92695=CARTESIAN_POINT('Ctrl Pts',(0.076990404695308,30.8582543783197,53.1317257734965));
#92696=CARTESIAN_POINT('Ctrl Pts',(0.0808396945522218,30.9217758215303,
53.163610363419));
#92697=CARTESIAN_POINT('Ctrl Pts',(0.084691250721741,30.9853346637036,53.1955137257517));
#92698=CARTESIAN_POINT('Ctrl Pts',(0.08854280689126,31.047174871546,53.2306903488843));
#92699=CARTESIAN_POINT('Ctrl Pts',(0.0923943630607791,31.1069511199342,
53.2689145657778));
#92700=CARTESIAN_POINT('Ctrl Pts',(0.0962523586056887,31.1668273075901,
53.3072026893289));
#92701=CARTESIAN_POINT('Ctrl Pts',(0.100110354150598,31.2246322528145,53.3485482903));
#92702=CARTESIAN_POINT('Ctrl Pts',(0.103968349695508,31.2800521355636,53.3926841963263));
#92703=CARTESIAN_POINT('Ctrl Pts',(0.105632531586408,31.3039580121239,53.411722625659));
#92704=CARTESIAN_POINT('Ctrl Pts',(0.107296713477309,31.3274205505818,53.4312797685466));
#92705=CARTESIAN_POINT('Ctrl Pts',(0.108960895368209,31.3504167214721,53.4513321076265));
#92706=CARTESIAN_POINT('Ctrl Pts',(0.1129239713703,31.4051797095168,53.4990846665434));
#92707=CARTESIAN_POINT('Ctrl Pts',(0.116887047372392,31.4575298680422,53.5498532961102));
#92708=CARTESIAN_POINT('Ctrl Pts',(0.120850123374483,31.5071127270913,53.6033580307253));
#92709=CARTESIAN_POINT('Ctrl Pts',(0.124661299696715,31.5547951380006,53.6548119966813));
#92710=CARTESIAN_POINT('Ctrl Pts',(0.128472476018948,31.5999181155289,53.7087957560177));
#92711=CARTESIAN_POINT('Ctrl Pts',(0.13228365234118,31.6421997492177,53.7650192122266));
#92712=CARTESIAN_POINT('Ctrl Pts',(0.136091341570936,31.6844426966968,53.8211912259479));
#92713=CARTESIAN_POINT('Ctrl Pts',(0.139899030800692,31.7238491543833,53.8795984771563));
#92714=CARTESIAN_POINT('Ctrl Pts',(0.143706720030447,31.7601762542011,53.9399164577041));
#92715=CARTESIAN_POINT('Ctrl Pts',(0.147512279769376,31.7964830377006,54.0002007047776));
#92716=CARTESIAN_POINT('Ctrl Pts',(0.151317839508305,31.8297136215381,54.062393134388));
#92717=CARTESIAN_POINT('Ctrl Pts',(0.155123399247234,31.8596685075762,54.1261403977586));
#92718=CARTESIAN_POINT('Ctrl Pts',(0.158928184040522,31.8896172937472,54.1898746799472));
#92719=CARTESIAN_POINT('Ctrl Pts',(0.162732968833809,31.9162914953339,54.2551627143676));
#92720=CARTESIAN_POINT('Ctrl Pts',(0.166537753627097,31.9395384961683,54.3216284319187));
#92721=CARTESIAN_POINT('Ctrl Pts',(0.170345033965938,31.9628007446324,54.3881377441104));
#92722=CARTESIAN_POINT('Ctrl Pts',(0.174152314304778,31.9826311393778,54.455825808995));
#92723=CARTESIAN_POINT('Ctrl Pts',(0.177959594643619,31.9989264298968,54.5242997894053));
#92724=CARTESIAN_POINT('Ctrl Pts',(0.18176838555138,32.0152281857027,54.5928009374148));
#92725=CARTESIAN_POINT('Ctrl Pts',(0.185577176459142,32.0279919539674,54.6620881300336));
#92726=CARTESIAN_POINT('Ctrl Pts',(0.189385967366902,32.0371658013398,54.7317593238308));
#92727=CARTESIAN_POINT('Ctrl Pts',(0.193199808432185,32.046351812513,54.8015228961576));
#92728=CARTESIAN_POINT('Ctrl Pts',(0.197013649497467,32.0519383688091,54.8716709875907));
#92729=CARTESIAN_POINT('Ctrl Pts',(0.20082749056275,32.0539255509878,54.9417986812918));
#92730=CARTESIAN_POINT('Ctrl Pts',(0.201909900181299,32.0544895349261,54.9617016842984));
#92731=CARTESIAN_POINT('Ctrl Pts',(0.202992309799848,32.0547639158599,54.9816030621975));
#92732=CARTESIAN_POINT('Ctrl Pts',(0.204074719418398,32.0547494571313,55.0014936260708));
#92733=CARTESIAN_POINT('Ctrl Pts',(0.204074719462323,32.0547494571307,55.001493626878));
#92734=CARTESIAN_POINT('Ctrl Pts',(0.209415201710472,32.0546781194191,55.099631338747));
#92735=CARTESIAN_POINT('Ctrl Pts',(0.214755683958621,32.0475753669382,55.1975148182993));
#92736=CARTESIAN_POINT('Ctrl Pts',(0.22009616620677,32.0335530902504,55.2943796725878));
#92737=CARTESIAN_POINT('Ctrl Pts',(0.223961018827296,32.0234053114012,55.3644797812556));
#92738=CARTESIAN_POINT('Ctrl Pts',(0.227825871447822,32.0096082627772,55.4341947647113));
#92739=CARTESIAN_POINT('Ctrl Pts',(0.231690724068348,31.9922030861659,55.5031147244626));
#92740=CARTESIAN_POINT('Ctrl Pts',(0.235549750404866,31.9748241479425,55.5719307870415));
#92741=CARTESIAN_POINT('Ctrl Pts',(0.239408776741384,31.9538479958985,55.6399537365013));
#92742=CARTESIAN_POINT('Ctrl Pts',(0.243267803077902,31.9293672381135,55.7067811705148));
#92743=CARTESIAN_POINT('Ctrl Pts',(0.247122226949458,31.9049156772866,55.7735289028375));
#92744=CARTESIAN_POINT('Ctrl Pts',(0.250976650821015,31.8769679793644,55.8390834967379));
#92745=CARTESIAN_POINT('Ctrl Pts',(0.254831074692571,31.8456668085387,55.9030568057207));
#92746=CARTESIAN_POINT('Ctrl Pts',(0.258683026364569,31.8143857140574,55.9669890826863));
#92747=CARTESIAN_POINT('Ctrl Pts',(0.262534978036566,31.7797556271541,56.0293416503832));
#92748=CARTESIAN_POINT('Ctrl Pts',(0.266386929708563,31.7419670894156,56.0897468613825));
#92749=CARTESIAN_POINT('Ctrl Pts',(0.270237707179487,31.7041900708614,56.1501336588944));
#92750=CARTESIAN_POINT('Ctrl Pts',(0.27408848465041,31.6632567708552,56.2085738654515));
#92751=CARTESIAN_POINT('Ctrl Pts',(0.277939262121334,31.6194025140626,56.264726476337));
#92752=CARTESIAN_POINT('Ctrl Pts',(0.28179016173665,31.5755468662387,56.3208808683503));
#92753=CARTESIAN_POINT('Ctrl Pts',(0.285641061351966,31.5287703791993,56.3747471381674));
#92754=CARTESIAN_POINT('Ctrl Pts',(0.289491960967283,31.4793492625247,56.4260165924588));
#92755=CARTESIAN_POINT('Ctrl Pts',(0.293346883174129,31.4298765212986,56.4773396020471));
#92756=CARTESIAN_POINT('Ctrl Pts',(0.297201805380976,31.377753974451,56.5260600297737));
#92757=CARTESIAN_POINT('Ctrl Pts',(0.301056727587822,31.3232947326731,56.5719060445776));
#92758=CARTESIAN_POINT('Ctrl Pts',(0.30491382072567,31.2688048217274,56.61777787794));
#92759=CARTESIAN_POINT('Ctrl Pts',(0.308770913863518,31.2119759850091,56.6607717822148));
#92760=CARTESIAN_POINT('Ctrl Pts',(0.312628007001366,31.153152247426,56.7006579481943));
#92761=CARTESIAN_POINT('Ctrl Pts',(0.316491882785907,31.0942250690871,56.7406142534632));
#92762=CARTESIAN_POINT('Ctrl Pts',(0.320355758570448,31.0332964030478,56.7774516576836));
#92763=CARTESIAN_POINT('Ctrl Pts',(0.324219634354988,30.9707362862754,56.8109855397016));
#92764=CARTESIAN_POINT('Ctrl Pts',(0.326556901918436,30.9328935242791,56.8312702639235));
#92765=CARTESIAN_POINT('Ctrl Pts',(0.328894169481882,30.8944542432968,56.8503471227924));
#92766=CARTESIAN_POINT('Ctrl Pts',(0.331231437045329,30.8555035810296,56.8681839270654));
#92767=CARTESIAN_POINT('Ctrl Pts',(0.335101212782371,30.7910136055811,56.8977160326239));
#92768=CARTESIAN_POINT('Ctrl Pts',(0.338970988519412,30.7248666075646,56.9239626367947));
#92769=CARTESIAN_POINT('Ctrl Pts',(0.342840764256454,30.6574305658347,56.9467364006476));
#92770=CARTESIAN_POINT('Ctrl Pts',(0.346704775982027,30.5900949697494,56.9694762430939));
#92771=CARTESIAN_POINT('Ctrl Pts',(0.3505687877076,30.52147459751,56.9887533590595));
#92772=CARTESIAN_POINT('Ctrl Pts',(0.354432799433173,30.4519589210478,57.0044277727534));
#92773=CARTESIAN_POINT('Ctrl Pts',(0.358292277119959,30.3825248144139,57.0200837940602));
#92774=CARTESIAN_POINT('Ctrl Pts',(0.362151754806745,30.3121979617338,57.0321454040004));
#92775=CARTESIAN_POINT('Ctrl Pts',(0.366011232493531,30.2413829000894,57.0405224473268));
#92776=CARTESIAN_POINT('Ctrl Pts',(0.369868277554051,30.1706124731322,57.0488942106082));
#92777=CARTESIAN_POINT('Ctrl Pts',(0.373725322614572,30.0993549288082,57.0535859579957));
#92778=CARTESIAN_POINT('Ctrl Pts',(0.377582367675092,30.0280234515252,57.0545588939392));
#92779=CARTESIAN_POINT('Ctrl Pts',(0.381438270602589,29.9567130966389,57.0555315417807));
#92780=CARTESIAN_POINT('Ctrl Pts',(0.385294173530085,29.8853293375297,57.0527875577745));
#92781=CARTESIAN_POINT('Ctrl Pts',(0.389150076457581,29.8142871840368,57.0463402240309));
#92782=CARTESIAN_POINT('Ctrl Pts',(0.393006126129889,29.7432423268796,57.03989264492));
#92783=CARTESIAN_POINT('Ctrl Pts',(0.396862175802196,29.6725395845461,57.0297414823329));
#92784=CARTESIAN_POINT('Ctrl Pts',(0.400718225474503,29.6025889352621,57.0159518863614));
#92785=CARTESIAN_POINT('Ctrl Pts',(0.40457829999136,29.5325652733063,57.0021478971675));
#92786=CARTESIAN_POINT('Ctrl Pts',(0.408438374508216,29.4632957488624,56.9846979875983));
#92787=CARTESIAN_POINT('Ctrl Pts',(0.412298449025072,29.3951793406887,56.963718292569));
#92788=CARTESIAN_POINT('Ctrl Pts',(0.416160703621026,29.3270244619733,56.9427267487025));
#92789=CARTESIAN_POINT('Ctrl Pts',(0.420022958216979,29.2600244522189,56.9182016177523));
#92790=CARTESIAN_POINT('Ctrl Pts',(0.423885212812933,29.1945597327353,56.8903077893212));
#92791=CARTESIAN_POINT('Ctrl Pts',(0.42775420848448,29.1289807528859,56.86236527575));
#92792=CARTESIAN_POINT('Ctrl Pts',(0.431623204156027,29.0649428496908,56.8310425391956));
#92793=CARTESIAN_POINT('Ctrl Pts',(0.435492199827575,29.002802575406,56.7965508227944));
#92794=CARTESIAN_POINT('Ctrl Pts',(0.437783702513013,28.9659985524797,56.7761223014238));
#92795=CARTESIAN_POINT('Ctrl Pts',(0.440075205198452,28.929859670375,56.754582989294));
#92796=CARTESIAN_POINT('Ctrl Pts',(0.44236670788389,28.894454859707,56.7319836908223));
#92797=CARTESIAN_POINT('Ctrl Pts',(0.445616969960976,28.8442367586366,56.6999288984549));
#92798=CARTESIAN_POINT('Ctrl Pts',(0.448867232038062,28.7953317342127,56.6656357553635));
#92799=CARTESIAN_POINT('Ctrl Pts',(0.452117494115148,28.7479524050421,56.6292250864936));
#92800=CARTESIAN_POINT('Origin',(-1.54592528053767,30.,125.));
#92801=CARTESIAN_POINT('',(9.49394826790656,28.7479590808042,126.629230216746));
#92802=CARTESIAN_POINT('',(9.55204643235015,28.7459520887588,126.631857121398));
#92803=CARTESIAN_POINT('',(-1.54592528053767,28.7479590808042,126.629230216746));
#92804=CARTESIAN_POINT('',(10.,32.0533758325287,124.92486510207));
#92805=CARTESIAN_POINT('Ctrl Pts',(9.55204643235015,28.7459520887588,126.631857121398));
#92806=CARTESIAN_POINT('Ctrl Pts',(9.55318392711536,28.7293562993152,126.619178672138));
#92807=CARTESIAN_POINT('Ctrl Pts',(9.59136651216008,28.1793709776662,126.184464664884));
#92808=CARTESIAN_POINT('Ctrl Pts',(9.66659418748432,27.5870688000586,124.728220627396));
#92809=CARTESIAN_POINT('Ctrl Pts',(9.77772945832287,28.9190809534992,122.823596121193));
#92810=CARTESIAN_POINT('Ctrl Pts',(9.88886472916145,31.2434480688362,122.91515608673));
#92811=CARTESIAN_POINT('Ctrl Pts',(9.96295490972048,32.0283922803563,124.242084880697));
#92812=CARTESIAN_POINT('Ctrl Pts',(10.,32.0533758325287,124.92486510207));
#92813=CARTESIAN_POINT('',(9.99999184700732,31.8181879239729,125.959175310784));
#92814=CARTESIAN_POINT('Origin',(10.,30.,125.));
#92815=CARTESIAN_POINT('',(9.94592528057841,32.0547499998285,125.000026545906));
#92816=CARTESIAN_POINT('Ctrl Pts',(9.94592528057841,32.0547499998285,125.000026545906));
#92817=CARTESIAN_POINT('Ctrl Pts',(9.94992641744506,32.054749041194,125.074228358377));
#92818=CARTESIAN_POINT('Ctrl Pts',(9.9539275543117,32.0507243787667,125.148359152486));
#92819=CARTESIAN_POINT('Ctrl Pts',(9.95792869117834,32.0427247640096,125.221975451349));
#92820=CARTESIAN_POINT('Ctrl Pts',(9.96193973980718,32.0347053323151,125.295774115194));
#92821=CARTESIAN_POINT('Ctrl Pts',(9.96595078843603,32.0226913261354,125.369055309329));
#92822=CARTESIAN_POINT('Ctrl Pts',(9.96996183706487,32.0067830122535,125.441383624788));
#92823=CARTESIAN_POINT('Ctrl Pts',(9.97397827600221,31.9908533197428,125.513809139749));
#92824=CARTESIAN_POINT('Ctrl Pts',(9.97799471493955,31.9710190057058,125.585278810454));
#92825=CARTESIAN_POINT('Ctrl Pts',(9.98201115387689,31.9474300268147,125.65537306411));
#92826=CARTESIAN_POINT('Ctrl Pts',(9.98603789130173,31.9237805637962,125.725647045331));
#92827=CARTESIAN_POINT('Ctrl Pts',(9.99006462872657,31.8963573593182,125.794538163325));
#92828=CARTESIAN_POINT('Ctrl Pts',(9.99409136615141,31.8653583165232,125.861647209406));
#92829=CARTESIAN_POINT('Ctrl Pts',(9.99605728180693,31.8502241031124,125.894410886398));
#92830=CARTESIAN_POINT('Ctrl Pts',(9.99802319746244,31.8342382610577,125.926750191666));
#92831=CARTESIAN_POINT('Ctrl Pts',(9.99998911311796,31.8174276116447,125.958621113335));
#92832=CARTESIAN_POINT('Ctrl Pts',(9.49394826790656,28.7479590808042,126.629230216746));
#92833=CARTESIAN_POINT('Ctrl Pts',(9.49780412631023,28.6914091793736,126.585772398545));
#92834=CARTESIAN_POINT('Ctrl Pts',(9.50165998471389,28.6371086349064,126.539354686076));
#92835=CARTESIAN_POINT('Ctrl Pts',(9.50551584311756,28.5853742599313,126.490245475764));
#92836=CARTESIAN_POINT('Ctrl Pts',(9.50937196777623,28.5336363125906,126.441132874359));
#92837=CARTESIAN_POINT('Ctrl Pts',(9.5132280924349,28.4844652370948,126.389328742153));
#92838=CARTESIAN_POINT('Ctrl Pts',(9.51708421709357,28.4381416398565,126.335138953574));
#92839=CARTESIAN_POINT('Ctrl Pts',(9.52094443867069,28.3917688263668,126.280891591351));
#92840=CARTESIAN_POINT('Ctrl Pts',(9.52480466024782,28.3482498452297,126.224253883872));
#92841=CARTESIAN_POINT('Ctrl Pts',(9.52866488182495,28.3078249672196,126.165564764796));
#92842=CARTESIAN_POINT('Ctrl Pts',(9.53252739110166,28.2673761320416,126.106840864537));
#92843=CARTESIAN_POINT('Ctrl Pts',(9.53638990037837,28.2300253039295,126.046063546692));
#92844=CARTESIAN_POINT('Ctrl Pts',(9.54025240965508,28.1959678988961,125.983598363503));
#92845=CARTESIAN_POINT('Ctrl Pts',(9.54412154523635,28.1618520668863,125.921026018545));
#92846=CARTESIAN_POINT('Ctrl Pts',(9.54799068081762,28.1310411454322,125.856760466181));
#92847=CARTESIAN_POINT('Ctrl Pts',(9.55185981639889,28.1036830108545,125.791188624272));
#92848=CARTESIAN_POINT('Ctrl Pts',(9.55378430830463,28.0900751887854,125.758573463509));
#92849=CARTESIAN_POINT('Ctrl Pts',(9.55570880021036,28.077320825225,125.725635382705));
#92850=CARTESIAN_POINT('Ctrl Pts',(9.5576332921161,28.0654334809787,125.692423241942));
#92851=CARTESIAN_POINT('Ctrl Pts',(9.56150282286142,28.0415318766622,125.625644369338));
#92852=CARTESIAN_POINT('Ctrl Pts',(9.56537235360673,28.0210453328819,125.557496028693));
#92853=CARTESIAN_POINT('Ctrl Pts',(9.56924188435204,28.0041289561955,125.488360869648));
#92854=CARTESIAN_POINT('Ctrl Pts',(9.57310565989046,27.9872377394715,125.419328536286));
#92855=CARTESIAN_POINT('Ctrl Pts',(9.57696943542886,27.973906264106,125.349312765815));
#92856=CARTESIAN_POINT('Ctrl Pts',(9.58083321096727,27.9642406054079,125.278713562336));
#92857=CARTESIAN_POINT('Ctrl Pts',(9.58469246665209,27.9545862536197,125.208196945969));
#92858=CARTESIAN_POINT('Ctrl Pts',(9.58855172233691,27.9485892660344,125.13709873111));
#92859=CARTESIAN_POINT('Ctrl Pts',(9.59241097802173,27.9463047893954,125.06582966231));
#92860=CARTESIAN_POINT('Ctrl Pts',(9.59626780995489,27.9440217474901,124.994605353054));
#92861=CARTESIAN_POINT('Ctrl Pts',(9.60012464188805,27.9454466061684,124.923210886997));
#92862=CARTESIAN_POINT('Ctrl Pts',(9.60398147382121,27.9505825998578,124.852061220452));
#92863=CARTESIAN_POINT('Ctrl Pts',(9.6078371727826,27.9557170848125,124.780932454626));
#92864=CARTESIAN_POINT('Ctrl Pts',(9.61169287174399,27.9645605055126,124.710048829665));
#92865=CARTESIAN_POINT('Ctrl Pts',(9.61554857070539,27.9770640538327,124.63982265451));
#92866=CARTESIAN_POINT('Ctrl Pts',(9.61940442586884,27.9895681086965,124.569593634352));
#92867=CARTESIAN_POINT('Ctrl Pts',(9.6232602810323,28.0057324982751,124.500022594616));
#92868=CARTESIAN_POINT('Ctrl Pts',(9.62711613619576,28.0254571691084,124.431512382303));
#92869=CARTESIAN_POINT('Ctrl Pts',(9.63097603195377,28.045202509649,124.362930377358));
#92870=CARTESIAN_POINT('Ctrl Pts',(9.63483592771178,28.068515444427,124.295411886582));
#92871=CARTESIAN_POINT('Ctrl Pts',(9.6386958234698,28.0952460660982,124.229344425969));
#92872=CARTESIAN_POINT('Ctrl Pts',(9.64255790792351,28.1219918449655,124.163239502798));
#92873=CARTESIAN_POINT('Ctrl Pts',(9.64641999237723,28.1521589631565,124.098587688006));
#92874=CARTESIAN_POINT('Ctrl Pts',(9.65028207683095,28.1855505308414,124.035753824809));
#92875=CARTESIAN_POINT('Ctrl Pts',(9.65415091781318,28.2190005154465,123.972810036831));
#92876=CARTESIAN_POINT('Ctrl Pts',(9.65801975879542,28.2556859620026,123.911690966773));
#92877=CARTESIAN_POINT('Ctrl Pts',(9.66188859977765,28.2953658457551,123.852733700189));
#92878=CARTESIAN_POINT('Ctrl Pts',(9.66418192083665,28.31888676932,123.817785781249));
#92879=CARTESIAN_POINT('Ctrl Pts',(9.66647524189564,28.3434590555142,123.783596865762));
#92880=CARTESIAN_POINT('Ctrl Pts',(9.66876856295463,28.3690260367847,123.750231423897));
#92881=CARTESIAN_POINT('Ctrl Pts',(9.6726337119706,28.4121164676299,123.693997516183));
#92882=CARTESIAN_POINT('Ctrl Pts',(9.67649886098656,28.4582040821038,123.63988326682));
#92883=CARTESIAN_POINT('Ctrl Pts',(9.68036401000252,28.5070524760954,123.588226203187));
#92884=CARTESIAN_POINT('Ctrl Pts',(9.68422338351675,28.5558278783387,123.53664632816));
#92885=CARTESIAN_POINT('Ctrl Pts',(9.68808275703098,28.6073555402847,123.48751670204));
#92886=CARTESIAN_POINT('Ctrl Pts',(9.69194213054521,28.6613578349713,123.441143137903));
#92887=CARTESIAN_POINT('Ctrl Pts',(9.69579697527658,28.7152967606512,123.394823990836));
#92888=CARTESIAN_POINT('Ctrl Pts',(9.69965182000794,28.7717041838798,123.351254797824));
#92889=CARTESIAN_POINT('Ctrl Pts',(9.70350666473931,28.8302657844179,123.310704458244));
#92890=CARTESIAN_POINT('Ctrl Pts',(9.70735908251337,28.8887905153765,123.270179648601));
#92891=CARTESIAN_POINT('Ctrl Pts',(9.71121150028743,28.9494663337615,123.232670198377));
#92892=CARTESIAN_POINT('Ctrl Pts',(9.71506391806149,29.0119471850551,123.198403708546));
#92893=CARTESIAN_POINT('Ctrl Pts',(9.71891520608934,29.0744097134385,123.164147267583));
#92894=CARTESIAN_POINT('Ctrl Pts',(9.72276649411718,29.1386757972613,123.133132133113));
#92895=CARTESIAN_POINT('Ctrl Pts',(9.72661778214502,29.2043733503988,123.105540763979));
#92896=CARTESIAN_POINT('Ctrl Pts',(9.73046923603155,29.2700737328518,123.077948206602));
#92897=CARTESIAN_POINT('Ctrl Pts',(9.73432068991807,29.3372052572478,123.053779893772));
#92898=CARTESIAN_POINT('Ctrl Pts',(9.7381721438046,29.4053759770119,123.033170105529));
#92899=CARTESIAN_POINT('Ctrl Pts',(9.74202768323323,29.4736190108565,123.012538454851));
#92900=CARTESIAN_POINT('Ctrl Pts',(9.74588322266187,29.5429029735657,122.995473005168));
#92901=CARTESIAN_POINT('Ctrl Pts',(9.7497387620905,29.6128217507138,122.982057838842));
#92902=CARTESIAN_POINT('Ctrl Pts',(9.75359650888248,29.6827805575773,122.9686349921));
#92903=CARTESIAN_POINT('Ctrl Pts',(9.75745425567446,29.7533744198051,122.95886665521));
#92904=CARTESIAN_POINT('Ctrl Pts',(9.76131200246644,29.8241908068457,122.952785138267));
#92905=CARTESIAN_POINT('Ctrl Pts',(9.76517658251364,29.8951326314726,122.946692849088));
#92906=CARTESIAN_POINT('Ctrl Pts',(9.76904116256084,29.9662972811123,122.944300434156));
#92907=CARTESIAN_POINT('Ctrl Pts',(9.77290574260804,30.0372716269973,122.945588067519));
#92908=CARTESIAN_POINT('Ctrl Pts',(9.77523843966978,30.0801124133396,122.946365295193));
#92909=CARTESIAN_POINT('Ctrl Pts',(9.77757113673153,30.1228839281888,122.94848231543));
#92910=CARTESIAN_POINT('Ctrl Pts',(9.77990383379327,30.1654967268378,122.951925685942));
#92911=CARTESIAN_POINT('Ctrl Pts',(9.7837796915926,30.2362993830008,122.957646966545));
#92912=CARTESIAN_POINT('Ctrl Pts',(9.78765554939193,30.3069415042382,122.967055082892));
#92913=CARTESIAN_POINT('Ctrl Pts',(9.79153140719126,30.3770094735591,122.980133316442));
#92914=CARTESIAN_POINT('Ctrl Pts',(9.79540148372107,30.4469729287734,122.993192042364));
#92915=CARTESIAN_POINT('Ctrl Pts',(9.79927156025088,30.5163634602671,123.009909929784));
#92916=CARTESIAN_POINT('Ctrl Pts',(9.80314163678069,30.5847718858269,123.030218437479));
#92917=CARTESIAN_POINT('Ctrl Pts',(9.8070071246871,30.6530992017497,123.05050286604));
#92918=CARTESIAN_POINT('Ctrl Pts',(9.8108726125935,30.7204462633365,123.074369320275));
#92919=CARTESIAN_POINT('Ctrl Pts',(9.8147381004999,30.7864151190072,123.101698437261));
#92920=CARTESIAN_POINT('Ctrl Pts',(9.81860111864384,30.8523418254312,123.129010092952));
#92921=CARTESIAN_POINT('Ctrl Pts',(9.82246413678777,30.916891627173,123.159779836718));
#92922=CARTESIAN_POINT('Ctrl Pts',(9.82632715493171,30.9796841247431,123.193839271209));
#92923=CARTESIAN_POINT('Ctrl Pts',(9.83018898513618,31.0424573126224,123.227888231883));
#92924=CARTESIAN_POINT('Ctrl Pts',(9.83405081534065,31.1034738441465,123.265224644079));
#92925=CARTESIAN_POINT('Ctrl Pts',(9.83791264554513,31.1623771550894,123.305633772815));
#92926=CARTESIAN_POINT('Ctrl Pts',(9.84177456797417,31.2212818727055,123.346043866563));
#92927=CARTESIAN_POINT('Ctrl Pts',(9.84563649040322,31.278072871718,123.389526546977));
#92928=CARTESIAN_POINT('Ctrl Pts',(9.84949841283227,31.3324232868658,123.435824259516));
#92929=CARTESIAN_POINT('Ctrl Pts',(9.85336423707635,31.3868286138537,123.482168748011));
#92930=CARTESIAN_POINT('Ctrl Pts',(9.85723006132043,31.4387880652972,123.531333631963));
#92931=CARTESIAN_POINT('Ctrl Pts',(9.86109588556451,31.4880092499235,123.583022218014));
#92932=CARTESIAN_POINT('Ctrl Pts',(9.86496382883615,31.5372574148367,123.634739136842));
#92933=CARTESIAN_POINT('Ctrl Pts',(9.86883177210779,31.5837640090157,123.68898214469));
#92934=CARTESIAN_POINT('Ctrl Pts',(9.87269971537943,31.6272765958774,123.745421009657));
#92935=CARTESIAN_POINT('Ctrl Pts',(9.87657424252348,31.6708632482824,123.801955942808));
#92936=CARTESIAN_POINT('Ctrl Pts',(9.88044876966754,31.7114454426296,123.860693797643));
#92937=CARTESIAN_POINT('Ctrl Pts',(9.88432329681159,31.7488141688587,123.921275491472));
#92938=CARTESIAN_POINT('Ctrl Pts',(9.88656189941833,31.7704048623388,123.956278043444));
#92939=CARTESIAN_POINT('Ctrl Pts',(9.88880050202507,31.7909236763886,123.991895640431));
#92940=CARTESIAN_POINT('Ctrl Pts',(9.89103910463182,31.8103375264705,124.0280557615));
#92941=CARTESIAN_POINT('Ctrl Pts',(9.89510077167261,31.8455615518402,124.093663820517));
#92942=CARTESIAN_POINT('Ctrl Pts',(9.8991624387134,31.8772691212244,124.161289087594));
#92943=CARTESIAN_POINT('Ctrl Pts',(9.90322410575419,31.9052369260509,124.230539267986));
#92944=CARTESIAN_POINT('Ctrl Pts',(9.90727424704382,31.9331253669229,124.299592937846));
#92945=CARTESIAN_POINT('Ctrl Pts',(9.91132438833347,31.9572950211504,124.370261955961));
#92946=CARTESIAN_POINT('Ctrl Pts',(9.9153745296231,31.9775692252997,124.442131268444));
#92947=CARTESIAN_POINT('Ctrl Pts',(9.91941770625547,31.9978085657558,124.513876993849));
#92948=CARTESIAN_POINT('Ctrl Pts',(9.92346088288783,32.0141656631297,124.586818512363));
#92949=CARTESIAN_POINT('Ctrl Pts',(9.9275040595202,32.0265123954516,124.660522351868));
#92950=CARTESIAN_POINT('Ctrl Pts',(9.93153868618936,32.0388330185734,124.73407033246));
#92951=CARTESIAN_POINT('Ctrl Pts',(9.93557331285852,32.047160093344,124.808377016412));
#92952=CARTESIAN_POINT('Ctrl Pts',(9.93960793952768,32.0514160614572,124.882996985956));
#92953=CARTESIAN_POINT('Ctrl Pts',(9.94171371986435,32.0536373658557,124.921943158049));
#92954=CARTESIAN_POINT('Ctrl Pts',(9.94381950020102,32.0547505043392,124.96097446499));
#92955=CARTESIAN_POINT('Ctrl Pts',(9.94592528053769,32.0547499998285,125.00002654515));
#92956=CARTESIAN_POINT('Origin',(-1.54592528053767,30.,125.));
#92957=CARTESIAN_POINT('',(8.79398045138579,28.7479590808042,126.629230216746));
#92958=CARTESIAN_POINT('',(8.852020734751,28.7479590808042,126.629230216746));
#92959=CARTESIAN_POINT('',(-1.54592528053767,28.7479590808042,126.629230216746));
#92960=CARTESIAN_POINT('',(9.30407471946232,32.0547491738536,125.001842565591));
#92961=CARTESIAN_POINT('Ctrl Pts',(8.85202073475099,28.7479590808042,126.629230216746));
#92962=CARTESIAN_POINT('Ctrl Pts',(8.85588087637188,28.6913947464198,126.585761307019));
#92963=CARTESIAN_POINT('Ctrl Pts',(8.85974101799276,28.6371344517981,126.539372158411));
#92964=CARTESIAN_POINT('Ctrl Pts',(8.86360115961365,28.5854809162024,126.490346712706));
#92965=CARTESIAN_POINT('Ctrl Pts',(8.86746399129527,28.5337913842206,126.441287102081));
#92966=CARTESIAN_POINT('Ctrl Pts',(8.8713268229769,28.4847125588429,126.389587891694));
#92967=CARTESIAN_POINT('Ctrl Pts',(8.87518965465852,28.4385084505345,126.335567932921));
#92968=CARTESIAN_POINT('Ctrl Pts',(8.87905875237596,28.3922293929087,126.281460346464));
#92969=CARTESIAN_POINT('Ctrl Pts',(8.88292785009341,28.3488346463894,126.225024888472));
#92970=CARTESIAN_POINT('Ctrl Pts',(8.88679694781086,28.3085457296492,126.166610480757));
#92971=CARTESIAN_POINT('Ctrl Pts',(8.88741372907871,28.302123185955,126.157298513192));
#92972=CARTESIAN_POINT('Ctrl Pts',(8.88803051034656,28.2957794736538,126.147936307201));
#92973=CARTESIAN_POINT('Ctrl Pts',(8.8886472916144,28.2895153812363,126.138525331942));
#92974=CARTESIAN_POINT('Ctrl Pts',(8.89251643699301,28.2502199527083,126.079489117112));
#92975=CARTESIAN_POINT('Ctrl Pts',(8.89638558237161,28.2139075453724,126.01830051077));
#92976=CARTESIAN_POINT('Ctrl Pts',(8.90025472775021,28.1808210041849,125.955293328609));
#92977=CARTESIAN_POINT('Ctrl Pts',(8.90411810779598,28.1477837645623,125.892380032136));
#92978=CARTESIAN_POINT('Ctrl Pts',(8.90798148784175,28.1179630737262,125.827653965344));
#92979=CARTESIAN_POINT('Ctrl Pts',(8.91184486788753,28.0915583867166,125.761477623564));
#92980=CARTESIAN_POINT('Ctrl Pts',(8.91570371513117,28.0651846796314,125.695378924744));
#92981=CARTESIAN_POINT('Ctrl Pts',(8.91956256237482,28.0422191944493,125.627833779822));
#92982=CARTESIAN_POINT('Ctrl Pts',(8.92342140961847,28.0228145568944,125.559227401038));
#92983=CARTESIAN_POINT('Ctrl Pts',(8.92727782536573,28.0034221463863,125.490664251785));
#92984=CARTESIAN_POINT('Ctrl Pts',(8.93113424111299,27.9875862638826,125.421041661673));
#92985=CARTESIAN_POINT('Ctrl Pts',(8.93499065686025,27.9754101749661,125.350761461494));
#92986=CARTESIAN_POINT('Ctrl Pts',(8.93884593257506,27.9632376855413,125.280502037526));
#92987=CARTESIAN_POINT('Ctrl Pts',(8.94270120828986,27.9547229246952,125.209585867809));
#92988=CARTESIAN_POINT('Ctrl Pts',(8.94655648400467,27.9499180152724,125.138424775222));
#92989=CARTESIAN_POINT('Ctrl Pts',(8.95041190953726,27.9451129191286,125.067260917283));
#92990=CARTESIAN_POINT('Ctrl Pts',(8.95426733506985,27.94401799116,124.995852602389));
#92991=CARTESIAN_POINT('Ctrl Pts',(8.95812276060244,27.9466333401222,124.924614838314));
#92992=CARTESIAN_POINT('Ctrl Pts',(8.96198222008824,27.9492514255386,124.853302537769));
#92993=CARTESIAN_POINT('Ctrl Pts',(8.96584167957404,27.9555875195432,124.782161630701));
#92994=CARTESIAN_POINT('Ctrl Pts',(8.96970113905983,27.9655896507679,124.711604276319));
#92995=CARTESIAN_POINT('Ctrl Pts',(8.97356278284336,27.9755974427937,124.641006989333));
#92996=CARTESIAN_POINT('Ctrl Pts',(8.97742442662689,27.9892753092108,124.570994389477));
#92997=CARTESIAN_POINT('Ctrl Pts',(8.98128607041042,28.006520213743,124.501967968616));
#92998=CARTESIAN_POINT('Ctrl Pts',(8.98515446867269,28.0237952816842,124.432820812255));
#92999=CARTESIAN_POINT('Ctrl Pts',(8.98902286693495,28.0446497022752,124.364663743452));
#93000=CARTESIAN_POINT('Ctrl Pts',(8.99289126519722,28.0689309111879,124.297881963816));
#93001=CARTESIAN_POINT('Ctrl Pts',(8.99518836428247,28.0833493704573,124.258226180076));
#93002=CARTESIAN_POINT('Ctrl Pts',(8.99748546336772,28.0989752341499,124.219054955029));
#93003=CARTESIAN_POINT('Ctrl Pts',(8.99978256245297,28.1157688523033,124.180444910607));
#93004=CARTESIAN_POINT('Ctrl Pts',(9.00365172648552,28.1440555134024,124.115411322753));
#93005=CARTESIAN_POINT('Ctrl Pts',(9.00752089051807,28.1757684267354,124.051716582142));
#93006=CARTESIAN_POINT('Ctrl Pts',(9.01139005455062,28.2107588361673,123.989745764599));
#93007=CARTESIAN_POINT('Ctrl Pts',(9.01525345479223,28.2456971213151,123.927867263337));
#93008=CARTESIAN_POINT('Ctrl Pts',(9.01911685503385,28.2839029742327,123.867708007108));
#93009=CARTESIAN_POINT('Ctrl Pts',(9.02298025527546,28.3251800113167,123.809632171131));
#93010=CARTESIAN_POINT('Ctrl Pts',(9.02683912487806,28.3664086425036,123.751624441131));
#93011=CARTESIAN_POINT('Ctrl Pts',(9.03069799448066,28.4107010238021,123.695695672289));
#93012=CARTESIAN_POINT('Ctrl Pts',(9.03455686408325,28.4578162883206,123.64218301604));
#93013=CARTESIAN_POINT('Ctrl Pts',(9.03841330350832,28.504901881337,123.58870406014));
#93014=CARTESIAN_POINT('Ctrl Pts',(9.04226974293338,28.5548065102983,123.537638561759));
#93015=CARTESIAN_POINT('Ctrl Pts',(9.04612618235844,28.6072485761315,123.489291214756));
#93016=CARTESIAN_POINT('Ctrl Pts',(9.04998148302309,28.6596751564503,123.440958144147));
#93017=CARTESIAN_POINT('Ctrl Pts',(9.05383678368775,28.7146373291714,123.395341960534));
#93018=CARTESIAN_POINT('Ctrl Pts',(9.05769208435241,28.7718173635003,123.352709808837));
#93019=CARTESIAN_POINT('Ctrl Pts',(9.06154753606142,28.8289996380491,123.310075986883));
#93020=CARTESIAN_POINT('Ctrl Pts',(9.06540298777042,28.8883995559704,123.270426717542));
#93021=CARTESIAN_POINT('Ctrl Pts',(9.06925843947943,28.9496685012271,123.233987172984));
#93022=CARTESIAN_POINT('Ctrl Pts',(9.07311792680895,29.0110015785831,123.197509486028));
#93023=CARTESIAN_POINT('Ctrl Pts',(9.07697741413847,29.0742071702716,123.164248479424));
#93024=CARTESIAN_POINT('Ctrl Pts',(9.08083690146798,29.1389108080243,123.134384025057));
#93025=CARTESIAN_POINT('Ctrl Pts',(9.08469857407678,29.2036510816062,123.104502661145));
#93026=CARTESIAN_POINT('Ctrl Pts',(9.08856024668558,29.2698906385116,123.078021858301));
#93027=CARTESIAN_POINT('Ctrl Pts',(9.09242191929437,29.3372362779288,123.055072800538));
#93028=CARTESIAN_POINT('Ctrl Pts',(9.09629034760057,29.4046997333308,123.032083595174));
#93029=CARTESIAN_POINT('Ctrl Pts',(9.10015877590678,29.47327266706,123.012638603043));
#93030=CARTESIAN_POINT('Ctrl Pts',(9.10402720421298,29.5425487032,122.996818561998));
#93031=CARTESIAN_POINT('Ctrl Pts',(9.10632408057249,29.5836812968778,122.987425424681));
#93032=CARTESIAN_POINT('Ctrl Pts',(9.10862095693201,29.6250615840998,122.979309237482));
#93033=CARTESIAN_POINT('Ctrl Pts',(9.11091783329152,29.6666037127054,122.972478242258));
#93034=CARTESIAN_POINT('Ctrl Pts',(9.11478641228267,29.7365722181084,122.960972945291));
#93035=CARTESIAN_POINT('Ctrl Pts',(9.11865499127382,29.8072742400406,122.953071185289));
#93036=CARTESIAN_POINT('Ctrl Pts',(9.12252357026497,29.8783056996825,122.948856889495));
#93037=CARTESIAN_POINT('Ctrl Pts',(9.12638638331592,29.9492312901799,122.944648874918));
#93038=CARTESIAN_POINT('Ctrl Pts',(9.13024919636687,30.0204848626401,122.944117443783));
#93039=CARTESIAN_POINT('Ctrl Pts',(9.13411200941782,30.0916540559551,122.9472951755));
#93040=CARTESIAN_POINT('Ctrl Pts',(9.13797029147812,30.1627397694472,122.950469179811));
#93041=CARTESIAN_POINT('Ctrl Pts',(9.14182857353843,30.2337408173102,122.957343683396));
#93042=CARTESIAN_POINT('Ctrl Pts',(9.14568685559873,30.3042434075366,122.967899236881));
#93043=CARTESIAN_POINT('Ctrl Pts',(9.14954270758185,30.3747015928353,122.978448142119));
#93044=CARTESIAN_POINT('Ctrl Pts',(9.15339855956497,30.4446614639241,122.992673425752));
#93045=CARTESIAN_POINT('Ctrl Pts',(9.15725441154809,30.5137143999239,123.01050381307));
#93046=CARTESIAN_POINT('Ctrl Pts',(9.16110912573307,30.5827469595445,123.028328938935));
#93047=CARTESIAN_POINT('Ctrl Pts',(9.16496383991805,30.650872645138,123.049756935133));
#93048=CARTESIAN_POINT('Ctrl Pts',(9.16881855410303,30.717694781864,123.074665804961));
#93049=CARTESIAN_POINT('Ctrl Pts',(9.17267342115715,30.7845195686029,123.099575662619));
#93050=CARTESIAN_POINT('Ctrl Pts',(9.17652828821127,30.8500402492908,123.127966496182));
#93051=CARTESIAN_POINT('Ctrl Pts',(9.18038315526539,30.9138786595047,123.159667595731));
#93052=CARTESIAN_POINT('Ctrl Pts',(9.18424206474163,30.977784014129,123.191401938768));
#93053=CARTESIAN_POINT('Ctrl Pts',(9.18810097421787,31.0400031405998,123.226453260751));
#93054=CARTESIAN_POINT('Ctrl Pts',(9.19195988369411,31.1001819112534,123.264604562455));
#93055=CARTESIAN_POINT('Ctrl Pts',(9.19582098141221,31.1603948070156,123.302777498323));
#93056=CARTESIAN_POINT('Ctrl Pts',(9.19968207913031,31.218564647273,123.344053631923));
#93057=CARTESIAN_POINT('Ctrl Pts',(9.20354317684842,31.2743680517039,123.388173821004));
#93058=CARTESIAN_POINT('Ctrl Pts',(9.20741104118738,31.3302692522818,123.432371331255));
#93059=CARTESIAN_POINT('Ctrl Pts',(9.21127890552634,31.383795371967,123.479422527217));
#93060=CARTESIAN_POINT('Ctrl Pts',(9.2151467698653,31.4346582690326,123.529029839325));
#93061=CARTESIAN_POINT('Ctrl Pts',(9.2174488812869,31.4649313205176,123.558555580093));
#93062=CARTESIAN_POINT('Ctrl Pts',(9.21975099270849,31.4942616564072,123.588986141993));
#93063=CARTESIAN_POINT('Ctrl Pts',(9.22205310413008,31.5225954262331,123.620253381771));
#93064=CARTESIAN_POINT('Ctrl Pts',(9.22588174244541,31.5697172795699,123.67225388492));
#93065=CARTESIAN_POINT('Ctrl Pts',(9.22971038076074,31.6142741301639,123.726783950541));
#93066=CARTESIAN_POINT('Ctrl Pts',(9.23353901907606,31.6559786780319,123.783557572097));
#93067=CARTESIAN_POINT('Ctrl Pts',(9.23736240814987,31.6976260470216,123.840253354372));
#93068=CARTESIAN_POINT('Ctrl Pts',(9.24118579722367,31.7364285742198,123.899186198871));
#93069=CARTESIAN_POINT('Ctrl Pts',(9.24500918629747,31.7721371255726,123.960034822378));
#93070=CARTESIAN_POINT('Ctrl Pts',(9.24882867712127,31.8078092692101,124.02082140586));
#93071=CARTESIAN_POINT('Ctrl Pts',(9.25264816794507,31.8403934429899,124.083519468726));
#93072=CARTESIAN_POINT('Ctrl Pts',(9.25646765876886,31.8696831258354,124.147777862605));
#93073=CARTESIAN_POINT('Ctrl Pts',(9.26043491382665,31.9001059355162,124.214522214112));
#93074=CARTESIAN_POINT('Ctrl Pts',(9.26440216888444,31.9269738125268,124.282949638816));
#93075=CARTESIAN_POINT('Ctrl Pts',(9.26836942394223,31.9501078793459,124.352638569721));
#93076=CARTESIAN_POINT('Ctrl Pts',(9.27218609766135,31.9723638683253,124.419682383951));
#93077=CARTESIAN_POINT('Ctrl Pts',(9.27600277138047,31.9911642561016,124.48789314573));
#93078=CARTESIAN_POINT('Ctrl Pts',(9.2798194450996,32.0063997648491,124.556877504392));
#93079=CARTESIAN_POINT('Ctrl Pts',(9.28363614006936,32.0216353584255,124.625862247149));
#93080=CARTESIAN_POINT('Ctrl Pts',(9.28745283503914,32.03330593664,124.69562010812));
#93081=CARTESIAN_POINT('Ctrl Pts',(9.2912695300089,32.0413532894075,124.765747336568));
#93082=CARTESIAN_POINT('Ctrl Pts',(9.29508879757109,32.0494060663859,124.835921833339));
#93083=CARTESIAN_POINT('Ctrl Pts',(9.29890806513328,32.0538307059046,124.906465699354));
#93084=CARTESIAN_POINT('Ctrl Pts',(9.30272733269546,32.0546209489418,124.976971351112));
#93085=CARTESIAN_POINT('Ctrl Pts',(9.30317646161775,32.0547138780173,124.985262502981));
#93086=CARTESIAN_POINT('Ctrl Pts',(9.30362559054003,32.0547566072828,124.993553127999));
#93087=CARTESIAN_POINT('Ctrl Pts',(9.30407471946232,32.0547491738536,125.001842565591));
#93088=CARTESIAN_POINT('Ctrl Pts',(9.30407499487673,32.0541926768234,125.001847148429));
#93089=CARTESIAN_POINT('Ctrl Pts',(9.31377945490737,32.0557826428579,125.180912501179));
#93090=CARTESIAN_POINT('Ctrl Pts',(9.36052900521752,31.9523516367539,126.041729875259));
#93091=CARTESIAN_POINT('Ctrl Pts',(9.443186151042,30.7618134898646,127.294355624062));
#93092=CARTESIAN_POINT('Ctrl Pts',(9.51613883683583,29.2698357256828,127.032081053584));
#93093=CARTESIAN_POINT('Ctrl Pts',(9.55204643235015,28.7459520887588,126.631857121398));
#93094=CARTESIAN_POINT('',(9.24592528058239,32.0547492111101,124.998199460483));
#93095=CARTESIAN_POINT('Ctrl Pts',(9.24592528058239,32.0547492111101,124.998199460483));
#93096=CARTESIAN_POINT('Ctrl Pts',(9.24973097260797,32.0548106153326,125.068273055967));
#93097=CARTESIAN_POINT('Ctrl Pts',(9.25353666463355,32.0512831902227,125.138464586469));
#93098=CARTESIAN_POINT('Ctrl Pts',(9.25734235665914,32.0441573624556,125.208370439407));
#93099=CARTESIAN_POINT('Ctrl Pts',(9.26114473195258,32.0370377449812,125.27821536808));
#93100=CARTESIAN_POINT('Ctrl Pts',(9.26494710724602,32.0263259898409,125.347774616338));
#93101=CARTESIAN_POINT('Ctrl Pts',(9.26874948253946,32.0120645565245,125.416645872268));
#93102=CARTESIAN_POINT('Ctrl Pts',(9.27254990270275,31.9978104562451,125.485481715525));
#93103=CARTESIAN_POINT('Ctrl Pts',(9.27635032286603,31.9800103979003,125.553629777835));
#93104=CARTESIAN_POINT('Ctrl Pts',(9.28015074302932,31.9587582599149,125.62069609449));
#93105=CARTESIAN_POINT('Ctrl Pts',(9.28395056682591,31.9375094568417,125.687751887014));
#93106=CARTESIAN_POINT('Ctrl Pts',(9.2877503906225,31.912809801656,125.753725793385));
#93107=CARTESIAN_POINT('Ctrl Pts',(9.29155021441908,31.8848030010516,125.818239090808));
#93108=CARTESIAN_POINT('Ctrl Pts',(9.29535341054954,31.8567713444835,125.882809643618));
#93109=CARTESIAN_POINT('Ctrl Pts',(9.29915660668,31.8254268793358,125.945916537134));
#93110=CARTESIAN_POINT('Ctrl Pts',(9.30295980281046,31.7909610139902,126.007202168816));
#93111=CARTESIAN_POINT('Ctrl Pts',(9.30676464085467,31.7564802690602,126.068514258697));
#93112=CARTESIAN_POINT('Ctrl Pts',(9.31056947889889,31.7188757098795,126.128003097546));
#93113=CARTESIAN_POINT('Ctrl Pts',(9.3143743169431,31.6783826326264,126.185339318929));
#93114=CARTESIAN_POINT('Ctrl Pts',(9.31818598583954,31.6378168578698,126.242778476428));
#93115=CARTESIAN_POINT('Ctrl Pts',(9.32199765473598,31.5943525193413,126.298056904219));
#93116=CARTESIAN_POINT('Ctrl Pts',(9.32580932363243,31.5482653438227,126.350878228271));
#93117=CARTESIAN_POINT('Ctrl Pts',(9.32899379923462,31.5097616096317,126.395008036575));
#93118=CARTESIAN_POINT('Ctrl Pts',(9.33217827483681,31.4694279859487,126.4374233548));
#93119=CARTESIAN_POINT('Ctrl Pts',(9.335362750439,31.4274433973735,126.477972567335));
#93120=CARTESIAN_POINT('Ctrl Pts',(9.33923133005976,31.3764394821177,126.527232752322));
#93121=CARTESIAN_POINT('Ctrl Pts',(9.34309990968052,31.3227826115909,126.573946299928));
#93122=CARTESIAN_POINT('Ctrl Pts',(9.34696848930128,31.2667573975064,126.617814346074));
#93123=CARTESIAN_POINT('Ctrl Pts',(9.35083130298269,31.2108156864174,126.661617008922));
#93124=CARTESIAN_POINT('Ctrl Pts',(9.35469411666409,31.1525130179493,126.702582291555));
#93125=CARTESIAN_POINT('Ctrl Pts',(9.3585569303455,31.0921700218974,126.740448851811));
#93126=CARTESIAN_POINT('Ctrl Pts',(9.36241521303453,31.0318978068041,126.778270995455));
#93127=CARTESIAN_POINT('Ctrl Pts',(9.36627349572356,30.9695904274972,126.813001379431));
#93128=CARTESIAN_POINT('Ctrl Pts',(9.37013177841259,30.9055992840115,126.844420640553));
#93129=CARTESIAN_POINT('Ctrl Pts',(9.37398763102304,30.8416484443396,126.875820112748));
#93130=CARTESIAN_POINT('Ctrl Pts',(9.37784348363349,30.7760163796195,126.903912385907));
#93131=CARTESIAN_POINT('Ctrl Pts',(9.38169933624394,30.7090797143445,126.928523663636));
#93132=CARTESIAN_POINT('Ctrl Pts',(9.38555405105399,30.6421628010084,126.953127678971));
#93133=CARTESIAN_POINT('Ctrl Pts',(9.38940876586403,30.5739425072005,126.974252570507));
#93134=CARTESIAN_POINT('Ctrl Pts',(9.39326348067407,30.504814482049,126.991773054646));
#93135=CARTESIAN_POINT('Ctrl Pts',(9.39711834835005,30.4356837154963,127.009294233592));
#93136=CARTESIAN_POINT('Ctrl Pts',(9.40097321602602,30.3656456177036,127.023210604109));
#93137=CARTESIAN_POINT('Ctrl Pts',(9.404828083702,30.2951083207736,127.033447476949));
#93138=CARTESIAN_POINT('Ctrl Pts',(9.40868699379105,30.2244970547956,127.043695084702));
#93139=CARTESIAN_POINT('Ctrl Pts',(9.41254590388011,30.1533860265598,127.050255422412));
#93140=CARTESIAN_POINT('Ctrl Pts',(9.41640481396917,30.0821899271222,127.053105544871));
#93141=CARTESIAN_POINT('Ctrl Pts',(9.42026591229591,30.0109534551483,127.055957283523));
#93142=CARTESIAN_POINT('Ctrl Pts',(9.42412701062264,29.9396323020567,127.055094624619));
#93143=CARTESIAN_POINT('Ctrl Pts',(9.42798810894938,29.8686398401611,127.050546773645));
#93144=CARTESIAN_POINT('Ctrl Pts',(9.43185597388382,29.7975229633716,127.045990952524));
#93145=CARTESIAN_POINT('Ctrl Pts',(9.43572383881826,29.7267364106452,127.037737101432));
#93146=CARTESIAN_POINT('Ctrl Pts',(9.43959170375269,29.6566864281149,127.025866075006));
#93147=CARTESIAN_POINT('Ctrl Pts',(9.44189380959432,29.6149935363716,127.018800585454));
#93148=CARTESIAN_POINT('Ctrl Pts',(9.44419591543594,29.5735613605143,127.010454695704));
#93149=CARTESIAN_POINT('Ctrl Pts',(9.44649802127757,29.5324729501561,127.000853822788));
#93150=CARTESIAN_POINT('Ctrl Pts',(9.45045220849665,29.4618978861634,126.984362987183));
#93151=CARTESIAN_POINT('Ctrl Pts',(9.45440639571573,29.3920553464406,126.964100580526));
#93152=CARTESIAN_POINT('Ctrl Pts',(9.45836058293481,29.3233780040058,126.940149539865));
#93153=CARTESIAN_POINT('Ctrl Pts',(9.4622239475365,29.2562780921907,126.91674862394));
#93154=CARTESIAN_POINT('Ctrl Pts',(9.4660873121382,29.1902909208563,126.889826853226));
#93155=CARTESIAN_POINT('Ctrl Pts',(9.46995067673989,29.1258096198384,126.859513038871));
#93156=CARTESIAN_POINT('Ctrl Pts',(9.47395027526767,29.0590545130314,126.828130267696));
#93157=CARTESIAN_POINT('Ctrl Pts',(9.47794987379545,28.9939139882292,126.793111859723));
#93158=CARTESIAN_POINT('Ctrl Pts',(9.48194947232322,28.9308044976357,126.7546562456));
#93159=CARTESIAN_POINT('Ctrl Pts',(9.485949070851,28.8676950070421,126.716200631477));
#93160=CARTESIAN_POINT('Ctrl Pts',(9.48994866937878,28.8066170704991,126.674308071663));
#93161=CARTESIAN_POINT('Ctrl Pts',(9.49394826790656,28.7479590808042,126.629230216746));
#93162=CARTESIAN_POINT('Ctrl Pts',(8.79398045138579,28.7479590808042,126.629230216746));
#93163=CARTESIAN_POINT('Ctrl Pts',(8.79801550203991,28.6890704171239,126.583975092058));
#93164=CARTESIAN_POINT('Ctrl Pts',(8.80205055269404,28.6325495847743,126.535454723247));
#93165=CARTESIAN_POINT('Ctrl Pts',(8.80608560334816,28.5787741825237,126.483952404304));
#93166=CARTESIAN_POINT('Ctrl Pts',(8.80994358492291,28.5273585922768,126.43471014824));
#93167=CARTESIAN_POINT('Ctrl Pts',(8.81380156649766,28.4784529275307,126.382742540837));
#93168=CARTESIAN_POINT('Ctrl Pts',(8.81765954807242,28.4323541291087,126.328338806923));
#93169=CARTESIAN_POINT('Ctrl Pts',(8.82151545604507,28.3862801080382,126.273964314128));
#93170=CARTESIAN_POINT('Ctrl Pts',(8.82537136401772,28.3430102733044,126.217156662901));
#93171=CARTESIAN_POINT('Ctrl Pts',(8.82922727199037,28.3028032515543,126.158240372101));
#93172=CARTESIAN_POINT('Ctrl Pts',(8.83308239733767,28.2626043905369,126.099336039414));
#93173=CARTESIAN_POINT('Ctrl Pts',(8.83693752268498,28.2254673815428,126.038324318359));
#93174=CARTESIAN_POINT('Ctrl Pts',(8.84079264803228,28.1916082143369,125.975559691688));
#93175=CARTESIAN_POINT('Ctrl Pts',(8.84464828047665,28.1577445933498,125.912786809057));
#93176=CARTESIAN_POINT('Ctrl Pts',(8.84850391292102,28.1271598984163,125.848260991818));
#93177=CARTESIAN_POINT('Ctrl Pts',(8.85235954536539,28.1000239191649,125.782360821331));
#93178=CARTESIAN_POINT('Ctrl Pts',(8.85621943189836,28.0728579995958,125.716387940293));
#93179=CARTESIAN_POINT('Ctrl Pts',(8.86007931843133,28.0491485725025,125.649038130586));
#93180=CARTESIAN_POINT('Ctrl Pts',(8.8639392049643,28.0290167046793,125.580708543132));
#93181=CARTESIAN_POINT('Ctrl Pts',(8.86780159697256,28.0088717691411,125.512334602537));
#93182=CARTESIAN_POINT('Ctrl Pts',(8.87166398898081,27.992309126067,125.442980090994));
#93183=CARTESIAN_POINT('Ctrl Pts',(8.87552638098906,27.9793988842256,125.373053204558));
#93184=CARTESIAN_POINT('Ctrl Pts',(8.87939521111159,27.9664671226595,125.303009758932));
#93185=CARTESIAN_POINT('Ctrl Pts',(8.88326404123413,27.9571999712989,125.232392515708));
#93186=CARTESIAN_POINT('Ctrl Pts',(8.88713287135666,27.9516157013587,125.161614750502));
#93187=CARTESIAN_POINT('Ctrl Pts',(8.88836246993269,27.949840898602,125.13912003335));
#93188=CARTESIAN_POINT('Ctrl Pts',(8.88959206850872,27.9484377112274,125.116609094769));
#93189=CARTESIAN_POINT('Ctrl Pts',(8.89082166708475,27.9474056254475,125.094095143633));
#93190=CARTESIAN_POINT('Ctrl Pts',(8.89469075534478,27.9441580363138,125.02325213379));
#93191=CARTESIAN_POINT('Ctrl Pts',(8.89855984360481,27.9445759933657,124.952102042037));
#93192=CARTESIAN_POINT('Ctrl Pts',(8.90242893186485,27.9486955595437,124.881056084375));
#93193=CARTESIAN_POINT('Ctrl Pts',(8.90629225530753,27.9528089877002,124.810115982911));
#93194=CARTESIAN_POINT('Ctrl Pts',(8.91015557875022,27.9606130494148,124.739280188572));
#93195=CARTESIAN_POINT('Ctrl Pts',(8.9140189021929,27.9720918431932,124.66896213199));
#93196=CARTESIAN_POINT('Ctrl Pts',(8.91787769385889,27.9835571720544,124.598726560278));
#93197=CARTESIAN_POINT('Ctrl Pts',(8.92173648552489,27.998688592875,124.529007997088));
#93198=CARTESIAN_POINT('Ctrl Pts',(8.92559527719088,28.0174183654138,124.460215205196));
#93199=CARTESIAN_POINT('Ctrl Pts',(8.92945163802158,28.0361363391835,124.391465749136));
#93200=CARTESIAN_POINT('Ctrl Pts',(8.93330799885228,28.0584480401178,124.32364137495));
#93201=CARTESIAN_POINT('Ctrl Pts',(8.93716435968298,28.0842348635052,124.257139646844));
#93202=CARTESIAN_POINT('Ctrl Pts',(8.94101958121716,28.1100140686122,124.190657565548));
#93203=CARTESIAN_POINT('Ctrl Pts',(8.94487480275135,28.1392661824246,124.125497807253));
#93204=CARTESIAN_POINT('Ctrl Pts',(8.94873002428554,28.1718236234698,124.062040140093));
#93205=CARTESIAN_POINT('Ctrl Pts',(8.952585396449,28.2043823365829,123.998579993547));
#93206=CARTESIAN_POINT('Ctrl Pts',(8.95644076861247,28.2402464096163,123.93682250138));
#93207=CARTESIAN_POINT('Ctrl Pts',(8.96029614077593,28.2792020461361,123.877123352956));
#93208=CARTESIAN_POINT('Ctrl Pts',(8.96415554848578,28.3181984588174,123.817361715445));
#93209=CARTESIAN_POINT('Ctrl Pts',(8.96801495619562,28.3602926288398,123.759663130279));
#93210=CARTESIAN_POINT('Ctrl Pts',(8.97187436390547,28.4052275978471,123.70435400366));
#93211=CARTESIAN_POINT('Ctrl Pts',(8.97573595673313,28.4501880081161,123.649013562144));
#93212=CARTESIAN_POINT('Ctrl Pts',(8.9795975495608,28.4979920935116,123.596065633046));
#93213=CARTESIAN_POINT('Ctrl Pts',(8.98345914238846,28.5483446338577,123.545801161997));
#93214=CARTESIAN_POINT('Ctrl Pts',(8.98732749153428,28.5987852719909,123.495448747248));
#93215=CARTESIAN_POINT('Ctrl Pts',(8.99119584068009,28.6517829059278,123.447789489243));
#93216=CARTESIAN_POINT('Ctrl Pts',(8.99506418982591,28.7070082687023,123.403074846683));
#93217=CARTESIAN_POINT('Ctrl Pts',(8.99736177252505,28.7398090406287,123.376516853785));
#93218=CARTESIAN_POINT('Ctrl Pts',(8.99965935522418,28.7733950950642,123.350996826026));
#93219=CARTESIAN_POINT('Ctrl Pts',(9.00195693792331,28.8076929148876,123.326560016824));
#93220=CARTESIAN_POINT('Ctrl Pts',(9.00582595067416,28.8654487041671,123.285409669363));
#93221=CARTESIAN_POINT('Ctrl Pts',(9.00969496342501,28.9254504889425,123.24717222179));
#93222=CARTESIAN_POINT('Ctrl Pts',(9.01356397617586,28.987372364539,123.212100999944));
#93223=CARTESIAN_POINT('Ctrl Pts',(9.01742722389497,29.0492019732962,123.177082036057));
#93224=CARTESIAN_POINT('Ctrl Pts',(9.02129047161409,29.1129455745374,123.145220170585));
#93225=CARTESIAN_POINT('Ctrl Pts',(9.0251537193332,29.1782472182896,123.116726273679));
#93226=CARTESIAN_POINT('Ctrl Pts',(9.02901243532262,29.243472260845,123.088265801148));
#93227=CARTESIAN_POINT('Ctrl Pts',(9.03287115131202,29.3102512725042,123.063165643009));
#93228=CARTESIAN_POINT('Ctrl Pts',(9.03672986730144,29.3782041085501,123.041590586247));
#93229=CARTESIAN_POINT('Ctrl Pts',(9.04058615252545,29.4461141382834,123.020029120509));
#93230=CARTESIAN_POINT('Ctrl Pts',(9.04444243774945,29.5151960634365,123.001988497164));
#93231=CARTESIAN_POINT('Ctrl Pts',(9.04829872297347,29.5850515599355,122.987584696295));
#93232=CARTESIAN_POINT('Ctrl Pts',(9.05215386908144,29.6548864216754,122.973185150193));
#93233=CARTESIAN_POINT('Ctrl Pts',(9.05600901518941,29.725493925578,122.962420391861));
#93234=CARTESIAN_POINT('Ctrl Pts',(9.05986416129738,29.7964641351358,122.955355602014));
#93235=CARTESIAN_POINT('Ctrl Pts',(9.06371945832583,29.8674371230208,122.948290535597));
#93236=CARTESIAN_POINT('Ctrl Pts',(9.06757475535427,29.9387723611197,122.944925771168));
#93237=CARTESIAN_POINT('Ctrl Pts',(9.07143005238271,30.0100550770384,122.945274602793));
#93238=CARTESIAN_POINT('Ctrl Pts',(9.07528938591728,30.081412426148,122.945623799646));
#93239=CARTESIAN_POINT('Ctrl Pts',(9.07914871945184,30.1527166565108,122.94969435178));
#93240=CARTESIAN_POINT('Ctrl Pts',(9.08300805298641,30.2235541882578,122.957447408899));
#93241=CARTESIAN_POINT('Ctrl Pts',(9.08686957206813,30.2944318354196,122.965204856588));
#93242=CARTESIAN_POINT('Ctrl Pts',(9.09073109114985,30.3648417781052,122.976648882686));
#93243=CARTESIAN_POINT('Ctrl Pts',(9.09459261023157,30.4343794770015,122.991689258989));
#93244=CARTESIAN_POINT('Ctrl Pts',(9.0984608871096,30.5040388693545,123.006755956488));
#93245=CARTESIAN_POINT('Ctrl Pts',(9.10232916398764,30.5728225013246,123.025431442491));
#93246=CARTESIAN_POINT('Ctrl Pts',(9.10619744086568,30.6403405429456,123.047575468409));
#93247=CARTESIAN_POINT('Ctrl Pts',(9.10849569683108,30.6804549780857,123.0607318792));
#93248=CARTESIAN_POINT('Ctrl Pts',(9.11079395279648,30.7201230286415,123.075111713347));
#93249=CARTESIAN_POINT('Ctrl Pts',(9.11309220876188,30.7592667329505,123.090677714283));
#93250=CARTESIAN_POINT('Ctrl Pts',(9.11696135407878,30.8251656939425,123.116883289524));
#93251=CARTESIAN_POINT('Ctrl Pts',(9.12083049939568,30.8898354221716,123.146555879442));
#93252=CARTESIAN_POINT('Ctrl Pts',(9.12469964471258,30.952886311134,123.179559053264));
#93253=CARTESIAN_POINT('Ctrl Pts',(9.1285630246973,31.0158432492909,123.212513049749));
#93254=CARTESIAN_POINT('Ctrl Pts',(9.13242640468201,31.0771857094646,123.248787555605));
#93255=CARTESIAN_POINT('Ctrl Pts',(9.13628978466673,31.1365434600309,123.288197871844));
#93256=CARTESIAN_POINT('Ctrl Pts',(9.14014863185054,31.1958315677284,123.327561949007));
#93257=CARTESIAN_POINT('Ctrl Pts',(9.14400747903436,31.2531391885007,123.370054261092));
#93258=CARTESIAN_POINT('Ctrl Pts',(9.14786632621817,31.3081216859858,123.415444788859));
#93259=CARTESIAN_POINT('Ctrl Pts',(9.15172274190637,31.3630695384864,123.460806715631));
#93260=CARTESIAN_POINT('Ctrl Pts',(9.15557915759458,31.4156948006809,123.50906292642));
#93261=CARTESIAN_POINT('Ctrl Pts',(9.15943557328279,31.4656839817026,123.559941658029));
#93262=CARTESIAN_POINT('Ctrl Pts',(9.1632908489394,31.5156583849488,123.610805348894));
#93263=CARTESIAN_POINT('Ctrl Pts',(9.16714612459602,31.5629979138436,123.664289675139));
#93264=CARTESIAN_POINT('Ctrl Pts',(9.17100140025264,31.6074254582294,123.720085565854));
#93265=CARTESIAN_POINT('Ctrl Pts',(9.17485682572797,31.6518547291008,123.775883624836));
#93266=CARTESIAN_POINT('Ctrl Pts',(9.17871225120331,31.6933714899315,123.833993045247));
#93267=CARTESIAN_POINT('Ctrl Pts',(9.18256767667864,31.7317395997958,123.894072551657));
#93268=CARTESIAN_POINT('Ctrl Pts',(9.186427136109,31.7701478544457,123.954214919618));
#93269=CARTESIAN_POINT('Ctrl Pts',(9.19028659553936,31.8054006196676,124.016331078181));
#93270=CARTESIAN_POINT('Ctrl Pts',(9.19414605496972,31.8373062098376,124.080052472261));
#93271=CARTESIAN_POINT('Ctrl Pts',(9.19800769869874,31.8692298572872,124.143809930085));
#93272=CARTESIAN_POINT('Ctrl Pts',(9.20186934242776,31.8978023639166,124.209173986659));
#93273=CARTESIAN_POINT('Ctrl Pts',(9.20573098615679,31.9228801116375,124.275755815509));
#93274=CARTESIAN_POINT('Ctrl Pts',(9.20959938436661,31.9480017233648,124.342454104011));
#93275=CARTESIAN_POINT('Ctrl Pts',(9.21346778257643,31.9696162245264,124.410373954418));
#93276=CARTESIAN_POINT('Ctrl Pts',(9.21733618078625,31.9876299987723,124.479111767766));
#93277=CARTESIAN_POINT('Ctrl Pts',(9.21963328039098,31.9983267862941,124.519929076457));
#93278=CARTESIAN_POINT('Ctrl Pts',(9.22193037999571,32.0077548910856,124.561034600731));
#93279=CARTESIAN_POINT('Ctrl Pts',(9.22422747960044,32.0159033429618,124.602342767782));
#93280=CARTESIAN_POINT('Ctrl Pts',(9.22983481554542,32.0357941248016,124.703178086132));
#93281=CARTESIAN_POINT('Ctrl Pts',(9.23544215149041,32.0481241011246,124.805550423609));
#93282=CARTESIAN_POINT('Ctrl Pts',(9.24104948743539,32.0527129388303,124.908527855286));
#93283=CARTESIAN_POINT('Ctrl Pts',(9.24267475180283,32.0540429954711,124.938375460636));
#93284=CARTESIAN_POINT('Ctrl Pts',(9.24430001617026,32.0547229877209,124.968273728132));
#93285=CARTESIAN_POINT('Ctrl Pts',(9.24592528053769,32.0547492111093,124.99819945966));
#93286=CARTESIAN_POINT('Origin',(-1.54592528053767,30.,125.));
#93287=CARTESIAN_POINT('',(8.09385900549202,28.7479590808042,126.629230216746));
#93288=CARTESIAN_POINT('',(8.1521135920327,28.7479590808041,126.629230216746));
#93289=CARTESIAN_POINT('',(-1.54592528053767,28.7479590808042,126.629230216746));
#93290=CARTESIAN_POINT('',(8.60407471942971,32.0547498911252,124.999331104703));
#93291=CARTESIAN_POINT('Ctrl Pts',(8.1521135920327,28.7479590808041,126.629230216746));
#93292=CARTESIAN_POINT('Ctrl Pts',(8.15596912515558,28.6914354667109,126.585792600001));
#93293=CARTESIAN_POINT('Ctrl Pts',(8.15982465827847,28.6371472850519,126.539388739369));
#93294=CARTESIAN_POINT('Ctrl Pts',(8.16368019140134,28.5854141825686,126.490283371585));
#93295=CARTESIAN_POINT('Ctrl Pts',(8.16753532555932,28.5336864333507,126.441183085152));
#93296=CARTESIAN_POINT('Ctrl Pts',(8.17139045971729,28.484513589786,126.389382181945));
#93297=CARTESIAN_POINT('Ctrl Pts',(8.17524559387527,28.4381796297543,126.335183393241));
#93298=CARTESIAN_POINT('Ctrl Pts',(8.17912809993425,28.3915166932162,126.280599786832));
#93299=CARTESIAN_POINT('Ctrl Pts',(8.18301060599323,28.3477334539812,126.223584474127));
#93300=CARTESIAN_POINT('Ctrl Pts',(8.18689311205222,28.3070784500729,126.164480222371));
#93301=CARTESIAN_POINT('Ctrl Pts',(8.19075363060142,28.2666536846453,126.105710691357));
#93302=CARTESIAN_POINT('Ctrl Pts',(8.19461414915062,28.2293220239667,126.04487626749));
#93303=CARTESIAN_POINT('Ctrl Pts',(8.19847466769982,28.1952828349408,125.982340835271));
#93304=CARTESIAN_POINT('Ctrl Pts',(8.20236816751369,28.1609528415868,125.919271149009));
#93305=CARTESIAN_POINT('Ctrl Pts',(8.20626166732756,28.1299720655184,125.854471704079));
#93306=CARTESIAN_POINT('Ctrl Pts',(8.21015516714143,28.1024956005184,125.788336613667));
#93307=CARTESIAN_POINT('Ctrl Pts',(8.21404866695531,28.0750191355185,125.722201523256));
#93308=CARTESIAN_POINT('Ctrl Pts',(8.21794216676918,28.0510470881701,125.654731279922));
#93309=CARTESIAN_POINT('Ctrl Pts',(8.22183566658305,28.0306827603615,125.586333669648));
#93310=CARTESIAN_POINT('Ctrl Pts',(8.22570474050518,28.0104461882713,125.518365152144));
#93311=CARTESIAN_POINT('Ctrl Pts',(8.22957381442732,27.9936928812771,125.449214612468));
#93312=CARTESIAN_POINT('Ctrl Pts',(8.23344288834945,27.9805570105946,125.379272428528));
#93313=CARTESIAN_POINT('Ctrl Pts',(8.23730619731202,27.9674407124932,125.309434459154));
#93314=CARTESIAN_POINT('Ctrl Pts',(8.24116950627459,27.9579312406085,125.238807660454));
#93315=CARTESIAN_POINT('Ctrl Pts',(8.24503281523716,27.9521128697065,125.167797091983));
#93316=CARTESIAN_POINT('Ctrl Pts',(8.24889159228369,27.946301324137,125.09686982359));
#93317=CARTESIAN_POINT('Ctrl Pts',(8.25275036933023,27.944172318373,125.025560161463));
#93318=CARTESIAN_POINT('Ctrl Pts',(8.25660914637676,27.945758692832,124.954281137102));
#93319=CARTESIAN_POINT('Ctrl Pts',(8.26046549251019,27.9473440679229,124.883047016375));
#93320=CARTESIAN_POINT('Ctrl Pts',(8.26432183864362,27.9526401687858,124.81184397964));
#93321=CARTESIAN_POINT('Ctrl Pts',(8.26817818477705,27.9616277719837,124.74108645738));
#93322=CARTESIAN_POINT('Ctrl Pts',(8.27203339155849,27.970612719807,124.670349840331));
#93323=CARTESIAN_POINT('Ctrl Pts',(8.27588859833991,27.9832869435458,124.600058958094));
#93324=CARTESIAN_POINT('Ctrl Pts',(8.27974380512135,27.9995793967808,124.530622782065));
#93325=CARTESIAN_POINT('Ctrl Pts',(8.28359916249883,28.0158724864484,124.461183893649));
#93326=CARTESIAN_POINT('Ctrl Pts',(8.28745451987631,28.0357839731073,124.392600250166));
#93327=CARTESIAN_POINT('Ctrl Pts',(8.29130987725379,28.0591921524534,124.325268600552));
#93328=CARTESIAN_POINT('Ctrl Pts',(8.29516927023008,28.0826248343324,124.257866471472));
#93329=CARTESIAN_POINT('Ctrl Pts',(8.29902866320638,28.1095613555654,124.191719412152));
#93330=CARTESIAN_POINT('Ctrl Pts',(8.30288805618267,28.1398310617643,124.127206161959));
#93331=CARTESIAN_POINT('Ctrl Pts',(8.30674963428417,28.1701179061759,124.062656385418));
#93332=CARTESIAN_POINT('Ctrl Pts',(8.31061121238567,28.2037414632937,123.999742688106));
#93333=CARTESIAN_POINT('Ctrl Pts',(8.31447279048717,28.2404853943586,123.938818622933));
#93334=CARTESIAN_POINT('Ctrl Pts',(8.31834112507955,28.2772936152109,123.877787960694));
#93335=CARTESIAN_POINT('Ctrl Pts',(8.32220945967192,28.3172328380164,123.818754283396));
#93336=CARTESIAN_POINT('Ctrl Pts',(8.3260777942643,28.360044159249,123.76204103344));
#93337=CARTESIAN_POINT('Ctrl Pts',(8.32837550865007,28.3854732389526,123.728354482503));
#93338=CARTESIAN_POINT('Ctrl Pts',(8.33067322303584,28.4119148620755,123.695485968757));
#93339=CARTESIAN_POINT('Ctrl Pts',(8.33297093742161,28.4393085841369,123.663497150414));
#93340=CARTESIAN_POINT('Ctrl Pts',(8.3368400130158,28.48543632835,123.609631814886));
#93341=CARTESIAN_POINT('Ctrl Pts',(8.34070908860998,28.5344463408364,123.558051838837));
#93342=CARTESIAN_POINT('Ctrl Pts',(8.34457816420417,28.5860834172975,123.509081672371));
#93343=CARTESIAN_POINT('Ctrl Pts',(8.34844147486131,28.6376435543222,123.460184471636));
#93344=CARTESIAN_POINT('Ctrl Pts',(8.35230478551845,28.691822635864,123.413889693227));
#93345=CARTESIAN_POINT('Ctrl Pts',(8.35616809617559,28.74832606092,123.370487829831));
#93346=CARTESIAN_POINT('Ctrl Pts',(8.36002687494163,28.8047632041282,123.327136879379));
#93347=CARTESIAN_POINT('Ctrl Pts',(8.36388565370767,28.8635188915363,123.286672397668));
#93348=CARTESIAN_POINT('Ctrl Pts',(8.36774443247371,28.9242639284487,123.249345988819));
#93349=CARTESIAN_POINT('Ctrl Pts',(8.37160078034105,28.9849706980646,123.212043094332));
#93350=CARTESIAN_POINT('Ctrl Pts',(8.3754571282084,29.0476639178999,123.177874604336));
#93351=CARTESIAN_POINT('Ctrl Pts',(8.37931347607574,29.1119849803721,123.147049140583));
#93352=CARTESIAN_POINT('Ctrl Pts',(8.3831686846028,29.1762870394816,123.116232784071));
#93353=CARTESIAN_POINT('Ctrl Pts',(8.38702389312987,29.2422155485944,123.088757702811));
#93354=CARTESIAN_POINT('Ctrl Pts',(8.39087910165693,29.3093883796462,123.064786018981));
#93355=CARTESIAN_POINT('Ctrl Pts',(8.39473446078913,29.3765638348293,123.040813398688));
#93356=CARTESIAN_POINT('Ctrl Pts',(8.39858981992133,29.4449832501951,123.020344608747));
#93357=CARTESIAN_POINT('Ctrl Pts',(8.40244517905353,29.5142472913024,123.00349258241));
#93358=CARTESIAN_POINT('Ctrl Pts',(8.406304573786,29.5835838346004,122.986622916201));
#93359=CARTESIAN_POINT('Ctrl Pts',(8.41016396851848,29.6537662955446,122.973377686081));
#93360=CARTESIAN_POINT('Ctrl Pts',(8.41402336325095,29.7243839215627,122.96381893246));
#93361=CARTESIAN_POINT('Ctrl Pts',(8.41788494311211,29.7950415301716,122.954254766824));
#93362=CARTESIAN_POINT('Ctrl Pts',(8.42174652297327,29.8661343099628,122.948381272724));
#93363=CARTESIAN_POINT('Ctrl Pts',(8.42560810283443,29.9372478910485,122.946208448912));
#93364=CARTESIAN_POINT('Ctrl Pts',(8.42947643917265,30.0084858971871,122.944031823382));
#93365=CARTESIAN_POINT('Ctrl Pts',(8.43334477551087,30.0797442914579,122.945568785064));
#93366=CARTESIAN_POINT('Ctrl Pts',(8.43721311184909,30.1506109155235,122.950777241336));
#93367=CARTESIAN_POINT('Ctrl Pts',(8.43951081065278,30.192703986834,122.953870939169));
#93368=CARTESIAN_POINT('Ctrl Pts',(8.44180850945647,30.2346589582454,122.958258975204));
#93369=CARTESIAN_POINT('Ctrl Pts',(8.44410620826017,30.2763912468542,122.963924008991));
#93370=CARTESIAN_POINT('Ctrl Pts',(8.44797527432202,30.346663721767,122.973463288));
#93371=CARTESIAN_POINT('Ctrl Pts',(8.45184434038386,30.4165794115984,122.986663565757));
#93372=CARTESIAN_POINT('Ctrl Pts',(8.45571340644571,30.4857273196364,123.003486405391));
#93373=CARTESIAN_POINT('Ctrl Pts',(8.45957670755058,30.5547721964238,123.020284178783));
#93374=CARTESIAN_POINT('Ctrl Pts',(8.46344000865546,30.6230510940604,123.040693685944));
#93375=CARTESIAN_POINT('Ctrl Pts',(8.46730330976033,30.6901601774277,123.064624973812));
#93376=CARTESIAN_POINT('Ctrl Pts',(8.47116207899044,30.7571905379739,123.0885281889));
#93377=CARTESIAN_POINT('Ctrl Pts',(8.47502084822055,30.8230533546779,123.115944816256));
#93378=CARTESIAN_POINT('Ctrl Pts',(8.47887961745066,30.8873587018988,123.146734747354));
#93379=CARTESIAN_POINT('Ctrl Pts',(8.4827359557973,30.9516235391031,123.177505281922));
#93380=CARTESIAN_POINT('Ctrl Pts',(8.48659229414393,31.0143324162908,123.211644694856));
#93381=CARTESIAN_POINT('Ctrl Pts',(8.49044863249057,31.0751155666091,123.248964854455));
#93382=CARTESIAN_POINT('Ctrl Pts',(8.49430383152602,31.1358807592387,123.286273988238));
#93383=CARTESIAN_POINT('Ctrl Pts',(8.49815903056147,31.1947209407328,123.326761749048));
#93384=CARTESIAN_POINT('Ctrl Pts',(8.50201422959692,31.2512926538453,123.370195024878));
#93385=CARTESIAN_POINT('Ctrl Pts',(8.50586957928047,31.3078665775885,123.413629997933));
#93386=CARTESIAN_POINT('Ctrl Pts',(8.50972492896403,31.3621714729788,123.460010416944));
#93387=CARTESIAN_POINT('Ctrl Pts',(8.51358027864759,31.413895876396,123.509062035761));
#93388=CARTESIAN_POINT('Ctrl Pts',(8.51743966406173,31.465674424255,123.558165001182));
#93389=CARTESIAN_POINT('Ctrl Pts',(8.52129904947586,31.5148667346747,123.609944413246));
#93390=CARTESIAN_POINT('Ctrl Pts',(8.52515843489,31.5611979085457,123.664088830478));
#93391=CARTESIAN_POINT('Ctrl Pts',(8.52902000549224,31.6075553151763,123.718263904337));
#93392=CARTESIAN_POINT('Ctrl Pts',(8.53288157609448,31.651048064057,123.774806263801));
#93393=CARTESIAN_POINT('Ctrl Pts',(8.53674314669673,31.6914430166796,123.833373202851));
#93394=CARTESIAN_POINT('Ctrl Pts',(8.54061147397022,31.7319086491999,123.892042617705));
#93395=CARTESIAN_POINT('Ctrl Pts',(8.54447980124372,31.7692654090247,123.952743270899));
#93396=CARTESIAN_POINT('Ctrl Pts',(8.54834812851722,31.8033251213736,124.015106061993));
#93397=CARTESIAN_POINT('Ctrl Pts',(8.55064591204439,31.8235565652103,124.052149513581));
#93398=CARTESIAN_POINT('Ctrl Pts',(8.55294369557156,31.842625593561,124.089778987952));
#93399=CARTESIAN_POINT('Ctrl Pts',(8.55524147909873,31.8605008968746,124.127914009269));
#93400=CARTESIAN_POINT('Ctrl Pts',(8.559432104139,31.8931013106136,124.197463456967));
#93401=CARTESIAN_POINT('Ctrl Pts',(8.56362272917927,31.9218404086957,124.268933251934));
#93402=CARTESIAN_POINT('Ctrl Pts',(8.56781335421954,31.9465077850154,124.341892861781));
#93403=CARTESIAN_POINT('Ctrl Pts',(8.57199336345927,31.9711126732947,124.414667648444));
#93404=CARTESIAN_POINT('Ctrl Pts',(8.57617337269901,31.9916662582748,124.488924405375));
#93405=CARTESIAN_POINT('Ctrl Pts',(8.58035338193875,32.0080055595422,124.56421193758));
#93406=CARTESIAN_POINT('Ctrl Pts',(8.58451634367378,32.0242782235609,124.639192421526));
#93407=CARTESIAN_POINT('Ctrl Pts',(8.58867930540881,32.0363707665731,124.715194962654));
#93408=CARTESIAN_POINT('Ctrl Pts',(8.59284226714384,32.0441701294669,124.791754845686));
#93409=CARTESIAN_POINT('Ctrl Pts',(8.5965864179058,32.0511848445616,124.860612491428));
#93410=CARTESIAN_POINT('Ctrl Pts',(8.60033056866774,32.0547272954872,124.929920563126));
#93411=CARTESIAN_POINT('Ctrl Pts',(8.6040747194297,32.0547498911252,124.999331104703));
#93412=CARTESIAN_POINT('Ctrl Pts',(8.60407471946233,32.0547498911254,124.999331105308));
#93413=CARTESIAN_POINT('Ctrl Pts',(8.60802536883305,32.0547737329438,125.07256979943));
#93414=CARTESIAN_POINT('Ctrl Pts',(8.61197601820377,32.0508774975988,125.145776561394));
#93415=CARTESIAN_POINT('Ctrl Pts',(8.61592666757449,32.0430975791866,125.218517377849));
#93416=CARTESIAN_POINT('Ctrl Pts',(8.61988033452302,32.0353117183313,125.291313755061));
#93417=CARTESIAN_POINT('Ctrl Pts',(8.62383400147154,32.0236363229151,125.363643030758));
#93418=CARTESIAN_POINT('Ctrl Pts',(8.62778766842007,32.0081592793619,125.435079155112));
#93419=CARTESIAN_POINT('Ctrl Pts',(8.63174857351,31.9926539013458,125.506646060529));
#93420=CARTESIAN_POINT('Ctrl Pts',(8.63570947859993,31.9733330790047,125.57731610935));
#93421=CARTESIAN_POINT('Ctrl Pts',(8.63967038368986,31.950335120339,125.646676488572));
#93422=CARTESIAN_POINT('Ctrl Pts',(8.64363548345035,31.9273128064167,125.716110321699));
#93423=CARTESIAN_POINT('Ctrl Pts',(8.64760058321084,31.9006057650142,125.784231303702));
#93424=CARTESIAN_POINT('Ctrl Pts',(8.65156568297133,31.87040019397,125.850647210597));
#93425=CARTESIAN_POINT('Ctrl Pts',(8.65553895286672,31.8401323839897,125.917199968254));
#93426=CARTESIAN_POINT('Ctrl Pts',(8.65951222276212,31.8063518609842,125.982040237618));
#93427=CARTESIAN_POINT('Ctrl Pts',(8.66348549265752,31.7692902203559,126.044801262754));
#93428=CARTESIAN_POINT('Ctrl Pts',(8.66444924508411,31.7603005853628,126.060024515104));
#93429=CARTESIAN_POINT('Ctrl Pts',(8.6654129975107,31.7511180998049,126.075125578529));
#93430=CARTESIAN_POINT('Ctrl Pts',(8.66637674993729,31.7417464325632,126.090099503327));
#93431=CARTESIAN_POINT('Ctrl Pts',(8.67024583823578,31.7041228613408,126.150213943116));
#93432=CARTESIAN_POINT('Ctrl Pts',(8.67411492653427,31.663309772076,126.208496033772));
#93433=CARTESIAN_POINT('Ctrl Pts',(8.67798401483276,31.6195113983516,126.264587044497));
#93434=CARTESIAN_POINT('Ctrl Pts',(8.68184733831414,31.5757782827953,126.32059448142));
#93435=CARTESIAN_POINT('Ctrl Pts',(8.68571066179551,31.5290690084294,126.374416938867));
#93436=CARTESIAN_POINT('Ctrl Pts',(8.68957398527689,31.4796318084124,126.425723421297));
#93437=CARTESIAN_POINT('Ctrl Pts',(8.69343277698174,31.4302525994862,126.47696971992));
#93438=CARTESIAN_POINT('Ctrl Pts',(8.69729156868659,31.3781521564779,126.525705557696));
#93439=CARTESIAN_POINT('Ctrl Pts',(8.70115036039145,31.3236186940698,126.571633263586));
#93440=CARTESIAN_POINT('Ctrl Pts',(8.70500672126109,31.2691195848661,126.617532037443));
#93441=CARTESIAN_POINT('Ctrl Pts',(8.70886308213074,31.212190867749,126.660625876843));
#93442=CARTESIAN_POINT('Ctrl Pts',(8.71271944300038,31.1531562230052,126.700655252497));
#93443=CARTESIAN_POINT('Ctrl Pts',(8.71657466457353,31.0941390190471,126.740672802149));
#93444=CARTESIAN_POINT('Ctrl Pts',(8.72042988614668,31.0330175244716,126.777627412935));
#93445=CARTESIAN_POINT('Ctrl Pts',(8.72428510771983,30.9701455799791,126.811302049948));
#93446=CARTESIAN_POINT('Ctrl Pts',(8.72814047992222,30.9072711789862,126.84497800268));
#93447=CARTESIAN_POINT('Ctrl Pts',(8.73199585212462,30.8426466215573,126.875373499789));
#93448=CARTESIAN_POINT('Ctrl Pts',(8.73585122432701,30.7766500637452,126.902317597297));
#93449=CARTESIAN_POINT('Ctrl Pts',(8.73971063207546,30.7105844251453,126.929289898085));
#93450=CARTESIAN_POINT('Ctrl Pts',(8.74357003982391,30.6431443700123,126.952803403531));
#93451=CARTESIAN_POINT('Ctrl Pts',(8.74742944757237,30.5747268984803,126.972735804578));
#93452=CARTESIAN_POINT('Ctrl Pts',(8.75129104043852,30.5062706903758,126.992679490942));
#93453=CARTESIAN_POINT('Ctrl Pts',(8.75515263330467,30.4368364372972,127.009037925231));
#93454=CARTESIAN_POINT('Ctrl Pts',(8.75901422617082,30.3668324395648,127.021739727013));
#93455=CARTESIAN_POINT('Ctrl Pts',(8.76288257535451,30.2967059614845,127.034463752113));
#93456=CARTESIAN_POINT('Ctrl Pts',(8.76675092453821,30.2260082305367,127.04351830975));
#93457=CARTESIAN_POINT('Ctrl Pts',(8.77061927372191,30.1551530902908,127.048883862271));
#93458=CARTESIAN_POINT('Ctrl Pts',(8.77291685607322,30.1130691128632,127.052070699392));
#93459=CARTESIAN_POINT('Ctrl Pts',(8.77521443842453,30.0709296353044,127.053957167735));
#93460=CARTESIAN_POINT('Ctrl Pts',(8.77751202077585,30.0288208638428,127.054547862744));
#93461=CARTESIAN_POINT('Ctrl Pts',(8.78138027673787,29.9579256873689,127.055542368769));
#93462=CARTESIAN_POINT('Ctrl Pts',(8.78524853269989,29.8868401127541,127.052865003996));
#93463=CARTESIAN_POINT('Ctrl Pts',(8.78911678866191,29.8159760378281,127.046492791057));
#93464=CARTESIAN_POINT('Ctrl Pts',(8.79297966466309,29.7452105204824,127.040129440575));
#93465=CARTESIAN_POINT('Ctrl Pts',(8.79684254066427,29.6746663711641,127.030081480092));
#93466=CARTESIAN_POINT('Ctrl Pts',(8.80070541666546,29.604756174732,127.016377911277));
#93467=CARTESIAN_POINT('Ctrl Pts',(8.8045642130925,29.5349198102917,127.002688814769));
#93468=CARTESIAN_POINT('Ctrl Pts',(8.80842300951955,29.4657165441792,126.985351865614));
#93469=CARTESIAN_POINT('Ctrl Pts',(8.8122818059466,29.3975527960711,126.964447741473));
#93470=CARTESIAN_POINT('Ctrl Pts',(8.81613815589117,29.3294322638773,126.943556870576));
#93471=CARTESIAN_POINT('Ctrl Pts',(8.81999450583573,29.2623504054606,126.919103454006));
#93472=CARTESIAN_POINT('Ctrl Pts',(8.8238508557803,29.1967008280559,126.891218655485));
#93473=CARTESIAN_POINT('Ctrl Pts',(8.82770577827881,29.1310755511508,126.863344178653));
#93474=CARTESIAN_POINT('Ctrl Pts',(8.83156070077733,29.0668819478089,126.832041035445));
#93475=CARTESIAN_POINT('Ctrl Pts',(8.83541562327585,29.0044941995705,126.79748873816));
#93476=CARTESIAN_POINT('Ctrl Pts',(8.83927149035687,28.9420911642866,126.762927974428));
#93477=CARTESIAN_POINT('Ctrl Pts',(8.8431273574379,28.8814952931375,126.725116701829));
#93478=CARTESIAN_POINT('Ctrl Pts',(8.84698322451892,28.8230554528631,126.684279993191));
#93479=CARTESIAN_POINT('Ctrl Pts',(8.84866239459628,28.7976058123407,126.666496242413));
#93480=CARTESIAN_POINT('Ctrl Pts',(8.85034156467364,28.7725646904092,126.648139287884));
#93481=CARTESIAN_POINT('Ctrl Pts',(8.85202073475099,28.7479590808042,126.629230216746));
#93482=CARTESIAN_POINT('',(8.54592528048629,32.0547496520905,125.001195714812));
#93483=CARTESIAN_POINT('Ctrl Pts',(8.54592528053769,32.05474965209,125.001195715756));
#93484=CARTESIAN_POINT('Ctrl Pts',(8.54975547188149,32.0547087341196,125.071510240684));
#93485=CARTESIAN_POINT('Ctrl Pts',(8.55358566322529,32.0510587896527,125.141718266712));
#93486=CARTESIAN_POINT('Ctrl Pts',(8.55741585456908,32.0438307944864,125.211549630132));
#93487=CARTESIAN_POINT('Ctrl Pts',(8.56128493015697,32.0365294204461,125.282089924135));
#93488=CARTESIAN_POINT('Ctrl Pts',(8.56515400574485,32.02555754131,125.352389946217));
#93489=CARTESIAN_POINT('Ctrl Pts',(8.56902308133273,32.0109405151941,125.42203768416));
#93490=CARTESIAN_POINT('Ctrl Pts',(8.57288639198354,31.9963452685017,125.491581646712));
#93491=CARTESIAN_POINT('Ctrl Pts',(8.57674970263436,31.9781157547389,125.560474782776));
#93492=CARTESIAN_POINT('Ctrl Pts',(8.58061301328517,31.9563290497598,125.628310601189));
#93493=CARTESIAN_POINT('Ctrl Pts',(8.58447179204486,31.9345679018699,125.696066844188));
#93494=CARTESIAN_POINT('Ctrl Pts',(8.58833057080455,31.909257999171,125.762767772912));
#93495=CARTESIAN_POINT('Ctrl Pts',(8.59218934956424,31.8805269896333,125.828019204947));
#93496=CARTESIAN_POINT('Ctrl Pts',(8.59604569742522,31.8518140796495,125.89322953081));
#93497=CARTESIAN_POINT('Ctrl Pts',(8.5999020452862,31.8196845339681,125.956991728081));
#93498=CARTESIAN_POINT('Ctrl Pts',(8.60375839314718,31.7843146400526,126.018930236961));
#93499=CARTESIAN_POINT('Ctrl Pts',(8.60761360166789,31.7489551960099,126.080850446393));
#93500=CARTESIAN_POINT('Ctrl Pts',(8.6114688101886,31.7103575450951,126.140947615484));
#93501=CARTESIAN_POINT('Ctrl Pts',(8.61532401870931,31.6687437683968,126.198871051422));
#93502=CARTESIAN_POINT('Ctrl Pts',(8.61917937783514,31.6271283660412,126.25679675016));
#93503=CARTESIAN_POINT('Ctrl Pts',(8.62303473696097,31.5824968892007,126.312548153912));
#93504=CARTESIAN_POINT('Ctrl Pts',(8.6268900960868,31.5351135490116,126.365805240194));
#93505=CARTESIAN_POINT('Ctrl Pts',(8.63074949081298,31.487680610272,126.419118073375));
#93506=CARTESIAN_POINT('Ctrl Pts',(8.63460888553917,31.4374903815943,126.46993101341));
#93507=CARTESIAN_POINT('Ctrl Pts',(8.63846828026535,31.38484541259,126.517959401871));
#93508=CARTESIAN_POINT('Ctrl Pts',(8.64232986012025,31.3321706368306,126.566014983252));
#93509=CARTESIAN_POINT('Ctrl Pts',(8.64619143997515,31.2770387296325,126.611282566182));
#93510=CARTESIAN_POINT('Ctrl Pts',(8.65005301983005,31.2197848164688,126.653518238185));
#93511=CARTESIAN_POINT('Ctrl Pts',(8.65392135616211,31.1624307280476,126.695827808533));
#93512=CARTESIAN_POINT('Ctrl Pts',(8.65778969249417,31.102947626487,126.735094608986));
#93513=CARTESIAN_POINT('Ctrl Pts',(8.66165802882622,31.0416984472471,126.771118829301));
#93514=CARTESIAN_POINT('Ctrl Pts',(8.66395572768669,31.0053179060367,126.792516350834));
#93515=CARTESIAN_POINT('Ctrl Pts',(8.66625342654716,30.9683147455938,126.812770750143));
#93516=CARTESIAN_POINT('Ctrl Pts',(8.66855112540763,30.9307683970591,126.831848179718));
#93517=CARTESIAN_POINT('Ctrl Pts',(8.67242019148436,30.8675445752087,126.863972422311));
#93518=CARTESIAN_POINT('Ctrl Pts',(8.67628925756109,30.8025318708695,126.892882616512));
#93519=CARTESIAN_POINT('Ctrl Pts',(8.68015832363782,30.7360901847401,126.918376605995));
#93520=CARTESIAN_POINT('Ctrl Pts',(8.68402162475757,30.6697474975563,126.943832609114));
#93521=CARTESIAN_POINT('Ctrl Pts',(8.68788492587733,30.6019805048365,126.965882338784));
#93522=CARTESIAN_POINT('Ctrl Pts',(8.69174822699708,30.5331725187789,126.984370083356));
#93523=CARTESIAN_POINT('Ctrl Pts',(8.69560699624201,30.4644452484538,127.002836140739));
#93524=CARTESIAN_POINT('Ctrl Pts',(8.69946576548694,30.3946798772693,127.017748387325));
#93525=CARTESIAN_POINT('Ctrl Pts',(8.70332453473188,30.3242768049301,127.029000275082));
#93526=CARTESIAN_POINT('Ctrl Pts',(8.70718087309328,30.253918083952,127.040245074562));
#93527=CARTESIAN_POINT('Ctrl Pts',(8.71103721145469,30.1829229374078,127.047834013581));
#93528=CARTESIAN_POINT('Ctrl Pts',(8.7148935498161,30.1117024997309,127.051711508486));
#93529=CARTESIAN_POINT('Ctrl Pts',(8.71874874886626,30.0405031033212,127.055587857829));
#93530=CARTESIAN_POINT('Ctrl Pts',(8.72260394791642,29.9690790327236,127.055754913527));
#93531=CARTESIAN_POINT('Ctrl Pts',(8.72645914696657,29.8978453674011,127.052209052104));
#93532=CARTESIAN_POINT('Ctrl Pts',(8.73031449666474,29.8266089185103,127.048663052121));
#93533=CARTESIAN_POINT('Ctrl Pts',(8.73416984636291,29.7555633747443,127.041403873315));
#93534=CARTESIAN_POINT('Ctrl Pts',(8.73802519606107,29.6851208979289,127.030479921984));
#93535=CARTESIAN_POINT('Ctrl Pts',(8.74188458148958,29.6146046828372,127.019544535601));
#93536=CARTESIAN_POINT('Ctrl Pts',(8.7457439669181,29.5446932759119,127.004936793299));
#93537=CARTESIAN_POINT('Ctrl Pts',(8.74960335234661,29.4757899215076,126.986756491397));
#93538=CARTESIAN_POINT('Ctrl Pts',(8.75346492296311,29.4068475539533,126.968565895788));
#93539=CARTESIAN_POINT('Ctrl Pts',(8.75732649357962,29.3389148379663,126.946798862138));
#93540=CARTESIAN_POINT('Ctrl Pts',(8.76118806419612,29.2723784533722,126.921604654288));
#93541=CARTESIAN_POINT('Ctrl Pts',(8.76505639148356,29.2057256486734,126.896366363606));
#93542=CARTESIAN_POINT('Ctrl Pts',(8.76892471877099,29.1404744981413,126.867689121859));
#93543=CARTESIAN_POINT('Ctrl Pts',(8.77279304605842,29.076989712482,126.835769476714));
#93544=CARTESIAN_POINT('Ctrl Pts',(8.77509082945434,29.0392797992448,126.816809232359));
#93545=CARTESIAN_POINT('Ctrl Pts',(8.77738861285027,29.0021926314037,126.796705825613));
#93546=CARTESIAN_POINT('Ctrl Pts',(8.7796863962462,28.9657997342526,126.775507638065));
#93547=CARTESIAN_POINT('Ctrl Pts',(8.78355540286644,28.9045213908469,126.739814139667));
#93548=CARTESIAN_POINT('Ctrl Pts',(8.78742440948668,28.8449730340153,126.700874643057));
#93549=CARTESIAN_POINT('Ctrl Pts',(8.79129341610692,28.7875196822617,126.658881864871));
#93550=CARTESIAN_POINT('Ctrl Pts',(8.79218909453321,28.7742191809355,126.649160499887));
#93551=CARTESIAN_POINT('Ctrl Pts',(8.7930847729595,28.7610308635729,126.639275701261));
#93552=CARTESIAN_POINT('Ctrl Pts',(8.79398045138579,28.7479590808042,126.629230216746));
#93553=CARTESIAN_POINT('Ctrl Pts',(8.09385900549202,28.7479590808042,126.629230216746));
#93554=CARTESIAN_POINT('Ctrl Pts',(8.09772727053521,28.6914420071518,126.585797626239));
#93555=CARTESIAN_POINT('Ctrl Pts',(8.1015955355784,28.6372602689121,126.539476708772));
#93556=CARTESIAN_POINT('Ctrl Pts',(8.10546380062159,28.5857065484924,126.490560832547));
#93557=CARTESIAN_POINT('Ctrl Pts',(8.10793412415267,28.5527836832683,126.459322528363));
#93558=CARTESIAN_POINT('Ctrl Pts',(8.11040444768375,28.5209318401603,126.427026677829));
#93559=CARTESIAN_POINT('Ctrl Pts',(8.11287477121484,28.490218582045,126.393756661867));
#93560=CARTESIAN_POINT('Ctrl Pts',(8.11674384460118,28.4421148223202,126.341648453488));
#93561=CARTESIAN_POINT('Ctrl Pts',(8.12061291798752,28.3966176809064,126.28694489407));
#93562=CARTESIAN_POINT('Ctrl Pts',(8.12448199137386,28.3540195505217,126.229937365249));
#93563=CARTESIAN_POINT('Ctrl Pts',(8.12834529980684,28.3114848917257,126.173014778147));
#93564=CARTESIAN_POINT('Ctrl Pts',(8.13220860823982,28.2718409581833,126.113795421894));
#93565=CARTESIAN_POINT('Ctrl Pts',(8.13607191667281,28.2353418126453,126.052605835202));
#93566=CARTESIAN_POINT('Ctrl Pts',(8.13993069320138,28.1988854829067,125.991488027755));
#93567=CARTESIAN_POINT('Ctrl Pts',(8.14378946972996,28.165566861152,125.92840499588));
#93568=CARTESIAN_POINT('Ctrl Pts',(8.14764824625854,28.1355973442775,125.863713088841));
#93569=CARTESIAN_POINT('Ctrl Pts',(8.15150459188144,28.1056467072391,125.799061935632));
#93570=CARTESIAN_POINT('Ctrl Pts',(8.15536093750435,28.0790411929319,125.732804357848));
#93571=CARTESIAN_POINT('Ctrl Pts',(8.15921728312725,28.0559460722781,125.665320891457));
#93572=CARTESIAN_POINT('Ctrl Pts',(8.16307248940628,28.0328577749974,125.597857362821));
#93573=CARTESIAN_POINT('Ctrl Pts',(8.1669276956853,28.0132779695831,125.529169123978));
#93574=CARTESIAN_POINT('Ctrl Pts',(8.17078290196433,27.997322996701,125.459654634435));
#93575=CARTESIAN_POINT('Ctrl Pts',(8.17463825884822,27.9813674005329,125.390137429286));
#93576=CARTESIAN_POINT('Ctrl Pts',(8.17849361573211,27.9690370245609,125.31979438332));
#93577=CARTESIAN_POINT('Ctrl Pts',(8.182348972616,27.9603973463798,125.249035294377));
#93578=CARTESIAN_POINT('Ctrl Pts',(8.18620836511539,27.9517486245691,125.178202137978));
#93579=CARTESIAN_POINT('Ctrl Pts',(8.19006775761479,27.9467983714776,125.106952552449));
#93580=CARTESIAN_POINT('Ctrl Pts',(8.19392715011418,27.9455601860251,125.035701726213));
#93581=CARTESIAN_POINT('Ctrl Pts',(8.19778872774748,27.9443212995293,124.96441055876));
#93582=CARTESIAN_POINT('Ctrl Pts',(8.20165030538077,27.9467986476714,124.893118634925));
#93583=CARTESIAN_POINT('Ctrl Pts',(8.20551188301407,27.9529537216554,124.822238652077));
#93584=CARTESIAN_POINT('Ctrl Pts',(8.20938021715695,27.9591195650244,124.751234652226));
#93585=CARTESIAN_POINT('Ctrl Pts',(8.21324855129984,27.9689759143582,124.68064451366));
#93586=CARTESIAN_POINT('Ctrl Pts',(8.21711688544273,27.9824327851579,124.610872647974));
#93587=CARTESIAN_POINT('Ctrl Pts',(8.21941460431295,27.9904259172992,124.569429451375));
#93588=CARTESIAN_POINT('Ctrl Pts',(8.22171232318318,27.9996883921957,124.528274718171));
#93589=CARTESIAN_POINT('Ctrl Pts',(8.2240100420534,28.0101930999335,124.487490426482));
#93590=CARTESIAN_POINT('Ctrl Pts',(8.22787911571879,28.0278817252034,124.418814736439));
#93591=CARTESIAN_POINT('Ctrl Pts',(8.23174818938418,28.0491645546055,124.350921355076));
#93592=CARTESIAN_POINT('Ctrl Pts',(8.23561726304956,28.0739553689881,124.284213969227));
#93593=CARTESIAN_POINT('Ctrl Pts',(8.23948057176422,28.0987092448589,124.217605977916));
#93594=CARTESIAN_POINT('Ctrl Pts',(8.24334388047887,28.1269605625616,124.152180926039));
#93595=CARTESIAN_POINT('Ctrl Pts',(8.24720718919353,28.1585727771566,124.088329365686));
#93596=CARTESIAN_POINT('Ctrl Pts',(8.25106596600628,28.1901479086537,124.024552707192));
#93597=CARTESIAN_POINT('Ctrl Pts',(8.25492474281903,28.2250758913303,123.96234630707));
#93598=CARTESIAN_POINT('Ctrl Pts',(8.25878351963178,28.2631719946789,123.902081040134));
#93599=CARTESIAN_POINT('Ctrl Pts',(8.26263986554025,28.3012440987176,123.841853738363));
#93600=CARTESIAN_POINT('Ctrl Pts',(8.26649621144872,28.3424801048097,123.783565553315));
#93601=CARTESIAN_POINT('Ctrl Pts',(8.27035255735718,28.3866499450746,123.727561725359));
#93602=CARTESIAN_POINT('Ctrl Pts',(8.27420776392272,28.4308067355261,123.671574443523));
#93603=CARTESIAN_POINT('Ctrl Pts',(8.27806297048826,28.4778953386646,123.617870560131));
#93604=CARTESIAN_POINT('Ctrl Pts',(8.2819181770538,28.5276440902535,123.566763928191));
#93605=CARTESIAN_POINT('Ctrl Pts',(8.28577353422473,28.5773947852999,123.515655299748));
#93606=CARTESIAN_POINT('Ctrl Pts',(8.28962889139566,28.6298054946908,123.467144470758));
#93607=CARTESIAN_POINT('Ctrl Pts',(8.29348424856659,28.6845674420588,123.421508711456));
#93608=CARTESIAN_POINT('Ctrl Pts',(8.29734364135182,28.7393867117677,123.375825182696));
#93609=CARTESIAN_POINT('Ctrl Pts',(8.30120303413705,28.7965617585492,123.333023042882));
#93610=CARTESIAN_POINT('Ctrl Pts',(8.30506242692227,28.8557511400428,123.293338900371));
#93611=CARTESIAN_POINT('Ctrl Pts',(8.30892400484116,28.9149740337277,123.253632289259));
#93612=CARTESIAN_POINT('Ctrl Pts',(8.31278558276005,28.9762131152528,123.217047439008));
#93613=CARTESIAN_POINT('Ctrl Pts',(8.31664716067893,29.039100773748,123.183775828955));
#93614=CARTESIAN_POINT('Ctrl Pts',(8.3205154951039,29.1020984652027,123.150446004399));
#93615=CARTESIAN_POINT('Ctrl Pts',(8.32438382952886,29.1667500517798,123.120441198674));
#93616=CARTESIAN_POINT('Ctrl Pts',(8.32825216395382,29.2326669652735,123.093905150231));
#93617=CARTESIAN_POINT('Ctrl Pts',(8.33054988026653,29.2718203451986,123.078143247384));
#93618=CARTESIAN_POINT('Ctrl Pts',(8.33284759657924,29.311419819351,123.063604224152));
#93619=CARTESIAN_POINT('Ctrl Pts',(8.33514531289195,29.3513818111861,123.050309766235));
#93620=CARTESIAN_POINT('Ctrl Pts',(8.33901438538704,29.4186729047829,123.027923529439));
#93621=CARTESIAN_POINT('Ctrl Pts',(8.34288345788212,29.4872561137565,123.008981234008));
#93622=CARTESIAN_POINT('Ctrl Pts',(8.3467525303772,29.5567455212836,122.993629388772));
#93623=CARTESIAN_POINT('Ctrl Pts',(8.35061583791992,29.6261313889768,122.978300417922));
#93624=CARTESIAN_POINT('Ctrl Pts',(8.35447914546264,29.6964203045437,122.966551381999));
#93625=CARTESIAN_POINT('Ctrl Pts',(8.35834245300537,29.7672100913159,122.958479385136));
#93626=CARTESIAN_POINT('Ctrl Pts',(8.36220122864938,29.8379168372896,122.950416857225));
#93627=CARTESIAN_POINT('Ctrl Pts',(8.3660600042934,29.9091228070739,122.946022855284));
#93628=CARTESIAN_POINT('Ctrl Pts',(8.36991877993741,29.9804162215998,122.945343328407));
#93629=CARTESIAN_POINT('Ctrl Pts',(8.37377512467975,30.0516647236204,122.944664229609));
#93630=CARTESIAN_POINT('Ctrl Pts',(8.37763146942208,30.1230000764747,122.947694967979));
#93631=CARTESIAN_POINT('Ctrl Pts',(8.38148781416442,30.1940074483337,122.954429499506));
#93632=CARTESIAN_POINT('Ctrl Pts',(8.38534301956812,30.264993841404,122.961162041348));
#93633=CARTESIAN_POINT('Ctrl Pts',(8.38919822497183,30.3356519625006,122.971596158081));
#93634=CARTESIAN_POINT('Ctrl Pts',(8.39305343037553,30.4055707893079,122.985673835408));
#93635=CARTESIAN_POINT('Ctrl Pts',(8.39690878639061,30.4754923476351,122.999752062707));
#93636=CARTESIAN_POINT('Ctrl Pts',(8.4007641424057,30.544674078537,123.017474035159));
#93637=CARTESIAN_POINT('Ctrl Pts',(8.40461949842078,30.6127155661947,123.038730717764));
#93638=CARTESIAN_POINT('Ctrl Pts',(8.4084788900672,30.6808282769402,123.060009651008));
#93639=CARTESIAN_POINT('Ctrl Pts',(8.41233828171362,30.7477978971905,123.084830535264));
#93640=CARTESIAN_POINT('Ctrl Pts',(8.41619767336005,30.8132404560791,123.113034837869));
#93641=CARTESIAN_POINT('Ctrl Pts',(8.42005925014802,30.8787200677644,123.141255109414));
#93642=CARTESIAN_POINT('Ctrl Pts',(8.42392082693599,30.9426704612239,123.172862397432));
#93643=CARTESIAN_POINT('Ctrl Pts',(8.42778240372396,31.0047313875944,123.207651707596));
#93644=CARTESIAN_POINT('Ctrl Pts',(8.43165073704272,31.0669009008409,123.242501887985));
#93645=CARTESIAN_POINT('Ctrl Pts',(8.43551907036148,31.1271739356095,123.280544946878));
#93646=CARTESIAN_POINT('Ctrl Pts',(8.43938740368024,31.1852189857341,123.32153238984));
#93647=CARTESIAN_POINT('Ctrl Pts',(8.44168513036367,31.2196967955612,123.345878260172));
#93648=CARTESIAN_POINT('Ctrl Pts',(8.44398285704709,31.253389149455,123.371262169097));
#93649=CARTESIAN_POINT('Ctrl Pts',(8.44628058373052,31.2862324985407,123.397625661027));
#93650=CARTESIAN_POINT('Ctrl Pts',(8.45010049336537,31.3408336948092,123.441454266736));
#93651=CARTESIAN_POINT('Ctrl Pts',(8.45392040300023,31.3933122556876,123.488173581411));
#93652=CARTESIAN_POINT('Ctrl Pts',(8.45774031263508,31.4433401853721,123.537547719825));
#93653=CARTESIAN_POINT('Ctrl Pts',(8.46155371406939,31.493282879585,123.586837736669));
#93654=CARTESIAN_POINT('Ctrl Pts',(8.4653671155037,31.5407828803758,123.63877324907));
#93655=CARTESIAN_POINT('Ctrl Pts',(8.46918051693801,31.5855446175212,123.693077726738));
#93656=CARTESIAN_POINT('Ctrl Pts',(8.4729902881967,31.6302637436357,123.747330509142));
#93657=CARTESIAN_POINT('Ctrl Pts',(8.4768000594554,31.6722494565306,123.803947404127));
#93658=CARTESIAN_POINT('Ctrl Pts',(8.48060983071409,31.7112435016815,123.862615614468));
#93659=CARTESIAN_POINT('Ctrl Pts',(8.48441732747834,31.750214266763,123.921248798947));
#93660=CARTESIAN_POINT('Ctrl Pts',(8.48822482424259,31.7861966299445,123.981930455412));
#93661=CARTESIAN_POINT('Ctrl Pts',(8.49203232100684,31.8189742451768,124.044316863242));
#93662=CARTESIAN_POINT('Ctrl Pts',(8.49583889577238,31.8517439231946,124.106688163984));
#93663=CARTESIAN_POINT('Ctrl Pts',(8.49964547053792,31.8813101621532,124.170762954494));
#93664=CARTESIAN_POINT('Ctrl Pts',(8.50345204530346,31.9075023321529,124.236172522534));
#93665=CARTESIAN_POINT('Ctrl Pts',(8.50726133137383,31.9337131580207,124.301628679776));
#93666=CARTESIAN_POINT('Ctrl Pts',(8.51107061744421,31.9565449262708,124.368421050014));
#93667=CARTESIAN_POINT('Ctrl Pts',(8.51487990351458,31.9758754657729,124.436161631088));
#93668=CARTESIAN_POINT('Ctrl Pts',(8.51869054789537,31.9952128981343,124.503926367014));
#93669=CARTESIAN_POINT('Ctrl Pts',(8.52250119227616,32.0110465016042,124.572639500276));
#93670=CARTESIAN_POINT('Ctrl Pts',(8.52631183665695,32.0233049403347,124.641901297242));
#93671=CARTESIAN_POINT('Ctrl Pts',(8.53012846309201,32.0355826226992,124.71127182328));
#93672=CARTESIAN_POINT('Ctrl Pts',(8.53394508952706,32.0442738707611,124.781192236842));
#93673=CARTESIAN_POINT('Ctrl Pts',(8.53776171596212,32.0493591892279,124.85125701352));
#93674=CARTESIAN_POINT('Ctrl Pts',(8.54048290413684,32.0529849327247,124.901211978985));
#93675=CARTESIAN_POINT('Ctrl Pts',(8.54320409231157,32.0547787225466,124.951240233068));
#93676=CARTESIAN_POINT('Ctrl Pts',(8.54592528048629,32.0547496520905,125.001195714812));
#93677=CARTESIAN_POINT('Origin',(-1.54592528053767,30.,125.));
#93678=CARTESIAN_POINT('',(7.39391265022091,28.7479590808041,126.629230216746));
#93679=CARTESIAN_POINT('',(7.45211278982742,28.7479590808042,126.629230216746));
#93680=CARTESIAN_POINT('',(-1.54592528053767,28.7479590808042,126.629230216746));
#93681=CARTESIAN_POINT('',(7.90407471950836,32.0547494456331,124.998490639097));
#93682=CARTESIAN_POINT('Ctrl Pts',(7.45211278982742,28.7479590808042,126.629230216746));
#93683=CARTESIAN_POINT('Ctrl Pts',(7.45597763088531,28.6916459119271,126.585954324243));
#93684=CARTESIAN_POINT('Ctrl Pts',(7.4598424719432,28.6374854701366,126.539683431744));
#93685=CARTESIAN_POINT('Ctrl Pts',(7.46370731300109,28.5858120325335,126.490660912204));
#93686=CARTESIAN_POINT('Ctrl Pts',(7.46756704224479,28.5342069405642,126.441703232073));
#93687=CARTESIAN_POINT('Ctrl Pts',(7.47142677148849,28.4850826687522,126.390001486985));
#93688=CARTESIAN_POINT('Ctrl Pts',(7.47528650073219,28.4387407708862,126.335839504584));
#93689=CARTESIAN_POINT('Ctrl Pts',(7.47914342184703,28.3924325888621,126.281716927492));
#93690=CARTESIAN_POINT('Ctrl Pts',(7.48300034296188,28.348903079861,126.225138031865));
#93691=CARTESIAN_POINT('Ctrl Pts',(7.48685726407672,28.3084162342584,126.166422704674));
#93692=CARTESIAN_POINT('Ctrl Pts',(7.49071266934076,28.2679453008343,126.107730453837));
#93693=CARTESIAN_POINT('Ctrl Pts',(7.4945680746048,28.230514932911,126.046903837491));
#93694=CARTESIAN_POINT('Ctrl Pts',(7.49842347986884,28.196347115702,125.984293571788));
#93695=CARTESIAN_POINT('Ctrl Pts',(7.50227865956733,28.162181297526,125.921686969181));
#93696=CARTESIAN_POINT('Ctrl Pts',(7.50613383926581,28.1312778823822,125.857297351586));
#93697=CARTESIAN_POINT('Ctrl Pts',(7.5099890189643,28.1038131550659,125.791500481111));
#93698=CARTESIAN_POINT('Ctrl Pts',(7.51384799268039,28.0763213987479,125.725638857627));
#93699=CARTESIAN_POINT('Ctrl Pts',(7.51770696639648,28.0522752778304,125.658367664183));
#93700=CARTESIAN_POINT('Ctrl Pts',(7.52156594011256,28.031802750325,125.590082323809));
#93701=CARTESIAN_POINT('Ctrl Pts',(7.5254267610758,28.0113204228518,125.521764296013));
#93702=CARTESIAN_POINT('Ctrl Pts',(7.52928758203904,27.9944152119565,125.452431626849));
#93703=CARTESIAN_POINT('Ctrl Pts',(7.53314840300228,27.9811643120378,125.38249186594));
#93704=CARTESIAN_POINT('Ctrl Pts',(7.53701633832392,27.9678889946048,125.312423226606));
#93705=CARTESIAN_POINT('Ctrl Pts',(7.54088427364555,27.958281507931,125.241745742989));
#93706=CARTESIAN_POINT('Ctrl Pts',(7.54475220896719,27.9523672730575,125.170873573305));
#93707=CARTESIAN_POINT('Ctrl Pts',(7.54817615316203,27.9471319191857,125.108136651979));
#93708=CARTESIAN_POINT('Ctrl Pts',(7.55160009735686,27.9447898338038,125.045247454545));
#93709=CARTESIAN_POINT('Ctrl Pts',(7.5550240415517,27.945324596286,124.982491491417));
#93710=CARTESIAN_POINT('Ctrl Pts',(7.55889311490067,27.9459288804537,124.911576952333));
#93711=CARTESIAN_POINT('Ctrl Pts',(7.56276218824965,27.9502099474241,124.840554831223));
#93712=CARTESIAN_POINT('Ctrl Pts',(7.56663126159862,27.9581814784833,124.769837692722));
#93713=CARTESIAN_POINT('Ctrl Pts',(7.57049456999505,27.9661411318927,124.699225923365));
#93714=CARTESIAN_POINT('Ctrl Pts',(7.57435787839147,27.9777802804095,124.628918713388));
#93715=CARTESIAN_POINT('Ctrl Pts',(7.5782211867879,27.9930605972998,124.55932801724));
#93716=CARTESIAN_POINT('Ctrl Pts',(7.58207996328128,28.00832298942,124.489818955344));
#93717=CARTESIAN_POINT('Ctrl Pts',(7.58593873977465,28.0272179619513,124.421025209909));
#93718=CARTESIAN_POINT('Ctrl Pts',(7.58979751626803,28.0496556793524,124.353351259633));
#93719=CARTESIAN_POINT('Ctrl Pts',(7.59365386185659,28.0720792617147,124.285719941765));
#93720=CARTESIAN_POINT('Ctrl Pts',(7.59751020744516,28.0980410085421,124.219207479496));
#93721=CARTESIAN_POINT('Ctrl Pts',(7.60136655303372,28.127400902946,124.154204407547));
#93722=CARTESIAN_POINT('Ctrl Pts',(7.6052217592793,28.1567521230781,124.089220540514));
#93723=CARTESIAN_POINT('Ctrl Pts',(7.60907696552488,28.1894992977735,124.02574562096));
#93724=CARTESIAN_POINT('Ctrl Pts',(7.61293217177046,28.2254544719855,123.964149754306));
#93725=CARTESIAN_POINT('Ctrl Pts',(7.61678752862185,28.2614110508067,123.902551481375));
#93726=CARTESIAN_POINT('Ctrl Pts',(7.62064288547323,28.3005756311566,123.842832825513));
#93727=CARTESIAN_POINT('Ctrl Pts',(7.62449824232462,28.3427154187412,123.785337339332));
#93728=CARTESIAN_POINT('Ctrl Pts',(7.62835763479315,28.3848993163929,123.727781669417));
#93729=CARTESIAN_POINT('Ctrl Pts',(7.63221702726169,28.4300643503926,123.672454207248));
#93730=CARTESIAN_POINT('Ctrl Pts',(7.63607641973023,28.4779362183637,123.61966692167));
#93731=CARTESIAN_POINT('Ctrl Pts',(7.63993799733355,28.5258351907262,123.56684974866));
#93732=CARTESIAN_POINT('Ctrl Pts',(7.64379957493687,28.5764437031346,123.516575957801));
#93733=CARTESIAN_POINT('Ctrl Pts',(7.6476611525402,28.629451173511,123.469120031907));
#93734=CARTESIAN_POINT('Ctrl Pts',(7.65152948665481,28.6825513898086,123.421581073497));
#93735=CARTESIAN_POINT('Ctrl Pts',(7.65539782076942,28.738058565867,123.376870128474));
#93736=CARTESIAN_POINT('Ctrl Pts',(7.65926615488404,28.7956302673745,123.335220402085));
#93737=CARTESIAN_POINT('Ctrl Pts',(7.66156387405278,28.8298267969945,123.310481232235));
#93738=CARTESIAN_POINT('Ctrl Pts',(7.66386159322151,28.8647511726965,123.286821267237));
#93739=CARTESIAN_POINT('Ctrl Pts',(7.66615931239025,28.9003275143506,123.264281708685));
#93740=CARTESIAN_POINT('Ctrl Pts',(7.67002838578168,28.9602336502836,123.226327894557));
#93741=CARTESIAN_POINT('Ctrl Pts',(7.67389745917311,29.0222243255323,123.191404757273));
#93742=CARTESIAN_POINT('Ctrl Pts',(7.67776653256454,29.0859603468053,123.159747551316));
#93743=CARTESIAN_POINT('Ctrl Pts',(7.68162984100372,29.1496014008647,123.128137514865));
#93744=CARTESIAN_POINT('Ctrl Pts',(7.6854931494429,29.2149822073397,123.099783964679));
#93745=CARTESIAN_POINT('Ctrl Pts',(7.68935645788208,29.2817358782989,123.074878130097));
#93746=CARTESIAN_POINT('Ctrl Pts',(7.69321523441845,29.3484112430204,123.05000151162));
#93747=CARTESIAN_POINT('Ctrl Pts',(7.69707401095481,29.4164558203857,123.028564744215));
#93748=CARTESIAN_POINT('Ctrl Pts',(7.70093278749118,29.4854810666423,123.010711727849));
#93749=CARTESIAN_POINT('Ctrl Pts',(7.70478913312285,29.5544628292212,122.992869958308));
#93750=CARTESIAN_POINT('Ctrl Pts',(7.70864547875453,29.6244235658091,122.978607582025));
#93751=CARTESIAN_POINT('Ctrl Pts',(7.7125018243862,29.6949592310368,122.968018776718));
#93752=CARTESIAN_POINT('Ctrl Pts',(7.71635703067495,29.7654740567655,122.957433099834));
#93753=CARTESIAN_POINT('Ctrl Pts',(7.7202122369637,29.8365629937725,122.950518911299));
#93754=CARTESIAN_POINT('Ctrl Pts',(7.72406744325245,29.9078131602965,122.947319033779));
#93755=CARTESIAN_POINT('Ctrl Pts',(7.727922800147,29.9790661102483,122.944119031254));
#93756=CARTESIAN_POINT('Ctrl Pts',(7.73177815704155,30.0504798168263,122.944633647418));
#93757=CARTESIAN_POINT('Ctrl Pts',(7.7356335139361,30.1216393872444,122.948853632241));
#93758=CARTESIAN_POINT('Ctrl Pts',(7.73949290644749,30.1928734443492,122.953078034358));
#93759=CARTESIAN_POINT('Ctrl Pts',(7.74335229895888,30.2638523483338,122.961015518905));
#93760=CARTESIAN_POINT('Ctrl Pts',(7.74721169147027,30.3341652288182,122.972604833204));
#93761=CARTESIAN_POINT('Ctrl Pts',(7.75107326911633,30.4045179194833,122.984200709212));
#93762=CARTESIAN_POINT('Ctrl Pts',(7.7549348467624,30.4742033611939,122.999452427044));
#93763=CARTESIAN_POINT('Ctrl Pts',(7.75879642440846,30.5428225004122,123.018247922785));
#93764=CARTESIAN_POINT('Ctrl Pts',(7.76266475856518,30.6115617009079,123.037076304558));
#93765=CARTESIAN_POINT('Ctrl Pts',(7.7665330927219,30.679230412665,123.059460691033));
#93766=CARTESIAN_POINT('Ctrl Pts',(7.77040142687861,30.7454469857162,123.085239870379));
#93767=CARTESIAN_POINT('Ctrl Pts',(7.77269914566201,30.7847784026796,123.100552225052));
#93768=CARTESIAN_POINT('Ctrl Pts',(7.77499686444541,30.8235978903797,123.117061396472));
#93769=CARTESIAN_POINT('Ctrl Pts',(7.77729458322881,30.8618296789442,123.134725980723));
#93770=CARTESIAN_POINT('Ctrl Pts',(7.781163656479,30.9262072657535,123.164470948163));
#93771=CARTESIAN_POINT('Ctrl Pts',(7.78503272972918,30.9891692283516,123.197610957942));
#93772=CARTESIAN_POINT('Ctrl Pts',(7.78890180297937,31.050333952957,123.233988632606));
#93773=CARTESIAN_POINT('Ctrl Pts',(7.79276511127721,31.1114075415978,123.270312104222));
#93774=CARTESIAN_POINT('Ctrl Pts',(7.79662841957505,31.1706887936818,123.309863418628));
#93775=CARTESIAN_POINT('Ctrl Pts',(7.80049172787288,31.2278180622896,123.352438053239));
#93776=CARTESIAN_POINT('Ctrl Pts',(7.80435050426844,31.2848803146919,123.39496274514));
#93777=CARTESIAN_POINT('Ctrl Pts',(7.80820928066399,31.3397952103248,123.440503423738));
#93778=CARTESIAN_POINT('Ctrl Pts',(7.81206805705954,31.3922311203958,123.488811702698));
#93779=CARTESIAN_POINT('Ctrl Pts',(7.81592440255081,31.4446339975397,123.537089549005));
#93780=CARTESIAN_POINT('Ctrl Pts',(7.81978074804207,31.4945606310389,123.588131208226));
#93781=CARTESIAN_POINT('Ctrl Pts',(7.82363709353333,31.5417127584062,123.64164830288));
#93782=CARTESIAN_POINT('Ctrl Pts',(7.82749229968227,31.5888509548604,123.695149586116));
#93783=CARTESIAN_POINT('Ctrl Pts',(7.83134750583121,31.6332159515802,123.751124488543));
#93784=CARTESIAN_POINT('Ctrl Pts',(7.83520271198014,31.6745478391525,123.809249355705));
#93785=CARTESIAN_POINT('Ctrl Pts',(7.83905806873569,31.715881341387,123.867376493559));
#93786=CARTESIAN_POINT('Ctrl Pts',(7.84291342549123,31.7541812195027,123.927653365725));
#93787=CARTESIAN_POINT('Ctrl Pts',(7.84676878224677,31.7892302219191,123.989726385838));
#93788=CARTESIAN_POINT('Ctrl Pts',(7.85062817462134,31.8243159121,124.051864381277));
#93789=CARTESIAN_POINT('Ctrl Pts',(7.85448756699591,31.8561436943397,124.115801853944));
#93790=CARTESIAN_POINT('Ctrl Pts',(7.85834695937048,31.8845421883571,124.181160392505));
#93791=CARTESIAN_POINT('Ctrl Pts',(7.86220853688075,31.9129567612171,124.246555936185));
#93792=CARTESIAN_POINT('Ctrl Pts',(7.86607011439102,31.9379380104941,124.313373692206));
#93793=CARTESIAN_POINT('Ctrl Pts',(7.86993169190128,31.95936365367,124.381217618886));
#93794=CARTESIAN_POINT('Ctrl Pts',(7.87380002592529,31.9808267848032,124.449180250532));
#93795=CARTESIAN_POINT('Ctrl Pts',(7.8776683599493,31.9987217670988,124.518172167164));
#93796=CARTESIAN_POINT('Ctrl Pts',(7.8815366939733,32.0129770484167,124.587785292538));
#93797=CARTESIAN_POINT('Ctrl Pts',(7.88383441400466,32.0214444261647,124.629134222498));
#93798=CARTESIAN_POINT('Ctrl Pts',(7.88613213403602,32.0286286525971,124.670702169053));
#93799=CARTESIAN_POINT('Ctrl Pts',(7.88842985406737,32.0345234180833,124.712403018495));
#93800=CARTESIAN_POINT('Ctrl Pts',(7.89364480919903,32.0479023054596,124.807048169263));
#93801=CARTESIAN_POINT('Ctrl Pts',(7.89885976433068,32.0546790423352,124.90264805037));
#93802=CARTESIAN_POINT('Ctrl Pts',(7.90407471946233,32.0547494456325,124.998490638251));
#93803=CARTESIAN_POINT('Ctrl Pts',(7.90407471950836,32.0547494456331,124.998490639097));
#93804=CARTESIAN_POINT('Ctrl Pts',(7.90805348639992,32.0548031600265,125.071614051636));
#93805=CARTESIAN_POINT('Ctrl Pts',(7.91203225329149,32.0509484181439,125.144885851501));
#93806=CARTESIAN_POINT('Ctrl Pts',(7.91601102018305,32.0431692286218,125.2178464269));
#93807=CARTESIAN_POINT('Ctrl Pts',(7.91981486837858,32.0357320359355,125.287599433457));
#93808=CARTESIAN_POINT('Ctrl Pts',(7.92361871657411,32.0247082535841,125.357067439174));
#93809=CARTESIAN_POINT('Ctrl Pts',(7.92742256476964,32.0101370400902,125.42584814495));
#93810=CARTESIAN_POINT('Ctrl Pts',(7.93122379847059,31.9955758418117,125.494581575763));
#93811=CARTESIAN_POINT('Ctrl Pts',(7.93502503217154,31.9774721486446,125.562628154096));
#93812=CARTESIAN_POINT('Ctrl Pts',(7.93882626587248,31.9559166138979,125.629593330634));
#93813=CARTESIAN_POINT('Ctrl Pts',(7.94262624496905,31.9343681935962,125.696536405188));
#93814=CARTESIAN_POINT('Ctrl Pts',(7.94642622406562,31.9093703451663,125.762398309188));
#93815=CARTESIAN_POINT('Ctrl Pts',(7.95022620316219,31.8810637191461,125.826799157602));
#93816=CARTESIAN_POINT('Ctrl Pts',(7.9540262856104,31.8527563232437,125.891201757588));
#93817=CARTESIAN_POINT('Ctrl Pts',(7.95782636805862,31.8211401758106,125.954142765617));
#93818=CARTESIAN_POINT('Ctrl Pts',(7.96162645050683,31.7864034775327,126.015263600233));
#93819=CARTESIAN_POINT('Ctrl Pts',(7.96543037574972,31.7516316521226,126.076446242671));
#93820=CARTESIAN_POINT('Ctrl Pts',(7.9692343009926,31.7137332295808,126.13580460387));
#93821=CARTESIAN_POINT('Ctrl Pts',(7.97303822623548,31.672941063085,126.193007025102));
#93822=CARTESIAN_POINT('Ctrl Pts',(7.97684442188819,31.6321245493875,126.250243588157));
#93823=CARTESIAN_POINT('Ctrl Pts',(7.98065061754089,31.5884111702421,126.305321261529));
#93824=CARTESIAN_POINT('Ctrl Pts',(7.9844568131936,31.5420737759433,126.357941836769));
#93825=CARTESIAN_POINT('Ctrl Pts',(7.98826926353303,31.4956602358255,126.410648882923));
#93826=CARTESIAN_POINT('Ctrl Pts',(7.99208171387245,31.4466144322414,126.460890422923));
#93827=CARTESIAN_POINT('Ctrl Pts',(7.99589416421188,31.3952448791565,126.508406208449));
#93828=CARTESIAN_POINT('Ctrl Pts',(7.99711781777657,31.3787571793434,126.52365699342));
#93829=CARTESIAN_POINT('Ctrl Pts',(7.99834147134126,31.3620303335553,126.538627302503));
#93830=CARTESIAN_POINT('Ctrl Pts',(7.99956512490594,31.3450751861379,126.553309468888));
#93831=CARTESIAN_POINT('Ctrl Pts',(8.00343419857232,31.2914646575736,126.599733052296));
#93832=CARTESIAN_POINT('Ctrl Pts',(8.0073032722387,31.2353429211326,126.643468858699));
#93833=CARTESIAN_POINT('Ctrl Pts',(8.01117234590508,31.177010502966,126.684233902523));
#93834=CARTESIAN_POINT('Ctrl Pts',(8.01503565462073,31.1187650005694,126.724938206105));
#93835=CARTESIAN_POINT('Ctrl Pts',(8.01889896333638,31.0583157497566,126.762680257503));
#93836=CARTESIAN_POINT('Ctrl Pts',(8.02276227205203,30.9959971979523,126.79721649897));
#93837=CARTESIAN_POINT('Ctrl Pts',(8.02662104886578,30.9337517496933,126.831712227274));
#93838=CARTESIAN_POINT('Ctrl Pts',(8.03047982567953,30.8696417789356,126.863009381168));
#93839=CARTESIAN_POINT('Ctrl Pts',(8.03433860249328,30.8040301727672,126.890907994531));
#93840=CARTESIAN_POINT('Ctrl Pts',(8.03819494840275,30.7384598997835,126.918789032671));
#93841=CARTESIAN_POINT('Ctrl Pts',(8.04205129431221,30.6713903141947,126.94327558829));
#93842=CARTESIAN_POINT('Ctrl Pts',(8.04590764022167,30.6032070117903,126.964214566545));
#93843=CARTESIAN_POINT('Ctrl Pts',(8.04976284678821,30.5350438538867,126.985147358457));
#93844=CARTESIAN_POINT('Ctrl Pts',(8.05361805335475,30.4657680965384,127.002534511279));
#93845=CARTESIAN_POINT('Ctrl Pts',(8.05747325992129,30.3957816951196,127.016272405284));
#93846=CARTESIAN_POINT('Ctrl Pts',(8.0613286170932,30.3257925596506,127.030010835966));
#93847=CARTESIAN_POINT('Ctrl Pts',(8.06518397426512,30.2550932021072,127.040099633387));
#93848=CARTESIAN_POINT('Ctrl Pts',(8.06903933143703,30.1840952941523,127.046486375516));
#93849=CARTESIAN_POINT('Ctrl Pts',(8.07289872422324,30.113023068784,127.052879802998));
#93850=CARTESIAN_POINT('Ctrl Pts',(8.07675811700946,30.0416521539894,127.055563395913));
#93851=CARTESIAN_POINT('Ctrl Pts',(8.08061750979567,29.9703979606998,127.054536756003));
#93852=CARTESIAN_POINT('Ctrl Pts',(8.08447908771554,29.8991034242929,127.053509534825));
#93853=CARTESIAN_POINT('Ctrl Pts',(8.08834066563541,29.8279262258892,127.048767931317));
#93854=CARTESIAN_POINT('Ctrl Pts',(8.09220224355529,29.7572776307531,127.040363549461));
#93855=CARTESIAN_POINT('Ctrl Pts',(8.09607057798121,29.6865054235418,127.031944462668));
#93856=CARTESIAN_POINT('Ctrl Pts',(8.09993891240713,29.6162641450483,127.019849884887));
#93857=CARTESIAN_POINT('Ctrl Pts',(8.10380724683306,29.5469551431653,127.0041826065));
#93858=CARTESIAN_POINT('Ctrl Pts',(8.10610496313687,29.5057869280907,126.994876544246));
#93859=CARTESIAN_POINT('Ctrl Pts',(8.10840267944068,29.4649473669824,126.984310949874));
#93860=CARTESIAN_POINT('Ctrl Pts',(8.11070039574449,29.4245175347868,126.972515524586));
#93861=CARTESIAN_POINT('Ctrl Pts',(8.1145684545292,29.3564564920335,126.952658678756));
#93862=CARTESIAN_POINT('Ctrl Pts',(8.11843651331391,29.2892911078502,126.929236177456));
#93863=CARTESIAN_POINT('Ctrl Pts',(8.12230457209862,29.2234218115874,126.902346939909));
#93864=CARTESIAN_POINT('Ctrl Pts',(8.12616759077854,29.1576383434297,126.875492739207));
#93865=CARTESIAN_POINT('Ctrl Pts',(8.13003060945846,29.0931480601149,126.845180941222));
#93866=CARTESIAN_POINT('Ctrl Pts',(8.13389362813838,29.0303368956155,126.811560384446));
#93867=CARTESIAN_POINT('Ctrl Pts',(8.13775232965377,28.9675959265135,126.777977400741));
#93868=CARTESIAN_POINT('Ctrl Pts',(8.14161103116916,28.9065307762037,126.741093228774));
#93869=CARTESIAN_POINT('Ctrl Pts',(8.14546973268454,28.8475062487581,126.701104263662));
#93870=CARTESIAN_POINT('Ctrl Pts',(8.14768435246726,28.8136303748079,126.678153446431));
#93871=CARTESIAN_POINT('Ctrl Pts',(8.14989897224998,28.7804262675646,126.654180801346));
#93872=CARTESIAN_POINT('Ctrl Pts',(8.1521135920327,28.7479590808041,126.629230216746));
#93873=CARTESIAN_POINT('',(7.8459252805834,32.0547497348706,125.001043814792));
#93874=CARTESIAN_POINT('Ctrl Pts',(7.8459252805834,32.0547497348706,125.001043814792));
#93875=CARTESIAN_POINT('Ctrl Pts',(7.85018308156599,32.0547096589831,125.079933211422));
#93876=CARTESIAN_POINT('Ctrl Pts',(7.85444088254858,32.0501221476059,125.158666320287));
#93877=CARTESIAN_POINT('Ctrl Pts',(7.85869868353118,32.041065772293,125.236744747933));
#93878=CARTESIAN_POINT('Ctrl Pts',(7.86297170281514,32.0319770275365,125.315102244763));
#93879=CARTESIAN_POINT('Ctrl Pts',(7.8672447220991,32.0183875520912,125.392800086567));
#93880=CARTESIAN_POINT('Ctrl Pts',(7.87151774138306,32.0004267208688,125.469351144596));
#93881=CARTESIAN_POINT('Ctrl Pts',(7.87581130795464,31.9823795229954,125.546270306888));
#93882=CARTESIAN_POINT('Ctrl Pts',(7.88010487452622,31.9599189696943,125.62203135299));
#93883=CARTESIAN_POINT('Ctrl Pts',(7.8843984410978,31.9332245829694,125.696161097953));
#93884=CARTESIAN_POINT('Ctrl Pts',(7.88646703724444,31.9203635024212,125.731876045474));
#93885=CARTESIAN_POINT('Ctrl Pts',(7.88853563339108,31.9065203606893,125.767212670556));
#93886=CARTESIAN_POINT('Ctrl Pts',(7.89060422953772,31.8917190494166,125.802120066183));
#93887=CARTESIAN_POINT('Ctrl Pts',(7.894473302929,31.8640348831796,125.867410372268));
#93888=CARTESIAN_POINT('Ctrl Pts',(7.89834237632028,31.8329124035663,125.931393656006));
#93889=CARTESIAN_POINT('Ctrl Pts',(7.90221144971156,31.7984967817137,125.993683495216));
#93890=CARTESIAN_POINT('Ctrl Pts',(7.90607475815059,31.7641324394302,126.055880522036));
#93891=CARTESIAN_POINT('Ctrl Pts',(7.90993806658963,31.7264849278007,126.116388691164));
#93892=CARTESIAN_POINT('Ctrl Pts',(7.91380137502866,31.6857472373416,126.174842038018));
#93893=CARTESIAN_POINT('Ctrl Pts',(7.91766015156488,31.6450573347453,126.233226815435));
#93894=CARTESIAN_POINT('Ctrl Pts',(7.9215189281011,31.6012847301518,126.289561161906));
#93895=CARTESIAN_POINT('Ctrl Pts',(7.92537770463731,31.5546671460301,126.343505722933));
#93896=CARTESIAN_POINT('Ctrl Pts',(7.92923405026884,31.508078929482,126.397416300628));
#93897=CARTESIAN_POINT('Ctrl Pts',(7.93309039590037,31.4586496060732,126.448939713055));
#93898=CARTESIAN_POINT('Ctrl Pts',(7.93694674153189,31.4066579295296,126.497768684341));
#93899=CARTESIAN_POINT('Ctrl Pts',(7.9408019478205,31.3546816137329,126.546583229288));
#93900=CARTESIAN_POINT('Ctrl Pts',(7.9446571541091,31.3001448016416,126.592704581117));
#93901=CARTESIAN_POINT('Ctrl Pts',(7.9485123603977,31.2433627249165,126.635862676629));
#93902=CARTESIAN_POINT('Ctrl Pts',(7.9523677172921,31.1865784299676,126.679022458137));
#93903=CARTESIAN_POINT('Ctrl Pts',(7.95622307418651,31.1275490843282,126.719218461297));
#93904=CARTESIAN_POINT('Ctrl Pts',(7.96007843108091,31.0666211920245,126.756222308031));
#93905=CARTESIAN_POINT('Ctrl Pts',(7.96393782359215,31.0056295231018,126.793264888752));
#93906=CARTESIAN_POINT('Ctrl Pts',(7.9677972161034,30.9427357564469,126.827108390158));
#93907=CARTESIAN_POINT('Ctrl Pts',(7.97165660861464,30.8783126662094,126.857569493418));
#93908=CARTESIAN_POINT('Ctrl Pts',(7.97551818626056,30.813853100509,126.888047843333));
#93909=CARTESIAN_POINT('Ctrl Pts',(7.97937976390648,30.7478629371237,126.915139798214));
#93910=CARTESIAN_POINT('Ctrl Pts',(7.9832413415524,30.6807341318648,126.938710551943));
#93911=CARTESIAN_POINT('Ctrl Pts',(7.98710967570898,30.6134878729303,126.962322546859));
#93912=CARTESIAN_POINT('Ctrl Pts',(7.99097800986555,30.5450994607886,126.982400903193));
#93913=CARTESIAN_POINT('Ctrl Pts',(7.99484634402213,30.4759744918409,126.998861137152));
#93914=CARTESIAN_POINT('Ctrl Pts',(7.99714406280685,30.4349155416016,127.008638211013));
#93915=CARTESIAN_POINT('Ctrl Pts',(7.99944178159156,30.3935969099127,127.017139742854));
#93916=CARTESIAN_POINT('Ctrl Pts',(8.00173950037628,30.3521044663438,127.024356689736));
#93917=CARTESIAN_POINT('Ctrl Pts',(8.00560732713476,30.2822588505194,127.03650521742));
#93918=CARTESIAN_POINT('Ctrl Pts',(8.00947515389324,30.2116469980773,127.045058506921));
#93919=CARTESIAN_POINT('Ctrl Pts',(8.01334298065171,30.1406719027978,127.04992901786));
#93920=CARTESIAN_POINT('Ctrl Pts',(8.01720559832235,30.0697923949189,127.054792969321));
#93921=CARTESIAN_POINT('Ctrl Pts',(8.02106821599298,29.9985510945436,127.055983946858));
#93922=CARTESIAN_POINT('Ctrl Pts',(8.02493083366361,29.927359911755,127.053465602361));
#93923=CARTESIAN_POINT('Ctrl Pts',(8.02878954173858,29.8562407859919,127.050949806837));
#93924=CARTESIAN_POINT('Ctrl Pts',(8.03264824981354,29.7851721600219,127.044732155691));
#93925=CARTESIAN_POINT('Ctrl Pts',(8.0365069578885,29.7145680506028,127.034828288766));
#93926=CARTESIAN_POINT('Ctrl Pts',(8.04036305129555,29.644011782662,127.02493113272));
#93927=CARTESIAN_POINT('Ctrl Pts',(8.04421914470261,29.5739198862576,127.011352786759));
#93928=CARTESIAN_POINT('Ctrl Pts',(8.04807523810967,29.5047016271448,126.994160746867));
#93929=CARTESIAN_POINT('Ctrl Pts',(8.0519314655949,29.4354809612807,126.976968109201));
#93930=CARTESIAN_POINT('Ctrl Pts',(8.05578769308013,29.3671344693989,126.956161625204));
#93931=CARTESIAN_POINT('Ctrl Pts',(8.05964392056537,29.3000603365109,126.931859733515));
#93932=CARTESIAN_POINT('Ctrl Pts',(8.0634999444501,29.2329897449925,126.907559124913));
#93933=CARTESIAN_POINT('Ctrl Pts',(8.06735596833484,29.1671918335515,126.879763648173));
#93934=CARTESIAN_POINT('Ctrl Pts',(8.07121199221957,29.1030466060486,126.848640628023));
#93935=CARTESIAN_POINT('Ctrl Pts',(8.07507195470925,29.0388358595764,126.81748581832));
#93936=CARTESIAN_POINT('Ctrl Pts',(8.07893191719892,28.9762816047668,126.782996893776));
#93937=CARTESIAN_POINT('Ctrl Pts',(8.0827918796886,28.9157401949308,126.745387704097));
#93938=CARTESIAN_POINT('Ctrl Pts',(8.08648092162307,28.857879580934,126.709443863134));
#93939=CARTESIAN_POINT('Ctrl Pts',(8.09016996355755,28.8018576250842,126.670650503597));
#93940=CARTESIAN_POINT('Ctrl Pts',(8.09385900549202,28.7479590808042,126.629230216746));
#93941=CARTESIAN_POINT('Ctrl Pts',(7.39391265022091,28.7479590808041,126.629230216746));
#93942=CARTESIAN_POINT('Ctrl Pts',(7.39776808670206,28.6914048962311,126.585769107009));
#93943=CARTESIAN_POINT('Ctrl Pts',(7.40162352318322,28.6371232308455,126.539365203168));
#93944=CARTESIAN_POINT('Ctrl Pts',(7.40547895966437,28.5854248540264,126.490293500923));
#93945=CARTESIAN_POINT('Ctrl Pts',(7.40933850650131,28.5336713605626,126.441169482382));
#93946=CARTESIAN_POINT('Ctrl Pts',(7.41319805333826,28.4845070053736,126.389372323985));
#93947=CARTESIAN_POINT('Ctrl Pts',(7.4170576001752,28.4382058739118,126.335214091528));
#93948=CARTESIAN_POINT('Ctrl Pts',(7.42091944001119,28.3918772344406,126.281023683073));
#93949=CARTESIAN_POINT('Ctrl Pts',(7.42478127984718,28.3484155004047,126.224469793889));
#93950=CARTESIAN_POINT('Ctrl Pts',(7.42864311968317,28.3080529063201,126.165895619122));
#93951=CARTESIAN_POINT('Ctrl Pts',(7.43251160661999,28.2676208390714,126.107220624937));
#93952=CARTESIAN_POINT('Ctrl Pts',(7.43638009355682,28.2302988135901,126.046518817859));
#93953=CARTESIAN_POINT('Ctrl Pts',(7.44024858049364,28.1962739987851,125.984159578037));
#93954=CARTESIAN_POINT('Ctrl Pts',(7.44218676905692,28.1792268927718,125.952916363981));
#93955=CARTESIAN_POINT('Ctrl Pts',(7.4441249576202,28.1630067093441,125.921257441353));
#93956=CARTESIAN_POINT('Ctrl Pts',(7.44606314618348,28.1476323957825,125.889231028106));
#93957=CARTESIAN_POINT('Ctrl Pts',(7.44993221953134,28.1169417045001,125.825298888441));
#93958=CARTESIAN_POINT('Ctrl Pts',(7.45380129287919,28.0895045899316,125.759650781342));
#93959=CARTESIAN_POINT('Ctrl Pts',(7.45767036622704,28.065515042618,125.692651075335));
#93960=CARTESIAN_POINT('Ctrl Pts',(7.46153367462244,28.0415612399355,125.625751199465));
#93961=CARTESIAN_POINT('Ctrl Pts',(7.46539698301783,28.0210449703193,125.557504175837));
#93962=CARTESIAN_POINT('Ctrl Pts',(7.46926029141322,28.004113263557,125.488296731293));
#93963=CARTESIAN_POINT('Ctrl Pts',(7.47311906790573,27.987201418748,125.419170471418));
#93964=CARTESIAN_POINT('Ctrl Pts',(7.47697784439825,27.9738658992889,125.349086498082));
#93965=CARTESIAN_POINT('Ctrl Pts',(7.48083662089076,27.9642041985661,125.278447512763));
#93966=CARTESIAN_POINT('Ctrl Pts',(7.48469296647855,27.9545485844031,125.207853027727));
#93967=CARTESIAN_POINT('Ctrl Pts',(7.48854931206635,27.9485622629447,125.136704704553));
#93968=CARTESIAN_POINT('Ctrl Pts',(7.49240565765414,27.9462915341202,125.065414827627));
#93969=CARTESIAN_POINT('Ctrl Pts',(7.49626086389906,27.944021476174,124.994146013029));
#93970=CARTESIAN_POINT('Ctrl Pts',(7.50011607014396,27.9454648469652,124.92273621298));
#93971=CARTESIAN_POINT('Ctrl Pts',(7.50397127638888,27.9506159105085,124.85160048437));
#93972=CARTESIAN_POINT('Ctrl Pts',(7.50782663323969,27.9557671752812,124.780461976801));
#93973=CARTESIAN_POINT('Ctrl Pts',(7.5116819900905,27.9646263830915,124.709598046287));
#93974=CARTESIAN_POINT('Ctrl Pts',(7.51553734694131,27.9771358471879,124.639419659759));
#93975=CARTESIAN_POINT('Ctrl Pts',(7.51939673940942,27.989658405639,124.569167813596));
#93976=CARTESIAN_POINT('Ctrl Pts',(7.52325613187754,28.0058387623819,124.499603423131));
#93977=CARTESIAN_POINT('Ctrl Pts',(7.52711552434565,28.0255680547611,124.431127381464));
#93978=CARTESIAN_POINT('Ctrl Pts',(7.53097710194864,28.0453085175939,124.362612569605));
#93979=CARTESIAN_POINT('Ctrl Pts',(7.53483867955163,28.0686017573754,124.295187792598));
#93980=CARTESIAN_POINT('Ctrl Pts',(7.53870025715462,28.0952898299455,124.229236267984));
#93981=CARTESIAN_POINT('Ctrl Pts',(7.54256859126903,28.1220245980078,124.163169349541));
#93982=CARTESIAN_POINT('Ctrl Pts',(7.54643692538344,28.1521658524618,124.098581270323));
#93983=CARTESIAN_POINT('Ctrl Pts',(7.55030525949785,28.1855088726354,124.035832218328));
#93984=CARTESIAN_POINT('Ctrl Pts',(7.55260297867259,28.2053140121426,123.99856043784));
#93985=CARTESIAN_POINT('Ctrl Pts',(7.55490069784731,28.2262479198027,123.961936982506));
#93986=CARTESIAN_POINT('Ctrl Pts',(7.55719841702205,28.2482606181941,123.926032262714));
#93987=CARTESIAN_POINT('Ctrl Pts',(7.56106749037592,28.2853272648625,123.865573179572));
#93988=CARTESIAN_POINT('Ctrl Pts',(7.56493656372979,28.3256001936858,123.806916888848));
#93989=CARTESIAN_POINT('Ctrl Pts',(7.56880563708366,28.368878496293,123.750423990849));
#93990=CARTESIAN_POINT('Ctrl Pts',(7.57266894548512,28.4120923138589,123.694015267752));
#93991=CARTESIAN_POINT('Ctrl Pts',(7.57653225388659,28.4583023234205,123.639763921366));
#93992=CARTESIAN_POINT('Ctrl Pts',(7.58039556228805,28.5072633625889,123.588003224568));
#93993=CARTESIAN_POINT('Ctrl Pts',(7.58425433878664,28.5561669673899,123.536303246312));
#93994=CARTESIAN_POINT('Ctrl Pts',(7.58811311528523,28.6078148594203,123.487088465385));
#93995=CARTESIAN_POINT('Ctrl Pts',(7.59197189178381,28.661921588537,123.440659201048));
#93996=CARTESIAN_POINT('Ctrl Pts',(7.59582823737769,28.7159942321598,123.39425918565));
#93997=CARTESIAN_POINT('Ctrl Pts',(7.59968458297157,28.7725222719124,123.350641520977));
#93998=CARTESIAN_POINT('Ctrl Pts',(7.60354092856544,28.8311844411433,123.31006871386));
#93999=CARTESIAN_POINT('Ctrl Pts',(7.60739613481643,28.8898292788556,123.269507893827));
#94000=CARTESIAN_POINT('Ctrl Pts',(7.61125134106742,28.9506065949708,123.231990421594));
#94001=CARTESIAN_POINT('Ctrl Pts',(7.61510654731841,29.013164571123,123.197736590059));
#94002=CARTESIAN_POINT('Ctrl Pts',(7.61896190417531,29.0757249911396,123.163481420378));
#94003=CARTESIAN_POINT('Ctrl Pts',(7.62281726103221,29.1400657821498,123.132490375898));
#94004=CARTESIAN_POINT('Ctrl Pts',(7.62667261788911,29.2058103857097,123.104937885173));
#94005=CARTESIAN_POINT('Ctrl Pts',(7.63053201036323,29.271623807816,123.077356553717));
#94006=CARTESIAN_POINT('Ctrl Pts',(7.63439140283736,29.3388435268718,123.053221149227));
#94007=CARTESIAN_POINT('Ctrl Pts',(7.63825079531149,29.4070736919278,123.032657641463));
#94008=CARTESIAN_POINT('Ctrl Pts',(7.64211237292047,29.4753424879634,123.012082490923));
#94009=CARTESIAN_POINT('Ctrl Pts',(7.64597395052945,29.5446223968602,122.995083378818));
#94010=CARTESIAN_POINT('Ctrl Pts',(7.64983552813843,29.6145057976293,122.981735452811));
#94011=CARTESIAN_POINT('Ctrl Pts',(7.65370386225874,29.6845114717375,122.968364172253));
#94012=CARTESIAN_POINT('Ctrl Pts',(7.65757219637904,29.7551222644717,122.958656898589));
#94013=CARTESIAN_POINT('Ctrl Pts',(7.66144053049935,29.8259245330664,122.952636990099));
#94014=CARTESIAN_POINT('Ctrl Pts',(7.66373824961977,29.867979774744,122.949061275486));
#94015=CARTESIAN_POINT('Ctrl Pts',(7.66603596874018,29.9101025335228,122.946785516384));
#94016=CARTESIAN_POINT('Ctrl Pts',(7.6683336878606,29.9522065486158,122.94580591265));
#94017=CARTESIAN_POINT('Ctrl Pts',(7.6722027611979,30.0231044754954,122.94415638175));
#94018=CARTESIAN_POINT('Ctrl Pts',(7.6760718345352,30.0942267702318,122.946178357979));
#94019=CARTESIAN_POINT('Ctrl Pts',(7.6799409078725,30.1651615113171,122.951898626122));
#94020=CARTESIAN_POINT('Ctrl Pts',(7.68380421625738,30.2359905590305,122.957610371017));
#94021=CARTESIAN_POINT('Ctrl Pts',(7.68766752464226,30.3066321275373,122.967009430934));
#94022=CARTESIAN_POINT('Ctrl Pts',(7.69153083302714,30.3766732525031,122.980070589513));
#94023=CARTESIAN_POINT('Ctrl Pts',(7.69538960950924,30.4466322148411,122.993116426536));
#94024=CARTESIAN_POINT('Ctrl Pts',(7.69924838599134,30.5159916574953,123.009815740546));
#94025=CARTESIAN_POINT('Ctrl Pts',(7.70310716247344,30.5843444512707,123.030091594828));
#94026=CARTESIAN_POINT('Ctrl Pts',(7.70696350805088,30.6526541849918,123.050354675975));
#94027=CARTESIAN_POINT('Ctrl Pts',(7.71081985362832,30.7199580633634,123.074189689446));
#94028=CARTESIAN_POINT('Ctrl Pts',(7.71467619920577,30.7858612994716,123.101469099411));
#94029=CARTESIAN_POINT('Ctrl Pts',(7.7185314054404,30.8517450647164,123.128740449776));
#94030=CARTESIAN_POINT('Ctrl Pts',(7.72238661167505,30.9162285606263,123.159453990657));
#94031=CARTESIAN_POINT('Ctrl Pts',(7.72624181790968,30.9789358958969,123.193433623078));
#94032=CARTESIAN_POINT('Ctrl Pts',(7.73009717475033,31.0416456808683,123.227414582935));
#94033=CARTESIAN_POINT('Ctrl Pts',(7.73395253159098,31.1025787413811,123.264661654271));
#94034=CARTESIAN_POINT('Ctrl Pts',(7.73780788843163,31.1613843006375,123.304953077719));
#94035=CARTESIAN_POINT('Ctrl Pts',(7.74166728088979,31.2202514149598,123.345286676453));
#94036=CARTESIAN_POINT('Ctrl Pts',(7.74552667334794,31.2769861809183,123.388670713517));
#94037=CARTESIAN_POINT('Ctrl Pts',(7.7493860658061,31.3312680704952,123.434840938761));
#94038=CARTESIAN_POINT('Ctrl Pts',(7.75324764339922,31.385580693732,123.481037304951));
#94039=CARTESIAN_POINT('Ctrl Pts',(7.75710922099235,31.4374373226377,123.530022665896));
#94040=CARTESIAN_POINT('Ctrl Pts',(7.76097079858548,31.4865537434053,123.581495318842));
#94041=CARTESIAN_POINT('Ctrl Pts',(7.76483913269032,31.5357561020219,123.63305803228));
#94042=CARTESIAN_POINT('Ctrl Pts',(7.76870746679515,31.5822083634828,123.687116357967));
#94043=CARTESIAN_POINT('Ctrl Pts',(7.77257580089999,31.6256665585024,123.743335445289));
#94044=CARTESIAN_POINT('Ctrl Pts',(7.77487352016638,31.65147992655,123.776728548516));
#94045=CARTESIAN_POINT('Ctrl Pts',(7.77717123943277,31.676237764067,123.81088342508));
#94046=CARTESIAN_POINT('Ctrl Pts',(7.77946895869917,31.6998964789576,123.845725542461));
#94047=CARTESIAN_POINT('Ctrl Pts',(7.78339694507706,31.740341415451,123.905288677283));
#94048=CARTESIAN_POINT('Ctrl Pts',(7.78732493145496,31.7777270929251,123.967090244454));
#94049=CARTESIAN_POINT('Ctrl Pts',(7.79125291783286,31.8118021955754,124.030788791538));
#94050=CARTESIAN_POINT('Ctrl Pts',(7.79517455591723,31.8458222270689,124.094384390945));
#94051=CARTESIAN_POINT('Ctrl Pts',(7.7990961940016,31.8765420914259,124.159870473948));
#94052=CARTESIAN_POINT('Ctrl Pts',(7.80301783208597,31.9037535790036,124.226876547419));
#94053=CARTESIAN_POINT('Ctrl Pts',(7.80693336836421,31.9309227273297,124.293778363929));
#94054=CARTESIAN_POINT('Ctrl Pts',(7.81084890464245,31.9545941797125,124.362195038262));
#94055=CARTESIAN_POINT('Ctrl Pts',(7.81476444092069,31.9746063344711,124.431732997292));
#94056=CARTESIAN_POINT('Ctrl Pts',(7.81867638559684,31.99460013269,124.501207171272));
#94057=CARTESIAN_POINT('Ctrl Pts',(7.822588330273,32.010941171143,124.571800140764));
#94058=CARTESIAN_POINT('Ctrl Pts',(7.82650027494915,32.0235168923249,124.643100926065));
#94059=CARTESIAN_POINT('Ctrl Pts',(7.83040988896528,32.0360851211384,124.714359231754));
#94060=CARTESIAN_POINT('Ctrl Pts',(7.8343195029814,32.0448924075045,124.786324057116));
#94061=CARTESIAN_POINT('Ctrl Pts',(7.83822911699753,32.0498770839559,124.858573329346));
#94062=CARTESIAN_POINT('Ctrl Pts',(7.84079450484425,32.0531479000354,124.905981437704));
#94063=CARTESIAN_POINT('Ctrl Pts',(7.84335989269096,32.0547738811643,124.953511789743));
#94064=CARTESIAN_POINT('Ctrl Pts',(7.84592528053768,32.054749734871,125.001043813945));
#94065=CARTESIAN_POINT('Origin',(-1.54592528053767,30.,125.));
#94066=CARTESIAN_POINT('',(6.69398884866211,28.7479590808042,126.629230216746));
#94067=CARTESIAN_POINT('',(6.75200666580924,28.7479590808042,126.629230216746));
#94068=CARTESIAN_POINT('',(-1.54592528053767,28.7479590808042,126.629230216746));
#94069=CARTESIAN_POINT('',(7.20407471942241,32.054749359036,125.001622972929));
#94070=CARTESIAN_POINT('Ctrl Pts',(6.75200666580924,28.7479590808042,126.629230216746));
#94071=CARTESIAN_POINT('Ctrl Pts',(6.75586954865699,28.6914516806324,126.585805060175));
#94072=CARTESIAN_POINT('Ctrl Pts',(6.75973243150475,28.637266657374,126.539483217538));
#94073=CARTESIAN_POINT('Ctrl Pts',(6.7635953143525,28.5856997459588,126.490554378048));
#94074=CARTESIAN_POINT('Ctrl Pts',(6.76746446443362,28.5340491711553,126.441546155241));
#94075=CARTESIAN_POINT('Ctrl Pts',(6.77133361451474,28.4850255120238,126.389922852198));
#94076=CARTESIAN_POINT('Ctrl Pts',(6.77520276459586,28.438885369153,126.336008484949));
#94077=CARTESIAN_POINT('Ctrl Pts',(6.77582755829117,28.4314346190498,126.327302346382));
#94078=CARTESIAN_POINT('Ctrl Pts',(6.77645235198647,28.4240589685884,126.318536528105));
#94079=CARTESIAN_POINT('Ctrl Pts',(6.77707714568178,28.4167593915136,126.309712463917));
#94080=CARTESIAN_POINT('Ctrl Pts',(6.78094621902987,28.3715563119621,126.255068904245));
#94081=CARTESIAN_POINT('Ctrl Pts',(6.78481529237797,28.32909694316,126.197975373757));
#94082=CARTESIAN_POINT('Ctrl Pts',(6.78868436572606,28.2896574231008,126.138738702313));
#94083=CARTESIAN_POINT('Ctrl Pts',(6.79254767412172,28.2502766682644,126.079590294017));
#94084=CARTESIAN_POINT('Ctrl Pts',(6.79641098251739,28.2139070976185,126.018305484439));
#94085=CARTESIAN_POINT('Ctrl Pts',(6.80027429091305,28.1807846665672,125.955224127157));
#94086=CARTESIAN_POINT('Ctrl Pts',(6.80413306740584,28.1477010902034,125.892216768261));
#94087=CARTESIAN_POINT('Ctrl Pts',(6.80799184389864,28.1178573120154,125.827417475809));
#94088=CARTESIAN_POINT('Ctrl Pts',(6.81185062039143,28.0914450656681,125.761193553006));
#94089=CARTESIAN_POINT('Ctrl Pts',(6.81570696597952,28.0650494581839,125.695011349137));
#94090=CARTESIAN_POINT('Ctrl Pts',(6.81956331156761,28.0420812731913,125.62740674564));
#94091=CARTESIAN_POINT('Ctrl Pts',(6.82341965715569,28.0226848730009,125.558768691894));
#94092=CARTESIAN_POINT('Ctrl Pts',(6.82727486340091,28.0032942034043,125.490150917004));
#94093=CARTESIAN_POINT('Ctrl Pts',(6.83113006964612,27.9874733556387,125.420500765251));
#94094=CARTESIAN_POINT('Ctrl Pts',(6.83498527589134,27.9753168606325,125.350222425982));
#94095=CARTESIAN_POINT('Ctrl Pts',(6.83884063274247,27.9631598907256,125.279941341248));
#94096=CARTESIAN_POINT('Ctrl Pts',(6.8426959895936,27.9546676384135,125.209032499328));
#94097=CARTESIAN_POINT('Ctrl Pts',(6.84655134644473,27.9498832308849,125.137908649088));
#94098=CARTESIAN_POINT('Ctrl Pts',(6.85041073891317,27.9450938152499,125.066710349542));
#94099=CARTESIAN_POINT('Ctrl Pts',(6.85427013138162,27.9440200248333,124.995297078087));
#94100=CARTESIAN_POINT('Ctrl Pts',(6.85812952385006,27.9466528919678,124.924084148982));
#94101=CARTESIAN_POINT('Ctrl Pts',(6.86199110145338,27.9492872497954,124.852830900098));
#94102=CARTESIAN_POINT('Ctrl Pts',(6.86585267905671,27.9556323997252,124.78177870346));
#94103=CARTESIAN_POINT('Ctrl Pts',(6.86971425666003,27.9656274785372,124.711337556276));
#94104=CARTESIAN_POINT('Ctrl Pts',(6.87358259077479,27.9756400455033,124.640773159874));
#94105=CARTESIAN_POINT('Ctrl Pts',(6.87745092488956,27.9893151983398,124.570822424404));
#94106=CARTESIAN_POINT('Ctrl Pts',(6.88131925900432,28.0065411240329,124.501884278176));
#94107=CARTESIAN_POINT('Ctrl Pts',(6.88361697817632,28.0167730064263,124.460936289825));
#94108=CARTESIAN_POINT('Ctrl Pts',(6.88591469734833,28.0282566940969,124.420345270082));
#94109=CARTESIAN_POINT('Ctrl Pts',(6.88821241652033,28.0409606653547,124.380191603951));
#94110=CARTESIAN_POINT('Ctrl Pts',(6.89208148986845,28.0623525731246,124.312577823577));
#94111=CARTESIAN_POINT('Ctrl Pts',(6.89595056321656,28.0872908982659,124.245940377934));
#94112=CARTESIAN_POINT('Ctrl Pts',(6.89981963656468,28.1156676269778,124.180677676076));
#94113=CARTESIAN_POINT('Ctrl Pts',(6.90368294496036,28.1440020741209,124.115512216202));
#94114=CARTESIAN_POINT('Ctrl Pts',(6.90754625335605,28.1757645631989,124.051717876002));
#94115=CARTESIAN_POINT('Ctrl Pts',(6.91140956175174,28.2107975421538,123.989677216263));
#94116=CARTESIAN_POINT('Ctrl Pts',(6.91526833824455,28.2457894252287,123.927709334107));
#94117=CARTESIAN_POINT('Ctrl Pts',(6.91912711473736,28.2840439399123,123.867491467115));
#94118=CARTESIAN_POINT('Ctrl Pts',(6.92298589123017,28.3253564882379,123.809383911156));
#94119=CARTESIAN_POINT('Ctrl Pts',(6.92684223681827,28.3666430109907,123.751312961084));
#94120=CARTESIAN_POINT('Ctrl Pts',(6.93069858240637,28.4109834644939,123.695350079465));
#94121=CARTESIAN_POINT('Ctrl Pts',(6.93455492799447,28.4581293723644,123.641827503542));
#94122=CARTESIAN_POINT('Ctrl Pts',(6.9384101342397,28.5052613511528,123.588320740664));
#94123=CARTESIAN_POINT('Ctrl Pts',(6.94226534048493,28.5551968178644,123.537253216468));
#94124=CARTESIAN_POINT('Ctrl Pts',(6.94612054673015,28.6076474656051,123.488923568292));
#94125=CARTESIAN_POINT('Ctrl Pts',(6.94997590358129,28.6601001623613,123.440592032089));
#94126=CARTESIAN_POINT('Ctrl Pts',(6.95383126043243,28.7150678764803,123.394998911815));
#94127=CARTESIAN_POINT('Ctrl Pts',(6.95768661728358,28.7722272302995,123.352404300661));
#94128=CARTESIAN_POINT('Ctrl Pts',(6.96154600975203,28.8294464160063,123.309765103348));
#94129=CARTESIAN_POINT('Ctrl Pts',(6.96540540222048,28.8888614306513,123.270130971586));
#94130=CARTESIAN_POINT('Ctrl Pts',(6.96926479468893,28.9501184868936,123.233719622784));
#94131=CARTESIAN_POINT('Ctrl Pts',(6.97312637229226,29.0114102260377,123.197287658378));
#94132=CARTESIAN_POINT('Ctrl Pts',(6.97698794989559,29.0745456527964,123.164082335572));
#94133=CARTESIAN_POINT('Ctrl Pts',(6.98084952749892,29.1391473006333,123.134274888283));
#94134=CARTESIAN_POINT('Ctrl Pts',(6.98471786161368,29.2038619804528,123.104415287604));
#94135=CARTESIAN_POINT('Ctrl Pts',(6.98858619572845,29.270047552029,123.077965612503));
#94136=CARTESIAN_POINT('Ctrl Pts',(6.99245452984321,29.3373082149498,123.055048288382));
#94137=CARTESIAN_POINT('Ctrl Pts',(6.99475224901511,29.3772598091303,123.041435820214));
#94138=CARTESIAN_POINT('Ctrl Pts',(6.997049968187,29.4175904326575,123.029068655139));
#94139=CARTESIAN_POINT('Ctrl Pts',(6.99934768735889,29.4582154543571,123.01796390835));
#94140=CARTESIAN_POINT('Ctrl Pts',(7.00321676070783,29.5266229389101,122.999264895707));
#94141=CARTESIAN_POINT('Ctrl Pts',(7.00708583405677,29.596133611542,122.984074911669));
#94142=CARTESIAN_POINT('Ctrl Pts',(7.01095490740571,29.6663541686468,122.972519291899));
#94143=CARTESIAN_POINT('Ctrl Pts',(7.01481821580223,29.7364700965202,122.960980890102));
#94144=CARTESIAN_POINT('Ctrl Pts',(7.01868152419874,29.8072933338607,122.953066181724));
#94145=CARTESIAN_POINT('Ctrl Pts',(7.02254483259525,29.8784170241083,122.94885028765));
#94146=CARTESIAN_POINT('Ctrl Pts',(7.02640360908889,29.9494572818097,122.944639339084));
#94147=CARTESIAN_POINT('Ctrl Pts',(7.03026238558253,30.020796809752,122.944118614824));
#94148=CARTESIAN_POINT('Ctrl Pts',(7.03412116207617,30.0920219410923,122.947311634744));
#94149=CARTESIAN_POINT('Ctrl Pts',(7.03797750766511,30.1632022028975,122.950502643165));
#94150=CARTESIAN_POINT('Ctrl Pts',(7.04183385325404,30.2342677269276,122.957402732454));
#94151=CARTESIAN_POINT('Ctrl Pts',(7.04569019884297,30.3048046215392,122.967983340327));
#94152=CARTESIAN_POINT('Ctrl Pts',(7.04954540508902,30.3753206762891,122.978560822199));
#94153=CARTESIAN_POINT('Ctrl Pts',(7.05340061133508,30.4453079315347,122.992816591849));
#94154=CARTESIAN_POINT('Ctrl Pts',(7.05725581758114,30.5143591217371,123.010670400264));
#94155=CARTESIAN_POINT('Ctrl Pts',(7.06111117443311,30.583413009465,123.028524906148));
#94156=CARTESIAN_POINT('Ctrl Pts',(7.06496653128508,30.6515302897811,123.049977606121));
#94157=CARTESIAN_POINT('Ctrl Pts',(7.06882188813704,30.718317058636,123.074897881729));
#94158=CARTESIAN_POINT('Ctrl Pts',(7.07268128060632,30.7851737369313,123.09984424278));
#94159=CARTESIAN_POINT('Ctrl Pts',(7.07654067307558,30.850696667515,123.128265255));
#94160=CARTESIAN_POINT('Ctrl Pts',(7.08040006554485,30.9145110549591,123.159981768336));
#94161=CARTESIAN_POINT('Ctrl Pts',(7.08426164314899,30.9783615732306,123.191716239125));
#94162=CARTESIAN_POINT('Ctrl Pts',(7.08812322075314,31.0405011992929,123.226749686708));
#94163=CARTESIAN_POINT('Ctrl Pts',(7.09198479835728,31.10058134778,123.264857856134));
#94164=CARTESIAN_POINT('Ctrl Pts',(7.09585313247284,31.1607666170885,123.303032702527));
#94165=CARTESIAN_POINT('Ctrl Pts',(7.09972146658841,31.2188848182504,123.344292730323));
#94166=CARTESIAN_POINT('Ctrl Pts',(7.10358980070397,31.2746184284222,123.388371809496));
#94167=CARTESIAN_POINT('Ctrl Pts',(7.10588751986847,31.3077231655965,123.414553970071));
#94168=CARTESIAN_POINT('Ctrl Pts',(7.10818523903296,31.339987241309,123.441729977376));
#94169=CARTESIAN_POINT('Ctrl Pts',(7.11048295819745,31.3713503754315,123.469838011744));
#94170=CARTESIAN_POINT('Ctrl Pts',(7.11438261491516,31.4245794464856,123.517542573179));
#94171=CARTESIAN_POINT('Ctrl Pts',(7.11828227163287,31.4754382086281,123.568137518425));
#94172=CARTESIAN_POINT('Ctrl Pts',(7.12218192835057,31.5235907696476,123.621352572575));
#94173=CARTESIAN_POINT('Ctrl Pts',(7.12598698948198,31.5705752740736,123.673276767142));
#94174=CARTESIAN_POINT('Ctrl Pts',(7.1297920506134,31.6149830001644,123.727695018052));
#94175=CARTESIAN_POINT('Ctrl Pts',(7.13359711174481,31.6565353095317,123.784315694444));
#94176=CARTESIAN_POINT('Ctrl Pts',(7.13739855500656,31.6980481107719,123.840882535636));
#94177=CARTESIAN_POINT('Ctrl Pts',(7.14119999826832,31.7367105810086,123.89964724987));
#94178=CARTESIAN_POINT('Ctrl Pts',(7.14500144153007,31.7722833964744,123.960284113288));
#94179=CARTESIAN_POINT('Ctrl Pts',(7.14880063066542,31.807835118472,124.020885021111));
#94180=CARTESIAN_POINT('Ctrl Pts',(7.15259981980078,31.8403005657239,124.083355444928));
#94181=CARTESIAN_POINT('Ctrl Pts',(7.15639900893613,31.8694840247516,124.147341191508));
#94182=CARTESIAN_POINT('Ctrl Pts',(7.16037198480999,31.9000024260477,124.214253845334));
#94183=CARTESIAN_POINT('Ctrl Pts',(7.16434496068385,31.9269310579514,124.282823287038));
#94184=CARTESIAN_POINT('Ctrl Pts',(7.1683179365577,31.9501011080216,124.352618172179));
#94185=CARTESIAN_POINT('Ctrl Pts',(7.17211850690861,31.9722657040629,124.419384339287));
#94186=CARTESIAN_POINT('Ctrl Pts',(7.17591907725952,31.9909910752724,124.487271268715));
#94187=CARTESIAN_POINT('Ctrl Pts',(7.17971964761043,32.0061804532505,124.555885654932));
#94188=CARTESIAN_POINT('Ctrl Pts',(7.1835216969548,32.0213757421811,124.624526742464));
#94189=CARTESIAN_POINT('Ctrl Pts',(7.18732374629917,32.0330322152424,124.693895355795));
#94190=CARTESIAN_POINT('Ctrl Pts',(7.19112579564354,32.0411045496223,124.763589805611));
#94191=CARTESIAN_POINT('Ctrl Pts',(7.19493249874043,32.0491867646331,124.833369562242));
#94192=CARTESIAN_POINT('Ctrl Pts',(7.19873920183731,32.0536760627127,124.9034754511));
#94193=CARTESIAN_POINT('Ctrl Pts',(7.2025459049342,32.0545791584134,124.973503881167));
#94194=CARTESIAN_POINT('Ctrl Pts',(7.2030555097636,32.0547000561874,124.982878614434));
#94195=CARTESIAN_POINT('Ctrl Pts',(7.20356511459301,32.0547567608592,124.992251965448));
#94196=CARTESIAN_POINT('Ctrl Pts',(7.20407471942241,32.054749359036,125.001622972929));
#94197=CARTESIAN_POINT('Ctrl Pts',(7.20407471946233,32.0547493590354,125.001622973663));
#94198=CARTESIAN_POINT('Ctrl Pts',(7.20992255598689,32.0546644213169,125.109157511514));
#94199=CARTESIAN_POINT('Ctrl Pts',(7.21577039251145,32.0461359067699,125.216366166843));
#94200=CARTESIAN_POINT('Ctrl Pts',(7.22161822903602,32.0293269300174,125.322226277026));
#94201=CARTESIAN_POINT('Ctrl Pts',(7.22548730238386,32.0182056950642,125.392265945404));
#94202=CARTESIAN_POINT('Ctrl Pts',(7.22935637573169,32.0034324231356,125.461866373981));
#94203=CARTESIAN_POINT('Ctrl Pts',(7.23322544907953,31.9850548085808,125.530617535924));
#94204=CARTESIAN_POINT('Ctrl Pts',(7.23708875747492,31.9667045768292,125.599266258047));
#94205=CARTESIAN_POINT('Ctrl Pts',(7.24095206587031,31.944760787173,125.667067759863));
#94206=CARTESIAN_POINT('Ctrl Pts',(7.2448153742657,31.9193224755762,125.733620335901));
#94207=CARTESIAN_POINT('Ctrl Pts',(7.2486741507582,31.8939140047133,125.800094841597));
#94208=CARTESIAN_POINT('Ctrl Pts',(7.25253292725071,31.8650193270942,125.86532288007));
#94209=CARTESIAN_POINT('Ctrl Pts',(7.25639170374321,31.8327873077696,125.92891778268));
#94210=CARTESIAN_POINT('Ctrl Pts',(7.26024804933099,31.8005755935773,125.992472622552));
#94211=CARTESIAN_POINT('Ctrl Pts',(7.26410439491877,31.7650309279384,126.054395935445));
#94212=CARTESIAN_POINT('Ctrl Pts',(7.26796074050655,31.7263497323502,126.114322289158));
#94213=CARTESIAN_POINT('Ctrl Pts',(7.27181594675145,31.6876799649766,126.174230937854));
#94214=CARTESIAN_POINT('Ctrl Pts',(7.27567115299635,31.6458757706677,126.23214339075));
#94215=CARTESIAN_POINT('Ctrl Pts',(7.27952635924124,31.6011779466017,126.287721532714));
#94216=CARTESIAN_POINT('Ctrl Pts',(7.28338171609205,31.5564783763889,126.343301845871));
#94217=CARTESIAN_POINT('Ctrl Pts',(7.28723707294285,31.508885258151,126.396547289877));
#94218=CARTESIAN_POINT('Ctrl Pts',(7.29109242979365,31.4586797914259,126.447152662502));
#94219=CARTESIAN_POINT('Ctrl Pts',(7.29495182226175,31.4084217718353,126.497811006596));
#94220=CARTESIAN_POINT('Ctrl Pts',(7.29881121472986,31.3555462879374,126.545823417153));
#94221=CARTESIAN_POINT('Ctrl Pts',(7.30267060719796,31.3003709007601,126.590922085759));
#94222=CARTESIAN_POINT('Ctrl Pts',(7.30653218480093,31.2451642740384,126.63604628861));
#94223=CARTESIAN_POINT('Ctrl Pts',(7.31039376240389,31.1876555436276,126.678253177863));
#94224=CARTESIAN_POINT('Ctrl Pts',(7.31425534000686,31.1281925856658,126.717317399944));
#94225=CARTESIAN_POINT('Ctrl Pts',(7.31812367412126,31.0686255867662,126.756449971774));
#94226=CARTESIAN_POINT('Ctrl Pts',(7.32199200823566,31.0070979531369,126.79242865292));
#94227=CARTESIAN_POINT('Ctrl Pts',(7.32586034235006,30.9439829349224,126.825073637165));
#94228=CARTESIAN_POINT('Ctrl Pts',(7.32815806152489,30.9064937772428,126.844464156196));
#94229=CARTESIAN_POINT('Ctrl Pts',(7.33045578069973,30.8684449853415,126.862679408199));
#94230=CARTESIAN_POINT('Ctrl Pts',(7.33275349987457,30.8299177134446,126.879689908312));
#94231=CARTESIAN_POINT('Ctrl Pts',(7.33662257322846,30.7650425786904,126.908333475135));
#94232=CARTESIAN_POINT('Ctrl Pts',(7.34049164658236,30.6985557347294,126.933670578712));
#94233=CARTESIAN_POINT('Ctrl Pts',(7.34436071993625,30.6308275306673,126.955518905317));
#94234=CARTESIAN_POINT('Ctrl Pts',(7.34822402833774,30.563200242209,126.977334677728));
#94235=CARTESIAN_POINT('Ctrl Pts',(7.35208733673922,30.4943357236864,126.995671843735));
#94236=CARTESIAN_POINT('Ctrl Pts',(7.35595064514071,30.424625178915,127.010395737145));
#94237=CARTESIAN_POINT('Ctrl Pts',(7.35980942163932,30.3549964089815,127.025102358506));
#94238=CARTESIAN_POINT('Ctrl Pts',(7.36366819813793,30.2845240571169,127.03620402665));
#94239=CARTESIAN_POINT('Ctrl Pts',(7.36752697463654,30.2136137195477,127.043616094407));
#94240=CARTESIAN_POINT('Ctrl Pts',(7.37138332023044,30.1427480532036,127.051023492802));
#94241=CARTESIAN_POINT('Ctrl Pts',(7.37523966582434,30.0714454305808,127.054745851857));
#94242=CARTESIAN_POINT('Ctrl Pts',(7.37909601141824,30.000119399154,127.054749996531));
#94243=CARTESIAN_POINT('Ctrl Pts',(7.38295121766926,29.9288144407364,127.05475413998));
#94244=CARTESIAN_POINT('Ctrl Pts',(7.38680642392028,29.8574865727665,127.051042249909));
#94245=CARTESIAN_POINT('Ctrl Pts',(7.39066163017129,29.7865504602363,127.043633249014));
#94246=CARTESIAN_POINT('Ctrl Pts',(7.3945169870282,29.7156115765452,127.036223958681));
#94247=CARTESIAN_POINT('Ctrl Pts',(7.39837234388512,29.6450649616074,127.025117323432));
#94248=CARTESIAN_POINT('Ctrl Pts',(7.40222770074203,29.5753195416403,127.010384060519));
#94249=CARTESIAN_POINT('Ctrl Pts',(7.40608709321618,29.5055011152488,126.995635375477));
#94250=CARTESIAN_POINT('Ctrl Pts',(7.40994648569033,29.4364860342437,126.977252585325));
#94251=CARTESIAN_POINT('Ctrl Pts',(7.41380587816449,29.3686715298374,126.955357237249));
#94252=CARTESIAN_POINT('Ctrl Pts',(7.41766745577349,29.3008186297929,126.933449492329));
#94253=CARTESIAN_POINT('Ctrl Pts',(7.42152903338249,29.2341681136199,126.908025403692));
#94254=CARTESIAN_POINT('Ctrl Pts',(7.4253906109915,29.1690979861963,126.879255013551));
#94255=CARTESIAN_POINT('Ctrl Pts',(7.42925894511183,29.1039140071045,126.850434284536));
#94256=CARTESIAN_POINT('Ctrl Pts',(7.43312727923216,29.0403163711,126.818255783837));
#94257=CARTESIAN_POINT('Ctrl Pts',(7.43699561335248,28.9786585786913,126.782935574725));
#94258=CARTESIAN_POINT('Ctrl Pts',(7.4392933324727,28.9420349872122,126.761956021955));
#94259=CARTESIAN_POINT('Ctrl Pts',(7.44159105159292,28.9060952632211,126.739868873525));
#94260=CARTESIAN_POINT('Ctrl Pts',(7.44388877071313,28.8709081933679,126.716726319102));
#94261=CARTESIAN_POINT('Ctrl Pts',(7.44663011041789,28.8289275566425,126.689115632158));
#94262=CARTESIAN_POINT('Ctrl Pts',(7.44937145012266,28.7879021272144,126.659925896233));
#94263=CARTESIAN_POINT('Ctrl Pts',(7.45211278982742,28.7479590808042,126.629230216746));
#94264=CARTESIAN_POINT('',(7.14592528050144,32.0547492461588,124.998239912027));
#94265=CARTESIAN_POINT('Ctrl Pts',(7.14592528053768,32.0547492461594,124.998239912697));
#94266=CARTESIAN_POINT('Ctrl Pts',(7.14975890798153,32.0548099310451,125.069084252562));
#94267=CARTESIAN_POINT('Ctrl Pts',(7.15359253542538,32.0512024328575,125.139993721177));
#94268=CARTESIAN_POINT('Ctrl Pts',(7.15742616286923,32.0439332342781,125.210557584317));
#94269=CARTESIAN_POINT('Ctrl Pts',(7.1612583463496,32.036666773695,125.281094869068));
#94270=CARTESIAN_POINT('Ctrl Pts',(7.16509052982997,32.0257413995742,125.351286317587));
#94271=CARTESIAN_POINT('Ctrl Pts',(7.16892271331034,32.0112155594126,125.420725012421));
#94272=CARTESIAN_POINT('Ctrl Pts',(7.17275477350104,31.9966901865788,125.490161473262));
#94273=CARTESIAN_POINT('Ctrl Pts',(7.17658683369175,31.9785646802636,125.558844747243));
#94274=CARTESIAN_POINT('Ctrl Pts',(7.18041889388246,31.9569484900836,125.626378615264));
#94275=CARTESIAN_POINT('Ctrl Pts',(7.18425485641164,31.935310287282,125.693981255694));
#94276=CARTESIAN_POINT('Ctrl Pts',(7.18809081894083,31.910174452894,125.760431683198));
#94277=CARTESIAN_POINT('Ctrl Pts',(7.19192678147001,31.8816998964671,125.825350266333));
#94278=CARTESIAN_POINT('Ctrl Pts',(7.19576473620573,31.8532105517838,125.890302564924));
#94279=CARTESIAN_POINT('Ctrl Pts',(7.19960269094144,31.8213792546822,125.953720995477));
#94280=CARTESIAN_POINT('Ctrl Pts',(7.20344064567716,31.7864112720226,126.015249885344));
#94281=CARTESIAN_POINT('Ctrl Pts',(7.20728565488989,31.7513790153299,126.07689187038));
#94282=CARTESIAN_POINT('Ctrl Pts',(7.21113066410261,31.7131988248325,126.136636963837));
#94283=CARTESIAN_POINT('Ctrl Pts',(7.21497567331534,31.672119382862,126.194158419958));
#94284=CARTESIAN_POINT('Ctrl Pts',(7.21791465037902,31.640719838398,126.238125607254));
#94285=CARTESIAN_POINT('Ctrl Pts',(7.22085362744269,31.6076273167987,126.280794230264));
#94286=CARTESIAN_POINT('Ctrl Pts',(7.22379260450636,31.572967724563,126.322032563889));
#94287=CARTESIAN_POINT('Ctrl Pts',(7.2276616778553,31.5273394322359,126.376321567895));
#94288=CARTESIAN_POINT('Ctrl Pts',(7.23153075120424,31.4788078915284,126.428351931928));
#94289=CARTESIAN_POINT('Ctrl Pts',(7.23539982455317,31.4276252989682,126.477796862984));
#94290=CARTESIAN_POINT('Ctrl Pts',(7.23926313294969,31.3765189689092,126.52716812067));
#94291=CARTESIAN_POINT('Ctrl Pts',(7.2431264413462,31.3227697743507,126.573961257351));
#94292=CARTESIAN_POINT('Ctrl Pts',(7.24698974974272,31.2666696204782,126.617883072122));
#94293=CARTESIAN_POINT('Ctrl Pts',(7.25084852623635,31.2106352756022,126.661753363851));
#94294=CARTESIAN_POINT('Ctrl Pts',(7.25470730272998,31.1522558300256,126.702758726121));
#94295=CARTESIAN_POINT('Ctrl Pts',(7.25856607922361,31.0918581403232,126.74064452543));
#94296=CARTESIAN_POINT('Ctrl Pts',(7.26242242481254,31.0314984992169,126.778506457907));
#94297=CARTESIAN_POINT('Ctrl Pts',(7.26627877040147,30.9691235470309,126.813252468868));
#94298=CARTESIAN_POINT('Ctrl Pts',(7.2701351159904,30.9050899489487,126.844670633694));
#94299=CARTESIAN_POINT('Ctrl Pts',(7.27399032223645,30.8410752693535,126.876079516141));
#94300=CARTESIAN_POINT('Ctrl Pts',(7.2778455284825,30.77540335261,126.904162290511));
#94301=CARTESIAN_POINT('Ctrl Pts',(7.28170073472854,30.7084548128327,126.92875331255));
#94302=CARTESIAN_POINT('Ctrl Pts',(7.2855560915805,30.6415036576711,126.953345295253));
#94303=CARTESIAN_POINT('Ctrl Pts',(7.28941144843246,30.5732762372185,126.974445089379));
#94304=CARTESIAN_POINT('Ctrl Pts',(7.29326680528442,30.5041708255149,126.991936078593));
#94305=CARTESIAN_POINT('Ctrl Pts',(7.29712619775369,30.434993077318,127.009445376602));
#94306=CARTESIAN_POINT('Ctrl Pts',(7.30098559022295,30.3649359751554,127.023338209445));
#94307=CARTESIAN_POINT('Ctrl Pts',(7.30484498269221,30.2944096807248,127.033548746009));
#94308=CARTESIAN_POINT('Ctrl Pts',(7.30870656029635,30.2238434552775,127.043765063638));
#94309=CARTESIAN_POINT('Ctrl Pts',(7.31256813790048,30.1528079927104,127.050294890176));
#94310=CARTESIAN_POINT('Ctrl Pts',(7.31642971550461,30.0817175524931,127.053124400545));
#94311=CARTESIAN_POINT('Ctrl Pts',(7.32029804962017,30.0105027270062,127.055958861642));
#94312=CARTESIAN_POINT('Ctrl Pts',(7.32416638373573,29.93923321772,127.055080086321));
#94313=CARTESIAN_POINT('Ctrl Pts',(7.32803471785129,29.8683215537164,127.050526359081));
#94314=CARTESIAN_POINT('Ctrl Pts',(7.33033243701584,29.826201332323,127.047821529033));
#94315=CARTESIAN_POINT('Ctrl Pts',(7.33263015618038,29.7842072534164,127.043821117613));
#94316=CARTESIAN_POINT('Ctrl Pts',(7.33492787534493,29.742424058736,127.038541683896));
#94317=CARTESIAN_POINT('Ctrl Pts',(7.33879679457315,29.6720691573147,127.029652128142));
#94318=CARTESIAN_POINT('Ctrl Pts',(7.34266571380137,29.6020371943226,127.017098714014));
#94319=CARTESIAN_POINT('Ctrl Pts',(7.3465346330296,29.5327394560202,127.000916076836));
#94320=CARTESIAN_POINT('Ctrl Pts',(7.35048280112887,29.4620222599304,126.984401963177));
#94321=CARTESIAN_POINT('Ctrl Pts',(7.35443096922814,29.3920702167941,126.964108264813));
#94322=CARTESIAN_POINT('Ctrl Pts',(7.35837913732742,29.323315123349,126.94012760926));
#94323=CARTESIAN_POINT('Ctrl Pts',(7.36223776870244,29.2561192608404,126.916690788034));
#94324=CARTESIAN_POINT('Ctrl Pts',(7.36609640007746,29.1900671186566,126.889732637857));
#94325=CARTESIAN_POINT('Ctrl Pts',(7.36995503145248,29.1255495136279,126.85939073607));
#94326=CARTESIAN_POINT('Ctrl Pts',(7.37394796791389,29.058786282709,126.827992741761));
#94327=CARTESIAN_POINT('Ctrl Pts',(7.37794090437529,28.993666907158,126.792971229341));
#94328=CARTESIAN_POINT('Ctrl Pts',(7.3819338408367,28.9306027627195,126.754533303017));
#94329=CARTESIAN_POINT('Ctrl Pts',(7.3859267772981,28.8675386182809,126.716095376693));
#94330=CARTESIAN_POINT('Ctrl Pts',(7.3899197137595,28.806530209321,126.674241320047));
#94331=CARTESIAN_POINT('Ctrl Pts',(7.39391265022091,28.7479590808041,126.629230216746));
#94332=CARTESIAN_POINT('Ctrl Pts',(6.69398884866211,28.7479590808042,126.629230216746));
#94333=CARTESIAN_POINT('Ctrl Pts',(6.6978469486556,28.6915134540401,126.585852532186));
#94334=CARTESIAN_POINT('Ctrl Pts',(6.70170504864909,28.6372663028371,126.539493111356));
#94335=CARTESIAN_POINT('Ctrl Pts',(6.70556314864259,28.5855443913852,126.490406955753));
#94336=CARTESIAN_POINT('Ctrl Pts',(6.70941911634607,28.5338510655364,126.441347929027));
#94337=CARTESIAN_POINT('Ctrl Pts',(6.71327508404956,28.4846805619422,126.389565491501));
#94338=CARTESIAN_POINT('Ctrl Pts',(6.71713105175305,28.4383254317381,126.335353925124));
#94339=CARTESIAN_POINT('Ctrl Pts',(6.7209861782402,28.3919804143504,126.281154185521));
#94340=CARTESIAN_POINT('Ctrl Pts',(6.72484130472734,28.3484498661655,126.224526738619));
#94341=CARTESIAN_POINT('Ctrl Pts',(6.72869643121448,28.3079872435019,126.165800323532));
#94342=CARTESIAN_POINT('Ctrl Pts',(6.73255200624573,28.2675199130106,126.107067075625));
#94343=CARTESIAN_POINT('Ctrl Pts',(6.73640758127698,28.2301214901697,126.046234776163));
#94344=CARTESIAN_POINT('Ctrl Pts',(6.74026315630823,28.196002150772,125.983661182766));
#94345=CARTESIAN_POINT('Ctrl Pts',(6.74412295033885,28.161845475965,125.921019117624));
#94346=CARTESIAN_POINT('Ctrl Pts',(6.74798274436946,28.1309752768927,125.856632383921));
#94347=CARTESIAN_POINT('Ctrl Pts',(6.75184253840008,28.1035553368084,125.790882546243));
#94348=CARTESIAN_POINT('Ctrl Pts',(6.75570478529074,28.0761179716298,125.725090925209));
#94349=CARTESIAN_POINT('Ctrl Pts',(6.7595670321814,28.0521353916157,125.65793493382));
#94350=CARTESIAN_POINT('Ctrl Pts',(6.76342927907205,28.0317219363814,125.589812704829));
#94351=CARTESIAN_POINT('Ctrl Pts',(6.76729801520192,28.0112741830305,125.521576018774));
#94352=CARTESIAN_POINT('Ctrl Pts',(6.77116675133179,27.994407634488,125.452370327107));
#94353=CARTESIAN_POINT('Ctrl Pts',(6.77503548746166,27.981185660923,125.382604530602));
#94354=CARTESIAN_POINT('Ctrl Pts',(6.77644083202515,27.9763826896051,125.357261633194));
#94355=CARTESIAN_POINT('Ctrl Pts',(6.77784617658864,27.9720601435449,125.331844874585));
#94356=CARTESIAN_POINT('Ctrl Pts',(6.77925152115213,27.9682193607167,125.306373948523));
#94357=CARTESIAN_POINT('Ctrl Pts',(6.78312059450033,27.9576452489559,125.236249593444));
#94358=CARTESIAN_POINT('Ctrl Pts',(6.78698966784853,27.9506850681282,125.165439812299));
#94359=CARTESIAN_POINT('Ctrl Pts',(6.79085874119674,27.9474173181754,125.094349863665));
#94360=CARTESIAN_POINT('Ctrl Pts',(6.79472204959251,27.944154437198,125.023365839664));
#94361=CARTESIAN_POINT('Ctrl Pts',(6.79858535798829,27.9445730883938,124.952102958123));
#94362=CARTESIAN_POINT('Ctrl Pts',(6.80244866638406,27.9487003168899,124.880974067647));
#94363=CARTESIAN_POINT('Ctrl Pts',(6.80630744287696,27.9528227038883,124.809928615817));
#94364=CARTESIAN_POINT('Ctrl Pts',(6.81016621936986,27.9606449988303,124.739017325455));
#94365=CARTESIAN_POINT('Ctrl Pts',(6.81402499586275,27.9721422035054,124.668653776699));
#94366=CARTESIAN_POINT('Ctrl Pts',(6.81788134145095,27.9836321653125,124.598334554709));
#94367=CARTESIAN_POINT('Ctrl Pts',(6.82173768703914,27.9987923656303,124.528562868027));
#94368=CARTESIAN_POINT('Ctrl Pts',(6.82559403262733,28.0175460548874,124.45974643175));
#94369=CARTESIAN_POINT('Ctrl Pts',(6.82944923887265,28.036294203437,124.390950327031));
#94370=CARTESIAN_POINT('Ctrl Pts',(6.83330444511796,28.0586336055338,124.323109380861));
#94371=CARTESIAN_POINT('Ctrl Pts',(6.83715965136327,28.0844369538239,124.256618685583));
#94372=CARTESIAN_POINT('Ctrl Pts',(6.84101500821451,28.1102413101371,124.190125392807));
#94373=CARTESIAN_POINT('Ctrl Pts',(6.84487036506575,28.1395097035015,124.124982907731));
#94374=CARTESIAN_POINT('Ctrl Pts',(6.84872572191698,28.172066364392,124.06156716473));
#94375=CARTESIAN_POINT('Ctrl Pts',(6.85258511438553,28.2046571041575,123.99808504093));
#94376=CARTESIAN_POINT('Ctrl Pts',(6.85644450685407,28.2405427601609,123.936333700384));
#94377=CARTESIAN_POINT('Ctrl Pts',(6.86030389932261,28.2795015977766,123.876664426608));
#94378=CARTESIAN_POINT('Ctrl Pts',(6.86416547692604,28.3184824933498,123.816961368912));
#94379=CARTESIAN_POINT('Ctrl Pts',(6.86802705452946,28.360539747782,123.75934311725));
#94380=CARTESIAN_POINT('Ctrl Pts',(6.87188863213289,28.4054098946934,123.704129652103));
#94381=CARTESIAN_POINT('Ctrl Pts',(6.87575696624774,28.4503585498446,123.648819581256));
#94382=CARTESIAN_POINT('Ctrl Pts',(6.8796253003626,28.4981295980007,123.595923058155));
#94383=CARTESIAN_POINT('Ctrl Pts',(6.88349363447745,28.5484216159555,123.545724318613));
#94384=CARTESIAN_POINT('Ctrl Pts',(6.88579135364853,28.5782941477421,123.515907192484));
#94385=CARTESIAN_POINT('Ctrl Pts',(6.88808907281961,28.6090554407216,123.487041142892));
#94386=CARTESIAN_POINT('Ctrl Pts',(6.89038679199069,28.6406370524375,123.459178810084));
#94387=CARTESIAN_POINT('Ctrl Pts',(6.89425586533899,28.6938165591956,123.412262106491));
#94388=CARTESIAN_POINT('Ctrl Pts',(6.89812493868729,28.7495319885931,123.368009873212));
#94389=CARTESIAN_POINT('Ctrl Pts',(6.9019940120356,28.8074854407965,123.326707859163));
#94390=CARTESIAN_POINT('Ctrl Pts',(6.90585732043149,28.8653525418598,123.285467385469));
#94391=CARTESIAN_POINT('Ctrl Pts',(6.90972062882737,28.9254506541184,123.247168685001));
#94392=CARTESIAN_POINT('Ctrl Pts',(6.91358393722326,28.9874475937836,123.212058393804));
#94393=CARTESIAN_POINT('Ctrl Pts',(6.91744271371626,29.0493718071528,123.17698928918));
#94394=CARTESIAN_POINT('Ctrl Pts',(6.92130149020926,29.113190002817,123.145101402743));
#94395=CARTESIAN_POINT('Ctrl Pts',(6.92516026670227,29.1785411559556,123.116598043422));
#94396=CARTESIAN_POINT('Ctrl Pts',(6.92901661229056,29.2438511399759,123.088112640298));
#94397=CARTESIAN_POINT('Ctrl Pts',(6.93287295787886,29.3106917212872,123.063007727904));
#94398=CARTESIAN_POINT('Ctrl Pts',(6.93672930346716,29.3786787344663,123.041439955606));
#94399=CARTESIAN_POINT('Ctrl Pts',(6.94058450971258,29.4466456611367,123.019878555426));
#94400=CARTESIAN_POINT('Ctrl Pts',(6.944439715958,29.5157578844515,123.001852367474));
#94401=CARTESIAN_POINT('Ctrl Pts',(6.94829492220343,29.5856144231854,122.987468719193));
#94402=CARTESIAN_POINT('Ctrl Pts',(6.95215027905476,29.6554736909063,122.973084509006));
#94403=CARTESIAN_POINT('Ctrl Pts',(6.95600563590609,29.7260768555264,122.962343216817));
#94404=CARTESIAN_POINT('Ctrl Pts',(6.95986099275742,29.7970127471239,122.955301064296));
#94405=CARTESIAN_POINT('Ctrl Pts',(6.96372038522607,29.8680228912806,122.94825154036));
#94406=CARTESIAN_POINT('Ctrl Pts',(6.96757977769471,29.9393659732674,122.944908933754));
#94407=CARTESIAN_POINT('Ctrl Pts',(6.97143917016336,30.0106266036029,122.945277479124));
#94408=CARTESIAN_POINT('Ctrl Pts',(6.97530074776688,30.081927580726,122.945646233159));
#94409=CARTESIAN_POINT('Ctrl Pts',(6.9791623253704,30.1531455280473,122.949730294191));
#94410=CARTESIAN_POINT('Ctrl Pts',(6.98302390297392,30.2238687213255,122.95748185856));
#94411=CARTESIAN_POINT('Ctrl Pts',(6.98689223708888,30.2947156573103,122.965246985658));
#94412=CARTESIAN_POINT('Ctrl Pts',(6.99076057120383,30.3650656313036,122.976692349675));
#94413=CARTESIAN_POINT('Ctrl Pts',(6.99462890531879,30.4345163632976,122.991718871142));
#94414=CARTESIAN_POINT('Ctrl Pts',(6.99692662448894,30.475768818112,123.000644347952));
#94415=CARTESIAN_POINT('Ctrl Pts',(6.9992243436591,30.5167042642521,123.010832341508));
#94416=CARTESIAN_POINT('Ctrl Pts',(7.00152206282925,30.5572413556232,123.022253900501));
#94417=CARTESIAN_POINT('Ctrl Pts',(7.00539113617735,30.6255007764743,123.04148638551));
#94418=CARTESIAN_POINT('Ctrl Pts',(7.00926020952544,30.6928970531184,123.064294522592));
#94419=CARTESIAN_POINT('Ctrl Pts',(7.01312928287354,30.7590285452722,123.090583013074));
#94420=CARTESIAN_POINT('Ctrl Pts',(7.0169925912692,30.8250615009361,123.116832333479));
#94421=CARTESIAN_POINT('Ctrl Pts',(7.02085589966486,30.8898329651199,123.146551535715));
#94422=CARTESIAN_POINT('Ctrl Pts',(7.02471920806053,30.9529555635828,123.179595304242));
#94423=CARTESIAN_POINT('Ctrl Pts',(7.02857798455332,31.0160041152818,123.212600310359));
#94424=CARTESIAN_POINT('Ctrl Pts',(7.03243676104611,31.0774072149879,123.248921911992));
#94425=CARTESIAN_POINT('Ctrl Pts',(7.0362955375389,31.1367982471179,123.288367063927));
#94426=CARTESIAN_POINT('Ctrl Pts',(7.04015188312699,31.1961518648137,123.327787366689));
#94427=CARTESIAN_POINT('Ctrl Pts',(7.04400822871507,31.2534955259985,123.370327047667));
#94428=CARTESIAN_POINT('Ctrl Pts',(7.04786457430316,31.3084892651872,123.415748313749));
#94429=CARTESIAN_POINT('Ctrl Pts',(7.05171978054837,31.3634667566816,123.461156160287));
#94430=CARTESIAN_POINT('Ctrl Pts',(7.05557498679359,31.4160953301631,123.50944359257));
#94431=CARTESIAN_POINT('Ctrl Pts',(7.05943019303881,31.4660673373546,123.560331939355));
#94432=CARTESIAN_POINT('Ctrl Pts',(7.06328554988996,31.5160412967324,123.611222274123));
#94433=CARTESIAN_POINT('Ctrl Pts',(7.0671409067411,31.5633581449818,123.664713376968));
#94434=CARTESIAN_POINT('Ctrl Pts',(7.07099626359225,31.6077476440311,123.720490298742));
#94435=CARTESIAN_POINT('Ctrl Pts',(7.07485565606069,31.6521836080477,123.776325605335));
#94436=CARTESIAN_POINT('Ctrl Pts',(7.07871504852913,31.6936858028699,123.834451126328));
#94437=CARTESIAN_POINT('Ctrl Pts',(7.08257444099757,31.7320253784512,123.894520171645));
#94438=CARTESIAN_POINT('Ctrl Pts',(7.08643601860089,31.7703866613724,123.954623227227));
#94439=CARTESIAN_POINT('Ctrl Pts',(7.09029759620421,31.8055815206696,124.016671574939));
#94440=CARTESIAN_POINT('Ctrl Pts',(7.09415917380753,31.8374268138397,124.08029338032));
#94441=CARTESIAN_POINT('Ctrl Pts',(7.09802750792229,31.8693278259698,124.144026503277));
#94442=CARTESIAN_POINT('Ctrl Pts',(7.10189584203705,31.8978673764232,124.209338135149));
#94443=CARTESIAN_POINT('Ctrl Pts',(7.10576417615181,31.9229105239492,124.275836565832));
#94444=CARTESIAN_POINT('Ctrl Pts',(7.10806189532381,31.9377856920423,124.315335408113));
#94445=CARTESIAN_POINT('Ctrl Pts',(7.1103596144958,31.9514282307018,124.35525266134));
#94446=CARTESIAN_POINT('Ctrl Pts',(7.1126573336678,31.9638183439836,124.395504280964));
#94447=CARTESIAN_POINT('Ctrl Pts',(7.11737359945938,31.9892501148184,124.478124184649));
#94448=CARTESIAN_POINT('Ctrl Pts',(7.12208986525095,32.0094837420629,124.562414597948));
#94449=CARTESIAN_POINT('Ctrl Pts',(7.12680613104252,32.024337058193,124.647782684517));
#94450=CARTESIAN_POINT('Ctrl Pts',(7.1314577452802,32.0389867619716,124.731980527572));
#94451=CARTESIAN_POINT('Ctrl Pts',(7.13610935951787,32.0484026072813,124.81722670766));
#94452=CARTESIAN_POINT('Ctrl Pts',(7.14076097375554,32.0524559155862,124.902931585593));
#94453=CARTESIAN_POINT('Ctrl Pts',(7.14248240933751,32.0539559344579,124.934648623784));
#94454=CARTESIAN_POINT('Ctrl Pts',(7.14420384491947,32.0547219964684,124.9664282743));
#94455=CARTESIAN_POINT('Ctrl Pts',(7.14592528050144,32.0547492461588,124.998239912027));
#94456=CARTESIAN_POINT('Origin',(-1.54592528053767,30.,125.));
#94457=CARTESIAN_POINT('',(5.99388605120356,28.7479590808042,126.629230216746));
#94458=CARTESIAN_POINT('',(6.05208070802109,28.7479590808042,126.629230216746));
#94459=CARTESIAN_POINT('',(-1.54592528053767,28.7479590808042,126.629230216746));
#94460=CARTESIAN_POINT('',(6.50407471951103,32.0547499427048,125.000485236461));
#94461=CARTESIAN_POINT('Ctrl Pts',(6.05208070802109,28.7479590808042,126.629230216746));
#94462=CARTESIAN_POINT('Ctrl Pts',(6.05593584239997,28.6914085092978,126.585771883601));
#94463=CARTESIAN_POINT('Ctrl Pts',(6.05979097677885,28.6371182741293,126.539361986267));
#94464=CARTESIAN_POINT('Ctrl Pts',(6.06364611115773,28.585402293254,126.490272086087));
#94465=CARTESIAN_POINT('Ctrl Pts',(6.06753106194879,28.533286330212,126.440802514394));
#94466=CARTESIAN_POINT('Ctrl Pts',(6.07141601273984,28.4837849922821,126.38861163239));
#94467=CARTESIAN_POINT('Ctrl Pts',(6.0753009635309,28.4371816356836,126.334015113353));
#94468=CARTESIAN_POINT('Ctrl Pts',(6.07916147856999,28.3908714071385,126.279761998151));
#94469=CARTESIAN_POINT('Ctrl Pts',(6.08302199360908,28.3474230615833,126.223133846222));
#94470=CARTESIAN_POINT('Ctrl Pts',(6.08688250864816,28.307072697256,126.16447185888));
#94471=CARTESIAN_POINT('Ctrl Pts',(6.09077967731521,28.2663392267299,126.105252905787));
#94472=CARTESIAN_POINT('Ctrl Pts',(6.09467684598224,28.2287631453916,126.043961720597));
#94473=CARTESIAN_POINT('Ctrl Pts',(6.09857401464929,28.1945401890826,125.980975246202));
#94474=CARTESIAN_POINT('Ctrl Pts',(6.10247118331633,28.1603172327736,125.917988771808));
#94475=CARTESIAN_POINT('Ctrl Pts',(6.10636835198337,28.129447559376,125.853307489303));
#94476=CARTESIAN_POINT('Ctrl Pts',(6.11026552065042,28.1020766226353,125.787327388164));
#94477=CARTESIAN_POINT('Ctrl Pts',(6.11413459399863,28.0749030074016,125.721822948238));
#94478=CARTESIAN_POINT('Ctrl Pts',(6.11800366734684,28.0510713524173,125.654781756097));
#94479=CARTESIAN_POINT('Ctrl Pts',(6.12187274069505,28.0307555752007,125.58657817714));
#94480=CARTESIAN_POINT('Ctrl Pts',(6.12573604909084,28.010470068666,125.518476222099));
#94481=CARTESIAN_POINT('Ctrl Pts',(6.12959935748662,27.9936901788,125.449215779923));
#94482=CARTESIAN_POINT('Ctrl Pts',(6.13346266588241,27.9805417175088,125.379190991161));
#94483=CARTESIAN_POINT('Ctrl Pts',(6.13732144237532,27.9674086801868,125.309248345865));
#94484=CARTESIAN_POINT('Ctrl Pts',(6.14118021886823,27.9578986990641,125.238543610111));
#94485=CARTESIAN_POINT('Ctrl Pts',(6.14503899536114,27.9520872552484,125.167484185474));
#94486=CARTESIAN_POINT('Ctrl Pts',(6.14889534094935,27.9462794724548,125.096469525983));
#94487=CARTESIAN_POINT('Ctrl Pts',(6.15275168653755,27.9441656438702,125.02510110394));
#94488=CARTESIAN_POINT('Ctrl Pts',(6.15660803212576,27.9457696122914,124.953793109662));
#94489=CARTESIAN_POINT('Ctrl Pts',(6.16046323837109,27.9473731068262,124.882506183064));
#94490=CARTESIAN_POINT('Ctrl Pts',(6.16431844461642,27.9526922068022,124.811280134185));
#94491=CARTESIAN_POINT('Ctrl Pts',(6.16817365086174,27.9616986453253,124.740529095983));
#94492=CARTESIAN_POINT('Ctrl Pts',(6.172029007713,27.9707054356902,124.66977529385));
#94493=CARTESIAN_POINT('Ctrl Pts',(6.17588436456425,27.9833997870615,124.599497020854));
#94494=CARTESIAN_POINT('Ctrl Pts',(6.1797397214155,27.9997017805379,124.530101504879));
#94495=CARTESIAN_POINT('Ctrl Pts',(6.18359911388406,28.0160208382212,124.460633348743));
#94496=CARTESIAN_POINT('Ctrl Pts',(6.18745850635261,28.0359549650724,124.392050268083));
#94497=CARTESIAN_POINT('Ctrl Pts',(6.19131789882117,28.0593736888523,124.324746652744));
#94498=CARTESIAN_POINT('Ctrl Pts',(6.19517947642461,28.082805671991,124.257404931023));
#94499=CARTESIAN_POINT('Ctrl Pts',(6.19904105402804,28.1097259961427,124.191344566791));
#94500=CARTESIAN_POINT('Ctrl Pts',(6.20290263163148,28.1399561398452,124.126939635076));
#94501=CARTESIAN_POINT('Ctrl Pts',(6.20677096574635,28.1702391765186,124.062422015569));
#94502=CARTESIAN_POINT('Ctrl Pts',(6.21063929986123,28.2038433657611,123.99956604001));
#94503=CARTESIAN_POINT('Ctrl Pts',(6.2145076339761,28.240544729224,123.938720247702));
#94504=CARTESIAN_POINT('Ctrl Pts',(6.21680535314706,28.2623446627161,123.902578968456));
#94505=CARTESIAN_POINT('Ctrl Pts',(6.21910307231802,28.2852364919428,123.867146354676));
#94506=CARTESIAN_POINT('Ctrl Pts',(6.22140079148898,28.3091664896413,123.832489998866));
#94507=CARTESIAN_POINT('Ctrl Pts',(6.22526986483719,28.3494616299212,123.774133005415));
#94508=CARTESIAN_POINT('Ctrl Pts',(6.2291389381854,28.3928604218902,123.717750259131));
#94509=CARTESIAN_POINT('Ctrl Pts',(6.23300801153361,28.4391426714857,123.663690918042));
#94510=CARTESIAN_POINT('Ctrl Pts',(6.23687131992939,28.4853559601328,123.609712125835));
#94511=CARTESIAN_POINT('Ctrl Pts',(6.24073462832517,28.5344438648622,123.558050233075));
#94512=CARTESIAN_POINT('Ctrl Pts',(6.24459793672094,28.5861434868903,123.509024707503));
#94513=CARTESIAN_POINT('Ctrl Pts',(6.24845671321385,28.6377824620217,123.460056691945));
#94514=CARTESIAN_POINT('Ctrl Pts',(6.25231548970676,28.6920267181045,123.41371923322));
#94515=CARTESIAN_POINT('Ctrl Pts',(6.25617426619967,28.748574917571,123.370296706278));
#94516=CARTESIAN_POINT('Ctrl Pts',(6.26003061178788,28.8050874934961,123.326901534128));
#94517=CARTESIAN_POINT('Ctrl Pts',(6.26388695737608,28.8639007488459,123.286417945709));
#94518=CARTESIAN_POINT('Ctrl Pts',(6.26774330296429,28.9246796357716,123.249090614345));
#94519=CARTESIAN_POINT('Ctrl Pts',(6.27159850920962,28.9854405658025,123.211774311201));
#94520=CARTESIAN_POINT('Ctrl Pts',(6.27545371545495,29.0481655607565,123.177612667924));
#94521=CARTESIAN_POINT('Ctrl Pts',(6.27930892170027,29.1124913585492,123.146806547106));
#94522=CARTESIAN_POINT('Ctrl Pts',(6.28316427855152,29.1768196692674,123.115999222828));
#94523=CARTESIAN_POINT('Ctrl Pts',(6.28701963540277,29.2427484678968,123.088547889102));
#94524=CARTESIAN_POINT('Ctrl Pts',(6.29087499225402,29.3098922794118,123.064606268357));
#94525=CARTESIAN_POINT('Ctrl Pts',(6.29473438472258,29.3771063741038,123.04063958658));
#94526=CARTESIAN_POINT('Ctrl Pts',(6.29859377719114,29.4455375620182,123.020190115029));
#94527=CARTESIAN_POINT('Ctrl Pts',(6.30245316965969,29.5147837356122,123.00336214118));
#94528=CARTESIAN_POINT('Ctrl Pts',(6.30631474726314,29.5840691154363,122.986524639564));
#94529=CARTESIAN_POINT('Ctrl Pts',(6.31017632486658,29.6541699219043,122.973312807461));
#94530=CARTESIAN_POINT('Ctrl Pts',(6.31403790247002,29.7246750546594,122.963779546077));
#94531=CARTESIAN_POINT('Ctrl Pts',(6.31790623658489,29.7953035485856,122.954229604571));
#94532=CARTESIAN_POINT('Ctrl Pts',(6.32177457069976,29.8663372969278,122.948371124002));
#94533=CARTESIAN_POINT('Ctrl Pts',(6.32564290481463,29.9373619988242,122.946204965604));
#94534=CARTESIAN_POINT('Ctrl Pts',(6.3279406239856,29.9795493627679,122.944918307438));
#94535=CARTESIAN_POINT('Ctrl Pts',(6.33023834315657,30.0217335510174,122.944933353137));
#94536=CARTESIAN_POINT('Ctrl Pts',(6.33253606232754,30.0638286364277,122.946241623834));
#94537=CARTESIAN_POINT('Ctrl Pts',(6.33640513567576,30.1347115254724,122.948444588996));
#94538=CARTESIAN_POINT('Ctrl Pts',(6.34027420902399,30.2056190726874,122.954325827891));
#94539=CARTESIAN_POINT('Ctrl Pts',(6.34414328237221,30.2761385098518,122.963889716671));
#94540=CARTESIAN_POINT('Ctrl Pts',(6.348006590768,30.3465528724506,122.973439355175));
#94541=CARTESIAN_POINT('Ctrl Pts',(6.35186989916379,30.4165797954258,122.986660686914));
#94542=CARTESIAN_POINT('Ctrl Pts',(6.35573320755958,30.4858082931544,123.003506106996));
#94543=CARTESIAN_POINT('Ctrl Pts',(6.3595919840525,30.5549555815166,123.020331766345));
#94544=CARTESIAN_POINT('Ctrl Pts',(6.36345076054542,30.6233058353202,123.040772955254));
#94545=CARTESIAN_POINT('Ctrl Pts',(6.36730953703834,30.6904567041093,123.064730741667));
#94546=CARTESIAN_POINT('Ctrl Pts',(6.37116588262656,30.7575652700174,123.088673435447));
#94547=CARTESIAN_POINT('Ctrl Pts',(6.37502222821477,30.8234754935007,123.116128168673));
#94548=CARTESIAN_POINT('Ctrl Pts',(6.37887857380298,30.887800095922,123.146946155078));
#94549=CARTESIAN_POINT('Ctrl Pts',(6.38273378004833,30.9521056938803,123.177755036424));
#94550=CARTESIAN_POINT('Ctrl Pts',(6.38658898629367,31.0148261629487,123.211924988476));
#94551=CARTESIAN_POINT('Ctrl Pts',(6.39044419253901,31.0755957294053,123.249259759592));
#94552=CARTESIAN_POINT('Ctrl Pts',(6.39429954939027,31.1363676698609,123.286595989212));
#94553=CARTESIAN_POINT('Ctrl Pts',(6.39815490624154,31.1951881436347,123.327097027188));
#94554=CARTESIAN_POINT('Ctrl Pts',(6.4020102630928,31.2517189340083,123.370522392684));
#94555=CARTESIAN_POINT('Ctrl Pts',(6.40586965556137,31.308308898317,123.413993213935));
#94556=CARTESIAN_POINT('Ctrl Pts',(6.40972904802994,31.3626040087628,123.460394176724));
#94557=CARTESIAN_POINT('Ctrl Pts',(6.41358844049851,31.4142985602054,123.509444014771));
#94558=CARTESIAN_POINT('Ctrl Pts',(6.41745001810195,31.4660223803912,123.558521624161));
#94559=CARTESIAN_POINT('Ctrl Pts',(6.42131159570539,31.515142375816,123.610250741924));
#94560=CARTESIAN_POINT('Ctrl Pts',(6.42517317330884,31.5613911358037,123.664314676455));
#94561=CARTESIAN_POINT('Ctrl Pts',(6.42904150742372,31.6077208161582,123.71847320538));
#94562=CARTESIAN_POINT('Ctrl Pts',(6.4329098415386,31.651168934825,123.774974322028));
#94563=CARTESIAN_POINT('Ctrl Pts',(6.43677817565348,31.6915100663368,123.8334704213));
#94564=CARTESIAN_POINT('Ctrl Pts',(6.43907589482435,31.715471954968,123.868216026185));
#94565=CARTESIAN_POINT('Ctrl Pts',(6.44137361399522,31.7383385030997,123.903664960457));
#94566=CARTESIAN_POINT('Ctrl Pts',(6.44367133316609,31.7600702303999,123.939740434346));
#94567=CARTESIAN_POINT('Ctrl Pts',(6.447668184011,31.7978722706675,124.002493224209));
#94568=CARTESIAN_POINT('Ctrl Pts',(6.4516650348559,31.8323780045921,124.067375195747));
#94569=CARTESIAN_POINT('Ctrl Pts',(6.4556618857008,31.8633501421989,124.134018585611));
#94570=CARTESIAN_POINT('Ctrl Pts',(6.45969628851426,31.8946132750874,124.201288116048));
#94571=CARTESIAN_POINT('Ctrl Pts',(6.46373069132772,31.922275754658,124.27035199445));
#94572=CARTESIAN_POINT('Ctrl Pts',(6.46776509414118,31.9461388143962,124.340802550369));
#94573=CARTESIAN_POINT('Ctrl Pts',(6.47174648700002,31.9696883259411,124.410327422625));
#94574=CARTESIAN_POINT('Ctrl Pts',(6.47572787985886,31.989537493609,124.481202326664));
#94575=CARTESIAN_POINT('Ctrl Pts',(6.4797092727177,32.005542326812,124.553012821363));
#94576=CARTESIAN_POINT('Ctrl Pts',(6.48377018050848,32.0218668027299,124.626257489177));
#94577=CARTESIAN_POINT('Ctrl Pts',(6.48783108829924,32.0341915119557,124.700475103802));
#94578=CARTESIAN_POINT('Ctrl Pts',(6.49189199609001,32.0424167700166,124.775208318537));
#94579=CARTESIAN_POINT('Ctrl Pts',(6.49595290388078,32.0506420280775,124.849941533272));
#94580=CARTESIAN_POINT('Ctrl Pts',(6.50001381167156,32.0547677239393,124.9251898674));
#94581=CARTESIAN_POINT('Ctrl Pts',(6.50407471946233,32.0547499427051,125.000485235558));
#94582=CARTESIAN_POINT('Ctrl Pts',(6.50407471951103,32.0547499427048,125.000485236461));
#94583=CARTESIAN_POINT('Ctrl Pts',(6.50830237655217,32.054731431302,125.078872387748));
#94584=CARTESIAN_POINT('Ctrl Pts',(6.5125300335933,32.050222603001,125.157140435482));
#94585=CARTESIAN_POINT('Ctrl Pts',(6.51675769063444,32.0412922455004,125.234784009166));
#94586=CARTESIAN_POINT('Ctrl Pts',(6.52089243721851,32.0325581488575,125.310721224021));
#94587=CARTESIAN_POINT('Ctrl Pts',(6.52502718380259,32.0195950692566,125.38606079366));
#94588=CARTESIAN_POINT('Ctrl Pts',(6.52916193038667,32.0025186272063,125.460344121491));
#94589=CARTESIAN_POINT('Ctrl Pts',(6.53343604265633,31.9848666069422,125.537131241684));
#94590=CARTESIAN_POINT('Ctrl Pts',(6.537710154926,31.9628191668451,125.612789222109));
#94591=CARTESIAN_POINT('Ctrl Pts',(6.54198426719566,31.936558210849,125.686833210098));
#94592=CARTESIAN_POINT('Ctrl Pts',(6.54625837946533,31.9102972548528,125.760877198087));
#94593=CARTESIAN_POINT('Ctrl Pts',(6.55053249173499,31.8798230313505,125.833306828918));
#94594=CARTESIAN_POINT('Ctrl Pts',(6.55480660400465,31.8453691251967,125.903664956868));
#94595=CARTESIAN_POINT('Ctrl Pts',(6.55867567735285,31.8141802650006,125.967355552833));
#94596=CARTESIAN_POINT('Ctrl Pts',(6.56254475070105,31.7796291418859,126.029554339915));
#94597=CARTESIAN_POINT('Ctrl Pts',(6.56641382404924,31.7418816971559,126.089883349544));
#94598=CARTESIAN_POINT('Ctrl Pts',(6.570277132445,31.704190496442,126.150122468432));
#94599=CARTESIAN_POINT('Ctrl Pts',(6.57414044084076,31.6633126832059,126.208496931507));
#94600=CARTESIAN_POINT('Ctrl Pts',(6.57800374923652,31.6194608366348,126.264651794411));
#94601=CARTESIAN_POINT('Ctrl Pts',(6.58186252572942,31.5756604310279,126.320740784141));
#94602=CARTESIAN_POINT('Ctrl Pts',(6.58572130222231,31.5288932194177,126.374614964573));
#94603=CARTESIAN_POINT('Ctrl Pts',(6.5895800787152,31.4794150018976,126.425948391303));
#94604=CARTESIAN_POINT('Ctrl Pts',(6.59343642430339,31.4299679540584,126.477249479631));
#94605=CARTESIAN_POINT('Ctrl Pts',(6.59729276989158,31.3778136249756,126.52601264087));
#94606=CARTESIAN_POINT('Ctrl Pts',(6.60114911547976,31.323247043448,126.57194619008));
#94607=CARTESIAN_POINT('Ctrl Pts',(6.60500432172508,31.2686965834128,126.617866168394));
#94608=CARTESIAN_POINT('Ctrl Pts',(6.60885952797039,31.2117356572602,126.660957881695));
#94609=CARTESIAN_POINT('Ctrl Pts',(6.61271473421571,31.1526936970903,126.70096878372));
#94610=CARTESIAN_POINT('Ctrl Pts',(6.61657009106693,31.0936494304113,126.740981248793));
#94611=CARTESIAN_POINT('Ctrl Pts',(6.62042544791816,31.0325243716912,126.777912392946));
#94612=CARTESIAN_POINT('Ctrl Pts',(6.62428080476939,30.96967691557,126.811552991748));
#94613=CARTESIAN_POINT('Ctrl Pts',(6.62814019723793,30.9067636735069,126.845228804043));
#94614=CARTESIAN_POINT('Ctrl Pts',(6.63199958970647,30.842124864157,126.875606965473));
#94615=CARTESIAN_POINT('Ctrl Pts',(6.63585898217501,30.7761426666099,126.902524670949));
#94616=CARTESIAN_POINT('Ctrl Pts',(6.63972055977842,30.710123110851,126.929457616859));
#94617=CARTESIAN_POINT('Ctrl Pts',(6.64358213738184,30.6427591117206,126.952926046633));
#94618=CARTESIAN_POINT('Ctrl Pts',(6.64744371498526,30.5744493672173,126.972816637958));
#94619=CARTESIAN_POINT('Ctrl Pts',(6.65131204910011,30.506020102762,126.992742031382));
#94620=CARTESIAN_POINT('Ctrl Pts',(6.65518038321497,30.4366422621867,127.009076976597));
#94621=CARTESIAN_POINT('Ctrl Pts',(6.65904871732982,30.3667254312339,127.021759140102));
#94622=CARTESIAN_POINT('Ctrl Pts',(6.66134643650095,30.3251961222096,127.029292111493));
#94623=CARTESIAN_POINT('Ctrl Pts',(6.66364415567209,30.2834767822568,127.035537320761));
#94624=CARTESIAN_POINT('Ctrl Pts',(6.66594187484322,30.241653645354,127.040490401395));
#94625=CARTESIAN_POINT('Ctrl Pts',(6.66980984684837,30.1712487304541,127.048828399126));
#94626=CARTESIAN_POINT('Ctrl Pts',(6.67367781885353,30.1002739036248,127.053534580682));
#94627=CARTESIAN_POINT('Ctrl Pts',(6.67754579085868,30.0291363638787,127.054543412732));
#94628=CARTESIAN_POINT('Ctrl Pts',(6.68140849508152,29.958095706187,127.055550870856));
#94629=CARTESIAN_POINT('Ctrl Pts',(6.68527119930435,29.8868932563362,127.052870960964));
#94630=CARTESIAN_POINT('Ctrl Pts',(6.68913390352719,29.8159423184307,127.046489758673));
#94631=CARTESIAN_POINT('Ctrl Pts',(6.69299263972165,29.7450642660785,127.040115111581));
#94632=CARTESIAN_POINT('Ctrl Pts',(6.69685137591611,29.6744376942221,127.030046760409));
#94633=CARTESIAN_POINT('Ctrl Pts',(6.70071011211057,29.6044751682032,127.01632280896));
#94634=CARTESIAN_POINT('Ctrl Pts',(6.70456617537579,29.534561104912,127.00260836403));
#94635=CARTESIAN_POINT('Ctrl Pts',(6.70842223864102,29.4653106496237,126.985243439874));
#94636=CARTESIAN_POINT('Ctrl Pts',(6.71227830190625,29.3971287887083,126.964317658907));
#94637=CARTESIAN_POINT('Ctrl Pts',(6.71613400852199,29.3289532339721,126.943393813379));
#94638=CARTESIAN_POINT('Ctrl Pts',(6.71998971513772,29.261846545289,126.918909895312));
#94639=CARTESIAN_POINT('Ctrl Pts',(6.72384542175346,29.1961997300817,126.891005734676));
#94640=CARTESIAN_POINT('Ctrl Pts',(6.72770090156705,29.1305567763815,126.863103215432));
#94641=CARTESIAN_POINT('Ctrl Pts',(6.73155638138065,29.0663739695936,126.831781050833));
#94642=CARTESIAN_POINT('Ctrl Pts',(6.73541186119425,29.004021513207,126.797226868357));
#94643=CARTESIAN_POINT('Ctrl Pts',(6.73927005804661,28.9416251157159,126.762648334813));
#94644=CARTESIAN_POINT('Ctrl Pts',(6.74312825489898,28.8810620638715,126.724833480967));
#94645=CARTESIAN_POINT('Ctrl Pts',(6.74698645175134,28.8226761136759,126.684014854207));
#94646=CARTESIAN_POINT('Ctrl Pts',(6.74865985643731,28.7973525424869,126.666310707968));
#94647=CARTESIAN_POINT('Ctrl Pts',(6.75033326112327,28.7724381426773,126.648042037699));
#94648=CARTESIAN_POINT('Ctrl Pts',(6.75200666580924,28.7479590808042,126.629230216746));
#94649=CARTESIAN_POINT('',(6.44592528053627,32.0547499999799,124.999990915418));
#94650=CARTESIAN_POINT('Ctrl Pts',(6.44592528053768,32.0547499999799,124.999990915444));
#94651=CARTESIAN_POINT('Ctrl Pts',(6.44979385259826,32.0547503134814,125.070898847444));
#94652=CARTESIAN_POINT('Ctrl Pts',(6.45366242465885,32.0510758456684,125.141945865384));
#94653=CARTESIAN_POINT('Ctrl Pts',(6.45753099671943,32.0437093535415,125.212719629435));
#94654=CARTESIAN_POINT('Ctrl Pts',(6.4613938042328,32.0363538382016,125.28338793372));
#94655=CARTESIAN_POINT('Ctrl Pts',(6.46525661174617,32.0253172686326,125.353783312964));
#94656=CARTESIAN_POINT('Ctrl Pts',(6.46911941925955,32.0106344132236,125.423493587745));
#94657=CARTESIAN_POINT('Ctrl Pts',(6.47297769671014,31.9959687769632,125.493122110609));
#94658=CARTESIAN_POINT('Ctrl Pts',(6.47683597416074,31.9776654483258,125.562066651731));
#94659=CARTESIAN_POINT('Ctrl Pts',(6.48069425161134,31.95581076705,125.629922063426));
#94660=CARTESIAN_POINT('Ctrl Pts',(6.48455010010933,31.9339698442417,125.697734757204));
#94661=CARTESIAN_POINT('Ctrl Pts',(6.48840594860733,31.9085821530335,125.764459220432));
#94662=CARTESIAN_POINT('Ctrl Pts',(6.49226179710532,31.8797843322491,125.829703818679));
#94663=CARTESIAN_POINT('Ctrl Pts',(6.49611650897049,31.8509950005295,125.894929184025));
#94664=CARTESIAN_POINT('Ctrl Pts',(6.49997122083567,31.8187977310236,125.958675106127));
#94665=CARTESIAN_POINT('Ctrl Pts',(6.50382593270084,31.7833772733353,126.020569969895));
#94666=CARTESIAN_POINT('Ctrl Pts',(6.5076807986421,31.7479553998615,126.082467307653));
#94667=CARTESIAN_POINT('Ctrl Pts',(6.51153566458336,31.7093103257038,126.142513019533));
#94668=CARTESIAN_POINT('Ctrl Pts',(6.51539053052462,31.6676718636714,126.200361661175));
#94669=CARTESIAN_POINT('Ctrl Pts',(6.51924943297198,31.6259898011847,126.25827087727));
#94670=CARTESIAN_POINT('Ctrl Pts',(6.52310833541935,31.5813083783217,126.313978035487));
#94671=CARTESIAN_POINT('Ctrl Pts',(6.52696723786672,31.5338991807731,126.367168923624));
#94672=CARTESIAN_POINT('Ctrl Pts',(6.53082833001037,31.486463081341,126.420389994408));
#94673=CARTESIAN_POINT('Ctrl Pts',(6.53468942215402,31.436296467927,126.471091607219));
#94674=CARTESIAN_POINT('Ctrl Pts',(6.53855051429767,31.3837075199641,126.518996728665));
#94675=CARTESIAN_POINT('Ctrl Pts',(6.54241835505554,31.3310266543496,126.566985581131));
#94676=CARTESIAN_POINT('Ctrl Pts',(6.54628619581342,31.2759153771664,126.612167875522));
#94677=CARTESIAN_POINT('Ctrl Pts',(6.55015403657129,31.2187140609584,126.654307589332));
#94678=CARTESIAN_POINT('Ctrl Pts',(6.55242968420586,31.1850596144411,126.679100528353));
#94679=CARTESIAN_POINT('Ctrl Pts',(6.55470533184043,31.1506822350121,126.702841082442));
#94680=CARTESIAN_POINT('Ctrl Pts',(6.556980979475,31.1156552945761,126.72548857608));
#94681=CARTESIAN_POINT('Ctrl Pts',(6.56085005282323,31.0561022250886,126.763994016338));
#94682=CARTESIAN_POINT('Ctrl Pts',(6.56471912617146,30.9944367163052,126.799488160214));
#94683=CARTESIAN_POINT('Ctrl Pts',(6.56858819951969,30.9309957744205,126.831732630738));
#94684=CARTESIAN_POINT('Ctrl Pts',(6.57245150791549,30.8676493600825,126.863929056725));
#94685=CARTESIAN_POINT('Ctrl Pts',(6.5763148163113,30.8025331932406,126.892885202362));
#94686=CARTESIAN_POINT('Ctrl Pts',(6.58017812470711,30.7360123801297,126.918406458182));
#94687=CARTESIAN_POINT('Ctrl Pts',(6.58403690120003,30.6695696001018,126.94389777597));
#94688=CARTESIAN_POINT('Ctrl Pts',(6.58789567769296,30.6017258981203,126.96596203441));
#94689=CARTESIAN_POINT('Ctrl Pts',(6.59175445418588,30.5328684724145,126.984451751393));
#94690=CARTESIAN_POINT('Ctrl Pts',(6.5956107997741,30.4640544246657,127.002929820451));
#94691=CARTESIAN_POINT('Ctrl Pts',(6.59946714536232,30.3942283882477,127.017837689994));
#94692=CARTESIAN_POINT('Ctrl Pts',(6.60332349095054,30.3237935215411,127.029077454881));
#94693=CARTESIAN_POINT('Ctrl Pts',(6.60717869719588,30.2533794645522,127.040313899022));
#94694=CARTESIAN_POINT('Ctrl Pts',(6.61103390344123,30.1823574138346,127.047884313496));
#94695=CARTESIAN_POINT('Ctrl Pts',(6.61488910968657,30.1111398380587,127.051742064417));
#94696=CARTESIAN_POINT('Ctrl Pts',(6.61874446653784,30.0399194801259,127.055599966043));
#94697=CARTESIAN_POINT('Ctrl Pts',(6.6225998233891,29.9685040671639,127.055744892087));
#94698=CARTESIAN_POINT('Ctrl Pts',(6.62645518024037,29.8973085596836,127.052182260567));
#94699=CARTESIAN_POINT('Ctrl Pts',(6.63031457270894,29.82603852789,127.048615899841));
#94700=CARTESIAN_POINT('Ctrl Pts',(6.63417396517751,29.754989347257,127.041334258715));
#94701=CARTESIAN_POINT('Ctrl Pts',(6.63803335764608,29.6845724363159,127.030394792785));
#94702=CARTESIAN_POINT('Ctrl Pts',(6.64189493524953,29.6141156562895,127.01944913308));
#94703=CARTESIAN_POINT('Ctrl Pts',(6.64575651285299,29.5442923343048,127.004841625352));
#94704=CARTESIAN_POINT('Ctrl Pts',(6.64961809045644,29.475502541807,126.986680643397));
#94705=CARTESIAN_POINT('Ctrl Pts',(6.65348642457132,29.4065923894286,126.9684878856));
#94706=CARTESIAN_POINT('Ctrl Pts',(6.6573547586862,29.3387198396882,126.946729388641));
#94707=CARTESIAN_POINT('Ctrl Pts',(6.66122309280108,29.2722680150932,126.921562832864));
#94708=CARTESIAN_POINT('Ctrl Pts',(6.66352081197191,29.2327968559911,126.906614362552));
#94709=CARTESIAN_POINT('Ctrl Pts',(6.66581853114274,29.1938265516438,126.890464398356));
#94710=CARTESIAN_POINT('Ctrl Pts',(6.66811625031357,29.1554332511046,126.8731536427));
#94711=CARTESIAN_POINT('Ctrl Pts',(6.67198550524007,29.0907806733909,126.844003114883));
#94712=CARTESIAN_POINT('Ctrl Pts',(6.67585476016658,29.0275124357899,126.811444295521));
#94713=CARTESIAN_POINT('Ctrl Pts',(6.67972401509308,28.9660116427636,126.775631053907));
#94714=CARTESIAN_POINT('Ctrl Pts',(6.68358710221244,28.9046088854154,126.739874900589));
#94715=CARTESIAN_POINT('Ctrl Pts',(6.6874501893318,28.8449683939462,126.700874869843));
#94716=CARTESIAN_POINT('Ctrl Pts',(6.69131327645116,28.787451626233,126.658832120431));
#94717=CARTESIAN_POINT('Ctrl Pts',(6.69220513385481,28.7741729313617,126.649125858011));
#94718=CARTESIAN_POINT('Ctrl Pts',(6.69309699125846,28.7610073299989,126.639257616034));
#94719=CARTESIAN_POINT('Ctrl Pts',(6.69398884866211,28.7479590808042,126.629230216746));
#94720=CARTESIAN_POINT('Ctrl Pts',(5.99388605120356,28.7479590808042,126.629230216746));
#94721=CARTESIAN_POINT('Ctrl Pts',(5.99635890922978,28.711936345746,126.601547242388));
#94722=CARTESIAN_POINT('Ctrl Pts',(5.998831767256,28.6768711114662,126.572698926717));
#94723=CARTESIAN_POINT('Ctrl Pts',(6.00130462528222,28.6428394576485,126.542761428343));
#94724=CARTESIAN_POINT('Ctrl Pts',(6.00517369863043,28.589592986001,126.495920738));
#94725=CARTESIAN_POINT('Ctrl Pts',(6.00904277197863,28.5386700366482,126.446228460409));
#94726=CARTESIAN_POINT('Ctrl Pts',(6.01291184532684,28.4903916335173,126.393944095847));
#94727=CARTESIAN_POINT('Ctrl Pts',(6.01677515372263,28.4421851656207,126.341737635435));
#94728=CARTESIAN_POINT('Ctrl Pts',(6.02063846211841,28.3966157492422,126.286947108469));
#94729=CARTESIAN_POINT('Ctrl Pts',(6.02450177051419,28.3539699294822,126.229870956422));
#94730=CARTESIAN_POINT('Ctrl Pts',(6.0283605470071,28.3113741359415,126.172861758279));
#94731=CARTESIAN_POINT('Ctrl Pts',(6.03221932350001,28.2716954161049,126.113572648055));
#94732=CARTESIAN_POINT('Ctrl Pts',(6.03607809999291,28.2351809694626,126.052336140191));
#94733=CARTESIAN_POINT('Ctrl Pts',(6.03993444558111,28.1986895257437,125.991138209352));
#94734=CARTESIAN_POINT('Ctrl Pts',(6.04379079116931,28.1653586485718,125.927995731075));
#94735=CARTESIAN_POINT('Ctrl Pts',(6.04764713675752,28.1353921673442,125.863270057919));
#94736=CARTESIAN_POINT('Ctrl Pts',(6.05150234300284,28.1054345396013,125.798563507721));
#94737=CARTESIAN_POINT('Ctrl Pts',(6.05535754924817,28.0788395384251,125.732275131848));
#94738=CARTESIAN_POINT('Ctrl Pts',(6.0592127554935,28.0557641846639,125.664789182271));
#94739=CARTESIAN_POINT('Ctrl Pts',(6.06306811234474,28.0326879294503,125.597300596315));
#94740=CARTESIAN_POINT('Ctrl Pts',(6.06692346919598,28.0131317497201,125.528614804142));
#94741=CARTESIAN_POINT('Ctrl Pts',(6.07077882604722,27.9972032527053,125.459132607779));
#94742=CARTESIAN_POINT('Ctrl Pts',(6.07463821851578,27.9812580824431,125.38957768052));
#94743=CARTESIAN_POINT('Ctrl Pts',(6.07849761098433,27.9689482839275,125.31922515941));
#94744=CARTESIAN_POINT('Ctrl Pts',(6.08235700345289,27.9603304240579,125.24848658611));
#94745=CARTESIAN_POINT('Ctrl Pts',(6.08621858105632,27.9517076848748,125.177707961603));
#94746=CARTESIAN_POINT('Ctrl Pts',(6.09008015865975,27.9467810790954,125.106543334643));
#94747=CARTESIAN_POINT('Ctrl Pts',(6.09394173626318,27.9455550884156,125.035407171095));
#94748=CARTESIAN_POINT('Ctrl Pts',(6.09781007037804,27.9443269526488,124.964146542277));
#94749=CARTESIAN_POINT('Ctrl Pts',(6.10167840449291,27.9468123423206,124.892914961947));
#94750=CARTESIAN_POINT('Ctrl Pts',(6.10554673860778,27.9529636818119,124.822123991166));
#94751=CARTESIAN_POINT('Ctrl Pts',(6.10784445777877,27.9566174641007,124.780075459196));
#94752=CARTESIAN_POINT('Ctrl Pts',(6.11014217694977,27.9615636544421,124.738182247744));
#94753=CARTESIAN_POINT('Ctrl Pts',(6.11243989612077,27.9677837873881,124.696528703668));
#94754=CARTESIAN_POINT('Ctrl Pts',(6.11630896946898,27.9782577177568,124.626389315323));
#94755=CARTESIAN_POINT('Ctrl Pts',(6.1201780428172,27.9923875858268,124.556655420757));
#94756=CARTESIAN_POINT('Ctrl Pts',(6.12404711616542,28.010129485962,124.487737469785));
#94757=CARTESIAN_POINT('Ctrl Pts',(6.12791042456121,28.027844950514,124.418922207151));
#94758=CARTESIAN_POINT('Ctrl Pts',(6.13177373295699,28.0491616439716,124.350920941469));
#94759=CARTESIAN_POINT('Ctrl Pts',(6.13563704135278,28.0739842444241,124.284136275697));
#94760=CARTESIAN_POINT('Ctrl Pts',(6.1394958178457,28.0987777264106,124.217429952523));
#94761=CARTESIAN_POINT('Ctrl Pts',(6.14335459433861,28.1270687778571,124.151937847601));
#94762=CARTESIAN_POINT('Ctrl Pts',(6.14721337083153,28.1587121110232,124.088047987881));
#94763=CARTESIAN_POINT('Ctrl Pts',(6.15106971641973,28.1903355099103,124.024198376712));
#94764=CARTESIAN_POINT('Ctrl Pts',(6.15492606200794,28.225306785587,123.961949442474));
#94765=CARTESIAN_POINT('Ctrl Pts',(6.15878240759615,28.2634328997717,123.901668415776));
#94766=CARTESIAN_POINT('Ctrl Pts',(6.16263761384149,28.3015477497386,123.841405198881));
#94767=CARTESIAN_POINT('Ctrl Pts',(6.16649282008682,28.3428153282392,123.7831091456));
#94768=CARTESIAN_POINT('Ctrl Pts',(6.17034802633216,28.3869979709246,123.727120580456));
#94769=CARTESIAN_POINT('Ctrl Pts',(6.17420338318341,28.4311823396311,123.671129828086));
#94770=CARTESIAN_POINT('Ctrl Pts',(6.17805874003466,28.4782816959494,123.617447122803));
#94771=CARTESIAN_POINT('Ctrl Pts',(6.18191409688591,28.5280176709366,123.566380250755));
#94772=CARTESIAN_POINT('Ctrl Pts',(6.18577348935447,28.5778057073463,123.515259924161));
#94773=CARTESIAN_POINT('Ctrl Pts',(6.18963288182303,28.6302355321652,123.466761245462));
#94774=CARTESIAN_POINT('Ctrl Pts',(6.19349227429159,28.6849920711719,123.421154944392));
#94775=CARTESIAN_POINT('Ctrl Pts',(6.19735385189503,28.7397796125771,123.375522821662));
#94776=CARTESIAN_POINT('Ctrl Pts',(6.20121542949847,28.7968961014709,123.332786627734));
#94777=CARTESIAN_POINT('Ctrl Pts',(6.20507700710191,28.8559957577356,123.293174919278));
#94778=CARTESIAN_POINT('Ctrl Pts',(6.20894534121678,28.9151988192777,123.253493903148));
#94779=CARTESIAN_POINT('Ctrl Pts',(6.21281367533165,28.9763915587476,123.216948536352));
#94780=CARTESIAN_POINT('Ctrl Pts',(6.21668200944653,29.0392024024643,123.183722064476));
#94781=CARTESIAN_POINT('Ctrl Pts',(6.21897972861746,29.0765108860298,123.163986152546));
#94782=CARTESIAN_POINT('Ctrl Pts',(6.2212774477884,29.1143898337748,123.145420289185));
#94783=CARTESIAN_POINT('Ctrl Pts',(6.22357516695933,29.152758367233,123.128054707475));
#94784=CARTESIAN_POINT('Ctrl Pts',(6.22744424030755,29.2173662062113,123.098813227393));
#94785=CARTESIAN_POINT('Ctrl Pts',(6.23131331365577,29.2836162215103,123.072863185084));
#94786=CARTESIAN_POINT('Ctrl Pts',(6.23518238700398,29.3511397635226,123.050390306749));
#94787=CARTESIAN_POINT('Ctrl Pts',(6.23904569539977,29.4185626948789,123.027950913195));
#94788=CARTESIAN_POINT('Ctrl Pts',(6.24290900379556,29.4872549291607,123.008978551621));
#94789=CARTESIAN_POINT('Ctrl Pts',(6.24677231219135,29.5568265229058,122.993611495323));
#94790=CARTESIAN_POINT('Ctrl Pts',(6.25063108868426,29.6263165048113,122.978262465545));
#94791=CARTESIAN_POINT('Ctrl Pts',(6.25448986517718,29.6966833251354,122.966510444591));
#94792=CARTESIAN_POINT('Ctrl Pts',(6.25834864167009,29.7675221866832,122.958443821783));
#94793=CARTESIAN_POINT('Ctrl Pts',(6.2622049872583,29.8383164220336,122.950382280688));
#94794=CARTESIAN_POINT('Ctrl Pts',(6.26606133284651,29.9095816271033,122.946001586392));
#94795=CARTESIAN_POINT('Ctrl Pts',(6.26991767843472,29.9809045784329,122.945338731719));
#94796=CARTESIAN_POINT('Ctrl Pts',(6.27377288468005,30.0522064576634,122.944676072884));
#94797=CARTESIAN_POINT('Ctrl Pts',(6.27762809092539,30.1235655637827,122.947729077512));
#94798=CARTESIAN_POINT('Ctrl Pts',(6.28148329717073,30.1945670747283,122.954482653231));
#94799=CARTESIAN_POINT('Ctrl Pts',(6.28533865402197,30.2655713593899,122.961236492783));
#94800=CARTESIAN_POINT('Ctrl Pts',(6.28919401087323,30.3362175377482,122.971691142247));
#94801=CARTESIAN_POINT('Ctrl Pts',(6.29304936772447,30.4060960479373,122.985779663902));
#94802=CARTESIAN_POINT('Ctrl Pts',(6.29690876019304,30.4760477038653,122.9998829328));
#94803=CARTESIAN_POINT('Ctrl Pts',(6.3007681526616,30.5452296103558,123.017627570876));
#94804=CARTESIAN_POINT('Ctrl Pts',(6.30462754513016,30.6132434306251,123.038895704636));
#94805=CARTESIAN_POINT('Ctrl Pts',(6.3084891227336,30.6812957593831,123.060175880121));
#94806=CARTESIAN_POINT('Ctrl Pts',(6.31235070033704,30.7481782296867,123.084983353613));
#94807=CARTESIAN_POINT('Ctrl Pts',(6.31621227794047,30.8135112824055,123.113151581102));
#94808=CARTESIAN_POINT('Ctrl Pts',(6.32008061205535,30.8789586468287,123.141369093875));
#94809=CARTESIAN_POINT('Ctrl Pts',(6.32394894617022,30.9428507455124,123.172958885326));
#94810=CARTESIAN_POINT('Ctrl Pts',(6.3278172802851,31.0048320976367,123.207708166046));
#94811=CARTESIAN_POINT('Ctrl Pts',(6.33011499945603,31.0416478784838,123.228348598365));
#94812=CARTESIAN_POINT('Ctrl Pts',(6.33241271862696,31.0777900498444,123.250102894812));
#94813=CARTESIAN_POINT('Ctrl Pts',(6.33471043779789,31.1131893460155,123.272919503203));
#94814=CARTESIAN_POINT('Ctrl Pts',(6.33857951114609,31.1727973586454,123.311339834345));
#94815=CARTESIAN_POINT('Ctrl Pts',(6.3424485844943,31.2305307484908,123.352924986983));
#94816=CARTESIAN_POINT('Ctrl Pts',(6.34631765784251,31.2860335365731,123.397465973744));
#94817=CARTESIAN_POINT('Ctrl Pts',(6.35018096623829,31.3414536250258,123.441940594053));
#94818=CARTESIAN_POINT('Ctrl Pts',(6.35404427463407,31.3946493332136,123.489362004667));
#94819=CARTESIAN_POINT('Ctrl Pts',(6.35790758302985,31.4452930003888,123.53947759157));
#94820=CARTESIAN_POINT('Ctrl Pts',(6.36176635952276,31.4958772593683,123.589534389747));
#94821=CARTESIAN_POINT('Ctrl Pts',(6.36562513601567,31.5439150802219,123.642278746475));
#94822=CARTESIAN_POINT('Ctrl Pts',(6.36948391250857,31.589112655769,123.697418513192));
#94823=CARTESIAN_POINT('Ctrl Pts',(6.37334025809677,31.6342817583016,123.752523543634));
#94824=CARTESIAN_POINT('Ctrl Pts',(6.37719660368497,31.6766138581668,123.810020615361));
#94825=CARTESIAN_POINT('Ctrl Pts',(6.38105294927317,31.7158537585188,123.869582624923));
#94826=CARTESIAN_POINT('Ctrl Pts',(6.3849081555185,31.7550820655891,123.929127037111));
#94827=CARTESIAN_POINT('Ctrl Pts',(6.38876336176383,31.7912197197443,123.990734770518));
#94828=CARTESIAN_POINT('Ctrl Pts',(6.39261856800916,31.8240544161559,124.054049129499));
#94829=CARTESIAN_POINT('Ctrl Pts',(6.3964739248604,31.8568903952743,124.117365961892));
#94830=CARTESIAN_POINT('Ctrl Pts',(6.40032928171164,31.8864229387857,124.182389119965));
#94831=CARTESIAN_POINT('Ctrl Pts',(6.40418463856289,31.9124861523391,124.248738208338));
#94832=CARTESIAN_POINT('Ctrl Pts',(6.40804403103144,31.9385766477135,124.315156748007));
#94833=CARTESIAN_POINT('Ctrl Pts',(6.41190342349999,31.9611903857793,124.382903535508));
#94834=CARTESIAN_POINT('Ctrl Pts',(6.41576281596854,31.9802103536273,124.45157998041));
#94835=CARTESIAN_POINT('Ctrl Pts',(6.41962439357197,31.9992410903193,124.520295308969));
#94836=CARTESIAN_POINT('Ctrl Pts',(6.4234859711754,32.0146739011013,124.589940868241));
#94837=CARTESIAN_POINT('Ctrl Pts',(6.42734754877883,32.0264428476096,124.660107446578));
#94838=CARTESIAN_POINT('Ctrl Pts',(6.43121588289369,32.0382323859666,124.730396793725));
#94839=CARTESIAN_POINT('Ctrl Pts',(6.43508421700856,32.0463452058351,124.80120849722));
#94840=CARTESIAN_POINT('Ctrl Pts',(6.43895255112342,32.0507672808363,124.872128492809));
#94841=CARTESIAN_POINT('Ctrl Pts',(6.44125027029443,32.0533939118884,124.914253663137));
#94842=CARTESIAN_POINT('Ctrl Pts',(6.44354798946544,32.0547193955748,124.956417024693));
#94843=CARTESIAN_POINT('Ctrl Pts',(6.44584570863644,32.0547494759025,124.998532424289));
#94844=CARTESIAN_POINT('Ctrl Pts',(6.44587223260258,32.054749823138,124.999018587893));
#94845=CARTESIAN_POINT('Ctrl Pts',(6.44589875656872,32.0547499978305,124.99950475162));
#94846=CARTESIAN_POINT('Ctrl Pts',(6.44592528053486,32.0547499999799,124.999990915392));
#94847=CARTESIAN_POINT('Origin',(-1.54592528053767,30.,125.));
#94848=CARTESIAN_POINT('',(5.29388025228517,28.7479590808042,126.629230216746));
#94849=CARTESIAN_POINT('',(5.35213747706482,28.7479590808042,126.629230216746));
#94850=CARTESIAN_POINT('',(-1.54592528053767,28.7479590808042,126.629230216746));
#94851=CARTESIAN_POINT('',(5.80407471941277,32.0547491412311,124.998121407385));
#94852=CARTESIAN_POINT('Ctrl Pts',(5.35213747706482,28.7479590808042,126.629230216746));
#94853=CARTESIAN_POINT('Ctrl Pts',(5.35599720622694,28.6915568646519,126.585885892641));
#94854=CARTESIAN_POINT('Ctrl Pts',(5.35985693538906,28.6373376428878,126.539555115962));
#94855=CARTESIAN_POINT('Ctrl Pts',(5.36371666455118,28.5856307672311,126.490488925117));
#94856=CARTESIAN_POINT('Ctrl Pts',(5.36757358561901,28.5339615102197,126.441458431723));
#94857=CARTESIAN_POINT('Ctrl Pts',(5.37143050668683,28.4848013246118,126.389696805431));
#94858=CARTESIAN_POINT('Ctrl Pts',(5.37528742775466,28.4384459391161,126.335494843658));
#94859=CARTESIAN_POINT('Ctrl Pts',(5.37914283300616,28.3921087718439,126.281314183907));
#94860=CARTESIAN_POINT('Ctrl Pts',(5.38299823825766,28.3485745323137,126.224695461029));
#94861=CARTESIAN_POINT('Ctrl Pts',(5.38685364350916,28.3081003662311,126.165964489919));
#94862=CARTESIAN_POINT('Ctrl Pts',(5.39070882322953,28.2676285677814,126.107236954418));
#94863=CARTESIAN_POINT('Ctrl Pts',(5.39456400294989,28.2302167617084,126.046397816908));
#94864=CARTESIAN_POINT('Ctrl Pts',(5.39841918267026,28.1960792358592,125.983802540758));
#94865=CARTESIAN_POINT('Ctrl Pts',(5.40227815643071,28.1619081138742,125.921145662036));
#94866=CARTESIAN_POINT('Ctrl Pts',(5.40613713019115,28.1310179420956,125.856729619846));
#94867=CARTESIAN_POINT('Ctrl Pts',(5.4099961039516,28.1035769800651,125.790934442265));
#94868=CARTESIAN_POINT('Ctrl Pts',(5.41385692499008,28.0761228821365,125.725107768749));
#94869=CARTESIAN_POINT('Ctrl Pts',(5.41771774602856,28.0521214469396,125.657901102821));
#94870=CARTESIAN_POINT('Ctrl Pts',(5.42157856706705,28.0316917009795,125.58971179614));
#94871=CARTESIAN_POINT('Ctrl Pts',(5.42544650242978,28.0112243091829,125.521396837213));
#94872=CARTESIAN_POINT('Ctrl Pts',(5.42931443779252,27.9943418718265,125.452096092942));
#94873=CARTESIAN_POINT('Ctrl Pts',(5.43318237315526,27.9811126060574,125.382218854951));
#94874=CARTESIAN_POINT('Ctrl Pts',(5.43660621397653,27.9694022500334,125.320364527648));
#94875=CARTESIAN_POINT('Ctrl Pts',(5.4400300547978,27.9605536157451,125.258058844669));
#94876=CARTESIAN_POINT('Ctrl Pts',(5.44345389561907,27.9545799673092,125.195587454524));
#94877=CARTESIAN_POINT('Ctrl Pts',(5.44732296896728,27.9478295121444,125.124992352924));
#94878=CARTESIAN_POINT('Ctrl Pts',(5.45119204231549,27.9447248768961,125.053909088628));
#94879=CARTESIAN_POINT('Ctrl Pts',(5.4550611156637,27.9453224383922,124.982746585111));
#94880=CARTESIAN_POINT('Ctrl Pts',(5.45892442405948,27.9459191095165,124.911690114334));
#94881=CARTESIAN_POINT('Ctrl Pts',(5.46278773245526,27.9502070236293,124.840555120507));
#94882=CARTESIAN_POINT('Ctrl Pts',(5.46665104085104,27.9581907664977,124.769755311712));
#94883=CARTESIAN_POINT('Ctrl Pts',(5.47050981734395,27.9661651439354,124.699038555531));
#94884=CARTESIAN_POINT('Ctrl Pts',(5.47436859383686,27.9778266843104,124.628656683752));
#94885=CARTESIAN_POINT('Ctrl Pts',(5.47822737032977,27.9931279671206,124.559021308739));
#94886=CARTESIAN_POINT('Ctrl Pts',(5.48208371591797,28.0084196106162,124.489429801765));
#94887=CARTESIAN_POINT('Ctrl Pts',(5.48594006150617,28.0273463434201,124.420584331896));
#94888=CARTESIAN_POINT('Ctrl Pts',(5.48979640709437,28.0498093885281,124.352887844785));
#94889=CARTESIAN_POINT('Ctrl Pts',(5.4936516133397,28.0722657970135,124.285211358348));
#94890=CARTESIAN_POINT('Ctrl Pts',(5.49750681958503,28.0982562906977,124.218683641557));
#94891=CARTESIAN_POINT('Ctrl Pts',(5.50136202583035,28.1276322948654,124.153692290435));
#94892=CARTESIAN_POINT('Ctrl Pts',(5.5052173826816,28.1570094466242,124.088698400387));
#94893=CARTESIAN_POINT('Ctrl Pts',(5.50907273953284,28.1897721693534,124.025241436929));
#94894=CARTESIAN_POINT('Ctrl Pts',(5.51292809638408,28.2257245380356,123.963687234677));
#94895=CARTESIAN_POINT('Ctrl Pts',(5.51678748885264,28.2617145400699,123.902068600205));
#94896=CARTESIAN_POINT('Ctrl Pts',(5.52064688132119,28.3009006075052,123.842357123209));
#94897=CARTESIAN_POINT('Ctrl Pts',(5.52450627378975,28.3430422566957,123.784891527721));
#94898=CARTESIAN_POINT('Ctrl Pts',(5.52836785139318,28.3852077659077,123.727393396004));
#94899=CARTESIAN_POINT('Ctrl Pts',(5.53222942899661,28.4303318806798,123.672144053556));
#94900=CARTESIAN_POINT('Ctrl Pts',(5.53609100660004,28.4781341470793,123.619448701346));
#94901=CARTESIAN_POINT('Ctrl Pts',(5.53995934071491,28.5260200519791,123.56666114932));
#94902=CARTESIAN_POINT('Ctrl Pts',(5.54382767482978,28.576593119241,123.516436851755));
#94903=CARTESIAN_POINT('Ctrl Pts',(5.54769600894465,28.629536935203,123.469043256481));
#94904=CARTESIAN_POINT('Ctrl Pts',(5.54999372811564,28.6609845861321,123.44089233435));
#94905=CARTESIAN_POINT('Ctrl Pts',(5.55229144728663,28.6932680392849,123.41373934893));
#94906=CARTESIAN_POINT('Ctrl Pts',(5.55458916645762,28.7263160946048,123.387633146075));
#94907=CARTESIAN_POINT('Ctrl Pts',(5.55845823980583,28.7819649100314,123.343673546936));
#94908=CARTESIAN_POINT('Ctrl Pts',(5.56232731315405,28.840001213987,123.302512198001));
#94909=CARTESIAN_POINT('Ctrl Pts',(5.56619638650227,28.9001120288155,123.264418249306));
#94910=CARTESIAN_POINT('Ctrl Pts',(5.57005969489806,28.960133278015,123.22638106092));
#94911=CARTESIAN_POINT('Ctrl Pts',(5.57392300329384,29.0222224954769,123.191402458471));
#94912=CARTESIAN_POINT('Ctrl Pts',(5.57778631168963,29.0860345941753,123.159710675069));
#94913=CARTESIAN_POINT('Ctrl Pts',(5.58164508818254,29.1497718372826,123.128056068115));
#94914=CARTESIAN_POINT('Ctrl Pts',(5.58550386467546,29.2152275141707,123.099680836624));
#94915=CARTESIAN_POINT('Ctrl Pts',(5.58936264116837,29.282030092187,123.07476838433));
#94916=CARTESIAN_POINT('Ctrl Pts',(5.59321898675658,29.3487905867342,123.049871626077));
#94917=CARTESIAN_POINT('Ctrl Pts',(5.59707533234479,29.4168958449018,123.028433488424));
#94918=CARTESIAN_POINT('Ctrl Pts',(5.600931677933,29.4859537613948,123.010589527756));
#94919=CARTESIAN_POINT('Ctrl Pts',(5.60478688417833,29.5549912749848,122.992750839019));
#94920=CARTESIAN_POINT('Ctrl Pts',(5.60864209042367,29.6249804180435,122.978504340596));
#94921=CARTESIAN_POINT('Ctrl Pts',(5.612497296669,29.6955149726789,122.967935426558));
#94922=CARTESIAN_POINT('Ctrl Pts',(5.61635265352025,29.7660522827885,122.95736609964));
#94923=CARTESIAN_POINT('Ctrl Pts',(5.62020801037151,29.8371345660277,122.950474712148));
#94924=CARTESIAN_POINT('Ctrl Pts',(5.62406336722276,29.9083482061054,122.947295074499));
#94925=CARTESIAN_POINT('Ctrl Pts',(5.62792275969132,29.9796363894768,122.944112108546));
#94926=CARTESIAN_POINT('Ctrl Pts',(5.63178215215988,30.0510557178678,122.944648670073));
#94927=CARTESIAN_POINT('Ctrl Pts',(5.63564154462844,30.1221911847723,122.948886430042));
#94928=CARTESIAN_POINT('Ctrl Pts',(5.63950312223188,30.1933669275988,122.953126589374));
#94929=CARTESIAN_POINT('Ctrl Pts',(5.64336469983532,30.2642580060058,122.961072064643));
#94930=CARTESIAN_POINT('Ctrl Pts',(5.64722627743876,30.3344558992232,122.972652764331));
#94931=CARTESIAN_POINT('Ctrl Pts',(5.65109461155363,30.4047766160419,122.984253726497));
#94932=CARTESIAN_POINT('Ctrl Pts',(5.65496294566851,30.4744012514923,122.999502507974));
#94933=CARTESIAN_POINT('Ctrl Pts',(5.65883127978338,30.5429334995985,123.018278329958));
#94934=CARTESIAN_POINT('Ctrl Pts',(5.66112899895431,30.583640391926,123.029430822179));
#94935=CARTESIAN_POINT('Ctrl Pts',(5.66342671812525,30.6239621832624,123.041826753286));
#94936=CARTESIAN_POINT('Ctrl Pts',(5.66572443729618,30.6638192197252,123.055432797247));
#94937=CARTESIAN_POINT('Ctrl Pts',(5.66959351064439,30.7309335126585,123.078343683281));
#94938=CARTESIAN_POINT('Ctrl Pts',(5.6734625839926,30.7969917617406,123.104778072836));
#94939=CARTESIAN_POINT('Ctrl Pts',(5.67733165734081,30.8615980944628,123.134618997063));
#94940=CARTESIAN_POINT('Ctrl Pts',(5.68119496573659,30.9261081631958,123.164415458058));
#94941=CARTESIAN_POINT('Ctrl Pts',(5.68505827413237,30.9891701723712,123.197608176431));
#94942=CARTESIAN_POINT('Ctrl Pts',(5.68892158252814,31.050405210603,123.234031014984));
#94943=CARTESIAN_POINT('Ctrl Pts',(5.69278035902105,31.1115684162972,123.270411127264));
#94944=CARTESIAN_POINT('Ctrl Pts',(5.69663913551396,31.170908492586,123.31001358609));
#94945=CARTESIAN_POINT('Ctrl Pts',(5.70049791200686,31.2280698480367,123.352625722295));
#94946=CARTESIAN_POINT('Ctrl Pts',(5.70435425759507,31.2851951936774,123.395211014229));
#94947=CARTESIAN_POINT('Ctrl Pts',(5.70821060318327,31.3401441529922,123.440801932254));
#94948=CARTESIAN_POINT('Ctrl Pts',(5.71206694877147,31.3925901753256,123.489142572548));
#94949=CARTESIAN_POINT('Ctrl Pts',(5.71592215501679,31.445020702678,123.537468930781));
#94950=CARTESIAN_POINT('Ctrl Pts',(5.71977736126212,31.4949494041244,123.588543069396));
#94951=CARTESIAN_POINT('Ctrl Pts',(5.72363256750745,31.5420842183893,123.642070021726));
#94952=CARTESIAN_POINT('Ctrl Pts',(5.72748792435869,31.5892208740036,123.695599065118));
#94953=CARTESIAN_POINT('Ctrl Pts',(5.73134328120994,31.6335631063536,123.751580746428));
#94954=CARTESIAN_POINT('Ctrl Pts',(5.73519863806119,31.6748581792137,123.809685906149));
#94955=CARTESIAN_POINT('Ctrl Pts',(5.73905803052974,31.7161964779325,123.867851887785));
#94956=CARTESIAN_POINT('Ctrl Pts',(5.74291742299829,31.7544809679474,123.928145388184));
#94957=CARTESIAN_POINT('Ctrl Pts',(5.74677681546684,31.7895019636561,123.990207801292));
#94958=CARTESIAN_POINT('Ctrl Pts',(5.75063839307027,31.8245427877703,124.052305353284));
#94959=CARTESIAN_POINT('Ctrl Pts',(5.7544999706737,31.8563162228096,124.116173376588));
#94960=CARTESIAN_POINT('Ctrl Pts',(5.75836154827713,31.8846595887185,124.181430639987));
#94961=CARTESIAN_POINT('Ctrl Pts',(5.762229882392,31.9130525463476,124.246802082484));
#94962=CARTESIAN_POINT('Ctrl Pts',(5.76609821650687,31.9380032825452,124.313567162888));
#94963=CARTESIAN_POINT('Ctrl Pts',(5.76996655062173,31.959398326717,124.3813274212));
#94964=CARTESIAN_POINT('Ctrl Pts',(5.77226426979273,31.9721065886453,124.421575765819));
#94965=CARTESIAN_POINT('Ctrl Pts',(5.77456198896374,31.9835613184562,124.462174966916));
#94966=CARTESIAN_POINT('Ctrl Pts',(5.77685970813474,31.993747313396,124.50304002895));
#94967=CARTESIAN_POINT('Ctrl Pts',(5.78191177765028,32.0161435901778,124.592891363594));
#94968=CARTESIAN_POINT('Ctrl Pts',(5.78696384716583,32.0324751044743,124.684310306464));
#94969=CARTESIAN_POINT('Ctrl Pts',(5.79201591668137,32.0425683991186,124.776590292462));
#94970=CARTESIAN_POINT('Ctrl Pts',(5.79603551759184,32.050598972771,124.850011434945));
#94971=CARTESIAN_POINT('Ctrl Pts',(5.80005511850231,32.0546813536987,124.923977405718));
#94972=CARTESIAN_POINT('Ctrl Pts',(5.80407471941277,32.0547491412311,124.998121407385));
#94973=CARTESIAN_POINT('Ctrl Pts',(5.80407471946232,32.0547491412319,124.998121408299));
#94974=CARTESIAN_POINT('Ctrl Pts',(5.80788808427068,32.0548134507169,125.068461258701));
#94975=CARTESIAN_POINT('Ctrl Pts',(5.81170144907905,32.0512616122161,125.138896596669));
#94976=CARTESIAN_POINT('Ctrl Pts',(5.81551481388741,32.0440909046791,125.209021376677));
#94977=CARTESIAN_POINT('Ctrl Pts',(5.81932566294079,32.036924927805,125.279099893929));
#94978=CARTESIAN_POINT('Ctrl Pts',(5.82313651199416,32.0261448653963,125.348867764812));
#94979=CARTESIAN_POINT('Ctrl Pts',(5.82694736104754,32.0118000195851,125.417921336734));
#94980=CARTESIAN_POINT('Ctrl Pts',(5.83075704398274,31.9974595632906,125.486953778293));
#94981=CARTESIAN_POINT('Ctrl Pts',(5.83456672691795,31.9795565892288,125.555271866759));
#94982=CARTESIAN_POINT('Ctrl Pts',(5.83837640985316,31.9581916522906,125.62248133739));
#94983=CARTESIAN_POINT('Ctrl Pts',(5.84218627454151,31.9368256960695,125.689694014466));
#94984=CARTESIAN_POINT('Ctrl Pts',(5.84599613922986,31.9119976032409,125.755797494637));
#94985=CARTESIAN_POINT('Ctrl Pts',(5.84980600391822,31.8838574485761,125.820413722426));
#94986=CARTESIAN_POINT('Ctrl Pts',(5.85361981396699,31.8556881529677,125.885096864483));
#94987=CARTESIAN_POINT('Ctrl Pts',(5.85743362401575,31.8242001532027,125.948289224179));
#94988=CARTESIAN_POINT('Ctrl Pts',(5.86124743406452,31.7895907717114,126.009634801453));
#94989=CARTESIAN_POINT('Ctrl Pts',(5.86506356527418,31.75496032626,126.07101771487));
#94990=CARTESIAN_POINT('Ctrl Pts',(5.86887969648384,31.7172049893137,126.130551190878));
#94991=CARTESIAN_POINT('Ctrl Pts',(5.8726958276935,31.6765654040786,126.187908249128));
#94992=CARTESIAN_POINT('Ctrl Pts',(5.87651830066288,31.6358582827786,126.245360625035));
#94993=CARTESIAN_POINT('Ctrl Pts',(5.88034077363226,31.5922576630893,126.300628980545));
#94994=CARTESIAN_POINT('Ctrl Pts',(5.88416324660164,31.5460437137614,126.353420259062));
#94995=CARTESIAN_POINT('Ctrl Pts',(5.88544049072553,31.5306017483915,126.371059978379));
#94996=CARTESIAN_POINT('Ctrl Pts',(5.88671773484941,31.5148682976354,126.388423448839));
#94997=CARTESIAN_POINT('Ctrl Pts',(5.88799497897329,31.4988546567116,126.40550072236));
#94998=CARTESIAN_POINT('Ctrl Pts',(5.89186405232151,31.4503455658121,126.45723180697));
#94999=CARTESIAN_POINT('Ctrl Pts',(5.89573312566972,31.3990601643257,126.50654992552));
#95000=CARTESIAN_POINT('Ctrl Pts',(5.89960219901793,31.3452680229113,126.553142462568));
#95001=CARTESIAN_POINT('Ctrl Pts',(5.90346550741372,31.2915560322484,126.599665576337));
#95002=CARTESIAN_POINT('Ctrl Pts',(5.9073288158095,31.2353450798584,126.643470854395));
#95003=CARTESIAN_POINT('Ctrl Pts',(5.91119212420528,31.1769425622697,126.684281380179));
#95004=CARTESIAN_POINT('Ctrl Pts',(5.91505090069819,31.1186085544943,126.725044032659));
#95005=CARTESIAN_POINT('Ctrl Pts',(5.9189096771911,31.0580884843514,126.762818634032));
#95006=CARTESIAN_POINT('Ctrl Pts',(5.92276845368401,30.9957225538103,126.797368676241));
#95007=CARTESIAN_POINT('Ctrl Pts',(5.92662479927221,30.9333959117936,126.831896953038));
#95008=CARTESIAN_POINT('Ctrl Pts',(5.9304811448604,30.8692261403504,126.863204466019));
#95009=CARTESIAN_POINT('Ctrl Pts',(5.93433749044861,30.8035808867985,126.891098971728));
#95010=CARTESIAN_POINT('Ctrl Pts',(5.93819269669394,30.737955027891,126.91898523611));
#95011=CARTESIAN_POINT('Ctrl Pts',(5.94204790293927,30.6708549991597,126.943460305214));
#95012=CARTESIAN_POINT('Ctrl Pts',(5.9459031091846,30.6026698482921,126.964379448187));
#95013=CARTESIAN_POINT('Ctrl Pts',(5.94975846603584,30.5344820337313,126.985299408378));
#95014=CARTESIAN_POINT('Ctrl Pts',(5.95361382288709,30.4652094779392,127.002663026264));
#95015=CARTESIAN_POINT('Ctrl Pts',(5.95746917973834,30.3952562000437,127.016375485575));
#95016=CARTESIAN_POINT('Ctrl Pts',(5.96132857220689,30.325229698146,127.030102298483));
#95017=CARTESIAN_POINT('Ctrl Pts',(5.96518796467544,30.2545215294256,127.040170229863));
#95018=CARTESIAN_POINT('Ctrl Pts',(5.969047357144,30.1835448252715,127.046535819285));
#95019=CARTESIAN_POINT('Ctrl Pts',(5.97290893474743,30.1125279350846,127.052905012816));
#95020=CARTESIAN_POINT('Ctrl Pts',(5.97677051235087,30.0412426924747,127.055567673329));
#95021=CARTESIAN_POINT('Ctrl Pts',(5.98063208995431,29.9701034964048,127.054532492216));
#95022=CARTESIAN_POINT('Ctrl Pts',(5.98450042406917,29.8988398297581,127.053495499872));
#95023=CARTESIAN_POINT('Ctrl Pts',(5.98836875818404,29.8277232046938,127.048747780675));
#95024=CARTESIAN_POINT('Ctrl Pts',(5.99223709229891,29.7571634625664,127.040349964733));
#95025=CARTESIAN_POINT('Ctrl Pts',(5.99453481146989,29.7152522761561,127.035361816835));
#95026=CARTESIAN_POINT('Ctrl Pts',(5.99683253064088,29.6735374017371,127.029086849354));
#95027=CARTESIAN_POINT('Ctrl Pts',(5.99913024981186,29.6321025567787,127.021546198772));
#95028=CARTESIAN_POINT('Ctrl Pts',(6.00299944643827,29.5623292074706,127.008848276345));
#95029=CARTESIAN_POINT('Ctrl Pts',(6.00686864306468,29.4930773581584,126.992508916017));
#95030=CARTESIAN_POINT('Ctrl Pts',(6.01073783969108,29.4247558951416,126.97258505072));
#95031=CARTESIAN_POINT('Ctrl Pts',(6.01460043069499,29.3565510728223,126.952695200117));
#95032=CARTESIAN_POINT('Ctrl Pts',(6.01846302169889,29.2892739434971,126.929233137685));
#95033=CARTESIAN_POINT('Ctrl Pts',(6.02232561270279,29.2233236559803,126.902306867764));
#95034=CARTESIAN_POINT('Ctrl Pts',(6.02618437409812,29.1574387556056,126.87540729419));
#95035=CARTESIAN_POINT('Ctrl Pts',(6.03004313549344,29.0928785346375,126.845050509388));
#95036=CARTESIAN_POINT('Ctrl Pts',(6.03390189688877,29.030026205475,126.811394048912));
#95037=CARTESIAN_POINT('Ctrl Pts',(6.03775817556283,28.9672143154064,126.777759242953));
#95038=CARTESIAN_POINT('Ctrl Pts',(6.0416144542369,28.9061085638573,126.740829202853));
#95039=CARTESIAN_POINT('Ctrl Pts',(6.04547073291096,28.8470698469948,126.700808520907));
#95040=CARTESIAN_POINT('Ctrl Pts',(6.04767405794767,28.8133374604137,126.677942286911));
#95041=CARTESIAN_POINT('Ctrl Pts',(6.04987738298438,28.7802794301862,126.654067958849));
#95042=CARTESIAN_POINT('Ctrl Pts',(6.05208070802109,28.7479590808042,126.629230216746));
#95043=CARTESIAN_POINT('',(5.74592528057331,32.0547492412561,125.001765802243));
#95044=CARTESIAN_POINT('Ctrl Pts',(5.74592528057331,32.0547492412561,125.001765802243));
#95045=CARTESIAN_POINT('Ctrl Pts',(5.75057817989322,32.0546753518283,125.087746124368));
#95046=CARTESIAN_POINT('Ctrl Pts',(5.75523107921313,32.0492009128721,125.173490900321));
#95047=CARTESIAN_POINT('Ctrl Pts',(5.75988397853304,32.038437023012,125.258402913517));
#95048=CARTESIAN_POINT('Ctrl Pts',(5.76460377517814,32.0275183747119,125.344535754023));
#95049=CARTESIAN_POINT('Ctrl Pts',(5.76932357182325,32.011157157185,125.42981172292));
#95050=CARTESIAN_POINT('Ctrl Pts',(5.77404336846835,31.9895181111569,125.513629485017));
#95051=CARTESIAN_POINT('Ctrl Pts',(5.7757069401806,31.9818910654261,125.543172465042));
#95052=CARTESIAN_POINT('Ctrl Pts',(5.77737051189285,31.9736087726741,125.572534484309));
#95053=CARTESIAN_POINT('Ctrl Pts',(5.77903408360509,31.9646798449384,125.601689844848));
#95054=CARTESIAN_POINT('Ctrl Pts',(5.78290315695331,31.9439132761898,125.669498300347));
#95055=CARTESIAN_POINT('Ctrl Pts',(5.78677223030153,31.9195914246618,125.736363214624));
#95056=CARTESIAN_POINT('Ctrl Pts',(5.79064130364975,31.8918186201618,125.801885198086));
#95057=CARTESIAN_POINT('Ctrl Pts',(5.79450461204554,31.8640871973784,125.867309553231));
#95058=CARTESIAN_POINT('Ctrl Pts',(5.79836792044133,31.8329152162861,125.931394505826));
#95059=CARTESIAN_POINT('Ctrl Pts',(5.80223122883712,31.7984566891989,125.993756056372));
#95060=CARTESIAN_POINT('Ctrl Pts',(5.80609000533003,31.7640385841237,126.056044452911));
#95061=CARTESIAN_POINT('Ctrl Pts',(5.80994878182295,31.7263418248365,126.116613039969));
#95062=CARTESIAN_POINT('Ctrl Pts',(5.81380755831586,31.6855676731745,126.17509964754));
#95063=CARTESIAN_POINT('Ctrl Pts',(5.81766390390407,31.6448192079127,126.233549410435));
#95064=CARTESIAN_POINT('Ctrl Pts',(5.82152024949228,31.6009974737035,126.289919398434));
#95065=CARTESIAN_POINT('Ctrl Pts',(5.82537659508049,31.5543478680564,126.343875093738));
#95066=CARTESIAN_POINT('Ctrl Pts',(5.82923180132582,31.5077120448608,126.397814848033));
#95067=CARTESIAN_POINT('Ctrl Pts',(5.83308700757116,31.4582503264415,126.449341358437));
#95068=CARTESIAN_POINT('Ctrl Pts',(5.83694221381649,31.4062482494225,126.498153337778));
#95069=CARTESIAN_POINT('Ctrl Pts',(5.84079757066774,31.3542441409115,126.546967223989));
#95070=CARTESIAN_POINT('Ctrl Pts',(5.84465292751899,31.2996998324739,126.593066037739));
#95071=CARTESIAN_POINT('Ctrl Pts',(5.84850828437024,31.2429362859692,126.636186710471));
#95072=CARTESIAN_POINT('Ctrl Pts',(5.8523676768388,31.1861133218904,126.679352520019));
#95073=CARTESIAN_POINT('Ctrl Pts',(5.85622706930737,31.1270668701352,126.719533671088));
#95074=CARTESIAN_POINT('Ctrl Pts',(5.86008646177593,31.0661486922933,126.756509188254));
#95075=CARTESIAN_POINT('Ctrl Pts',(5.86394803937936,31.005196023418,126.793505640449));
#95076=CARTESIAN_POINT('Ctrl Pts',(5.8678096169828,30.9423699468735,126.827292615469));
#95077=CARTESIAN_POINT('Ctrl Pts',(5.87167119458624,30.8780463317198,126.857695400719));
#95078=CARTESIAN_POINT('Ctrl Pts',(5.87553952870111,30.8136101710508,126.888151381007));
#95079=CARTESIAN_POINT('Ctrl Pts',(5.87940786281599,30.7476716900085,126.915211165115));
#95080=CARTESIAN_POINT('Ctrl Pts',(5.88327619693086,30.6806255415029,126.938748677563));
#95081=CARTESIAN_POINT('Ctrl Pts',(5.88557391610179,30.6408013649495,126.952729526162));
#95082=CARTESIAN_POINT('Ctrl Pts',(5.88787163527272,30.600586674591,126.965468625186));
#95083=CARTESIAN_POINT('Ctrl Pts',(5.89016935444365,30.5600659399301,126.976948078587));
#95084=CARTESIAN_POINT('Ctrl Pts',(5.89403860385591,30.4918309568413,126.996278930193));
#95085=CARTESIAN_POINT('Ctrl Pts',(5.89790785326818,30.4224603226495,127.012110772205));
#95086=CARTESIAN_POINT('Ctrl Pts',(5.90177710268044,30.3523462206453,127.02431462557));
#95087=CARTESIAN_POINT('Ctrl Pts',(5.90563962094158,30.2823540928449,127.036497248466));
#95088=CARTESIAN_POINT('Ctrl Pts',(5.90950213920273,30.2116215417877,127.045064340978));
#95089=CARTESIAN_POINT('Ctrl Pts',(5.91336465746388,30.1405544631544,127.049937073519));
#95090=CARTESIAN_POINT('Ctrl Pts',(5.91722337855583,30.069557249232,127.054805015768));
#95091=CARTESIAN_POINT('Ctrl Pts',(5.92108209964779,29.998226642092,127.055985769382));
#95092=CARTESIAN_POINT('Ctrl Pts',(5.92494082073974,29.9269760550714,127.053451987743));
#95093=CARTESIAN_POINT('Ctrl Pts',(5.92879703930303,29.8557716767901,127.050919849359));
#95094=CARTESIAN_POINT('Ctrl Pts',(5.93265325786631,29.7846476999144,127.044677973575));
#95095=CARTESIAN_POINT('Ctrl Pts',(5.9365094764296,29.7140182217139,127.03475108674));
#95096=CARTESIAN_POINT('Ctrl Pts',(5.94036448407861,29.6434109222987,127.024827317106));
#95097=CARTESIAN_POINT('Ctrl Pts',(5.94421949172763,29.5732982938219,127.011220902373));
#95098=CARTESIAN_POINT('Ctrl Pts',(5.94807449937664,29.5040882647224,126.994008303221));
#95099=CARTESIAN_POINT('Ctrl Pts',(5.95193183765665,29.4348363931536,126.976785297807));
#95100=CARTESIAN_POINT('Ctrl Pts',(5.95578917593665,29.3664886850711,126.95595186316));
#95101=CARTESIAN_POINT('Ctrl Pts',(5.95964651421665,29.2994408433327,126.931635170137));
#95102=CARTESIAN_POINT('Ctrl Pts',(5.96350485068227,29.2323756512388,126.907312184543));
#95103=CARTESIAN_POINT('Ctrl Pts',(5.96736318714789,29.1666114466945,126.879504327395));
#95104=CARTESIAN_POINT('Ctrl Pts',(5.9712215236135,29.1025243520487,126.848387141222));
#95105=CARTESIAN_POINT('Ctrl Pts',(5.97508578864727,29.0383387836925,126.817222141604));
#95106=CARTESIAN_POINT('Ctrl Pts',(5.97895005368104,28.9758359044361,126.782737881705));
#95107=CARTESIAN_POINT('Ctrl Pts',(5.98281431871481,28.9153670784502,126.745155863523));
#95108=CARTESIAN_POINT('Ctrl Pts',(5.98650489621106,28.8576161513119,126.70926304837));
#95109=CARTESIAN_POINT('Ctrl Pts',(5.99019547370731,28.8017206368457,126.670545230028));
#95110=CARTESIAN_POINT('Ctrl Pts',(5.99388605120356,28.7479590808042,126.629230216746));
#95111=CARTESIAN_POINT('Ctrl Pts',(5.29388025228516,28.7479590808042,126.629230216746));
#95112=CARTESIAN_POINT('Ctrl Pts',(5.29773979489958,28.691380642155,126.585750468087));
#95113=CARTESIAN_POINT('Ctrl Pts',(5.30159933751399,28.637099473738,126.539342931937));
#95114=CARTESIAN_POINT('Ctrl Pts',(5.30545888012841,28.5854206239971,126.4902894858));
#95115=CARTESIAN_POINT('Ctrl Pts',(5.30932071288091,28.5337111095598,126.441206932804));
#95116=CARTESIAN_POINT('Ctrl Pts',(5.31318254563342,28.4846073216076,126.389475697383));
#95117=CARTESIAN_POINT('Ctrl Pts',(5.31704437838592,28.4383759216136,126.335412969947));
#95118=CARTESIAN_POINT('Ctrl Pts',(5.32091286111107,28.3920649123862,126.281257147942));
#95119=CARTESIAN_POINT('Ctrl Pts',(5.32478134383621,28.3486364598602,126.224762205235));
#95120=CARTESIAN_POINT('Ctrl Pts',(5.32864982656136,28.3083151279993,126.166276063522));
#95121=CARTESIAN_POINT('Ctrl Pts',(5.33059755112453,28.2880139261936,126.136829145204));
#95122=CARTESIAN_POINT('Ctrl Pts',(5.33254527568769,28.2684996609268,126.106877883204));
#95123=CARTESIAN_POINT('Ctrl Pts',(5.33449300025086,28.2497965371345,126.076468950353));
#95124=CARTESIAN_POINT('Ctrl Pts',(5.33836207359907,28.2126435642954,126.016062877611));
#95125=CARTESIAN_POINT('Ctrl Pts',(5.34223114694728,28.1785487493109,125.953612795032));
#95126=CARTESIAN_POINT('Ctrl Pts',(5.3461002202955,28.147742810437,125.889460997578));
#95127=CARTESIAN_POINT('Ctrl Pts',(5.34996352869128,28.1169827726759,125.825404786851));
#95128=CARTESIAN_POINT('Ctrl Pts',(5.35382683708706,28.0895020923367,125.759652328628));
#95129=CARTESIAN_POINT('Ctrl Pts',(5.35769014548284,28.0654870977575,125.692573023989));
#95130=CARTESIAN_POINT('Ctrl Pts',(5.36154892197575,28.0415002742719,125.625572407578));
#95131=CARTESIAN_POINT('Ctrl Pts',(5.36540769846866,28.0209712240985,125.557248491575));
#95132=CARTESIAN_POINT('Ctrl Pts',(5.36926647496157,28.0040386621117,125.487991700908));
#95133=CARTESIAN_POINT('Ctrl Pts',(5.37312282054977,27.9871167670928,125.418778539785));
#95134=CARTESIAN_POINT('Ctrl Pts',(5.37697916613798,27.9737869803036,125.34863414072));
#95135=CARTESIAN_POINT('Ctrl Pts',(5.38083551172618,27.9641380924166,125.277963766975));
#95136=CARTESIAN_POINT('Ctrl Pts',(5.38469071797151,27.9544920552575,125.207314272528));
#95137=CARTESIAN_POINT('Ctrl Pts',(5.38854592421683,27.9485248236773,125.136139592967));
#95138=CARTESIAN_POINT('Ctrl Pts',(5.39240113046216,27.946273720216,125.06485314352));
#95139=CARTESIAN_POINT('Ctrl Pts',(5.3962564873134,27.944022528814,124.993563909226));
#95140=CARTESIAN_POINT('Ctrl Pts',(5.40011184416465,27.9454877668835,124.922163381991));
#95141=CARTESIAN_POINT('Ctrl Pts',(5.40396720101589,27.950654662112,124.851066294692));
#95142=CARTESIAN_POINT('Ctrl Pts',(5.40782659348445,27.9558269658184,124.779894786101));
#95143=CARTESIAN_POINT('Ctrl Pts',(5.411685985953,27.9647086262348,124.709027837004));
#95144=CARTESIAN_POINT('Ctrl Pts',(5.41554537842156,27.9772329265542,124.638875465963));
#95145=CARTESIAN_POINT('Ctrl Pts',(5.41940695602499,27.9897643179601,124.568683375614));
#95146=CARTESIAN_POINT('Ctrl Pts',(5.42326853362842,28.0059423446726,124.499207142076));
#95147=CARTESIAN_POINT('Ctrl Pts',(5.42713011123186,28.0256496404587,124.43084429171));
#95148=CARTESIAN_POINT('Ctrl Pts',(5.43099844534672,28.0453914176364,124.362361828474));
#95149=CARTESIAN_POINT('Ctrl Pts',(5.43486677946159,28.0686746338712,124.294997097049));
#95150=CARTESIAN_POINT('Ctrl Pts',(5.43873511357646,28.0953330110469,124.229129567507));
#95151=CARTESIAN_POINT('Ctrl Pts',(5.44103283274744,28.1111675957764,124.190005468895));
#95152=CARTESIAN_POINT('Ctrl Pts',(5.44333055191843,28.1281920767404,124.151409186527));
#95153=CARTESIAN_POINT('Ctrl Pts',(5.44562827108941,28.1463640450114,124.113415932427));
#95154=CARTESIAN_POINT('Ctrl Pts',(5.44949734443763,28.1769633797821,124.049440017222));
#95155=CARTESIAN_POINT('Ctrl Pts',(5.45336641778585,28.2109386112394,123.986924796112));
#95156=CARTESIAN_POINT('Ctrl Pts',(5.45723549113407,28.2481272957716,123.926249754049));
#95157=CARTESIAN_POINT('Ctrl Pts',(5.46109879952985,28.2852605688453,123.865665118319));
#95158=CARTESIAN_POINT('Ctrl Pts',(5.46496210792564,28.3255975390154,123.80691562988));
#95159=CARTESIAN_POINT('Ctrl Pts',(5.46882541632142,28.3689289141425,123.750358181166));
#95160=CARTESIAN_POINT('Ctrl Pts',(5.47268419281434,28.4122094588509,123.693867077883));
#95161=CARTESIAN_POINT('Ctrl Pts',(5.47654296930725,28.458477137248,123.639563290402));
#95162=CARTESIAN_POINT('Ctrl Pts',(5.48040174580017,28.5074791703107,123.58777511159));
#95163=CARTESIAN_POINT('Ctrl Pts',(5.48425809138837,28.5564503336734,123.536019557661));
#95164=CARTESIAN_POINT('Ctrl Pts',(5.48811443697657,28.6081521010899,123.486776820306));
#95165=CARTESIAN_POINT('Ctrl Pts',(5.49197078256478,28.6622921501115,123.440341296678));
#95166=CARTESIAN_POINT('Ctrl Pts',(5.49582598881011,28.7164162036583,123.393919492252));
#95167=CARTESIAN_POINT('Ctrl Pts',(5.49968119505544,28.7729767401191,123.350303571092));
#95168=CARTESIAN_POINT('Ctrl Pts',(5.50353640130078,28.8316466737578,123.309749111061));
#95169=CARTESIAN_POINT('Ctrl Pts',(5.50739175815202,28.8903188993721,123.269193066747));
#95170=CARTESIAN_POINT('Ctrl Pts',(5.51124711500327,28.9511002849052,123.231698995419));
#95171=CARTESIAN_POINT('Ctrl Pts',(5.51510247185452,29.0136343832301,123.197479422433));
#95172=CARTESIAN_POINT('Ctrl Pts',(5.51896186432308,29.0762339394879,123.163224029908));
#95173=CARTESIAN_POINT('Ctrl Pts',(5.52282125679164,29.1405894439089,123.132250211661));
#95174=CARTESIAN_POINT('Ctrl Pts',(5.5266806492602,29.2063202372392,123.104724295337));
#95175=CARTESIAN_POINT('Ctrl Pts',(5.53054222686364,29.2720882464397,123.077182794219));
#95176=CARTESIAN_POINT('Ctrl Pts',(5.53440380446707,29.3392326371753,123.053093245288));
#95177=CARTESIAN_POINT('Ctrl Pts',(5.53826538207051,29.4073557750043,123.032572648081));
#95178=CARTESIAN_POINT('Ctrl Pts',(5.54213371618538,29.4755981062841,123.012016146468));
#95179=CARTESIAN_POINT('Ctrl Pts',(5.54600205030026,29.5448221317373,122.995041179658));
#95180=CARTESIAN_POINT('Ctrl Pts',(5.54987038441513,29.6146188587507,122.981713861102));
#95181=CARTESIAN_POINT('Ctrl Pts',(5.55216810358608,29.6560768282449,122.973797679501));
#95182=CARTESIAN_POINT('Ctrl Pts',(5.55446582275702,29.6977367133038,122.967167450132));
#95183=CARTESIAN_POINT('Ctrl Pts',(5.55676354192797,29.739512323952,122.961828335707));
#95184=CARTESIAN_POINT('Ctrl Pts',(5.56063261527618,29.8098572572268,122.952837930967));
#95185=CARTESIAN_POINT('Ctrl Pts',(5.5645016886244,29.8808059628848,122.947475992101));
#95186=CARTESIAN_POINT('Ctrl Pts',(5.56837076197261,29.9519515155082,122.945811862161));
#95187=CARTESIAN_POINT('Ctrl Pts',(5.57223407036839,30.0229910606489,122.944150211789));
#95188=CARTESIAN_POINT('Ctrl Pts',(5.57609737876418,30.0942263888592,122.946175444879));
#95189=CARTESIAN_POINT('Ctrl Pts',(5.57996068715996,30.1652441467213,122.951905291625));
#95190=CARTESIAN_POINT('Ctrl Pts',(5.58381946365287,30.2361785963026,122.957628416901));
#95191=CARTESIAN_POINT('Ctrl Pts',(5.58767824014578,30.306895500634,122.967047484839));
#95192=CARTESIAN_POINT('Ctrl Pts',(5.59153701663869,30.3769819483138,122.980128179031));
#95193=CARTESIAN_POINT('Ctrl Pts',(5.5953933622269,30.4470242437925,122.993200632807));
#95194=CARTESIAN_POINT('Ctrl Pts',(5.5992497078151,30.516436394182,123.009930047454));
#95195=CARTESIAN_POINT('Ctrl Pts',(5.6031060534033,30.584812518415,123.03023050059));
#95196=CARTESIAN_POINT('Ctrl Pts',(5.60696125964862,30.6531684411778,123.050524956034));
#95197=CARTESIAN_POINT('Ctrl Pts',(5.61081646589394,30.7204884800164,123.074388217214));
#95198=CARTESIAN_POINT('Ctrl Pts',(5.61467167213927,30.7863805132784,123.101684101411));
#95199=CARTESIAN_POINT('Ctrl Pts',(5.61852702899051,30.8522751206518,123.128981051938));
#95200=CARTESIAN_POINT('Ctrl Pts',(5.62238238584174,30.9167411637344,123.159710703763));
#95201=CARTESIAN_POINT('Ctrl Pts',(5.62623774269298,30.9794067665987,123.193688856249));
#95202=CARTESIAN_POINT('Ctrl Pts',(5.63009713516154,31.042137965049,123.227702575564));
#95203=CARTESIAN_POINT('Ctrl Pts',(5.6339565276301,31.1030645332285,123.264971351448));
#95204=CARTESIAN_POINT('Ctrl Pts',(5.63781592009865,31.161840276128,123.305265585625));
#95205=CARTESIAN_POINT('Ctrl Pts',(5.64167749770208,31.2206492970438,123.345582633842));
#95206=CARTESIAN_POINT('Ctrl Pts',(5.6455390753055,31.2773046824779,123.388928255031));
#95207=CARTESIAN_POINT('Ctrl Pts',(5.64940065290893,31.3314924733828,123.435031835524));
#95208=CARTESIAN_POINT('Ctrl Pts',(5.6532689870238,31.3857750753901,123.481216082366));
#95209=CARTESIAN_POINT('Ctrl Pts',(5.65713732113867,31.4375811096654,123.530167589092));
#95210=CARTESIAN_POINT('Ctrl Pts',(5.66100565525355,31.4866332085155,123.581578600754));
#95211=CARTESIAN_POINT('Ctrl Pts',(5.66330337442454,31.5157692512043,123.612115794178));
#95212=CARTESIAN_POINT('Ctrl Pts',(5.66560109359554,31.5439344211598,123.64352007997));
#95213=CARTESIAN_POINT('Ctrl Pts',(5.66789881276654,31.5710776346151,123.675721846245));
#95214=CARTESIAN_POINT('Ctrl Pts',(5.67174314546748,31.6164911666133,123.729598884259));
#95215=CARTESIAN_POINT('Ctrl Pts',(5.67558747816843,31.6592258384196,123.785928448142));
#95216=CARTESIAN_POINT('Ctrl Pts',(5.67943181086938,31.6990035717014,123.844411653812));
#95217=CARTESIAN_POINT('Ctrl Pts',(5.68327073565044,31.7387253486413,123.90281258968));
#95218=CARTESIAN_POINT('Ctrl Pts',(5.6871096604315,31.7754981613695,123.963360756745));
#95219=CARTESIAN_POINT('Ctrl Pts',(5.69094858521257,31.8090834220943,124.02572348155));
#95220=CARTESIAN_POINT('Ctrl Pts',(5.69478343427781,31.8426330259657,124.088019996997));
#95221=CARTESIAN_POINT('Ctrl Pts',(5.69861828334306,31.8730015594205,124.152126817328));
#95222=CARTESIAN_POINT('Ctrl Pts',(5.70245313240831,31.8999941282689,124.217683008593));
#95223=CARTESIAN_POINT('Ctrl Pts',(5.70628582152479,31.9269714937638,124.283202275846));
#95224=CARTESIAN_POINT('Ctrl Pts',(5.71011851064127,31.9505764742472,124.350168842788));
#95225=CARTESIAN_POINT('Ctrl Pts',(5.71395119975776,31.970661212502,124.418199391509));
#95226=CARTESIAN_POINT('Ctrl Pts',(5.71778249936704,31.9907386692143,124.486205276363));
#95227=CARTESIAN_POINT('Ctrl Pts',(5.72161379897631,32.0072982815489,124.555273904177));
#95228=CARTESIAN_POINT('Ctrl Pts',(5.72544509858559,32.0202418689665,124.625006195551));
#95229=CARTESIAN_POINT('Ctrl Pts',(5.72927810286533,32.0331912154092,124.694769513102));
#95230=CARTESIAN_POINT('Ctrl Pts',(5.73311110714508,32.0425212306723,124.765196599798));
#95231=CARTESIAN_POINT('Ctrl Pts',(5.73694411142483,32.048185000157,124.835878802003));
#95232=CARTESIAN_POINT('Ctrl Pts',(5.73993783446244,32.0526086208859,124.891084307044));
#95233=CARTESIAN_POINT('Ctrl Pts',(5.74293155750006,32.0547967824529,124.946445182454));
#95234=CARTESIAN_POINT('Ctrl Pts',(5.74592528053768,32.0547492412566,125.001765801585));
#95235=CARTESIAN_POINT('Origin',(-1.54592528053767,30.,125.));
#95236=CARTESIAN_POINT('',(4.59397334930969,28.7479590808042,126.629230216746));
#95237=CARTESIAN_POINT('',(4.65201706778823,28.7479590808042,126.629230216746));
#95238=CARTESIAN_POINT('',(-1.54592528053767,28.7479590808042,126.629230216746));
#95239=CARTESIAN_POINT('',(5.10407471942417,32.0547498925786,125.000664415722));
#95240=CARTESIAN_POINT('Ctrl Pts',(4.65201706778823,28.7479590808042,126.629230216746));
#95241=CARTESIAN_POINT('Ctrl Pts',(4.65588621633621,28.6915030279502,126.58584451988));
#95242=CARTESIAN_POINT('Ctrl Pts',(4.6597553648842,28.6373884230477,126.53958531662));
#95243=CARTESIAN_POINT('Ctrl Pts',(4.66362451343219,28.5859041009941,126.490748252025));
#95244=CARTESIAN_POINT('Ctrl Pts',(4.66425200887117,28.5775544145276,126.482827895671));
#95245=CARTESIAN_POINT('Ctrl Pts',(4.66487950431016,28.5692738251231,126.474839808126));
#95246=CARTESIAN_POINT('Ctrl Pts',(4.66550699974915,28.5610634645336,126.466785331737));
#95247=CARTESIAN_POINT('Ctrl Pts',(4.66937607309736,28.5104392123683,126.417122245773));
#95248=CARTESIAN_POINT('Ctrl Pts',(4.67324514644557,28.4622899074249,126.364737957514));
#95249=CARTESIAN_POINT('Ctrl Pts',(4.67711421979379,28.4169220079585,126.309909017304));
#95250=CARTESIAN_POINT('Ctrl Pts',(4.68097752818957,28.3716217070509,126.255161772684));
#95251=CARTESIAN_POINT('Ctrl Pts',(4.68484083658536,28.3290948924323,126.197977477701));
#95252=CARTESIAN_POINT('Ctrl Pts',(4.68870414498114,28.2896114797321,126.138669694089));
#95253=CARTESIAN_POINT('Ctrl Pts',(4.69256292147405,28.2501743835496,126.079431482223));
#95254=CARTESIAN_POINT('Ctrl Pts',(4.69642169796697,28.2137738657557,126.018075132076));
#95255=CARTESIAN_POINT('Ctrl Pts',(4.70028047445988,28.1806387041184,125.954946091436));
#95256=CARTESIAN_POINT('Ctrl Pts',(4.70413682004808,28.147524416564,125.891856820054));
#95257=CARTESIAN_POINT('Ctrl Pts',(4.70799316563629,28.1176716292101,125.826997502888));
#95258=CARTESIAN_POINT('Ctrl Pts',(4.7118495112245,28.0912642476934,125.760740028108));
#95259=CARTESIAN_POINT('Ctrl Pts',(4.71570471746983,28.0648646681387,125.694502128852));
#95260=CARTESIAN_POINT('Ctrl Pts',(4.71955992371516,28.0419086533008,125.626867343082));
#95261=CARTESIAN_POINT('Ctrl Pts',(4.72341512996049,28.0225321258002,125.558227882686));
#95262=CARTESIAN_POINT('Ctrl Pts',(4.72727048681174,28.0031548413441,125.489585740848));
#95263=CARTESIAN_POINT('Ctrl Pts',(4.73112584366298,27.9873574517059,125.419939314574));
#95264=CARTESIAN_POINT('Ctrl Pts',(4.73498120051423,27.9752256400638,125.349694658016));
#95265=CARTESIAN_POINT('Ctrl Pts',(4.73884059298279,27.963081129377,125.279376472453));
#95266=CARTESIAN_POINT('Ctrl Pts',(4.74269998545134,27.9546099389754,125.208459286248));
#95267=CARTESIAN_POINT('Ctrl Pts',(4.7465593779199,27.9498462038099,125.137357105631));
#95268=CARTESIAN_POINT('Ctrl Pts',(4.75042095552334,27.9450797714831,125.066214667938));
#95269=CARTESIAN_POINT('Ctrl Pts',(4.75428253312677,27.9440249802595,124.994887513288));
#95270=CARTESIAN_POINT('Ctrl Pts',(4.75814411073021,27.9466637979444,124.923789739352));
#95271=CARTESIAN_POINT('Ctrl Pts',(4.76201244484508,27.9493072327066,124.852567567315));
#95272=CARTESIAN_POINT('Ctrl Pts',(4.76588077895995,27.9556571358942,124.78157606129));
#95273=CARTESIAN_POINT('Ctrl Pts',(4.76974911307482,27.9656436525551,124.711223591492));
#95274=CARTESIAN_POINT('Ctrl Pts',(4.77204683224578,27.9715754594005,124.669435521026));
#95275=CARTESIAN_POINT('Ctrl Pts',(4.77434455141674,27.9787893326922,124.627872725201));
#95276=CARTESIAN_POINT('Ctrl Pts',(4.7766422705877,27.9872622538326,124.586618423665));
#95277=CARTESIAN_POINT('Ctrl Pts',(4.78051134393592,28.0015295993726,124.517151310107));
#95278=CARTESIAN_POINT('Ctrl Pts',(4.78438041728413,28.0194254679784,124.448287625122));
#95279=CARTESIAN_POINT('Ctrl Pts',(4.78824949063234,28.0408837296111,124.380434828612));
#95280=CARTESIAN_POINT('Ctrl Pts',(4.79211279902813,28.0623100182503,124.312683133349));
#95281=CARTESIAN_POINT('Ctrl Pts',(4.79597610742391,28.0872880184085,124.245939796136));
#95282=CARTESIAN_POINT('Ctrl Pts',(4.79983941581969,28.1157006857585,124.180601649471));
#95283=CARTESIAN_POINT('Ctrl Pts',(4.8036981923126,28.1440800232691,124.115340148548));
#95284=CARTESIAN_POINT('Ctrl Pts',(4.80755696880551,28.1758858320734,124.051481007265));
#95285=CARTESIAN_POINT('Ctrl Pts',(4.81141574529843,28.2109519672824,123.989403790266));
#95286=CARTESIAN_POINT('Ctrl Pts',(4.81527209088663,28.2459960119574,123.92736567991));
#95287=CARTESIAN_POINT('Ctrl Pts',(4.81912843647484,28.2842960697706,123.867107688676));
#95288=CARTESIAN_POINT('Ctrl Pts',(4.82298478206304,28.3256394450813,123.808986022487));
#95289=CARTESIAN_POINT('Ctrl Pts',(4.82683998830837,28.3669706056465,123.750881528126));
#95290=CARTESIAN_POINT('Ctrl Pts',(4.8306951945537,28.4113430172466,123.694912501404));
#95291=CARTESIAN_POINT('Ctrl Pts',(4.83455040079903,28.4585008851387,123.641405858477));
#95292=CARTESIAN_POINT('Ctrl Pts',(4.83840575765028,28.5056605952808,123.58789712528));
#95293=CARTESIAN_POINT('Ctrl Pts',(4.84226111450152,28.5556056549012,123.536851329845));
#95294=CARTESIAN_POINT('Ctrl Pts',(4.84611647135276,28.608041391699,123.488560687531));
#95295=CARTESIAN_POINT('Ctrl Pts',(4.84997586382132,28.6605320159108,123.440219496705));
#95296=CARTESIAN_POINT('Ctrl Pts',(4.85383525628988,28.7155181636508,123.394639545818));
#95297=CARTESIAN_POINT('Ctrl Pts',(4.85769464875844,28.772670523823,123.352074055242));
#95298=CARTESIAN_POINT('Ctrl Pts',(4.86155622636187,28.8298552428746,123.309484464671));
#95299=CARTESIAN_POINT('Ctrl Pts',(4.8654178039653,28.8892082115199,123.26991300162));
#95300=CARTESIAN_POINT('Ctrl Pts',(4.86927938156873,28.9503717482536,123.233569108163));
#95301=CARTESIAN_POINT('Ctrl Pts',(4.8731477156836,29.0116423013879,123.197161624651));
#95302=CARTESIAN_POINT('Ctrl Pts',(4.87701604979848,29.074729317315,123.163993211672));
#95303=CARTESIAN_POINT('Ctrl Pts',(4.88088438391335,29.1392518196133,123.134226666376));
#95304=CARTESIAN_POINT('Ctrl Pts',(4.88318210308432,29.177576996831,123.116545887067));
#95305=CARTESIAN_POINT('Ctrl Pts',(4.88547982225529,29.2164082578054,123.100064408499));
#95306=CARTESIAN_POINT('Ctrl Pts',(4.88777754142626,29.2556632016255,123.084808027093));
#95307=CARTESIAN_POINT('Ctrl Pts',(4.89164661477448,29.3217636454217,123.059118178033));
#95308=CARTESIAN_POINT('Ctrl Pts',(4.8955156881227,29.389325103184,123.036804087238));
#95309=CARTESIAN_POINT('Ctrl Pts',(4.89938476147091,29.4579693835414,123.018031187601));
#95310=CARTESIAN_POINT('Ctrl Pts',(4.9032480698667,29.5265113833331,122.999286259746));
#95311=CARTESIAN_POINT('Ctrl Pts',(4.90711137826249,29.5961325383754,122.984072176635));
#95312=CARTESIAN_POINT('Ctrl Pts',(4.91097468665828,29.6664359717598,122.972505831928));
#95313=CARTESIAN_POINT('Ctrl Pts',(4.9148334631512,29.7366569348108,122.960953055269));
#95314=CARTESIAN_POINT('Ctrl Pts',(4.91869223964411,29.807558109412,122.953039595899));
#95315=CARTESIAN_POINT('Ctrl Pts',(4.92255101613703,29.8787304957541,122.948831730491));
#95316=CARTESIAN_POINT('Ctrl Pts',(4.92640736172524,29.9498580457888,122.944626515902));
#95317=CARTESIAN_POINT('Ctrl Pts',(4.93026370731345,30.0212559847986,122.944122292457));
#95318=CARTESIAN_POINT('Ctrl Pts',(4.93412005290166,30.0925096901938,122.947333558583));
#95319=CARTESIAN_POINT('Ctrl Pts',(4.93797525914699,30.1637423439484,122.950543875952));
#95320=CARTESIAN_POINT('Ctrl Pts',(4.94183046539232,30.2348303636584,122.957467481741));
#95321=CARTESIAN_POINT('Ctrl Pts',(4.94568567163766,30.3053603589397,122.968066779225));
#95322=CARTESIAN_POINT('Ctrl Pts',(4.94954102848891,30.3758931095171,122.978666490777));
#95323=CARTESIAN_POINT('Ctrl Pts',(4.95339638534016,30.4458673123213,122.992942104738));
#95324=CARTESIAN_POINT('Ctrl Pts',(4.95725174219141,30.5148776448284,123.010804541189));
#95325=CARTESIAN_POINT('Ctrl Pts',(4.96111113465997,30.5839602143043,123.028685675249));
#95326=CARTESIAN_POINT('Ctrl Pts',(4.96497052712853,30.6520764281672,123.050161004701));
#95327=CARTESIAN_POINT('Ctrl Pts',(4.96882991959709,30.7188349384432,123.075091198583));
#95328=CARTESIAN_POINT('Ctrl Pts',(4.97269149720053,30.7856312464686,123.100035507598));
#95329=CARTESIAN_POINT('Ctrl Pts',(4.97655307480396,30.8510678748066,123.128438381514));
#95330=CARTESIAN_POINT('Ctrl Pts',(4.9804146524074,30.9147748684468,123.160112910378));
#95331=CARTESIAN_POINT('Ctrl Pts',(4.98428298652227,30.9785933287141,123.191842859419));
#95332=CARTESIAN_POINT('Ctrl Pts',(4.98815132063715,31.0406756889188,123.226855653503));
#95333=CARTESIAN_POINT('Ctrl Pts',(4.99201965475202,31.1006785481559,123.264919513069));
#95334=CARTESIAN_POINT('Ctrl Pts',(4.99431737392296,31.1363191406915,123.287528744135));
#95335=CARTESIAN_POINT('Ctrl Pts',(4.99661509309389,31.1712266300885,123.311213615859));
#95336=CARTESIAN_POINT('Ctrl Pts',(4.99891281226483,31.2053346523551,123.335918890699));
#95337=CARTESIAN_POINT('Ctrl Pts',(5.00275064676246,31.2623046015798,123.377183618458));
#95338=CARTESIAN_POINT('Ctrl Pts',(5.00658848126009,31.3172734889279,123.421464682555));
#95339=CARTESIAN_POINT('Ctrl Pts',(5.01042631575773,31.3699002709867,123.468539647901));
#95340=CARTESIAN_POINT('Ctrl Pts',(5.01432833257716,31.4234071611021,123.516401875068));
#95341=CARTESIAN_POINT('Ctrl Pts',(5.0182303493966,31.4744924192991,123.567152086287));
#95342=CARTESIAN_POINT('Ctrl Pts',(5.02213236621603,31.5228283369254,123.620510449928));
#95343=CARTESIAN_POINT('Ctrl Pts',(5.02595997436975,31.5702425232257,123.672851307796));
#95344=CARTESIAN_POINT('Ctrl Pts',(5.02978758252347,31.615010950279,123.727701341682));
#95345=CARTESIAN_POINT('Ctrl Pts',(5.03361519067718,31.656859368321,123.784757392079));
#95346=CARTESIAN_POINT('Ctrl Pts',(5.03744050268938,31.6986826819409,123.841779215157));
#95347=CARTESIAN_POINT('Ctrl Pts',(5.04126581470157,31.7375891686524,123.901004032373));
#95348=CARTESIAN_POINT('Ctrl Pts',(5.04509112671377,31.7733450235495,123.962095866685));
#95349=CARTESIAN_POINT('Ctrl Pts',(5.04891547573736,31.8090918772252,124.023172321666));
#95350=CARTESIAN_POINT('Ctrl Pts',(5.05273982476096,31.8416894240058,124.086114434042));
#95351=CARTESIAN_POINT('Ctrl Pts',(5.05656417378455,31.8709483479536,124.150559100473));
#95352=CARTESIAN_POINT('Ctrl Pts',(5.06052338592119,31.9012390683048,124.217276365006));
#95353=CARTESIAN_POINT('Ctrl Pts',(5.06448259805782,31.9279510192918,124.285603645033));
#95354=CARTESIAN_POINT('Ctrl Pts',(5.06844181019445,31.9509280911051,124.355114625816));
#95355=CARTESIAN_POINT('Ctrl Pts',(5.07227054686677,31.9731479556736,124.422334878751));
#95356=CARTESIAN_POINT('Ctrl Pts',(5.07609928353909,31.9918752129522,124.490661515233));
#95357=CARTESIAN_POINT('Ctrl Pts',(5.07992802021141,32.0070199603934,124.559695058985));
#95358=CARTESIAN_POINT('Ctrl Pts',(5.08395247008021,32.0229388605606,124.632257384334));
#95359=CARTESIAN_POINT('Ctrl Pts',(5.087976919949,32.0348990846249,124.70560020682));
#95360=CARTESIAN_POINT('Ctrl Pts',(5.09200136981779,32.0428577974624,124.779252221195));
#95361=CARTESIAN_POINT('Ctrl Pts',(5.09602581968658,32.0508165102998,124.85290423557));
#95362=CARTESIAN_POINT('Ctrl Pts',(5.10005026955538,32.0547737561236,124.92686481261));
#95363=CARTESIAN_POINT('Ctrl Pts',(5.10407471942417,32.0547498925786,125.000664415722));
#95364=CARTESIAN_POINT('Ctrl Pts',(5.10407471946233,32.0547498925784,125.000664416421));
#95365=CARTESIAN_POINT('Ctrl Pts',(5.10606584067601,32.0547380859309,125.037177221924));
#95366=CARTESIAN_POINT('Ctrl Pts',(5.1080569618897,32.0537530962652,125.073673053094));
#95367=CARTESIAN_POINT('Ctrl Pts',(5.11004808310338,32.0517972511101,125.110116315035));
#95368=CARTESIAN_POINT('Ctrl Pts',(5.11391715645159,32.0479967248987,125.180931518313));
#95369=CARTESIAN_POINT('Ctrl Pts',(5.1177862297998,32.0405183040001,125.251688443372));
#95370=CARTESIAN_POINT('Ctrl Pts',(5.12165530314801,32.0293669196201,125.321974328249));
#95371=CARTESIAN_POINT('Ctrl Pts',(5.12551861154379,32.0182321508984,125.392155486556));
#95372=CARTESIAN_POINT('Ctrl Pts',(5.12938191993958,32.0034353574457,125.461866521965));
#95373=CARTESIAN_POINT('Ctrl Pts',(5.13324522833536,31.985033398107,125.53069762662));
#95374=CARTESIAN_POINT('Ctrl Pts',(5.13710400482826,31.9666530254199,125.599447988075));
#95375=CARTESIAN_POINT('Ctrl Pts',(5.14096278132117,31.9446760121003,125.667320002076));
#95376=CARTESIAN_POINT('Ctrl Pts',(5.14482155781407,31.9192103364247,125.733913650957));
#95377=CARTESIAN_POINT('Ctrl Pts',(5.14867790340227,31.8937607033032,125.800465347987));
#95378=CARTESIAN_POINT('Ctrl Pts',(5.15253424899047,31.864826941218,125.865739824988));
#95379=CARTESIAN_POINT('Ctrl Pts',(5.15639059457868,31.8325665301762,125.929353256291));
#95380=CARTESIAN_POINT('Ctrl Pts',(5.160245800824,31.8003156503523,125.992947893243));
#95381=CARTESIAN_POINT('Ctrl Pts',(5.16410100706933,31.764740292392,126.05488202575));
#95382=CARTESIAN_POINT('Ctrl Pts',(5.16795621331465,31.7260449047639,126.114794397743));
#95383=CARTESIAN_POINT('Ctrl Pts',(5.17181157016589,31.6873480054775,126.174709110248));
#95384=CARTESIAN_POINT('Ctrl Pts',(5.17566692701713,31.6455310999461,126.232601498554));
#95385=CARTESIAN_POINT('Ctrl Pts',(5.17952228386837,31.6008422332886,126.288138853781));
#95386=CARTESIAN_POINT('Ctrl Pts',(5.18338167633693,31.5561065882988,126.343734343058));
#95387=CARTESIAN_POINT('Ctrl Pts',(5.18724106880548,31.5084932862153,126.396969499024));
#95388=CARTESIAN_POINT('Ctrl Pts',(5.19110046127403,31.4582904142315,126.447545035659));
#95389=CARTESIAN_POINT('Ctrl Pts',(5.19496203887746,31.4080591180729,126.498149207466));
#95390=CARTESIAN_POINT('Ctrl Pts',(5.19882361648089,31.3552356931987,126.546090435647));
#95391=CARTESIAN_POINT('Ctrl Pts',(5.20268519408432,31.3001427797347,126.591108517608));
#95392=CARTESIAN_POINT('Ctrl Pts',(5.20655352819918,31.244953471497,126.636205366647));
#95393=CARTESIAN_POINT('Ctrl Pts',(5.21042186231405,31.1874871385065,126.678368570637));
#95394=CARTESIAN_POINT('Ctrl Pts',(5.21429019642891,31.1280963799313,126.717380598495));
#95395=CARTESIAN_POINT('Ctrl Pts',(5.21658791559992,31.0928193639066,126.740553024052));
#95396=CARTESIAN_POINT('Ctrl Pts',(5.21888563477093,31.0568638927513,126.762614530318));
#95397=CARTESIAN_POINT('Ctrl Pts',(5.22118335394194,31.0203076268374,126.783527378292));
#95398=CARTESIAN_POINT('Ctrl Pts',(5.22505242729016,30.958751421039,126.818742013638));
#95399=CARTESIAN_POINT('Ctrl Pts',(5.22892150063837,30.8952494193226,126.85083508144));
#95400=CARTESIAN_POINT('Ctrl Pts',(5.23279057398659,30.8301510755014,126.879586857356));
#95401=CARTESIAN_POINT('Ctrl Pts',(5.23665388238237,30.7651497287701,126.908295792879));
#95402=CARTESIAN_POINT('Ctrl Pts',(5.24051719077816,30.6985572020688,126.933673124138));
#95403=CARTESIAN_POINT('Ctrl Pts',(5.24438049917394,30.6307486310241,126.955544355662));
#95404=CARTESIAN_POINT('Ctrl Pts',(5.24823927566686,30.563019603683,126.977389930861));
#95405=CARTESIAN_POINT('Ctrl Pts',(5.25209805215977,30.4940778255901,126.995737427486));
#95406=CARTESIAN_POINT('Ctrl Pts',(5.25595682865268,30.4243179325502,127.010460607576));
#95407=CARTESIAN_POINT('Ctrl Pts',(5.25981317424089,30.3546019859924,127.025174512538));
#95408=CARTESIAN_POINT('Ctrl Pts',(5.26366951982909,30.2840694211964,127.036268530721));
#95409=CARTESIAN_POINT('Ctrl Pts',(5.2675258654173,30.2131281183253,127.04366679468));
#95410=CARTESIAN_POINT('Ctrl Pts',(5.27138107166263,30.1422077747966,127.051062872851));
#95411=CARTESIAN_POINT('Ctrl Pts',(5.27523627790796,30.0708794158375,127.054765314154));
#95412=CARTESIAN_POINT('Ctrl Pts',(5.2790914841533,29.9995574339136,127.054749952339));
#95413=CARTESIAN_POINT('Ctrl Pts',(5.28294684100454,29.9282326657543,127.054734589923));
#95414=CARTESIAN_POINT('Ctrl Pts',(5.28680219785578,29.8569147609102,127.051001138343));
#95415=CARTESIAN_POINT('Ctrl Pts',(5.29065755470703,29.7860177733689,127.04357754176));
#95416=CARTESIAN_POINT('Ctrl Pts',(5.29451694717559,29.7150465739914,127.036146174484));
#95417=CARTESIAN_POINT('Ctrl Pts',(5.29837633964415,29.6444976555832,127.02501700212));
#95418=CARTESIAN_POINT('Ctrl Pts',(5.30223573211271,29.5747787095142,127.010269737278));
#95419=CARTESIAN_POINT('Ctrl Pts',(5.30609730971614,29.5050202895379,126.995514122739));
#95420=CARTESIAN_POINT('Ctrl Pts',(5.30995888731958,29.4360932469752,126.977136462971));
#95421=CARTESIAN_POINT('Ctrl Pts',(5.31382046492301,29.3683911777763,126.955266697458));
#95422=CARTESIAN_POINT('Ctrl Pts',(5.31768879903788,29.3005706518605,126.933358666931));
#95423=CARTESIAN_POINT('Ctrl Pts',(5.32155713315276,29.2339798324881,126.907946505012));
#95424=CARTESIAN_POINT('Ctrl Pts',(5.32542546726763,29.1689927141232,126.879208464572));
#95425=CARTESIAN_POINT('Ctrl Pts',(5.32772318643859,29.130391563525,126.862138598192));
#95426=CARTESIAN_POINT('Ctrl Pts',(5.33002090560955,29.0923557749172,126.843896209379));
#95427=CARTESIAN_POINT('Ctrl Pts',(5.33231862478051,29.0549591746737,126.824526075716));
#95428=CARTESIAN_POINT('Ctrl Pts',(5.33618678852251,28.9920027546881,126.791916847547));
#95429=CARTESIAN_POINT('Ctrl Pts',(5.34005495226452,28.9306128321502,126.755981411748));
#95430=CARTESIAN_POINT('Ctrl Pts',(5.34392311600652,28.8711632767676,126.716894060442));
#95431=CARTESIAN_POINT('Ctrl Pts',(5.34666123635929,28.8290812842738,126.689225668077));
#95432=CARTESIAN_POINT('Ctrl Pts',(5.34939935671205,28.7879712291961,126.659979000151));
#95433=CARTESIAN_POINT('Ctrl Pts',(5.35213747706482,28.7479590808042,126.629230216746));
#95434=CARTESIAN_POINT('',(5.04592528049233,32.0547497417017,124.998969719981));
#95435=CARTESIAN_POINT('Ctrl Pts',(5.04592528053768,32.0547497417021,124.998969720821));
#95436=CARTESIAN_POINT('Ctrl Pts',(5.04983580638861,32.0547860725486,125.071426584005));
#95437=CARTESIAN_POINT('Ctrl Pts',(5.05374633223954,32.0509854787254,125.143878332678));
#95438=CARTESIAN_POINT('Ctrl Pts',(5.05765685809047,32.0433759542004,125.215898754734));
#95439=CARTESIAN_POINT('Ctrl Pts',(5.06156889758468,32.0357634842644,125.287947053662));
#95440=CARTESIAN_POINT('Ctrl Pts',(5.06548093707889,32.0243392038325,125.359563230797));
#95441=CARTESIAN_POINT('Ctrl Pts',(5.0693929765731,32.0091827682208,125.430327975368));
#95442=CARTESIAN_POINT('Ctrl Pts',(5.07331083119333,31.9940038030351,125.501197909549));
#95443=CARTESIAN_POINT('Ctrl Pts',(5.07722868581356,31.9750817055283,125.571213427758));
#95444=CARTESIAN_POINT('Ctrl Pts',(5.08114654043379,31.9525468000694,125.639967621086));
#95445=CARTESIAN_POINT('Ctrl Pts',(5.0850675173693,31.9299939355267,125.708776607735));
#95446=CARTESIAN_POINT('Ctrl Pts',(5.08898849430482,31.9038226982916,125.776321833249));
#95447=CARTESIAN_POINT('Ctrl Pts',(5.09290947124033,31.8742116465834,125.842216282383));
#95448=CARTESIAN_POINT('Ctrl Pts',(5.09683849198294,31.8445398483848,125.908245912684));
#95449=CARTESIAN_POINT('Ctrl Pts',(5.10076751272554,31.8114143545465,125.972617587759));
#95450=CARTESIAN_POINT('Ctrl Pts',(5.10469653346815,31.7750596081158,126.034969057574));
#95451=CARTESIAN_POINT('Ctrl Pts',(5.10720517517001,31.7518474545204,126.07477986734));
#95452=CARTESIAN_POINT('Ctrl Pts',(5.10971381687188,31.7273197264878,126.113767668479));
#95453=CARTESIAN_POINT('Ctrl Pts',(5.11222245857374,31.7015435920206,126.151845027316));
#95454=CARTESIAN_POINT('Ctrl Pts',(5.11609153192196,31.661789108623,126.210571665775));
#95455=CARTESIAN_POINT('Ctrl Pts',(5.11996060527018,31.6189128733263,126.267352804102));
#95456=CARTESIAN_POINT('Ctrl Pts',(5.12382967861839,31.5731318462583,126.321837265622));
#95457=CARTESIAN_POINT('Ctrl Pts',(5.12769298701418,31.5274190333129,126.376240544828));
#95458=CARTESIAN_POINT('Ctrl Pts',(5.13155629540996,31.4788103298453,126.428353571045));
#95459=CARTESIAN_POINT('Ctrl Pts',(5.13541960380575,31.4275656730796,126.477854462234));
#95460=CARTESIAN_POINT('Ctrl Pts',(5.13927838029866,31.3763811295078,126.527297285775));
#95461=CARTESIAN_POINT('Ctrl Pts',(5.14313715679157,31.3225671223705,126.574133724953));
#95462=CARTESIAN_POINT('Ctrl Pts',(5.14699593328449,31.2664223501252,126.618076634033));
#95463=CARTESIAN_POINT('Ctrl Pts',(5.15085227887269,31.2103129472752,126.661991860498));
#95464=CARTESIAN_POINT('Ctrl Pts',(5.1547086244609,31.151876074057,126.703016874631));
#95465=CARTESIAN_POINT('Ctrl Pts',(5.15856497004911,31.0914445044241,126.740903919308));
#95466=CARTESIAN_POINT('Ctrl Pts',(5.16242017629444,31.0310307890723,126.7787797704));
#95467=CARTESIAN_POINT('Ctrl Pts',(5.16627538253977,30.9686239586422,126.813519234689));
#95468=CARTESIAN_POINT('Ctrl Pts',(5.1701305887851,30.9045854047206,126.844918103349));
#95469=CARTESIAN_POINT('Ctrl Pts',(5.17398594563635,30.840544349095,126.876318198626));
#95470=CARTESIAN_POINT('Ctrl Pts',(5.17784130248759,30.7748718805691,126.904377227293));
#95471=CARTESIAN_POINT('Ctrl Pts',(5.18169665933884,30.7079520380723,126.928937913539));
#95472=CARTESIAN_POINT('Ctrl Pts',(5.1855560518074,30.6409621468395,126.953524308827));
#95473=CARTESIAN_POINT('Ctrl Pts',(5.18941544427596,30.5727227321491,126.974604883981));
#95474=CARTESIAN_POINT('Ctrl Pts',(5.19327483674452,30.5036349212805,126.992071642428));
#95475=CARTESIAN_POINT('Ctrl Pts',(5.19713641434795,30.4345079938446,127.009548290314));
#95476=CARTESIAN_POINT('Ctrl Pts',(5.20099799195139,30.3645321907575,127.023406953932));
#95477=CARTESIAN_POINT('Ctrl Pts',(5.20485956955482,30.2941181062911,127.033590937738));
#95478=CARTESIAN_POINT('Ctrl Pts',(5.2087279036697,30.2235808199586,127.043792740222));
#95479=CARTESIAN_POINT('Ctrl Pts',(5.21259623778457,30.1526042051138,127.050306981796));
#95480=CARTESIAN_POINT('Ctrl Pts',(5.21646457189944,30.0816025369967,127.053128975115));
#95481=CARTESIAN_POINT('Ctrl Pts',(5.21876229107039,30.0394288546939,127.054805187137));
#95482=CARTESIAN_POINT('Ctrl Pts',(5.22106001024135,29.9972463264548,127.055179721477));
#95483=CARTESIAN_POINT('Ctrl Pts',(5.2233577294123,29.9551409540642,127.054260263087));
#95484=CARTESIAN_POINT('Ctrl Pts',(5.22722618552694,29.8842520537394,127.052712256491));
#95485=CARTESIAN_POINT('Ctrl Pts',(5.23109464164159,29.8133045455,127.047487535505));
#95486=CARTESIAN_POINT('Ctrl Pts',(5.23496309775624,29.7427109417857,127.038577911934));
#95487=CARTESIAN_POINT('Ctrl Pts',(5.23882613528347,29.6722162192791,127.029680768166));
#95488=CARTESIAN_POINT('Ctrl Pts',(5.24268917281071,29.6020748954899,127.017109022759));
#95489=CARTESIAN_POINT('Ctrl Pts',(5.24655221033795,29.5326982922555,127.000906463691));
#95490=CARTESIAN_POINT('Ctrl Pts',(5.25049621383355,29.46186761465,126.984364312817));
#95491=CARTESIAN_POINT('Ctrl Pts',(5.25444021732915,29.3918345959394,126.964037416345));
#95492=CARTESIAN_POINT('Ctrl Pts',(5.25838422082475,29.3230296683319,126.940028023648));
#95493=CARTESIAN_POINT('Ctrl Pts',(5.26224043487251,29.2557562674104,126.916553055257));
#95494=CARTESIAN_POINT('Ctrl Pts',(5.26609664892028,29.1896573266088,126.889558019786));
#95495=CARTESIAN_POINT('Ctrl Pts',(5.26995286296804,29.1251210615865,126.859189179621));
#95496=CARTESIAN_POINT('Ctrl Pts',(5.27394076118756,29.0583809757952,126.827783287178));
#95497=CARTESIAN_POINT('Ctrl Pts',(5.27792865940708,28.9933127468431,126.792769154415));
#95498=CARTESIAN_POINT('Ctrl Pts',(5.2819165576266,28.9303221637766,126.754362245716));
#95499=CARTESIAN_POINT('Ctrl Pts',(5.28590445584612,28.8673315807101,126.715955337016));
#95500=CARTESIAN_POINT('Ctrl Pts',(5.28989235406564,28.8064191309432,126.674155957848));
#95501=CARTESIAN_POINT('Ctrl Pts',(5.29388025228516,28.7479590808042,126.629230216746));
#95502=CARTESIAN_POINT('Ctrl Pts',(4.59397334930969,28.7479590808042,126.629230216746));
#95503=CARTESIAN_POINT('Ctrl Pts',(4.59782931953988,28.6914508880382,126.585804451078));
#95504=CARTESIAN_POINT('Ctrl Pts',(4.60168528977007,28.6371690268486,126.539408000481));
#95505=CARTESIAN_POINT('Ctrl Pts',(4.60554126000026,28.5854350349871,126.490303164547));
#95506=CARTESIAN_POINT('Ctrl Pts',(4.60939638682258,28.5337123587876,126.441209069205));
#95507=CARTESIAN_POINT('Ctrl Pts',(4.6132515136449,28.4845367973786,126.389408099351));
#95508=CARTESIAN_POINT('Ctrl Pts',(4.61710664046723,28.4381945849889,126.335200886811));
#95509=CARTESIAN_POINT('Ctrl Pts',(4.62096221364327,28.391847007012,126.280987398061));
#95510=CARTESIAN_POINT('Ctrl Pts',(4.62481778681932,28.3483337430163,126.224367484424));
#95511=CARTESIAN_POINT('Ctrl Pts',(4.62867335999537,28.3079009955974,126.165675135619));
#95512=CARTESIAN_POINT('Ctrl Pts',(4.6325331508483,28.2674240181103,126.106918582258));
#95513=CARTESIAN_POINT('Ctrl Pts',(4.63639294170124,28.2300345569746,126.046085471014));
#95514=CARTESIAN_POINT('Ctrl Pts',(4.64025273255417,28.1959351466428,125.983538289738));
#95515=CARTESIAN_POINT('Ctrl Pts',(4.64411497429854,28.1618140838547,125.92095139223));
#95516=CARTESIAN_POINT('Ctrl Pts',(4.6479772160429,28.1309874387423,125.856648696817));
#95517=CARTESIAN_POINT('Ctrl Pts',(4.65183945778726,28.103610290807,125.791014306677));
#95518=CARTESIAN_POINT('Ctrl Pts',(4.65570819068367,28.0761871309332,125.725269606815));
#95519=CARTESIAN_POINT('Ctrl Pts',(4.65957692358008,28.0522251990167,125.658189203244));
#95520=CARTESIAN_POINT('Ctrl Pts',(4.66344565647649,28.0318299997003,125.590173205441));
#95521=CARTESIAN_POINT('Ctrl Pts',(4.66485756272416,28.0243867075143,125.565350552957));
#95522=CARTESIAN_POINT('Ctrl Pts',(4.66626946897183,28.017417978701,125.540403387799));
#95523=CARTESIAN_POINT('Ctrl Pts',(4.6676813752195,28.0109272352027,125.515351432366));
#95524=CARTESIAN_POINT('Ctrl Pts',(4.67155044856771,27.9931405282447,125.446701085896));
#95525=CARTESIAN_POINT('Ctrl Pts',(4.67541952191593,27.9788772247288,125.376994361717));
#95526=CARTESIAN_POINT('Ctrl Pts',(4.67928859526414,27.9682574135064,125.306626197068));
#95527=CARTESIAN_POINT('Ctrl Pts',(4.68315190365993,27.9576534258936,125.236362881586));
#95528=CARTESIAN_POINT('Ctrl Pts',(4.68701521205572,27.9506822263921,125.16544055836));
#95529=CARTESIAN_POINT('Ctrl Pts',(4.69087852045151,27.9474135131066,125.094267047915));
#95530=CARTESIAN_POINT('Ctrl Pts',(4.69473729694442,27.9441486342267,125.02317702846));
#95531=CARTESIAN_POINT('Ctrl Pts',(4.69859607343734,27.9445776365808,124.951836889996));
#95532=CARTESIAN_POINT('Ctrl Pts',(4.70245484993025,27.9487185311775,124.880660575812));
#95533=CARTESIAN_POINT('Ctrl Pts',(4.70631119551846,27.9528568171443,124.809529100409));
#95534=CARTESIAN_POINT('Ctrl Pts',(4.71016754110667,27.960702327913,124.73856172835));
#95535=CARTESIAN_POINT('Ctrl Pts',(4.71402388669488,27.9722209939527,124.668171934379));
#95536=CARTESIAN_POINT('Ctrl Pts',(4.71787909294022,27.9837362568456,124.597802936809));
#95537=CARTESIAN_POINT('Ctrl Pts',(4.72173429918555,27.9989224421391,124.5280116577));
#95538=CARTESIAN_POINT('Ctrl Pts',(4.72558950543088,28.0176938863608,124.459204258219));
#95539=CARTESIAN_POINT('Ctrl Pts',(4.72944486228212,28.0364660639001,124.390394170736));
#95540=CARTESIAN_POINT('Ctrl Pts',(4.73330021913336,28.0588236484584,124.322568507269));
#95541=CARTESIAN_POINT('Ctrl Pts',(4.73715557598461,28.0846307894568,124.256119398154));
#95542=CARTESIAN_POINT('Ctrl Pts',(4.74101496845316,28.1104649442308,124.189600733046));
#95543=CARTESIAN_POINT('Ctrl Pts',(4.74487436092172,28.1397556872703,124.124461952444));
#95544=CARTESIAN_POINT('Ctrl Pts',(4.74873375339028,28.1723188950762,124.061075433698));
#95545=CARTESIAN_POINT('Ctrl Pts',(4.75259533099371,28.2049005397219,123.997653026379));
#95546=CARTESIAN_POINT('Ctrl Pts',(4.75645690859714,28.2407580932328,123.935985276046));
#95547=CARTESIAN_POINT('Ctrl Pts',(4.76031848620058,28.2796626801174,123.876417751867));
#95548=CARTESIAN_POINT('Ctrl Pts',(4.76418682031545,28.3186353374418,123.816746003794));
#95549=CARTESIAN_POINT('Ctrl Pts',(4.76805515443032,28.3606653857265,123.759182211013));
#95550=CARTESIAN_POINT('Ctrl Pts',(4.77192348854519,28.4054824916262,123.704040325477));
#95551=CARTESIAN_POINT('Ctrl Pts',(4.77422120771614,28.4321030265527,123.671287061732));
#95552=CARTESIAN_POINT('Ctrl Pts',(4.7765189268871,28.4597061291631,123.639387615171));
#95553=CARTESIAN_POINT('Ctrl Pts',(4.77881664605805,28.4882291828091,123.60840143763));
#95554=CARTESIAN_POINT('Ctrl Pts',(4.78268571940627,28.5362584581298,123.556224567975));
#95555=CARTESIAN_POINT('Ctrl Pts',(4.78655479275448,28.5870862098637,123.506434921696));
#95556=CARTESIAN_POINT('Ctrl Pts',(4.79042386610269,28.6404457659139,123.459347590441));
#95557=CARTESIAN_POINT('Ctrl Pts',(4.79428717449847,28.6937258157686,123.412330419714));
#95558=CARTESIAN_POINT('Ctrl Pts',(4.79815048289426,28.7495298205365,123.368007890384));
#95559=CARTESIAN_POINT('Ctrl Pts',(4.80201379129004,28.807552954178,123.326659746074));
#95560=CARTESIAN_POINT('Ctrl Pts',(4.80587256778296,28.8655080230472,123.285360105728));
#95561=CARTESIAN_POINT('Ctrl Pts',(4.80973134427587,28.9256766563069,123.24702820034));
#95562=CARTESIAN_POINT('Ctrl Pts',(4.81359012076878,28.9877208506948,123.211903669714));
#95563=CARTESIAN_POINT('Ctrl Pts',(4.81744646635699,29.0497259592419,123.17680126641));
#95564=CARTESIAN_POINT('Ctrl Pts',(4.82130281194519,29.113603863011,123.144902467903));
#95565=CARTESIAN_POINT('Ctrl Pts',(4.8251591575334,29.1789887057697,123.116402904747));
#95566=CARTESIAN_POINT('Ctrl Pts',(4.82901436377873,29.2443542308214,123.08791176168));
#95567=CARTESIAN_POINT('Ctrl Pts',(4.83286957002406,29.3112253658995,123.062818054167));
#95568=CARTESIAN_POINT('Ctrl Pts',(4.83672477626939,29.379214416526,123.041270099822));
#95569=CARTESIAN_POINT('Ctrl Pts',(4.84058013312064,29.4472061231851,123.019721303694));
#95570=CARTESIAN_POINT('Ctrl Pts',(4.84443548997189,29.5163153683473,123.001718680408));
#95571=CARTESIAN_POINT('Ctrl Pts',(4.84829084682315,29.5861390257614,122.987360773387));
#95572=CARTESIAN_POINT('Ctrl Pts',(4.8521502392917,29.6560357714966,122.972987837143));
#95573=CARTESIAN_POINT('Ctrl Pts',(4.85600963176026,29.7266479454857,122.962267331063));
#95574=CARTESIAN_POINT('Ctrl Pts',(4.85986902422882,29.7975628353236,122.955246529075));
#95575=CARTESIAN_POINT('Ctrl Pts',(4.86373060183225,29.8685178761958,122.948221752007));
#95576=CARTESIAN_POINT('Ctrl Pts',(4.86759217943569,29.9397754886193,122.944900871601));
#95577=CARTESIAN_POINT('Ctrl Pts',(4.87145375703912,30.0109212110364,122.945279023894));
#95578=CARTESIAN_POINT('Ctrl Pts',(4.875322091154,30.0821914154493,122.945657837831));
#95579=CARTESIAN_POINT('Ctrl Pts',(4.87919042526887,30.1533488538536,122.949748578334));
#95580=CARTESIAN_POINT('Ctrl Pts',(4.88305875938374,30.2239831424414,122.957494402847));
#95581=CARTESIAN_POINT('Ctrl Pts',(4.8853564785547,30.2659386080748,122.962095279852));
#95582=CARTESIAN_POINT('Ctrl Pts',(4.88765419772566,30.3077096541242,122.967984734544));
#95583=CARTESIAN_POINT('Ctrl Pts',(4.88995191689662,30.3492123714913,122.975142404489));
#95584=CARTESIAN_POINT('Ctrl Pts',(4.89382099024483,30.4190977864161,122.987195030576));
#95585=CARTESIAN_POINT('Ctrl Pts',(4.89769006359304,30.4884953840998,123.002893522819));
#95586=CARTESIAN_POINT('Ctrl Pts',(4.90155913694126,30.556995808955,123.022184732765));
#95587=CARTESIAN_POINT('Ctrl Pts',(4.90542244533704,30.6253941675905,123.041447198644));
#95588=CARTESIAN_POINT('Ctrl Pts',(4.90928575373283,30.6928975431111,123.064291625702));
#95589=CARTESIAN_POINT('Ctrl Pts',(4.91314906212862,30.7591055840197,123.0906136392));
#95590=CARTESIAN_POINT('Ctrl Pts',(4.91700783862153,30.8252359587468,123.116904775326));
#95591=CARTESIAN_POINT('Ctrl Pts',(4.92086661511444,30.8900735678922,123.146665216172));
#95592=CARTESIAN_POINT('Ctrl Pts',(4.92472539160736,30.9532337587871,123.179740962498));
#95593=CARTESIAN_POINT('Ctrl Pts',(4.92858173719556,31.0163541607992,123.212795872171));
#95594=CARTESIAN_POINT('Ctrl Pts',(4.93243808278376,31.0777988117449,123.249161718872));
#95595=CARTESIAN_POINT('Ctrl Pts',(4.93629442837197,31.1372049265935,123.28863723383));
#95596=CARTESIAN_POINT('Ctrl Pts',(4.9401496346173,31.1965934901279,123.328101085896));
#95597=CARTESIAN_POINT('Ctrl Pts',(4.94400484086263,31.2539443088718,123.370672513554));
#95598=CARTESIAN_POINT('Ctrl Pts',(4.94786004710797,31.3089225031754,123.416106239932));
#95599=CARTESIAN_POINT('Ctrl Pts',(4.95171540395921,31.3639028452346,123.461541741206));
#95600=CARTESIAN_POINT('Ctrl Pts',(4.95557076081045,31.4165100057711,123.509839452046));
#95601=CARTESIAN_POINT('Ctrl Pts',(4.95942611766169,31.4664425529626,123.56071413494));
#95602=CARTESIAN_POINT('Ctrl Pts',(4.96328551013024,31.5164273673398,123.611642071207));
#95603=CARTESIAN_POINT('Ctrl Pts',(4.9671449025988,31.5637316386327,123.665152016857));
#95604=CARTESIAN_POINT('Ctrl Pts',(4.97100429506736,31.6080918095682,123.720922873905));
#95605=CARTESIAN_POINT('Ctrl Pts',(4.97486587267079,31.6524770966218,123.776725307644));
#95606=CARTESIAN_POINT('Ctrl Pts',(4.97872745027423,31.6939146826955,123.834790805449));
#95607=CARTESIAN_POINT('Ctrl Pts',(4.98258902787766,31.7321838651537,123.894768522073));
#95608=CARTESIAN_POINT('Ctrl Pts',(4.98645736199253,31.7705200062996,123.954851180295));
#95609=CARTESIAN_POINT('Ctrl Pts',(4.99032569610741,31.8056764360191,124.016852314539));
#95610=CARTESIAN_POINT('Ctrl Pts',(4.99419403022228,31.8374783327799,124.080396314131));
#95611=CARTESIAN_POINT('Ctrl Pts',(4.99649174939324,31.8563680733479,124.118140278774));
#95612=CARTESIAN_POINT('Ctrl Pts',(4.99878946856421,31.8740752011141,124.156428182751));
#95613=CARTESIAN_POINT('Ctrl Pts',(5.00108718773517,31.8905713141637,124.195178486519));
#95614=CARTESIAN_POINT('Ctrl Pts',(5.00537446195653,31.9213511244747,124.267482004075));
#95615=CARTESIAN_POINT('Ctrl Pts',(5.00966173617788,31.9480150746286,124.341637213737));
#95616=CARTESIAN_POINT('Ctrl Pts',(5.01394901039923,31.9703612656983,124.417184381527));
#95617=CARTESIAN_POINT('Ctrl Pts',(5.01822262075598,31.9926362377804,124.492490774826));
#95618=CARTESIAN_POINT('Ctrl Pts',(5.02249623111273,32.0106207692067,124.5691800047));
#95619=CARTESIAN_POINT('Ctrl Pts',(5.02676984146948,32.0241613070718,124.646774058918));
#95620=CARTESIAN_POINT('Ctrl Pts',(5.03102083155061,32.0376301746924,124.723957406789));
#95621=CARTESIAN_POINT('Ctrl Pts',(5.03527182163173,32.046701841573,124.802035744087));
#95622=CARTESIAN_POINT('Ctrl Pts',(5.03952281171286,32.0512732988447,124.880520227877));
#95623=CARTESIAN_POINT('Ctrl Pts',(5.04165696797268,32.0535683416387,124.919922378713));
#95624=CARTESIAN_POINT('Ctrl Pts',(5.04379112423251,32.0547299142489,124.959426631909));
#95625=CARTESIAN_POINT('Ctrl Pts',(5.04592528049234,32.0547497417017,124.998969719981));
#95626=CARTESIAN_POINT('Origin',(-1.54592528053767,30.,125.));
#95627=CARTESIAN_POINT('',(3.89394636966105,28.7479590808042,126.629230216746));
#95628=CARTESIAN_POINT('',(3.95204573436854,28.7479590808042,126.629230216746));
#95629=CARTESIAN_POINT('',(-1.54592528053767,28.7479590808042,126.629230216746));
#95630=CARTESIAN_POINT('',(4.40407471951208,32.0547494817011,125.001459434548));
#95631=CARTESIAN_POINT('Ctrl Pts',(3.95204573436854,28.7479590808042,126.629230216746));
#95632=CARTESIAN_POINT('Ctrl Pts',(3.95593320439764,28.6909466062034,126.585416917452));
#95633=CARTESIAN_POINT('Ctrl Pts',(3.95982067442675,28.6362547070576,126.538621365018));
#95634=CARTESIAN_POINT('Ctrl Pts',(3.96370814445585,28.5841986334277,126.489128622018));
#95635=CARTESIAN_POINT('Ctrl Pts',(3.96756865504022,28.5325035665271,126.439979109154));
#95636=CARTESIAN_POINT('Ctrl Pts',(3.97142916562458,28.4834081758202,126.388170095774));
#95637=CARTESIAN_POINT('Ctrl Pts',(3.97528967620894,28.4371827374804,126.334016404124));
#95638=CARTESIAN_POINT('Ctrl Pts',(3.97919062596042,28.3904730838574,126.279295448082));
#95639=CARTESIAN_POINT('Ctrl Pts',(3.98309157571189,28.346694173615,126.222180805065));
#95640=CARTESIAN_POINT('Ctrl Pts',(3.98699252546337,28.3060805130307,126.163028088296));
#95641=CARTESIAN_POINT('Ctrl Pts',(3.99089347521484,28.2654668524464,126.103875371528));
#95642=CARTESIAN_POINT('Ctrl Pts',(3.99479442496632,28.2280186495009,126.04268504536));
#95643=CARTESIAN_POINT('Ctrl Pts',(3.99869537471779,28.1939221902578,125.979836980144));
#95644=CARTESIAN_POINT('Ctrl Pts',(4.002564448066,28.1601043484165,125.917502474547));
#95645=CARTESIAN_POINT('Ctrl Pts',(4.00643352141422,28.1294511504299,125.853293046297));
#95646=CARTESIAN_POINT('Ctrl Pts',(4.01030259476243,28.1021743860266,125.78756301427));
#95647=CARTESIAN_POINT('Ctrl Pts',(4.01416590315821,28.0749382642358,125.721930920554));
#95648=CARTESIAN_POINT('Ctrl Pts',(4.01802921155399,28.0510687744828,125.654783165467));
#95649=CARTESIAN_POINT('Ctrl Pts',(4.02189251994977,28.0307319100997,125.586498723443));
#95650=CARTESIAN_POINT('Ctrl Pts',(4.02575129644268,28.0104189021331,125.518294383349));
#95651=CARTESIAN_POINT('Ctrl Pts',(4.02961007293559,27.9936304261563,125.448956468227));
#95652=CARTESIAN_POINT('Ctrl Pts',(4.0334688494285,27.9804837906095,125.378882359723));
#95653=CARTESIAN_POINT('Ctrl Pts',(4.03732519501671,27.967345437019,125.308852395646));
#95654=CARTESIAN_POINT('Ctrl Pts',(4.04118154060491,27.9578444614835,125.238087634642));
#95655=CARTESIAN_POINT('Ctrl Pts',(4.04503788619312,27.9520475161225,125.166997563695));
#95656=CARTESIAN_POINT('Ctrl Pts',(4.04889309243845,27.9462522834474,125.095928496044));
#95657=CARTESIAN_POINT('Ctrl Pts',(4.05274829868378,27.9441589478354,125.024534793175));
#95658=CARTESIAN_POINT('Ctrl Pts',(4.05660350492912,27.9457823265314,124.953231287068));
#95659=CARTESIAN_POINT('Ctrl Pts',(4.06045886178037,27.9474057686457,124.881924995447));
#95660=CARTESIAN_POINT('Ctrl Pts',(4.06431421863162,27.9527462000759,124.810709393194));
#95661=CARTESIAN_POINT('Ctrl Pts',(4.06816957548287,27.9617663485297,124.739997799021));
#95662=CARTESIAN_POINT('Ctrl Pts',(4.07202896795143,27.9707959388766,124.669212187073));
#95663=CARTESIAN_POINT('Ctrl Pts',(4.07588836041999,27.9835128736403,124.598932119228));
#95664=CARTESIAN_POINT('Ctrl Pts',(4.07974775288854,27.9998282686891,124.529563386029));
#95665=CARTESIAN_POINT('Ctrl Pts',(4.08360933049198,28.0161529012899,124.460155377208));
#95666=CARTESIAN_POINT('Ctrl Pts',(4.08747090809541,28.0360799142421,124.391660196868));
#95667=CARTESIAN_POINT('Ctrl Pts',(4.09133248569884,28.059470527105,124.324468411304));
#95668=CARTESIAN_POINT('Ctrl Pts',(4.09520081981371,28.0829020659726,124.257159061854));
#95669=CARTESIAN_POINT('Ctrl Pts',(4.09906915392858,28.1098091206268,124.191158110286));
#95670=CARTESIAN_POINT('Ctrl Pts',(4.10293748804345,28.1400050514508,124.126835437119));
#95671=CARTESIAN_POINT('Ctrl Pts',(4.10523520721442,28.1579408778502,124.088628954722));
#95672=CARTESIAN_POINT('Ctrl Pts',(4.10753292638539,28.1770361820225,124.051014126221));
#95673=CARTESIAN_POINT('Ctrl Pts',(4.10983064555635,28.1972445332815,124.014063749669));
#95674=CARTESIAN_POINT('Ctrl Pts',(4.11369971890457,28.2312728837673,123.951843910566));
#95675=CARTESIAN_POINT('Ctrl Pts',(4.11756879225279,28.2685928276123,123.891265935902));
#95676=CARTESIAN_POINT('Ctrl Pts',(4.12143786560101,28.3090215532381,123.832699929287));
#95677=CARTESIAN_POINT('Ctrl Pts',(4.1253011739968,28.3493900397164,123.774221186523));
#95678=CARTESIAN_POINT('Ctrl Pts',(4.1291644823926,28.3928578396386,123.717748857686));
#95679=CARTESIAN_POINT('Ctrl Pts',(4.13302779078839,28.439196588897,123.663627943128));
#95680=CARTESIAN_POINT('Ctrl Pts',(4.13688656728131,28.4854809798984,123.609570515794));
#95681=CARTESIAN_POINT('Ctrl Pts',(4.14074534377422,28.5346293162262,123.557859390924));
#95682=CARTESIAN_POINT('Ctrl Pts',(4.14460412026714,28.5863713641367,123.508808649982));
#95683=CARTESIAN_POINT('Ctrl Pts',(4.14846046585534,28.6380808162262,123.459788809425));
#95684=CARTESIAN_POINT('Ctrl Pts',(4.15231681144355,28.6923803864433,123.413426361147));
#95685=CARTESIAN_POINT('Ctrl Pts',(4.15617315703175,28.7489621966506,123.369999393531));
#95686=CARTESIAN_POINT('Ctrl Pts',(4.16002836327709,28.8055272899739,123.32658525625));
#95687=CARTESIAN_POINT('Ctrl Pts',(4.16388356952242,28.8643728995,123.286105173457));
#95688=CARTESIAN_POINT('Ctrl Pts',(4.16773877576775,28.9251585431536,123.248796583733));
#95689=CARTESIAN_POINT('Ctrl Pts',(4.17159413261901,28.9859465614344,123.211486536528));
#95690=CARTESIAN_POINT('Ctrl Pts',(4.17544948947026,29.0486743491377,123.177348480609));
#95691=CARTESIAN_POINT('Ctrl Pts',(4.17930484632152,29.1129744440581,123.146575271125));
#95692=CARTESIAN_POINT('Ctrl Pts',(4.18316423879008,29.1773418454784,123.115769849604));
#95693=CARTESIAN_POINT('Ctrl Pts',(4.18702363125864,29.2432844004596,123.088336515709));
#95694=CARTESIAN_POINT('Ctrl Pts',(4.1908830237272,29.3104129791301,123.064420680223));
#95695=CARTESIAN_POINT('Ctrl Pts',(4.19474460133064,29.3775795650775,123.040491303921));
#95696=CARTESIAN_POINT('Ctrl Pts',(4.19860617893407,29.4459330457811,123.020083529651));
#95697=CARTESIAN_POINT('Ctrl Pts',(4.20246775653751,29.5150700199579,123.00329259105));
#95698=CARTESIAN_POINT('Ctrl Pts',(4.20633609065238,29.5843279614709,122.986472273739));
#95699=CARTESIAN_POINT('Ctrl Pts',(4.21020442476726,29.6543716558731,122.973281516649));
#95700=CARTESIAN_POINT('Ctrl Pts',(4.21407275888213,29.7247891238029,122.963764125617));
#95701=CARTESIAN_POINT('Ctrl Pts',(4.21637047805306,29.7666158019609,122.95811097075));
#95702=CARTESIAN_POINT('Ctrl Pts',(4.21866819722398,29.8085742650121,122.953752835488));
#95703=CARTESIAN_POINT('Ctrl Pts',(4.22096591639491,29.8505781698027,122.950690194441));
#95704=CARTESIAN_POINT('Ctrl Pts',(4.22483498974313,29.9213075220243,122.945533087776));
#95705=CARTESIAN_POINT('Ctrl Pts',(4.22870406309136,29.992442714435,122.944031880373));
#95706=CARTESIAN_POINT('Ctrl Pts',(4.23257313643958,30.0635736564372,122.946233715169));
#95707=CARTESIAN_POINT('Ctrl Pts',(4.23643644483536,30.1345986127262,122.948432269213));
#95708=CARTESIAN_POINT('Ctrl Pts',(4.24029975323114,30.2056188495803,122.954322898336));
#95709=CARTESIAN_POINT('Ctrl Pts',(4.24416306162692,30.2762206606867,122.963900859705));
#95710=CARTESIAN_POINT('Ctrl Pts',(4.24802183811984,30.3467396514441,122.973467585525));
#95711=CARTESIAN_POINT('Ctrl Pts',(4.25188061461276,30.4168407123872,122.986712986754));
#95712=CARTESIAN_POINT('Ctrl Pts',(4.25573939110568,30.486113404921,123.003580374757));
#95713=CARTESIAN_POINT('Ctrl Pts',(4.25959573669389,30.5553424578932,123.020437136849));
#95714=CARTESIAN_POINT('Ctrl Pts',(4.2634520822821,30.6237437069094,123.040911244136));
#95715=CARTESIAN_POINT('Ctrl Pts',(4.26730842787031,30.6909165357611,123.064894859933));
#95716=CARTESIAN_POINT('Ctrl Pts',(4.27116363411565,30.758069518652,123.088871389862));
#95717=CARTESIAN_POINT('Ctrl Pts',(4.27501884036099,30.823994344649,123.116355206567));
#95718=CARTESIAN_POINT('Ctrl Pts',(4.27887404660633,30.8883068660086,123.147189034385));
#95719=CARTESIAN_POINT('Ctrl Pts',(4.28272940345757,30.9526218997746,123.178024066745));
#95720=CARTESIAN_POINT('Ctrl Pts',(4.28658476030882,31.0153240667623,123.212209158044));
#95721=CARTESIAN_POINT('Ctrl Pts',(4.29044011716006,31.076052042658,123.249540184982));
#95722=CARTESIAN_POINT('Ctrl Pts',(4.29429950962863,31.1368435859175,123.286910288391));
#95723=CARTESIAN_POINT('Ctrl Pts',(4.2981589020972,31.1956563982011,123.327432646139));
#95724=CARTESIAN_POINT('Ctrl Pts',(4.30201829456576,31.2521572635066,123.370859198857));
#95725=CARTESIAN_POINT('Ctrl Pts',(4.30587987216921,31.3086901188242,123.414310339092));
#95726=CARTESIAN_POINT('Ctrl Pts',(4.30974144977265,31.3629080519682,123.460668631776));
#95727=CARTESIAN_POINT('Ctrl Pts',(4.31360302737609,31.4145122626436,123.509646813225));
#95728=CARTESIAN_POINT('Ctrl Pts',(4.31747136149097,31.4662067639916,123.558710690645));
#95729=CARTESIAN_POINT('Ctrl Pts',(4.32133969560585,31.5152780778472,123.610403256402));
#95730=CARTESIAN_POINT('Ctrl Pts',(4.32520802972072,31.5614659582079,123.664402147404));
#95731=CARTESIAN_POINT('Ctrl Pts',(4.32750574889164,31.5889007079005,123.696476493461));
#95732=CARTESIAN_POINT('Ctrl Pts',(4.32980346806255,31.6153189306065,123.729363929871));
#95733=CARTESIAN_POINT('Ctrl Pts',(4.33210118723347,31.6406733981607,123.762992173401));
#95734=CARTESIAN_POINT('Ctrl Pts',(4.33598223894951,31.6834993453242,123.819793262894));
#95735=CARTESIAN_POINT('Ctrl Pts',(4.33986329066555,31.7234572903184,123.878933890298));
#95736=CARTESIAN_POINT('Ctrl Pts',(4.34374434238158,31.7602831217962,123.940093922265));
#95737=CARTESIAN_POINT('Ctrl Pts',(4.34761960540831,31.7970540265912,124.001162732458));
#95738=CARTESIAN_POINT('Ctrl Pts',(4.35149486843504,31.8307018422713,124.064244561641));
#95739=CARTESIAN_POINT('Ctrl Pts',(4.35537013146177,31.8610038890162,124.128987894707));
#95740=CARTESIAN_POINT('Ctrl Pts',(4.35942884712848,31.892740416578,124.196796138539));
#95741=CARTESIAN_POINT('Ctrl Pts',(4.36348756279519,31.9208061964461,124.266426682191));
#95742=CARTESIAN_POINT('Ctrl Pts',(4.3675462784619,31.9449979565051,124.337443955811));
#95743=CARTESIAN_POINT('Ctrl Pts',(4.3714136667849,31.9680493200514,124.405113484126));
#95744=CARTESIAN_POINT('Ctrl Pts',(4.3752810551079,31.9875834868983,124.474041440803));
#95745=CARTESIAN_POINT('Ctrl Pts',(4.3791484434309,32.0034736409933,124.543830149675));
#95746=CARTESIAN_POINT('Ctrl Pts',(4.38301406018542,32.019356516146,124.613586889822));
#95747=CARTESIAN_POINT('Ctrl Pts',(4.38687967693995,32.0315985897938,124.684203129537));
#95748=CARTESIAN_POINT('Ctrl Pts',(4.39074529369447,32.0401235137114,124.755268287094));
#95749=CARTESIAN_POINT('Ctrl Pts',(4.39461092103537,32.0486484609754,124.826333639271));
#95750=CARTESIAN_POINT('Ctrl Pts',(4.39847654837627,32.0534561785914,124.897847434106));
#95751=CARTESIAN_POINT('Ctrl Pts',(4.40234217571717,32.0545220261427,124.969392703572));
#95752=CARTESIAN_POINT('Ctrl Pts',(4.40291969029889,32.0546812609701,124.980081379103));
#95753=CARTESIAN_POINT('Ctrl Pts',(4.4034972048806,32.0547570735857,124.990770753233));
#95754=CARTESIAN_POINT('Ctrl Pts',(4.40407471946232,32.0547494817017,125.001459433627));
#95755=CARTESIAN_POINT('Ctrl Pts',(4.40407471951208,32.0547494817011,125.001459434548));
#95756=CARTESIAN_POINT('Ctrl Pts',(4.40849095806784,32.054691426731,125.083195487561));
#95757=CARTESIAN_POINT('Ctrl Pts',(4.41290719662359,32.0497522762919,125.164736898229));
#95758=CARTESIAN_POINT('Ctrl Pts',(4.41732343517935,32.0400254037025,125.245548192314));
#95759=CARTESIAN_POINT('Ctrl Pts',(4.4217797159882,32.0302103370789,125.327092206393));
#95760=CARTESIAN_POINT('Ctrl Pts',(4.42623599679705,32.0155204432693,125.407892614198));
#95761=CARTESIAN_POINT('Ctrl Pts',(4.4306922776059,31.9961013728879,125.487418579513));
#95762=CARTESIAN_POINT('Ctrl Pts',(4.43487367109461,31.9778801750029,125.562038956419));
#95763=CARTESIAN_POINT('Ctrl Pts',(4.43905506458332,31.9554957935067,125.635537342885));
#95764=CARTESIAN_POINT('Ctrl Pts',(4.44323645807203,31.929106484379,125.70749256846));
#95765=CARTESIAN_POINT('Ctrl Pts',(4.44710553142024,31.9046882676053,125.774073254131));
#95766=CARTESIAN_POINT('Ctrl Pts',(4.45097460476846,31.8767712524526,125.839518723707));
#95767=CARTESIAN_POINT('Ctrl Pts',(4.45484367811667,31.8454813033536,125.903435842477));
#95768=CARTESIAN_POINT('Ctrl Pts',(4.45870698651246,31.8142379765467,125.967257724193));
#95769=CARTESIAN_POINT('Ctrl Pts',(4.46257029490824,31.7796319035186,126.029555342638));
#95770=CARTESIAN_POINT('Ctrl Pts',(4.46643360330402,31.7418377221508,126.08995362846));
#95771=CARTESIAN_POINT('Ctrl Pts',(4.47029237979693,31.7040878757263,126.150281063307));
#95772=CARTESIAN_POINT('Ctrl Pts',(4.47415115628985,31.663157606008,126.208713181357));
#95773=CARTESIAN_POINT('Ctrl Pts',(4.47800993278276,31.6192675452454,126.264899276391));
#95774=CARTESIAN_POINT('Ctrl Pts',(4.48186627837097,31.5754051338052,126.321049975998));
#95775=CARTESIAN_POINT('Ctrl Pts',(4.48572262395917,31.5285869289447,126.374957077847));
#95776=CARTESIAN_POINT('Ctrl Pts',(4.48957896954738,31.4790761318271,126.426299883881));
#95777=CARTESIAN_POINT('Ctrl Pts',(4.49343417579271,31.4295799624892,126.477627520875));
#95778=CARTESIAN_POINT('Ctrl Pts',(4.49728938203805,31.3773931172376,126.526392016629));
#95779=CARTESIAN_POINT('Ctrl Pts',(4.50114458828338,31.3228170725558,126.572308034405));
#95780=CARTESIAN_POINT('Ctrl Pts',(4.50499994513463,31.2682388958286,126.618225845918));
#95781=CARTESIAN_POINT('Ctrl Pts',(4.50885530198588,31.2112717075103,126.66129464747));
#95782=CARTESIAN_POINT('Ctrl Pts',(4.51271065883712,31.1522502816128,126.701269188289));
#95783=CARTESIAN_POINT('Ctrl Pts',(4.51657005130568,31.0931670746929,126.741285572693));
#95784=CARTESIAN_POINT('Ctrl Pts',(4.52042944377424,31.0320257407811,126.778200957745));
#95785=CARTESIAN_POINT('Ctrl Pts',(4.5242888362428,30.9691895223346,126.811813796254));
#95786=CARTESIAN_POINT('Ctrl Pts',(4.52815041384624,30.9063177268864,126.845445665889));
#95787=CARTESIAN_POINT('Ctrl Pts',(4.53201199144967,30.8417495765083,126.875771060062));
#95788=CARTESIAN_POINT('Ctrl Pts',(4.53587356905311,30.7758698732851,126.902635935283));
#95789=CARTESIAN_POINT('Ctrl Pts',(4.53974190316798,30.7098749018958,126.929547815343));
#95790=CARTESIAN_POINT('Ctrl Pts',(4.54361023728285,30.6425642549527,126.952986928087));
#95791=CARTESIAN_POINT('Ctrl Pts',(4.54747857139773,30.5743388494691,126.972848815417));
#95792=CARTESIAN_POINT('Ctrl Pts',(4.54977629056868,30.533814216004,126.984646410436));
#95793=CARTESIAN_POINT('Ctrl Pts',(4.55207400973964,30.4929670773005,126.995182881589));
#95794=CARTESIAN_POINT('Ctrl Pts',(4.55437172891059,30.451882750053,127.004444946289));
#95795=CARTESIAN_POINT('Ctrl Pts',(4.55844028469716,30.3791350098275,127.020845221574));
#95796=CARTESIAN_POINT('Ctrl Pts',(4.56250884048373,30.3053433991469,127.03331376979));
#95797=CARTESIAN_POINT('Ctrl Pts',(4.56657739627029,30.2309718247415,127.041727106808));
#95798=CARTESIAN_POINT('Ctrl Pts',(4.57043972402091,30.1603700164458,127.049713986366));
#95799=CARTESIAN_POINT('Ctrl Pts',(4.57430205177154,30.0892461673342,127.054046646543));
#95800=CARTESIAN_POINT('Ctrl Pts',(4.57816437952216,30.0180102763838,127.054671066727));
#95801=CARTESIAN_POINT('Ctrl Pts',(4.58202291837601,29.9468442669799,127.055294874362));
#95802=CARTESIAN_POINT('Ctrl Pts',(4.58588145722987,29.8755669170033,127.052217654884));
#95803=CARTESIAN_POINT('Ctrl Pts',(4.58973999608372,29.8045925651953,127.045437238569));
#95804=CARTESIAN_POINT('Ctrl Pts',(4.59359604063054,29.733664093922,127.038661205374));
#95805=CARTESIAN_POINT('Ctrl Pts',(4.59745208517735,29.6630387144404,127.028186773093));
#95806=CARTESIAN_POINT('Ctrl Pts',(4.60130812972416,29.5931282481697,127.014063787486));
#95807=CARTESIAN_POINT('Ctrl Pts',(4.6051629715136,29.5232395880081,126.999945207047));
#95808=CARTESIAN_POINT('Ctrl Pts',(4.60901781330305,29.4540658736896,126.982180430866));
#95809=CARTESIAN_POINT('Ctrl Pts',(4.6128726550925,29.3860095914793,126.960870556856));
#95810=CARTESIAN_POINT('Ctrl Pts',(4.61672928267136,29.3179217815969,126.939550810859));
#95811=CARTESIAN_POINT('Ctrl Pts',(4.62058591025023,29.2509529028989,126.914682828748));
#95812=CARTESIAN_POINT('Ctrl Pts',(4.62444253782909,29.1854899614899,126.886417493469));
#95813=CARTESIAN_POINT('Ctrl Pts',(4.62830019968253,29.1200094641579,126.858144577962));
#95814=CARTESIAN_POINT('Ctrl Pts',(4.63215786153597,29.0560361472741,126.826472703826));
#95815=CARTESIAN_POINT('Ctrl Pts',(4.63601552338942,28.9939345295402,126.791599796732));
#95816=CARTESIAN_POINT('Ctrl Pts',(4.63987764453128,28.9317611250517,126.756686578081));
#95817=CARTESIAN_POINT('Ctrl Pts',(4.64373976567315,28.8714641517747,126.718565195949));
#95818=CARTESIAN_POINT('Ctrl Pts',(4.64760188681501,28.8133802409445,126.677477603403));
#95819=CARTESIAN_POINT('Ctrl Pts',(4.64907361380609,28.7912463781847,126.661820476988));
#95820=CARTESIAN_POINT('Ctrl Pts',(4.65054534079716,28.769433546249,126.645733046843));
#95821=CARTESIAN_POINT('Ctrl Pts',(4.65201706778823,28.7479590808042,126.629230216746));
#95822=CARTESIAN_POINT('',(4.34592528058851,32.054749644159,124.998790732221));
#95823=CARTESIAN_POINT('Ctrl Pts',(4.34592528058851,32.054749644159,124.998790732221));
#95824=CARTESIAN_POINT('Ctrl Pts',(4.34974237135631,32.054790885948,125.068867478462));
#95825=CARTESIAN_POINT('Ctrl Pts',(4.35355946212412,32.0512429716114,125.139087448465));
#95826=CARTESIAN_POINT('Ctrl Pts',(4.35737655289193,32.0440883161919,125.209046688822));
#95827=CARTESIAN_POINT('Ctrl Pts',(4.36118805254433,32.0369441406135,125.278903455801));
#95828=CARTESIAN_POINT('Ctrl Pts',(4.36499955219674,32.0262037618738,125.348499758144));
#95829=CARTESIAN_POINT('Ctrl Pts',(4.36881105184914,32.0119016127191,125.417431986362));
#95830=CARTESIAN_POINT('Ctrl Pts',(4.37261948474207,31.9976109711744,125.486308751224));
#95831=CARTESIAN_POINT('Ctrl Pts',(4.37642791763499,31.9797643402254,125.554522013912));
#95832=CARTESIAN_POINT('Ctrl Pts',(4.38023635052792,31.9584477379755,125.621675172513));
#95833=CARTESIAN_POINT('Ctrl Pts',(4.3840430711884,31.9371407194517,125.688798139741));
#95834=CARTESIAN_POINT('Ctrl Pts',(4.38784979184888,31.9123669742972,125.754861472596));
#95835=CARTESIAN_POINT('Ctrl Pts',(4.39165651250936,31.8842627237944,125.819482489269));
#95836=CARTESIAN_POINT('Ctrl Pts',(4.39546287300873,31.8561611322884,125.884097392025));
#95837=CARTESIAN_POINT('Ctrl Pts',(4.3992692335081,31.824729861666,125.947269792158));
#95838=CARTESIAN_POINT('Ctrl Pts',(4.40307559400747,31.790153006837,126.008637583383));
#95839=CARTESIAN_POINT('Ctrl Pts',(4.40688551323035,31.7555438246795,126.070062749889));
#95840=CARTESIAN_POINT('Ctrl Pts',(4.41069543245322,31.7177834317559,126.129679502484));
#95841=CARTESIAN_POINT('Ctrl Pts',(4.4145053516761,31.6771010428774,126.187151908763));
#95842=CARTESIAN_POINT('Ctrl Pts',(4.41831711300213,31.636398983987,126.244652103059));
#95843=CARTESIAN_POINT('Ctrl Pts',(4.42212887432815,31.5927724276009,126.300005495642));
#95844=CARTESIAN_POINT('Ctrl Pts',(4.42594063565417,31.5464911598374,126.352908960368));
#95845=CARTESIAN_POINT('Ctrl Pts',(4.42975910316259,31.5001284676098,126.405905500251));
#95846=CARTESIAN_POINT('Ctrl Pts',(4.43357757067101,31.4511020881567,126.456443149052));
#95847=CARTESIAN_POINT('Ctrl Pts',(4.43739603817942,31.3997183644,126.504255983156));
#95848=CARTESIAN_POINT('Ctrl Pts',(4.44006763663374,31.3637676389681,126.537708328478));
#95849=CARTESIAN_POINT('Ctrl Pts',(4.44273923508806,31.3266637077768,126.569827654897));
#95850=CARTESIAN_POINT('Ctrl Pts',(4.44541083354239,31.2885201183749,126.600535368882));
#95851=CARTESIAN_POINT('Ctrl Pts',(4.4492799068906,31.233279651784,126.645007021265));
#95852=CARTESIAN_POINT('Ctrl Pts',(4.45314898023881,31.1756259560803,126.686702591709));
#95853=CARTESIAN_POINT('Ctrl Pts',(4.45701805358702,31.1158695099186,126.725350051246));
#95854=CARTESIAN_POINT('Ctrl Pts',(4.46088136198281,31.0562021013734,126.763939925737));
#95855=CARTESIAN_POINT('Ctrl Pts',(4.4647446703786,30.9944385661034,126.799490442826));
#95856=CARTESIAN_POINT('Ctrl Pts',(4.4686079787744,30.93092186864,126.831770192188));
#95857=CARTESIAN_POINT('Ctrl Pts',(4.47246675526731,30.8674796802436,126.864012075381));
#95858=CARTESIAN_POINT('Ctrl Pts',(4.47632553176023,30.8022888456627,126.892990593039));
#95859=CARTESIAN_POINT('Ctrl Pts',(4.48018430825314,30.7357191879357,126.918518918073));
#95860=CARTESIAN_POINT('Ctrl Pts',(4.48404065384135,30.6691914669456,126.944031161085));
#95861=CARTESIAN_POINT('Ctrl Pts',(4.48789699942955,30.6012870986315,126.966097350154));
#95862=CARTESIAN_POINT('Ctrl Pts',(4.49175334501776,30.5323969196767,126.984578313501));
#95863=CARTESIAN_POINT('Ctrl Pts',(4.4956085512631,30.4635270940674,127.003053816717));
#95864=CARTESIAN_POINT('Ctrl Pts',(4.49946375750843,30.3936725049776,127.017946071298));
#95865=CARTESIAN_POINT('Ctrl Pts',(4.50331896375376,30.3232385643445,127.02916593531));
#95866=CARTESIAN_POINT('Ctrl Pts',(4.50717432060501,30.252801872168,127.040386237632));
#95867=CARTESIAN_POINT('Ctrl Pts',(4.51102967745625,30.1817862635977,127.047933790311));
#95868=CARTESIAN_POINT('Ctrl Pts',(4.51488503430749,30.1106050250402,127.051770964542));
#95869=CARTESIAN_POINT('Ctrl Pts',(4.51874442677605,30.0393492771052,127.055612155357));
#95870=CARTESIAN_POINT('Ctrl Pts',(4.52260381924461,29.9679280391648,127.055735188464));
#95871=CARTESIAN_POINT('Ctrl Pts',(4.52646321171317,29.8967564692991,127.052154559449));
#95872=CARTESIAN_POINT('Ctrl Pts',(4.53032478931661,29.8255446030706,127.048571903132));
#95873=CARTESIAN_POINT('Ctrl Pts',(4.53418636692004,29.7545831697897,127.041281459958));
#95874=CARTESIAN_POINT('Ctrl Pts',(4.53804794452347,29.6842813201143,127.030349545687));
#95875=CARTESIAN_POINT('Ctrl Pts',(4.54191627863834,29.6138564649473,127.019398504103));
#95876=CARTESIAN_POINT('Ctrl Pts',(4.54578461275322,29.5440939731246,127.00479337032));
#95877=CARTESIAN_POINT('Ctrl Pts',(4.54965294686809,29.4753912491378,126.986651258027));
#95878=CARTESIAN_POINT('Ctrl Pts',(4.55195066603904,29.4345830972788,126.975875177683));
#95879=CARTESIAN_POINT('Ctrl Pts',(4.55424838520999,29.3941485465819,126.963852154995));
#95880=CARTESIAN_POINT('Ctrl Pts',(4.55654610438094,29.3541675553052,126.950614778955));
#95881=CARTESIAN_POINT('Ctrl Pts',(4.56041440943521,29.2868579064214,126.928329110068));
#95882=CARTESIAN_POINT('Ctrl Pts',(4.56428271448948,29.2205713092772,126.902511739845));
#95883=CARTESIAN_POINT('Ctrl Pts',(4.56815101954375,29.1557044645014,126.873275903661));
#95884=CARTESIAN_POINT('Ctrl Pts',(4.57201426861242,29.0909224025513,126.844078279553));
#95885=CARTESIAN_POINT('Ctrl Pts',(4.57587751768109,29.0275568522896,126.811471247144));
#95886=CARTESIAN_POINT('Ctrl Pts',(4.57974076674976,28.9659882294994,126.77561741965));
#95887=CARTESIAN_POINT('Ctrl Pts',(4.5835995535365,28.9044907221223,126.739805005455));
#95888=CARTESIAN_POINT('Ctrl Pts',(4.58745834032323,28.8447864376399,126.700753487886));
#95889=CARTESIAN_POINT('Ctrl Pts',(4.59131712710997,28.7872329245225,126.658672234993));
#95890=CARTESIAN_POINT('Ctrl Pts',(4.59220253450987,28.7740271401086,126.649016595859));
#95891=CARTESIAN_POINT('Ctrl Pts',(4.59308794190978,28.7609344849291,126.639201635604));
#95892=CARTESIAN_POINT('Ctrl Pts',(4.59397334930969,28.7479590808042,126.629230216746));
#95893=CARTESIAN_POINT('Ctrl Pts',(3.89394636966105,28.7479590808042,126.629230216746));
#95894=CARTESIAN_POINT('Ctrl Pts',(3.89781318580622,28.6916844716005,126.585983956819));
#95895=CARTESIAN_POINT('Ctrl Pts',(3.9016800019514,28.6375514615491,126.539740510312));
#95896=CARTESIAN_POINT('Ctrl Pts',(3.90554681809657,28.585895921426,126.490740492997));
#95897=CARTESIAN_POINT('Ctrl Pts',(3.90951860693371,28.5328380852282,126.440410269246));
#95898=CARTESIAN_POINT('Ctrl Pts',(3.91349039577086,28.4823946506547,126.387171875852));
#95899=CARTESIAN_POINT('Ctrl Pts',(3.91746218460801,28.434895455922,126.331332163138));
#95900=CARTESIAN_POINT('Ctrl Pts',(3.92131985599883,28.3887610081656,126.277096837183));
#95901=CARTESIAN_POINT('Ctrl Pts',(3.92517752738964,28.3454042309927,126.220408057136));
#95902=CARTESIAN_POINT('Ctrl Pts',(3.92903519878045,28.3050902823745,126.161584526239));
#95903=CARTESIAN_POINT('Ctrl Pts',(3.93289094488817,28.2647964536047,126.102790352936));
#95904=CARTESIAN_POINT('Ctrl Pts',(3.93674669099589,28.2275427141598,126.041863943026));
#95905=CARTESIAN_POINT('Ctrl Pts',(3.94060243710361,28.1935524070084,125.979155072639));
#95906=CARTESIAN_POINT('Ctrl Pts',(3.94445754870422,28.1595676933507,125.916456521714));
#95907=CARTESIAN_POINT('Ctrl Pts',(3.94831266030482,28.1288455764369,125.851976520105));
#95908=CARTESIAN_POINT('Ctrl Pts',(3.95216777190542,28.1015638481471,125.78609016012));
#95909=CARTESIAN_POINT('Ctrl Pts',(3.95622627009564,28.0728428002602,125.71672779128));
#95910=CARTESIAN_POINT('Ctrl Pts',(3.96028476828587,28.0479354221679,125.6458071135));
#95911=CARTESIAN_POINT('Ctrl Pts',(3.9643432664761,28.026990986085,125.573788282828));
#95912=CARTESIAN_POINT('Ctrl Pts',(3.96820348502378,28.0070697992694,125.505287962533));
#95913=CARTESIAN_POINT('Ctrl Pts',(3.97206370357146,27.9907334521896,125.43579478774));
#95914=CARTESIAN_POINT('Ctrl Pts',(3.97592392211914,27.9780581556152,125.3657167489));
#95915=CARTESIAN_POINT('Ctrl Pts',(3.97978684019179,27.9653739949625,125.295589703142));
#95916=CARTESIAN_POINT('Ctrl Pts',(3.98364975826444,27.9563560389418,125.224877460961));
#95917=CARTESIAN_POINT('Ctrl Pts',(3.98751267633709,27.9510286398102,125.153993271353));
#95918=CARTESIAN_POINT('Ctrl Pts',(3.99138185011661,27.9456926133542,125.082994290102));
#95919=CARTESIAN_POINT('Ctrl Pts',(3.99525102389613,27.9440590725777,125.011823290158));
#95920=CARTESIAN_POINT('Ctrl Pts',(3.99912019767565,27.9461003233506,124.940892633628));
#95921=CARTESIAN_POINT('Ctrl Pts',(3.99970338184648,27.9464079924312,124.93020155629));
#95922=CARTESIAN_POINT('Ctrl Pts',(4.00028656601731,27.9467990508151,124.919515925859));
#95923=CARTESIAN_POINT('Ctrl Pts',(4.00086975018814,27.947273302386,124.90883713803));
#95924=CARTESIAN_POINT('Ctrl Pts',(4.00473882353636,27.9504196739869,124.837989856074));
#95925=CARTESIAN_POINT('Ctrl Pts',(4.00860789688458,27.9572443216409,124.76716688376));
#95926=CARTESIAN_POINT('Ctrl Pts',(4.01247697023279,27.9677461262914,124.696781010989));
#95927=CARTESIAN_POINT('Ctrl Pts',(4.01634027862858,27.9782322831631,124.626500013772));
#95928=CARTESIAN_POINT('Ctrl Pts',(4.02020358702437,27.9923846502762,124.556655299875));
#95929=CARTESIAN_POINT('Ctrl Pts',(4.02406689542016,28.0101501558678,124.487657184781));
#95930=CARTESIAN_POINT('Ctrl Pts',(4.02792567191308,28.0278948214079,124.4187400088));
#95931=CARTESIAN_POINT('Ctrl Pts',(4.03178444840599,28.0492440859145,124.350667927121));
#95932=CARTESIAN_POINT('Ctrl Pts',(4.03564322489891,28.074093669959,124.283841937553));
#95933=CARTESIAN_POINT('Ctrl Pts',(4.03949957048712,28.0989275995671,124.217058046203));
#95934=CARTESIAN_POINT('Ctrl Pts',(4.04335591607532,28.1272573049389,124.151519143788));
#95935=CARTESIAN_POINT('Ctrl Pts',(4.04721226166353,28.1589288574896,124.087610493969));
#95936=CARTESIAN_POINT('Ctrl Pts',(4.05106746790887,28.1905910527986,124.023720725721));
#95937=CARTESIAN_POINT('Ctrl Pts',(4.0549226741542,28.2255929195603,123.961460688887));
#95938=CARTESIAN_POINT('Ctrl Pts',(4.05877788039954,28.2637333542969,123.901193512251));
#95939=CARTESIAN_POINT('Ctrl Pts',(4.06263323725079,28.3018752790121,123.840923981242));
#95940=CARTESIAN_POINT('Ctrl Pts',(4.06648859410204,28.3431557534862,123.78264787431));
#95941=CARTESIAN_POINT('Ctrl Pts',(4.07034395095329,28.3873298158111,123.726700176891));
#95942=CARTESIAN_POINT('Ctrl Pts',(4.07420334342185,28.4315501175939,123.670693915894));
#95943=CARTESIAN_POINT('Ctrl Pts',(4.07806273589041,28.4786697519009,123.617021311813));
#95944=CARTESIAN_POINT('Ctrl Pts',(4.08192212835897,28.5284034077903,123.565984298448));
#95945=CARTESIAN_POINT('Ctrl Pts',(4.08578370596241,28.5781652221908,123.51491838863));
#95946=CARTESIAN_POINT('Ctrl Pts',(4.08964528356585,28.6305436475806,123.466491370049));
#95947=CARTESIAN_POINT('Ctrl Pts',(4.09350686116929,28.6852184606156,123.420966413849));
#95948=CARTESIAN_POINT('Ctrl Pts',(4.09737519528416,28.739988936884,123.375361803704));
#95949=CARTESIAN_POINT('Ctrl Pts',(4.10124352939904,28.7970634335981,123.332669684725));
#95950=CARTESIAN_POINT('Ctrl Pts',(4.10511186351391,28.8560913755696,123.293110835041));
#95951=CARTESIAN_POINT('Ctrl Pts',(4.10740958268484,28.891152885217,123.269613607398));
#95952=CARTESIAN_POINT('Ctrl Pts',(4.10970730185577,28.9269030806235,123.247220986002));
#95953=CARTESIAN_POINT('Ctrl Pts',(4.1120050210267,28.963264653256,123.225971425452));
#95954=CARTESIAN_POINT('Ctrl Pts',(4.11587409437491,29.0244930197819,123.190189808002));
#95955=CARTESIAN_POINT('Ctrl Pts',(4.11974316772313,29.0876959275458,123.15751165516));
#95956=CARTESIAN_POINT('Ctrl Pts',(4.12361224107134,29.1525259668354,123.128159909177));
#95957=CARTESIAN_POINT('Ctrl Pts',(4.12747554946713,29.2172594088112,123.098851897547));
#95958=CARTESIAN_POINT('Ctrl Pts',(4.13133885786291,29.2836147309308,123.072860653239));
#95959=CARTESIAN_POINT('Ctrl Pts',(4.1352021662587,29.3512184250661,123.050364128734));
#95960=CARTESIAN_POINT('Ctrl Pts',(4.13906094275161,29.4187428158311,123.027893994063));
#95961=CARTESIAN_POINT('Ctrl Pts',(4.14291971924452,29.4875122110835,123.008910588793));
#95962=CARTESIAN_POINT('Ctrl Pts',(4.14677849573743,29.5571331576807,122.993543790043));
#95963=CARTESIAN_POINT('Ctrl Pts',(4.15063484132563,29.6267102453275,122.978186671881));
#95964=CARTESIAN_POINT('Ctrl Pts',(4.15449118691384,29.6971373467644,122.966441744494));
#95965=CARTESIAN_POINT('Ctrl Pts',(4.15834753250204,29.7680072998736,122.958388638945));
#95966=CARTESIAN_POINT('Ctrl Pts',(4.16220273874737,29.8388563147202,122.950337912657));
#95967=CARTESIAN_POINT('Ctrl Pts',(4.1660579449927,29.910147439071,122.945976897614));
#95968=CARTESIAN_POINT('Ctrl Pts',(4.16991315123804,29.9814665213124,122.945333586037));
#95969=CARTESIAN_POINT('Ctrl Pts',(4.17376850808928,30.052788389676,122.944690249329));
#95970=CARTESIAN_POINT('Ctrl Pts',(4.17762386494053,30.1241377323125,122.947764906609));
#95971=CARTESIAN_POINT('Ctrl Pts',(4.18147922179178,30.1951002548221,122.95453343878));
#95972=CARTESIAN_POINT('Ctrl Pts',(4.18533861426034,30.2661370577668,122.961309055952));
#95973=CARTESIAN_POINT('Ctrl Pts',(4.18919800672889,30.3367857477186,122.971786220367));
#95974=CARTESIAN_POINT('Ctrl Pts',(4.19305739919745,30.4066379145317,122.985888987924));
#95975=CARTESIAN_POINT('Ctrl Pts',(4.19691897680088,30.47652963068,122.999999740275));
#95976=CARTESIAN_POINT('Ctrl Pts',(4.20078055440432,30.5456234551795,123.017740061325));
#95977=CARTESIAN_POINT('Ctrl Pts',(4.20464213200775,30.6135246088483,123.038983652073));
#95978=CARTESIAN_POINT('Ctrl Pts',(4.20851046612262,30.6815445675673,123.060264412231));
#95979=CARTESIAN_POINT('Ctrl Pts',(4.21237880023749,30.7483672335371,123.085060510933));
#95980=CARTESIAN_POINT('Ctrl Pts',(4.21624713435236,30.8136169820417,123.11319715682));
#95981=CARTESIAN_POINT('Ctrl Pts',(4.21854485352333,30.8523741301027,123.129909805919));
#95982=CARTESIAN_POINT('Ctrl Pts',(4.22084257269429,30.890576768762,123.14780014868));
#95983=CARTESIAN_POINT('Ctrl Pts',(4.22314029186526,30.9281506612642,123.16682409123));
#95984=CARTESIAN_POINT('Ctrl Pts',(4.22700936521348,30.9914204236903,123.198858044738));
#95985=CARTESIAN_POINT('Ctrl Pts',(4.2308784385617,31.053153750569,123.234234104093));
#95986=CARTESIAN_POINT('Ctrl Pts',(4.23474751190992,31.1129749158546,123.272781311131));
#95987=CARTESIAN_POINT('Ctrl Pts',(4.23861082030571,31.1727069470915,123.3112710825));
#95988=CARTESIAN_POINT('Ctrl Pts',(4.24247412870151,31.2305320671689,123.352922361501));
#95989=CARTESIAN_POINT('Ctrl Pts',(4.2463374370973,31.2860981930608,123.397517862719));
#95990=CARTESIAN_POINT('Ctrl Pts',(4.25019621359021,31.3415991364045,123.442061050619));
#95991=CARTESIAN_POINT('Ctrl Pts',(4.25405499008313,31.3948459722219,123.489541297822));
#95992=CARTESIAN_POINT('Ctrl Pts',(4.25791376657605,31.4455161902342,123.53969848789));
#95993=CARTESIAN_POINT('Ctrl Pts',(4.26177011216426,31.4961544876437,123.589824080546));
#95994=CARTESIAN_POINT('Ctrl Pts',(4.26562645775247,31.5442190431934,123.642622929359));
#95995=CARTESIAN_POINT('Ctrl Pts',(4.26948280334068,31.5894221252485,123.697796148727));
#95996=CARTESIAN_POINT('Ctrl Pts',(4.27333800958602,31.6346118522222,123.752953067373));
#95997=CARTESIAN_POINT('Ctrl Pts',(4.27719321583136,31.6769414763768,123.810482588337));
#95998=CARTESIAN_POINT('Ctrl Pts',(4.28104842207669,31.7161628592682,123.870051946783));
#95999=CARTESIAN_POINT('Ctrl Pts',(4.28490377892795,31.7553857743661,123.929623632341));
#96000=CARTESIAN_POINT('Ctrl Pts',(4.28875913577921,31.7914999418229,123.991234906642));
#96001=CARTESIAN_POINT('Ctrl Pts',(4.29261449263046,31.8243009267402,124.054524621582));
#96002=CARTESIAN_POINT('Ctrl Pts',(4.29647388509903,31.8571362462801,124.117880585401));
#96003=CARTESIAN_POINT('Ctrl Pts',(4.30033327756759,31.886651236199,124.182918064873));
#96004=CARTESIAN_POINT('Ctrl Pts',(4.30419267003616,31.9126881934482,124.249252747495));
#96005=CARTESIAN_POINT('Ctrl Pts',(4.3080542476396,31.9387398924641,124.3156249879));
#96006=CARTESIAN_POINT('Ctrl Pts',(4.31191582524304,31.9613094849422,124.383295432486));
#96007=CARTESIAN_POINT('Ctrl Pts',(4.31577740284648,31.9802889661263,124.45186391002));
#96008=CARTESIAN_POINT('Ctrl Pts',(4.31964573696136,31.9993016552619,124.520552360206));
#96009=CARTESIAN_POINT('Ctrl Pts',(4.32351407107624,32.0147115867778,124.590141505974));
#96010=CARTESIAN_POINT('Ctrl Pts',(4.32738240519111,32.0264618851514,124.660220968086));
#96011=CARTESIAN_POINT('Ctrl Pts',(4.32968012436202,32.0334413458276,124.701846877017));
#96012=CARTESIAN_POINT('Ctrl Pts',(4.33197784353292,32.0391306287757,124.743645657191));
#96013=CARTESIAN_POINT('Ctrl Pts',(4.33427556270382,32.0435265158289,124.785531024145));
#96014=CARTESIAN_POINT('Ctrl Pts',(4.33815880198178,32.0509557445539,124.856319005629));
#96015=CARTESIAN_POINT('Ctrl Pts',(4.34204204125973,32.0547076876349,124.927499585747));
#96016=CARTESIAN_POINT('Ctrl Pts',(4.34592528053768,32.0547496441584,124.998790731288));
#96017=CARTESIAN_POINT('Origin',(-1.54592528053767,30.,125.));
#96018=CARTESIAN_POINT('',(3.19385981572075,28.7479590808042,126.629230216746));
#96019=CARTESIAN_POINT('',(3.25213329794676,28.7479590808042,126.629230216746));
#96020=CARTESIAN_POINT('',(-1.54592528053767,28.7479590808042,126.629230216746));
#96021=CARTESIAN_POINT('',(3.70407471941286,32.0547494644754,124.998516511556));
#96022=CARTESIAN_POINT('Ctrl Pts',(3.25213329794676,28.7479590808042,126.629230216746));
#96023=CARTESIAN_POINT('Ctrl Pts',(3.25599022148438,28.6914802934207,126.585827048708));
#96024=CARTESIAN_POINT('Ctrl Pts',(3.259847145022,28.6372135453225,126.539447080033));
#96025=CARTESIAN_POINT('Ctrl Pts',(3.26370406855962,28.5854831545881,126.490348837201));
#96026=CARTESIAN_POINT('Ctrl Pts',(3.26755947480621,28.533773114285,126.441269909328));
#96027=CARTESIAN_POINT('Ctrl Pts',(3.2714148810528,28.4845978030209,126.389475163782));
#96028=CARTESIAN_POINT('Ctrl Pts',(3.27527028729939,28.4382467997662,126.335261960837));
#96029=CARTESIAN_POINT('Ctrl Pts',(3.27912546654167,28.3918985256343,126.281051949938));
#96030=CARTESIAN_POINT('Ctrl Pts',(3.28298064578395,28.3483745438087,126.224424134623));
#96031=CARTESIAN_POINT('Ctrl Pts',(3.28683582502624,28.3079248849838,126.165709812793));
#96032=CARTESIAN_POINT('Ctrl Pts',(3.29069479734036,28.2674354281489,126.106937722537));
#96033=CARTESIAN_POINT('Ctrl Pts',(3.29455376965448,28.2300266127931,126.046075426003));
#96034=CARTESIAN_POINT('Ctrl Pts',(3.29841274196861,28.1959052402902,125.98348343173));
#96035=CARTESIAN_POINT('Ctrl Pts',(3.30227356023783,28.16176754569,125.920861496322));
#96036=CARTESIAN_POINT('Ctrl Pts',(3.30613437850706,28.1309206370948,125.856508653557));
#96037=CARTESIAN_POINT('Ctrl Pts',(3.30999519677628,28.1035241472872,125.790807753235));
#96038=CARTESIAN_POINT('Ctrl Pts',(3.3138631308159,28.0760771637456,125.72498576135));
#96039=CARTESIAN_POINT('Ctrl Pts',(3.31773106485551,28.0520934688296,125.657811206416));
#96040=CARTESIAN_POINT('Ctrl Pts',(3.32159899889512,28.0316834001859,125.589684089489));
#96041=CARTESIAN_POINT('Ctrl Pts',(3.32502724915889,28.0135934269613,125.529301258711));
#96042=CARTESIAN_POINT('Ctrl Pts',(3.32845549942266,27.998310112601,125.468170553243));
#96043=CARTESIAN_POINT('Ctrl Pts',(3.33188374968643,27.9858764481741,125.406575799182));
#96044=CARTESIAN_POINT('Ctrl Pts',(3.33575282303466,27.9718439954785,125.337060856283));
#96045=CARTESIAN_POINT('Ctrl Pts',(3.33962189638289,27.9613871130559,125.266682430377));
#96046=CARTESIAN_POINT('Ctrl Pts',(3.34349096973111,27.9546042657694,125.195841397287));
#96047=CARTESIAN_POINT('Ctrl Pts',(3.34735427812691,27.9478315249835,125.125105917943));
#96048=CARTESIAN_POINT('Ctrl Pts',(3.35121758652271,27.9447219988389,125.053909679268));
#96049=CARTESIAN_POINT('Ctrl Pts',(3.35508089491851,27.9453231361891,124.982663684928));
#96050=CARTESIAN_POINT('Ctrl Pts',(3.35893967141143,27.9459235683675,124.911501266606));
#96051=CARTESIAN_POINT('Ctrl Pts',(3.36279844790435,27.9502260137478,124.840289691965));
#96052=CARTESIAN_POINT('Ctrl Pts',(3.36665722439727,27.9582259778627,124.769443271568));
#96053=CARTESIAN_POINT('Ctrl Pts',(3.37051356998549,27.9662209022584,124.69864148213));
#96054=CARTESIAN_POINT('Ctrl Pts',(3.37436991557371,27.9779086696809,124.628204872126));
#96055=CARTESIAN_POINT('Ctrl Pts',(3.37822626116192,27.9932328074159,124.558544456068));
#96056=CARTESIAN_POINT('Ctrl Pts',(3.38208146740726,28.0085524176919,124.488904620919));
#96057=CARTESIAN_POINT('Ctrl Pts',(3.3859366736526,28.0275061610818,124.420040998629));
#96058=CARTESIAN_POINT('Ctrl Pts',(3.38979187989794,28.049986444219,124.352354499151));
#96059=CARTESIAN_POINT('Ctrl Pts',(3.39364723674921,28.0724676055618,124.284665355459));
#96060=CARTESIAN_POINT('Ctrl Pts',(3.39750259360047,28.0984754249617,124.218153886206));
#96061=CARTESIAN_POINT('Ctrl Pts',(3.40135795045173,28.1278529579342,124.153204265844));
#96062=CARTESIAN_POINT('Ctrl Pts',(3.4052173429203,28.1572612420109,124.088186659088));
#96063=CARTESIAN_POINT('Ctrl Pts',(3.40907673538887,28.1900460802679,124.024734608321));
#96064=CARTESIAN_POINT('Ctrl Pts',(3.41293612785744,28.2260033992025,123.963209942728));
#96065=CARTESIAN_POINT('Ctrl Pts',(3.41679770546088,28.261981076676,123.901650442716));
#96066=CARTESIAN_POINT('Ctrl Pts',(3.42065928306432,28.3011345437782,123.842020906504));
#96067=CARTESIAN_POINT('Ctrl Pts',(3.42452086066776,28.3432164968478,123.784653964427));
#96068=CARTESIAN_POINT('Ctrl Pts',(3.42838919478264,28.3853720797202,123.727186648762));
#96069=CARTESIAN_POINT('Ctrl Pts',(3.43225752889752,28.430466071138,123.671990207426));
#96070=CARTESIAN_POINT('Ctrl Pts',(3.4361258630124,28.478211487711,123.619363448852));
#96071=CARTESIAN_POINT('Ctrl Pts',(3.43842358218327,28.5065713852076,123.58810412417));
#96072=CARTESIAN_POINT('Ctrl Pts',(3.44072130135413,28.5358660346019,123.557750714455));
#96073=CARTESIAN_POINT('Ctrl Pts',(3.44301902052499,28.5660296831504,123.528359183464));
#96074=CARTESIAN_POINT('Ctrl Pts',(3.4468880938732,28.6168215162709,123.478867500293));
#96075=CARTESIAN_POINT('Ctrl Pts',(3.45075716722141,28.6702780599787,123.431911487284));
#96076=CARTESIAN_POINT('Ctrl Pts',(3.45462624056962,28.726115924839,123.387791289705));
#96077=CARTESIAN_POINT('Ctrl Pts',(3.4584895489654,28.7818705908023,123.343736831598));
#96078=CARTESIAN_POINT('Ctrl Pts',(3.46235285736118,28.8399991568083,123.302510100363));
#96079=CARTESIAN_POINT('Ctrl Pts',(3.46621616575696,28.9001820553279,123.264373873475));
#96080=CARTESIAN_POINT('Ctrl Pts',(3.47007494224987,28.9602943555357,123.226282382771));
#96081=CARTESIAN_POINT('Ctrl Pts',(3.47393371874278,29.0224557931118,123.19127445399));
#96082=CARTESIAN_POINT('Ctrl Pts',(3.47779249523568,29.0863158500692,123.159571018304));
#96083=CARTESIAN_POINT('Ctrl Pts',(3.48164884082389,29.1501356772509,123.12788755476));
#96084=CARTESIAN_POINT('Ctrl Pts',(3.48550518641209,29.2156515667144,123.099504669707));
#96085=CARTESIAN_POINT('Ctrl Pts',(3.48936153200029,29.282487578493,123.074597837468));
#96086=CARTESIAN_POINT('Ctrl Pts',(3.49321673824562,29.3493038438221,123.049698363859));
#96087=CARTESIAN_POINT('Ctrl Pts',(3.49707194449095,29.4174390022008,123.028273073754));
#96088=CARTESIAN_POINT('Ctrl Pts',(3.50092715073628,29.4864978769364,123.010449012438));
#96089=CARTESIAN_POINT('Ctrl Pts',(3.50478250758752,29.5555594494978,122.992624254815));
#96090=CARTESIAN_POINT('Ctrl Pts',(3.50863786443876,29.6255443391371,122.978401124561));
#96091=CARTESIAN_POINT('Ctrl Pts',(3.51249322129,29.6960446631114,122.967856128204));
#96092=CARTESIAN_POINT('Ctrl Pts',(3.51635261375855,29.766618783712,122.957300093811));
#96093=CARTESIAN_POINT('Ctrl Pts',(3.52021200622711,29.8377089342526,122.950429951004));
#96094=CARTESIAN_POINT('Ctrl Pts',(3.52407139869566,29.9089004441357,122.947270491901));
#96095=CARTESIAN_POINT('Ctrl Pts',(3.52793297629909,29.9801322616715,122.944109243955));
#96096=CARTESIAN_POINT('Ctrl Pts',(3.53179455390252,30.0514650667905,122.94466285826));
#96097=CARTESIAN_POINT('Ctrl Pts',(3.53565613150595,30.1224852736351,122.948903970985));
#96098=CARTESIAN_POINT('Ctrl Pts',(3.53952446562081,30.1936297428639,122.953152504285));
#96099=CARTESIAN_POINT('Ctrl Pts',(3.54339279973568,30.2644600389161,122.961101363275));
#96100=CARTESIAN_POINT('Ctrl Pts',(3.54726113385054,30.3345694703278,122.972671503672));
#96101=CARTESIAN_POINT('Ctrl Pts',(3.54955885302155,30.3762131804726,122.97954395383));
#96102=CARTESIAN_POINT('Ctrl Pts',(3.55185657219255,30.4176027678518,122.987693065516));
#96103=CARTESIAN_POINT('Ctrl Pts',(3.55415429136355,30.4586555529481,122.99709394972));
#96104=CARTESIAN_POINT('Ctrl Pts',(3.55802336471178,30.5277833378797,123.012923869659));
#96105=CARTESIAN_POINT('Ctrl Pts',(3.56189243806,30.5962260391797,123.032367785461));
#96106=CARTESIAN_POINT('Ctrl Pts',(3.56576151140822,30.6635777914816,123.055350397333));
#96107=CARTESIAN_POINT('Ctrl Pts',(3.569624819804,30.7308291890953,123.078298764916));
#96108=CARTESIAN_POINT('Ctrl Pts',(3.57348812819978,30.7969924083189,123.104775206827));
#96109=CARTESIAN_POINT('Ctrl Pts',(3.57735143659556,30.8616733563976,123.13465376153));
#96110=CARTESIAN_POINT('Ctrl Pts',(3.58121021308847,30.9262784296706,123.164497266816));
#96111=CARTESIAN_POINT('Ctrl Pts',(3.58506898958139,30.989404246771,123.197734754904));
#96112=CARTESIAN_POINT('Ctrl Pts',(3.5889277660743,31.0506750854314,123.234191565499));
#96113=CARTESIAN_POINT('Ctrl Pts',(3.59278411166251,31.11190732544,123.27062540948));
#96114=CARTESIAN_POINT('Ctrl Pts',(3.59664045725072,31.1712864889583,123.310274304496));
#96115=CARTESIAN_POINT('Ctrl Pts',(3.60049680283892,31.2284612560282,123.352917577977));
#96116=CARTESIAN_POINT('Ctrl Pts',(3.60435200908425,31.2856191310272,123.395548252662));
#96117=CARTESIAN_POINT('Ctrl Pts',(3.60820721532958,31.3405735133575,123.441171259206));
#96118=CARTESIAN_POINT('Ctrl Pts',(3.61206242157491,31.3930033370947,123.489523497256));
#96119=CARTESIAN_POINT('Ctrl Pts',(3.61591777842617,31.4454352090343,123.537877624214));
#96120=CARTESIAN_POINT('Ctrl Pts',(3.61977313527743,31.4953419709618,123.588960863403));
#96121=CARTESIAN_POINT('Ctrl Pts',(3.62362849212869,31.5424381254604,123.642472029155));
#96122=CARTESIAN_POINT('Ctrl Pts',(3.62748788459725,31.5895835781337,123.696039208033));
#96123=CARTESIAN_POINT('Ctrl Pts',(3.63134727706582,31.6339122288398,123.75203902136));
#96124=CARTESIAN_POINT('Ctrl Pts',(3.63520666953438,31.6751783462025,123.810136532658));
#96125=CARTESIAN_POINT('Ctrl Pts',(3.63906824713783,31.7164678278727,123.868266937968));
#96126=CARTESIAN_POINT('Ctrl Pts',(3.64292982474127,31.7546910639906,123.928496995212));
#96127=CARTESIAN_POINT('Ctrl Pts',(3.64679140234471,31.7896467299866,123.990464391738));
#96128=CARTESIAN_POINT('Ctrl Pts',(3.65065973645959,31.8246635570886,124.052540211159));
#96129=CARTESIAN_POINT('Ctrl Pts',(3.65452807057446,31.8564011831501,124.116359003769));
#96130=CARTESIAN_POINT('Ctrl Pts',(3.65839640468934,31.8847054418733,124.181536219572));
#96131=CARTESIAN_POINT('Ctrl Pts',(3.66069412386026,31.9015176499081,124.220250284544));
#96132=CARTESIAN_POINT('Ctrl Pts',(3.66299184303119,31.9171194519224,124.259443265274));
#96133=CARTESIAN_POINT('Ctrl Pts',(3.66528956220212,31.9314869158582,124.299032200191));
#96134=CARTESIAN_POINT('Ctrl Pts',(3.66976608681316,31.9594782851779,124.376161226108));
#96135=CARTESIAN_POINT('Ctrl Pts',(3.67424261142421,31.9828725789903,124.455042428842));
#96136=CARTESIAN_POINT('Ctrl Pts',(3.67871913603526,32.0014795158366,124.535158833378));
#96137=CARTESIAN_POINT('Ctrl Pts',(3.68315616207663,32.0199222745636,124.614568331629));
#96138=CARTESIAN_POINT('Ctrl Pts',(3.687593188118,32.0336616960581,124.695191164253));
#96139=CARTESIAN_POINT('Ctrl Pts',(3.69203021415936,32.0425588387462,124.776502902122));
#96140=CARTESIAN_POINT('Ctrl Pts',(3.69604504924386,32.0506094024081,124.850077682827));
#96141=CARTESIAN_POINT('Ctrl Pts',(3.70005988432836,32.0546958210969,124.924216166571));
#96142=CARTESIAN_POINT('Ctrl Pts',(3.70407471941286,32.0547494644754,124.998516511556));
#96143=CARTESIAN_POINT('Ctrl Pts',(3.70407471946232,32.0547494644761,124.998516512471));
#96144=CARTESIAN_POINT('Ctrl Pts',(3.70793830290603,32.0548010869056,125.07001772652));
#96145=CARTESIAN_POINT('Ctrl Pts',(3.71180188634973,32.05111623467,125.141552238129));
#96146=CARTESIAN_POINT('Ctrl Pts',(3.71566546979344,32.0437110737996,125.212703101362));
#96147=CARTESIAN_POINT('Ctrl Pts',(3.71952882663486,32.0363063472477,125.28384979154));
#96148=CARTESIAN_POINT('Ctrl Pts',(3.72339218347628,32.0251817962445,125.354612398351));
#96149=CARTESIAN_POINT('Ctrl Pts',(3.72725554031771,32.0104054413673,125.4245792315));
#96150=CARTESIAN_POINT('Ctrl Pts',(3.73111993974985,31.9956250988464,125.494564946355));
#96151=CARTESIAN_POINT('Ctrl Pts',(3.73498433918199,31.9771910976808,125.563753989812));
#96152=CARTESIAN_POINT('Ctrl Pts',(3.73884873861412,31.9552221704324,125.631746647597));
#96153=CARTESIAN_POINT('Ctrl Pts',(3.74271803189443,31.9332254218896,125.699825410803));
#96154=CARTESIAN_POINT('Ctrl Pts',(3.74658732517474,31.9076849661823,125.766704306559));
#96155=CARTESIAN_POINT('Ctrl Pts',(3.75045661845505,31.8787685660619,125.832001344757));
#96156=CARTESIAN_POINT('Ctrl Pts',(3.75432884727595,31.849830227758,125.897347922262));
#96157=CARTESIAN_POINT('Ctrl Pts',(3.75820107609685,31.8175110677532,125.961109825251));
#96158=CARTESIAN_POINT('Ctrl Pts',(3.76207330491775,31.7820246506346,126.022929961938));
#96159=CARTESIAN_POINT('Ctrl Pts',(3.7659523107069,31.7464761270824,126.084858292929));
#96160=CARTESIAN_POINT('Ctrl Pts',(3.76983131649604,31.7077495507253,126.14483767518));
#96161=CARTESIAN_POINT('Ctrl Pts',(3.77371032228519,31.6661010629575,126.202540980804));
#96162=CARTESIAN_POINT('Ctrl Pts',(3.77461515920368,31.6563859216609,126.216001151808));
#96163=CARTESIAN_POINT('Ctrl Pts',(3.77551999612218,31.6465119574739,126.229337625414));
#96164=CARTESIAN_POINT('Ctrl Pts',(3.77642483304067,31.6364827163499,126.242546530955));
#96165=CARTESIAN_POINT('Ctrl Pts',(3.78029390638889,31.5935977845543,126.299027675063));
#96166=CARTESIAN_POINT('Ctrl Pts',(3.7841629797371,31.5477013562299,126.353396665213));
#96167=CARTESIAN_POINT('Ctrl Pts',(3.78803205308531,31.499029141768,126.405314624783));
#96168=CARTESIAN_POINT('Ctrl Pts',(3.79189536148109,31.4504294493225,126.457155226149));
#96169=CARTESIAN_POINT('Ctrl Pts',(3.79575866987688,31.3990625100133,126.506551694649));
#96170=CARTESIAN_POINT('Ctrl Pts',(3.79962197827266,31.3452053570871,126.553196738911));
#96171=CARTESIAN_POINT('Ctrl Pts',(3.80348075476557,31.2914113819767,126.599787065613));
#96172=CARTESIAN_POINT('Ctrl Pts',(3.80733953125848,31.2351333611201,126.643632062676));
#96173=CARTESIAN_POINT('Ctrl Pts',(3.8111983077514,31.1766851454725,126.684461228679));
#96174=CARTESIAN_POINT('Ctrl Pts',(3.8150546533396,31.1182737503153,126.725264673625));
#96175=CARTESIAN_POINT('Ctrl Pts',(3.81891099892781,31.0576952700762,126.763055779299));
#96176=CARTESIAN_POINT('Ctrl Pts',(3.82276734451601,30.9952954419552,126.797605225216));
#96177=CARTESIAN_POINT('Ctrl Pts',(3.82662255076135,30.9329140496297,126.832144463628));
#96178=CARTESIAN_POINT('Ctrl Pts',(3.83047775700669,30.8687128024804,126.863443708473));
#96179=CARTESIAN_POINT('Ctrl Pts',(3.83433296325203,30.8030636482531,126.891318677366));
#96180=CARTESIAN_POINT('Ctrl Pts',(3.83818832010328,30.7374119294027,126.919194735212));
#96181=CARTESIAN_POINT('Ctrl Pts',(3.84204367695452,30.6703126391835,126.943646063685));
#96182=CARTESIAN_POINT('Ctrl Pts',(3.84589903380577,30.6021577906023,126.96453647401));
#96183=CARTESIAN_POINT('Ctrl Pts',(3.84975842627433,30.5339316005351,126.985448751494));
#96184=CARTESIAN_POINT('Ctrl Pts',(3.85361781874289,30.4646481118627,127.002792527424));
#96185=CARTESIAN_POINT('Ctrl Pts',(3.85747721121145,30.3947137246523,127.016481747517));
#96186=CARTESIAN_POINT('Ctrl Pts',(3.86133878881489,30.3247397415547,127.030178718259));
#96187=CARTESIAN_POINT('Ctrl Pts',(3.86520036641832,30.2541146074701,127.040216945716));
#96188=CARTESIAN_POINT('Ctrl Pts',(3.86906194402176,30.1832513896225,127.046562115036));
#96189=CARTESIAN_POINT('Ctrl Pts',(3.87293027813663,30.1122641840707,127.05291838635));
#96190=CARTESIAN_POINT('Ctrl Pts',(3.8767986122515,30.041038548667,127.055568680571));
#96191=CARTESIAN_POINT('Ctrl Pts',(3.88066694636638,29.9699884019038,127.054530814196));
#96192=CARTESIAN_POINT('Ctrl Pts',(3.88296466553733,29.9277859241786,127.053914340697));
#96193=CARTESIAN_POINT('Ctrl Pts',(3.88526238470828,29.8856453002609,127.051997629856));
#96194=CARTESIAN_POINT('Ctrl Pts',(3.88756010387923,29.8436519877084,127.048793025552));
#96195=CARTESIAN_POINT('Ctrl Pts',(3.89142879128779,29.7729475249656,127.043397408683));
#96196=CARTESIAN_POINT('Ctrl Pts',(3.89529747869635,29.7023842190489,127.034326880076));
#96197=CARTESIAN_POINT('Ctrl Pts',(3.89916616610492,29.6323744923485,127.021595668927));
#96198=CARTESIAN_POINT('Ctrl Pts',(3.90302937629832,29.5624638841077,127.008882482388));
#96199=CARTESIAN_POINT('Ctrl Pts',(3.90689258649171,29.4931057738335,126.992518983125));
#96200=CARTESIAN_POINT('Ctrl Pts',(3.91075579668511,29.4247085528086,126.97257124416));
#96201=CARTESIAN_POINT('Ctrl Pts',(3.91461452951286,29.3563906024815,126.952646624135));
#96202=CARTESIAN_POINT('Ctrl Pts',(3.9184732623406,29.289031793557,126.929146150395));
#96203=CARTESIAN_POINT('Ctrl Pts',(3.92233199516835,29.2230295957748,126.902186781959));
#96204=CARTESIAN_POINT('Ctrl Pts',(3.9261881038897,29.157072282362,126.875245747067));
#96205=CARTESIAN_POINT('Ctrl Pts',(3.93004421261106,29.0924701971686,126.84485067038));
#96206=CARTESIAN_POINT('Ctrl Pts',(3.93390032133241,29.0296034510846,126.811167606919));
#96207=CARTESIAN_POINT('Ctrl Pts',(3.93775577558456,28.9667473749147,126.777490260239));
#96208=CARTESIAN_POINT('Ctrl Pts',(3.94161122983672,28.9056264847606,126.740526257113));
#96209=CARTESIAN_POINT('Ctrl Pts',(3.94546668408887,28.8465974085836,126.700488172442));
#96210=CARTESIAN_POINT('Ctrl Pts',(3.94765970084876,28.8130211436585,126.677714152838));
#96211=CARTESIAN_POINT('Ctrl Pts',(3.94985271760865,28.7801212097431,126.653946368624));
#96212=CARTESIAN_POINT('Ctrl Pts',(3.95204573436854,28.7479590808042,126.629230216746));
#96213=CARTESIAN_POINT('',(3.64592528049121,32.0547492155205,125.001795499313));
#96214=CARTESIAN_POINT('Ctrl Pts',(3.64592528053768,32.0547492155198,125.001795500168));
#96215=CARTESIAN_POINT('Ctrl Pts',(3.65155534725559,32.0546586344092,125.105455454746));
#96216=CARTESIAN_POINT('Ctrl Pts',(3.65718541397351,32.0467203700823,125.208784026605));
#96217=CARTESIAN_POINT('Ctrl Pts',(3.66281548069143,32.0311035472205,125.31083105213));
#96218=CARTESIAN_POINT('Ctrl Pts',(3.66436496635177,32.0268055443198,125.338916048393));
#96219=CARTESIAN_POINT('Ctrl Pts',(3.66591445201212,32.0219261885265,125.366904156545));
#96220=CARTESIAN_POINT('Ctrl Pts',(3.66746393767247,32.0164695735924,125.394775912736));
#96221=CARTESIAN_POINT('Ctrl Pts',(3.67133301102069,32.0028443791466,125.464371825627));
#96222=CARTESIAN_POINT('Ctrl Pts',(3.67520208436891,31.9855852435914,125.533397845814));
#96223=CARTESIAN_POINT('Ctrl Pts',(3.67907115771713,31.964754531172,125.601445920045));
#96224=CARTESIAN_POINT('Ctrl Pts',(3.68293446611291,31.9439548566924,125.669392602064));
#96225=CARTESIAN_POINT('Ctrl Pts',(3.6867977745087,31.91959430977,125.7363637698));
#96226=CARTESIAN_POINT('Ctrl Pts',(3.69066108290449,31.8917862649132,125.801961526749));
#96227=CARTESIAN_POINT('Ctrl Pts',(3.69451985939741,31.8640108406358,125.867482333418));
#96228=CARTESIAN_POINT('Ctrl Pts',(3.69837863589032,31.8327961401166,125.931632484396));
#96229=CARTESIAN_POINT('Ctrl Pts',(3.70223741238324,31.7983047958042,125.994030896848));
#96230=CARTESIAN_POINT('Ctrl Pts',(3.70609375797145,31.7638351799259,126.056390000312));
#96231=CARTESIAN_POINT('Ctrl Pts',(3.70995010355966,31.726093250008,126.116999130501));
#96232=CARTESIAN_POINT('Ctrl Pts',(3.71380644914788,31.6852884029878,126.175500132392));
#96233=CARTESIAN_POINT('Ctrl Pts',(3.71766165539321,31.644495611607,126.233983850382));
#96234=CARTESIAN_POINT('Ctrl Pts',(3.72151686163855,31.6006419774167,126.290360278362));
#96235=CARTESIAN_POINT('Ctrl Pts',(3.72537206788388,31.5539802651154,126.344300151801));
#96236=CARTESIAN_POINT('Ctrl Pts',(3.72922742473514,31.5073167299466,126.398242132433));
#96237=CARTESIAN_POINT('Ctrl Pts',(3.73308278158639,31.45784521836,126.449747003595));
#96238=CARTESIAN_POINT('Ctrl Pts',(3.73693813843765,31.4058576914228,126.498519841032));
#96239=CARTESIAN_POINT('Ctrl Pts',(3.74079753090621,31.3538157462381,126.547343731722));
#96240=CARTESIAN_POINT('Ctrl Pts',(3.74465692337477,31.2992528833456,126.593429546883));
#96241=CARTESIAN_POINT('Ctrl Pts',(3.74851631584333,31.2424960612573,126.636521035691));
#96242=CARTESIAN_POINT('Ctrl Pts',(3.75237789344677,31.1857071042378,126.679636922307));
#96243=CARTESIAN_POINT('Ctrl Pts',(3.75623947105021,31.1267221170804,126.719754834329));
#96244=CARTESIAN_POINT('Ctrl Pts',(3.76010104865366,31.0658968317975,126.756662035357));
#96245=CARTESIAN_POINT('Ctrl Pts',(3.76396938276853,31.0049651219447,126.793633812045));
#96246=CARTESIAN_POINT('Ctrl Pts',(3.7678377168834,30.9421871132999,126.827383431728));
#96247=CARTESIAN_POINT('Ctrl Pts',(3.77170605099828,30.8779422625739,126.857744585805));
#96248=CARTESIAN_POINT('Ctrl Pts',(3.77400377016919,30.839782005274,126.875778551771));
#96249=CARTESIAN_POINT('Ctrl Pts',(3.7763014893401,30.8011046100179,126.892617941925));
#96250=CARTESIAN_POINT('Ctrl Pts',(3.77859920851102,30.7619922359674,126.908236199957));
#96251=CARTESIAN_POINT('Ctrl Pts',(3.78246828185923,30.6961318619321,126.934535404255));
#96252=CARTESIAN_POINT('Ctrl Pts',(3.78633735520744,30.6287793604349,126.957472487004));
#96253=CARTESIAN_POINT('Ctrl Pts',(3.79020642855566,30.5603113789128,126.976878529693));
#96254=CARTESIAN_POINT('Ctrl Pts',(3.79406973695144,30.4919454152697,126.996255657212));
#96255=CARTESIAN_POINT('Ctrl Pts',(3.79793304534722,30.4224677343411,127.012112056774));
#96256=CARTESIAN_POINT('Ctrl Pts',(3.801796353743,30.3522741165742,127.024327174469));
#96257=CARTESIAN_POINT('Ctrl Pts',(3.80565513023591,30.2821628403201,127.036527963064));
#96258=CARTESIAN_POINT('Ctrl Pts',(3.80951390672882,30.211337771702,127.04509587146));
#96259=CARTESIAN_POINT('Ctrl Pts',(3.81337268322173,30.1402072810093,127.049960848614));
#96260=CARTESIAN_POINT('Ctrl Pts',(3.81722902880993,30.069121600231,127.054822760991));
#96261=CARTESIAN_POINT('Ctrl Pts',(3.82108537439814,29.9977313626166,127.05598633715));
#96262=CARTESIAN_POINT('Ctrl Pts',(3.82494171998634,29.9264510391781,127.05343325016));
#96263=CARTESIAN_POINT('Ctrl Pts',(3.82879692623167,29.8551917752445,127.05088091747));
#96264=CARTESIAN_POINT('Ctrl Pts',(3.832652132477,29.7840428462279,127.044614118991));
#96265=CARTESIAN_POINT('Ctrl Pts',(3.83650733872233,29.7134179720963,127.0346666321));
#96266=CARTESIAN_POINT('Ctrl Pts',(3.84036269557357,29.6427903389622,127.024718756606));
#96267=CARTESIAN_POINT('Ctrl Pts',(3.84421805242482,29.5726872820893,127.011089977162));
#96268=CARTESIAN_POINT('Ctrl Pts',(3.84807340927606,29.5035149293875,126.993865626656));
#96269=CARTESIAN_POINT('Ctrl Pts',(3.85193280174462,29.4342701701212,126.97662324646));
#96270=CARTESIAN_POINT('Ctrl Pts',(3.85579219421317,29.3659585321456,126.955777899661));
#96271=CARTESIAN_POINT('Ctrl Pts',(3.85965158668173,29.2989726334945,126.931465297102));
#96272=CARTESIAN_POINT('Ctrl Pts',(3.86351316428516,29.2319488083499,126.907138929083));
#96273=CARTESIAN_POINT('Ctrl Pts',(3.8673747418886,29.1662526643715,126.87934158674));
#96274=CARTESIAN_POINT('Ctrl Pts',(3.87123631949203,29.1022558669436,126.848256755449));
#96275=CARTESIAN_POINT('Ctrl Pts',(3.8751046536069,29.0381470958257,126.817117535761));
#96276=CARTESIAN_POINT('Ctrl Pts',(3.87897298772177,28.9757440330046,126.782679577797));
#96277=CARTESIAN_POINT('Ctrl Pts',(3.88284132183664,28.9153922052714,126.745171479859));
#96278=CARTESIAN_POINT('Ctrl Pts',(3.88513904100762,28.8795443318798,126.722892360957));
#96279=CARTESIAN_POINT('Ctrl Pts',(3.8874367601786,28.8444195966073,126.699530876914));
#96280=CARTESIAN_POINT('Ctrl Pts',(3.88973447934958,28.8100848707453,126.675141650032));
#96281=CARTESIAN_POINT('Ctrl Pts',(3.89113844278674,28.7891055011408,126.660239227127));
#96282=CARTESIAN_POINT('Ctrl Pts',(3.8925424062239,28.7683912634568,126.644932066913));
#96283=CARTESIAN_POINT('Ctrl Pts',(3.89394636966105,28.7479590808042,126.629230216746));
#96284=CARTESIAN_POINT('Ctrl Pts',(3.19385981572075,28.7479590808042,126.629230216746));
#96285=CARTESIAN_POINT('Ctrl Pts',(3.19772164131035,28.6914284965474,126.585787243526));
#96286=CARTESIAN_POINT('Ctrl Pts',(3.20158346689996,28.6372142192413,126.539439069122));
#96287=CARTESIAN_POINT('Ctrl Pts',(3.20544529248956,28.5856144481732,126.490473439308));
#96288=CARTESIAN_POINT('Ctrl Pts',(3.2093137709599,28.5339257846591,126.441423454961));
#96289=CARTESIAN_POINT('Ctrl Pts',(3.21318224943023,28.4848609521703,126.389747366776));
#96290=CARTESIAN_POINT('Ctrl Pts',(3.21705072790057,28.4386794775978,126.335767864872));
#96291=CARTESIAN_POINT('Ctrl Pts',(3.21900810337312,28.41531254243,126.30845527832));
#96292=CARTESIAN_POINT('Ctrl Pts',(3.22096547884567,28.3926831268905,126.280553475476));
#96293=CARTESIAN_POINT('Ctrl Pts',(3.22292285431822,28.3708205831168,126.252107020228));
#96294=CARTESIAN_POINT('Ctrl Pts',(3.22679192766653,28.3276056830492,126.195877940321));
#96295=CARTESIAN_POINT('Ctrl Pts',(3.23066100101483,28.28722056777,126.137298834087));
#96296=CARTESIAN_POINT('Ctrl Pts',(3.23453007436313,28.2499301970683,126.076686234409));
#96297=CARTESIAN_POINT('Ctrl Pts',(3.238393382759,28.2126953893384,126.016163948024));
#96298=CARTESIAN_POINT('Ctrl Pts',(3.24225669115488,28.1785464255689,125.953614592887));
#96299=CARTESIAN_POINT('Ctrl Pts',(3.24611999955075,28.1477069248048,125.889386263714));
#96300=CARTESIAN_POINT('Ctrl Pts',(3.24997877604375,28.1169036007079,125.825233278397));
#96301=CARTESIAN_POINT('Ctrl Pts',(3.25383755253675,28.0894022374881,125.759405667014));
#96302=CARTESIAN_POINT('Ctrl Pts',(3.25769632902976,28.0653812767394,125.692277370791));
#96303=CARTESIAN_POINT('Ctrl Pts',(3.26155267461805,28.041375448421,125.625191363229));
#96304=CARTESIAN_POINT('Ctrl Pts',(3.26540902020635,28.0208458358893,125.556806752784));
#96305=CARTESIAN_POINT('Ctrl Pts',(3.26926536579465,28.0039227637665,125.487517414551));
#96306=CARTESIAN_POINT('Ctrl Pts',(3.27312057204007,27.987004691502,125.418248547593));
#96307=CARTESIAN_POINT('Ctrl Pts',(3.27697577828549,27.9736911594534,125.348075955166));
#96308=CARTESIAN_POINT('Ctrl Pts',(3.28083098453091,27.9640621465046,125.277406955941));
#96309=CARTESIAN_POINT('Ctrl Pts',(3.28468634138225,27.9544327573927,125.20673519599));
#96310=CARTESIAN_POINT('Ctrl Pts',(3.28854169823359,27.9484882365528,125.135567472377));
#96311=CARTESIAN_POINT('Ctrl Pts',(3.29239705508493,27.9462568852957,125.064317814831));
#96312=CARTESIAN_POINT('Ctrl Pts',(3.29625644755358,27.9440231983586,124.99299357629));
#96313=CARTESIAN_POINT('Ctrl Pts',(3.30011584002223,27.9455104551316,124.921587719152));
#96314=CARTESIAN_POINT('Ctrl Pts',(3.30397523249088,27.9506948035853,124.850514969151));
#96315=CARTESIAN_POINT('Ctrl Pts',(3.30783681009441,27.9558820873458,124.779401978739));
#96316=CARTESIAN_POINT('Ctrl Pts',(3.31169838769794,27.9647705692282,124.708622953138));
#96317=CARTESIAN_POINT('Ctrl Pts',(3.31555996530147,27.9772847256459,124.638585443853));
#96318=CARTESIAN_POINT('Ctrl Pts',(3.31942829941643,27.9898207777885,124.568425391587));
#96319=CARTESIAN_POINT('Ctrl Pts',(3.32329663353139,28.0059950596886,124.499009919224));
#96320=CARTESIAN_POINT('Ctrl Pts',(3.32716496764636,28.0256815275713,124.430733689802));
#96321=CARTESIAN_POINT('Ctrl Pts',(3.3294626868165,28.0373749266683,124.390178867869));
#96322=CARTESIAN_POINT('Ctrl Pts',(3.33176040598664,28.0503065279579,124.350025665612));
#96323=CARTESIAN_POINT('Ctrl Pts',(3.33405812515678,28.0644419479985,124.310353286217));
#96324=CARTESIAN_POINT('Ctrl Pts',(3.33792719850497,28.0882442375279,124.243549932798));
#96325=CARTESIAN_POINT('Ctrl Pts',(3.34179627185317,28.1155556601758,124.177849434963));
#96326=CARTESIAN_POINT('Ctrl Pts',(3.34566534520137,28.1462539875549,124.113646073036));
#96327=CARTESIAN_POINT('Ctrl Pts',(3.34952865359713,28.1769065741631,124.049538374669));
#96328=CARTESIAN_POINT('Ctrl Pts',(3.3533919619929,28.2109358404626,123.986923818939));
#96329=CARTESIAN_POINT('Ctrl Pts',(3.35725527038866,28.2481706198596,123.926179072016));
#96330=CARTESIAN_POINT('Ctrl Pts',(3.36111404688156,28.2853617205268,123.865505582488));
#96331=CARTESIAN_POINT('Ctrl Pts',(3.36497282337445,28.3257506124864,123.806697957088));
#96332=CARTESIAN_POINT('Ctrl Pts',(3.36883159986734,28.3691199117396,123.75010892466));
#96333=CARTESIAN_POINT('Ctrl Pts',(3.37268794545553,28.4124618897335,123.693555541496));
#96334=CARTESIAN_POINT('Ctrl Pts',(3.37654429104372,28.4587802551696,123.639218363069));
#96335=CARTESIAN_POINT('Ctrl Pts',(3.3804006366319,28.5078147798201,123.587420504475));
#96336=CARTESIAN_POINT('Ctrl Pts',(3.38425584287721,28.5568348174038,123.535637949365));
#96337=CARTESIAN_POINT('Ctrl Pts',(3.38811104912253,28.6085690872771,123.48639357726));
#96338=CARTESIAN_POINT('Ctrl Pts',(3.39196625536784,28.662718760955,123.439975496924));
#96339=CARTESIAN_POINT('Ctrl Pts',(3.39582161221907,28.7168705500219,123.393555603238));
#96340=CARTESIAN_POINT('Ctrl Pts',(3.3996769690703,28.7734375599752,123.349962535017));
#96341=CARTESIAN_POINT('Ctrl Pts',(3.40353232592153,28.8320872960194,123.309444624279));
#96342=CARTESIAN_POINT('Ctrl Pts',(3.40739171839007,28.8907984240175,123.268884301181));
#96343=CARTESIAN_POINT('Ctrl Pts',(3.41125111085861,28.9515962295857,123.231405837977));
#96344=CARTESIAN_POINT('Ctrl Pts',(3.41511050332715,29.0141193470862,123.197214127881));
#96345=CARTESIAN_POINT('Ctrl Pts',(3.41897208093056,29.076677864315,123.163003058911));
#96346=CARTESIAN_POINT('Ctrl Pts',(3.42283365853398,29.1409632000927,123.13208265822));
#96347=CARTESIAN_POINT('Ctrl Pts',(3.4266952361374,29.2065919913672,123.104610516454));
#96348=CARTESIAN_POINT('Ctrl Pts',(3.43056357025225,29.2723356117929,123.077090307328));
#96349=CARTESIAN_POINT('Ctrl Pts',(3.4344319043671,29.3394269233642,123.053030566895));
#96350=CARTESIAN_POINT('Ctrl Pts',(3.43830023848196,29.4074659908564,123.032539451346));
#96351=CARTESIAN_POINT('Ctrl Pts',(3.44059795765308,29.4478799429921,123.02036810636));
#96352=CARTESIAN_POINT('Ctrl Pts',(3.44289567682421,29.4886280333437,123.00945485306));
#96353=CARTESIAN_POINT('Ctrl Pts',(3.44519339599534,29.529625071522,122.999813761381));
#96354=CARTESIAN_POINT('Ctrl Pts',(3.44906246934355,29.5986589855722,122.983579361925));
#96355=CARTESIAN_POINT('Ctrl Pts',(3.45293154269175,29.6686695703833,122.970891287314));
#96356=CARTESIAN_POINT('Ctrl Pts',(3.45680061603996,29.7392592815909,122.961860691645));
#96357=CARTESIAN_POINT('Ctrl Pts',(3.46066392443573,29.8097438135242,122.95284355164));
#96358=CARTESIAN_POINT('Ctrl Pts',(3.46452723283151,29.8808052810823,122.947473134267));
#96359=CARTESIAN_POINT('Ctrl Pts',(3.46839054122728,29.9520343959943,122.945809925218));
#96360=CARTESIAN_POINT('Ctrl Pts',(3.47224931772019,30.0231799546903,122.944148667218));
#96361=CARTESIAN_POINT('Ctrl Pts',(3.47610809421309,30.0944922868088,122.946185990665));
#96362=CARTESIAN_POINT('Ctrl Pts',(3.47996687070599,30.1655571482086,122.951930569249));
#96363=CARTESIAN_POINT('Ctrl Pts',(3.48382321629418,30.2365772410383,122.957671528934));
#96364=CARTESIAN_POINT('Ctrl Pts',(3.48767956188238,30.3073496893877,122.967115071211));
#96365=CARTESIAN_POINT('Ctrl Pts',(3.49153590747058,30.3774618917446,122.980217813035));
#96366=CARTESIAN_POINT('Ctrl Pts',(3.4953911137159,30.4475533797138,122.993316683703));
#96367=CARTESIAN_POINT('Ctrl Pts',(3.49924631996122,30.5169845316942,123.010072518449));
#96368=CARTESIAN_POINT('Ctrl Pts',(3.50310152620654,30.5853512211257,123.030390518294));
#96369=CARTESIAN_POINT('Ctrl Pts',(3.50695688305778,30.6537205813425,123.050709311873));
#96370=CARTESIAN_POINT('Ctrl Pts',(3.51081223990901,30.7210249314217,123.07459040633));
#96371=CARTESIAN_POINT('Ctrl Pts',(3.51466759676025,30.7868753035814,123.101889144672));
#96372=CARTESIAN_POINT('Ctrl Pts',(3.51852698922879,30.8527946050029,123.129216458128));
#96373=CARTESIAN_POINT('Ctrl Pts',(3.52238638169734,30.9172564406584,123.159968370426));
#96374=CARTESIAN_POINT('Ctrl Pts',(3.52624577416589,30.9798926790898,123.193952409274));
#96375=CARTESIAN_POINT('Ctrl Pts',(3.53010735176932,31.0425643812969,123.227955689417));
#96376=CARTESIAN_POINT('Ctrl Pts',(3.53396892937274,31.1034080141082,123.265194485333));
#96377=CARTESIAN_POINT('Ctrl Pts',(3.53783050697616,31.1620832564081,123.305432188528));
#96378=CARTESIAN_POINT('Ctrl Pts',(3.54169884109102,31.2208611613983,123.345740294686));
#96379=CARTESIAN_POINT('Ctrl Pts',(3.54556717520588,31.2774627151825,123.389057488816));
#96380=CARTESIAN_POINT('Ctrl Pts',(3.54943550932074,31.3315801405306,123.43510642795));
#96381=CARTESIAN_POINT('Ctrl Pts',(3.5517332284918,31.3637248938064,123.462458649116));
#96382=CARTESIAN_POINT('Ctrl Pts',(3.55403094766285,31.3949938940242,123.490773938098));
#96383=CARTESIAN_POINT('Ctrl Pts',(3.5563286668339,31.4253291162108,123.519988353768));
#96384=CARTESIAN_POINT('Ctrl Pts',(3.56013990426075,31.4756462896956,123.568446440295));
#96385=CARTESIAN_POINT('Ctrl Pts',(3.5639511416876,31.5236017843571,123.619581983346));
#96386=CARTESIAN_POINT('Ctrl Pts',(3.56776237911445,31.5688910656204,123.673132114068));
#96387=CARTESIAN_POINT('Ctrl Pts',(3.57156855056505,31.6141201474269,123.72661106484));
#96388=CARTESIAN_POINT('Ctrl Pts',(3.57537472201566,31.656689717376,123.782497865398));
#96389=CARTESIAN_POINT('Ctrl Pts',(3.57918089346626,31.696330794858,123.840491743489));
#96390=CARTESIAN_POINT('Ctrl Pts',(3.58298336737579,31.7359333626423,123.898429282882));
#96391=CARTESIAN_POINT('Ctrl Pts',(3.58678584128533,31.7726127957139,123.958469430919));
#96392=CARTESIAN_POINT('Ctrl Pts',(3.59058831519486,31.8061405313248,124.020278639814));
#96393=CARTESIAN_POINT('Ctrl Pts',(3.59438845464248,31.8396476831728,124.082049902033));
#96394=CARTESIAN_POINT('Ctrl Pts',(3.5981885940901,31.8700067369599,124.145587631282));
#96395=CARTESIAN_POINT('Ctrl Pts',(3.60198873353771,31.8970336521997,124.210531264126));
#96396=CARTESIAN_POINT('Ctrl Pts',(3.60578956781191,31.9240655091052,124.27548677142));
#96397=CARTESIAN_POINT('Ctrl Pts',(3.6095904020861,31.9477638020166,124.341848239274));
#96398=CARTESIAN_POINT('Ctrl Pts',(3.61339123636029,31.9679921061021,124.40923385945));
#96399=CARTESIAN_POINT('Ctrl Pts',(3.61719222217681,31.9882212167064,124.476622166346));
#96400=CARTESIAN_POINT('Ctrl Pts',(3.62099320799334,32.0049799299303,124.545034222851));
#96401=CARTESIAN_POINT('Ctrl Pts',(3.62479419380986,32.0181820637134,124.614074203757));
#96402=CARTESIAN_POINT('Ctrl Pts',(3.62859963984775,32.0313996893825,124.683195198803));
#96403=CARTESIAN_POINT('Ctrl Pts',(3.63240508588563,32.0410523192826,124.752945093908));
#96404=CARTESIAN_POINT('Ctrl Pts',(3.63621053192351,32.047105335722,124.822920054895));
#96405=CARTESIAN_POINT('Ctrl Pts',(3.63944878144608,32.0522561583587,124.88246534387));
#96406=CARTESIAN_POINT('Ctrl Pts',(3.64268703096864,32.0548013150982,124.942173328698));
#96407=CARTESIAN_POINT('Ctrl Pts',(3.6459252804912,32.0547492155205,125.001795499313));
#96408=CARTESIAN_POINT('Origin',(-1.54592528053767,30.,125.));
#96409=CARTESIAN_POINT('',(2.49394332694137,28.7479590808042,126.629230216746));
#96410=CARTESIAN_POINT('',(2.55206159834044,28.7479590808042,126.629230216746));
#96411=CARTESIAN_POINT('',(-1.54592528053767,28.7479590808042,126.629230216746));
#96412=CARTESIAN_POINT('',(3.00407471949958,32.0547499051081,124.999375533621));
#96413=CARTESIAN_POINT('Ctrl Pts',(2.55206159834044,28.7479590808042,126.629230216746));
#96414=CARTESIAN_POINT('Ctrl Pts',(2.55268668349913,28.738868829079,126.622244483847));
#96415=CARTESIAN_POINT('Ctrl Pts',(2.55331176865783,28.729839812397,126.615184797678));
#96416=CARTESIAN_POINT('Ctrl Pts',(2.55393685381652,28.720873281001,126.608052362096));
#96417=CARTESIAN_POINT('Ctrl Pts',(2.55780592716366,28.665373374855,126.563904911101));
#96418=CARTESIAN_POINT('Ctrl Pts',(2.5616750005108,28.612052982777,126.516794349563));
#96419=CARTESIAN_POINT('Ctrl Pts',(2.56554407385794,28.5612455809398,126.466963968247));
#96420=CARTESIAN_POINT('Ctrl Pts',(2.56940738225263,28.5105138825668,126.417207834626));
#96421=CARTESIAN_POINT('Ctrl Pts',(2.57327069064732,28.4622880859468,126.364740262816));
#96422=CARTESIAN_POINT('Ctrl Pts',(2.57713399904201,28.4168691583682,126.309845143814));
#96423=CARTESIAN_POINT('Ctrl Pts',(2.5809927755338,28.3715035100386,126.255014420228));
#96424=CARTESIAN_POINT('Ctrl Pts',(2.58485155202558,28.3289384986386,126.197762178345));
#96425=CARTESIAN_POINT('Ctrl Pts',(2.58871032851737,28.289437480768,126.138408288049));
#96426=CARTESIAN_POINT('Ctrl Pts',(2.59256667410444,28.2499613472646,126.079091788789));
#96427=CARTESIAN_POINT('Ctrl Pts',(2.5964230196915,28.2135456462783,126.01767667131));
#96428=CARTESIAN_POINT('Ctrl Pts',(2.60027936527857,28.1804118450352,125.954513755172));
#96429=CARTESIAN_POINT('Ctrl Pts',(2.60413457152274,28.1472878330499,125.891369500281));
#96430=CARTESIAN_POINT('Ctrl Pts',(2.60798977776692,28.1174440213778,125.826478901844));
#96431=CARTESIAN_POINT('Ctrl Pts',(2.6118449840111,28.0910562596518,125.760217967879));
#96432=CARTESIAN_POINT('Ctrl Pts',(2.61570034086117,28.0646674670723,125.693954445391));
#96433=CARTESIAN_POINT('Ctrl Pts',(2.61955569771125,28.0417351701739,125.626320933222));
#96434=CARTESIAN_POINT('Ctrl Pts',(2.62341105456133,28.0223866848161,125.557712415235));
#96435=CARTESIAN_POINT('Ctrl Pts',(2.62727044702871,28.0030179463183,125.489032080881));
#96436=CARTESIAN_POINT('Ctrl Pts',(2.63112983949609,27.9872406400749,125.419375171884));
#96437=CARTESIAN_POINT('Ctrl Pts',(2.63498923196346,27.9751316358225,125.34914992518));
#96438=CARTESIAN_POINT('Ctrl Pts',(2.63885080956571,27.9630157756187,125.278884917909));
#96439=CARTESIAN_POINT('Ctrl Pts',(2.64271238716795,27.9545724094827,125.208051414956));
#96440=CARTESIAN_POINT('Ctrl Pts',(2.6465739647702,27.9498265305573,125.137063152208));
#96441=CARTESIAN_POINT('Ctrl Pts',(2.65044229888388,27.9450723478793,125.065950682968));
#96442=CARTESIAN_POINT('Ctrl Pts',(2.65431063299756,27.9440285758856,124.994683399202));
#96443=CARTESIAN_POINT('Ctrl Pts',(2.65817896711124,27.946668070431,124.923674712498));
#96444=CARTESIAN_POINT('Ctrl Pts',(2.66047668629252,27.9482358815526,124.881496861081));
#96445=CARTESIAN_POINT('Ctrl Pts',(2.6627744054738,27.9511022049655,124.839410162816));
#96446=CARTESIAN_POINT('Ctrl Pts',(2.66507212465508,27.9552527732088,124.797499775235));
#96447=CARTESIAN_POINT('Ctrl Pts',(2.66894119800399,27.9622418139514,124.726927894671));
#96448=CARTESIAN_POINT('Ctrl Pts',(2.67281027135289,27.9729023830876,124.656580034074));
#96449=CARTESIAN_POINT('Ctrl Pts',(2.6766793447018,27.987210946947,124.586868313476));
#96450=CARTESIAN_POINT('Ctrl Pts',(2.68054265309829,28.0014981909238,124.517260463939));
#96451=CARTESIAN_POINT('Ctrl Pts',(2.68440596149477,28.0194225433456,124.448287344925));
#96452=CARTESIAN_POINT('Ctrl Pts',(2.68826926989126,28.0409087288666,124.380355784446));
#96453=CARTESIAN_POINT('Ctrl Pts',(2.69212804638489,28.0623697097455,124.312503911945));
#96454=CARTESIAN_POINT('Ctrl Pts',(2.69598682287851,28.0873840785132,124.245691631966));
#96455=CARTESIAN_POINT('Ctrl Pts',(2.69984559937214,28.115825933708,124.180313687797));
#96456=CARTESIAN_POINT('Ctrl Pts',(2.70370194496106,28.1442498714517,124.114976929624));
#96457=CARTESIAN_POINT('Ctrl Pts',(2.70755829054999,28.1760968184601,124.051073158967));
#96458=CARTESIAN_POINT('Ctrl Pts',(2.71141463613892,28.2111921518084,123.98897871202));
#96459=CARTESIAN_POINT('Ctrl Pts',(2.71526984238497,28.2462771163718,123.926902610646));
#96460=CARTESIAN_POINT('Ctrl Pts',(2.71912504863103,28.2846083230616,123.866635194417));
#96461=CARTESIAN_POINT('Ctrl Pts',(2.72298025487709,28.3259652456882,123.808528135516));
#96462=CARTESIAN_POINT('Ctrl Pts',(2.72683561172907,28.3673237839476,123.750418806629));
#96463=CARTESIAN_POINT('Ctrl Pts',(2.73069096858105,28.4117079893338,123.694470397125));
#96464=CARTESIAN_POINT('Ctrl Pts',(2.73454632543302,28.4588550702475,123.641004095665));
#96465=CARTESIAN_POINT('Ctrl Pts',(2.73840571790231,28.5060515026436,123.587481828043));
#96466=CARTESIAN_POINT('Ctrl Pts',(2.74226511037161,28.5560162618077,123.536447220084));
#96467=CARTESIAN_POINT('Ctrl Pts',(2.7461245028409,28.6084480614904,123.488186266457));
#96468=CARTESIAN_POINT('Ctrl Pts',(2.74998608044507,28.6609095473362,123.439897988142));
#96469=CARTESIAN_POINT('Ctrl Pts',(2.75384765804924,28.7158404800542,123.394386800424));
#96470=CARTESIAN_POINT('Ctrl Pts',(2.75770923565341,28.7729068174874,123.351898096618));
#96471=CARTESIAN_POINT('Ctrl Pts',(2.76157756976901,28.8300730025479,123.309335051327));
#96472=CARTESIAN_POINT('Ctrl Pts',(2.76544590388462,28.8893816475336,123.269805317836));
#96473=CARTESIAN_POINT('Ctrl Pts',(2.76931423800022,28.950470705352,123.233510310764));
#96474=CARTESIAN_POINT('Ctrl Pts',(2.77161195716469,28.9867564797174,123.211951745545));
#96475=CARTESIAN_POINT('Ctrl Pts',(2.77390967632917,29.0236699387709,123.191533555241));
#96476=CARTESIAN_POINT('Ctrl Pts',(2.77620739549364,29.0611317998039,123.172289939525));
#96477=CARTESIAN_POINT('Ctrl Pts',(2.78007646884175,29.1242129153441,123.139886083632));
#96478=CARTESIAN_POINT('Ctrl Pts',(2.78394554218985,29.1890971270914,123.110688339052));
#96479=CARTESIAN_POINT('Ctrl Pts',(2.78781461553796,29.2554254312378,123.084900453226));
#96480=CARTESIAN_POINT('Ctrl Pts',(2.79167792393363,29.3216549056429,123.059150991572));
#96481=CARTESIAN_POINT('Ctrl Pts',(2.79554123232931,29.3893237522822,123.036801478187));
#96482=CARTESIAN_POINT('Ctrl Pts',(2.79940454072499,29.4580493505793,123.018009319877));
#96483=CARTESIAN_POINT('Ctrl Pts',(2.80326331721779,29.5266943294424,122.999239205947));
#96484=CARTESIAN_POINT('Ctrl Pts',(2.80712209371059,29.5963931313173,122.984018285609));
#96485=CARTESIAN_POINT('Ctrl Pts',(2.8109808702034,29.6667458307424,122.972454878141));
#96486=CARTESIAN_POINT('Ctrl Pts',(2.81483721579149,29.7370542102364,122.960898755248));
#96487=CARTESIAN_POINT('Ctrl Pts',(2.81869356137959,29.8080151917885,122.952995652501));
#96488=CARTESIAN_POINT('Ctrl Pts',(2.82254990696769,29.879217889767,122.948802972811));
#96489=CARTESIAN_POINT('Ctrl Pts',(2.82640511321291,29.9503995511748,122.944611531833));
#96490=CARTESIAN_POINT('Ctrl Pts',(2.83026031945813,30.0218223025503,122.94412836613));
#96491=CARTESIAN_POINT('Ctrl Pts',(2.83411552570336,30.0930710832905,122.947358936405));
#96492=CARTESIAN_POINT('Ctrl Pts',(2.8379708825545,30.1643226474065,122.950589632885));
#96493=CARTESIAN_POINT('Ctrl Pts',(2.84182623940563,30.2353997422065,122.957534329175));
#96494=CARTESIAN_POINT('Ctrl Pts',(2.84568159625677,30.3058899943805,122.968146443801));
#96495=CARTESIAN_POINT('Ctrl Pts',(2.84954098872522,30.376454032638,122.97876966672));
#96496=CARTESIAN_POINT('Ctrl Pts',(2.85340038119368,30.4464295206696,122.993067898798));
#96497=CARTESIAN_POINT('Ctrl Pts',(2.85725977366213,30.515412775057,123.010943129569));
#96498=CARTESIAN_POINT('Ctrl Pts',(2.86112135126546,30.5844350868131,123.02882848105));
#96499=CARTESIAN_POINT('Ctrl Pts',(2.86498292886879,30.6524635830876,123.050294716614));
#96500=CARTESIAN_POINT('Ctrl Pts',(2.86884450647211,30.7191109257999,123.075194285416));
#96501=CARTESIAN_POINT('Ctrl Pts',(2.87271284058688,30.7858748797991,123.100137420407));
#96502=CARTESIAN_POINT('Ctrl Pts',(2.87658117470165,30.8512524097474,123.128525688683));
#96503=CARTESIAN_POINT('Ctrl Pts',(2.88044950881642,30.91487793711,123.160164158766));
#96504=CARTESIAN_POINT('Ctrl Pts',(2.88274722798835,30.9526703277639,123.178956826908));
#96505=CARTESIAN_POINT('Ctrl Pts',(2.88504494716027,30.9898450734053,123.198895338703));
#96506=CARTESIAN_POINT('Ctrl Pts',(2.8873426663322,31.0263304413067,123.219931633968));
#96507=CARTESIAN_POINT('Ctrl Pts',(2.89121173968032,31.0877672636426,123.255354139184));
#96508=CARTESIAN_POINT('Ctrl Pts',(2.89508081302843,31.1474884268371,123.294030383693));
#96509=CARTESIAN_POINT('Ctrl Pts',(2.89894988637655,31.2051280430165,123.335769258055));
#96510=CARTESIAN_POINT('Ctrl Pts',(2.90281319477223,31.262681775674,123.377445941136));
#96511=CARTESIAN_POINT('Ctrl Pts',(2.90667650316791,31.3181597274988,123.422175913362));
#96512=CARTESIAN_POINT('Ctrl Pts',(2.91053981156359,31.3712221345186,123.469723090318));
#96513=CARTESIAN_POINT('Ctrl Pts',(2.91439858805639,31.4242222960094,123.517214491455));
#96514=CARTESIAN_POINT('Ctrl Pts',(2.9182573645492,31.4748121811208,123.567516210344));
#96515=CARTESIAN_POINT('Ctrl Pts',(2.92211614104201,31.5226838808997,123.620351000671));
#96516=CARTESIAN_POINT('Ctrl Pts',(2.92597248663011,31.5705254230521,123.673152506785));
#96517=CARTESIAN_POINT('Ctrl Pts',(2.92982883221821,31.6156518517778,123.728483559245));
#96518=CARTESIAN_POINT('Ctrl Pts',(2.93368517780631,31.6577920907818,123.786030088412));
#96519=CARTESIAN_POINT('Ctrl Pts',(2.93754038405153,31.6999198796098,123.843559615672));
#96520=CARTESIAN_POINT('Ctrl Pts',(2.94139559029676,31.739062943392,123.903302928443));
#96521=CARTESIAN_POINT('Ctrl Pts',(2.94525079654198,31.7749915803893,123.964914277923));
#96522=CARTESIAN_POINT('Ctrl Pts',(2.94910615339311,31.81092162096,124.026528034287));
#96523=CARTESIAN_POINT('Ctrl Pts',(2.95296151024424,31.843636742623,124.09000955149));
#96524=CARTESIAN_POINT('Ctrl Pts',(2.95681686709537,31.8729524240308,124.154987112633));
#96525=CARTESIAN_POINT('Ctrl Pts',(2.96067625956382,31.9022987917995,124.220032689417));
#96526=CARTESIAN_POINT('Ctrl Pts',(2.96453565203227,31.9282384157911,124.286576992501));
#96527=CARTESIAN_POINT('Ctrl Pts',(2.96839504450071,31.9506346954787,124.354227712506));
#96528=CARTESIAN_POINT('Ctrl Pts',(2.97225662210403,31.9730436556314,124.421916735417));
#96529=CARTESIAN_POINT('Ctrl Pts',(2.97611819970736,31.991905149263,124.490712953574));
#96530=CARTESIAN_POINT('Ctrl Pts',(2.97997977731068,32.0071330620026,124.560210921104));
#96531=CARTESIAN_POINT('Ctrl Pts',(2.98384811142543,32.0223876186627,124.629830487592));
#96532=CARTESIAN_POINT('Ctrl Pts',(2.98771644554019,32.0339958221734,124.700153775407));
#96533=CARTESIAN_POINT('Ctrl Pts',(2.99158477965495,32.0419231662915,124.770767922266));
#96534=CARTESIAN_POINT('Ctrl Pts',(2.99388249882688,32.0466318625991,124.812711424103));
#96535=CARTESIAN_POINT('Ctrl Pts',(2.99618021799882,32.0500428972698,124.854757479907));
#96536=CARTESIAN_POINT('Ctrl Pts',(2.99847793717076,32.0521577425026,124.89681975777));
#96537=CARTESIAN_POINT('Ctrl Pts',(3.00034353126794,32.0538748552077,124.930971510628));
#96538=CARTESIAN_POINT('Ctrl Pts',(3.00220912536513,32.054739508502,124.965166482837));
#96539=CARTESIAN_POINT('Ctrl Pts',(3.00407471946232,32.0547499051079,124.999375532937));
#96540=CARTESIAN_POINT('Ctrl Pts',(3.00407471949959,32.0547499051081,124.999375533621));
#96541=CARTESIAN_POINT('Ctrl Pts',(3.00791348792961,32.054771297821,125.069766312486));
#96542=CARTESIAN_POINT('Ctrl Pts',(3.01175225635963,32.0511712983844,125.140303260411));
#96543=CARTESIAN_POINT('Ctrl Pts',(3.01559102478966,32.0439310014569,125.210579257724));
#96544=CARTESIAN_POINT('Ctrl Pts',(3.01950861575714,32.0365420374279,125.282298252323));
#96545=CARTESIAN_POINT('Ctrl Pts',(3.02342620672463,32.0253615175391,125.35374494479));
#96546=CARTESIAN_POINT('Ctrl Pts',(3.02734379769211,32.0104254036408,125.42448469807));
#96547=CARTESIAN_POINT('Ctrl Pts',(3.03117271153805,31.9958273780213,125.493623212796));
#96548=CARTESIAN_POINT('Ctrl Pts',(3.03500162538399,31.9776420963002,125.56208594356));
#96549=CARTESIAN_POINT('Ctrl Pts',(3.03883053922993,31.9559553954509,125.629472837783));
#96550=CARTESIAN_POINT('Ctrl Pts',(3.04265730106928,31.9342808834168,125.696821857808));
#96551=CARTESIAN_POINT('Ctrl Pts',(3.04648406290863,31.9091090062404,125.763095771074));
#96552=CARTESIAN_POINT('Ctrl Pts',(3.05031082474797,31.8805758631139,125.82790819876));
#96553=CARTESIAN_POINT('Ctrl Pts',(3.05413676563474,31.8520488411831,125.89270672228));
#96554=CARTESIAN_POINT('Ctrl Pts',(3.0579627065215,31.8201621840763,125.956043930674));
#96555=CARTESIAN_POINT('Ctrl Pts',(3.06178864740826,31.7850999946552,126.017553719261));
#96556=CARTESIAN_POINT('Ctrl Pts',(3.06577402745835,31.7485766519359,126.081626816984));
#96557=CARTESIAN_POINT('Ctrl Pts',(3.06975940750843,31.7086075443551,126.143716319391));
#96558=CARTESIAN_POINT('Ctrl Pts',(3.07374478755852,31.6654523582138,126.203439240269));
#96559=CARTESIAN_POINT('Ctrl Pts',(3.07757550004208,31.6239719703452,126.260844390013));
#96560=CARTESIAN_POINT('Ctrl Pts',(3.08140621252563,31.5795486186866,126.31606290598));
#96561=CARTESIAN_POINT('Ctrl Pts',(3.08523692500919,31.5324542628075,126.368788330935));
#96562=CARTESIAN_POINT('Ctrl Pts',(3.08907026922176,31.4853275527429,126.421549978663));
#96563=CARTESIAN_POINT('Ctrl Pts',(3.09290361343433,31.4355265377851,126.471814780226));
#96564=CARTESIAN_POINT('Ctrl Pts',(3.09673695764691,31.3833590795965,126.519314062134));
#96565=CARTESIAN_POINT('Ctrl Pts',(3.10057644985358,31.3311079541952,126.566889524341));
#96566=CARTESIAN_POINT('Ctrl Pts',(3.10441594206026,31.2764832013092,126.611690314674));
#96567=CARTESIAN_POINT('Ctrl Pts',(3.10825543426693,31.2198237246501,126.65348953528));
#96568=CARTESIAN_POINT('Ctrl Pts',(3.10870802551439,31.2131448249829,126.65841673929));
#96569=CARTESIAN_POINT('Ctrl Pts',(3.10916061676185,31.2064376818435,126.663302287643));
#96570=CARTESIAN_POINT('Ctrl Pts',(3.10961320800931,31.1997028730531,126.668145850604));
#96571=CARTESIAN_POINT('Ctrl Pts',(3.11348228135751,31.1421289156634,126.709552087396));
#96572=CARTESIAN_POINT('Ctrl Pts',(3.1173513547057,31.0822960432195,126.748055289834));
#96573=CARTESIAN_POINT('Ctrl Pts',(3.1212204280539,31.0205290485858,126.783400690673));
#96574=CARTESIAN_POINT('Ctrl Pts',(3.12508373644967,30.9588540873032,126.818693426561));
#96575=CARTESIAN_POINT('Ctrl Pts',(3.12894704484544,30.8952511424374,126.850837461135));
#96576=CARTESIAN_POINT('Ctrl Pts',(3.13281035324121,30.8300752390276,126.879620349978));
#96577=CARTESIAN_POINT('Ctrl Pts',(3.1366691297341,30.7649757910374,126.90836947469));
#96578=CARTESIAN_POINT('Ctrl Pts',(3.140527906227,30.6983074918774,126.933765090179));
#96579=CARTESIAN_POINT('Ctrl Pts',(3.14438668271989,30.6304497644014,126.955640728014));
#96580=CARTESIAN_POINT('Ctrl Pts',(3.14824302830808,30.5626347851046,126.977502584902));
#96581=CARTESIAN_POINT('Ctrl Pts',(3.15209937389627,30.4936323253551,126.995848714865));
#96582=CARTESIAN_POINT('Ctrl Pts',(3.15595571948446,30.4238402027558,127.010561375593));
#96583=CARTESIAN_POINT('Ctrl Pts',(3.15981092572978,30.3540686999779,127.025269689521));
#96584=CARTESIAN_POINT('Ctrl Pts',(3.16366613197509,30.2835084726011,127.03634656525));
#96585=CARTESIAN_POINT('Ctrl Pts',(3.16752133822041,30.2125691751402,127.043725007989));
#96586=CARTESIAN_POINT('Ctrl Pts',(3.17137669507164,30.1416271063936,127.051103738972));
#96587=CARTESIAN_POINT('Ctrl Pts',(3.17523205192287,30.0703064215698,127.054783702051));
#96588=CARTESIAN_POINT('Ctrl Pts',(3.17908740877411,29.9990218406489,127.054749767175));
#96589=CARTESIAN_POINT('Ctrl Pts',(3.18294680124265,29.9276626421765,127.054715796777));
#96590=CARTESIAN_POINT('Ctrl Pts',(3.18680619371119,29.8563401098298,127.050960168243));
#96591=CARTESIAN_POINT('Ctrl Pts',(3.19066558617973,29.7854680019227,127.043519900637));
#96592=CARTESIAN_POINT('Ctrl Pts',(3.19452716378315,29.7145557672039,127.036075420455));
#96593=CARTESIAN_POINT('Ctrl Pts',(3.19838874138656,29.6440949446598,127.02494222409));
#96594=CARTESIAN_POINT('Ctrl Pts',(3.20225031898998,29.5744904799883,127.010208748085));
#96595=CARTESIAN_POINT('Ctrl Pts',(3.20611865310484,29.5047642300233,126.995449493265));
#96596=CARTESIAN_POINT('Ctrl Pts',(3.20998698721969,29.4358977989483,126.977077507279));
#96597=CARTESIAN_POINT('Ctrl Pts',(3.21385532133455,29.3682816450813,126.955231311778));
#96598=CARTESIAN_POINT('Ctrl Pts',(3.21615304050566,29.328118895845,126.942255074275));
#96599=CARTESIAN_POINT('Ctrl Pts',(3.21845075967677,29.2883969108243,126.928054022522));
#96600=CARTESIAN_POINT('Ctrl Pts',(3.22074847884788,29.2491937605714,126.912665039503));
#96601=CARTESIAN_POINT('Ctrl Pts',(3.22461723641768,29.1831859184435,126.886754020742));
#96602=CARTESIAN_POINT('Ctrl Pts',(3.22848599398749,29.1183916892054,126.857371254928));
#96603=CARTESIAN_POINT('Ctrl Pts',(3.2323547515573,29.0552011749716,126.82465140307));
#96604=CARTESIAN_POINT('Ctrl Pts',(3.23621738607644,28.992110671843,126.791983336651));
#96605=CARTESIAN_POINT('Ctrl Pts',(3.24008002059558,28.9306192709831,126.755988893853));
#96606=CARTESIAN_POINT('Ctrl Pts',(3.24394265511472,28.8710978184853,126.71685102064));
#96607=CARTESIAN_POINT('Ctrl Pts',(3.24667286939206,28.8290264501969,126.689187316061));
#96608=CARTESIAN_POINT('Ctrl Pts',(3.24940308366941,28.7879389222963,126.659954172745));
#96609=CARTESIAN_POINT('Ctrl Pts',(3.25213329794676,28.7479590808042,126.629230216746));
#96610=CARTESIAN_POINT('',(2.94592528057306,32.0547499982312,125.000085258451));
#96611=CARTESIAN_POINT('Ctrl Pts',(2.94592528057306,32.0547499982312,125.000085258451));
#96612=CARTESIAN_POINT('Ctrl Pts',(2.94997591063978,32.0547468813374,125.075203179717));
#96613=CARTESIAN_POINT('Ctrl Pts',(2.9540265407065,32.0506202133333,125.150236380527));
#96614=CARTESIAN_POINT('Ctrl Pts',(2.95807717077322,32.042423424768,125.224731209357));
#96615=CARTESIAN_POINT('Ctrl Pts',(2.96213971866882,32.0342025194797,125.299445218068));
#96616=CARTESIAN_POINT('Ctrl Pts',(2.96620226656442,32.0218876070775,125.37361728161));
#96617=CARTESIAN_POINT('Ctrl Pts',(2.97026481446001,32.0055836153966,125.446801884679));
#96618=CARTESIAN_POINT('Ctrl Pts',(2.9743337120519,31.9892541408419,125.520100874092));
#96619=CARTESIAN_POINT('Ctrl Pts',(2.97840260964378,31.968923266179,125.592408932707));
#96620=CARTESIAN_POINT('Ctrl Pts',(2.98247150723566,31.9447455641367,125.663296504793));
#96621=CARTESIAN_POINT('Ctrl Pts',(2.98655160383586,31.9205013167266,125.734379183905));
#96622=CARTESIAN_POINT('Ctrl Pts',(2.99063170043607,31.8923892325071,125.804033182401));
#96623=CARTESIAN_POINT('Ctrl Pts',(2.99471179703627,31.8606118986796,125.871849141189));
#96624=CARTESIAN_POINT('Ctrl Pts',(2.99669196890455,31.8451895720389,125.90476190453));
#96625=CARTESIAN_POINT('Ctrl Pts',(2.99867214077283,31.8289046141268,125.937242126138));
#96626=CARTESIAN_POINT('Ctrl Pts',(3.0006523126411,31.8117839056016,125.969245398185));
#96627=CARTESIAN_POINT('Ctrl Pts',(3.00452138598921,31.7783316189004,126.031776842507));
#96628=CARTESIAN_POINT('Ctrl Pts',(3.00839045933732,31.7415727162655,126.092696890929));
#96629=CARTESIAN_POINT('Ctrl Pts',(3.01225953268542,31.7016865834987,126.151633767324));
#96630=CARTESIAN_POINT('Ctrl Pts',(3.0161228410811,31.6618598814113,126.210482827268));
#96631=CARTESIAN_POINT('Ctrl Pts',(3.01998614947678,31.6189154684186,126.267354181628));
#96632=CARTESIAN_POINT('Ctrl Pts',(3.02384945787245,31.5730785127423,126.321900735777));
#96633=CARTESIAN_POINT('Ctrl Pts',(3.02770823436526,31.5272953266877,126.3763833034));
#96634=CARTESIAN_POINT('Ctrl Pts',(3.03156701085806,31.4786266488691,126.428546117723));
#96635=CARTESIAN_POINT('Ctrl Pts',(3.03542578735086,31.4273398009013,126.478072615017));
#96636=CARTESIAN_POINT('Ctrl Pts',(3.03928213293896,31.3760852619932,126.527567912215));
#96637=CARTESIAN_POINT('Ctrl Pts',(3.04313847852706,31.3222161738659,126.574429850717));
#96638=CARTESIAN_POINT('Ctrl Pts',(3.04699482411516,31.2660378333257,126.618377510684));
#96639=CARTESIAN_POINT('Ctrl Pts',(3.05085003036038,31.209876090466,126.662312186479));
#96640=CARTESIAN_POINT('Ctrl Pts',(3.05470523660561,31.1514068320782,126.703333993932));
#96641=CARTESIAN_POINT('Ctrl Pts',(3.05856044285083,31.090968332925,126.741202360168));
#96642=CARTESIAN_POINT('Ctrl Pts',(3.06241579970197,31.030527472706,126.779072205754));
#96643=CARTESIAN_POINT('Ctrl Pts',(3.0662711565531,30.9681176318143,126.813788109482));
#96644=CARTESIAN_POINT('Ctrl Pts',(3.07012651340424,30.9041044757288,126.845153830841));
#96645=CARTESIAN_POINT('Ctrl Pts',(3.0739859058727,30.840024313498,126.876552384452));
#96646=CARTESIAN_POINT('Ctrl Pts',(3.07784529834115,30.7743379229772,126.9045935411));
#96647=CARTESIAN_POINT('Ctrl Pts',(3.0817046908096,30.7074330745457,126.929128302508));
#96648=CARTESIAN_POINT('Ctrl Pts',(3.08556626841293,30.6404903455103,126.953676955161));
#96649=CARTESIAN_POINT('Ctrl Pts',(3.08942784601626,30.5723282496367,126.974715117171));
#96650=CARTESIAN_POINT('Ctrl Pts',(3.09328942361959,30.5033492915031,126.992143833473));
#96651=CARTESIAN_POINT('Ctrl Pts',(3.09715775773435,30.43424964251,127.009603044389));
#96652=CARTESIAN_POINT('Ctrl Pts',(3.10102609184912,30.3643307544234,127.023440106453));
#96653=CARTESIAN_POINT('Ctrl Pts',(3.10489442596389,30.2940041844803,127.033607410984));
#96654=CARTESIAN_POINT('Ctrl Pts',(3.10719214513581,30.2522314980318,127.039646602495));
#96655=CARTESIAN_POINT('Ctrl Pts',(3.10948986430774,30.2103150725455,127.044392046685));
#96656=CARTESIAN_POINT('Ctrl Pts',(3.11178758347967,30.16834124311,127.047842471571));
#96657=CARTESIAN_POINT('Ctrl Pts',(3.11565566452761,30.0976806610281,127.053651067882));
#96658=CARTESIAN_POINT('Ctrl Pts',(3.11952374557556,30.0265807189343,127.05580954406));
#96659=CARTESIAN_POINT('Ctrl Pts',(3.1233918266235,29.9554507383329,127.054267004502));
#96660=CARTESIAN_POINT('Ctrl Pts',(3.12725460116857,29.8844183387909,127.052726581106));
#96661=CARTESIAN_POINT('Ctrl Pts',(3.13111737571364,29.8133564636762,127.04749522442));
#96662=CARTESIAN_POINT('Ctrl Pts',(3.13498015025872,29.7426786732666,127.038573839062));
#96663=CARTESIAN_POINT('Ctrl Pts',(3.1388389182363,29.6720741916493,127.029661707191));
#96664=CARTESIAN_POINT('Ctrl Pts',(3.14269768621389,29.6018534835615,127.017067202742));
#96665=CARTESIAN_POINT('Ctrl Pts',(3.14655645419147,29.5324274928773,127.000843200524));
#96666=CARTESIAN_POINT('Ctrl Pts',(3.15049840098558,29.4615049696795,126.984269477019));
#96667=CARTESIAN_POINT('Ctrl Pts',(3.15444034777968,29.3914123463251,126.96390797678));
#96668=CARTESIAN_POINT('Ctrl Pts',(3.15838229457379,29.322578411127,126.939870499139));
#96669=CARTESIAN_POINT('Ctrl Pts',(3.16223769300454,29.2552557759909,126.916360782134));
#96670=CARTESIAN_POINT('Ctrl Pts',(3.1660930914353,29.1891375852841,126.889335068584));
#96671=CARTESIAN_POINT('Ctrl Pts',(3.16994848986605,29.1246090616445,126.858948161608));
#96672=CARTESIAN_POINT('Ctrl Pts',(3.17393371084183,29.0579076738206,126.82753803857));
#96673=CARTESIAN_POINT('Ctrl Pts',(3.17791893181762,28.9929054419377,126.792536500927));
#96674=CARTESIAN_POINT('Ctrl Pts',(3.1819041527934,28.9300023970759,126.754167236109));
#96675=CARTESIAN_POINT('Ctrl Pts',(3.18588937376918,28.8670993522142,126.71579797129));
#96676=CARTESIAN_POINT('Ctrl Pts',(3.18987459474497,28.8062959644687,126.674061306113));
#96677=CARTESIAN_POINT('Ctrl Pts',(3.19385981572075,28.7479590808042,126.629230216746));
#96678=CARTESIAN_POINT('Ctrl Pts',(2.49394332694137,28.7479590808042,126.629230216746));
#96679=CARTESIAN_POINT('Ctrl Pts',(2.49779845423341,28.6914148374794,126.585776746721));
#96680=CARTESIAN_POINT('Ctrl Pts',(2.50165358152545,28.6371225734697,126.539366335534));
#96681=CARTESIAN_POINT('Ctrl Pts',(2.50550870881748,28.5853982276444,126.490268226914));
#96682=CARTESIAN_POINT('Ctrl Pts',(2.50936427936507,28.5336679346476,126.441164473082));
#96683=CARTESIAN_POINT('Ctrl Pts',(2.51321984991265,28.4845064965347,126.3893727446));
#96684=CARTESIAN_POINT('Ctrl Pts',(2.51707542046023,28.4381935061283,126.33519962485));
#96685=CARTESIAN_POINT('Ctrl Pts',(2.52093520681344,28.391829875599,126.280967270457));
#96686=CARTESIAN_POINT('Ctrl Pts',(2.52479499316666,28.3483212234455,126.224348699157));
#96687=CARTESIAN_POINT('Ctrl Pts',(2.52865477951988,28.3079066744851,126.165683379073));
#96688=CARTESIAN_POINT('Ctrl Pts',(2.53251701398007,28.2674664922046,126.106980849941));
#96689=CARTESIAN_POINT('Ctrl Pts',(2.53637924844027,28.2301245723542,126.04622940256));
#96690=CARTESIAN_POINT('Ctrl Pts',(2.54024148290046,28.1960750894974,125.983794937865));
#96691=CARTESIAN_POINT('Ctrl Pts',(2.54411021121953,28.1619683567407,125.921255497512));
#96692=CARTESIAN_POINT('Ctrl Pts',(2.54797893953859,28.1311653163517,125.85702783091));
#96693=CARTESIAN_POINT('Ctrl Pts',(2.55184766785766,28.1038125014745,125.791498915309));
#96694=CARTESIAN_POINT('Ctrl Pts',(2.55326885500073,28.093764375676,125.767426702253));
#96695=CARTESIAN_POINT('Ctrl Pts',(2.5546900421438,28.0841813656411,125.743179040737));
#96696=CARTESIAN_POINT('Ctrl Pts',(2.55611122928687,28.0750690305967,125.718775573828));
#96697=CARTESIAN_POINT('Ctrl Pts',(2.55998030264048,28.0502613950355,125.652339000705));
#96698=CARTESIAN_POINT('Ctrl Pts',(2.56384937599409,28.0288486678213,125.584486481582));
#96699=CARTESIAN_POINT('Ctrl Pts',(2.56771844934771,28.0109912326569,125.51559837658));
#96700=CARTESIAN_POINT('Ctrl Pts',(2.57158175774896,27.9931604052234,125.446812915444));
#96701=CARTESIAN_POINT('Ctrl Pts',(2.57544506615021,27.9788744755237,125.376995397717));
#96702=CARTESIAN_POINT('Ctrl Pts',(2.57930837455146,27.9682450435839,125.306544221245));
#96703=CARTESIAN_POINT('Ctrl Pts',(2.58316715104994,27.9576280806337,125.236175688416));
#96704=CARTESIAN_POINT('Ctrl Pts',(2.58702592754841,27.9506591675626,125.165175451347));
#96705=CARTESIAN_POINT('Ctrl Pts',(2.59088470404688,27.9473991305134,125.09395335589));
#96706=CARTESIAN_POINT('Ctrl Pts',(2.5947410496407,27.9441411471824,125.022776128055));
#96707=CARTESIAN_POINT('Ctrl Pts',(2.59859739523451,27.9445874265103,124.951377803251));
#96708=CARTESIAN_POINT('Ctrl Pts',(2.60245374082833,27.9487469461337,124.880173160335));
#96709=CARTESIAN_POINT('Ctrl Pts',(2.60630894707931,27.9529052368426,124.808989554563));
#96710=CARTESIAN_POINT('Ctrl Pts',(2.6101641533303,27.9607745615594,124.738000001772));
#96711=CARTESIAN_POINT('Ctrl Pts',(2.61401935958128,27.9723118237879,124.667617355222));
#96712=CARTESIAN_POINT('Ctrl Pts',(2.6178747164382,27.9838495367264,124.597231959133));
#96713=CARTESIAN_POINT('Ctrl Pts',(2.62173007329512,27.9990553909046,124.527453995389));
#96714=CARTESIAN_POINT('Ctrl Pts',(2.62558543015203,28.0178349185927,124.458687564756));
#96715=CARTESIAN_POINT('Ctrl Pts',(2.62944482262629,28.0366341038612,124.38984915246));
#96716=CARTESIAN_POINT('Ctrl Pts',(2.63330421510055,28.0590143018045,124.322024856521));
#96717=CARTESIAN_POINT('Ctrl Pts',(2.6371636075748,28.0848309841341,124.255604135445));
#96718=CARTESIAN_POINT('Ctrl Pts',(2.64102518518395,28.1106622835139,124.18914580787));
#96719=CARTESIAN_POINT('Ctrl Pts',(2.64488676279309,28.1399337411178,124.124093080345));
#96720=CARTESIAN_POINT('Ctrl Pts',(2.64874834040224,28.1724535386666,124.060813386931));
#96721=CARTESIAN_POINT('Ctrl Pts',(2.65261667452279,28.2050302353393,123.997422974528));
#96722=CARTESIAN_POINT('Ctrl Pts',(2.65648500864334,28.2408663749926,123.935812209991));
#96723=CARTESIAN_POINT('Ctrl Pts',(2.66035334276388,28.2797256272094,123.87632137832));
#96724=CARTESIAN_POINT('Ctrl Pts',(2.6626510618844,28.3028073063108,123.84098492155));
#96725=CARTESIAN_POINT('Ctrl Pts',(2.66494878100491,28.3269547715516,123.806395821985));
#96726=CARTESIAN_POINT('Ctrl Pts',(2.66724650012542,28.3521119068426,123.772619702403));
#96727=CARTESIAN_POINT('Ctrl Pts',(2.67111557347318,28.3944733951511,123.715744916056));
#96728=CARTESIAN_POINT('Ctrl Pts',(2.67498464682093,28.4398657577249,123.66095438182));
#96729=CARTESIAN_POINT('Ctrl Pts',(2.67885372016868,28.4880564238179,123.608589138701));
#96730=CARTESIAN_POINT('Ctrl Pts',(2.68271702856402,28.5361752854058,123.556301920242));
#96731=CARTESIAN_POINT('Ctrl Pts',(2.68658033695935,28.5870838479015,123.506433174339));
#96732=CARTESIAN_POINT('Ctrl Pts',(2.69044364535469,28.6405079277696,123.45929273772));
#96733=CARTESIAN_POINT('Ctrl Pts',(2.69430242184716,28.6938693378438,123.412207599787));
#96734=CARTESIAN_POINT('Ctrl Pts',(2.69816119833963,28.7497400413977,123.367844733757));
#96735=CARTESIAN_POINT('Ctrl Pts',(2.7020199748321,28.8078086989951,123.326477527994));
#96736=CARTESIAN_POINT('Ctrl Pts',(2.70587632041987,28.8658407752118,123.285136382236));
#96737=CARTESIAN_POINT('Ctrl Pts',(2.70973266600764,28.9260676636479,123.246787433824));
#96738=CARTESIAN_POINT('Ctrl Pts',(2.71358901159541,28.9881457596686,123.211663186415));
#96739=CARTESIAN_POINT('Ctrl Pts',(2.71744421784032,29.0502055149483,123.176549316334));
#96740=CARTESIAN_POINT('Ctrl Pts',(2.72129942408523,29.1141149694304,123.144658494925));
#96741=CARTESIAN_POINT('Ctrl Pts',(2.72515463033013,29.1795038931155,123.116178431728));
#96742=CARTESIAN_POINT('Ctrl Pts',(2.72900998718095,29.2448953712576,123.08769725594));
#96743=CARTESIAN_POINT('Ctrl Pts',(2.73286534403177,29.3117659870952,123.062627294863));
#96744=CARTESIAN_POINT('Ctrl Pts',(2.73672070088259,29.3797250020698,123.041108351786));
#96745=CARTESIAN_POINT('Ctrl Pts',(2.74058009335075,29.4477551535409,123.019566883629));
#96746=CARTESIAN_POINT('Ctrl Pts',(2.74443948581891,29.5168755143521,123.001584000482));
#96747=CARTESIAN_POINT('Ctrl Pts',(2.74829887828707,29.586680496496,122.987249506143));
#96748=CARTESIAN_POINT('Ctrl Pts',(2.75216045589011,29.6565250012597,122.972906895809));
#96749=CARTESIAN_POINT('Ctrl Pts',(2.75602203349315,29.7270544184664,122.962216859222));
#96750=CARTESIAN_POINT('Ctrl Pts',(2.7598836110962,29.7978560154116,122.955217524529));
#96751=CARTESIAN_POINT('Ctrl Pts',(2.7637519452107,29.8687814922449,122.948205943264));
#96752=CARTESIAN_POINT('Ctrl Pts',(2.7676202793252,29.9399796142001,122.9448979791));
#96753=CARTESIAN_POINT('Ctrl Pts',(2.7714886134397,30.0110363158979,122.945279638921));
#96754=CARTESIAN_POINT('Ctrl Pts',(2.77378633261446,30.0532426872075,122.945506337822));
#96755=CARTESIAN_POINT('Ctrl Pts',(2.77608405178923,30.0953992152986,122.947033789851));
#96756=CARTESIAN_POINT('Ctrl Pts',(2.77838177096399,30.1374203322592,122.949850440875));
#96757=CARTESIAN_POINT('Ctrl Pts',(2.78225084431114,30.2081786674968,122.954593330921));
#96758=CARTESIAN_POINT('Ctrl Pts',(2.78611991765828,30.2788297690987,122.963013013947));
#96759=CARTESIAN_POINT('Ctrl Pts',(2.78998899100542,30.3489609773221,122.975099064446));
#96760=CARTESIAN_POINT('Ctrl Pts',(2.79385229940011,30.4189876894441,122.987167106626));
#96761=CARTESIAN_POINT('Ctrl Pts',(2.79771560779481,30.4884955710087,123.002890590709));
#96762=CARTESIAN_POINT('Ctrl Pts',(2.8015789161895,30.5570756073842,123.022207207477));
#96763=CARTESIAN_POINT('Ctrl Pts',(2.80543769268129,30.6255751950785,123.041501164642));
#96764=CARTESIAN_POINT('Ctrl Pts',(2.80929646917308,30.6931486342329,123.06437975107));
#96765=CARTESIAN_POINT('Ctrl Pts',(2.81315524566487,30.7593973800472,123.09072967297));
#96766=CARTESIAN_POINT('Ctrl Pts',(2.81701159125195,30.8256043912887,123.117062995269));
#96767=CARTESIAN_POINT('Ctrl Pts',(2.82086793683902,30.8904879145281,123.146863135292));
#96768=CARTESIAN_POINT('Ctrl Pts',(2.8247242824261,30.9536662545008,123.179967517453));
#96769=CARTESIAN_POINT('Ctrl Pts',(2.82857948867028,31.0168259286689,123.213062119048));
#96770=CARTESIAN_POINT('Ctrl Pts',(2.83243469491446,31.0782809896736,123.249458799357));
#96771=CARTESIAN_POINT('Ctrl Pts',(2.83628990115864,31.1376729351003,123.288948318945));
#96772=CARTESIAN_POINT('Ctrl Pts',(2.84014525800872,31.1970672007082,123.328439381214));
#96773=CARTESIAN_POINT('Ctrl Pts',(2.84400061485879,31.2543977874148,123.371023251837));
#96774=CARTESIAN_POINT('Ctrl Pts',(2.84785597170887,31.3093353178271,123.416447478613));
#96775=CARTESIAN_POINT('Ctrl Pts',(2.85171536417625,31.3643303544203,123.461919253464));
#96776=CARTESIAN_POINT('Ctrl Pts',(2.85557475664364,31.4169269591328,123.510237009373));
#96777=CARTESIAN_POINT('Ctrl Pts',(2.85943414911102,31.4668297075149,123.561108700543));
#96778=CARTESIAN_POINT('Ctrl Pts',(2.86329572671327,31.5167607101459,123.612009194565));
#96779=CARTESIAN_POINT('Ctrl Pts',(2.86715730431552,31.5639944983842,123.665466138182));
#96780=CARTESIAN_POINT('Ctrl Pts',(2.87101888191777,31.608275187717,123.721153456011));
#96781=CARTESIAN_POINT('Ctrl Pts',(2.87488721603145,31.6526333539297,123.776938208628));
#96782=CARTESIAN_POINT('Ctrl Pts',(2.87875555014514,31.6940278230156,123.834960731191));
#96783=CARTESIAN_POINT('Ctrl Pts',(2.88262388425883,31.7322457770094,123.894865559973));
#96784=CARTESIAN_POINT('Ctrl Pts',(2.88492160344006,31.7549465374345,123.930447924396));
#96785=CARTESIAN_POINT('Ctrl Pts',(2.8872193226213,31.7765274453195,123.966693895145));
#96786=CARTESIAN_POINT('Ctrl Pts',(2.88951704180254,31.796951798833,124.003525316342));
#96787=CARTESIAN_POINT('Ctrl Pts',(2.89357123056498,31.8329893551935,124.068512167277));
#96788=CARTESIAN_POINT('Ctrl Pts',(2.89762541932743,31.8655537423432,124.135557009903));
#96789=CARTESIAN_POINT('Ctrl Pts',(2.90167960808987,31.8944168444081,124.204272419654));
#96790=CARTESIAN_POINT('Ctrl Pts',(2.90572241802451,31.9231989368586,124.272794966946));
#96791=CARTESIAN_POINT('Ctrl Pts',(2.90976522795915,31.9483002686216,124.342978361099));
#96792=CARTESIAN_POINT('Ctrl Pts',(2.91380803789379,31.9695390125992,124.414411714299));
#96793=CARTESIAN_POINT('Ctrl Pts',(2.91784402707256,31.9907419240024,124.485724549971));
#96794=CARTESIAN_POINT('Ctrl Pts',(2.92188001625134,32.0080950852903,124.558282753119));
#96795=CARTESIAN_POINT('Ctrl Pts',(2.92591600543012,32.0214649404621,124.63165633305));
#96796=CARTESIAN_POINT('Ctrl Pts',(2.92994364805396,32.0348071463451,124.704878174066));
#96797=CARTESIAN_POINT('Ctrl Pts',(2.9339712906778,32.0441823724021,124.778911624371));
#96798=CARTESIAN_POINT('Ctrl Pts',(2.93799893330165,32.0495074524504,124.853314060489));
#96799=CARTESIAN_POINT('Ctrl Pts',(2.94064104904699,32.0530006814071,124.902121729471));
#96800=CARTESIAN_POINT('Ctrl Pts',(2.94328316479234,32.0547520312806,124.951087882258));
#96801=CARTESIAN_POINT('Ctrl Pts',(2.94592528053768,32.0547499982312,125.000085257794));
#96802=CARTESIAN_POINT('Origin',(-1.54592528053767,30.,125.));
#96803=CARTESIAN_POINT('',(1.79398326352072,28.7479590808042,126.629230216746));
#96804=CARTESIAN_POINT('',(1.85201788434095,28.7479590808042,126.629230216746));
#96805=CARTESIAN_POINT('',(-1.54592528053767,28.7479590808042,126.629230216746));
#96806=CARTESIAN_POINT('',(2.30407471949582,32.0547491423791,125.001877336539));
#96807=CARTESIAN_POINT('Ctrl Pts',(1.85201788434095,28.7479590808042,126.629230216746));
#96808=CARTESIAN_POINT('Ctrl Pts',(1.85587837143644,28.6913998975434,126.585765265587));
#96809=CARTESIAN_POINT('Ctrl Pts',(1.85973885853193,28.6371473338627,126.5393829153));
#96810=CARTESIAN_POINT('Ctrl Pts',(1.86359934562742,28.585503225249,126.490367886369));
#96811=CARTESIAN_POINT('Ctrl Pts',(1.86752032615371,28.5330498588311,126.440584797038));
#96812=CARTESIAN_POINT('Ctrl Pts',(1.87144130668,28.4832877655838,126.388086181911));
#96813=CARTESIAN_POINT('Ctrl Pts',(1.87536228720629,28.4364915744155,126.333206272722));
#96814=CARTESIAN_POINT('Ctrl Pts',(1.87928326773258,28.3896953832472,126.278326363534));
#96815=CARTESIAN_POINT('Ctrl Pts',(1.88320424825887,28.3458653561315,126.221065611797));
#96816=CARTESIAN_POINT('Ctrl Pts',(1.88712522878516,28.3052297563666,126.161788011556));
#96817=CARTESIAN_POINT('Ctrl Pts',(1.89099430204314,28.2651321044353,126.103295148265));
#96818=CARTESIAN_POINT('Ctrl Pts',(1.89486337530113,28.2279876780811,126.042609395796));
#96819=CARTESIAN_POINT('Ctrl Pts',(1.89873244855911,28.1940438570375,125.980061208393));
#96820=CARTESIAN_POINT('Ctrl Pts',(1.902595756863,28.1601506125936,125.917606218353));
#96821=CARTESIAN_POINT('Ctrl Pts',(1.90645906516689,28.1294487370859,125.853294725252));
#96822=CARTESIAN_POINT('Ctrl Pts',(1.91032237347079,28.1021426165629,125.787486453619));
#96823=CARTESIAN_POINT('Ctrl Pts',(1.91418114986976,28.0748685278459,125.721755379249));
#96824=CARTESIAN_POINT('Ctrl Pts',(1.91803992626874,28.0509824669386,125.654531460506));
#96825=CARTESIAN_POINT('Ctrl Pts',(1.92189870266772,28.0306423055256,125.586197776961));
#96826=CARTESIAN_POINT('Ctrl Pts',(1.92575504816078,28.0103149577648,125.517907141455));
#96827=CARTESIAN_POINT('Ctrl Pts',(1.92961139365385,27.9935292159303,125.44850859268));
#96828=CARTESIAN_POINT('Ctrl Pts',(1.93346773914691,27.9803938232411,125.378402501706));
#96829=CARTESIAN_POINT('Ctrl Pts',(1.93732294529604,27.9672623113582,125.308317123334));
#96830=CARTESIAN_POINT('Ctrl Pts',(1.94117815144516,27.9577790969468,125.237525094986));
#96831=CARTESIAN_POINT('Ctrl Pts',(1.94503335759429,27.9520019217323,125.166437477486));
#96832=CARTESIAN_POINT('Ctrl Pts',(1.9488887143484,27.9462245208304,125.095347082923));
#96833=CARTESIAN_POINT('Ctrl Pts',(1.95274407110252,27.9441534837165,125.023961560652));
#96834=CARTESIAN_POINT('Ctrl Pts',(1.95659942785664,27.9457945863574,124.952695866338));
#96835=CARTESIAN_POINT('Ctrl Pts',(1.96045882022731,27.9474374068318,124.881355574254));
#96836=CARTESIAN_POINT('Ctrl Pts',(1.96431821259799,27.9528001125915,124.810135847169));
#96837=CARTESIAN_POINT('Ctrl Pts',(1.96817760496867,27.9618363654228,124.739449503576));
#96838=CARTESIAN_POINT('Ctrl Pts',(1.97203918247366,27.9708777344548,124.668723138357));
#96839=CARTESIAN_POINT('Ctrl Pts',(1.97590075997865,27.9835967043639,124.598531236038));
#96840=CARTESIAN_POINT('Ctrl Pts',(1.97976233748364,27.9998957312151,124.529276645482));
#96841=CARTESIAN_POINT('Ctrl Pts',(1.98363067150023,28.0162232760913,124.459900881794));
#96842=CARTESIAN_POINT('Ctrl Pts',(1.98749900551682,28.03614324824,124.391466170738));
#96843=CARTESIAN_POINT('Ctrl Pts',(1.99136733953341,28.0595083579832,124.324359748266));
#96844=CARTESIAN_POINT('Ctrl Pts',(1.99366505956351,28.0733868080943,124.284499754171));
#96845=CARTESIAN_POINT('Ctrl Pts',(1.99596277959362,28.0884798245971,124.245108027168));
#96846=CARTESIAN_POINT('Ctrl Pts',(1.99826049962372,28.1047487736662,124.206261786494));
#96847=CARTESIAN_POINT('Ctrl Pts',(2.00212957301354,28.1321436508049,124.140849571725));
#96848=CARTESIAN_POINT('Ctrl Pts',(2.00599864640336,28.1629825933744,124.076729146266));
#96849=CARTESIAN_POINT('Ctrl Pts',(2.00986771979318,28.1971221422172,124.014287571136));
#96850=CARTESIAN_POINT('Ctrl Pts',(2.01373102823112,28.2312108228451,123.951939034478));
#96851=CARTESIAN_POINT('Ctrl Pts',(2.01759433666905,28.2685901166468,123.891264805505));
#96852=CARTESIAN_POINT('Ctrl Pts',(2.02145764510699,28.3090686549949,123.832631699514));
#96853=CARTESIAN_POINT('Ctrl Pts',(2.02531642164265,28.3494997094873,123.774067373822));
#96854=CARTESIAN_POINT('Ctrl Pts',(2.02917519817831,28.393022512329,123.717539812924));
#96855=CARTESIAN_POINT('Ctrl Pts',(2.03303397471397,28.4394008455845,123.663389420311));
#96856=CARTESIAN_POINT('Ctrl Pts',(2.03689032034528,28.4857499619907,123.609273140692));
#96857=CARTESIAN_POINT('Ctrl Pts',(2.04074666597658,28.5349507245829,123.55753142635));
#96858=CARTESIAN_POINT('Ctrl Pts',(2.04460301160788,28.58672574257,123.508472784095));
#96859=CARTESIAN_POINT('Ctrl Pts',(2.04845821789659,28.6384854638258,123.459428636028));
#96860=CARTESIAN_POINT('Ctrl Pts',(2.0523134241853,28.6928175781301,123.413066320258));
#96861=CARTESIAN_POINT('Ctrl Pts',(2.05616863047401,28.7494080523871,123.369657292755));
#96862=CARTESIAN_POINT('Ctrl Pts',(2.06002398736886,28.8060007373877,123.326246569451));
#96863=CARTESIAN_POINT('Ctrl Pts',(2.06387934426371,28.8648515707109,123.285789657389));
#96864=CARTESIAN_POINT('Ctrl Pts',(2.06773470115855,28.9256150626758,123.248516466263));
#96865=CARTESIAN_POINT('Ctrl Pts',(2.07159409367074,28.9864421591807,123.211204259207));
#96866=CARTESIAN_POINT('Ctrl Pts',(2.07545348618293,29.0491854960062,123.177082680191));
#96867=CARTESIAN_POINT('Ctrl Pts',(2.07931287869512,29.1134731141439,123.146336696389));
#96868=CARTESIAN_POINT('Ctrl Pts',(2.08317445634226,29.1777971310468,123.115573304634));
#96869=CARTESIAN_POINT('Ctrl Pts',(2.08703603398941,29.2436667210448,123.088189499305));
#96870=CARTESIAN_POINT('Ctrl Pts',(2.09089761163656,29.3106905289069,123.06432182025));
#96871=CARTESIAN_POINT('Ctrl Pts',(2.0947659457948,29.3778316067407,123.040412380481));
#96872=CARTESIAN_POINT('Ctrl Pts',(2.09863427995304,29.4461304687944,123.020031488752));
#96873=CARTESIAN_POINT('Ctrl Pts',(2.10250261411128,29.515181896621,123.003265423464));
#96874=CARTESIAN_POINT('Ctrl Pts',(2.10480033289494,29.5561971647612,122.99330669147));
#96875=CARTESIAN_POINT('Ctrl Pts',(2.10709805167861,29.5974777581921,122.984622339476));
#96876=CARTESIAN_POINT('Ctrl Pts',(2.10939577046228,29.6389378482157,122.977221790445));
#96877=CARTESIAN_POINT('Ctrl Pts',(2.11326484381022,29.7087514957575,122.964760184083));
#96878=CARTESIAN_POINT('Ctrl Pts',(2.11713391715816,29.7793477922384,122.955892707146));
#96879=CARTESIAN_POINT('Ctrl Pts',(2.12100299050609,29.8503237437522,122.950708761348));
#96880=CARTESIAN_POINT('Ctrl Pts',(2.12486629890171,29.9211939404924,122.945532539673));
#96881=CARTESIAN_POINT('Ctrl Pts',(2.12872960729733,29.9924421888402,122.944028989731));
#96882=CARTESIAN_POINT('Ctrl Pts',(2.13259291569295,30.0636565198238,122.946236281851));
#96883=CARTESIAN_POINT('Ctrl Pts',(2.13645169218588,30.1347873119372,122.94844098468));
#96884=CARTESIAN_POINT('Ctrl Pts',(2.14031046867881,30.2058837825211,122.954347867964));
#96885=CARTESIAN_POINT('Ctrl Pts',(2.14416924517173,30.2765318276607,122.963943097359));
#96886=CARTESIAN_POINT('Ctrl Pts',(2.14802559076006,30.3471353668129,122.97353228207));
#96887=CARTESIAN_POINT('Ctrl Pts',(2.15188193634839,30.4172905607548,122.986805137805));
#96888=CARTESIAN_POINT('Ctrl Pts',(2.15573828193672,30.4865877726813,123.003695939498));
#96889=CARTESIAN_POINT('Ctrl Pts',(2.15959348818228,30.5558645110076,123.020581750867));
#96890=CARTESIAN_POINT('Ctrl Pts',(2.16344869442784,30.6242832988505,123.041083271137));
#96891=CARTESIAN_POINT('Ctrl Pts',(2.16730390067339,30.6914457539578,123.065083895402));
#96892=CARTESIAN_POINT('Ctrl Pts',(2.17115925752498,30.7586108328083,123.089085457265));
#96893=CARTESIAN_POINT('Ctrl Pts',(2.17501461437657,30.8245190247689,123.116586228966));
#96894=CARTESIAN_POINT('Ctrl Pts',(2.17886997122817,30.8887897915024,123.147420644339));
#96895=CARTESIAN_POINT('Ctrl Pts',(2.18272936369722,30.953127834039,123.178287335818));
#96896=CARTESIAN_POINT('Ctrl Pts',(2.18658875616628,31.0158245909643,123.21249442626));
#96897=CARTESIAN_POINT('Ctrl Pts',(2.19044814863534,31.0765229260956,123.249829736257));
#96898=CARTESIAN_POINT('Ctrl Pts',(2.19430972623936,31.1372556277899,123.287186184993));
#96899=CARTESIAN_POINT('Ctrl Pts',(2.19817130384338,31.195987255117,123.327674103258));
#96900=CARTESIAN_POINT('Ctrl Pts',(2.2020328814474,31.2523908379861,123.37103875079));
#96901=CARTESIAN_POINT('Ctrl Pts',(2.20590121556301,31.3088931088786,123.414479272426));
#96902=CARTESIAN_POINT('Ctrl Pts',(2.20976954967862,31.3630588335097,123.460806256701));
#96903=CARTESIAN_POINT('Ctrl Pts',(2.21363788379424,31.4145957497104,123.509726056256));
#96904=CARTESIAN_POINT('Ctrl Pts',(2.2159356029631,31.4452077280762,123.53878351557));
#96905=CARTESIAN_POINT('Ctrl Pts',(2.21823332213197,31.4748929468977,123.568755064472));
#96906=CARTESIAN_POINT('Ctrl Pts',(2.22053104130084,31.5035969390997,123.599573705178));
#96907=CARTESIAN_POINT('Ctrl Pts',(2.22435385578604,31.5513530089709,123.650848006972));
#96908=CARTESIAN_POINT('Ctrl Pts',(2.22817667027124,31.5965877387593,123.704680314487));
#96909=CARTESIAN_POINT('Ctrl Pts',(2.23199948475644,31.6390104049229,123.760789584028));
#96910=CARTESIAN_POINT('Ctrl Pts',(2.23581710151328,31.6813753906795,123.816822564032));
#96911=CARTESIAN_POINT('Ctrl Pts',(2.23963471827012,31.7209355935308,123.875125976649));
#96912=CARTESIAN_POINT('Ctrl Pts',(2.24345233502696,31.7574379329582,123.935382944764));
#96913=CARTESIAN_POINT('Ctrl Pts',(2.24726611122817,31.793903550715,123.995579293845));
#96914=CARTESIAN_POINT('Ctrl Pts',(2.25107988742938,31.8273171481452,124.057724877735));
#96915=CARTESIAN_POINT('Ctrl Pts',(2.25489366363059,31.857467826878,124.121472348407));
#96916=CARTESIAN_POINT('Ctrl Pts',(2.25870495117365,31.8875988309556,124.185178221027));
#96917=CARTESIAN_POINT('Ctrl Pts',(2.26251623871672,31.9144709287458,124.250483456992));
#96918=CARTESIAN_POINT('Ctrl Pts',(2.26632752625978,31.9379191584348,124.317016180374));
#96919=CARTESIAN_POINT('Ctrl Pts',(2.27013878558036,31.9613672144904,124.383548411083));
#96920=CARTESIAN_POINT('Ctrl Pts',(2.27395004490095,31.9813912732469,124.451307646262));
#96921=CARTESIAN_POINT('Ctrl Pts',(2.27776130422154,31.9978751103787,124.519903545286));
#96922=CARTESIAN_POINT('Ctrl Pts',(2.28157259449264,32.0143590813727,124.588500001364));
#96923=CARTESIAN_POINT('Ctrl Pts',(2.28538388476374,32.0273026673966,124.657932647783));
#96924=CARTESIAN_POINT('Ctrl Pts',(2.28919517503484,32.036640523058,124.727799812017));
#96925=CARTESIAN_POINT('Ctrl Pts',(2.29300941452528,32.0459856044573,124.79772104025));
#96926=CARTESIAN_POINT('Ctrl Pts',(2.29682365401572,32.0517193372988,124.868076961445));
#96927=CARTESIAN_POINT('Ctrl Pts',(2.30063789350616,32.0538282590476,124.938461029929));
#96928=CARTESIAN_POINT('Ctrl Pts',(2.30178350215821,32.0544616747018,124.959600918503));
#96929=CARTESIAN_POINT('Ctrl Pts',(2.30292911081027,32.054768451596,124.980743347368));
#96930=CARTESIAN_POINT('Ctrl Pts',(2.30407471946232,32.0547491423796,125.001877335921));
#96931=CARTESIAN_POINT('Ctrl Pts',(2.30407471949582,32.0547491423791,125.001877336539));
#96932=CARTESIAN_POINT('Ctrl Pts',(2.30909836680698,32.0546644688522,125.094552705719));
#96933=CARTESIAN_POINT('Ctrl Pts',(2.31412201411815,32.0483061334431,125.186948887716));
#96934=CARTESIAN_POINT('Ctrl Pts',(2.31914566142931,32.0358091348523,125.27835001159));
#96935=CARTESIAN_POINT('Ctrl Pts',(2.32331921166601,32.0254268671101,125.354284319583));
#96936=CARTESIAN_POINT('Ctrl Pts',(2.3274927619027,32.0108086257834,125.429532498928));
#96937=CARTESIAN_POINT('Ctrl Pts',(2.3316663121394,31.9920561093575,125.503696356619));
#96938=CARTESIAN_POINT('Ctrl Pts',(2.33553538549304,31.9746716626628,125.572449669584));
#96939=CARTESIAN_POINT('Ctrl Pts',(2.33940445884669,31.9536895845946,125.640436592137));
#96940=CARTESIAN_POINT('Ctrl Pts',(2.34327353220033,31.9291943064212,125.707253059783));
#96941=CARTESIAN_POINT('Ctrl Pts',(2.34713684060162,31.9047355264217,125.773969970321));
#96942=CARTESIAN_POINT('Ctrl Pts',(2.35100014900292,31.876774102893,125.839519435332));
#96943=CARTESIAN_POINT('Ctrl Pts',(2.35486345740421,31.8454448505431,125.903510302157));
#96944=CARTESIAN_POINT('Ctrl Pts',(2.35872223390271,31.814152349369,125.967426103686));
#96945=CARTESIAN_POINT('Ctrl Pts',(2.36258101040121,31.7795000793208,126.029786504534));
#96946=CARTESIAN_POINT('Ctrl Pts',(2.36643978689972,31.7416711273088,126.090219815816));
#96947=CARTESIAN_POINT('Ctrl Pts',(2.37029613249356,31.7038660063157,126.150615056063));
#96948=CARTESIAN_POINT('Ctrl Pts',(2.37415247808741,31.6628884308627,126.209085204516));
#96949=CARTESIAN_POINT('Ctrl Pts',(2.37800882368126,31.6189669382656,126.265284005788));
#96950=CARTESIAN_POINT('Ctrl Pts',(2.38186402993228,31.5750584221086,126.321466203335));
#96951=CARTESIAN_POINT('Ctrl Pts',(2.38571923618329,31.5282080145169,126.375378003394));
#96952=CARTESIAN_POINT('Ctrl Pts',(2.38957444243431,31.4786859876977,126.426704353497));
#96953=CARTESIAN_POINT('Ctrl Pts',(2.39342979929127,31.4291620262708,126.478032708694));
#96954=CARTESIAN_POINT('Ctrl Pts',(2.39728515614824,31.3769665772944,126.526775065344));
#96955=CARTESIAN_POINT('Ctrl Pts',(2.4011405130052,31.3224071866831,126.572652789114));
#96956=CARTESIAN_POINT('Ctrl Pts',(2.40499990547949,31.2677906857108,126.61857853566));
#96957=CARTESIAN_POINT('Ctrl Pts',(2.40885929795377,31.2108056760759,126.661633350218));
#96958=CARTESIAN_POINT('Ctrl Pts',(2.41271869042806,31.1517925493631,126.701579115331));
#96959=CARTESIAN_POINT('Ctrl Pts',(2.41658026803724,31.0927460102302,126.741547497187));
#96960=CARTESIAN_POINT('Ctrl Pts',(2.42044184564642,31.0316694842483,126.778403074278));
#96961=CARTESIAN_POINT('Ctrl Pts',(2.4243034232556,30.9689297310249,126.811952741888));
#96962=CARTESIAN_POINT('Ctrl Pts',(2.42817175737618,30.9060802035329,126.845561110561));
#96963=CARTESIAN_POINT('Ctrl Pts',(2.43204009149675,30.8415620785549,126.87585181477));
#96964=CARTESIAN_POINT('Ctrl Pts',(2.43590842561733,30.7757632841604,126.902679397442));
#96965=CARTESIAN_POINT('Ctrl Pts',(2.43820614473754,30.7366800138806,126.918614486742));
#96966=CARTESIAN_POINT('Ctrl Pts',(2.44050386385775,30.6971452393366,126.933328680147));
#96967=CARTESIAN_POINT('Ctrl Pts',(2.44280158297796,30.657242440575,126.94679992213));
#96968=CARTESIAN_POINT('Ctrl Pts',(2.44667069996888,30.590050330227,126.96948407477));
#96969=CARTESIAN_POINT('Ctrl Pts',(2.45053981695979,30.5215508422643,126.988729960308));
#96970=CARTESIAN_POINT('Ctrl Pts',(2.45440893395071,30.4521292545118,127.004389358312));
#96971=CARTESIAN_POINT('Ctrl Pts',(2.45827227326041,30.3828113327391,127.020025372426));
#96972=CARTESIAN_POINT('Ctrl Pts',(2.46213561257011,30.3125745144788,127.032085423932));
#96973=CARTESIAN_POINT('Ctrl Pts',(2.46599895187981,30.2418205526408,127.040470627777));
#96974=CARTESIAN_POINT('Ctrl Pts',(2.46985771072421,30.1711504783521,127.048845889928));
#96975=CARTESIAN_POINT('Ctrl Pts',(2.47371646956861,30.099964958548,127.0535549026));
#96976=CARTESIAN_POINT('Ctrl Pts',(2.47757522841301,30.0286755594982,127.054549895911));
#96977=CARTESIAN_POINT('Ctrl Pts',(2.48143153832715,29.9574314036922,127.055544257758));
#96978=CARTESIAN_POINT('Ctrl Pts',(2.48528784824128,29.8860839840186,127.052829270173));
#96979=CARTESIAN_POINT('Ctrl Pts',(2.48914415815541,29.8150481436358,127.046409141234));
#96980=CARTESIAN_POINT('Ctrl Pts',(2.49299931071212,29.7440336225606,127.039990939108));
#96981=CARTESIAN_POINT('Ctrl Pts',(2.49685446326883,29.6733309786274,127.02986984722));
#96982=CARTESIAN_POINT('Ctrl Pts',(2.50070961582553,29.6033514699089,127.016102057456));
#96983=CARTESIAN_POINT('Ctrl Pts',(2.50456490096022,29.533369554608,127.00233379422));
#96984=CARTESIAN_POINT('Ctrl Pts',(2.50842018609492,29.4641113000198,126.984918680344));
#96985=CARTESIAN_POINT('Ctrl Pts',(2.51227547122961,29.3959775787253,126.963963970417));
#96986=CARTESIAN_POINT('Ctrl Pts',(2.51613458281872,29.3277762332291,126.942988462485));
#96987=CARTESIAN_POINT('Ctrl Pts',(2.51999369440783,29.2607021136925,126.918466490122));
#96988=CARTESIAN_POINT('Ctrl Pts',(2.52385280599695,29.1951398065005,126.890554847504));
#96989=CARTESIAN_POINT('Ctrl Pts',(2.52771409532938,29.1295405017061,126.862627454009));
#96990=CARTESIAN_POINT('Ctrl Pts',(2.53157538466181,29.0654551440428,126.831306795806));
#96991=CARTESIAN_POINT('Ctrl Pts',(2.53543667399424,29.0032448093244,126.79679621893));
#96992=CARTESIAN_POINT('Ctrl Pts',(2.53930424299694,28.9409333010456,126.762229517007));
#96993=CARTESIAN_POINT('Ctrl Pts',(2.54317181199964,28.880503313439,126.724462799672));
#96994=CARTESIAN_POINT('Ctrl Pts',(2.54703938100235,28.822287261403,126.683742934015));
#96995=CARTESIAN_POINT('Ctrl Pts',(2.54871345344838,28.7970885154822,126.666117390669));
#96996=CARTESIAN_POINT('Ctrl Pts',(2.55038752589441,28.7723041475986,126.647939064332));
#96997=CARTESIAN_POINT('Ctrl Pts',(2.55206159834044,28.7479590808042,126.629230216746));
#96998=CARTESIAN_POINT('',(2.24592528056747,32.0547491760428,124.998159877295));
#96999=CARTESIAN_POINT('Ctrl Pts',(2.24592528056747,32.0547491760428,124.998159877295));
#97000=CARTESIAN_POINT('Ctrl Pts',(2.24973199310623,32.0548119777186,125.06828655489));
#97001=CARTESIAN_POINT('Ctrl Pts',(2.25353870564499,32.0512805114038,125.138525579216));
#97002=CARTESIAN_POINT('Ctrl Pts',(2.25734541818375,32.0441469197713,125.208472858879));
#97003=CARTESIAN_POINT('Ctrl Pts',(2.26114901952491,32.0370191583699,125.278362971156));
#97004=CARTESIAN_POINT('Ctrl Pts',(2.26495262086607,32.0262951565311,125.347961315228));
#97005=CARTESIAN_POINT('Ctrl Pts',(2.26875622220723,32.0120190903817,125.416865376878));
#97006=CARTESIAN_POINT('Ctrl Pts',(2.2725580718171,31.9977495990097,125.485737705075));
#97007=CARTESIAN_POINT('Ctrl Pts',(2.27635992142697,31.9799313885755,125.553915895173));
#97008=CARTESIAN_POINT('Ctrl Pts',(2.28016177103684,31.9586600142903,125.62100604741));
#97009=CARTESIAN_POINT('Ctrl Pts',(2.28396322582631,31.937390849028,125.688089232365));
#97010=CARTESIAN_POINT('Ctrl Pts',(2.28776468061578,31.9126693846252,125.754084126914));
#97011=CARTESIAN_POINT('Ctrl Pts',(2.29156613540525,31.8846409268587,125.818612325408));
#97012=CARTESIAN_POINT('Ctrl Pts',(2.29537111048262,31.8565865137025,125.883200279403));
#97013=CARTESIAN_POINT('Ctrl Pts',(2.29917608555998,31.8252191922844,125.946318365001));
#97014=CARTESIAN_POINT('Ctrl Pts',(2.30298106063735,31.7907318525525,126.007609544791));
#97015=CARTESIAN_POINT('Ctrl Pts',(2.30678785553278,31.7562280184462,126.068930038517));
#97016=CARTESIAN_POINT('Ctrl Pts',(2.3105946504282,31.7186014651685,126.128421464589));
#97017=CARTESIAN_POINT('Ctrl Pts',(2.31440144532363,31.6780888208102,126.185755232741));
#97018=CARTESIAN_POINT('Ctrl Pts',(2.31821492439134,31.6375050422032,126.243189670562));
#97019=CARTESIAN_POINT('Ctrl Pts',(2.32202840345906,31.5940253663411,126.298458493991));
#97020=CARTESIAN_POINT('Ctrl Pts',(2.32584188252678,31.5479266065822,126.351266362763));
#97021=CARTESIAN_POINT('Ctrl Pts',(2.32850815088777,31.515695758466,126.388188015464));
#97022=CARTESIAN_POINT('Ctrl Pts',(2.33117441924876,31.4821854267664,126.423907392274));
#97023=CARTESIAN_POINT('Ctrl Pts',(2.33384068760975,31.4475000613344,126.458335055787));
#97024=CARTESIAN_POINT('Ctrl Pts',(2.3377097609577,31.3971674598155,126.50829370109));
#97025=CARTESIAN_POINT('Ctrl Pts',(2.34157883430565,31.3441468439275,126.555741393499));
#97026=CARTESIAN_POINT('Ctrl Pts',(2.34544790765359,31.2887188191192,126.600375383386));
#97027=CARTESIAN_POINT('Ctrl Pts',(2.34931121604922,31.2333733825411,126.644942868247));
#97028=CARTESIAN_POINT('Ctrl Pts',(2.35317452444486,31.1756280325353,126.686704670265));
#97029=CARTESIAN_POINT('Ctrl Pts',(2.35703783284049,31.1157998962009,126.7253950719));
#97030=CARTESIAN_POINT('Ctrl Pts',(2.36089660933342,31.0560419420173,126.764040087272));
#97031=CARTESIAN_POINT('Ctrl Pts',(2.36475538582635,30.9942064605435,126.79962059641));
#97032=CARTESIAN_POINT('Ctrl Pts',(2.36861416231929,30.9306419144751,126.831912440463));
#97033=CARTESIAN_POINT('Ctrl Pts',(2.37247050790762,30.8671174120184,126.864183941696));
#97034=CARTESIAN_POINT('Ctrl Pts',(2.37632685349596,30.8018664381098,126.893170668666));
#97035=CARTESIAN_POINT('Ctrl Pts',(2.38018319908429,30.7352632961439,126.918693682651));
#97036=CARTESIAN_POINT('Ctrl Pts',(2.38403840532987,30.668679831825,126.944209155958));
#97037=CARTESIAN_POINT('Ctrl Pts',(2.38789361157544,30.6007454459252,126.966262774158));
#97038=CARTESIAN_POINT('Ctrl Pts',(2.39174881782102,30.5318541249963,126.98472384785));
#97039=CARTESIAN_POINT('Ctrl Pts',(2.39560417467261,30.4629601127853,127.003185642735));
#97040=CARTESIAN_POINT('Ctrl Pts',(2.39945953152421,30.3931095611263,127.01805449086));
#97041=CARTESIAN_POINT('Ctrl Pts',(2.40331488837581,30.3227096288147,127.029250122082));
#97042=CARTESIAN_POINT('Ctrl Pts',(2.40717428084488,30.2522360049596,127.040457472397));
#97043=CARTESIAN_POINT('Ctrl Pts',(2.41103367331395,30.1812123332285,127.047983853952));
#97044=CARTESIAN_POINT('Ctrl Pts',(2.41489306578302,30.1100530375752,127.05180064612));
#97045=CARTESIAN_POINT('Ctrl Pts',(2.41875464338706,30.0388534525067,127.055619599305));
#97046=CARTESIAN_POINT('Ctrl Pts',(2.4226162209911,29.9675185766697,127.055724781301));
#97047=CARTESIAN_POINT('Ctrl Pts',(2.42647779859514,29.8964622309945,127.052139735225));
#97048=CARTESIAN_POINT('Ctrl Pts',(2.43034613271076,29.8252815597013,127.048548416478));
#97049=CARTESIAN_POINT('Ctrl Pts',(2.43421446682637,29.7543808749425,127.041254028392));
#97050=CARTESIAN_POINT('Ctrl Pts',(2.43808280094199,29.6841675808283,127.030331856003));
#97051=CARTESIAN_POINT('Ctrl Pts',(2.44038052011077,29.642462178201,127.023844286907));
#97052=CARTESIAN_POINT('Ctrl Pts',(2.44267823927954,29.6009990972783,127.016077763855));
#97053=CARTESIAN_POINT('Ctrl Pts',(2.44497595844831,29.5598612439062,127.007056411236));
#97054=CARTESIAN_POINT('Ctrl Pts',(2.44884535140177,29.4905844923686,126.991864320432));
#97055=CARTESIAN_POINT('Ctrl Pts',(2.45271474435522,29.4219595270247,126.973051462177));
#97056=CARTESIAN_POINT('Ctrl Pts',(2.45658413730868,29.3543929918247,126.950689404671));
#97057=CARTESIAN_POINT('Ctrl Pts',(2.46044683557572,29.2869433578469,126.928366037204));
#97058=CARTESIAN_POINT('Ctrl Pts',(2.46430953384276,29.2205489728531,126.90250582308));
#97059=CARTESIAN_POINT('Ctrl Pts',(2.46817223210981,29.155604888851,126.873231021195));
#97060=CARTESIAN_POINT('Ctrl Pts',(2.47203108524594,29.0907254535705,126.843985360972));
#97061=CARTESIAN_POINT('Ctrl Pts',(2.47588993838208,29.0272938956955,126.811332054863));
#97062=CARTESIAN_POINT('Ctrl Pts',(2.47974879151821,28.9656875582782,126.775442292895));
#97063=CARTESIAN_POINT('Ctrl Pts',(2.48360488023173,28.9041253546868,126.739578241797));
#97064=CARTESIAN_POINT('Ctrl Pts',(2.48746096894525,28.8443861933981,126.700482583483));
#97065=CARTESIAN_POINT('Ctrl Pts',(2.49131705765877,28.7868233491138,126.658372689188));
#97066=CARTESIAN_POINT('Ctrl Pts',(2.49219248075297,28.7737552256867,126.648812749908));
#97067=CARTESIAN_POINT('Ctrl Pts',(2.49306790384717,28.7607991591468,126.63909763961));
#97068=CARTESIAN_POINT('Ctrl Pts',(2.49394332694137,28.7479590808042,126.629230216746));
#97069=CARTESIAN_POINT('Ctrl Pts',(1.79398326352072,28.7479590808042,126.629230216746));
#97070=CARTESIAN_POINT('Ctrl Pts',(1.797954777718,28.6899760925928,126.584671091147));
#97071=CARTESIAN_POINT('Ctrl Pts',(1.80192629191528,28.6342918285549,126.536949012551));
#97072=CARTESIAN_POINT('Ctrl Pts',(1.80589780611257,28.5812660683278,126.486334953374));
#97073=CARTESIAN_POINT('Ctrl Pts',(1.8097554753957,28.5297603110066,126.437171764806));
#97074=CARTESIAN_POINT('Ctrl Pts',(1.81361314467883,28.4807630703145,126.385280526293));
#97075=CARTESIAN_POINT('Ctrl Pts',(1.81747081396196,28.4345710965617,126.330950754453));
#97076=CARTESIAN_POINT('Ctrl Pts',(1.8213265585967,28.3884021686694,126.276648088542));
#97077=CARTESIAN_POINT('Ctrl Pts',(1.82518230323143,28.3450360446497,126.219909673037));
#97078=CARTESIAN_POINT('Ctrl Pts',(1.82903804786617,28.3047311040181,126.161060262353));
#97079=CARTESIAN_POINT('Ctrl Pts',(1.83289315862884,28.2644327893895,126.102220526325));
#97080=CARTESIAN_POINT('Ctrl Pts',(1.83674826939151,28.2271949327246,126.041270885359));
#97081=CARTESIAN_POINT('Ctrl Pts',(1.84060338015418,28.193233230365,125.978565992993));
#97082=CARTESIAN_POINT('Ctrl Pts',(1.84466139882929,28.1574840052718,125.912560723649));
#97083=CARTESIAN_POINT('Ctrl Pts',(1.8487194175044,28.1253656047626,125.844610853344));
#97084=CARTESIAN_POINT('Ctrl Pts',(1.85277743617951,28.097074105914,125.775158438074));
#97085=CARTESIAN_POINT('Ctrl Pts',(1.85663765466487,28.0701616208867,125.709091345055));
#97086=CARTESIAN_POINT('Ctrl Pts',(1.86049787315022,28.0467117881968,125.641665263829));
#97087=CARTESIAN_POINT('Ctrl Pts',(1.86435809163558,28.0268426842568,125.573278091182));
#97088=CARTESIAN_POINT('Ctrl Pts',(1.86822101007597,28.0069596832569,125.504843086451));
#97089=CARTESIAN_POINT('Ctrl Pts',(1.87208392851635,27.9906625037277,125.435446125403));
#97090=CARTESIAN_POINT('Ctrl Pts',(1.87594684695674,27.9780181876272,125.365495708502));
#97091=CARTESIAN_POINT('Ctrl Pts',(1.87981602070602,27.9653533963072,125.295432019351));
#97092=CARTESIAN_POINT('Ctrl Pts',(1.8836851944553,27.9563533248157,125.224813567457));
#97093=CARTESIAN_POINT('Ctrl Pts',(1.88755436820458,27.9510331570283,125.154053363815));
#97094=CARTESIAN_POINT('Ctrl Pts',(1.88813611355489,27.9502332490703,125.143414291464));
#97095=CARTESIAN_POINT('Ctrl Pts',(1.8887178589052,27.9495164341508,125.132772011345));
#97096=CARTESIAN_POINT('Ctrl Pts',(1.88929960425551,27.9488826622359,125.122127921556));
#97097=CARTESIAN_POINT('Ctrl Pts',(1.89316867791212,27.9446675701536,125.051336178438));
#97098=CARTESIAN_POINT('Ctrl Pts',(1.89703775156872,27.9441134566319,124.980187299026));
#97099=CARTESIAN_POINT('Ctrl Pts',(1.90090682522533,27.9472620012012,124.909091965219));
#97100=CARTESIAN_POINT('Ctrl Pts',(1.90477013393318,27.9504058544156,124.838102563993));
#97101=CARTESIAN_POINT('Ctrl Pts',(1.90863344264103,27.9572413933367,124.767167031359));
#97102=CARTESIAN_POINT('Ctrl Pts',(1.91249675134888,27.9677583681898,124.696698973893));
#97103=CARTESIAN_POINT('Ctrl Pts',(1.91635552815778,27.9782630059839,124.626313579797));
#97104=CARTESIAN_POINT('Ctrl Pts',(1.92021430496668,27.9924404302484,124.556395049738));
#97105=CARTESIAN_POINT('Ctrl Pts',(1.92407308177558,28.0102284935119,124.487353031348));
#97106=CARTESIAN_POINT('Ctrl Pts',(1.92792942768202,28.0280053508806,124.418354507159));
#97107=CARTESIAN_POINT('Ctrl Pts',(1.93178577358846,28.0493882135971,124.350231868445));
#97108=CARTESIAN_POINT('Ctrl Pts',(1.9356421194949,28.074263921432,124.283384260429));
#97109=CARTESIAN_POINT('Ctrl Pts',(1.93949732606024,28.0991322798441,124.216556402255));
#97110=CARTESIAN_POINT('Ctrl Pts',(1.94335253262557,28.1274912653449,124.151003281955));
#97111=CARTESIAN_POINT('Ctrl Pts',(1.94720773919091,28.1591785023363,124.087106919602));
#97112=CARTESIAN_POINT('Ctrl Pts',(1.95106309636345,28.1908669772189,124.023208061078));
#97113=CARTESIAN_POINT('Ctrl Pts',(1.954918453536,28.2258837439318,123.960966523228));
#97114=CARTESIAN_POINT('Ctrl Pts',(1.95877381070854,28.2640198872233,123.900740881073));
#97115=CARTESIAN_POINT('Ctrl Pts',(1.96263320349815,28.3021959497398,123.840452197385));
#97116=CARTESIAN_POINT('Ctrl Pts',(1.96649259628776,28.3434976465376,123.782184032988));
#97117=CARTESIAN_POINT('Ctrl Pts',(1.97035198907737,28.3876725043722,123.726266272197));
#97118=CARTESIAN_POINT('Ctrl Pts',(1.9742135670022,28.431872373405,123.670316851538));
#97119=CARTESIAN_POINT('Ctrl Pts',(1.97807514492703,28.478948321085,123.616720848788));
#97120=CARTESIAN_POINT('Ctrl Pts',(1.98193672285186,28.5286091314708,123.565773213711));
#97121=CARTESIAN_POINT('Ctrl Pts',(1.98580505728517,28.5783568321624,123.514736436803));
#97122=CARTESIAN_POINT('Ctrl Pts',(1.98967339171848,28.6306980683504,123.46635760889));
#97123=CARTESIAN_POINT('Ctrl Pts',(1.9935417261518,28.6853070410347,123.420892661613));
#97124=CARTESIAN_POINT('Ctrl Pts',(1.99583944246589,28.7177437213672,123.393887356648));
#97125=CARTESIAN_POINT('Ctrl Pts',(1.99813715877998,28.7509798858357,123.367909310026));
#97126=CARTESIAN_POINT('Ctrl Pts',(2.00043487509407,28.7849426291869,123.34300478331));
#97127=CARTESIAN_POINT('Ctrl Pts',(2.0043039484699,28.8421317370261,123.301068604913));
#97128=CARTESIAN_POINT('Ctrl Pts',(2.00817302184573,28.9016064736999,123.262014475619));
#97129=CARTESIAN_POINT('Ctrl Pts',(2.01204209522156,28.9630444130083,123.226100151331));
#97130=CARTESIAN_POINT('Ctrl Pts',(2.01590540364639,29.0243908092844,123.190239339681));
#97131=CARTESIAN_POINT('Ctrl Pts',(2.01976871207123,29.087694185809,123.157509289833));
#97132=CARTESIAN_POINT('Ctrl Pts',(2.02363202049606,29.1526014946385,123.128125715864));
#97133=CARTESIAN_POINT('Ctrl Pts',(2.02749079702003,29.2174326631611,123.098776610653));
#97134=CARTESIAN_POINT('Ctrl Pts',(2.03134957354399,29.2838635862665,123.072766383073));
#97135=CARTESIAN_POINT('Ctrl Pts',(2.03520835006796,29.351516394641,123.050264998498));
#97136=CARTESIAN_POINT('Ctrl Pts',(2.03906469568844,29.4191265839505,123.027777789063));
#97137=CARTESIAN_POINT('Ctrl Pts',(2.04292104130893,29.4879566714932,123.008795190075));
#97138=CARTESIAN_POINT('Ctrl Pts',(2.04677738692941,29.5576099439968,122.993438612738));
#97139=CARTESIAN_POINT('Ctrl Pts',(2.0506325932082,29.627242637723,122.978086572441));
#97140=CARTESIAN_POINT('Ctrl Pts',(2.05448779948698,29.6976975594426,122.966358531514));
#97141=CARTESIAN_POINT('Ctrl Pts',(2.05834300576577,29.768565690814,122.958325265124));
#97142=CARTESIAN_POINT('Ctrl Pts',(2.0621983626516,29.8394365907116,122.950291684907));
#97143=CARTESIAN_POINT('Ctrl Pts',(2.06605371953743,29.9107202493668,122.945953218321));
#97144=CARTESIAN_POINT('Ctrl Pts',(2.06990907642327,29.9820021042085,122.945328824788));
#97145=CARTESIAN_POINT('Ctrl Pts',(2.07376846892791,30.0533585737753,122.944703777667));
#97146=CARTESIAN_POINT('Ctrl Pts',(2.07762786143256,30.1247127489968,122.947800568642));
#97147=CARTESIAN_POINT('Ctrl Pts',(2.08148725393721,30.1956505473206,122.95458600136));
#97148=CARTESIAN_POINT('Ctrl Pts',(2.08534883157763,30.2666285096654,122.961375275898));
#97149=CARTESIAN_POINT('Ctrl Pts',(2.08921040921806,30.3371891450725,122.97185727824));
#97150=CARTESIAN_POINT('Ctrl Pts',(2.09307198685849,30.4069267083804,122.98594731536));
#97151=CARTESIAN_POINT('Ctrl Pts',(2.09694032101139,30.4767862898788,123.000062005489));
#97152=CARTESIAN_POINT('Ctrl Pts',(2.10080865516429,30.5458194534001,123.017797213357));
#97153=CARTESIAN_POINT('Ctrl Pts',(2.10467698931718,30.6136344780001,123.039018029173));
#97154=CARTESIAN_POINT('Ctrl Pts',(2.106974708189,30.6539153471434,123.051622800903));
#97155=CARTESIAN_POINT('Ctrl Pts',(2.10927242706081,30.6937667823746,123.065456404862));
#97156=CARTESIAN_POINT('Ctrl Pts',(2.11157014593263,30.7331103758812,123.080482680652));
#97157=CARTESIAN_POINT('Ctrl Pts',(2.11543921919087,30.7993601018102,123.105785063178));
#97158=CARTESIAN_POINT('Ctrl Pts',(2.11930829244911,30.86442813594,123.13457082176));
#97159=CARTESIAN_POINT('Ctrl Pts',(2.12317736570736,30.9279230539306,123.166708869687));
#97160=CARTESIAN_POINT('Ctrl Pts',(2.1270406740115,30.99132336392,123.198799031633));
#97161=CARTESIAN_POINT('Ctrl Pts',(2.13090398231565,31.0531547805624,123.234231350513));
#97162=CARTESIAN_POINT('Ctrl Pts',(2.13476729061979,31.1130445925503,123.272826210975));
#97163=CARTESIAN_POINT('Ctrl Pts',(2.13862606701903,31.1728641500021,123.311375797226));
#97164=CARTESIAN_POINT('Ctrl Pts',(2.14248484341828,31.2307462205748,123.353080294151));
#97165=CARTESIAN_POINT('Ctrl Pts',(2.14634361981752,31.286343066215,123.397714420429));
#97166=CARTESIAN_POINT('Ctrl Pts',(2.15019996531085,31.3419048876177,123.442320428633));
#97167=CARTESIAN_POINT('Ctrl Pts',(2.15405631080419,31.3951839623497,123.489852101205));
#97168=CARTESIAN_POINT('Ctrl Pts',(2.15791265629752,31.4458631245401,123.540041991153));
#97169=CARTESIAN_POINT('Ctrl Pts',(2.16176786244692,31.4965273137473,123.590217052673));
#97170=CARTESIAN_POINT('Ctrl Pts',(2.16562306859632,31.5445927703971,123.643048430764));
#97171=CARTESIAN_POINT('Ctrl Pts',(2.16947827474572,31.5897781963307,123.69823087724));
#97172=CARTESIAN_POINT('Ctrl Pts',(2.17333363150011,31.6349653874489,123.753415479438));
#97173=CARTESIAN_POINT('Ctrl Pts',(2.17718898825451,31.6772720184169,123.810950955116));
#97174=CARTESIAN_POINT('Ctrl Pts',(2.1810443450089,31.716457316747,123.870499295137));
#97175=CARTESIAN_POINT('Ctrl Pts',(2.18490373737986,31.7556836325105,123.930109967721));
#97176=CARTESIAN_POINT('Ctrl Pts',(2.18876312975082,31.7917818258409,123.991737304011));
#97177=CARTESIAN_POINT('Ctrl Pts',(2.19262252212177,31.8245552029329,124.055015410734));
#97178=CARTESIAN_POINT('Ctrl Pts',(2.19648409962704,31.8573471358554,124.118329344641));
#97179=CARTESIAN_POINT('Ctrl Pts',(2.20034567713231,31.8868103043958,124.183295466943));
#97180=CARTESIAN_POINT('Ctrl Pts',(2.20420725463758,31.9127958012473,124.249526959025));
#97181=CARTESIAN_POINT('Ctrl Pts',(2.20807558865445,31.9388267643132,124.315874334795));
#97182=CARTESIAN_POINT('Ctrl Pts',(2.21194392267132,31.9613677535286,124.383491039636));
#97183=CARTESIAN_POINT('Ctrl Pts',(2.21581225668819,31.9803196571083,124.451974801519));
#97184=CARTESIAN_POINT('Ctrl Pts',(2.21810997671586,31.991576743034,124.492652910121));
#97185=CARTESIAN_POINT('Ctrl Pts',(2.22040769674352,32.0015685226665,124.533636707399));
#97186=CARTESIAN_POINT('Ctrl Pts',(2.22270541677119,32.0102828503303,124.574840707302));
#97187=CARTESIAN_POINT('Ctrl Pts',(2.22812785149402,32.0308479637217,124.672078837752));
#97188=CARTESIAN_POINT('Ctrl Pts',(2.23355028621685,32.0443637952467,124.770855989235));
#97189=CARTESIAN_POINT('Ctrl Pts',(2.23897272093967,32.0506537437881,124.870320450387));
#97190=CARTESIAN_POINT('Ctrl Pts',(2.24129024080568,32.0533420344631,124.912831034002));
#97191=CARTESIAN_POINT('Ctrl Pts',(2.24360776067168,32.0547109424816,124.955466879361));
#97192=CARTESIAN_POINT('Ctrl Pts',(2.24592528053768,32.0547491760423,124.998159876746));
#97193=CARTESIAN_POINT('Origin',(-1.54592528053767,30.,125.));
#97194=CARTESIAN_POINT('',(1.09386069726047,28.7479590808042,126.629230216746));
#97195=CARTESIAN_POINT('',(1.15210970476697,28.7479590808042,126.629230216746));
#97196=CARTESIAN_POINT('',(-1.54592528053767,28.7479590808042,126.629230216746));
#97197=CARTESIAN_POINT('',(1.60407471941017,32.0547499336679,124.999477896888));
#97198=CARTESIAN_POINT('Ctrl Pts',(1.15210970476697,28.7479590808042,126.629230216746));
#97199=CARTESIAN_POINT('Ctrl Pts',(1.15596511927351,28.6914303187086,126.585788643832));
#97200=CARTESIAN_POINT('Ctrl Pts',(1.15982053378006,28.637140397984,126.539382594661));
#97201=CARTESIAN_POINT('Ctrl Pts',(1.16367594828661,28.5854082337326,126.490277724892));
#97202=CARTESIAN_POINT('Ctrl Pts',(1.16753113318894,28.5336791503234,126.441175779499));
#97203=CARTESIAN_POINT('Ctrl Pts',(1.17138631809126,28.484507872185,126.389375668203));
#97204=CARTESIAN_POINT('Ctrl Pts',(1.17524150299359,28.4381775077876,126.335180911083));
#97205=CARTESIAN_POINT('Ctrl Pts',(1.17910047930994,28.3918015794037,126.280932855672));
#97206=CARTESIAN_POINT('Ctrl Pts',(1.18295945562628,28.3482724622444,126.224285820236));
#97207=CARTESIAN_POINT('Ctrl Pts',(1.18681843194263,28.3078333058655,126.165576870808));
#97208=CARTESIAN_POINT('Ctrl Pts',(1.19067925186039,28.2673748299366,126.106839873552));
#97209=CARTESIAN_POINT('Ctrl Pts',(1.19454007177816,28.2300095104467,126.046039414369));
#97210=CARTESIAN_POINT('Ctrl Pts',(1.19840089169592,28.1959359058974,125.983539682407));
#97211=CARTESIAN_POINT('Ctrl Pts',(1.20226883009373,28.1617994773162,125.920924715054));
#97212=CARTESIAN_POINT('Ctrl Pts',(1.20613676849153,28.13096710053,125.856604654191));
#97213=CARTESIAN_POINT('Ctrl Pts',(1.21000470688934,28.1035900889946,125.790965872804));
#97214=CARTESIAN_POINT('Ctrl Pts',(1.21344100584417,28.0792681928189,125.732651997897));
#97215=CARTESIAN_POINT('Ctrl Pts',(1.21687730479899,28.057672865426,125.673297805368));
#97216=CARTESIAN_POINT('Ctrl Pts',(1.22031360375381,28.0388768364194,125.613183088292));
#97217=CARTESIAN_POINT('Ctrl Pts',(1.22418267030568,28.0177136349363,125.545497521882));
#97218=CARTESIAN_POINT('Ctrl Pts',(1.22805173685754,28.0000172088715,125.476582456488));
#97219=CARTESIAN_POINT('Ctrl Pts',(1.23192080340941,27.9859270510232,125.406826398726));
#97220=CARTESIAN_POINT('Ctrl Pts',(1.23578410489414,27.9718578880855,125.337174280337));
#97221=CARTESIAN_POINT('Ctrl Pts',(1.23964740637886,27.9613844225443,125.266684129265));
#97222=CARTESIAN_POINT('Ctrl Pts',(1.24351070786359,27.9545964560466,125.19575981427));
#97223=CARTESIAN_POINT('Ctrl Pts',(1.24736947730855,27.9478164525138,125.124918700603));
#97224=CARTESIAN_POINT('Ctrl Pts',(1.25122824675351,27.9447134062291,125.053644915922));
#97225=CARTESIAN_POINT('Ctrl Pts',(1.25508701619847,27.9453257982332,124.982351003036));
#97226=CARTESIAN_POINT('Ctrl Pts',(1.25894335465805,27.9459378044365,124.911102004587));
#97227=CARTESIAN_POINT('Ctrl Pts',(1.26279969311762,27.950260600879,124.839833387712));
#97228=CARTESIAN_POINT('Ctrl Pts',(1.2666560315772,27.9582806287272,124.768959805511));
#97229=CARTESIAN_POINT('Ctrl Pts',(1.27051123062385,27.966298286938,124.698107163972));
#97230=CARTESIAN_POINT('Ctrl Pts',(1.27436642967051,27.9780109532406,124.627649807831));
#97231=CARTESIAN_POINT('Ctrl Pts',(1.27822162871716,27.9933531760644,124.557997639724));
#97232=CARTESIAN_POINT('Ctrl Pts',(1.28207697831025,28.0086959980057,124.488342751684));
#97233=CARTESIAN_POINT('Ctrl Pts',(1.28593232790333,28.0276685512144,124.419493588044));
#97234=CARTESIAN_POINT('Ctrl Pts',(1.28978767749641,28.0501545639622,124.351848522286));
#97235=CARTESIAN_POINT('Ctrl Pts',(1.29364706266578,28.0726641138803,124.284132649247));
#97236=CARTESIAN_POINT('Ctrl Pts',(1.29750644783515,28.0986943113096,124.217623852034));
#97237=CARTESIAN_POINT('Ctrl Pts',(1.30136583300452,28.1280796929401,124.15270316505));
#97238=CARTESIAN_POINT('Ctrl Pts',(1.30522740327461,28.1574817119403,124.087745721371));
#97239=CARTESIAN_POINT('Ctrl Pts',(1.30908897354469,28.190242473519,124.024378609592));
#97240=CARTESIAN_POINT('Ctrl Pts',(1.31295054381478,28.2261504901487,123.962958304165));
#97241=CARTESIAN_POINT('Ctrl Pts',(1.31681887062171,28.2621213345455,123.901430532467));
#97242=CARTESIAN_POINT('Ctrl Pts',(1.32068719742865,28.3012501615227,123.841856774067));
#97243=CARTESIAN_POINT('Ctrl Pts',(1.32455552423558,28.3432825113791,123.78456397725));
#97244=CARTESIAN_POINT('Ctrl Pts',(1.32685330768785,28.3682496981706,123.750532095502));
#97245=CARTESIAN_POINT('Ctrl Pts',(1.3291510911401,28.3942405723508,123.717304389099));
#97246=CARTESIAN_POINT('Ctrl Pts',(1.33144887459237,28.421195531819,123.684943341999));
#97247=CARTESIAN_POINT('Ctrl Pts',(1.33531795015252,28.4665830877268,123.630452856262));
#97248=CARTESIAN_POINT('Ctrl Pts',(1.33918702571268,28.5148838644452,123.578208140637));
#97249=CARTESIAN_POINT('Ctrl Pts',(1.34305610127283,28.5658471139435,123.528537101414));
#97250=CARTESIAN_POINT('Ctrl Pts',(1.34691941190361,28.6167344281107,123.478940072126));
#97251=CARTESIAN_POINT('Ctrl Pts',(1.35078272253439,28.6702759954471,123.431909443606));
#97252=CARTESIAN_POINT('Ctrl Pts',(1.35464603316517,28.7261812109882,123.387739706108));
#97253=CARTESIAN_POINT('Ctrl Pts',(1.35850481191629,28.7820208465816,123.343621782185));
#97254=CARTESIAN_POINT('Ctrl Pts',(1.3623635906674,28.8402182435544,123.302358382856));
#97255=CARTESIAN_POINT('Ctrl Pts',(1.36622236941852,28.9004476752037,123.26420558604));
#97256=CARTESIAN_POINT('Ctrl Pts',(1.37007871727802,28.9606391644807,123.226076824111));
#97257=CARTESIAN_POINT('Ctrl Pts',(1.37393506513752,29.0228597393117,123.191055036286));
#97258=CARTESIAN_POINT('Ctrl Pts',(1.37779141299703,29.0867536756516,123.159353723943));
#97259=CARTESIAN_POINT('Ctrl Pts',(1.38164662152332,29.1506287349384,123.127661777548));
#97260=CARTESIAN_POINT('Ctrl Pts',(1.38550183004962,29.2161757393154,123.099288574846));
#97261=CARTESIAN_POINT('Ctrl Pts',(1.38935703857592,29.2830148112008,123.074401443306));
#97262=CARTESIAN_POINT('Ctrl Pts',(1.39321239771438,29.3498564943008,123.049513339495));
#97263=CARTESIAN_POINT('Ctrl Pts',(1.39706775685283,29.4179898891058,123.028111744681));
#97264=CARTESIAN_POINT('Ctrl Pts',(1.40092311599129,29.4870172412722,123.01031503706));
#97265=CARTESIAN_POINT('Ctrl Pts',(1.40478251074077,29.5561168480673,122.992499700672));
#97266=CARTESIAN_POINT('Ctrl Pts',(1.40864190549024,29.6261118088308,122.978296905618));
#97267=CARTESIAN_POINT('Ctrl Pts',(1.41250130023971,29.6965922568846,122.967774297988));
#97268=CARTESIAN_POINT('Ctrl Pts',(1.41636288012395,29.767112609972,122.957245732606));
#97269=CARTESIAN_POINT('Ctrl Pts',(1.42022446000818,29.8381185137698,122.950401549224));
#97270=CARTESIAN_POINT('Ctrl Pts',(1.42408603989241,29.9091957736597,122.947257406546));
#97271=CARTESIAN_POINT('Ctrl Pts',(1.42795437626303,29.9803973952236,122.94410776266));
#97272=CARTESIAN_POINT('Ctrl Pts',(1.43182271263365,30.051670136221,122.944671080859));
#97273=CARTESIAN_POINT('Ctrl Pts',(1.43569104900427,30.1226013017354,122.948910903127));
#97274=CARTESIAN_POINT('Ctrl Pts',(1.43798874781315,30.1647327088573,122.951429255628));
#97275=CARTESIAN_POINT('Ctrl Pts',(1.44028644662203,30.2067437115844,122.955243712156));
#97276=CARTESIAN_POINT('Ctrl Pts',(1.44258414543092,30.2485494980138,122.960338089404));
#97277=CARTESIAN_POINT('Ctrl Pts',(1.44645321925177,30.3189458759938,122.96891646424));
#97278=CARTESIAN_POINT('Ctrl Pts',(1.45032229307263,30.3890355122788,122.981160384508));
#97279=CARTESIAN_POINT('Ctrl Pts',(1.45419136689349,30.4584069220931,122.997037030727));
#97280=CARTESIAN_POINT('Ctrl Pts',(1.45805467577754,30.5276749682054,123.012890020675));
#97281=CARTESIAN_POINT('Ctrl Pts',(1.4619179846616,30.5962264424015,123.03236488487));
#97282=CARTESIAN_POINT('Ctrl Pts',(1.46578129354566,30.6636563171689,123.055377194626));
#97283=CARTESIAN_POINT('Ctrl Pts',(1.46964007054779,30.7310070928427,123.078362509628));
#97284=CARTESIAN_POINT('Ctrl Pts',(1.47349884754992,30.7972384249955,123.10487687149));
#97285=CARTESIAN_POINT('Ctrl Pts',(1.47735762455205,30.8619585091962,123.134785510746));
#97286=CARTESIAN_POINT('Ctrl Pts',(1.48121397066214,30.9266378220495,123.164675308624));
#97287=CARTESIAN_POINT('Ctrl Pts',(1.48507031677223,30.9898073358345,123.19795493829));
#97288=CARTESIAN_POINT('Ctrl Pts',(1.48892666288232,31.051094747024,123.234441336212));
#97289=CARTESIAN_POINT('Ctrl Pts',(1.49278186966143,31.1123640512688,123.270916954477));
#97290=CARTESIAN_POINT('Ctrl Pts',(1.49663707644054,31.1717519396523,123.310597211745));
#97291=CARTESIAN_POINT('Ctrl Pts',(1.50049228321965,31.228911801337,123.353253708966));
#97292=CARTESIAN_POINT('Ctrl Pts',(1.50434764061583,31.2860738961709,123.395911872712));
#97293=CARTESIAN_POINT('Ctrl Pts',(1.50820299801202,31.3410074034804,123.441546214958));
#97294=CARTESIAN_POINT('Ctrl Pts',(1.51205835540821,31.3933971411248,123.489886769277));
#97295=CARTESIAN_POINT('Ctrl Pts',(1.5159177484351,31.4458417182073,123.538277924514));
#97296=CARTESIAN_POINT('Ctrl Pts',(1.51977714146198,31.4957368524949,123.589380616532));
#97297=CARTESIAN_POINT('Ctrl Pts',(1.52363653448887,31.542803414801,123.642887187527));
#97298=CARTESIAN_POINT('Ctrl Pts',(1.52749811265903,31.5898966256451,123.696424053318));
#97299=CARTESIAN_POINT('Ctrl Pts',(1.53135969082919,31.6341577748484,123.752367126364));
#97300=CARTESIAN_POINT('Ctrl Pts',(1.53522126899934,31.6753490627772,123.810376916687));
#97301=CARTESIAN_POINT('Ctrl Pts',(1.53908960368816,31.7166124221993,123.868488205468));
#97302=CARTESIAN_POINT('Ctrl Pts',(1.54295793837697,31.7547949361307,123.928673020824));
#97303=CARTESIAN_POINT('Ctrl Pts',(1.54682627306579,31.7897034038552,123.990564866507));
#97304=CARTESIAN_POINT('Ctrl Pts',(1.54912398746702,31.8104383442023,124.027327400411));
#97305=CARTESIAN_POINT('Ctrl Pts',(1.55142170186825,31.8300190525612,124.064691745954));
#97306=CARTESIAN_POINT('Ctrl Pts',(1.55371941626948,31.8484131256698,124.102577870035));
#97307=CARTESIAN_POINT('Ctrl Pts',(1.5579156915312,31.8820058967761,124.171768629842));
#97308=CARTESIAN_POINT('Ctrl Pts',(1.56211196679292,31.9117555498864,124.242941993056));
#97309=CARTESIAN_POINT('Ctrl Pts',(1.56630824205465,31.9374426338775,124.315665576685));
#97310=CARTESIAN_POINT('Ctrl Pts',(1.57045672473028,31.9628371602797,124.3875608905));
#97311=CARTESIAN_POINT('Ctrl Pts',(1.57460520740591,31.9842610035269,124.460970953717));
#97312=CARTESIAN_POINT('Ctrl Pts',(1.57875369008154,32.001547918388,124.535453454542));
#97313=CARTESIAN_POINT('Ctrl Pts',(1.58297386163631,32.0191335640494,124.611223068613));
#97314=CARTESIAN_POINT('Ctrl Pts',(1.58719403319109,32.0324377308413,124.688102209905));
#97315=CARTESIAN_POINT('Ctrl Pts',(1.59141420474586,32.0413368923456,124.765604491407));
#97316=CARTESIAN_POINT('Ctrl Pts',(1.59563437630063,32.05023605385,124.843106772909));
#97317=CARTESIAN_POINT('Ctrl Pts',(1.5998545478554,32.0547300516731,124.921231805861));
#97318=CARTESIAN_POINT('Ctrl Pts',(1.60407471941017,32.0547499336679,124.999477896888));
#97319=CARTESIAN_POINT('Ctrl Pts',(1.60407471946232,32.0547499336682,124.999477897855));
#97320=CARTESIAN_POINT('Ctrl Pts',(1.60804279144016,32.0547686279415,125.073049817185));
#97321=CARTESIAN_POINT('Ctrl Pts',(1.61201086341801,32.0508315372123,125.146579353464));
#97322=CARTESIAN_POINT('Ctrl Pts',(1.61597893539585,32.0429783696597,125.219629104635));
#97323=CARTESIAN_POINT('Ctrl Pts',(1.6200519147052,32.0349175811625,125.294610134902));
#97324=CARTESIAN_POINT('Ctrl Pts',(1.62412489401455,32.0227307791439,125.369085155989));
#97325=CARTESIAN_POINT('Ctrl Pts',(1.6281978733239,32.0065169291057,125.442591657978));
#97326=CARTESIAN_POINT('Ctrl Pts',(1.63217761780328,31.9906742313461,125.514415517928));
#97327=CARTESIAN_POINT('Ctrl Pts',(1.63615736228266,31.9709871018473,125.585314321767));
#97328=CARTESIAN_POINT('Ctrl Pts',(1.64013710676205,31.9475982431018,125.654872999876));
#97329=CARTESIAN_POINT('Ctrl Pts',(1.64425670348638,31.9233874762115,125.726876040265));
#97330=CARTESIAN_POINT('Ctrl Pts',(1.64837630021071,31.8952101842859,125.79744252895));
#97331=CARTESIAN_POINT('Ctrl Pts',(1.65249589693504,31.8632776562454,125.86613736684));
#97332=CARTESIAN_POINT('Ctrl Pts',(1.65661549365937,31.831345128205,125.93483220473));
#97333=CARTESIAN_POINT('Ctrl Pts',(1.66073509038371,31.7956576771194,126.001654970645));
#97334=CARTESIAN_POINT('Ctrl Pts',(1.66485468710804,31.7564763038383,126.066202868386));
#97335=CARTESIAN_POINT('Ctrl Pts',(1.66872376076561,31.719677648685,126.126825445671));
#97336=CARTESIAN_POINT('Ctrl Pts',(1.67259283442317,31.6796647620033,126.185659440821));
#97337=CARTESIAN_POINT('Ctrl Pts',(1.67646190808074,31.6366369540205,126.242343367686));
#97338=CARTESIAN_POINT('Ctrl Pts',(1.68032521678957,31.593673257794,126.298942835076));
#97339=CARTESIAN_POINT('Ctrl Pts',(1.68418852549839,31.5477038485901,126.353398209488));
#97340=CARTESIAN_POINT('Ctrl Pts',(1.68805183420721,31.4989724111852,126.405375136042));
#97341=CARTESIAN_POINT('Ctrl Pts',(1.6919106110171,31.4502981387562,126.457291090462));
#97342=CARTESIAN_POINT('Ctrl Pts',(1.69576938782699,31.3988686045674,126.50673401938));
#97343=CARTESIAN_POINT('Ctrl Pts',(1.69962816463688,31.3449679266251,126.553402342875));
#97344=CARTESIAN_POINT('Ctrl Pts',(1.70348451054431,31.2911012043367,126.600041266862));
#97345=CARTESIAN_POINT('Ctrl Pts',(1.70734085645174,31.234766793229,126.643908736025));
#97346=CARTESIAN_POINT('Ctrl Pts',(1.71119720235918,31.176284794844,126.68474082396));
#97347=CARTESIAN_POINT('Ctrl Pts',(1.71505240892552,31.1178200747181,126.725560848228));
#97348=CARTESIAN_POINT('Ctrl Pts',(1.71890761549186,31.0572094250554,126.763346993699));
#97349=CARTESIAN_POINT('Ctrl Pts',(1.7227628220582,30.9948036856758,126.797877412246));
#97350=CARTESIAN_POINT('Ctrl Pts',(1.72661817923176,30.9323955083583,126.832409179757));
#97351=CARTESIAN_POINT('Ctrl Pts',(1.73047353640531,30.8681925282185,126.863684734564));
#97352=CARTESIAN_POINT('Ctrl Pts',(1.73432889357887,30.8025705279352,126.891527982925));
#97353=CARTESIAN_POINT('Ctrl Pts',(1.73818828636949,30.7368798374496,126.919400376366));
#97354=CARTESIAN_POINT('Ctrl Pts',(1.7420476791601,30.6697676098064,126.943833101219));
#97355=CARTESIAN_POINT('Ctrl Pts',(1.74590707195072,30.6016291345085,126.964698436659));
#97356=CARTESIAN_POINT('Ctrl Pts',(1.74976864987655,30.5334520801414,126.985575585766));
#97357=CARTESIAN_POINT('Ctrl Pts',(1.75363022780239,30.4642480929311,127.002881206742));
#97358=CARTESIAN_POINT('Ctrl Pts',(1.75749180572823,30.3944244572758,127.01653834826));
#97359=CARTESIAN_POINT('Ctrl Pts',(1.76136014016254,30.3244786529126,127.030219385344));
#97360=CARTESIAN_POINT('Ctrl Pts',(1.76522847459685,30.2539115166146,127.040239129505));
#97361=CARTESIAN_POINT('Ctrl Pts',(1.76909680903117,30.183136583751,127.046572391632));
#97362=CARTESIAN_POINT('Ctrl Pts',(1.77139452533631,30.1410976339142,127.050334227612));
#97363=CARTESIAN_POINT('Ctrl Pts',(1.77369224164145,30.0989854134141,127.052796422884));
#97364=CARTESIAN_POINT('Ctrl Pts',(1.7759899579466,30.0568861986886,127.053962395688));
#97365=CARTESIAN_POINT('Ctrl Pts',(1.77985822425496,29.986011054718,127.055925341811));
#97366=CARTESIAN_POINT('Ctrl Pts',(1.78372649056332,29.914895393203,127.054219342807));
#97367=CARTESIAN_POINT('Ctrl Pts',(1.78759475687167,29.8439507547856,127.048815803231));
#97368=CARTESIAN_POINT('Ctrl Pts',(1.79145765803481,29.7731045140113,127.043419758168));
#97369=CARTESIAN_POINT('Ctrl Pts',(1.79532055919795,29.7024293057619,127.034336383239));
#97370=CARTESIAN_POINT('Ctrl Pts',(1.79918346036109,29.6323380715102,127.021589045489));
#97371=CARTESIAN_POINT('Ctrl Pts',(1.8030422966023,29.5623205941017,127.008855121732));
#97372=CARTESIAN_POINT('Ctrl Pts',(1.8069011328435,29.4928863465248,126.992464974017));
#97373=CARTESIAN_POINT('Ctrl Pts',(1.81075996908471,29.4244428158648,126.972493723765));
#97374=CARTESIAN_POINT('Ctrl Pts',(1.81461644855455,29.3560410868629,126.952534670886));
#97375=CARTESIAN_POINT('Ctrl Pts',(1.81847292802439,29.2886293399383,126.928998989315));
#97376=CARTESIAN_POINT('Ctrl Pts',(1.82232940749423,29.2226029680551,126.902012465055));
#97377=CARTESIAN_POINT('Ctrl Pts',(1.8261844651669,29.1566009386091,126.875035890118));
#97378=CARTESIAN_POINT('Ctrl Pts',(1.83003952283957,29.0919837179562,126.844611186077));
#97379=CARTESIAN_POINT('Ctrl Pts',(1.83389458051224,29.0291279358746,126.81091275262));
#97380=CARTESIAN_POINT('Ctrl Pts',(1.83775080895684,28.9662530646401,126.777204085027));
#97381=CARTESIAN_POINT('Ctrl Pts',(1.84160703740144,28.9051411295302,126.740219930772));
#97382=CARTESIAN_POINT('Ctrl Pts',(1.84546326584604,28.8461441294545,126.700180635258));
#97383=CARTESIAN_POINT('Ctrl Pts',(1.84764813867768,28.8127174420926,126.677495057829));
#97384=CARTESIAN_POINT('Ctrl Pts',(1.84983301150931,28.7799691924376,126.653829545424));
#97385=CARTESIAN_POINT('Ctrl Pts',(1.85201788434095,28.7479590808042,126.629230216746));
#97386=CARTESIAN_POINT('',(1.54592528048733,32.0547497262092,125.0010607277));
#97387=CARTESIAN_POINT('Ctrl Pts',(1.54592528053768,32.0547497262087,125.001060728624));
#97388=CARTESIAN_POINT('Ctrl Pts',(1.54924811760506,32.0547182468784,125.062039704689));
#97389=CARTESIAN_POINT('Ctrl Pts',(1.55257095467244,32.0519724942774,125.122946605602));
#97390=CARTESIAN_POINT('Ctrl Pts',(1.55589379173983,32.0465301533583,125.183607989737));
#97391=CARTESIAN_POINT('Ctrl Pts',(1.55976286729383,32.0401931504359,125.25424144954));
#97392=CARTESIAN_POINT('Ctrl Pts',(1.56363194284784,32.0301827024085,125.324684804482));
#97393=CARTESIAN_POINT('Ctrl Pts',(1.56750101840185,32.0165185363462,125.39452573436));
#97394=CARTESIAN_POINT('Ctrl Pts',(1.5713643290264,32.0028747299156,125.464262601128));
#97395=CARTESIAN_POINT('Ctrl Pts',(1.57522763965095,31.9855881042439,125.533398351708));
#97396=CARTESIAN_POINT('Ctrl Pts',(1.5790909502755,31.9647301747385,125.601525479903));
#97397=CARTESIAN_POINT('Ctrl Pts',(1.58294972902032,31.9438967127526,125.669572691161));
#97398=CARTESIAN_POINT('Ctrl Pts',(1.58680850776514,31.9195004099013,125.736613167962));
#97399=CARTESIAN_POINT('Ctrl Pts',(1.59066728650996,31.8916635171442,125.802251020819));
#97400=CARTESIAN_POINT('Ctrl Pts',(1.59452363436312,31.8638441606273,125.867847524193));
#97401=CARTESIAN_POINT('Ctrl Pts',(1.59837998221628,31.8325887036063,125.932042710504));
#97402=CARTESIAN_POINT('Ctrl Pts',(1.60223633006943,31.7980682864068,125.994458646661));
#97403=CARTESIAN_POINT('Ctrl Pts',(1.60609153858935,31.7635580680431,126.056856142429));
#97404=CARTESIAN_POINT('Ctrl Pts',(1.60994674710926,31.7257850395042,126.11747500677));
#97405=CARTESIAN_POINT('Ctrl Pts',(1.61380195562917,31.6849664701856,126.175961545651));
#97406=CARTESIAN_POINT('Ctrl Pts',(1.61765731476124,31.6441463062003,126.234450369437));
#97407=CARTESIAN_POINT('Ctrl Pts',(1.6215126738933,31.6002806450424,126.290806305275));
#97408=CARTESIAN_POINT('Ctrl Pts',(1.62536803302536,31.5536293012231,126.34470575104));
#97409=CARTESIAN_POINT('Ctrl Pts',(1.62922742776844,31.5069291249422,126.398661616244));
#97410=CARTESIAN_POINT('Ctrl Pts',(1.63308682251151,31.4574377637294,126.450155490342));
#97411=CARTESIAN_POINT('Ctrl Pts',(1.63694621725458,31.4054538501172,126.498898608209));
#97412=CARTESIAN_POINT('Ctrl Pts',(1.64080779713241,31.3534405039478,126.54766932374));
#97413=CARTESIAN_POINT('Ctrl Pts',(1.64466937701023,31.2989321673928,126.593685869142));
#97414=CARTESIAN_POINT('Ctrl Pts',(1.64853095688806,31.2422606024531,126.636699776408));
#97415=CARTESIAN_POINT('Ctrl Pts',(1.65239929325233,31.1854898810355,126.679788943771));
#97416=CARTESIAN_POINT('Ctrl Pts',(1.6562676296166,31.126548776353,126.719864710759));
#97417=CARTESIAN_POINT('Ctrl Pts',(1.66013596598087,31.065797460298,126.756722327553));
#97418=CARTESIAN_POINT('Ctrl Pts',(1.66243366484671,31.0297126380765,126.778614866445));
#97419=CARTESIAN_POINT('Ctrl Pts',(1.66473136371255,30.9929896379703,126.799372895742));
#97420=CARTESIAN_POINT('Ctrl Pts',(1.66702906257839,30.9557074212992,126.818961485951));
#97421=CARTESIAN_POINT('Ctrl Pts',(1.67089813639883,30.8929282422543,126.851946531418));
#97422=CARTESIAN_POINT('Ctrl Pts',(1.67476721021927,30.8283164347397,126.881742253029));
#97423=CARTESIAN_POINT('Ctrl Pts',(1.67863628403971,30.7622291057691,126.908141596638));
#97424=CARTESIAN_POINT('Ctrl Pts',(1.68249959292333,30.6962402472061,126.93450160511));
#97425=CARTESIAN_POINT('Ctrl Pts',(1.68636290180695,30.6287806786634,126.957475102026));
#97426=CARTESIAN_POINT('Ctrl Pts',(1.69022621069057,30.5602315508614,126.976901153806));
#97427=CARTESIAN_POINT('Ctrl Pts',(1.69408498769223,30.4917628351015,126.996304417718));
#97428=CARTESIAN_POINT('Ctrl Pts',(1.69794376469388,30.4222075639637,127.012168370547));
#97429=CARTESIAN_POINT('Ctrl Pts',(1.70180254169554,30.3519646456321,127.024381004338));
#97430=CARTESIAN_POINT('Ctrl Pts',(1.70565888780513,30.2817659778371,127.036585944604));
#97431=CARTESIAN_POINT('Ctrl Pts',(1.70951523391472,30.2108809997711,127.045144046379));
#97432=CARTESIAN_POINT('Ctrl Pts',(1.71337158002432,30.1397200495256,127.049994114689));
#97433=CARTESIAN_POINT('Ctrl Pts',(1.71722678680292,30.0685801232945,127.05484275008));
#97434=CARTESIAN_POINT('Ctrl Pts',(1.72108199358152,29.997164871149,127.05598549389));
#97435=CARTESIAN_POINT('Ctrl Pts',(1.72493720036013,29.9258892856538,127.053413052583));
#97436=CARTESIAN_POINT('Ctrl Pts',(1.72879255775578,29.8546109155301,127.050840510775));
#97437=CARTESIAN_POINT('Ctrl Pts',(1.73264791515144,29.7834727082802,127.044552515403));
#97438=CARTESIAN_POINT('Ctrl Pts',(1.73650327254709,29.7128874498955,127.034591837709));
#97439=CARTESIAN_POINT('Ctrl Pts',(1.74036266557341,29.6422283057451,127.024620733584));
#97440=CARTESIAN_POINT('Ctrl Pts',(1.74422205859973,29.5721237478891,127.010969340842));
#97441=CARTESIAN_POINT('Ctrl Pts',(1.74808145162605,29.5029783477431,126.993731937771));
#97442=CARTESIAN_POINT('Ctrl Pts',(1.75194302979563,29.4337937982791,126.976484775084));
#97443=CARTESIAN_POINT('Ctrl Pts',(1.7558046079652,29.3655699524173,126.95564770222));
#97444=CARTESIAN_POINT('Ctrl Pts',(1.75966618613478,29.298695494437,126.931364686686));
#97445=CARTESIAN_POINT('Ctrl Pts',(1.76353452082299,29.2317040276841,126.907039183692));
#97446=CARTESIAN_POINT('Ctrl Pts',(1.7674028555112,29.1660671101076,126.879255889797));
#97447=CARTESIAN_POINT('Ctrl Pts',(1.77127119019941,29.10215210493,126.848206352066));
#97448=CARTESIAN_POINT('Ctrl Pts',(1.77356890460526,29.064187854165,126.829763539878));
#97449=CARTESIAN_POINT('Ctrl Pts',(1.7758666190111,29.0268306375569,126.810169233755));
#97450=CARTESIAN_POINT('Ctrl Pts',(1.77816433341695,28.9901526281511,126.789470829064));
#97451=CARTESIAN_POINT('Ctrl Pts',(1.78203306929966,28.9283966802693,126.754620257234));
#97452=CARTESIAN_POINT('Ctrl Pts',(1.78590180518237,28.8683259744342,126.716500811269));
#97453=CARTESIAN_POINT('Ctrl Pts',(1.78977054106508,28.8103080527618,126.675300162113));
#97454=CARTESIAN_POINT('Ctrl Pts',(1.79117478188363,28.7892492014239,126.660345501199));
#97455=CARTESIAN_POINT('Ctrl Pts',(1.79257902270217,28.7684606010765,126.644985351916));
#97456=CARTESIAN_POINT('Ctrl Pts',(1.79398326352072,28.7479590808042,126.629230216746));
#97457=CARTESIAN_POINT('Ctrl Pts',(1.09386069726047,28.7479590808042,126.629230216746));
#97458=CARTESIAN_POINT('Ctrl Pts',(1.09772924549863,28.6914573570451,126.58580942242));
#97459=CARTESIAN_POINT('Ctrl Pts',(1.1015977937368,28.6372927651895,126.539504229736));
#97460=CARTESIAN_POINT('Ctrl Pts',(1.10546634197497,28.5857569445798,126.490608648404));
#97461=CARTESIAN_POINT('Ctrl Pts',(1.10742846411185,28.5596180500294,126.465808879441));
#97462=CARTESIAN_POINT('Ctrl Pts',(1.10939058624872,28.5341547936423,126.440343296117));
#97463=CARTESIAN_POINT('Ctrl Pts',(1.1113527083856,28.5094012387782,126.414253476412));
#97464=CARTESIAN_POINT('Ctrl Pts',(1.11522172486416,28.460590866645,126.362808186406));
#97465=CARTESIAN_POINT('Ctrl Pts',(1.11909074134271,28.4143512962968,126.308732231128));
#97466=CARTESIAN_POINT('Ctrl Pts',(1.12295975782127,28.3709788742317,126.252312953818));
#97467=CARTESIAN_POINT('Ctrl Pts',(1.12682300843003,28.3276710886807,126.195977756328));
#97468=CARTESIAN_POINT('Ctrl Pts',(1.13068625903878,28.2872222636681,126.13730655068));
#97469=CARTESIAN_POINT('Ctrl Pts',(1.13454950964754,28.249890900826,126.076622358809));
#97470=CARTESIAN_POINT('Ctrl Pts',(1.13840822727143,28.2126033411229,126.01600937136));
#97471=CARTESIAN_POINT('Ctrl Pts',(1.14226694489532,28.1784262310649,125.953388501099));
#97472=CARTESIAN_POINT('Ctrl Pts',(1.14612566251921,28.1475758185352,125.889113161765));
#97473=CARTESIAN_POINT('Ctrl Pts',(1.14998194860246,28.1167448461508,125.824878325033));
#97474=CARTESIAN_POINT('Ctrl Pts',(1.15383823468571,28.0892366220044,125.75899152456));
#97475=CARTESIAN_POINT('Ctrl Pts',(1.15769452076896,28.0652216033881,125.691830989841));
#97476=CARTESIAN_POINT('Ctrl Pts',(1.16154966696221,28.0412136834359,125.624690307285));
#97477=CARTESIAN_POINT('Ctrl Pts',(1.16540481315546,28.0206970825669,125.55627709514));
#97478=CARTESIAN_POINT('Ctrl Pts',(1.16925995934871,28.0037935776479,125.486988174251));
#97479=CARTESIAN_POINT('Ctrl Pts',(1.17311525568896,27.9868894143853,125.417696554755));
#97480=CARTESIAN_POINT('Ctrl Pts',(1.17697055202921,27.9735987394515,125.347529631285));
#97481=CARTESIAN_POINT('Ctrl Pts',(1.18082584836946,27.9639926264908,125.276896257678));
#97482=CARTESIAN_POINT('Ctrl Pts',(1.18468518004213,27.9543764588272,125.206188952234));
#97483=CARTESIAN_POINT('Ctrl Pts',(1.1885445117148,27.9484526174281,125.135014704389));
#97484=CARTESIAN_POINT('Ctrl Pts',(1.19240384338747,27.9462403758186,125.063788467469));
#97485=CARTESIAN_POINT('Ctrl Pts',(1.19626535994249,27.9440268817932,124.99252190726));
#97486=CARTESIAN_POINT('Ctrl Pts',(1.2001268764975,27.9455291602523,124.921203785309));
#97487=CARTESIAN_POINT('Ctrl Pts',(1.20398839305252,27.9507143478077,124.850247276423));
#97488=CARTESIAN_POINT('Ctrl Pts',(1.2078566663814,27.9559086082595,124.779166609818));
#97489=CARTESIAN_POINT('Ctrl Pts',(1.21172493971028,27.9647985833273,124.708449301724));
#97490=CARTESIAN_POINT('Ctrl Pts',(1.21559321303916,27.977299825455,124.638500945512));
#97491=CARTESIAN_POINT('Ctrl Pts',(1.21789146843416,27.9847271825007,124.59694256187));
#97492=CARTESIAN_POINT('Ctrl Pts',(1.22018972382915,27.9934283053086,124.555655389018));
#97493=CARTESIAN_POINT('Ctrl Pts',(1.22248797922415,28.0033771870154,124.514721827021));
#97494=CARTESIAN_POINT('Ctrl Pts',(1.22635706753339,28.0201260226695,124.445810614402));
#97495=CARTESIAN_POINT('Ctrl Pts',(1.23022615584263,28.0404794416406,124.3776325501));
#97496=CARTESIAN_POINT('Ctrl Pts',(1.23409524415187,28.0643567448886,124.310592463458));
#97497=CARTESIAN_POINT('Ctrl Pts',(1.2379585676327,28.0881984716531,124.243652264583));
#97498=CARTESIAN_POINT('Ctrl Pts',(1.24182189111353,28.1155534989662,124.177847131634));
#97499=CARTESIAN_POINT('Ctrl Pts',(1.24568521459436,28.1462906273317,124.113569447626));
#97500=CARTESIAN_POINT('Ctrl Pts',(1.24954400628193,28.1769917001321,124.049367163252));
#97501=CARTESIAN_POINT('Ctrl Pts',(1.25340279796949,28.2110667850215,123.986689204937));
#97502=CARTESIAN_POINT('Ctrl Pts',(1.25726158965706,28.2483362327094,123.925908938283));
#97503=CARTESIAN_POINT('Ctrl Pts',(1.2611179504991,28.2855822025117,123.865166960153));
#97504=CARTESIAN_POINT('Ctrl Pts',(1.26497431134114,28.3260182894283,123.806320715076));
#97505=CARTESIAN_POINT('Ctrl Pts',(1.26883067218318,28.36941916093,123.749718555781));
#97506=CARTESIAN_POINT('Ctrl Pts',(1.27268589371849,28.4128072102641,123.693133118785));
#97507=CARTESIAN_POINT('Ctrl Pts',(1.2765411152538,28.4591580098432,123.638790836655));
#97508=CARTESIAN_POINT('Ctrl Pts',(1.28039633678911,28.5082042059661,123.587009245818));
#97509=CARTESIAN_POINT('Ctrl Pts',(1.28425170894349,28.5572523182675,123.535225631934));
#97510=CARTESIAN_POINT('Ctrl Pts',(1.28810708109787,28.6089957005272,123.48600325914));
#97511=CARTESIAN_POINT('Ctrl Pts',(1.29196245325224,28.6631293906798,123.439623591425));
#97512=CARTESIAN_POINT('Ctrl Pts',(1.2958218609375,28.7173197441505,123.393195376755));
#97513=CARTESIAN_POINT('Ctrl Pts',(1.29968126862277,28.7739050304206,123.349616123726));
#97514=CARTESIAN_POINT('Ctrl Pts',(1.30354067630803,28.8325470690385,123.309127084465));
#97515=CARTESIAN_POINT('Ctrl Pts',(1.30740226910233,28.8912223094478,123.268615121229));
#97516=CARTESIAN_POINT('Ctrl Pts',(1.31126386189663,28.9519562065549,123.231197109626));
#97517=CARTESIAN_POINT('Ctrl Pts',(1.31512545469094,29.0143837973087,123.197069534482));
#97518=CARTESIAN_POINT('Ctrl Pts',(1.3189938037899,29.0769206123762,123.162882249185));
#97519=CARTESIAN_POINT('Ctrl Pts',(1.32286215288887,29.1411565994881,123.131997104933));
#97520=CARTESIAN_POINT('Ctrl Pts',(1.32673050198783,29.2067051879891,123.104563136441));
#97521=CARTESIAN_POINT('Ctrl Pts',(1.32902808467946,29.2456373780649,123.088268895783));
#97522=CARTESIAN_POINT('Ctrl Pts',(1.33132566737108,29.2850322712179,123.073191185541));
#97523=CARTESIAN_POINT('Ctrl Pts',(1.33362325006271,29.3248066099531,123.059352827396));
#97524=CARTESIAN_POINT('Ctrl Pts',(1.33749232926375,29.3917857299198,123.036049333741));
#97525=CARTESIAN_POINT('Ctrl Pts',(1.34136140846479,29.4601038938102,123.016171823725));
#97526=CARTESIAN_POINT('Ctrl Pts',(1.34523048766583,29.5293772204397,122.999872063627));
#97527=CARTESIAN_POINT('Ctrl Pts',(1.34909380207173,29.5985473321916,122.983596589612));
#97528=CARTESIAN_POINT('Ctrl Pts',(1.35295711647764,29.668669312732,122.970888394534));
#97529=CARTESIAN_POINT('Ctrl Pts',(1.35682043088354,29.7393423478386,122.961850066636));
#97530=CARTESIAN_POINT('Ctrl Pts',(1.36067921359172,29.8099324829276,122.952822340768));
#97531=CARTESIAN_POINT('Ctrl Pts',(1.36453799629991,29.88107190911,122.94745599265));
#97532=CARTESIAN_POINT('Ctrl Pts',(1.36839677900809,29.9523495120027,122.945802591401));
#97533=CARTESIAN_POINT('Ctrl Pts',(1.37225313093495,30.0235822146564,122.944150231687));
#97534=CARTESIAN_POINT('Ctrl Pts',(1.37610948286181,30.0949524368243,122.946206189712));
#97535=CARTESIAN_POINT('Ctrl Pts',(1.37996583478866,30.1660453015422,122.951970088027));
#97536=CARTESIAN_POINT('Ctrl Pts',(1.38382104748671,30.2371171642766,122.957732283594));
#97537=CARTESIAN_POINT('Ctrl Pts',(1.38767626018475,30.3079113482947,122.967200205572));
#97538=CARTESIAN_POINT('Ctrl Pts',(1.3915314728828,30.3780160759691,122.980321459041));
#97539=CARTESIAN_POINT('Ctrl Pts',(1.39538683629162,30.4481235442284,122.993443225456));
#97540=CARTESIAN_POINT('Ctrl Pts',(1.39924219970043,30.5175410255454,123.010218515374));
#97541=CARTESIAN_POINT('Ctrl Pts',(1.40309756310925,30.5858666509226,123.030543773059));
#97542=CARTESIAN_POINT('Ctrl Pts',(1.40695696225114,30.6542637984771,123.0508903069));
#97543=CARTESIAN_POINT('Ctrl Pts',(1.41081636139302,30.7215663419588,123.074794087784));
#97544=CARTESIAN_POINT('Ctrl Pts',(1.41467576053491,30.7873881796827,123.102101842301));
#97545=CARTESIAN_POINT('Ctrl Pts',(1.41853734488708,30.8532472860464,123.1294250586));
#97546=CARTESIAN_POINT('Ctrl Pts',(1.42239892923925,30.9176235790874,123.16015587591));
#97547=CARTESIAN_POINT('Ctrl Pts',(1.42626051359142,30.9801540422591,123.194094239462));
#97548=CARTESIAN_POINT('Ctrl Pts',(1.43012885450178,31.0427939140761,123.228091984477));
#97549=CARTESIAN_POINT('Ctrl Pts',(1.43399719541214,31.1035810935558,123.265308226916));
#97550=CARTESIAN_POINT('Ctrl Pts',(1.4378655363225,31.1621807099525,123.305499023336));
#97551=CARTESIAN_POINT('Ctrl Pts',(1.44016319784876,31.1969868677261,123.329370974848));
#97552=CARTESIAN_POINT('Ctrl Pts',(1.44246085937501,31.2310218669175,123.354291537472));
#97553=CARTESIAN_POINT('Ctrl Pts',(1.44475852090127,31.2642213716314,123.380203134337));
#97554=CARTESIAN_POINT('Ctrl Pts',(1.44858235651171,31.3194729597889,123.423325972791));
#97555=CARTESIAN_POINT('Ctrl Pts',(1.45240619212214,31.3726361632414,123.469373338719));
#97556=CARTESIAN_POINT('Ctrl Pts',(1.45623002773257,31.4233794277243,123.518113173272));
#97557=CARTESIAN_POINT('Ctrl Pts',(1.4600473584239,31.4740363702874,123.56677009404));
#97558=CARTESIAN_POINT('Ctrl Pts',(1.46386468911523,31.522281191662,123.618110047023));
#97559=CARTESIAN_POINT('Ctrl Pts',(1.46768201980656,31.5678142343074,123.671859913562));
#97560=CARTESIAN_POINT('Ctrl Pts',(1.47149571669541,31.6133039330309,123.725558614401));
#97561=CARTESIAN_POINT('Ctrl Pts',(1.47530941358426,31.6560866490738,123.78166230389));
#97562=CARTESIAN_POINT('Ctrl Pts',(1.47912311047312,31.6958995585341,123.839861107512));
#97563=CARTESIAN_POINT('Ctrl Pts',(1.4829345252099,31.735688643575,123.898025084422));
#97564=CARTESIAN_POINT('Ctrl Pts',(1.48674593994668,31.7725111653249,123.958281279008));
#97565=CARTESIAN_POINT('Ctrl Pts',(1.49055735468346,31.8061457882238,124.020288331099));
#97566=CARTESIAN_POINT('Ctrl Pts',(1.49436783578483,31.8397721720627,124.082280194084));
#97567=CARTESIAN_POINT('Ctrl Pts',(1.4981783168862,31.8702119700892,124.146021625177));
#97568=CARTESIAN_POINT('Ctrl Pts',(1.50198879798757,31.8972892160619,124.211145645182));
#97569=CARTESIAN_POINT('Ctrl Pts',(1.50580209417981,31.9243864660461,124.276317777232));
#97570=CARTESIAN_POINT('Ctrl Pts',(1.50961539037206,31.9481160067823,124.342874078778));
#97571=CARTESIAN_POINT('Ctrl Pts',(1.5134286865643,31.9683500464069,124.410427563984));
#97572=CARTESIAN_POINT('Ctrl Pts',(1.51724331839847,31.9885911731893,124.478004710417));
#97573=CARTESIAN_POINT('Ctrl Pts',(1.52105795023265,32.0053342400584,124.546579251802));
#97574=CARTESIAN_POINT('Ctrl Pts',(1.52487258206682,32.0185021276165,124.615751742609));
#97575=CARTESIAN_POINT('Ctrl Pts',(1.52869351656884,32.031691771618,124.685038522621));
#97576=CARTESIAN_POINT('Ctrl Pts',(1.53251445107087,32.0412943683235,124.75492473087));
#97577=CARTESIAN_POINT('Ctrl Pts',(1.53633538557289,32.0472845563241,124.825004263089));
#97578=CARTESIAN_POINT('Ctrl Pts',(1.53953201721104,32.0522960069184,124.88363349365));
#97579=CARTESIAN_POINT('Ctrl Pts',(1.54272864884919,32.0547800098895,124.942397807972));
#97580=CARTESIAN_POINT('Ctrl Pts',(1.54592528048733,32.0547497262092,125.0010607277));
#97581=CARTESIAN_POINT('Origin',(-1.54592528053767,30.,125.));
#97582=CARTESIAN_POINT('',(0.393902765004298,28.7479590808042,126.629230216746));
#97583=CARTESIAN_POINT('',(0.45211710701879,28.7479590808042,126.629230216746));
#97584=CARTESIAN_POINT('',(-1.54592528053767,28.7479590808042,126.629230216746));
#97585=CARTESIAN_POINT('',(0.145925136815139,32.0544293158457,124.997774677963));
#97586=CARTESIAN_POINT('Ctrl Pts',(0.145925280537677,32.0547487974726,124.997776987473));
#97587=CARTESIAN_POINT('Ctrl Pts',(0.149742847505049,32.0548251766857,125.068374923493));
#97588=CARTESIAN_POINT('Ctrl Pts',(0.153560414472421,32.0512588264106,125.139037406976));
#97589=CARTESIAN_POINT('Ctrl Pts',(0.157377981439792,32.0440566342328,125.209356247934));
#97590=CARTESIAN_POINT('Ctrl Pts',(0.161194267518903,32.0368568585688,125.27965149518));
#97591=CARTESIAN_POINT('Ctrl Pts',(0.165010553598014,32.0260237115458,125.349602835495));
#97592=CARTESIAN_POINT('Ctrl Pts',(0.168826839677125,32.011616039834,125.418806006144));
#97593=CARTESIAN_POINT('Ctrl Pts',(0.172643182166181,31.997208155157,125.488010199712));
#97594=CARTESIAN_POINT('Ctrl Pts',(0.176459524655237,31.9792257443085,125.556465716465));
#97595=CARTESIAN_POINT('Ctrl Pts',(0.180275867144293,31.9577786210231,125.623779154481));
#97596=CARTESIAN_POINT('Ctrl Pts',(0.184096314207838,31.9363084308052,125.69116498983));
#97597=CARTESIAN_POINT('Ctrl Pts',(0.187916761271383,31.9113662409764,125.757405820921));
#97598=CARTESIAN_POINT('Ctrl Pts',(0.191737208334928,31.8831112492071,125.822125042563));
#97599=CARTESIAN_POINT('Ctrl Pts',(0.195559834797493,31.8548401391929,125.886881183709));
#97600=CARTESIAN_POINT('Ctrl Pts',(0.199382461260057,31.8232526902279,125.950113545109));
#97601=CARTESIAN_POINT('Ctrl Pts',(0.203205087722621,31.7885543176414,126.011469730316));
#97602=CARTESIAN_POINT('Ctrl Pts',(0.207034783311059,31.7537917778742,126.072939380598));
#97603=CARTESIAN_POINT('Ctrl Pts',(0.210864478899498,31.7159070973764,126.132525510666));
#97604=CARTESIAN_POINT('Ctrl Pts',(0.214694174487936,31.6751488627916,126.189904975193));
#97605=CARTESIAN_POINT('Ctrl Pts',(0.217219630217664,31.6482712390514,126.227743308321));
#97606=CARTESIAN_POINT('Ctrl Pts',(0.219745085947392,31.6201448756126,126.264622703573));
#97607=CARTESIAN_POINT('Ctrl Pts',(0.22227054167712,31.5908499886023,126.300459102111));
#97608=CARTESIAN_POINT('Ctrl Pts',(0.226141676453319,31.5459454375006,126.355390783156));
#97609=CARTESIAN_POINT('Ctrl Pts',(0.230012811229518,31.4981043722261,126.408101583541));
#97610=CARTESIAN_POINT('Ctrl Pts',(0.233883946005718,31.4475746723825,126.458260995287));
#97611=CARTESIAN_POINT('Ctrl Pts',(0.237749271054588,31.397120806576,126.508345128718));
#97612=CARTESIAN_POINT('Ctrl Pts',(0.241614596103459,31.3439866574102,126.555885135297));
#97613=CARTESIAN_POINT('Ctrl Pts',(0.245479921152329,31.2884602743133,126.600583544841));
#97614=CARTESIAN_POINT('Ctrl Pts',(0.249340636948719,31.2330001043073,126.645228653239));
#97615=CARTESIAN_POINT('Ctrl Pts',(0.253201352745109,31.1751537431435,126.687038592961));
#97616=CARTESIAN_POINT('Ctrl Pts',(0.257062068541499,31.1152447204755,126.725753973181));
#97617=CARTESIAN_POINT('Ctrl Pts',(0.260920304427269,31.0553741800551,126.76444448478));
#97618=CARTESIAN_POINT('Ctrl Pts',(0.264778540313038,30.9934440134148,126.80004411804));
#97619=CARTESIAN_POINT('Ctrl Pts',(0.268636776198808,30.9298081599305,126.832335762961));
#97620=CARTESIAN_POINT('Ctrl Pts',(0.272493820670667,30.8661919570439,126.8646174363));
#97621=CARTESIAN_POINT('Ctrl Pts',(0.276350865142527,30.8008715454328,126.89359292988));
#97622=CARTESIAN_POINT('Ctrl Pts',(0.280207909614387,30.7342254730604,126.919091065377));
#97623=CARTESIAN_POINT('Ctrl Pts',(0.284065049503794,30.6675777519632,126.944589831659));
#97624=CARTESIAN_POINT('Ctrl Pts',(0.287922189393201,30.5996047589391,126.966610897738));
#97625=CARTESIAN_POINT('Ctrl Pts',(0.291779329282608,30.5307034092699,126.98503185211));
#97626=CARTESIAN_POINT('Ctrl Pts',(0.295640407261538,30.4617317122214,127.003471614035));
#97627=CARTESIAN_POINT('Ctrl Pts',(0.299501485240468,30.3918302360401,127.01830380093));
#97628=CARTESIAN_POINT('Ctrl Pts',(0.303362563219398,30.3214085129597,127.029456609612));
#97629=CARTESIAN_POINT('Ctrl Pts',(0.307225773774024,30.2509478940953,127.040615578286));
#97630=CARTESIAN_POINT('Ctrl Pts',(0.31108898432865,30.1799669390398,127.048091071826));
#97631=CARTESIAN_POINT('Ctrl Pts',(0.314952194883276,30.1088800485825,127.051863225832));
#97632=CARTESIAN_POINT('Ctrl Pts',(0.318822060279675,30.0376707024626,127.055641877823));
#97633=CARTESIAN_POINT('Ctrl Pts',(0.322691925676074,29.9663555419922,127.055704452657));
#97634=CARTESIAN_POINT('Ctrl Pts',(0.326561791072473,29.8953480046004,127.052083215262));
#97635=CARTESIAN_POINT('Ctrl Pts',(0.328843131553543,29.853488055243,127.04994844451));
#97636=CARTESIAN_POINT('Ctrl Pts',(0.331124472034613,29.8117349175731,127.046534437514));
#97637=CARTESIAN_POINT('Ctrl Pts',(0.333405812515682,29.7701717568777,127.041856150948));
#97638=CARTESIAN_POINT('Ctrl Pts',(0.337280820487943,29.699573974397,127.033909771224));
#97639=CARTESIAN_POINT('Ctrl Pts',(0.341155828460203,29.6292554674172,127.022282690525));
#97640=CARTESIAN_POINT('Ctrl Pts',(0.345030836432464,29.5596290834691,127.007005485387));
#97641=CARTESIAN_POINT('Ctrl Pts',(0.349103497146784,29.4864512627742,126.990949035017));
#97642=CARTESIAN_POINT('Ctrl Pts',(0.353176157861103,29.414038594576,126.970860123394));
#97643=CARTESIAN_POINT('Ctrl Pts',(0.357248818575423,29.3428649859014,126.946836186161));
#97644=CARTESIAN_POINT('Ctrl Pts',(0.36111377939119,29.2753211299458,126.924037435526));
#97645=CARTESIAN_POINT('Ctrl Pts',(0.364978740206958,29.2088935797027,126.897695353925));
#97646=CARTESIAN_POINT('Ctrl Pts',(0.368843701022725,29.1439752527045,126.867945179741));
#97647=CARTESIAN_POINT('Ctrl Pts',(0.372706168135226,29.0790988115239,126.838214200604));
#97648=CARTESIAN_POINT('Ctrl Pts',(0.376568635247727,29.015730098834,126.805079696651));
#97649=CARTESIAN_POINT('Ctrl Pts',(0.380431102360228,28.954242424875,126.768725150092));
#97650=CARTESIAN_POINT('Ctrl Pts',(0.384292622927454,28.89276981923,126.732379512664));
#97651=CARTESIAN_POINT('Ctrl Pts',(0.38815414349468,28.8331777535429,126.692815645137));
#97652=CARTESIAN_POINT('Ctrl Pts',(0.392015664061906,28.7758138465268,126.650262350096));
#97653=CARTESIAN_POINT('Ctrl Pts',(0.39264469770937,28.7664693857023,126.643330507076));
#97654=CARTESIAN_POINT('Ctrl Pts',(0.393273731356834,28.7571839880914,126.636319430585));
#97655=CARTESIAN_POINT('Ctrl Pts',(0.393902765004298,28.7479590808042,126.629230216746));
#97656=CARTESIAN_POINT('',(0.,30.5301702171886,123.014825674328));
#97657=CARTESIAN_POINT('Ctrl Pts',(-2.77555756156289E-16,30.5301702171886,
123.014825674328));
#97658=CARTESIAN_POINT('Ctrl Pts',(0.0370450902795195,31.1902723495278,
123.191115729233));
#97659=CARTESIAN_POINT('Ctrl Pts',(0.0856865378388906,31.9249100643917,
123.887375341273));
#97660=CARTESIAN_POINT('Ctrl Pts',(0.134327985398261,32.0542758854422,124.783527116577));
#97661=CARTESIAN_POINT('Ctrl Pts',(0.145924342678113,32.0526640242463,124.997761916792));
#97662=CARTESIAN_POINT('',(7.76557151915824E-9,29.4696366853849,123.014877253918));
#97663=CARTESIAN_POINT('Origin',(0.,30.,125.));
#97664=CARTESIAN_POINT('',(0.20407471941795,32.054749451866,125.001500851857));
#97665=CARTESIAN_POINT('Ctrl Pts',(7.76557151915824E-9,29.4696366853849,
123.014877253918));
#97666=CARTESIAN_POINT('Ctrl Pts',(0.00385761022877746,29.5379454299378,
122.996627273029));
#97667=CARTESIAN_POINT('Ctrl Pts',(0.00771521269198336,29.6073355558211,
122.981870298801));
#97668=CARTESIAN_POINT('Ctrl Pts',(0.0115728151551893,29.6774154225185,
122.970729995079));
#97669=CARTESIAN_POINT('Ctrl Pts',(0.0154246336215809,29.747390213141,122.959606394862));
#97670=CARTESIAN_POINT('Ctrl Pts',(0.0192764520879721,29.8180522132104,
122.952088779147));
#97671=CARTESIAN_POINT('Ctrl Pts',(0.0231282705543638,29.8889963546714,
122.948250562758));
#97672=CARTESIAN_POINT('Ctrl Pts',(0.0269755489459578,29.9598568754449,
122.944416870411));
#97673=CARTESIAN_POINT('Ctrl Pts',(0.030822827337552,30.0309983912348,122.94425399043));
#97674=CARTESIAN_POINT('Ctrl Pts',(0.0346701057291459,30.1020091979917,
122.947783713634));
#97675=CARTESIAN_POINT('Ctrl Pts',(0.0385149683480649,30.1729754158344,
122.951311220464));
#97676=CARTESIAN_POINT('Ctrl Pts',(0.0423598309669836,30.2438106001824,
122.958526706804));
#97677=CARTESIAN_POINT('Ctrl Pts',(0.0462046935859026,30.3141030405584,
122.969399881214));
#97678=CARTESIAN_POINT('Ctrl Pts',(0.0500484485266476,30.3843752301713,
122.980269923139));
#97679=CARTESIAN_POINT('Ctrl Pts',(0.0538922034673924,30.4541045031858,
122.994795486533));
#97680=CARTESIAN_POINT('Ctrl Pts',(0.0577359584081374,30.5228860355374,
123.012894628778));
#97681=CARTESIAN_POINT('Ctrl Pts',(0.0615799121663579,30.5916711256003,
123.030994707197));
#97682=CARTESIAN_POINT('Ctrl Pts',(0.0654238659245789,30.6595079054338,
123.052668604445));
#97683=CARTESIAN_POINT('Ctrl Pts',(0.0692678196827994,30.726005208168,123.077784091156));
#97684=CARTESIAN_POINT('Ctrl Pts',(0.0731157450116613,30.7925712158741,
123.102925527172));
#97685=CARTESIAN_POINT('Ctrl Pts',(0.0769636703405231,30.8577945264371,
123.131515475442));
#97686=CARTESIAN_POINT('Ctrl Pts',(0.0808115956693851,30.9213034447518,
123.163373329937));
#97687=CARTESIAN_POINT('Ctrl Pts',(0.0846617836232696,30.984849707052,123.195249917222));
#97688=CARTESIAN_POINT('Ctrl Pts',(0.0885119715771539,31.0466791460969,
123.230397992699));
#97689=CARTESIAN_POINT('Ctrl Pts',(0.0923621595310384,31.1064466115173,
123.268592058941));
#97690=CARTESIAN_POINT('Ctrl Pts',(0.0962187949191377,31.16631416213,123.306850084069));
#97691=CARTESIAN_POINT('Ctrl Pts',(0.100075430307237,31.2241124513603,123.348163994447));
#97692=CARTESIAN_POINT('Ctrl Pts',(0.103932065695336,31.279527830583,123.392266784176));
#97693=CARTESIAN_POINT('Ctrl Pts',(0.105608342252961,31.3036139812752,123.411435947218));
#97694=CARTESIAN_POINT('Ctrl Pts',(0.107284618810585,31.3272504139545,123.431131494297));
#97695=CARTESIAN_POINT('Ctrl Pts',(0.10896089536821,31.350413588026,123.451329375311));
#97696=CARTESIAN_POINT('Ctrl Pts',(0.112923971370282,31.405176281495,123.499081482311));
#97697=CARTESIAN_POINT('Ctrl Pts',(0.116887047372355,31.4575262780038,123.549849701845));
#97698=CARTESIAN_POINT('Ctrl Pts',(0.120850123374427,31.507109086759,123.603354102462));
#97699=CARTESIAN_POINT('Ctrl Pts',(0.124661304975432,31.5547915153461,123.65480781849));
#97700=CARTESIAN_POINT('Ctrl Pts',(0.128472486576437,31.5999146066877,123.708791405287));
#97701=CARTESIAN_POINT('Ctrl Pts',(0.132283668177441,31.6421964245354,123.765014791286));
#97702=CARTESIAN_POINT('Ctrl Pts',(0.136091357626874,31.684439499932,123.821186660299));
#97703=CARTESIAN_POINT('Ctrl Pts',(0.139899047076306,31.7238461632285,123.879593863066));
#97704=CARTESIAN_POINT('Ctrl Pts',(0.143706736525739,31.7601735166201,123.939911912203));
#97705=CARTESIAN_POINT('Ctrl Pts',(0.147512291410529,31.7964805051461,124.000196147454));
#97706=CARTESIAN_POINT('Ctrl Pts',(0.151317846295318,31.8297113500592,124.062388677103));
#97707=CARTESIAN_POINT('Ctrl Pts',(0.155123401180107,31.8596665201771,124.126136168369));
#97708=CARTESIAN_POINT('Ctrl Pts',(0.158928176024214,31.8896155502571,124.189870593042));
#97709=CARTESIAN_POINT('Ctrl Pts',(0.16273295086832,31.9162900274481,124.255158893629));
#97710=CARTESIAN_POINT('Ctrl Pts',(0.166537725712426,31.9395372999307,124.321625011754));
#97711=CARTESIAN_POINT('Ctrl Pts',(0.17034498854872,31.9627997741097,124.388134592945));
#97712=CARTESIAN_POINT('Ctrl Pts',(0.174152251385013,31.9826304041421,124.455823056767));
#97713=CARTESIAN_POINT('Ctrl Pts',(0.177959514221306,31.9989259021712,124.52429757187));
#97714=CARTESIAN_POINT('Ctrl Pts',(0.18176828320523,32.0152278466756,124.59279917539));
#97715=CARTESIAN_POINT('Ctrl Pts',(0.185577052189154,32.0279917839574,124.662086957578));
#97716=CARTESIAN_POINT('Ctrl Pts',(0.189385821173078,32.0371657421938,124.731758874644));
#97717=CARTESIAN_POINT('Ctrl Pts',(0.193199633965217,32.0463518491549,124.801523055586));
#97718=CARTESIAN_POINT('Ctrl Pts',(0.197013446757356,32.0519384547796,124.871671888419));
#97719=CARTESIAN_POINT('Ctrl Pts',(0.200827259549495,32.0539256011114,124.94180045018));
#97720=CARTESIAN_POINT('Ctrl Pts',(0.201909746172313,32.0544896191791,124.961705263059));
#97721=CARTESIAN_POINT('Ctrl Pts',(0.202992232795132,32.054763981877,124.98160846073));
#97722=CARTESIAN_POINT('Ctrl Pts',(0.20407471941795,32.054749451866,125.001500851857));
#97723=CARTESIAN_POINT('Ctrl Pts',(0.204074719462323,32.0547494518654,125.001500852673));
#97724=CARTESIAN_POINT('Ctrl Pts',(0.209415201710472,32.0546777675541,125.099640598186));
#97725=CARTESIAN_POINT('Ctrl Pts',(0.214755683958621,32.0475743595618,125.197525900642));
#97726=CARTESIAN_POINT('Ctrl Pts',(0.22009616620677,32.0335513132822,125.294391947492));
#97727=CARTESIAN_POINT('Ctrl Pts',(0.223961505002541,32.0234017008875,125.364501737486));
#97728=CARTESIAN_POINT('Ctrl Pts',(0.227826843798313,32.0096018595663,125.434225914476));
#97729=CARTESIAN_POINT('Ctrl Pts',(0.231692182594084,31.9921930417871,125.503154495911));
#97730=CARTESIAN_POINT('Ctrl Pts',(0.235551702466996,31.9748104314305,125.571979311513));
#97731=CARTESIAN_POINT('Ctrl Pts',(0.239411222339908,31.9538297464012,125.640010440692));
#97732=CARTESIAN_POINT('Ctrl Pts',(0.243270742212821,31.9293437036226,125.706845411523));
#97733=CARTESIAN_POINT('Ctrl Pts',(0.247125668264792,31.9048868055304,125.773600831556));
#97734=CARTESIAN_POINT('Ctrl Pts',(0.250980594316762,31.8769330034826,125.839162466248));
#97735=CARTESIAN_POINT('Ctrl Pts',(0.254835520368733,31.8456250674413,125.90314211115));
#97736=CARTESIAN_POINT('Ctrl Pts',(0.258687979313753,31.8143371681078,125.967080809838));
#97737=CARTESIAN_POINT('Ctrl Pts',(0.262540438258773,31.7796996067612,126.029439091024));
#97738=CARTESIAN_POINT('Ctrl Pts',(0.266392897203793,31.7419030265743,126.089849259536));
#97739=CARTESIAN_POINT('Ctrl Pts',(0.270244186324789,31.704117923563,126.150241084111));
#97740=CARTESIAN_POINT('Ctrl Pts',(0.274095475445786,31.6631759640342,126.208685557808));
#97741=CARTESIAN_POINT('Ctrl Pts',(0.277946764566783,31.6193125696332,126.264841636067));
#97742=CARTESIAN_POINT('Ctrl Pts',(0.281798179498721,31.5754477423367,126.320999548789));
#97743=CARTESIAN_POINT('Ctrl Pts',(0.285649594430659,31.5286615921515,126.374868535323));
#97744=CARTESIAN_POINT('Ctrl Pts',(0.289501009362597,31.4792304211519,126.426139868189));
#97745=CARTESIAN_POINT('Ctrl Pts',(0.293356449034519,31.4297475944326,126.47746477975));
#97746=CARTESIAN_POINT('Ctrl Pts',(0.297211888706441,31.3776145678265,126.526186267525));
#97747=CARTESIAN_POINT('Ctrl Pts',(0.301067328378363,31.323144540542,126.572032470191));
#97748=CARTESIAN_POINT('Ctrl Pts',(0.304924940998853,31.2686438136283,126.617904512047));
#97749=CARTESIAN_POINT('Ctrl Pts',(0.308782553619344,31.2118038526668,126.660897749185));
#97750=CARTESIAN_POINT('Ctrl Pts',(0.312640166239834,31.1529687681419,126.700782344155));
#97751=CARTESIAN_POINT('Ctrl Pts',(0.316504559112776,31.0940302733564,126.740737041452));
#97752=CARTESIAN_POINT('Ctrl Pts',(0.320368951985719,31.0330900707049,126.777571936079));
#97753=CARTESIAN_POINT('Ctrl Pts',(0.324233344858661,30.9705182802118,126.811102379843));
#97754=CARTESIAN_POINT('Ctrl Pts',(0.326566042254217,30.9327475209962,126.831342655978));
#97755=CARTESIAN_POINT('Ctrl Pts',(0.328898739649774,30.8943826830153,126.850379771625));
#97756=CARTESIAN_POINT('Ctrl Pts',(0.33123143704533,30.855508387678,126.868181725934));
#97757=CARTESIAN_POINT('Ctrl Pts',(0.335101017398882,30.7910220081836,126.897712385496));
#97758=CARTESIAN_POINT('Ctrl Pts',(0.338970597752434,30.7248786638559,126.923957958651));
#97759=CARTESIAN_POINT('Ctrl Pts',(0.342840178105986,30.6574462840317,126.946731092399));
#97760=CARTESIAN_POINT('Ctrl Pts',(0.346703992403464,30.5901143850989,126.969470291934));
#97761=CARTESIAN_POINT('Ctrl Pts',(0.350567806700942,30.5214977197823,126.988747168817));
#97762=CARTESIAN_POINT('Ctrl Pts',(0.35443162099842,30.4519857149758,127.004421731063));
#97763=CARTESIAN_POINT('Ctrl Pts',(0.358290899187939,30.3825553170826,127.020077891414));
#97764=CARTESIAN_POINT('Ctrl Pts',(0.362150177377457,30.3122321390617,127.032140031349));
#97765=CARTESIAN_POINT('Ctrl Pts',(0.366009455566976,30.2414206768526,127.040517978183));
#97766=CARTESIAN_POINT('Ctrl Pts',(0.369866299964003,30.1706538707674,127.048890641598));
#97767=CARTESIAN_POINT('Ctrl Pts',(0.37372314436103,30.0993998725611,127.053583664579));
#97768=CARTESIAN_POINT('Ctrl Pts',(0.377579988758057,30.0280718289488,127.054558233519));
#97769=CARTESIAN_POINT('Ctrl Pts',(0.381435690157131,29.9567649238112,127.055532513639));
#97770=CARTESIAN_POINT('Ctrl Pts',(0.385291391556204,29.8853845021612,127.052790520854));
#97771=CARTESIAN_POINT('Ctrl Pts',(0.389147092955278,29.8143455388811,127.046345519106));
#97772=CARTESIAN_POINT('Ctrl Pts',(0.393002940534494,29.7433038823205,127.039900273011));
#97773=CARTESIAN_POINT('Ctrl Pts',(0.39685878811371,29.672604193286,127.029751785297));
#97774=CARTESIAN_POINT('Ctrl Pts',(0.400714635692925,29.6026564170064,127.015965188081));
#97775=CARTESIAN_POINT('Ctrl Pts',(0.404574508651722,29.5326356175212,127.002164198105));
#97776=CARTESIAN_POINT('Ctrl Pts',(0.408434381610518,29.463368775227,126.984717610905));
#97777=CARTESIAN_POINT('Ctrl Pts',(0.412294254569315,29.3952548372765,126.963741543753));
#97778=CARTESIAN_POINT('Ctrl Pts',(0.416156307606727,29.3271024281792,126.942753629198));
#97779=CARTESIAN_POINT('Ctrl Pts',(0.420018360644138,29.2601046759995,126.918232433224));
#97780=CARTESIAN_POINT('Ctrl Pts',(0.42388041368155,29.1946419708229,126.890342827992));
#97781=CARTESIAN_POINT('Ctrl Pts',(0.427749209984033,29.1290649657211,126.862404526639));
#97782=CARTESIAN_POINT('Ctrl Pts',(0.431618006286515,29.0650287952297,126.831086287122));
#97783=CARTESIAN_POINT('Ctrl Pts',(0.435486802588998,29.0028899805489,126.796599335303));
#97784=CARTESIAN_POINT('Ctrl Pts',(0.437780104353962,28.966056029563,126.77615654605));
#97785=CARTESIAN_POINT('Ctrl Pts',(0.440073406118926,28.9298882374949,126.754601199828));
#97786=CARTESIAN_POINT('Ctrl Pts',(0.44236670788389,28.8944556997489,126.73198422703));
#97787=CARTESIAN_POINT('Ctrl Pts',(0.445616840928857,28.8442396908682,126.699930804411));
#97788=CARTESIAN_POINT('Ctrl Pts',(0.448866973973823,28.795336617669,126.665639199464));
#97789=CARTESIAN_POINT('Ctrl Pts',(0.452117107018789,28.7479590808042,126.629230216746));
#97790=CARTESIAN_POINT('Origin',(-1.54592528053767,-30.,125.));
#97791=CARTESIAN_POINT('',(9.49394826732427,-31.2520409112987,126.629230222815));
#97792=CARTESIAN_POINT('',(9.55204643304504,-31.2540479291372,126.631857161249));
#97793=CARTESIAN_POINT('',(-1.54592528053767,-31.2520409112987,126.629230222815));
#97794=CARTESIAN_POINT('',(10.,-27.9466241674713,124.92486510207));
#97795=CARTESIAN_POINT('Ctrl Pts',(9.55204643304504,-31.2540479291372,126.631857161249));
#97796=CARTESIAN_POINT('Ctrl Pts',(9.55318392757862,-31.2706437159061,126.619178714129));
#97797=CARTESIAN_POINT('Ctrl Pts',(9.59136651239171,-31.8206290607534,126.184464695852));
#97798=CARTESIAN_POINT('Ctrl Pts',(9.66659418748432,-32.4129313959741,124.728220591155));
#97799=CARTESIAN_POINT('Ctrl Pts',(9.77772945832288,-31.0809188200307,122.823596089609));
#97800=CARTESIAN_POINT('Ctrl Pts',(9.88886472916144,-28.7565525546702,122.915156040329));
#97801=CARTESIAN_POINT('Ctrl Pts',(9.96295490972048,-27.9716077196437,124.242084880697));
#97802=CARTESIAN_POINT('Ctrl Pts',(10.,-27.9466241674713,124.92486510207));
#97803=CARTESIAN_POINT('',(9.99999184526219,-28.1818120683087,125.959175316415));
#97804=CARTESIAN_POINT('Origin',(10.,-30.,125.));
#97805=CARTESIAN_POINT('',(9.94592528057839,-27.9452500001719,125.000026582061));
#97806=CARTESIAN_POINT('Ctrl Pts',(9.94592528057839,-27.9452500001719,125.000026582061));
#97807=CARTESIAN_POINT('Ctrl Pts',(9.94992641061459,-27.9452509601105,125.074228272518));
#97808=CARTESIAN_POINT('Ctrl Pts',(9.95392754065078,-27.9492756106224,125.14835894506));
#97809=CARTESIAN_POINT('Ctrl Pts',(9.95792867068697,-27.9572752004394,125.221975124192));
#97810=CARTESIAN_POINT('Ctrl Pts',(9.96193971239158,-27.9652946069784,125.295773666595));
#97811=CARTESIAN_POINT('Ctrl Pts',(9.96595075409619,-27.9773085747598,125.369054741152));
#97812=CARTESIAN_POINT('Ctrl Pts',(9.9699617958008,-27.9932168371984,125.441382940309));
#97813=CARTESIAN_POINT('Ctrl Pts',(9.97397822777386,-28.0091464780746,125.513808338258));
#97814=CARTESIAN_POINT('Ctrl Pts',(9.97799465974692,-28.0289807273363,125.58527789525));
#97815=CARTESIAN_POINT('Ctrl Pts',(9.98201109171998,-28.0525696285214,125.655372039946));
#97816=CARTESIAN_POINT('Ctrl Pts',(9.9860378222072,-28.0762190138961,125.725645912706));
#97817=CARTESIAN_POINT('Ctrl Pts',(9.99006455269442,-28.1036421278151,125.794536926984));
#97818=CARTESIAN_POINT('Ctrl Pts',(9.99409128318165,-28.1346410673708,125.861645875613));
#97819=CARTESIAN_POINT('Ctrl Pts',(9.99605722571572,-28.1497754633721,125.894410009429));
#97820=CARTESIAN_POINT('Ctrl Pts',(9.99802316824979,-28.1657615112236,125.926749759945));
#97821=CARTESIAN_POINT('Ctrl Pts',(9.99998911078386,-28.1825723884147,125.958621113448));
#97822=CARTESIAN_POINT('Ctrl Pts',(9.49394826732428,-31.2520409112987,126.629230222815));
#97823=CARTESIAN_POINT('Ctrl Pts',(9.4978041255961,-31.3085908113369,126.58577240612));
#97824=CARTESIAN_POINT('Ctrl Pts',(9.50165998386792,-31.3628913545301,126.539354695332));
#97825=CARTESIAN_POINT('Ctrl Pts',(9.50551584213974,-31.4146257283712,126.490245486868));
#97826=CARTESIAN_POINT('Ctrl Pts',(9.50937196666856,-31.4663636746049,126.441132887286));
#97827=CARTESIAN_POINT('Ctrl Pts',(9.51322809119738,-31.5155347491312,126.389328757068));
#97828=CARTESIAN_POINT('Ctrl Pts',(9.5170842157262,-31.5618583455608,126.335138970633));
#97829=CARTESIAN_POINT('Ctrl Pts',(9.52094443717721,-31.6082311582875,126.280891610502));
#97830=CARTESIAN_POINT('Ctrl Pts',(9.52480465862823,-31.6517501388171,126.224253905268));
#97831=CARTESIAN_POINT('Ctrl Pts',(9.52866488007924,-31.6921750163993,126.165564788579));
#97832=CARTESIAN_POINT('Ctrl Pts',(9.53252738923184,-31.732623851171,126.106840890676));
#97833=CARTESIAN_POINT('Ctrl Pts',(9.53638989838445,-31.7699746790533,126.046063575328));
#97834=CARTESIAN_POINT('Ctrl Pts',(9.54025240753705,-31.8040320840594,125.983598394765));
#97835=CARTESIAN_POINT('Ctrl Pts',(9.54412154299831,-31.8381479160798,125.921026052367));
#97836=CARTESIAN_POINT('Ctrl Pts',(9.54799067845958,-31.8689588377403,125.856760502689));
#97837=CARTESIAN_POINT('Ctrl Pts',(9.55185981392084,-31.8963169727468,125.791188663577));
#97838=CARTESIAN_POINT('Ctrl Pts',(9.55378430665259,-31.9099248012919,125.758573489194));
#97839=CARTESIAN_POINT('Ctrl Pts',(9.55570879938434,-31.9226791705976,125.725635394501));
#97840=CARTESIAN_POINT('Ctrl Pts',(9.5576332921161,-31.9345665198439,125.692423239644));
#97841=CARTESIAN_POINT('Ctrl Pts',(9.56150282241141,-31.9584681211752,125.62564437513));
#97842=CARTESIAN_POINT('Ctrl Pts',(9.56537235270673,-31.9789546628836,125.557496042673));
#97843=CARTESIAN_POINT('Ctrl Pts',(9.56924188300204,-31.9958710383814,125.488360891811));
#97844=CARTESIAN_POINT('Ctrl Pts',(9.57310565808745,-32.0127622539026,125.419328566686));
#97845=CARTESIAN_POINT('Ctrl Pts',(9.57696943317286,-32.0260937289525,125.349312804447));
#97846=CARTESIAN_POINT('Ctrl Pts',(9.58083320825827,-32.0357593881892,125.278713609104));
#97847=CARTESIAN_POINT('Ctrl Pts',(9.58469246348782,-32.0454137405083,125.208197000913));
#97848=CARTESIAN_POINT('Ctrl Pts',(9.58855171871737,-32.0514107294817,125.137098794134));
#97849=CARTESIAN_POINT('Ctrl Pts',(9.59241097394691,-32.0536952083313,125.06582973323));
#97850=CARTESIAN_POINT('Ctrl Pts',(9.59626780542365,-32.0559782524449,124.994605431891));
#97851=CARTESIAN_POINT('Ctrl Pts',(9.60012463690039,-32.054553396799,124.923210973568));
#97852=CARTESIAN_POINT('Ctrl Pts',(9.60398146837713,-32.0494174069306,124.852061314492));
#97853=CARTESIAN_POINT('Ctrl Pts',(9.60783716688164,-32.0442829257965,124.780932556144));
#97854=CARTESIAN_POINT('Ctrl Pts',(9.61169286538615,-32.0354395097063,124.710048938397));
#97855=CARTESIAN_POINT('Ctrl Pts',(9.61554856389066,-32.0229359667501,124.639822770114));
#97856=CARTESIAN_POINT('Ctrl Pts',(9.61940441859746,-32.0104319172498,124.569593756824));
#97857=CARTESIAN_POINT('Ctrl Pts',(9.62326027330426,-31.9942675337882,124.500022723614));
#97858=CARTESIAN_POINT('Ctrl Pts',(9.62711612801105,-31.9745428697909,124.431512517413));
#97859=CARTESIAN_POINT('Ctrl Pts',(9.63097602331588,-31.9547975360732,124.362930518516));
#97860=CARTESIAN_POINT('Ctrl Pts',(9.63483591862072,-31.9314846088313,124.295412033373));
#97861=CARTESIAN_POINT('Ctrl Pts',(9.63869581392555,-31.9047539953752,124.229344577906));
#97862=CARTESIAN_POINT('Ctrl Pts',(9.64255789792737,-31.878008224717,124.163239659859));
#97863=CARTESIAN_POINT('Ctrl Pts',(9.64641998192919,-31.8478411154121,124.098587849704));
#97864=CARTESIAN_POINT('Ctrl Pts',(9.65028206593101,-31.814449557256,124.035753990585));
#97865=CARTESIAN_POINT('Ctrl Pts',(9.6541509064683,-31.7809995821294,123.972810206565));
#97866=CARTESIAN_POINT('Ctrl Pts',(9.65801974700559,-31.7443141456839,123.911691139911));
#97867=CARTESIAN_POINT('Ctrl Pts',(9.66188858754287,-31.7046342726389,123.852733876102));
#97868=CARTESIAN_POINT('Ctrl Pts',(9.66418191268013,-31.6811133108882,123.817785892639));
#97869=CARTESIAN_POINT('Ctrl Pts',(9.66647523781738,-31.6565409827353,123.783596915282));
#97870=CARTESIAN_POINT('Ctrl Pts',(9.66876856295464,-31.6309739560517,123.750231414549));
#97871=CARTESIAN_POINT('Ctrl Pts',(9.67263371316888,-31.587883511937,123.693997490185));
#97872=CARTESIAN_POINT('Ctrl Pts',(9.67649886338311,-31.5417958827293,123.639883225883));
#97873=CARTESIAN_POINT('Ctrl Pts',(9.68036401359735,-31.4929474727728,123.588226149115));
#97874=CARTESIAN_POINT('Ctrl Pts',(9.68422338831157,-31.4441720545441,123.536646260926));
#97875=CARTESIAN_POINT('Ctrl Pts',(9.6880827630258,-31.3926443753802,123.487516623446));
#97876=CARTESIAN_POINT('Ctrl Pts',(9.69194213774002,-31.3386420624652,123.441143049828));
#97877=CARTESIAN_POINT('Ctrl Pts',(9.69579698366837,-31.2847031186007,123.394823893312));
#97878=CARTESIAN_POINT('Ctrl Pts',(9.69965182959673,-31.2282956761813,123.351254692722));
#97879=CARTESIAN_POINT('Ctrl Pts',(9.70350667552509,-31.1697340556572,123.310704347506));
#97880=CARTESIAN_POINT('Ctrl Pts',(9.70735909449371,-31.1112093047505,123.270179532247));
#97881=CARTESIAN_POINT('Ctrl Pts',(9.71121151346233,-31.0505334656249,123.232670078342));
#97882=CARTESIAN_POINT('Ctrl Pts',(9.71506393243095,-30.9880525930008,123.198403586825));
#97883=CARTESIAN_POINT('Ctrl Pts',(9.71891522164929,-30.9255900433535,123.16414714421));
#97884=CARTESIAN_POINT('Ctrl Pts',(9.72276651086764,-30.8613239376804,123.133132010075));
#97885=CARTESIAN_POINT('Ctrl Pts',(9.72661780008598,-30.7956263623038,123.105540643321));
#97886=CARTESIAN_POINT('Ctrl Pts',(9.7304692551573,-30.7299259577087,123.077948088366));
#97887=CARTESIAN_POINT('Ctrl Pts',(9.73432071022861,-30.6627944107858,123.053779779993));
#97888=CARTESIAN_POINT('Ctrl Pts',(9.73817216529993,-30.5946236683056,123.033169998299));
#97889=CARTESIAN_POINT('Ctrl Pts',(9.7420277058967,-30.5263806120378,123.012538354273));
#97890=CARTESIAN_POINT('Ctrl Pts',(9.74588324649348,-30.4570966267253,122.995472913306));
#97891=CARTESIAN_POINT('Ctrl Pts',(9.74973878709025,-30.3871778269895,122.982057757817));
#97892=CARTESIAN_POINT('Ctrl Pts',(9.75359653504282,-30.3172189976746,122.968634921946));
#97893=CARTESIAN_POINT('Ctrl Pts',(9.75745428299538,-30.2466251130133,122.958866598036));
#97894=CARTESIAN_POINT('Ctrl Pts',(9.76131203094795,-30.1758087037608,122.952785096239));
#97895=CARTESIAN_POINT('Ctrl Pts',(9.76517661213126,-30.1048668573695,122.946692822275));
#97896=CARTESIAN_POINT('Ctrl Pts',(9.76904119331458,-30.0337021861904,122.944300424681));
#97897=CARTESIAN_POINT('Ctrl Pts',(9.7729057744979,-29.962727819202,122.945588077566));
#97898=CARTESIAN_POINT('Ctrl Pts',(9.77523846092969,-29.9198872279385,122.946365313254));
#97899=CARTESIAN_POINT('Ctrl Pts',(9.77757114736148,-29.8771159076542,122.948482329295));
#97900=CARTESIAN_POINT('Ctrl Pts',(9.77990383379327,-29.8345033018076,122.951925683627));
#97901=CARTESIAN_POINT('Ctrl Pts',(9.78377969104042,-29.7637006534364,122.957646962603));
#97902=CARTESIAN_POINT('Ctrl Pts',(9.78765554828756,-29.693058539817,122.967055076515));
#97903=CARTESIAN_POINT('Ctrl Pts',(9.79153140553471,-29.6229905778606,122.980133306845));
#97904=CARTESIAN_POINT('Ctrl Pts',(9.79540148151799,-29.5530271299125,122.993192029567));
#97905=CARTESIAN_POINT('Ctrl Pts',(9.79927155750128,-29.4836366054338,123.009909913015));
#97906=CARTESIAN_POINT('Ctrl Pts',(9.80314163348456,-29.4152281865604,123.03021841599));
#97907=CARTESIAN_POINT('Ctrl Pts',(9.80700712085521,-29.3469008771373,123.050502839889));
#97908=CARTESIAN_POINT('Ctrl Pts',(9.81087260822585,-29.2795538217276,123.074369288734));
#97909=CARTESIAN_POINT('Ctrl Pts',(9.8147380955965,-29.2135849718361,123.101698399627));
#97910=CARTESIAN_POINT('Ctrl Pts',(9.81860111321162,-29.147658271075,123.129010049275));
#97911=CARTESIAN_POINT('Ctrl Pts',(9.82246413082675,-29.0831084746034,123.159779786309));
#97912=CARTESIAN_POINT('Ctrl Pts',(9.82632714844188,-29.0203159818345,123.1938392134));
#97913=CARTESIAN_POINT('Ctrl Pts',(9.83018897812518,-28.9575427986333,123.227888166742));
#97914=CARTESIAN_POINT('Ctrl Pts',(9.83405080780849,-28.8965262713254,123.265224570954));
#97915=CARTESIAN_POINT('Ctrl Pts',(9.83791263749179,-28.8376229640577,123.305633691077));
#97916=CARTESIAN_POINT('Ctrl Pts',(9.84177455940801,-28.7787182499896,123.346043776299));
#97917=CARTESIAN_POINT('Ctrl Pts',(9.84563648132423,-28.721927253993,123.389526447573));
#97918=CARTESIAN_POINT('Ctrl Pts',(9.84949840324045,-28.6675768412463,123.435824150386));
#97919=CARTESIAN_POINT('Ctrl Pts',(9.85336422698768,-28.6131715164297,123.482168629341));
#97920=CARTESIAN_POINT('Ctrl Pts',(9.85723005073492,-28.5612120665622,123.531333503191));
#97921=CARTESIAN_POINT('Ctrl Pts',(9.86109587448215,-28.5119908828302,123.583022078605));
#97922=CARTESIAN_POINT('Ctrl Pts',(9.86496381726527,-28.4627427187025,123.634738986907));
#97923=CARTESIAN_POINT('Ctrl Pts',(9.86883176004839,-28.4162361246387,123.688981983705));
#97924=CARTESIAN_POINT('Ctrl Pts',(9.8726997028315,-28.3727235371298,123.745420837138));
#97925=CARTESIAN_POINT('Ctrl Pts',(9.87657422950515,-28.3291368838632,123.801955759011));
#97926=CARTESIAN_POINT('Ctrl Pts',(9.8804487561788,-28.2885546879188,123.860693602102));
#97927=CARTESIAN_POINT('Ctrl Pts',(9.88432328285245,-28.2511859592603,123.921275283767));
#97928=CARTESIAN_POINT('Ctrl Pts',(9.88656189011224,-28.229595216878,123.956277905715));
#97929=CARTESIAN_POINT('Ctrl Pts',(9.88880049737203,-28.2090763583662,123.991895575244));
#97930=CARTESIAN_POINT('Ctrl Pts',(9.89103910463182,-28.1896624684553,124.028055770952));
#97931=CARTESIAN_POINT('Ctrl Pts',(9.89510077117281,-28.1544384483701,124.093663820947));
#97932=CARTESIAN_POINT('Ctrl Pts',(9.89916243771379,-28.122730882925,124.161289079108));
#97933=CARTESIAN_POINT('Ctrl Pts',(9.90322410425478,-28.094763080848,124.230539250903));
#97934=CARTESIAN_POINT('Ctrl Pts',(9.90727424497689,-28.0668746431938,124.299592911014));
#97935=CARTESIAN_POINT('Ctrl Pts',(9.91132438569901,-28.0427049908748,124.370261919641));
#97936=CARTESIAN_POINT('Ctrl Pts',(9.91537452642113,-28.022430787494,124.442131223092));
#97937=CARTESIAN_POINT('Ctrl Pts',(9.91941770244941,-28.002191447993,124.513876938815));
#97938=CARTESIAN_POINT('Ctrl Pts',(9.92346087847769,-27.9858343503665,124.586818448078));
#97939=CARTESIAN_POINT('Ctrl Pts',(9.92750405450597,-27.9734876167677,124.660522278925));
#97940=CARTESIAN_POINT('Ctrl Pts',(9.93153868051992,-27.9611669925315,124.734070249922));
#97941=CARTESIAN_POINT('Ctrl Pts',(9.93557330653388,-27.9528399155232,124.80837692485));
#97942=CARTESIAN_POINT('Ctrl Pts',(9.93960793254784,-27.9485839442394,124.882996886077));
#97943=CARTESIAN_POINT('Ctrl Pts',(9.94171371521112,-27.9463626353712,124.921943103184));
#97944=CARTESIAN_POINT('Ctrl Pts',(9.9438194978744,-27.9452494949735,124.960974455546));
#97945=CARTESIAN_POINT('Ctrl Pts',(9.94592528053769,-27.9452500001719,125.000026581306));
#97946=CARTESIAN_POINT('Origin',(-1.54592528053767,-30.,125.));
#97947=CARTESIAN_POINT('',(8.79398045084826,-31.2520409112987,126.629230222815));
#97948=CARTESIAN_POINT('',(8.85202073424513,-31.2520409112987,126.629230222815));
#97949=CARTESIAN_POINT('',(-1.54592528053767,-31.2520409112987,126.629230222815));
#97950=CARTESIAN_POINT('',(9.30407471946233,-27.9452508261495,125.001842569092));
#97951=CARTESIAN_POINT('Ctrl Pts',(8.85202073424513,-31.2520409112987,126.629230222815));
#97952=CARTESIAN_POINT('Ctrl Pts',(8.85588087589068,-31.3086052462336,126.585761313101));
#97953=CARTESIAN_POINT('Ctrl Pts',(8.85974101753623,-31.3628655414002,126.539372164453));
#97954=CARTESIAN_POINT('Ctrl Pts',(8.86360115918179,-31.4145190775282,126.490346718656));
#97955=CARTESIAN_POINT('Ctrl Pts',(8.86746399088779,-31.4662086100386,126.441287107943));
#97956=CARTESIAN_POINT('Ctrl Pts',(8.8713268225938,-31.5152874359326,126.389587897415));
#97957=CARTESIAN_POINT('Ctrl Pts',(8.8751896542998,-31.5614915447377,126.335567938449));
#97958=CARTESIAN_POINT('Ctrl Pts',(8.8790587520412,-31.6077706028556,126.281460351804));
#97959=CARTESIAN_POINT('Ctrl Pts',(8.88292784978261,-31.6511653498478,126.225024893573));
#97960=CARTESIAN_POINT('Ctrl Pts',(8.88679694752401,-31.691454267034,126.166610485566));
#97961=CARTESIAN_POINT('Ctrl Pts',(8.88741372888748,-31.6978768117552,126.157298516568));
#97962=CARTESIAN_POINT('Ctrl Pts',(8.88803051025094,-31.7042205250594,126.147936309128));
#97963=CARTESIAN_POINT('Ctrl Pts',(8.88864729161441,-31.7104846184552,126.138525332405));
#97964=CARTESIAN_POINT('Ctrl Pts',(8.89251643697727,-31.7497800468686,126.079489117783));
#97965=CARTESIAN_POINT('Ctrl Pts',(8.89638558234013,-31.7860924541118,126.018300511658));
#97966=CARTESIAN_POINT('Ctrl Pts',(8.90025472770299,-31.8191789952293,125.955293329725));
#97967=CARTESIAN_POINT('Ctrl Pts',(8.90411810773317,-31.8522162347832,125.892380033477));
#97968=CARTESIAN_POINT('Ctrl Pts',(8.90798148776336,-31.8820369255731,125.827653966917));
#97969=CARTESIAN_POINT('Ctrl Pts',(8.91184486779355,-31.9084416125598,125.761477625377));
#97970=CARTESIAN_POINT('Ctrl Pts',(8.91570371502192,-31.9348153196242,125.695378926792));
#97971=CARTESIAN_POINT('Ctrl Pts',(8.9195625622503,-31.9577808048082,125.627833782111));
#97972=CARTESIAN_POINT('Ctrl Pts',(8.92342140947868,-31.9771854423888,125.559227403572));
#97973=CARTESIAN_POINT('Ctrl Pts',(8.92727782521086,-31.9965778529234,125.490664254561));
#97974=CARTESIAN_POINT('Ctrl Pts',(8.93113424094305,-32.012413735477,125.421041664695));
#97975=CARTESIAN_POINT('Ctrl Pts',(8.93499065667524,-32.0245898244675,125.350761464763));
#97976=CARTESIAN_POINT('Ctrl Pts',(8.9388459323752,-32.036762313967,125.280502041038));
#97977=CARTESIAN_POINT('Ctrl Pts',(8.94270120807515,-32.0452770749115,125.209585871567));
#97978=CARTESIAN_POINT('Ctrl Pts',(8.9465564837751,-32.0500819844574,125.138424779225));
#97979=CARTESIAN_POINT('Ctrl Pts',(8.95041190929307,-32.0548870807244,125.067260921526));
#97980=CARTESIAN_POINT('Ctrl Pts',(8.95426733481105,-32.0559820088406,124.995852606872));
#97981=CARTESIAN_POINT('Ctrl Pts',(8.95812276032902,-32.053366660051,124.924614843033));
#97982=CARTESIAN_POINT('Ctrl Pts',(8.96198221980066,-32.0507485748071,124.853302542717));
#97983=CARTESIAN_POINT('Ctrl Pts',(8.9658416792723,-32.0444124809993,124.782161635874));
#97984=CARTESIAN_POINT('Ctrl Pts',(8.96970113874394,-32.0344103499965,124.711604281712));
#97985=CARTESIAN_POINT('Ctrl Pts',(8.97356278251356,-32.0244025581922,124.641006994941));
#97986=CARTESIAN_POINT('Ctrl Pts',(8.97742442628316,-32.0107246920212,124.570994395295));
#97987=CARTESIAN_POINT('Ctrl Pts',(8.98128607005277,-31.9934797877607,124.501967974635));
#97988=CARTESIAN_POINT('Ctrl Pts',(8.98515446830165,-31.9762047200892,124.432820818465));
#97989=CARTESIAN_POINT('Ctrl Pts',(8.98902286655053,-31.9553502997926,124.364663749846));
#97990=CARTESIAN_POINT('Ctrl Pts',(8.9928912647994,-31.9310690911997,124.297881970383));
#97991=CARTESIAN_POINT('Ctrl Pts',(8.99518836401726,-31.9166506312381,124.258226184318));
#97992=CARTESIAN_POINT('Ctrl Pts',(8.99748546323511,-31.9010247667144,124.219054957003));
#97993=CARTESIAN_POINT('Ctrl Pts',(8.99978256245296,-31.8842311475986,124.180444910382));
#97994=CARTESIAN_POINT('Ctrl Pts',(9.00365172642783,-31.855944486933,124.115411323546));
#97995=CARTESIAN_POINT('Ctrl Pts',(9.00752089040269,-31.8242315741275,124.051716583882));
#97996=CARTESIAN_POINT('Ctrl Pts',(9.01139005437756,-31.7892411653051,123.989745767206));
#97997=CARTESIAN_POINT('Ctrl Pts',(9.01525345456108,-31.7543028807703,123.927867266819));
#97998=CARTESIAN_POINT('Ctrl Pts',(9.01911685474461,-31.7160970285483,123.867708011387));
#97999=CARTESIAN_POINT('Ctrl Pts',(9.02298025492813,-31.6748199922309,123.809632176122));
#98000=CARTESIAN_POINT('Ctrl Pts',(9.02683912447235,-31.6335913618136,123.751624446839));
#98001=CARTESIAN_POINT('Ctrl Pts',(9.03069799401657,-31.5892989813561,123.695695678629));
#98002=CARTESIAN_POINT('Ctrl Pts',(9.03455686356078,-31.5421837177392,123.642183022922));
#98003=CARTESIAN_POINT('Ctrl Pts',(9.0384133029273,-31.4950981256261,123.588704067568));
#98004=CARTESIAN_POINT('Ctrl Pts',(9.04226974229383,-31.445193497629,123.537638569641));
#98005=CARTESIAN_POINT('Ctrl Pts',(9.04612618166035,-31.3927514328102,123.489291223));
#98006=CARTESIAN_POINT('Ctrl Pts',(9.04998148226639,-31.3403248535067,123.440958152752));
#98007=CARTESIAN_POINT('Ctrl Pts',(9.05383678287242,-31.2853626818514,123.395341969407));
#98008=CARTESIAN_POINT('Ctrl Pts',(9.05769208347846,-31.2281826486284,123.35270981788));
#98009=CARTESIAN_POINT('Ctrl Pts',(9.06154753512888,-31.1710003751851,123.310075996096));
#98010=CARTESIAN_POINT('Ctrl Pts',(9.0654029867793,-31.1116004584095,123.270426726825));
#98011=CARTESIAN_POINT('Ctrl Pts',(9.06925843842972,-31.050331514329,123.233987182236));
#98012=CARTESIAN_POINT('Ctrl Pts',(9.07311792570109,-30.9889984381425,123.197509495244));
#98013=CARTESIAN_POINT('Ctrl Pts',(9.07697741297245,-30.9257928476536,123.164248488503));
#98014=CARTESIAN_POINT('Ctrl Pts',(9.08083690024381,-30.8610892111209,123.134384033894));
#98015=CARTESIAN_POINT('Ctrl Pts',(9.08469857279461,-30.7963489387564,123.104502669738));
#98016=CARTESIAN_POINT('Ctrl Pts',(9.08856024534542,-30.7301093830888,123.078021866545));
#98017=CARTESIAN_POINT('Ctrl Pts',(9.09242191789622,-30.6627637449199,123.055072808324));
#98018=CARTESIAN_POINT('Ctrl Pts',(9.09629034614531,-30.5953002907513,123.032083602496));
#98019=CARTESIAN_POINT('Ctrl Pts',(9.10015877439439,-30.5267273582656,123.012638609793));
#98020=CARTESIAN_POINT('Ctrl Pts',(9.10402720264347,-30.4574513233694,122.996818568065));
#98021=CARTESIAN_POINT('Ctrl Pts',(9.10632407952615,-30.4163187204538,122.987425428064));
#98022=CARTESIAN_POINT('Ctrl Pts',(9.10862095640884,-30.374938423874,122.979309238762));
#98023=CARTESIAN_POINT('Ctrl Pts',(9.11091783329152,-30.3333962858509,122.97247824202));
#98024=CARTESIAN_POINT('Ctrl Pts',(9.11478641244339,-30.2634277776161,122.960972944639));
#98025=CARTESIAN_POINT('Ctrl Pts',(9.11865499159526,-30.1927257528652,122.953071184525));
#98026=CARTESIAN_POINT('Ctrl Pts',(9.12252357074712,-30.1216942904492,122.94885688891));
#98027=CARTESIAN_POINT('Ctrl Pts',(9.12638638395902,-30.0507686971733,122.94464887451));
#98028=CARTESIAN_POINT('Ctrl Pts',(9.13024919717092,-29.9795151219791,122.944117443843));
#98029=CARTESIAN_POINT('Ctrl Pts',(9.13411201038282,-29.9083459260032,122.947295176305));
#98030=CARTESIAN_POINT('Ctrl Pts',(9.13797029260362,-29.8372602098581,122.950469181361));
#98031=CARTESIAN_POINT('Ctrl Pts',(9.14182857482442,-29.7662591594153,122.957343685967));
#98032=CARTESIAN_POINT('Ctrl Pts',(9.14568685704522,-29.6957565667091,122.967899240736));
#98033=CARTESIAN_POINT('Ctrl Pts',(9.14954270918848,-29.6252983789367,122.978448147258));
#98034=CARTESIAN_POINT('Ctrl Pts',(9.15339856133174,-29.5553385054741,122.992673432437));
#98035=CARTESIAN_POINT('Ctrl Pts',(9.157254413475,-29.4862855672259,123.010503821552));
#98036=CARTESIAN_POINT('Ctrl Pts',(9.16110912781955,-29.4172530053669,123.028328949211));
#98037=CARTESIAN_POINT('Ctrl Pts',(9.16496384216409,-29.3491273176599,123.049756947452));
#98038=CARTESIAN_POINT('Ctrl Pts',(9.16881855650864,-29.2823051789703,123.074665819561));
#98039=CARTESIAN_POINT('Ctrl Pts',(9.17267342372151,-29.2154803902819,123.099575679493));
#98040=CARTESIAN_POINT('Ctrl Pts',(9.17652829093437,-29.1499597077937,123.127966515567));
#98041=CARTESIAN_POINT('Ctrl Pts',(9.18038315814724,-29.0861212959532,123.15966761785));
#98042=CARTESIAN_POINT('Ctrl Pts',(9.18424206777992,-29.0222159397417,123.191401963603));
#98043=CARTESIAN_POINT('Ctrl Pts',(9.18810097741259,-28.9599968118557,123.226453288522));
#98044=CARTESIAN_POINT('Ctrl Pts',(9.19195988704527,-28.8998180399836,123.264604593369));
#98045=CARTESIAN_POINT('Ctrl Pts',(9.19582098491875,-28.83960514302,123.30277753237));
#98046=CARTESIAN_POINT('Ctrl Pts',(9.19968208279223,-28.781435301757,123.34405366931));
#98047=CARTESIAN_POINT('Ctrl Pts',(9.20354318066571,-28.7256318965417,123.388173861923));
#98048=CARTESIAN_POINT('Ctrl Pts',(9.20741104515668,-28.6697306952305,123.43237137567));
#98049=CARTESIAN_POINT('Ctrl Pts',(9.21127890964764,-28.6162045750296,123.479422575318));
#98050=CARTESIAN_POINT('Ctrl Pts',(9.21514677413861,-28.5653416776921,123.529029891285));
#98051=CARTESIAN_POINT('Ctrl Pts',(9.21744888413577,-28.5350686459666,123.558555614921));
#98052=CARTESIAN_POINT('Ctrl Pts',(9.21975099413293,-28.5057383286815,123.588986158559));
#98053=CARTESIAN_POINT('Ctrl Pts',(9.22205310413008,-28.4774045762066,123.620253379079));
#98054=CARTESIAN_POINT('Ctrl Pts',(9.22588174222822,-28.4302827252427,123.672253879425));
#98055=CARTESIAN_POINT('Ctrl Pts',(9.22971038032636,-28.3857258767059,123.726783942029));
#98056=CARTESIAN_POINT('Ctrl Pts',(9.2335390184245,-28.3440213305649,123.783557560393));
#98057=CARTESIAN_POINT('Ctrl Pts',(9.23736240728238,-28.3023739632892,123.840253339496));
#98058=CARTESIAN_POINT('Ctrl Pts',(9.24118579614027,-28.2635714374772,123.899186180647));
#98059=CARTESIAN_POINT('Ctrl Pts',(9.24500918499815,-28.2278628871692,123.960034800665));
#98060=CARTESIAN_POINT('Ctrl Pts',(9.24882867560751,-28.1921907445636,124.020821380683));
#98061=CARTESIAN_POINT('Ctrl Pts',(9.25264816621688,-28.1596065714772,124.083519439945));
#98062=CARTESIAN_POINT('Ctrl Pts',(9.25646765682624,-28.1303168889735,124.147777830116));
#98063=CARTESIAN_POINT('Ctrl Pts',(9.26043491204592,-28.0998940766984,124.214522184242));
#98064=CARTESIAN_POINT('Ctrl Pts',(9.26440216726559,-28.0730261974045,124.282949611777));
#98065=CARTESIAN_POINT('Ctrl Pts',(9.26836942248526,-28.0498921286478,124.352638545641));
#98066=CARTESIAN_POINT('Ctrl Pts',(9.27218609599499,-28.0276361399335,124.419682356304));
#98067=CARTESIAN_POINT('Ctrl Pts',(9.27600276950471,-28.0088357520803,124.487893114409));
#98068=CARTESIAN_POINT('Ctrl Pts',(9.27981944301444,-27.9936002428959,124.556877469324));
#98069=CARTESIAN_POINT('Ctrl Pts',(9.28363613777674,-27.9783646488747,124.625862208369));
#98070=CARTESIAN_POINT('Ctrl Pts',(9.28745283253905,-27.9666940698592,124.695620065554));
#98071=CARTESIAN_POINT('Ctrl Pts',(9.29126952730136,-27.958646715916,124.765747290177));
#98072=CARTESIAN_POINT('Ctrl Pts',(9.29508879465965,-27.9505939377532,124.835921783189));
#98073=CARTESIAN_POINT('Ctrl Pts',(9.29890806201793,-27.946169296682,124.906465645406));
#98074=CARTESIAN_POINT('Ctrl Pts',(9.30272732937622,-27.9453790517055,124.976971293364));
#98075=CARTESIAN_POINT('Ctrl Pts',(9.30317645940493,-27.945286122168,124.985262465654));
#98076=CARTESIAN_POINT('Ctrl Pts',(9.30362558943363,-27.9452433926879,124.99355311109));
#98077=CARTESIAN_POINT('Ctrl Pts',(9.30407471946233,-27.9452508261495,125.001842569092));
#98078=CARTESIAN_POINT('Ctrl Pts',(9.30407499484945,-27.9458072677851,125.001847151475));
#98079=CARTESIAN_POINT('Ctrl Pts',(9.31377945488918,-27.9442173011669,125.180912509003));
#98080=CARTESIAN_POINT('Ctrl Pts',(9.36052900520844,-28.047648310415,126.041729903938));
#98081=CARTESIAN_POINT('Ctrl Pts',(9.44318615127363,-29.2381865360278,127.294355664252));
#98082=CARTESIAN_POINT('Ctrl Pts',(9.5161388372991,-30.7301642665838,127.03208110996));
#98083=CARTESIAN_POINT('Ctrl Pts',(9.55204643304504,-31.2540479291372,126.631857161249));
#98084=CARTESIAN_POINT('',(9.24592528058238,-27.9452507888899,124.998199460575));
#98085=CARTESIAN_POINT('Ctrl Pts',(9.24592528058238,-27.9452507888899,124.998199460575));
#98086=CARTESIAN_POINT('Ctrl Pts',(9.24973097250201,-27.9451893846722,125.068273054101));
#98087=CARTESIAN_POINT('Ctrl Pts',(9.25353666442164,-27.9487168095866,125.138464582685));
#98088=CARTESIAN_POINT('Ctrl Pts',(9.25734235634127,-27.9558426369693,125.208370433764));
#98089=CARTESIAN_POINT('Ctrl Pts',(9.26114473152835,-27.9629622540585,125.278215360571));
#98090=CARTESIAN_POINT('Ctrl Pts',(9.26494710671543,-27.9736740086242,125.347774607021));
#98091=CARTESIAN_POINT('Ctrl Pts',(9.26874948190251,-27.9879354411875,125.416645861219));
#98092=CARTESIAN_POINT('Ctrl Pts',(9.27254990195913,-28.002189540713,125.485481702739));
#98093=CARTESIAN_POINT('Ctrl Pts',(9.27635032201574,-28.0199895981251,125.553629763388));
#98094=CARTESIAN_POINT('Ctrl Pts',(9.28015074207236,-28.04124173501,125.620696078474));
#98095=CARTESIAN_POINT('Ctrl Pts',(9.28395056576206,-28.0624905369817,125.687751869427));
#98096=CARTESIAN_POINT('Ctrl Pts',(9.28775038945177,-28.0871901908978,125.753725774317));
#98097=CARTESIAN_POINT('Ctrl Pts',(9.29155021314147,-28.1151969900754,125.81823907037));
#98098=CARTESIAN_POINT('Ctrl Pts',(9.29535340916529,-28.1432286452179,125.882809621812));
#98099=CARTESIAN_POINT('Ctrl Pts',(9.29915660518911,-28.1745731087831,125.945916514069));
#98100=CARTESIAN_POINT('Ctrl Pts',(9.30295980121293,-28.2090389723999,126.007202144615));
#98101=CARTESIAN_POINT('Ctrl Pts',(9.30676463915046,-28.2435197156005,126.06851423336));
#98102=CARTESIAN_POINT('Ctrl Pts',(9.31056947708799,-28.2811242729052,126.128003071197));
#98103=CARTESIAN_POINT('Ctrl Pts',(9.31437431502552,-28.3216173481466,126.185339291704));
#98104=CARTESIAN_POINT('Ctrl Pts',(9.31818598381621,-28.3621831209,126.242778448345));
#98105=CARTESIAN_POINT('Ctrl Pts',(9.32199765260691,-28.4056474572905,126.298056875414));
#98106=CARTESIAN_POINT('Ctrl Pts',(9.32580932139761,-28.4517346305472,126.350878198896));
#98107=CARTESIAN_POINT('Ctrl Pts',(9.32899379774474,-28.4902383729238,126.395008018272));
#98108=CARTESIAN_POINT('Ctrl Pts',(9.33217827409187,-28.5305720056642,126.437423346777));
#98109=CARTESIAN_POINT('Ctrl Pts',(9.335362750439,-28.5725566040327,126.477972568693));
#98110=CARTESIAN_POINT('Ctrl Pts',(9.33923133027462,-28.623560522087,126.527232756289));
#98111=CARTESIAN_POINT('Ctrl Pts',(9.34309991011025,-28.677217395628,126.573946306162));
#98112=CARTESIAN_POINT('Ctrl Pts',(9.34696848994588,-28.7332426128984,126.617814354221));
#98113=CARTESIAN_POINT('Ctrl Pts',(9.35083130384245,-28.7891843271776,126.661617018986));
#98114=CARTESIAN_POINT('Ctrl Pts',(9.35469411773903,-28.8474869990078,126.702582303184));
#98115=CARTESIAN_POINT('Ctrl Pts',(9.3585569316356,-28.9078299985523,126.740448864643));
#98116=CARTESIAN_POINT('Ctrl Pts',(9.3624152145392,-28.9681022171288,126.778271009486));
#98117=CARTESIAN_POINT('Ctrl Pts',(9.3662734974428,-29.0304096000489,126.813001394302));
#98118=CARTESIAN_POINT('Ctrl Pts',(9.3701317803464,-29.0944007472384,126.844420655896));
#98119=CARTESIAN_POINT('Ctrl Pts',(9.37398763317096,-29.1583515906063,126.875820128561));
#98120=CARTESIAN_POINT('Ctrl Pts',(9.37784348599552,-29.2239836591128,126.903912401826));
#98121=CARTESIAN_POINT('Ctrl Pts',(9.38169933882007,-29.2909203282268,126.928523679289));
#98122=CARTESIAN_POINT('Ctrl Pts',(9.38555405384343,-29.3578372453881,126.953127694353));
#98123=CARTESIAN_POINT('Ctrl Pts',(9.3894087688668,-29.4260575430735,126.97425258525));
#98124=CARTESIAN_POINT('Ctrl Pts',(9.39326348389015,-29.495185572118,126.991773068375));
#98125=CARTESIAN_POINT('Ctrl Pts',(9.39711835177837,-29.5643163425443,127.009294246302));
#98126=CARTESIAN_POINT('Ctrl Pts',(9.40097321966658,-29.6343544442259,127.023210615427));
#98127=CARTESIAN_POINT('Ctrl Pts',(9.40482808755479,-29.7048917450234,127.033447486498));
#98128=CARTESIAN_POINT('Ctrl Pts',(9.40868699785299,-29.7755030148122,127.043695092471));
#98129=CARTESIAN_POINT('Ctrl Pts',(9.41254590815119,-29.8466140468367,127.050255428029));
#98130=CARTESIAN_POINT('Ctrl Pts',(9.41640481844939,-29.9178101500043,127.053105547958));
#98131=CARTESIAN_POINT('Ctrl Pts',(9.42026591698384,-29.989046625682,127.055957284079));
#98132=CARTESIAN_POINT('Ctrl Pts',(9.4241270155183,-30.0603677824187,127.055094622268));
#98133=CARTESIAN_POINT('Ctrl Pts',(9.42798811405276,-30.1313602478627,127.050546768006));
#98134=CARTESIAN_POINT('Ctrl Pts',(9.43185597919042,-30.2024771281176,127.045990943597));
#98135=CARTESIAN_POINT('Ctrl Pts',(9.43572384432809,-30.2732636842133,127.037737088846));
#98136=CARTESIAN_POINT('Ctrl Pts',(9.43959170946575,-30.3433136699777,127.025866058383));
#98137=CARTESIAN_POINT('Ctrl Pts',(9.44189381340302,-30.3850065269659,127.018800572644));
#98138=CARTESIAN_POINT('Ctrl Pts',(9.4441959173403,-30.4264386684793,127.010454688827));
#98139=CARTESIAN_POINT('Ctrl Pts',(9.44649802127757,-30.467527045114,127.000853823893));
#98140=CARTESIAN_POINT('Ctrl Pts',(9.45045220844813,-30.5381021086969,126.98436298856));
#98141=CARTESIAN_POINT('Ctrl Pts',(9.45440639561869,-30.6079446480582,126.964100582213));
#98142=CARTESIAN_POINT('Ctrl Pts',(9.45836058278925,-30.6766219901702,126.940149541896));
#98143=CARTESIAN_POINT('Ctrl Pts',(9.46222394725379,-30.7437219001114,126.916748626851));
#98144=CARTESIAN_POINT('Ctrl Pts',(9.46608731171834,-30.8097090696607,126.889826857212));
#98145=CARTESIAN_POINT('Ctrl Pts',(9.46995067618289,-30.8741903690013,126.859513044118));
#98146=CARTESIAN_POINT('Ctrl Pts',(9.47395027470645,-30.9409454763712,126.828130273167));
#98147=CARTESIAN_POINT('Ctrl Pts',(9.47794987323002,-31.0060860017405,126.793111865367));
#98148=CARTESIAN_POINT('Ctrl Pts',(9.48194947175358,-31.0691954928842,126.754656251377));
#98149=CARTESIAN_POINT('Ctrl Pts',(9.48594907027715,-31.1323049840279,126.716200637386));
#98150=CARTESIAN_POINT('Ctrl Pts',(9.48994866880071,-31.193382921104,126.674308077663));
#98151=CARTESIAN_POINT('Ctrl Pts',(9.49394826732428,-31.2520409112987,126.629230222815));
#98152=CARTESIAN_POINT('Ctrl Pts',(8.79398045084826,-31.2520409112987,126.629230222815));
#98153=CARTESIAN_POINT('Ctrl Pts',(8.79801550152478,-31.3109295755264,126.58397509816));
#98154=CARTESIAN_POINT('Ctrl Pts',(8.8020505522013,-31.3674504084139,126.535454729334));
#98155=CARTESIAN_POINT('Ctrl Pts',(8.80608560287782,-31.4212258111848,126.483952410329));
#98156=CARTESIAN_POINT('Ctrl Pts',(8.80994358445035,-31.472641401614,126.434710154509));
#98157=CARTESIAN_POINT('Ctrl Pts',(8.81380156602287,-31.5215470665571,126.382742547341));
#98158=CARTESIAN_POINT('Ctrl Pts',(8.81765954759539,-31.5676458651896,126.328338813652));
#98159=CARTESIAN_POINT('Ctrl Pts',(8.8215154555658,-31.6137198864705,126.273964321082));
#98160=CARTESIAN_POINT('Ctrl Pts',(8.82537136353622,-31.6569897214282,126.21715667007));
#98161=CARTESIAN_POINT('Ctrl Pts',(8.82922727150664,-31.6971967434146,126.158240379473));
#98162=CARTESIAN_POINT('Ctrl Pts',(8.8330823968517,-31.7373956046681,126.09933604699));
#98163=CARTESIAN_POINT('Ctrl Pts',(8.83693752219675,-31.7745326139107,126.038324326127));
#98164=CARTESIAN_POINT('Ctrl Pts',(8.84079264754181,-31.808391781376,125.975559699635));
#98165=CARTESIAN_POINT('Ctrl Pts',(8.84464827998394,-31.8422554026225,125.912786817183));
#98166=CARTESIAN_POINT('Ctrl Pts',(8.84850391242607,-31.8728400978263,125.848261000111));
#98167=CARTESIAN_POINT('Ctrl Pts',(8.8523595448682,-31.8999760773574,125.782360829777));
#98168=CARTESIAN_POINT('Ctrl Pts',(8.85621943139899,-31.9271419972069,125.71638794889));
#98169=CARTESIAN_POINT('Ctrl Pts',(8.86007931792977,-31.95085142459,125.649038139322));
#98170=CARTESIAN_POINT('Ctrl Pts',(8.86393920446055,-31.9709832927106,125.580708551991));
#98171=CARTESIAN_POINT('Ctrl Pts',(8.86780159646662,-31.9911282285465,125.51233461152));
#98172=CARTESIAN_POINT('Ctrl Pts',(8.87166398847269,-32.007690871926,125.442980100085));
#98173=CARTESIAN_POINT('Ctrl Pts',(8.87552638047876,-32.0206011140789,125.373053213742));
#98174=CARTESIAN_POINT('Ctrl Pts',(8.87939521059924,-32.0335328759573,125.303009768206));
#98175=CARTESIAN_POINT('Ctrl Pts',(8.88326404071972,-32.0428000276362,125.232392525058));
#98176=CARTESIAN_POINT('Ctrl Pts',(8.88713287084019,-32.0483842978989,125.161614759911));
#98177=CARTESIAN_POINT('Ctrl Pts',(8.88836246958838,-32.0501591010075,125.139120039617));
#98178=CARTESIAN_POINT('Ctrl Pts',(8.88959206833657,-32.05156228863,125.116609097887));
#98179=CARTESIAN_POINT('Ctrl Pts',(8.89082166708476,-32.0525943745539,125.094095143603));
#98180=CARTESIAN_POINT('Ctrl Pts',(8.89469075533167,-32.0558419636751,125.023252134009));
#98181=CARTESIAN_POINT('Ctrl Pts',(8.89855984357858,-32.0554240066368,124.9521020425));
#98182=CARTESIAN_POINT('Ctrl Pts',(8.90242893182549,-32.0513044404969,124.881056085075));
#98183=CARTESIAN_POINT('Ctrl Pts',(8.90629225525498,-32.0471910123784,124.810115983849));
#98184=CARTESIAN_POINT('Ctrl Pts',(8.91015557868447,-32.0393869507265,124.739280189741));
#98185=CARTESIAN_POINT('Ctrl Pts',(8.91401890211395,-32.0279081570336,124.66896213338));
#98186=CARTESIAN_POINT('Ctrl Pts',(8.91787769376668,-32.016442828258,124.598726561889));
#98187=CARTESIAN_POINT('Ctrl Pts',(8.92173648541941,-32.0013114075459,124.529007998911));
#98188=CARTESIAN_POINT('Ctrl Pts',(8.92559527707215,-31.9825816351369,124.460215207219));
#98189=CARTESIAN_POINT('Ctrl Pts',(8.92945163788956,-31.963863661497,124.391465751358));
#98190=CARTESIAN_POINT('Ctrl Pts',(8.93330799870698,-31.9415519607138,124.323641377361));
#98191=CARTESIAN_POINT('Ctrl Pts',(8.93716435952439,-31.9157651374972,124.257139649429));
#98192=CARTESIAN_POINT('Ctrl Pts',(8.94101958104529,-31.8899859325611,124.190657568307));
#98193=CARTESIAN_POINT('Ctrl Pts',(8.94487480256618,-31.8607338189391,124.125497810172));
#98194=CARTESIAN_POINT('Ctrl Pts',(8.94873002408707,-31.8281763781024,124.062040143157));
#98195=CARTESIAN_POINT('Ctrl Pts',(8.95258539623725,-31.7956176651977,123.998579996756));
#98196=CARTESIAN_POINT('Ctrl Pts',(8.95644076838744,-31.7597535923906,123.936822504717));
#98197=CARTESIAN_POINT('Ctrl Pts',(8.96029614053762,-31.7207979561137,123.877123356403));
#98198=CARTESIAN_POINT('Ctrl Pts',(8.96415554823429,-31.6818015436743,123.817361719002));
#98199=CARTESIAN_POINT('Ctrl Pts',(8.96801495593096,-31.63970737391,123.759663133927));
#98200=CARTESIAN_POINT('Ctrl Pts',(8.97187436362763,-31.5947724051756,123.704354007381));
#98201=CARTESIAN_POINT('Ctrl Pts',(8.97573595644216,-31.549811995179,123.649013565936));
#98202=CARTESIAN_POINT('Ctrl Pts',(8.9795975492567,-31.5020079100707,123.59606563689));
#98203=CARTESIAN_POINT('Ctrl Pts',(8.98345914207123,-31.4516553700248,123.545801165872));
#98204=CARTESIAN_POINT('Ctrl Pts',(8.98732749120413,-31.4012147321894,123.495448751152));
#98205=CARTESIAN_POINT('Ctrl Pts',(8.99119584033703,-31.3482170985631,123.447789493155));
#98206=CARTESIAN_POINT('Ctrl Pts',(8.99506418946993,-31.2929917361105,123.40307485058));
#98207=CARTESIAN_POINT('Ctrl Pts',(8.99736177228772,-31.2601909625717,123.376516856212));
#98208=CARTESIAN_POINT('Ctrl Pts',(8.99965935510552,-31.2266049064413,123.350996827091));
#98209=CARTESIAN_POINT('Ctrl Pts',(9.00195693792331,-31.1923070848524,123.326560016639));
#98210=CARTESIAN_POINT('Ctrl Pts',(9.00582595070848,-31.1345512950706,123.285409668833));
#98211=CARTESIAN_POINT('Ctrl Pts',(9.00969496349365,-31.0745495097668,123.247172220975));
#98212=CARTESIAN_POINT('Ctrl Pts',(9.01356397627882,-31.0126276336229,123.212100998903));
#98213=CARTESIAN_POINT('Ctrl Pts',(9.01742722403229,-30.9507980243179,123.177082034789));
#98214=CARTESIAN_POINT('Ctrl Pts',(9.02129047178576,-30.8870544225097,123.145220169151));
#98215=CARTESIAN_POINT('Ctrl Pts',(9.02515371953923,-30.8217527781783,123.116726272138));
#98216=CARTESIAN_POINT('Ctrl Pts',(9.02901243556288,-30.7565277350457,123.0882657995));
#98217=CARTESIAN_POINT('Ctrl Pts',(9.03287115158653,-30.6897487227971,123.063165641315));
#98218=CARTESIAN_POINT('Ctrl Pts',(9.03672986761017,-30.6217958861558,123.041590584566));
#98219=CARTESIAN_POINT('Ctrl Pts',(9.04058615286833,-30.5538858558287,123.020029118841));
#98220=CARTESIAN_POINT('Ctrl Pts',(9.04444243812649,-30.4848039300759,123.00198849557));
#98221=CARTESIAN_POINT('Ctrl Pts',(9.04829872338465,-30.4149484329774,122.987584694833));
#98222=CARTESIAN_POINT('Ctrl Pts',(9.05215386952663,-30.3451135706405,122.973185148865));
#98223=CARTESIAN_POINT('Ctrl Pts',(9.05600901566861,-30.2745060661412,122.962420390725));
#98224=CARTESIAN_POINT('Ctrl Pts',(9.05986416181059,-30.2035358559927,122.955355601131));
#98225=CARTESIAN_POINT('Ctrl Pts',(9.06371945887285,-30.1325628675205,122.948290534967));
#98226=CARTESIAN_POINT('Ctrl Pts',(9.06757475593511,-30.0612276288406,122.944925770849));
#98227=CARTESIAN_POINT('Ctrl Pts',(9.07143005299737,-29.9899449123528,122.945274602845));
#98228=CARTESIAN_POINT('Ctrl Pts',(9.07528938656523,-29.9185875626837,122.94562380007));
#98229=CARTESIAN_POINT('Ctrl Pts',(9.0791487201331,-29.8472833317735,122.949694352633));
#98230=CARTESIAN_POINT('Ctrl Pts',(9.08300805370096,-29.776445799497,122.957447410239));
#98231=CARTESIAN_POINT('Ctrl Pts',(9.08686957281574,-29.7055681518101,122.965204858416));
#98232=CARTESIAN_POINT('Ctrl Pts',(9.09073109193052,-29.6351582086173,122.976648885059));
#98233=CARTESIAN_POINT('Ctrl Pts',(9.09459261104529,-29.5656205092378,122.991689261965));
#98234=CARTESIAN_POINT('Ctrl Pts',(9.09846088795565,-29.495961116415,123.006755960065));
#98235=CARTESIAN_POINT('Ctrl Pts',(9.10232916486601,-29.4271774839988,123.025431446726));
#98236=CARTESIAN_POINT('Ctrl Pts',(9.10619744177637,-29.3596594419617,123.047575473359));
#98237=CARTESIAN_POINT('Ctrl Pts',(9.1084956974382,-29.3195450122081,123.060731882727));
#98238=CARTESIAN_POINT('Ctrl Pts',(9.11079395310004,-29.279876966924,123.075111715127));
#98239=CARTESIAN_POINT('Ctrl Pts',(9.11309220876188,-29.2407332677406,123.090677714008));
#98240=CARTESIAN_POINT('Ctrl Pts',(9.11696135405773,-29.174834307032,123.116883289109));
#98241=CARTESIAN_POINT('Ctrl Pts',(9.12083049935358,-29.1101645790708,123.146555878858));
#98242=CARTESIAN_POINT('Ctrl Pts',(9.12469964464943,-29.047113690358,123.179559052483));
#98243=CARTESIAN_POINT('Ctrl Pts',(9.12856302461331,-28.9841567524474,123.212513048774));
#98244=CARTESIAN_POINT('Ctrl Pts',(9.1324264045772,-28.9228142925019,123.248787554408));
#98245=CARTESIAN_POINT('Ctrl Pts',(9.13628978454108,-28.8634565421432,123.2881978704));
#98246=CARTESIAN_POINT('Ctrl Pts',(9.14014863170448,-28.804168434647,123.327561947321));
#98247=CARTESIAN_POINT('Ctrl Pts',(9.14400747886788,-28.7468608140558,123.37005425914));
#98248=CARTESIAN_POINT('Ctrl Pts',(9.14786632603128,-28.6918783167288,123.415444786618));
#98249=CARTESIAN_POINT('Ctrl Pts',(9.15172274169934,-28.6369304643827,123.460806713105));
#98250=CARTESIAN_POINT('Ctrl Pts',(9.1555791573674,-28.5843052023202,123.509062923585));
#98251=CARTESIAN_POINT('Ctrl Pts',(9.15943557303546,-28.5343160214053,123.559941654866));
#98252=CARTESIAN_POINT('Ctrl Pts',(9.16329084867223,-28.4843416182621,123.610805345406));
#98253=CARTESIAN_POINT('Ctrl Pts',(9.167146124309,-28.4370020894456,123.664289671307));
#98254=CARTESIAN_POINT('Ctrl Pts',(9.17100139994577,-28.3925745451105,123.720085561659));
#98255=CARTESIAN_POINT('Ctrl Pts',(9.17485682540158,-28.3481452742862,123.775883620284));
#98256=CARTESIAN_POINT('Ctrl Pts',(9.17871225085739,-28.3066285134754,123.833993040319));
#98257=CARTESIAN_POINT('Ctrl Pts',(9.1825676763132,-28.2682604036012,123.894072546337));
#98258=CARTESIAN_POINT('Ctrl Pts',(9.18642713572464,-28.2298521489351,123.954214913916));
#98259=CARTESIAN_POINT('Ctrl Pts',(9.19028659513609,-28.1945993836681,124.016331072083));
#98260=CARTESIAN_POINT('Ctrl Pts',(9.19414605454754,-28.1626937934211,124.080052465753));
#98261=CARTESIAN_POINT('Ctrl Pts',(9.19800769825797,-28.1307701458917,124.143809923172));
#98262=CARTESIAN_POINT('Ctrl Pts',(9.20186934196841,-28.1021976391511,124.209173979329));
#98263=CARTESIAN_POINT('Ctrl Pts',(9.20573098567884,-28.0771198912845,124.275755807751));
#98264=CARTESIAN_POINT('Ctrl Pts',(9.20959938387077,-28.0519982794066,124.342454095837));
#98265=CARTESIAN_POINT('Ctrl Pts',(9.2134677820627,-28.0303837780611,124.410373945818));
#98266=CARTESIAN_POINT('Ctrl Pts',(9.21733618025462,-28.0123700035947,124.479111758733));
#98267=CARTESIAN_POINT('Ctrl Pts',(9.21963328003656,-28.0016732150674,124.519929070505));
#98268=CARTESIAN_POINT('Ctrl Pts',(9.2219303798185,-27.9922451094651,124.561034597905));
#98269=CARTESIAN_POINT('Ctrl Pts',(9.22422747960044,-27.9840966569744,124.602342768105));
#98270=CARTESIAN_POINT('Ctrl Pts',(9.22983481597178,-27.9642058736569,124.703178094032));
#98271=CARTESIAN_POINT('Ctrl Pts',(9.23544215234312,-27.9518758969885,124.805550439328));
#98272=CARTESIAN_POINT('Ctrl Pts',(9.24104948871445,-27.9472870601179,124.908527878888));
#98273=CARTESIAN_POINT('Ctrl Pts',(9.24267475265553,-27.9459570041692,124.938375476424));
#98274=CARTESIAN_POINT('Ctrl Pts',(9.2443000165966,-27.9452770122708,124.968273736077));
#98275=CARTESIAN_POINT('Ctrl Pts',(9.24592528053768,-27.9452507888906,124.998199459752));
#98276=CARTESIAN_POINT('Origin',(-1.54592528053767,-30.,125.));
#98277=CARTESIAN_POINT('',(8.09385900495164,-31.2520409112987,126.629230222815));
#98278=CARTESIAN_POINT('',(8.15211359149425,-31.2520409112987,126.629230222815));
#98279=CARTESIAN_POINT('',(-1.54592528053767,-31.2520409112987,126.629230222815));
#98280=CARTESIAN_POINT('',(8.60407471942971,-27.9452501088748,124.999331104759));
#98281=CARTESIAN_POINT('Ctrl Pts',(8.15211359149425,-31.2520409112987,126.629230222815));
#98282=CARTESIAN_POINT('Ctrl Pts',(8.15596912461769,-31.3085645256072,126.58579260634));
#98283=CARTESIAN_POINT('Ctrl Pts',(8.15982465774113,-31.3628527074967,126.539388745966));
#98284=CARTESIAN_POINT('Ctrl Pts',(8.16368019086458,-31.4145858102238,126.490283378426));
#98285=CARTESIAN_POINT('Ctrl Pts',(8.16753532502306,-31.4663135596848,126.441183092238));
#98286=CARTESIAN_POINT('Ctrl Pts',(8.17139045918155,-31.5154864035061,126.389382189262));
#98287=CARTESIAN_POINT('Ctrl Pts',(8.17524559334003,-31.561820363806,126.335183400773));
#98288=CARTESIAN_POINT('Ctrl Pts',(8.17912809944362,-31.6084833011442,126.280599793961));
#98289=CARTESIAN_POINT('Ctrl Pts',(8.1830106055472,-31.6522665411257,126.223584480783));
#98290=CARTESIAN_POINT('Ctrl Pts',(8.18689311165078,-31.6929215457164,126.164480228492));
#98291=CARTESIAN_POINT('Ctrl Pts',(8.19075363020041,-31.7333463113627,126.105710697616));
#98292=CARTESIAN_POINT('Ctrl Pts',(8.19461414875003,-31.7706779722671,126.044876273873));
#98293=CARTESIAN_POINT('Ctrl Pts',(8.19847466729966,-31.8047171615244,125.982340841765));
#98294=CARTESIAN_POINT('Ctrl Pts',(8.20236816718022,-31.839047155696,125.919271154542));
#98295=CARTESIAN_POINT('Ctrl Pts',(8.20626166706079,-31.8700279324735,125.854471708577));
#98296=CARTESIAN_POINT('Ctrl Pts',(8.21015516694136,-31.8975043980646,125.788336617078));
#98297=CARTESIAN_POINT('Ctrl Pts',(8.21404866682192,-31.9249808636556,125.722201525579));
#98298=CARTESIAN_POINT('Ctrl Pts',(8.21794216670249,-31.9489529114773,125.654731281105));
#98299=CARTESIAN_POINT('Ctrl Pts',(8.22183566658305,-31.9693172396355,125.586333669658));
#98300=CARTESIAN_POINT('Ctrl Pts',(8.22570474050503,-31.9895538117255,125.518365152156));
#98301=CARTESIAN_POINT('Ctrl Pts',(8.22957381442702,-32.0063071187198,125.449214612482));
#98302=CARTESIAN_POINT('Ctrl Pts',(8.233442888349,-32.0194429894025,125.379272428543));
#98303=CARTESIAN_POINT('Ctrl Pts',(8.23730619731142,-32.0325592875042,125.309434459171));
#98304=CARTESIAN_POINT('Ctrl Pts',(8.24116950627384,-32.0420687593893,125.238807660473));
#98305=CARTESIAN_POINT('Ctrl Pts',(8.24503281523626,-32.0478871302918,125.167797092004));
#98306=CARTESIAN_POINT('Ctrl Pts',(8.24889159228266,-32.0536986758619,125.096869823612));
#98307=CARTESIAN_POINT('Ctrl Pts',(8.25275036932905,-32.0558276816266,125.025560161487));
#98308=CARTESIAN_POINT('Ctrl Pts',(8.25660914637545,-32.0542413071686,124.954281137128));
#98309=CARTESIAN_POINT('Ctrl Pts',(8.26046549250875,-32.0526559320786,124.883047016403));
#98310=CARTESIAN_POINT('Ctrl Pts',(8.26432183864205,-32.0473598312168,124.811843979669));
#98311=CARTESIAN_POINT('Ctrl Pts',(8.26817818477534,-32.0383722280202,124.741086457411));
#98312=CARTESIAN_POINT('Ctrl Pts',(8.27203339155665,-32.0293872801981,124.670349840363));
#98313=CARTESIAN_POINT('Ctrl Pts',(8.27588859833795,-32.0167130564608,124.600058958127));
#98314=CARTESIAN_POINT('Ctrl Pts',(8.27974380511925,-32.0004206032274,124.5306227821));
#98315=CARTESIAN_POINT('Ctrl Pts',(8.28359916249661,-31.9841275135615,124.461183893686));
#98316=CARTESIAN_POINT('Ctrl Pts',(8.28745451987398,-31.9642160269044,124.392600250205));
#98317=CARTESIAN_POINT('Ctrl Pts',(8.29130987725134,-31.9408078475603,124.325268600591));
#98318=CARTESIAN_POINT('Ctrl Pts',(8.29516927022752,-31.9173751656833,124.257866471513));
#98319=CARTESIAN_POINT('Ctrl Pts',(8.2990286632037,-31.8904386444525,124.191719412194));
#98320=CARTESIAN_POINT('Ctrl Pts',(8.30288805617987,-31.860168938256,124.127206162002));
#98321=CARTESIAN_POINT('Ctrl Pts',(8.30674963428127,-31.8298820938467,124.062656385462));
#98322=CARTESIAN_POINT('Ctrl Pts',(8.31061121238265,-31.7962585367315,123.999742688151));
#98323=CARTESIAN_POINT('Ctrl Pts',(8.31447279048405,-31.7595146056693,123.938818622979));
#98324=CARTESIAN_POINT('Ctrl Pts',(8.31834112507632,-31.7227063848198,123.877787960742));
#98325=CARTESIAN_POINT('Ctrl Pts',(8.3222094596686,-31.6827671620172,123.818754283444));
#98326=CARTESIAN_POINT('Ctrl Pts',(8.32607779426087,-31.6399558407878,123.762041033489));
#98327=CARTESIAN_POINT('Ctrl Pts',(8.32837550864778,-31.6145267610728,123.728354482534));
#98328=CARTESIAN_POINT('Ctrl Pts',(8.33067322303469,-31.5880851379374,123.695485968772));
#98329=CARTESIAN_POINT('Ctrl Pts',(8.3329709374216,-31.5606914158628,123.663497150414));
#98330=CARTESIAN_POINT('Ctrl Pts',(8.33684001301417,-31.5145636716695,123.609631814909));
#98331=CARTESIAN_POINT('Ctrl Pts',(8.34070908860674,-31.4655536592048,123.55805183888));
#98332=CARTESIAN_POINT('Ctrl Pts',(8.34457816419931,-31.4139165827671,123.509081672433));
#98333=CARTESIAN_POINT('Ctrl Pts',(8.34844147485484,-31.3623564457655,123.460184471715));
#98334=CARTESIAN_POINT('Ctrl Pts',(8.35230478551036,-31.3081773642485,123.413889693321));
#98335=CARTESIAN_POINT('Ctrl Pts',(8.35616809616589,-31.2516739392184,123.370487829938));
#98336=CARTESIAN_POINT('Ctrl Pts',(8.3600268749303,-31.1952367960364,123.327136879498));
#98337=CARTESIAN_POINT('Ctrl Pts',(8.36388565369471,-31.1364811086558,123.286672397797));
#98338=CARTESIAN_POINT('Ctrl Pts',(8.36774443245912,-31.0757360717717,123.249345988955));
#98339=CARTESIAN_POINT('Ctrl Pts',(8.37160078032483,-31.0150293021842,123.212043094474));
#98340=CARTESIAN_POINT('Ctrl Pts',(8.37545712819055,-30.952336082378,123.177874604482));
#98341=CARTESIAN_POINT('Ctrl Pts',(8.37931347605626,-30.8880150199357,123.14704914073));
#98342=CARTESIAN_POINT('Ctrl Pts',(8.3831686845817,-30.8237129608559,123.11623278422));
#98343=CARTESIAN_POINT('Ctrl Pts',(8.38702389310713,-30.7577844517736,123.088757702958));
#98344=CARTESIAN_POINT('Ctrl Pts',(8.39087910163257,-30.6906116207524,123.064786019123));
#98345=CARTESIAN_POINT('Ctrl Pts',(8.39473446076312,-30.6234361656004,123.040813398826));
#98346=CARTESIAN_POINT('Ctrl Pts',(8.39858981989367,-30.555016750266,123.020344608877));
#98347=CARTESIAN_POINT('Ctrl Pts',(8.40244517902421,-30.4857527091902,123.00349258253));
#98348=CARTESIAN_POINT('Ctrl Pts',(8.40630457375508,-30.4164161659229,122.98662291631));
#98349=CARTESIAN_POINT('Ctrl Pts',(8.41016396848594,-30.3462337050095,122.973377686177));
#98350=CARTESIAN_POINT('Ctrl Pts',(8.4140233632168,-30.2756160790219,122.963818932539));
#98351=CARTESIAN_POINT('Ctrl Pts',(8.41788494307635,-30.2049584704434,122.954254766886));
#98352=CARTESIAN_POINT('Ctrl Pts',(8.4217465229359,-30.1338656906824,122.948381272767));
#98353=CARTESIAN_POINT('Ctrl Pts',(8.42560810279545,-30.0627521096263,122.946208448932));
#98354=CARTESIAN_POINT('Ctrl Pts',(8.42947643913209,-29.9915141035166,122.94403182338));
#98355=CARTESIAN_POINT('Ctrl Pts',(8.43334477546873,-29.9202557092741,122.945568785037));
#98356=CARTESIAN_POINT('Ctrl Pts',(8.43721311180537,-29.849389085236,122.950777241281));
#98357=CARTESIAN_POINT('Ctrl Pts',(8.43951081062364,-29.8072960136578,122.953870939117));
#98358=CARTESIAN_POINT('Ctrl Pts',(8.4418085094419,-29.7653410419802,122.958258975172));
#98359=CARTESIAN_POINT('Ctrl Pts',(8.44410620826017,-29.7236087531083,122.963924008996));
#98360=CARTESIAN_POINT('Ctrl Pts',(8.44797527432581,-29.6533362781294,122.973463288015));
#98361=CARTESIAN_POINT('Ctrl Pts',(8.45184434039146,-29.5834205882342,122.986663565789));
#98362=CARTESIAN_POINT('Ctrl Pts',(8.4557134064571,-29.5142726801353,123.003486405446));
#98363=CARTESIAN_POINT('Ctrl Pts',(8.45957670756576,-29.4452278032871,123.020284178862));
#98364=CARTESIAN_POINT('Ctrl Pts',(8.46344000867443,-29.3769489055926,123.040693686052));
#98365=CARTESIAN_POINT('Ctrl Pts',(8.46730330978309,-29.3098398221709,123.064624973955));
#98366=CARTESIAN_POINT('Ctrl Pts',(8.47116207901698,-29.2428094615703,123.088528189078));
#98367=CARTESIAN_POINT('Ctrl Pts',(8.47502084825087,-29.1769466448156,123.115944816475));
#98368=CARTESIAN_POINT('Ctrl Pts',(8.47887961748476,-29.1126412975478,123.146734747619));
#98369=CARTESIAN_POINT('Ctrl Pts',(8.48273595583517,-29.0483764602968,123.177505282233));
#98370=CARTESIAN_POINT('Ctrl Pts',(8.48659229418558,-28.9856675830665,123.211644695218));
#98371=CARTESIAN_POINT('Ctrl Pts',(8.49044863253599,-28.92488443271,123.248964854873));
#98372=CARTESIAN_POINT('Ctrl Pts',(8.49430383157519,-28.8641192400424,123.286273988712));
#98373=CARTESIAN_POINT('Ctrl Pts',(8.4981590306144,-28.805279058515,123.326761749583));
#98374=CARTESIAN_POINT('Ctrl Pts',(8.5020142296536,-28.748707345374,123.370195025477));
#98375=CARTESIAN_POINT('Ctrl Pts',(8.50586957934089,-28.6921334216027,123.413629998597));
#98376=CARTESIAN_POINT('Ctrl Pts',(8.50972492902817,-28.6378285261893,123.460010417677));
#98377=CARTESIAN_POINT('Ctrl Pts',(8.51358027871546,-28.5861041227543,123.509062036566));
#98378=CARTESIAN_POINT('Ctrl Pts',(8.51743966413327,-28.5343255748783,123.55816500206));
#98379=CARTESIAN_POINT('Ctrl Pts',(8.52129904955107,-28.4851332644469,123.6099444142));
#98380=CARTESIAN_POINT('Ctrl Pts',(8.52515843496888,-28.4388020905701,123.664088831512));
#98381=CARTESIAN_POINT('Ctrl Pts',(8.52902000557476,-28.392444683934,123.718263905449));
#98382=CARTESIAN_POINT('Ctrl Pts',(8.53288157618065,-28.3489519350537,123.774806264996));
#98383=CARTESIAN_POINT('Ctrl Pts',(8.53674314678653,-28.3085569824377,123.833373204131));
#98384=CARTESIAN_POINT('Ctrl Pts',(8.54061147406359,-28.268091349925,123.892042619069));
#98385=CARTESIAN_POINT('Ctrl Pts',(8.54447980134064,-28.2307345901141,123.95274327235));
#98386=CARTESIAN_POINT('Ctrl Pts',(8.5483481286177,-28.1966748777856,124.015106063533));
#98387=CARTESIAN_POINT('Ctrl Pts',(8.55064591211137,-28.1764434342746,124.0521495146));
#98388=CARTESIAN_POINT('Ctrl Pts',(8.55294369560505,-28.1573744062158,124.089778988432));
#98389=CARTESIAN_POINT('Ctrl Pts',(8.55524147909873,-28.1394991031592,124.127914009197));
#98390=CARTESIAN_POINT('Ctrl Pts',(8.55943210412707,-28.1068986895066,124.197463456703));
#98391=CARTESIAN_POINT('Ctrl Pts',(8.56362272915541,-28.0781595914887,124.268933251471));
#98392=CARTESIAN_POINT('Ctrl Pts',(8.56781335418376,-28.0534922152104,124.341892861113));
#98393=CARTESIAN_POINT('Ctrl Pts',(8.57199336341184,-28.0288873269709,124.414667647576));
#98394=CARTESIAN_POINT('Ctrl Pts',(8.57617337263993,-28.0083337420086,124.488924404301));
#98395=CARTESIAN_POINT('Ctrl Pts',(8.58035338186801,-27.9919944407361,124.564211936298));
#98396=CARTESIAN_POINT('Ctrl Pts',(8.58451634359201,-27.9757217767101,124.639192420046));
#98397=CARTESIAN_POINT('Ctrl Pts',(8.58867930531602,-27.9636292336692,124.715194960974));
#98398=CARTESIAN_POINT('Ctrl Pts',(8.59284226704002,-27.9558298707247,124.791754843805));
#98399=CARTESIAN_POINT('Ctrl Pts',(8.59658641783658,-27.948815155501,124.860612490186));
#98400=CARTESIAN_POINT('Ctrl Pts',(8.60033056863314,-27.9452727045111,124.929920562533));
#98401=CARTESIAN_POINT('Ctrl Pts',(8.6040747194297,-27.9452501088748,124.999331104759));
#98402=CARTESIAN_POINT('Ctrl Pts',(8.60407471946233,-27.9452501088746,124.999331105364));
#98403=CARTESIAN_POINT('Ctrl Pts',(8.60802536883708,-27.9452262670581,125.072569799569));
#98404=CARTESIAN_POINT('Ctrl Pts',(8.61197601821182,-27.9491225024139,125.145776561612));
#98405=CARTESIAN_POINT('Ctrl Pts',(8.61592666758657,-27.9569024208448,125.218517378142));
#98406=CARTESIAN_POINT('Ctrl Pts',(8.61988033453931,-27.9646882817192,125.291313755434));
#98407=CARTESIAN_POINT('Ctrl Pts',(8.62383400149206,-27.9763636771627,125.363643031206));
#98408=CARTESIAN_POINT('Ctrl Pts',(8.62778766844481,-27.9918407207505,125.43507915563));
#98409=CARTESIAN_POINT('Ctrl Pts',(8.63174857353918,-28.0073460988021,125.506646061123));
#98410=CARTESIAN_POINT('Ctrl Pts',(8.63570947863356,-28.0266669211867,125.577316110013));
#98411=CARTESIAN_POINT('Ctrl Pts',(8.63967038372794,-28.0496648799025,125.646676489301));
#98412=CARTESIAN_POINT('Ctrl Pts',(8.643635483493,-28.0726871938758,125.716110322494));
#98413=CARTESIAN_POINT('Ctrl Pts',(8.64760058325807,-28.0993942353363,125.784231304558));
#98414=CARTESIAN_POINT('Ctrl Pts',(8.65156568302313,-28.1295998064449,125.850647211509));
#98415=CARTESIAN_POINT('Ctrl Pts',(8.65553895292325,-28.1598676164907,125.917199969224));
#98416=CARTESIAN_POINT('Ctrl Pts',(8.65951222282338,-28.1936481395682,125.98204023864));
#98417=CARTESIAN_POINT('Ctrl Pts',(8.6634854927235,-28.2307097802741,126.044801263821));
#98418=CARTESIAN_POINT('Ctrl Pts',(8.6644492451281,-28.2396994150702,126.060024515816));
#98419=CARTESIAN_POINT('Ctrl Pts',(8.66541299753269,-28.2488819004221,126.075125578892));
#98420=CARTESIAN_POINT('Ctrl Pts',(8.66637674993729,-28.2582535674493,126.090099503347));
#98421=CARTESIAN_POINT('Ctrl Pts',(8.67024583822596,-28.2958771385732,126.150213942977));
#98422=CARTESIAN_POINT('Ctrl Pts',(8.67411492651463,-28.3366902277256,126.208496033488));
#98423=CARTESIAN_POINT('Ctrl Pts',(8.6779840148033,-28.3804886013258,126.264587044084));
#98424=CARTESIAN_POINT('Ctrl Pts',(8.6818473382748,-28.4242217167573,126.320594480877));
#98425=CARTESIAN_POINT('Ctrl Pts',(8.6857106617463,-28.4709309909865,126.374416938209));
#98426=CARTESIAN_POINT('Ctrl Pts',(8.6895739852178,-28.520368190857,126.425723420539));
#98427=CARTESIAN_POINT('Ctrl Pts',(8.69343277691273,-28.5697473996361,126.476969719061));
#98428=CARTESIAN_POINT('Ctrl Pts',(8.69729156860766,-28.6218478424875,126.525705556754));
#98429=CARTESIAN_POINT('Ctrl Pts',(8.70115036030259,-28.6763813047308,126.571633262576));
#98430=CARTESIAN_POINT('Ctrl Pts',(8.70500672116229,-28.7308804137692,126.617532036365));
#98431=CARTESIAN_POINT('Ctrl Pts',(8.70886308202199,-28.7878091307132,126.660625875713));
#98432=CARTESIAN_POINT('Ctrl Pts',(8.71271944288169,-28.8468437752777,126.700655251332));
#98433=CARTESIAN_POINT('Ctrl Pts',(8.7165746644449,-28.9058609790565,126.74067280095));
#98434=CARTESIAN_POINT('Ctrl Pts',(8.7204298860081,-28.9669824734465,126.777627411718));
#98435=CARTESIAN_POINT('Ctrl Pts',(8.7242851075713,-29.0298544177493,126.811302048732));
#98436=CARTESIAN_POINT('Ctrl Pts',(8.72814047976376,-29.0927288185526,126.844978001463));
#98437=CARTESIAN_POINT('Ctrl Pts',(8.73199585195621,-29.1573533757876,126.87537349859));
#98438=CARTESIAN_POINT('Ctrl Pts',(8.73585122414867,-29.2233499334031,126.902317596132));
#98439=CARTESIAN_POINT('Ctrl Pts',(8.73971063188726,-29.2894155718077,126.929289896957));
#98440=CARTESIAN_POINT('Ctrl Pts',(8.74357003962586,-29.3568556267428,126.952803402456));
#98441=CARTESIAN_POINT('Ctrl Pts',(8.74742944736446,-29.4252730980761,126.972735803575));
#98442=CARTESIAN_POINT('Ctrl Pts',(8.75129104022078,-29.4937293059824,126.992679490011));
#98443=CARTESIAN_POINT('Ctrl Pts',(8.7551526330771,-29.563163558862,127.00903792439));
#98444=CARTESIAN_POINT('Ctrl Pts',(8.75901422593343,-29.6331675563962,127.02173972628));
#98445=CARTESIAN_POINT('Ctrl Pts',(8.76288257510745,-29.7032940342811,127.03446375149));
#98446=CARTESIAN_POINT('Ctrl Pts',(8.76675092428148,-29.7739917650344,127.043518309254));
#98447=CARTESIAN_POINT('Ctrl Pts',(8.7706192734555,-29.8448469050885,127.048883861921));
#98448=CARTESIAN_POINT('Ctrl Pts',(8.77291685589562,-29.8869308841339,127.05207069926));
#98449=CARTESIAN_POINT('Ctrl Pts',(8.77521443833573,-29.9290703633161,127.053957167721));
#98450=CARTESIAN_POINT('Ctrl Pts',(8.77751202077585,-29.9711791363964,127.054547862748));
#98451=CARTESIAN_POINT('Ctrl Pts',(8.78138027676357,-30.0420743133264,127.055542368771));
#98452=CARTESIAN_POINT('Ctrl Pts',(8.78524853275129,-30.1131598883882,127.052865003948));
#98453=CARTESIAN_POINT('Ctrl Pts',(8.78911678873902,-30.1840239637477,127.046492790915));
#98454=CARTESIAN_POINT('Ctrl Pts',(8.79297966476592,-30.2547894815271,127.04012944034));
#98455=CARTESIAN_POINT('Ctrl Pts',(8.79684254079282,-30.3253336312653,127.030081479718));
#98456=CARTESIAN_POINT('Ctrl Pts',(8.80070541681972,-30.3952438280996,127.016377910722));
#98457=CARTESIAN_POINT('Ctrl Pts',(8.80456421327246,-30.4650801929417,127.002688814034));
#98458=CARTESIAN_POINT('Ctrl Pts',(8.8084230097252,-30.5342834594381,126.985351864656));
#98459=CARTESIAN_POINT('Ctrl Pts',(8.81228180617794,-30.6024472079082,126.964447740253));
#98460=CARTESIAN_POINT('Ctrl Pts',(8.81613815614803,-30.6705677404611,126.943556869095));
#98461=CARTESIAN_POINT('Ctrl Pts',(8.81999450611811,-30.7376495992151,126.919103452224));
#98462=CARTESIAN_POINT('Ctrl Pts',(8.82385085608819,-30.8032991769315,126.891218653366));
#98463=CARTESIAN_POINT('Ctrl Pts',(8.82770577861216,-30.8689244541473,126.863344176198));
#98464=CARTESIAN_POINT('Ctrl Pts',(8.83156070113612,-30.9331180577745,126.832041032617));
#98465=CARTESIAN_POINT('Ctrl Pts',(8.83541562366009,-30.995505806269,126.797488734926));
#98466=CARTESIAN_POINT('Ctrl Pts',(8.83927149076623,-31.0579088418036,126.76292797079));
#98467=CARTESIAN_POINT('Ctrl Pts',(8.84312735787237,-31.1185047131747,126.725116697754));
#98468=CARTESIAN_POINT('Ctrl Pts',(8.8469832249785,-31.1769445536386,126.684279988648));
#98469=CARTESIAN_POINT('Ctrl Pts',(8.84866239473405,-31.2023941892003,126.66649624119));
#98470=CARTESIAN_POINT('Ctrl Pts',(8.85034156448959,-31.227435306327,126.648139290202));
#98471=CARTESIAN_POINT('Ctrl Pts',(8.85202073424513,-31.2520409112987,126.629230222815));
#98472=CARTESIAN_POINT('',(8.54592528048628,-27.9452503479095,125.001195714817));
#98473=CARTESIAN_POINT('Ctrl Pts',(8.54592528053768,-27.94525034791,125.001195715761));
#98474=CARTESIAN_POINT('Ctrl Pts',(8.54975547188148,-27.9452912658805,125.071510240688));
#98475=CARTESIAN_POINT('Ctrl Pts',(8.55358566322528,-27.9489412103475,125.141718266714));
#98476=CARTESIAN_POINT('Ctrl Pts',(8.55741585456908,-27.9561692055137,125.211549630133));
#98477=CARTESIAN_POINT('Ctrl Pts',(8.56128493015481,-27.9634705795499,125.282089924095));
#98478=CARTESIAN_POINT('Ctrl Pts',(8.56515400574055,-27.9744424586778,125.352389946139));
#98479=CARTESIAN_POINT('Ctrl Pts',(8.56902308132629,-27.9890594847817,125.422037684045));
#98480=CARTESIAN_POINT('Ctrl Pts',(8.57288639197494,-28.0036547314622,125.49158164656));
#98481=CARTESIAN_POINT('Ctrl Pts',(8.57674970262359,-28.0218842452092,125.560474782588));
#98482=CARTESIAN_POINT('Ctrl Pts',(8.58061301327225,-28.0436709501691,125.628310600967));
#98483=CARTESIAN_POINT('Ctrl Pts',(8.58447179202976,-28.0654320980398,125.696066843933));
#98484=CARTESIAN_POINT('Ctrl Pts',(8.58833057078728,-28.090742000716,125.762767772626));
#98485=CARTESIAN_POINT('Ctrl Pts',(8.5921893495448,-28.1194730102278,125.828019204631));
#98486=CARTESIAN_POINT('Ctrl Pts',(8.59604569740361,-28.1481859201858,125.893229530466));
#98487=CARTESIAN_POINT('Ctrl Pts',(8.59990204526242,-28.1803154658383,125.95699172771));
#98488=CARTESIAN_POINT('Ctrl Pts',(8.60375839312123,-28.2156853597219,126.018930236566));
#98489=CARTESIAN_POINT('Ctrl Pts',(8.60761360163977,-28.2510448037328,126.080850445975));
#98490=CARTESIAN_POINT('Ctrl Pts',(8.61146881015831,-28.2896424546131,126.140947615044));
#98491=CARTESIAN_POINT('Ctrl Pts',(8.61532401867685,-28.3312562312742,126.198871050964));
#98492=CARTESIAN_POINT('Ctrl Pts',(8.61917937780052,-28.3728716335927,126.256796749683));
#98493=CARTESIAN_POINT('Ctrl Pts',(8.62303473692418,-28.4175031103935,126.31254815342));
#98494=CARTESIAN_POINT('Ctrl Pts',(8.62689009604785,-28.4648864505407,126.365805239691));
#98495=CARTESIAN_POINT('Ctrl Pts',(8.63074949077188,-28.5123193892386,126.41911807286));
#98496=CARTESIAN_POINT('Ctrl Pts',(8.63460888549592,-28.5625096178725,126.469931012886));
#98497=CARTESIAN_POINT('Ctrl Pts',(8.63846828021996,-28.6151545868309,126.517959401343));
#98498=CARTESIAN_POINT('Ctrl Pts',(8.64232986007272,-28.6678293625445,126.566014982719));
#98499=CARTESIAN_POINT('Ctrl Pts',(8.64619143992547,-28.7229612696949,126.611282565647));
#98500=CARTESIAN_POINT('Ctrl Pts',(8.65005301977823,-28.7802151828092,126.653518237653));
#98501=CARTESIAN_POINT('Ctrl Pts',(8.65392135610818,-28.8375692711816,126.695827808003));
#98502=CARTESIAN_POINT('Ctrl Pts',(8.65778969243814,-28.8970523726919,126.735094608463));
#98503=CARTESIAN_POINT('Ctrl Pts',(8.66165802876809,-28.9583015518801,126.771118828787));
#98504=CARTESIAN_POINT('Ctrl Pts',(8.66395572764794,-28.9946820933864,126.792516350519));
#98505=CARTESIAN_POINT('Ctrl Pts',(8.66625342652779,-29.0316852541359,126.812770750007));
#98506=CARTESIAN_POINT('Ctrl Pts',(8.66855112540763,-29.0692316029857,126.831848179741));
#98507=CARTESIAN_POINT('Ctrl Pts',(8.67242019148944,-29.1324554249167,126.863972422373));
#98508=CARTESIAN_POINT('Ctrl Pts',(8.67628925757124,-29.197468129339,126.892882616604));
#98509=CARTESIAN_POINT('Ctrl Pts',(8.68015832365304,-29.2639098155531,126.918376606108));
#98510=CARTESIAN_POINT('Ctrl Pts',(8.68402162477788,-29.3302525028216,126.943832609247));
#98511=CARTESIAN_POINT('Ctrl Pts',(8.68788492590271,-29.3980194956275,126.965882338929));
#98512=CARTESIAN_POINT('Ctrl Pts',(8.69174822702754,-29.4668274817719,126.984370083504));
#98513=CARTESIAN_POINT('Ctrl Pts',(8.69560699627753,-29.5355547521833,127.00283614089));
#98514=CARTESIAN_POINT('Ctrl Pts',(8.69946576552751,-29.6053201234546,127.017748387469));
#98515=CARTESIAN_POINT('Ctrl Pts',(8.7033245347775,-29.6757231958804,127.029000275212));
#98516=CARTESIAN_POINT('Ctrl Pts',(8.70718087314394,-29.7460819169446,127.040245074677));
#98517=CARTESIAN_POINT('Ctrl Pts',(8.71103721151039,-29.8170770635746,127.047834013672));
#98518=CARTESIAN_POINT('Ctrl Pts',(8.71489354987684,-29.888297501336,127.051711508544));
#98519=CARTESIAN_POINT('Ctrl Pts',(8.71874874893201,-29.9594968978298,127.055587857855));
#98520=CARTESIAN_POINT('Ctrl Pts',(8.72260394798719,-30.0309209685101,127.055754913512));
#98521=CARTESIAN_POINT('Ctrl Pts',(8.72645914704236,-30.1021546339133,127.052209052039));
#98522=CARTESIAN_POINT('Ctrl Pts',(8.73031449674551,-30.1733910828842,127.048663052006));
#98523=CARTESIAN_POINT('Ctrl Pts',(8.73416984644866,-30.2444366267281,127.041403873142));
#98524=CARTESIAN_POINT('Ctrl Pts',(8.73802519615181,-30.3148791036184,127.030479921744));
#98525=CARTESIAN_POINT('Ctrl Pts',(8.74188458158523,-30.3853953187836,127.019544535294));
#98526=CARTESIAN_POINT('Ctrl Pts',(8.74574396701865,-30.4553067257793,127.004936792918));
#98527=CARTESIAN_POINT('Ctrl Pts',(8.74960335245206,-30.5242100802503,126.986756490933));
#98528=CARTESIAN_POINT('Ctrl Pts',(8.75346492307344,-30.5931524478707,126.968565895242));
#98529=CARTESIAN_POINT('Ctrl Pts',(8.75732649369481,-30.6610851639198,126.946798861501));
#98530=CARTESIAN_POINT('Ctrl Pts',(8.76118806431618,-30.7276215485713,126.921604653553));
#98531=CARTESIAN_POINT('Ctrl Pts',(8.76505639160837,-30.7942743533256,126.896366362772));
#98532=CARTESIAN_POINT('Ctrl Pts',(8.76892471890055,-30.8595255039085,126.867689120919));
#98533=CARTESIAN_POINT('Ctrl Pts',(8.77279304619274,-30.923010289613,126.835769475661));
#98534=CARTESIAN_POINT('Ctrl Pts',(8.77509082954389,-30.9607202020959,126.816809231631));
#98535=CARTESIAN_POINT('Ctrl Pts',(8.77738861289505,-30.9978073692065,126.796705825255));
#98536=CARTESIAN_POINT('Ctrl Pts',(8.7796863962462,-31.0342002656552,126.775507638119));
#98537=CARTESIAN_POINT('Ctrl Pts',(8.78355540286408,-31.0954786090349,126.73981413974));
#98538=CARTESIAN_POINT('Ctrl Pts',(8.78742440948197,-31.1550269658424,126.700874643153));
#98539=CARTESIAN_POINT('Ctrl Pts',(8.79129341609986,-31.212480317574,126.658881864991));
#98540=CARTESIAN_POINT('Ctrl Pts',(8.79218909434932,-31.2257808162775,126.649160501926));
#98541=CARTESIAN_POINT('Ctrl Pts',(8.79308477259879,-31.2389691310616,126.639275705284));
#98542=CARTESIAN_POINT('Ctrl Pts',(8.79398045084826,-31.2520409112987,126.629230222815));
#98543=CARTESIAN_POINT('Ctrl Pts',(8.09385900495164,-31.2520409112987,126.629230222815));
#98544=CARTESIAN_POINT('Ctrl Pts',(8.09772726999485,-31.3085579851685,126.585797632577));
#98545=CARTESIAN_POINT('Ctrl Pts',(8.10159553503806,-31.3627397236403,126.539476715365));
#98546=CARTESIAN_POINT('Ctrl Pts',(8.10546380008126,-31.4142934443049,126.490560839381));
#98547=CARTESIAN_POINT('Ctrl Pts',(8.10793412379246,-31.4472163120855,126.459322533074));
#98548=CARTESIAN_POINT('Ctrl Pts',(8.11040444750365,-31.4790681575991,126.427026680256));
#98549=CARTESIAN_POINT('Ctrl Pts',(8.11287477121484,-31.5097814179538,126.393756661868));
#98550=CARTESIAN_POINT('Ctrl Pts',(8.11674384460118,-31.5578851776787,126.341648453489));
#98551=CARTESIAN_POINT('Ctrl Pts',(8.12061291798751,-31.6033823190926,126.286944894071));
#98552=CARTESIAN_POINT('Ctrl Pts',(8.12448199137385,-31.6459804494774,126.22993736525));
#98553=CARTESIAN_POINT('Ctrl Pts',(8.12834529980683,-31.6885151082736,126.173014778148));
#98554=CARTESIAN_POINT('Ctrl Pts',(8.13220860823981,-31.728159041816,126.113795421895));
#98555=CARTESIAN_POINT('Ctrl Pts',(8.13607191667279,-31.7646581873541,126.052605835203));
#98556=CARTESIAN_POINT('Ctrl Pts',(8.13993069320136,-31.8011145170929,125.991488027756));
#98557=CARTESIAN_POINT('Ctrl Pts',(8.14378946972994,-31.8344331388476,125.92840499588));
#98558=CARTESIAN_POINT('Ctrl Pts',(8.14764824625851,-31.8644026557222,125.863713088841));
#98559=CARTESIAN_POINT('Ctrl Pts',(8.15150459188142,-31.8943532927606,125.799061935633));
#98560=CARTESIAN_POINT('Ctrl Pts',(8.15536093750432,-31.9209588070679,125.732804357849));
#98561=CARTESIAN_POINT('Ctrl Pts',(8.15921728312723,-31.9440539277217,125.665320891458));
#98562=CARTESIAN_POINT('Ctrl Pts',(8.16307248940625,-31.9671422250025,125.597857362821));
#98563=CARTESIAN_POINT('Ctrl Pts',(8.16692769568528,-31.9867220304168,125.529169123979));
#98564=CARTESIAN_POINT('Ctrl Pts',(8.17078290196431,-32.0026770032989,125.459654634435));
#98565=CARTESIAN_POINT('Ctrl Pts',(8.1746382588482,-32.018632599467,125.390137429286));
#98566=CARTESIAN_POINT('Ctrl Pts',(8.17849361573209,-32.0309629754391,125.31979438332));
#98567=CARTESIAN_POINT('Ctrl Pts',(8.18234897261598,-32.0396026536202,125.249035294377));
#98568=CARTESIAN_POINT('Ctrl Pts',(8.18620836511537,-32.0482513754309,125.178202137978));
#98569=CARTESIAN_POINT('Ctrl Pts',(8.19006775761477,-32.0532016285224,125.106952552449));
#98570=CARTESIAN_POINT('Ctrl Pts',(8.19392715011417,-32.0544398139749,125.035701726213));
#98571=CARTESIAN_POINT('Ctrl Pts',(8.19778872774747,-32.0556787004707,124.96441055876));
#98572=CARTESIAN_POINT('Ctrl Pts',(8.20165030538077,-32.0532013523286,124.893118634925));
#98573=CARTESIAN_POINT('Ctrl Pts',(8.20551188301407,-32.0470462783446,124.822238652077));
#98574=CARTESIAN_POINT('Ctrl Pts',(8.20938021715696,-32.0408804349756,124.751234652226));
#98575=CARTESIAN_POINT('Ctrl Pts',(8.21324855129985,-32.0310240856418,124.68064451366));
#98576=CARTESIAN_POINT('Ctrl Pts',(8.21711688544274,-32.0175672148421,124.610872647974));
#98577=CARTESIAN_POINT('Ctrl Pts',(8.21941460431296,-32.0095740827008,124.569429451375));
#98578=CARTESIAN_POINT('Ctrl Pts',(8.22171232318319,-32.0003116078043,124.528274718171));
#98579=CARTESIAN_POINT('Ctrl Pts',(8.22401004205341,-31.9898069000665,124.487490426482));
#98580=CARTESIAN_POINT('Ctrl Pts',(8.22787911571846,-31.9721182747982,124.418814736446));
#98581=CARTESIAN_POINT('Ctrl Pts',(8.23174818938351,-31.9508354453984,124.350921355088));
#98582=CARTESIAN_POINT('Ctrl Pts',(8.23561726304855,-31.9260446310184,124.284213969244));
#98583=CARTESIAN_POINT('Ctrl Pts',(8.23948057176287,-31.9012907551503,124.217605977939));
#98584=CARTESIAN_POINT('Ctrl Pts',(8.24334388047719,-31.873039437451,124.152180926067));
#98585=CARTESIAN_POINT('Ctrl Pts',(8.2472071891915,-31.8414272228597,124.088329365718));
#98586=CARTESIAN_POINT('Ctrl Pts',(8.25106596600391,-31.8098520913663,124.024552707229));
#98587=CARTESIAN_POINT('Ctrl Pts',(8.25492474281632,-31.774924108694,123.962346307112));
#98588=CARTESIAN_POINT('Ctrl Pts',(8.25878351962873,-31.73682800535,123.90208104018));
#98589=CARTESIAN_POINT('Ctrl Pts',(8.26263986553686,-31.698755901316,123.841853738413));
#98590=CARTESIAN_POINT('Ctrl Pts',(8.26649621144499,-31.6575198952291,123.783565553368));
#98591=CARTESIAN_POINT('Ctrl Pts',(8.27035255735312,-31.6133500549696,123.727561725415));
#98592=CARTESIAN_POINT('Ctrl Pts',(8.27420776391832,-31.5691932645236,123.671574443582));
#98593=CARTESIAN_POINT('Ctrl Pts',(8.27806297048352,-31.5221046613909,123.617870560192));
#98594=CARTESIAN_POINT('Ctrl Pts',(8.28191817704872,-31.4723559098081,123.566763928254));
#98595=CARTESIAN_POINT('Ctrl Pts',(8.28577353421931,-31.4226052147679,123.515655299813));
#98596=CARTESIAN_POINT('Ctrl Pts',(8.2896288913899,-31.3701945053835,123.467144470825));
#98597=CARTESIAN_POINT('Ctrl Pts',(8.29348424856049,-31.3154325580222,123.421508711524));
#98598=CARTESIAN_POINT('Ctrl Pts',(8.29734364134539,-31.26061328832,123.375825182765));
#98599=CARTESIAN_POINT('Ctrl Pts',(8.30120303413028,-31.2034382415455,123.333023042951));
#98600=CARTESIAN_POINT('Ctrl Pts',(8.30506242691517,-31.1442488600592,123.293338900439));
#98601=CARTESIAN_POINT('Ctrl Pts',(8.30892400483373,-31.0850259663815,123.253632289327));
#98602=CARTESIAN_POINT('Ctrl Pts',(8.31278558275228,-31.0237868848638,123.217047439076));
#98603=CARTESIAN_POINT('Ctrl Pts',(8.31664716067083,-30.9608992263762,123.183775829021));
#98604=CARTESIAN_POINT('Ctrl Pts',(8.32051549509547,-30.897901534929,123.150446004464));
#98605=CARTESIAN_POINT('Ctrl Pts',(8.3243838295201,-30.8332499483595,123.120441198736));
#98606=CARTESIAN_POINT('Ctrl Pts',(8.32825216394474,-30.7673330348737,123.09390515029));
#98607=CARTESIAN_POINT('Ctrl Pts',(8.33054988026048,-30.7281796548982,123.07814324742));
#98608=CARTESIAN_POINT('Ctrl Pts',(8.33284759657622,-30.6885801806942,123.063604224167));
#98609=CARTESIAN_POINT('Ctrl Pts',(8.33514531289196,-30.6486181888067,123.050309766232));
#98610=CARTESIAN_POINT('Ctrl Pts',(8.33901438538775,-30.5813270951981,123.027923529433));
#98611=CARTESIAN_POINT('Ctrl Pts',(8.34288345788354,-30.5127438862126,123.008981234));
#98612=CARTESIAN_POINT('Ctrl Pts',(8.34675253037932,-30.4432544786734,122.993629388763));
#98613=CARTESIAN_POINT('Ctrl Pts',(8.35061583792275,-30.3738686109683,122.978300417911));
#98614=CARTESIAN_POINT('Ctrl Pts',(8.35447914546617,-30.3035796953893,122.966551381988));
#98615=CARTESIAN_POINT('Ctrl Pts',(8.3583424530096,-30.2327899086053,122.958479385127));
#98616=CARTESIAN_POINT('Ctrl Pts',(8.36220122865432,-30.1620831626198,122.950416857217));
#98617=CARTESIAN_POINT('Ctrl Pts',(8.36606000429903,-30.0908771928238,122.946022855279));
#98618=CARTESIAN_POINT('Ctrl Pts',(8.36991877994375,-30.0195837782864,122.945343328405));
#98619=CARTESIAN_POINT('Ctrl Pts',(8.37377512468678,-29.9483352762543,122.944664229612));
#98620=CARTESIAN_POINT('Ctrl Pts',(8.37763146942982,-29.8769999233888,122.947694967986));
#98621=CARTESIAN_POINT('Ctrl Pts',(8.38148781417285,-29.8059925515189,122.95442949952));
#98622=CARTESIAN_POINT('Ctrl Pts',(8.38534301957725,-29.7350061584378,122.961162041369));
#98623=CARTESIAN_POINT('Ctrl Pts',(8.38919822498165,-29.6643480373307,122.971596158109));
#98624=CARTESIAN_POINT('Ctrl Pts',(8.39305343038605,-29.5944292105134,122.985673835444));
#98625=CARTESIAN_POINT('Ctrl Pts',(8.39690878640181,-29.5245076521763,122.999752062752));
#98626=CARTESIAN_POINT('Ctrl Pts',(8.40076414241759,-29.4553259212649,123.017474035213));
#98627=CARTESIAN_POINT('Ctrl Pts',(8.40461949843336,-29.3872844335983,123.038730717829));
#98628=CARTESIAN_POINT('Ctrl Pts',(8.40847889008046,-29.3191717228442,123.060009651083));
#98629=CARTESIAN_POINT('Ctrl Pts',(8.41233828172756,-29.2522021025857,123.084830535351));
#98630=CARTESIAN_POINT('Ctrl Pts',(8.41619767337466,-29.1867595436897,123.113034837969));
#98631=CARTESIAN_POINT('Ctrl Pts',(8.4200592501633,-29.1212799319971,123.141255109526));
#98632=CARTESIAN_POINT('Ctrl Pts',(8.42392082695194,-29.0573295385309,123.172862397558));
#98633=CARTESIAN_POINT('Ctrl Pts',(8.42778240374059,-28.9952686121545,123.207651707737));
#98634=CARTESIAN_POINT('Ctrl Pts',(8.43165073706,-28.9330990989024,123.242501888141));
#98635=CARTESIAN_POINT('Ctrl Pts',(8.43551907037942,-28.8728260641291,123.280544947049));
#98636=CARTESIAN_POINT('Ctrl Pts',(8.43938740369884,-28.8147810140006,123.321532390028));
#98637=CARTESIAN_POINT('Ctrl Pts',(8.44168513037607,-28.78030320427,123.3458782603));
#98638=CARTESIAN_POINT('Ctrl Pts',(8.44398285705329,-28.7466108504686,123.371262169159));
#98639=CARTESIAN_POINT('Ctrl Pts',(8.44628058373051,-28.7137675014706,123.397625661018));
#98640=CARTESIAN_POINT('Ctrl Pts',(8.45010049336493,-28.6591663052068,123.441454266722));
#98641=CARTESIAN_POINT('Ctrl Pts',(8.45392040299934,-28.6066877443327,123.488173581393));
#98642=CARTESIAN_POINT('Ctrl Pts',(8.45774031263375,-28.5566598146521,123.537547719801));
#98643=CARTESIAN_POINT('Ctrl Pts',(8.46155371406763,-28.5067171204429,123.586837736639));
#98644=CARTESIAN_POINT('Ctrl Pts',(8.46536711550151,-28.4592171196553,123.638773249035));
#98645=CARTESIAN_POINT('Ctrl Pts',(8.46918051693538,-28.4144553825126,123.693077726697));
#98646=CARTESIAN_POINT('Ctrl Pts',(8.47299028819365,-28.3697362564007,123.747330509095));
#98647=CARTESIAN_POINT('Ctrl Pts',(8.47680005945192,-28.3277505435078,123.803947404073));
#98648=CARTESIAN_POINT('Ctrl Pts',(8.48060983071019,-28.2887564983585,123.862615614407));
#98649=CARTESIAN_POINT('Ctrl Pts',(8.48441732747402,-28.2497857332784,123.921248798881));
#98650=CARTESIAN_POINT('Ctrl Pts',(8.48822482423785,-28.2138033700979,123.981930455338));
#98651=CARTESIAN_POINT('Ctrl Pts',(8.49203232100168,-28.1810257548658,124.044316863161));
#98652=CARTESIAN_POINT('Ctrl Pts',(8.49583889576681,-28.1482560768483,124.106688163896));
#98653=CARTESIAN_POINT('Ctrl Pts',(8.49964547053193,-28.1186898378894,124.170762954398));
#98654=CARTESIAN_POINT('Ctrl Pts',(8.50345204529706,-28.0924976678887,124.236172522431));
#98655=CARTESIAN_POINT('Ctrl Pts',(8.50726133136703,-28.0662868420197,124.301628679665));
#98656=CARTESIAN_POINT('Ctrl Pts',(8.511070617437,-28.0434550737678,124.368421049895));
#98657=CARTESIAN_POINT('Ctrl Pts',(8.51487990350697,-28.0241245342633,124.436161630962));
#98658=CARTESIAN_POINT('Ctrl Pts',(8.51869054788737,-28.0047871018994,124.503926366879));
#98659=CARTESIAN_POINT('Ctrl Pts',(8.52250119226777,-27.9889534984263,124.572639500133));
#98660=CARTESIAN_POINT('Ctrl Pts',(8.52631183664817,-27.9766950596919,124.641901297091));
#98661=CARTESIAN_POINT('Ctrl Pts',(8.53012846308285,-27.9644173773235,124.711271823122));
#98662=CARTESIAN_POINT('Ctrl Pts',(8.53394508951753,-27.955726129257,124.781192236676));
#98663=CARTESIAN_POINT('Ctrl Pts',(8.53776171595221,-27.9506408107848,124.851257013345));
#98664=CARTESIAN_POINT('Ctrl Pts',(8.54048290413023,-27.9470150672793,124.901211978871));
#98665=CARTESIAN_POINT('Ctrl Pts',(8.54320409230826,-27.9452212774533,124.951240233013));
#98666=CARTESIAN_POINT('Ctrl Pts',(8.54592528048628,-27.9452503479095,125.001195714817));
#98667=CARTESIAN_POINT('Origin',(-1.54592528053767,-30.,125.));
#98668=CARTESIAN_POINT('',(7.39391264968254,-31.2520409112987,126.629230222815));
#98669=CARTESIAN_POINT('',(7.45211278928543,-31.2520409112987,126.629230222815));
#98670=CARTESIAN_POINT('',(-1.54592528053767,-31.2520409112987,126.629230222815));
#98671=CARTESIAN_POINT('',(7.90407471950836,-27.9452505543669,124.998490639097));
#98672=CARTESIAN_POINT('Ctrl Pts',(7.45211278928543,-31.2520409112987,126.629230222815));
#98673=CARTESIAN_POINT('Ctrl Pts',(7.45597763034358,-31.3083540803805,126.585954330588));
#98674=CARTESIAN_POINT('Ctrl Pts',(7.45984247140173,-31.3625145223919,126.539683438356));
#98675=CARTESIAN_POINT('Ctrl Pts',(7.46370731245988,-31.4141879602304,126.490660919069));
#98676=CARTESIAN_POINT('Ctrl Pts',(7.46756704170375,-31.4657930524336,126.441703239192));
#98677=CARTESIAN_POINT('Ctrl Pts',(7.47142677094762,-31.5149173244941,126.390001494346));
#98678=CARTESIAN_POINT('Ctrl Pts',(7.47528650019149,-31.5612592226217,126.335839512172));
#98679=CARTESIAN_POINT('Ctrl Pts',(7.47914342130644,-31.6075674049065,126.281716935308));
#98680=CARTESIAN_POINT('Ctrl Pts',(7.48300034242139,-31.6510969141813,126.225138039894));
#98681=CARTESIAN_POINT('Ctrl Pts',(7.48685726353634,-31.691583760069,126.166422712901));
#98682=CARTESIAN_POINT('Ctrl Pts',(7.49071266880043,-31.7320546937773,126.107730462262));
#98683=CARTESIAN_POINT('Ctrl Pts',(7.49456807406451,-31.7694850619962,126.046903846099));
#98684=CARTESIAN_POINT('Ctrl Pts',(7.4984234793286,-31.8036528795101,125.984293580562));
#98685=CARTESIAN_POINT('Ctrl Pts',(7.50227865902707,-31.8378186979904,125.921686978121));
#98686=CARTESIAN_POINT('Ctrl Pts',(7.50613383872555,-31.8687221134478,125.857297360676));
#98687=CARTESIAN_POINT('Ctrl Pts',(7.50998901842402,-31.8961868410849,125.791500490332));
#98688=CARTESIAN_POINT('Ctrl Pts',(7.51384799214005,-31.9236785977238,125.725638866981));
#98689=CARTESIAN_POINT('Ctrl Pts',(7.51770696585608,-31.9477247189694,125.658367673651));
#98690=CARTESIAN_POINT('Ctrl Pts',(7.52156593957212,-31.9681972468078,125.590082333372));
#98691=CARTESIAN_POINT('Ctrl Pts',(7.52542676053524,-31.9886795746138,125.521764305673));
#98692=CARTESIAN_POINT('Ctrl Pts',(7.52928758149837,-32.0055847858469,125.452431636587));
#98693=CARTESIAN_POINT('Ctrl Pts',(7.5331484024615,-32.0188356861061,125.382491875737));
#98694=CARTESIAN_POINT('Ctrl Pts',(7.53701633778309,-32.0321110038805,125.31242323646));
#98695=CARTESIAN_POINT('Ctrl Pts',(7.54088427310468,-32.041718490898,125.241745752882));
#98696=CARTESIAN_POINT('Ctrl Pts',(7.54475220842627,-32.0476327261154,125.170873583216));
#98697=CARTESIAN_POINT('Ctrl Pts',(7.54817615280141,-32.0528680805674,125.108136658603));
#98698=CARTESIAN_POINT('Ctrl Pts',(7.55160009717655,-32.0552101662244,125.04524745785));
#98699=CARTESIAN_POINT('Ctrl Pts',(7.55502404155169,-32.054675403714,124.982491491417));
#98700=CARTESIAN_POINT('Ctrl Pts',(7.55889311490067,-32.0540711195463,124.911576952333));
#98701=CARTESIAN_POINT('Ctrl Pts',(7.56276218824965,-32.0497900525759,124.840554831224));
#98702=CARTESIAN_POINT('Ctrl Pts',(7.56663126159862,-32.0418185215167,124.769837692722));
#98703=CARTESIAN_POINT('Ctrl Pts',(7.57049456999505,-32.0338588681072,124.699225923365));
#98704=CARTESIAN_POINT('Ctrl Pts',(7.57435787839148,-32.0222197195905,124.628918713387));
#98705=CARTESIAN_POINT('Ctrl Pts',(7.57822118678791,-32.0069394027001,124.55932801724));
#98706=CARTESIAN_POINT('Ctrl Pts',(7.5820799632813,-31.9916770105799,124.489818955344));
#98707=CARTESIAN_POINT('Ctrl Pts',(7.58593873977468,-31.9727820380486,124.421025209909));
#98708=CARTESIAN_POINT('Ctrl Pts',(7.58979751626806,-31.9503443206474,124.353351259633));
#98709=CARTESIAN_POINT('Ctrl Pts',(7.59365386185663,-31.927920738285,124.285719941764));
#98710=CARTESIAN_POINT('Ctrl Pts',(7.59751020744519,-31.9019589914577,124.219207479496));
#98711=CARTESIAN_POINT('Ctrl Pts',(7.60136655303376,-31.8725990970537,124.154204407547));
#98712=CARTESIAN_POINT('Ctrl Pts',(7.60522175927935,-31.8432478769215,124.089220540514));
#98713=CARTESIAN_POINT('Ctrl Pts',(7.60907696552493,-31.810500702226,124.025745620959));
#98714=CARTESIAN_POINT('Ctrl Pts',(7.61293217177052,-31.7745455280139,123.964149754305));
#98715=CARTESIAN_POINT('Ctrl Pts',(7.61678752862191,-31.7385889491926,123.902551481374));
#98716=CARTESIAN_POINT('Ctrl Pts',(7.6206428854733,-31.6994243688427,123.842832825512));
#98717=CARTESIAN_POINT('Ctrl Pts',(7.62449824232469,-31.657284581258,123.785337339331));
#98718=CARTESIAN_POINT('Ctrl Pts',(7.62835763479323,-31.6151006836062,123.727781669415));
#98719=CARTESIAN_POINT('Ctrl Pts',(7.63221702726178,-31.5699356496064,123.672454207247));
#98720=CARTESIAN_POINT('Ctrl Pts',(7.63607641973032,-31.5220637816352,123.619666921669));
#98721=CARTESIAN_POINT('Ctrl Pts',(7.63993799733364,-31.4741648092726,123.566849748658));
#98722=CARTESIAN_POINT('Ctrl Pts',(7.64379957493697,-31.4235562968641,123.5165759578));
#98723=CARTESIAN_POINT('Ctrl Pts',(7.64766115254029,-31.3705488264876,123.469120031905));
#98724=CARTESIAN_POINT('Ctrl Pts',(7.65152948665491,-31.3174486101899,123.421581073496));
#98725=CARTESIAN_POINT('Ctrl Pts',(7.65539782076953,-31.2619414341314,123.376870128472));
#98726=CARTESIAN_POINT('Ctrl Pts',(7.65926615488415,-31.2043697326239,123.335220402083));
#98727=CARTESIAN_POINT('Ctrl Pts',(7.66156387405285,-31.1701732030044,123.310481232234));
#98728=CARTESIAN_POINT('Ctrl Pts',(7.66386159322155,-31.135248827303,123.286821267237));
#98729=CARTESIAN_POINT('Ctrl Pts',(7.66615931239025,-31.0996724856495,123.264281708685));
#98730=CARTESIAN_POINT('Ctrl Pts',(7.67002838578164,-31.0397663497171,123.226327894557));
#98731=CARTESIAN_POINT('Ctrl Pts',(7.67389745917303,-30.977775674469,123.191404757273));
#98732=CARTESIAN_POINT('Ctrl Pts',(7.67776653256441,-30.9140396531967,123.159747551317));
#98733=CARTESIAN_POINT('Ctrl Pts',(7.68162984100355,-30.850398599138,123.128137514866));
#98734=CARTESIAN_POINT('Ctrl Pts',(7.68549314944269,-30.7850177926637,123.099783964681));
#98735=CARTESIAN_POINT('Ctrl Pts',(7.68935645788183,-30.7182641217052,123.074878130099));
#98736=CARTESIAN_POINT('Ctrl Pts',(7.69321523441816,-30.6515887569844,123.050001511621));
#98737=CARTESIAN_POINT('Ctrl Pts',(7.69707401095449,-30.5835441796199,123.028564744217));
#98738=CARTESIAN_POINT('Ctrl Pts',(7.70093278749081,-30.514518933364,123.010711727851));
#98739=CARTESIAN_POINT('Ctrl Pts',(7.70478913312245,-30.4455371707857,122.992869958309));
#98740=CARTESIAN_POINT('Ctrl Pts',(7.70864547875409,-30.3755764341985,122.978607582026));
#98741=CARTESIAN_POINT('Ctrl Pts',(7.71250182438572,-30.3050407689715,122.968018776719));
#98742=CARTESIAN_POINT('Ctrl Pts',(7.71635703067443,-30.2345259432436,122.957433099835));
#98743=CARTESIAN_POINT('Ctrl Pts',(7.72021223696314,-30.1634370062372,122.9505189113));
#98744=CARTESIAN_POINT('Ctrl Pts',(7.72406744325185,-30.0921868397139,122.94731903378));
#98745=CARTESIAN_POINT('Ctrl Pts',(7.72792280014636,-30.0209338897628,122.944119031254));
#98746=CARTESIAN_POINT('Ctrl Pts',(7.73177815704087,-29.9495201831855,122.944633647418));
#98747=CARTESIAN_POINT('Ctrl Pts',(7.73563351393538,-29.878360612768,122.94885363224));
#98748=CARTESIAN_POINT('Ctrl Pts',(7.73949290644673,-29.8071265556639,122.953078034356));
#98749=CARTESIAN_POINT('Ctrl Pts',(7.74335229895808,-29.73614765168,122.961015518903));
#98750=CARTESIAN_POINT('Ctrl Pts',(7.74721169146943,-29.6658347711962,122.972604833201));
#98751=CARTESIAN_POINT('Ctrl Pts',(7.75107326911546,-29.5954820805316,122.984200709209));
#98752=CARTESIAN_POINT('Ctrl Pts',(7.75493484676149,-29.5257966388214,122.999452427041));
#98753=CARTESIAN_POINT('Ctrl Pts',(7.75879642440752,-29.4571774996037,123.018247922781));
#98754=CARTESIAN_POINT('Ctrl Pts',(7.7626647585642,-29.3884382991085,123.037076304553));
#98755=CARTESIAN_POINT('Ctrl Pts',(7.76653309272088,-29.3207695873519,123.059460691027));
#98756=CARTESIAN_POINT('Ctrl Pts',(7.77040142687756,-29.2545530143012,123.085239870372));
#98757=CARTESIAN_POINT('Ctrl Pts',(7.77269914566131,-29.2152215973316,123.100552225048));
#98758=CARTESIAN_POINT('Ctrl Pts',(7.77499686444506,-29.1764021096255,123.11706139647));
#98759=CARTESIAN_POINT('Ctrl Pts',(7.77729458322881,-29.1381703210552,123.134725980723));
#98760=CARTESIAN_POINT('Ctrl Pts',(7.78116365647907,-29.0737927342447,123.164470948164));
#98761=CARTESIAN_POINT('Ctrl Pts',(7.78503272972934,-29.0108307716454,123.197610957943));
#98762=CARTESIAN_POINT('Ctrl Pts',(7.7889018029796,-28.949666047039,123.233988632608));
#98763=CARTESIAN_POINT('Ctrl Pts',(7.79276511127752,-28.8885924583971,123.270312104226));
#98764=CARTESIAN_POINT('Ctrl Pts',(7.79662841957544,-28.8293112063121,123.309863418632));
#98765=CARTESIAN_POINT('Ctrl Pts',(7.80049172787336,-28.7721819377034,123.352438053244));
#98766=CARTESIAN_POINT('Ctrl Pts',(7.80435050426899,-28.7151196853003,123.394962745146));
#98767=CARTESIAN_POINT('Ctrl Pts',(7.80820928066463,-28.6602047896665,123.440503423746));
#98768=CARTESIAN_POINT('Ctrl Pts',(7.81206805706026,-28.6077688795949,123.488811702707));
#98769=CARTESIAN_POINT('Ctrl Pts',(7.8159244025516,-28.5553660024503,123.537089549015));
#98770=CARTESIAN_POINT('Ctrl Pts',(7.81978074804294,-28.5054393689506,123.588131208238));
#98771=CARTESIAN_POINT('Ctrl Pts',(7.82363709353428,-28.4582872415828,123.641648302893));
#98772=CARTESIAN_POINT('Ctrl Pts',(7.8274922996833,-28.4111490451282,123.69514958613));
#98773=CARTESIAN_POINT('Ctrl Pts',(7.83134750583233,-28.3667840484081,123.751124488558));
#98774=CARTESIAN_POINT('Ctrl Pts',(7.83520271198135,-28.3254521608355,123.809249355722));
#98775=CARTESIAN_POINT('Ctrl Pts',(7.83905806873697,-28.2841186586008,123.867376493578));
#98776=CARTESIAN_POINT('Ctrl Pts',(7.8429134254926,-28.2458187804849,123.927653365745));
#98777=CARTESIAN_POINT('Ctrl Pts',(7.84676878224822,-28.2107697780686,123.98972638586));
#98778=CARTESIAN_POINT('Ctrl Pts',(7.85062817462287,-28.1756840878878,124.0518643813));
#98779=CARTESIAN_POINT('Ctrl Pts',(7.85448756699751,-28.1438563056484,124.115801853969));
#98780=CARTESIAN_POINT('Ctrl Pts',(7.85834695937215,-28.1154578116314,124.181160392532));
#98781=CARTESIAN_POINT('Ctrl Pts',(7.86220853688249,-28.0870432387717,124.246555936213));
#98782=CARTESIAN_POINT('Ctrl Pts',(7.86607011439284,-28.0620619894954,124.313373692235));
#98783=CARTESIAN_POINT('Ctrl Pts',(7.86993169190318,-28.0406363463201,124.381217618918));
#98784=CARTESIAN_POINT('Ctrl Pts',(7.87380002592726,-28.0191732151876,124.449180250565));
#98785=CARTESIAN_POINT('Ctrl Pts',(7.87766835995134,-28.0012782328927,124.518172167199));
#98786=CARTESIAN_POINT('Ctrl Pts',(7.88153669397541,-27.9870229515759,124.587785292575));
#98787=CARTESIAN_POINT('Ctrl Pts',(7.88383441400607,-27.9785555738312,124.629134222522));
#98788=CARTESIAN_POINT('Ctrl Pts',(7.88613213403672,-27.9713713474013,124.670702169065));
#98789=CARTESIAN_POINT('Ctrl Pts',(7.88842985406737,-27.9654765819169,124.712403018494));
#98790=CARTESIAN_POINT('Ctrl Pts',(7.89364480919903,-27.9520976945405,124.807048169262));
#98791=CARTESIAN_POINT('Ctrl Pts',(7.89885976433068,-27.9453209576648,124.90264805037));
#98792=CARTESIAN_POINT('Ctrl Pts',(7.90407471946233,-27.9452505543675,124.998490638251));
#98793=CARTESIAN_POINT('Ctrl Pts',(7.90407471950836,-27.9452505543669,124.998490639097));
#98794=CARTESIAN_POINT('Ctrl Pts',(7.90805348639992,-27.9451968399735,125.071614051636));
#98795=CARTESIAN_POINT('Ctrl Pts',(7.91203225329149,-27.9490515818561,125.144885851501));
#98796=CARTESIAN_POINT('Ctrl Pts',(7.91601102018306,-27.9568307713783,125.2178464269));
#98797=CARTESIAN_POINT('Ctrl Pts',(7.91981486837864,-27.9642679640647,125.287599433458));
#98798=CARTESIAN_POINT('Ctrl Pts',(7.92361871657422,-27.9752917464163,125.357067439177));
#98799=CARTESIAN_POINT('Ctrl Pts',(7.9274225647698,-27.9898629599105,125.425848144953));
#98800=CARTESIAN_POINT('Ctrl Pts',(7.93122379847079,-28.0044241581893,125.494581575767));
#98801=CARTESIAN_POINT('Ctrl Pts',(7.93502503217179,-28.0225278513569,125.562628154102));
#98802=CARTESIAN_POINT('Ctrl Pts',(7.93882626587279,-28.0440833861041,125.62959333064));
#98803=CARTESIAN_POINT('Ctrl Pts',(7.94262624496941,-28.0656318064063,125.696536405195));
#98804=CARTESIAN_POINT('Ctrl Pts',(7.94642622406603,-28.0906296548367,125.762398309196));
#98805=CARTESIAN_POINT('Ctrl Pts',(7.95022620316264,-28.1189362808575,125.826799157611));
#98806=CARTESIAN_POINT('Ctrl Pts',(7.95402628561092,-28.1472436767607,125.891201757597));
#98807=CARTESIAN_POINT('Ctrl Pts',(7.95782636805919,-28.1788598241947,125.954142765628));
#98808=CARTESIAN_POINT('Ctrl Pts',(7.96162645050747,-28.2135965224734,126.015263600244));
#98809=CARTESIAN_POINT('Ctrl Pts',(7.96543037575041,-28.2483683478844,126.076446242682));
#98810=CARTESIAN_POINT('Ctrl Pts',(7.96923430099335,-28.2862667704271,126.135804603882));
#98811=CARTESIAN_POINT('Ctrl Pts',(7.97303822623629,-28.3270589369239,126.193007025115));
#98812=CARTESIAN_POINT('Ctrl Pts',(7.97684442188905,-28.3678754506224,126.25024358817));
#98813=CARTESIAN_POINT('Ctrl Pts',(7.98065061754181,-28.4115888297688,126.305321261542));
#98814=CARTESIAN_POINT('Ctrl Pts',(7.98445681319456,-28.4579262240686,126.357941836783));
#98815=CARTESIAN_POINT('Ctrl Pts',(7.98826926353405,-28.5043397641874,126.410648882936));
#98816=CARTESIAN_POINT('Ctrl Pts',(7.99208171387354,-28.5533855677727,126.460890422937));
#98817=CARTESIAN_POINT('Ctrl Pts',(7.99589416421303,-28.6047551208587,126.508406208463));
#98818=CARTESIAN_POINT('Ctrl Pts',(7.99711781777733,-28.6212428206668,126.523656993429));
#98819=CARTESIAN_POINT('Ctrl Pts',(7.99834147134164,-28.6379696664498,126.538627302508));
#98820=CARTESIAN_POINT('Ctrl Pts',(7.99956512490594,-28.6549248138619,126.553309468887));
#98821=CARTESIAN_POINT('Ctrl Pts',(8.00343419857207,-28.7085353424225,126.599733052292));
#98822=CARTESIAN_POINT('Ctrl Pts',(8.00730327223819,-28.7646570788596,126.643468858693));
#98823=CARTESIAN_POINT('Ctrl Pts',(8.01117234590431,-28.8229894970222,126.684233902515));
#98824=CARTESIAN_POINT('Ctrl Pts',(8.01503565461971,-28.8812349994148,126.724938206094));
#98825=CARTESIAN_POINT('Ctrl Pts',(8.0188989633351,-28.9416842502233,126.762680257491));
#98826=CARTESIAN_POINT('Ctrl Pts',(8.0227622720505,-29.0040028020232,126.797216498957));
#98827=CARTESIAN_POINT('Ctrl Pts',(8.02662104886399,-29.0662482502779,126.831712227259));
#98828=CARTESIAN_POINT('Ctrl Pts',(8.03047982567748,-29.130358221031,126.863009381153));
#98829=CARTESIAN_POINT('Ctrl Pts',(8.03433860249097,-29.1959698271948,126.890907994514));
#98830=CARTESIAN_POINT('Ctrl Pts',(8.03819494840018,-29.2615401001739,126.918789032655));
#98831=CARTESIAN_POINT('Ctrl Pts',(8.04205129430939,-29.3286096857582,126.943275588273));
#98832=CARTESIAN_POINT('Ctrl Pts',(8.04590764021859,-29.3967929881579,126.964214566529));
#98833=CARTESIAN_POINT('Ctrl Pts',(8.04976284678488,-29.4649561460568,126.985147358442));
#98834=CARTESIAN_POINT('Ctrl Pts',(8.05361805335116,-29.5342319034004,127.002534511264));
#98835=CARTESIAN_POINT('Ctrl Pts',(8.05747325991744,-29.6042183048147,127.016272405271));
#98836=CARTESIAN_POINT('Ctrl Pts',(8.0613286170891,-29.6742074402792,127.030010835954));
#98837=CARTESIAN_POINT('Ctrl Pts',(8.06518397426077,-29.744906797818,127.040099633378));
#98838=CARTESIAN_POINT('Ctrl Pts',(8.06903933143243,-29.8159047057685,127.046486375508));
#98839=CARTESIAN_POINT('Ctrl Pts',(8.07289872421839,-29.8869769311322,127.052879802993));
#98840=CARTESIAN_POINT('Ctrl Pts',(8.07675811700435,-29.9583478459224,127.055563395911));
#98841=CARTESIAN_POINT('Ctrl Pts',(8.08061750979031,-30.0296020392076,127.054536756005));
#98842=CARTESIAN_POINT('Ctrl Pts',(8.08447908770992,-30.10089657561,127.053509534829));
#98843=CARTESIAN_POINT('Ctrl Pts',(8.08834066562953,-30.1720737740093,127.048767931325));
#98844=CARTESIAN_POINT('Ctrl Pts',(8.09220224354914,-30.2427223691411,127.040363549473));
#98845=CARTESIAN_POINT('Ctrl Pts',(8.09607057797482,-30.3134945763485,127.031944462685));
#98846=CARTESIAN_POINT('Ctrl Pts',(8.09993891240049,-30.3837358548381,127.019849884909));
#98847=CARTESIAN_POINT('Ctrl Pts',(8.10380724682617,-30.4530448567175,127.004182606526));
#98848=CARTESIAN_POINT('Ctrl Pts',(8.10610496313228,-30.4942130718339,126.994876544265));
#98849=CARTESIAN_POINT('Ctrl Pts',(8.10840267943838,-30.5350526329831,126.984310949884));
#98850=CARTESIAN_POINT('Ctrl Pts',(8.11070039574449,-30.5754824652189,126.972515524584));
#98851=CARTESIAN_POINT('Ctrl Pts',(8.11456845452976,-30.6435435079816,126.952658678751));
#98852=CARTESIAN_POINT('Ctrl Pts',(8.11843651331503,-30.7107088921738,126.929236177448));
#98853=CARTESIAN_POINT('Ctrl Pts',(8.1223045721003,-30.776578188445,126.902346939896));
#98854=CARTESIAN_POINT('Ctrl Pts',(8.12616759078078,-30.8423616566109,126.875492739189));
#98855=CARTESIAN_POINT('Ctrl Pts',(8.13003060946125,-30.9068519399335,126.845180941199));
#98856=CARTESIAN_POINT('Ctrl Pts',(8.13389362814173,-30.96966310444,126.811560384417));
#98857=CARTESIAN_POINT('Ctrl Pts',(8.13775232965764,-31.0324040735486,126.777977400706));
#98858=CARTESIAN_POINT('Ctrl Pts',(8.14161103117355,-31.0934692238645,126.741093228731));
#98859=CARTESIAN_POINT('Ctrl Pts',(8.14546973268947,-31.1524937513155,126.701104263612));
#98860=CARTESIAN_POINT('Ctrl Pts',(8.14768435229106,-31.1863696224936,126.678153448257));
#98861=CARTESIAN_POINT('Ctrl Pts',(8.14989897189265,-31.2195737270747,126.654180805215));
#98862=CARTESIAN_POINT('Ctrl Pts',(8.15211359149425,-31.2520409112987,126.629230222815));
#98863=CARTESIAN_POINT('',(7.8459252805834,-27.9452502651294,125.001043814792));
#98864=CARTESIAN_POINT('Ctrl Pts',(7.8459252805834,-27.9452502651294,125.001043814792));
#98865=CARTESIAN_POINT('Ctrl Pts',(7.85018308156602,-27.9452903410169,125.079933211422));
#98866=CARTESIAN_POINT('Ctrl Pts',(7.85444088254865,-27.9498778523941,125.158666320287));
#98867=CARTESIAN_POINT('Ctrl Pts',(7.85869868353127,-27.9589342277071,125.236744747935));
#98868=CARTESIAN_POINT('Ctrl Pts',(7.86297170281527,-27.9680229724638,125.315102244765));
#98869=CARTESIAN_POINT('Ctrl Pts',(7.86724472209928,-27.9816124479092,125.392800086569));
#98870=CARTESIAN_POINT('Ctrl Pts',(7.87151774138328,-27.999573279132,125.4693511446));
#98871=CARTESIAN_POINT('Ctrl Pts',(7.87581130795489,-28.0176204770056,125.546270306891));
#98872=CARTESIAN_POINT('Ctrl Pts',(7.88010487452649,-28.0400810303069,125.622031352994));
#98873=CARTESIAN_POINT('Ctrl Pts',(7.8843984410981,-28.0667754170322,125.696161097957));
#98874=CARTESIAN_POINT('Ctrl Pts',(7.88646703724464,-28.0796364975799,125.731876045476));
#98875=CARTESIAN_POINT('Ctrl Pts',(7.88853563339119,-28.0934796393112,125.767212670557));
#98876=CARTESIAN_POINT('Ctrl Pts',(7.89060422953773,-28.1082809505831,125.802120066183));
#98877=CARTESIAN_POINT('Ctrl Pts',(7.89447330292895,-28.1359651168198,125.867410372267));
#98878=CARTESIAN_POINT('Ctrl Pts',(7.89834237632017,-28.1670875964325,125.931393656004));
#98879=CARTESIAN_POINT('Ctrl Pts',(7.90221144971139,-28.2015032182845,125.993683495213));
#98880=CARTESIAN_POINT('Ctrl Pts',(7.90607475815036,-28.2358675605674,126.055880522032));
#98881=CARTESIAN_POINT('Ctrl Pts',(7.90993806658933,-28.2735150721962,126.116388691159));
#98882=CARTESIAN_POINT('Ctrl Pts',(7.91380137502831,-28.3142527626546,126.174842038013));
#98883=CARTESIAN_POINT('Ctrl Pts',(7.91766015156447,-28.35494266525,126.233226815429));
#98884=CARTESIAN_POINT('Ctrl Pts',(7.92151892810063,-28.3987152698427,126.289561161899));
#98885=CARTESIAN_POINT('Ctrl Pts',(7.92537770463679,-28.4453328539635,126.343505722926));
#98886=CARTESIAN_POINT('Ctrl Pts',(7.92923405026826,-28.4919210705108,126.39741630062));
#98887=CARTESIAN_POINT('Ctrl Pts',(7.93309039589973,-28.5413503939185,126.448939713047));
#98888=CARTESIAN_POINT('Ctrl Pts',(7.93694674153119,-28.5933420704611,126.497768684332));
#98889=CARTESIAN_POINT('Ctrl Pts',(7.94080194781973,-28.6453183862568,126.546583229279));
#98890=CARTESIAN_POINT('Ctrl Pts',(7.94465715410827,-28.699855198347,126.592704581107));
#98891=CARTESIAN_POINT('Ctrl Pts',(7.94851236039682,-28.756637275071,126.63586267662));
#98892=CARTESIAN_POINT('Ctrl Pts',(7.95236771729116,-28.8134215700188,126.679022458127));
#98893=CARTESIAN_POINT('Ctrl Pts',(7.95622307418551,-28.872450915657,126.719218461287));
#98894=CARTESIAN_POINT('Ctrl Pts',(7.96007843107985,-28.9333788079595,126.756222308021));
#98895=CARTESIAN_POINT('Ctrl Pts',(7.96393782359104,-28.9943704768811,126.793264888742));
#98896=CARTESIAN_POINT('Ctrl Pts',(7.96779721610223,-29.0572642435349,126.827108390148));
#98897=CARTESIAN_POINT('Ctrl Pts',(7.97165660861341,-29.1216873337711,126.857569493409));
#98898=CARTESIAN_POINT('Ctrl Pts',(7.97551818625927,-29.1861468994703,126.888047843324));
#98899=CARTESIAN_POINT('Ctrl Pts',(7.97937976390514,-29.2521370628543,126.915139798205));
#98900=CARTESIAN_POINT('Ctrl Pts',(7.983241341551,-29.319265868112,126.938710551935));
#98901=CARTESIAN_POINT('Ctrl Pts',(7.98710967570752,-29.3865121270452,126.962322546852));
#98902=CARTESIAN_POINT('Ctrl Pts',(7.99097800986404,-29.4549005391858,126.982400903186));
#98903=CARTESIAN_POINT('Ctrl Pts',(7.99484634402056,-29.5240255081322,126.998861137146));
#98904=CARTESIAN_POINT('Ctrl Pts',(7.9971440628058,-29.5650844583808,127.008638211009));
#98905=CARTESIAN_POINT('Ctrl Pts',(7.99944178159104,-29.606403090079,127.017139742853));
#98906=CARTESIAN_POINT('Ctrl Pts',(8.00173950037628,-29.6478955336573,127.024356689737));
#98907=CARTESIAN_POINT('Ctrl Pts',(8.00560732713487,-29.7177411494836,127.03650521742));
#98908=CARTESIAN_POINT('Ctrl Pts',(8.00947515389345,-29.7883530019275,127.045058506922));
#98909=CARTESIAN_POINT('Ctrl Pts',(8.01334298065203,-29.8593280972088,127.04992901786));
#98910=CARTESIAN_POINT('Ctrl Pts',(8.01720559832277,-29.9302076050894,127.054792969322));
#98911=CARTESIAN_POINT('Ctrl Pts',(8.0210682159935,-30.0014489054664,127.055983946858));
#98912=CARTESIAN_POINT('Ctrl Pts',(8.02493083366424,-30.0726400882567,127.053465602361));
#98913=CARTESIAN_POINT('Ctrl Pts',(8.0287895417393,-30.1437592140213,127.050949806836));
#98914=CARTESIAN_POINT('Ctrl Pts',(8.03264824981435,-30.2148278399929,127.04473215569));
#98915=CARTESIAN_POINT('Ctrl Pts',(8.03650695788941,-30.2854319494135,127.034828288764));
#98916=CARTESIAN_POINT('Ctrl Pts',(8.04036305129656,-30.3559882173556,127.024931132717));
#98917=CARTESIAN_POINT('Ctrl Pts',(8.0442191447037,-30.4260801137613,127.011352786755));
#98918=CARTESIAN_POINT('Ctrl Pts',(8.04807523811084,-30.4952983728753,126.994160746862));
#98919=CARTESIAN_POINT('Ctrl Pts',(8.05193146559612,-30.5645190387397,126.976968109195));
#98920=CARTESIAN_POINT('Ctrl Pts',(8.05578769308139,-30.6328655306219,126.956161625197));
#98921=CARTESIAN_POINT('Ctrl Pts',(8.05964392056666,-30.6999396635101,126.931859733507));
#98922=CARTESIAN_POINT('Ctrl Pts',(8.06349994445144,-30.7670102550287,126.907559124904));
#98923=CARTESIAN_POINT('Ctrl Pts',(8.06735596833621,-30.8328081664699,126.879763648163));
#98924=CARTESIAN_POINT('Ctrl Pts',(8.07121199222098,-30.896953393973,126.848640628013));
#98925=CARTESIAN_POINT('Ctrl Pts',(8.07507195471058,-30.9611641404433,126.817485818309));
#98926=CARTESIAN_POINT('Ctrl Pts',(8.07893191720017,-31.0237183952511,126.782996893766));
#98927=CARTESIAN_POINT('Ctrl Pts',(8.08279187968976,-31.0842598050853,126.745387704087));
#98928=CARTESIAN_POINT('Ctrl Pts',(8.08648092144372,-31.1421204162504,126.709443864883));
#98929=CARTESIAN_POINT('Ctrl Pts',(8.09016996319768,-31.1981423694488,126.670650507383));
#98930=CARTESIAN_POINT('Ctrl Pts',(8.09385900495164,-31.2520409112987,126.629230222815));
#98931=CARTESIAN_POINT('Ctrl Pts',(7.39391264968254,-31.2520409112987,126.629230222815));
#98932=CARTESIAN_POINT('Ctrl Pts',(7.39776808616367,-31.3085950960826,126.585769113352));
#98933=CARTESIAN_POINT('Ctrl Pts',(7.4016235226448,-31.3628767616946,126.539365209773));
#98934=CARTESIAN_POINT('Ctrl Pts',(7.40547895912594,-31.4145751387537,126.490293507776));
#98935=CARTESIAN_POINT('Ctrl Pts',(7.40933850596281,-31.4663286324569,126.441169489484));
#98936=CARTESIAN_POINT('Ctrl Pts',(7.41319805279968,-31.5154929878992,126.389372331323));
#98937=CARTESIAN_POINT('Ctrl Pts',(7.41705759963655,-31.5617941196262,126.335214099087));
#98938=CARTESIAN_POINT('Ctrl Pts',(7.42091943947241,-31.608122759362,126.281023690853));
#98939=CARTESIAN_POINT('Ctrl Pts',(7.42478127930827,-31.6515844936747,126.224469801876));
#98940=CARTESIAN_POINT('Ctrl Pts',(7.42864311914413,-31.6919470880459,126.165895627298));
#98941=CARTESIAN_POINT('Ctrl Pts',(7.43251160608088,-31.7323791555825,126.107220633302));
#98942=CARTESIAN_POINT('Ctrl Pts',(7.43638009301764,-31.7697011813615,126.046518826397));
#98943=CARTESIAN_POINT('Ctrl Pts',(7.44024857995439,-31.803725996472,125.984159586729));
#98944=CARTESIAN_POINT('Ctrl Pts',(7.44218676869742,-31.8207731042195,125.952916369853));
#98945=CARTESIAN_POINT('Ctrl Pts',(7.44412495744045,-31.83699328923,125.921257444323));
#98946=CARTESIAN_POINT('Ctrl Pts',(7.44606314618348,-31.8523676042174,125.889231028106));
#98947=CARTESIAN_POINT('Ctrl Pts',(7.44993221953132,-31.8830582954997,125.825298888442));
#98948=CARTESIAN_POINT('Ctrl Pts',(7.45380129287916,-31.9104954100681,125.759650781342));
#98949=CARTESIAN_POINT('Ctrl Pts',(7.457670366227,-31.9344849573817,125.692651075336));
#98950=CARTESIAN_POINT('Ctrl Pts',(7.4615336746224,-31.9584387600643,125.625751199465));
#98951=CARTESIAN_POINT('Ctrl Pts',(7.4653969830178,-31.9789550296805,125.557504175838));
#98952=CARTESIAN_POINT('Ctrl Pts',(7.4692602914132,-31.9958867364429,125.488296731293));
#98953=CARTESIAN_POINT('Ctrl Pts',(7.47311906790571,-32.0127985812519,125.419170471419));
#98954=CARTESIAN_POINT('Ctrl Pts',(7.47697784439821,-32.026134100711,125.349086498083));
#98955=CARTESIAN_POINT('Ctrl Pts',(7.48083662089072,-32.0357958014338,125.278447512764));
#98956=CARTESIAN_POINT('Ctrl Pts',(7.48469296647851,-32.0454514155968,125.207853027727));
#98957=CARTESIAN_POINT('Ctrl Pts',(7.4885493120663,-32.0514377370552,125.136704704554));
#98958=CARTESIAN_POINT('Ctrl Pts',(7.49240565765409,-32.0537084658798,125.065414827628));
#98959=CARTESIAN_POINT('Ctrl Pts',(7.49626086389899,-32.055978523826,124.99414601303));
#98960=CARTESIAN_POINT('Ctrl Pts',(7.5001160701439,-32.0545351530348,124.922736212981));
#98961=CARTESIAN_POINT('Ctrl Pts',(7.5039712763888,-32.0493840894916,124.851600484371));
#98962=CARTESIAN_POINT('Ctrl Pts',(7.50782663323961,-32.0442328247189,124.780461976803));
#98963=CARTESIAN_POINT('Ctrl Pts',(7.51168199009042,-32.0353736169087,124.709598046288));
#98964=CARTESIAN_POINT('Ctrl Pts',(7.51553734694123,-32.0228641528123,124.639419659761));
#98965=CARTESIAN_POINT('Ctrl Pts',(7.51939673940933,-32.0103415943612,124.569167813597));
#98966=CARTESIAN_POINT('Ctrl Pts',(7.52325613187744,-31.9941612376184,124.499603423133));
#98967=CARTESIAN_POINT('Ctrl Pts',(7.52711552434555,-31.9744319452394,124.431127381466));
#98968=CARTESIAN_POINT('Ctrl Pts',(7.53097710194852,-31.9546914824067,124.362612569607));
#98969=CARTESIAN_POINT('Ctrl Pts',(7.53483867955149,-31.9313982426254,124.2951877926));
#98970=CARTESIAN_POINT('Ctrl Pts',(7.53870025715446,-31.9047101700555,124.229236267987));
#98971=CARTESIAN_POINT('Ctrl Pts',(7.54256859126887,-31.8779754019933,124.163169349543));
#98972=CARTESIAN_POINT('Ctrl Pts',(7.54643692538327,-31.8478341475395,124.098581270326));
#98973=CARTESIAN_POINT('Ctrl Pts',(7.55030525949767,-31.8144911273661,124.03583221833));
#98974=CARTESIAN_POINT('Ctrl Pts',(7.55260297867246,-31.7946859878584,123.998560437841));
#98975=CARTESIAN_POINT('Ctrl Pts',(7.55490069784725,-31.7737520801978,123.961936982506));
#98976=CARTESIAN_POINT('Ctrl Pts',(7.55719841702204,-31.7517393818058,123.926032262714));
#98977=CARTESIAN_POINT('Ctrl Pts',(7.5610674903759,-31.7146727351375,123.865573179572));
#98978=CARTESIAN_POINT('Ctrl Pts',(7.56493656372977,-31.6743998063143,123.806916888848));
#98979=CARTESIAN_POINT('Ctrl Pts',(7.56880563708363,-31.6311215037072,123.75042399085));
#98980=CARTESIAN_POINT('Ctrl Pts',(7.57266894548509,-31.5879076861414,123.694015267753));
#98981=CARTESIAN_POINT('Ctrl Pts',(7.57653225388655,-31.5416976765799,123.639763921366));
#98982=CARTESIAN_POINT('Ctrl Pts',(7.58039556228801,-31.4927366374115,123.588003224568));
#98983=CARTESIAN_POINT('Ctrl Pts',(7.58425433878659,-31.4438330326106,123.536303246312));
#98984=CARTESIAN_POINT('Ctrl Pts',(7.58811311528517,-31.3921851405803,123.487088465385));
#98985=CARTESIAN_POINT('Ctrl Pts',(7.59197189178375,-31.3380784114637,123.440659201048));
#98986=CARTESIAN_POINT('Ctrl Pts',(7.59582823737763,-31.2840057678409,123.39425918565));
#98987=CARTESIAN_POINT('Ctrl Pts',(7.5996845829715,-31.2274777280884,123.350641520978));
#98988=CARTESIAN_POINT('Ctrl Pts',(7.60354092856538,-31.1688155588575,123.310068713861));
#98989=CARTESIAN_POINT('Ctrl Pts',(7.60739613481637,-31.1101707211453,123.269507893828));
#98990=CARTESIAN_POINT('Ctrl Pts',(7.61125134106735,-31.0493934050301,123.231990421594));
#98991=CARTESIAN_POINT('Ctrl Pts',(7.61510654731834,-30.9868354288779,123.197736590059));
#98992=CARTESIAN_POINT('Ctrl Pts',(7.61896190417522,-30.9242750088616,123.163481420378));
#98993=CARTESIAN_POINT('Ctrl Pts',(7.6228172610321,-30.8599342178517,123.132490375899));
#98994=CARTESIAN_POINT('Ctrl Pts',(7.62667261788899,-30.7941896142922,123.104937885174));
#98995=CARTESIAN_POINT('Ctrl Pts',(7.63053201036311,-30.7283761921859,123.077356553718));
#98996=CARTESIAN_POINT('Ctrl Pts',(7.63439140283724,-30.6611564731301,123.053221149228));
#98997=CARTESIAN_POINT('Ctrl Pts',(7.63825079531137,-30.5929263080741,123.032657641463));
#98998=CARTESIAN_POINT('Ctrl Pts',(7.64211237292035,-30.5246575120386,123.012082490923));
#98999=CARTESIAN_POINT('Ctrl Pts',(7.64597395052932,-30.455377603142,122.995083378819));
#99000=CARTESIAN_POINT('Ctrl Pts',(7.6498355281383,-30.385494202373,122.981735452812));
#99001=CARTESIAN_POINT('Ctrl Pts',(7.6537038622586,-30.3154885282649,122.968364172253));
#99002=CARTESIAN_POINT('Ctrl Pts',(7.6575721963789,-30.2448777355307,122.958656898589));
#99003=CARTESIAN_POINT('Ctrl Pts',(7.6614405304992,-30.1740754669361,122.952636990099));
#99004=CARTESIAN_POINT('Ctrl Pts',(7.66373824961967,-30.1320202252576,122.949061275486));
#99005=CARTESIAN_POINT('Ctrl Pts',(7.66603596874013,-30.0898974664779,122.946785516384));
#99006=CARTESIAN_POINT('Ctrl Pts',(7.6683336878606,-30.0477934513841,122.94580591265));
#99007=CARTESIAN_POINT('Ctrl Pts',(7.67220276119791,-29.9768955245042,122.94415638175));
#99008=CARTESIAN_POINT('Ctrl Pts',(7.67607183453523,-29.9057732297676,122.946178357979));
#99009=CARTESIAN_POINT('Ctrl Pts',(7.67994090787254,-29.8348384886821,122.951898626122));
#99010=CARTESIAN_POINT('Ctrl Pts',(7.68380421625744,-29.7640094409683,122.957610371017));
#99011=CARTESIAN_POINT('Ctrl Pts',(7.68766752464235,-29.6933678724612,122.967009430934));
#99012=CARTESIAN_POINT('Ctrl Pts',(7.69153083302725,-29.623326747495,122.980070589514));
#99013=CARTESIAN_POINT('Ctrl Pts',(7.69538960950936,-29.5533677851569,122.993116426536));
#99014=CARTESIAN_POINT('Ctrl Pts',(7.69924838599147,-29.4840083425025,123.009815740546));
#99015=CARTESIAN_POINT('Ctrl Pts',(7.70310716247358,-29.415655548727,123.030091594828));
#99016=CARTESIAN_POINT('Ctrl Pts',(7.70696350805104,-29.3473458150056,123.050354675976));
#99017=CARTESIAN_POINT('Ctrl Pts',(7.7108198536285,-29.2800419366338,123.074189689447));
#99018=CARTESIAN_POINT('Ctrl Pts',(7.71467619920596,-29.2141387005253,123.101469099412));
#99019=CARTESIAN_POINT('Ctrl Pts',(7.71853140544062,-29.1482549352802,123.128740449777));
#99020=CARTESIAN_POINT('Ctrl Pts',(7.72238661167528,-29.08377143937,123.159453990659));
#99021=CARTESIAN_POINT('Ctrl Pts',(7.72624181790994,-29.0210641040991,123.19343362308));
#99022=CARTESIAN_POINT('Ctrl Pts',(7.7300971747506,-28.9583543191277,123.227414582937));
#99023=CARTESIAN_POINT('Ctrl Pts',(7.73395253159126,-28.8974212586147,123.264661654274));
#99024=CARTESIAN_POINT('Ctrl Pts',(7.73780788843192,-28.8386156993583,123.304953077722));
#99025=CARTESIAN_POINT('Ctrl Pts',(7.74166728089009,-28.779748585036,123.345286676456));
#99026=CARTESIAN_POINT('Ctrl Pts',(7.74552667334827,-28.7230138190774,123.38867071352));
#99027=CARTESIAN_POINT('Ctrl Pts',(7.74938606580644,-28.6687319295004,123.434840938764));
#99028=CARTESIAN_POINT('Ctrl Pts',(7.75324764339958,-28.6144193062634,123.481037304956));
#99029=CARTESIAN_POINT('Ctrl Pts',(7.75710922099272,-28.5625626773577,123.530022665901));
#99030=CARTESIAN_POINT('Ctrl Pts',(7.76097079858587,-28.51344625659,123.581495318847));
#99031=CARTESIAN_POINT('Ctrl Pts',(7.76483913269071,-28.4642438979735,123.633058032286));
#99032=CARTESIAN_POINT('Ctrl Pts',(7.76870746679556,-28.4177916365127,123.687116357972));
#99033=CARTESIAN_POINT('Ctrl Pts',(7.7725758009004,-28.3743334414932,123.743335445295));
#99034=CARTESIAN_POINT('Ctrl Pts',(7.77487352016666,-28.3485200734473,123.77672854852));
#99035=CARTESIAN_POINT('Ctrl Pts',(7.77717123943291,-28.3237622359318,123.810883425082));
#99036=CARTESIAN_POINT('Ctrl Pts',(7.77946895869917,-28.3001035210426,123.84572554246));
#99037=CARTESIAN_POINT('Ctrl Pts',(7.78339694507704,-28.2596585845495,123.905288677283));
#99038=CARTESIAN_POINT('Ctrl Pts',(7.78732493145491,-28.2222729070755,123.967090244453));
#99039=CARTESIAN_POINT('Ctrl Pts',(7.79125291783279,-28.1881978044253,124.030788791537));
#99040=CARTESIAN_POINT('Ctrl Pts',(7.79517455591714,-28.1541777729319,124.094384390943));
#99041=CARTESIAN_POINT('Ctrl Pts',(7.79909619400149,-28.123457908575,124.159870473946));
#99042=CARTESIAN_POINT('Ctrl Pts',(7.80301783208584,-28.0962464209973,124.226876547417));
#99043=CARTESIAN_POINT('Ctrl Pts',(7.80693336836405,-28.0690772726713,124.293778363926));
#99044=CARTESIAN_POINT('Ctrl Pts',(7.81084890464227,-28.0454058202885,124.362195038258));
#99045=CARTESIAN_POINT('Ctrl Pts',(7.81476444092048,-28.02539366553,124.431732997288));
#99046=CARTESIAN_POINT('Ctrl Pts',(7.8186763855966,-28.0053998673111,124.501207171268));
#99047=CARTESIAN_POINT('Ctrl Pts',(7.82258833027271,-27.9890588288581,124.571800140759));
#99048=CARTESIAN_POINT('Ctrl Pts',(7.82650027494883,-27.9764831076761,124.643100926059));
#99049=CARTESIAN_POINT('Ctrl Pts',(7.83040988896492,-27.9639148788626,124.714359231747));
#99050=CARTESIAN_POINT('Ctrl Pts',(7.834319502981,-27.9551075924963,124.786324057108));
#99051=CARTESIAN_POINT('Ctrl Pts',(7.83822911699709,-27.9501229160446,124.858573329338));
#99052=CARTESIAN_POINT('Ctrl Pts',(7.84079450484395,-27.9468520999648,124.905981437698));
#99053=CARTESIAN_POINT('Ctrl Pts',(7.84335989269082,-27.9452261188357,124.95351178974));
#99054=CARTESIAN_POINT('Ctrl Pts',(7.84592528053768,-27.945250265129,125.001043813945));
#99055=CARTESIAN_POINT('Origin',(-1.54592528053767,-30.,125.));
#99056=CARTESIAN_POINT('',(6.69398884812234,-31.2520409112987,126.629230222815));
#99057=CARTESIAN_POINT('',(6.75200666526939,-31.2520409112987,126.629230222815));
#99058=CARTESIAN_POINT('',(-1.54592528053767,-31.2520409112987,126.629230222815));
#99059=CARTESIAN_POINT('',(7.20407471942241,-27.945250640964,125.001622972929));
#99060=CARTESIAN_POINT('Ctrl Pts',(6.75200666526939,-31.2520409112987,126.629230222815));
#99061=CARTESIAN_POINT('Ctrl Pts',(6.755869548117,-31.3085483116843,126.585805066515));
#99062=CARTESIAN_POINT('Ctrl Pts',(6.75973243096461,-31.3627333351714,126.539483224137));
#99063=CARTESIAN_POINT('Ctrl Pts',(6.76359531381222,-31.4143002468284,126.490554384892));
#99064=CARTESIAN_POINT('Ctrl Pts',(6.76746446389324,-31.4659508218749,126.441546162329));
#99065=CARTESIAN_POINT('Ctrl Pts',(6.77133361397426,-31.5149744812624,126.389922859516));
#99066=CARTESIAN_POINT('Ctrl Pts',(6.77520276405529,-31.5611146244003,126.336008492482));
#99067=CARTESIAN_POINT('Ctrl Pts',(6.77582755793078,-31.5685653766956,126.327302351438));
#99068=CARTESIAN_POINT('Ctrl Pts',(6.77645235180628,-31.5759410293061,126.31853653065));
#99069=CARTESIAN_POINT('Ctrl Pts',(6.77707714568177,-31.583240608486,126.309712463917));
#99070=CARTESIAN_POINT('Ctrl Pts',(6.78094621902986,-31.6284436880375,126.255068904246));
#99071=CARTESIAN_POINT('Ctrl Pts',(6.78481529237795,-31.6709030568395,126.197975373758));
#99072=CARTESIAN_POINT('Ctrl Pts',(6.78868436572603,-31.7103425768986,126.138738702314));
#99073=CARTESIAN_POINT('Ctrl Pts',(6.79254767412169,-31.749723331735,126.079590294018));
#99074=CARTESIAN_POINT('Ctrl Pts',(6.79641098251735,-31.7860929023809,126.01830548444));
#99075=CARTESIAN_POINT('Ctrl Pts',(6.800274290913,-31.8192153334322,125.955224127158));
#99076=CARTESIAN_POINT('Ctrl Pts',(6.80413306740579,-31.852298909796,125.892216768262));
#99077=CARTESIAN_POINT('Ctrl Pts',(6.80799184389858,-31.8821426879839,125.827417475811));
#99078=CARTESIAN_POINT('Ctrl Pts',(6.81185062039136,-31.9085549343313,125.761193553007));
#99079=CARTESIAN_POINT('Ctrl Pts',(6.81570696597944,-31.9349505418155,125.695011349139));
#99080=CARTESIAN_POINT('Ctrl Pts',(6.81956331156752,-31.9579187268081,125.627406745642));
#99081=CARTESIAN_POINT('Ctrl Pts',(6.8234196571556,-31.9773151269986,125.558768691896));
#99082=CARTESIAN_POINT('Ctrl Pts',(6.82727486340081,-31.9967057965952,125.490150917006));
#99083=CARTESIAN_POINT('Ctrl Pts',(6.83113006964602,-32.0125266443608,125.420500765254));
#99084=CARTESIAN_POINT('Ctrl Pts',(6.83498527589122,-32.0246831393671,125.350222425985));
#99085=CARTESIAN_POINT('Ctrl Pts',(6.83884063274235,-32.036840109274,125.279941341251));
#99086=CARTESIAN_POINT('Ctrl Pts',(6.84269598959347,-32.0453323615862,125.209032499331));
#99087=CARTESIAN_POINT('Ctrl Pts',(6.8465513464446,-32.0501167691149,125.137908649091));
#99088=CARTESIAN_POINT('Ctrl Pts',(6.85041073891303,-32.05490618475,125.066710349545));
#99089=CARTESIAN_POINT('Ctrl Pts',(6.85427013138147,-32.0559799751667,124.995297078089));
#99090=CARTESIAN_POINT('Ctrl Pts',(6.85812952384991,-32.0533471080323,124.924084148985));
#99091=CARTESIAN_POINT('Ctrl Pts',(6.86199110145323,-32.0507127502048,124.852830900101));
#99092=CARTESIAN_POINT('Ctrl Pts',(6.86585267905654,-32.0443676002752,124.781778703463));
#99093=CARTESIAN_POINT('Ctrl Pts',(6.86971425665986,-32.0343725214633,124.711337556279));
#99094=CARTESIAN_POINT('Ctrl Pts',(6.87358259077461,-32.0243599544973,124.640773159877));
#99095=CARTESIAN_POINT('Ctrl Pts',(6.87745092488936,-32.010684801661,124.570822424408));
#99096=CARTESIAN_POINT('Ctrl Pts',(6.88131925900412,-31.993458875968,124.50188427818));
#99097=CARTESIAN_POINT('Ctrl Pts',(6.88361697817619,-31.9832269935744,124.460936289827));
#99098=CARTESIAN_POINT('Ctrl Pts',(6.88591469734826,-31.9717433059035,124.420345270084));
#99099=CARTESIAN_POINT('Ctrl Pts',(6.88821241652033,-31.9590393346454,124.380191603951));
#99100=CARTESIAN_POINT('Ctrl Pts',(6.89208148986845,-31.9376474268754,124.312577823577));
#99101=CARTESIAN_POINT('Ctrl Pts',(6.89595056321657,-31.9127091017341,124.245940377934));
#99102=CARTESIAN_POINT('Ctrl Pts',(6.89981963656469,-31.8843323730222,124.180677676076));
#99103=CARTESIAN_POINT('Ctrl Pts',(6.90368294496038,-31.8559979258791,124.115512216202));
#99104=CARTESIAN_POINT('Ctrl Pts',(6.90754625335606,-31.824235436801,124.051717876002));
#99105=CARTESIAN_POINT('Ctrl Pts',(6.91140956175175,-31.7892024578461,123.989677216263));
#99106=CARTESIAN_POINT('Ctrl Pts',(6.91526833824456,-31.7542105747712,123.927709334107));
#99107=CARTESIAN_POINT('Ctrl Pts',(6.91912711473738,-31.7159560600875,123.867491467115));
#99108=CARTESIAN_POINT('Ctrl Pts',(6.92298589123019,-31.6746435117619,123.809383911156));
#99109=CARTESIAN_POINT('Ctrl Pts',(6.9268422368183,-31.6333569890091,123.751312961083));
#99110=CARTESIAN_POINT('Ctrl Pts',(6.9306985824064,-31.5890165355058,123.695350079465));
#99111=CARTESIAN_POINT('Ctrl Pts',(6.93455492799451,-31.5418706276353,123.641827503542));
#99112=CARTESIAN_POINT('Ctrl Pts',(6.93841013423974,-31.4947386488468,123.588320740663));
#99113=CARTESIAN_POINT('Ctrl Pts',(6.94226534048497,-31.4448031821351,123.537253216468));
#99114=CARTESIAN_POINT('Ctrl Pts',(6.9461205467302,-31.3923525343944,123.488923568291));
#99115=CARTESIAN_POINT('Ctrl Pts',(6.94997590358134,-31.3398998376382,123.440592032088));
#99116=CARTESIAN_POINT('Ctrl Pts',(6.95383126043248,-31.2849321235192,123.394998911814));
#99117=CARTESIAN_POINT('Ctrl Pts',(6.95768661728363,-31.2277727696999,123.35240430066));
#99118=CARTESIAN_POINT('Ctrl Pts',(6.96154600975208,-31.1705535839931,123.309765103348));
#99119=CARTESIAN_POINT('Ctrl Pts',(6.96540540222054,-31.111138569348,123.270130971585));
#99120=CARTESIAN_POINT('Ctrl Pts',(6.96926479468899,-31.0498815131056,123.233719622784));
#99121=CARTESIAN_POINT('Ctrl Pts',(6.97312637229232,-30.9885897739615,123.197287658378));
#99122=CARTESIAN_POINT('Ctrl Pts',(6.97698794989566,-30.9254543472026,123.164082335571));
#99123=CARTESIAN_POINT('Ctrl Pts',(6.98084952749899,-30.8608526993657,123.134274888282));
#99124=CARTESIAN_POINT('Ctrl Pts',(6.98471786161376,-30.7961380195462,123.104415287604));
#99125=CARTESIAN_POINT('Ctrl Pts',(6.98858619572852,-30.7299524479699,123.077965612502));
#99126=CARTESIAN_POINT('Ctrl Pts',(6.99245452984329,-30.662691785049,123.055048288381));
#99127=CARTESIAN_POINT('Ctrl Pts',(6.99475224901516,-30.6227401908689,123.041435820213));
#99128=CARTESIAN_POINT('Ctrl Pts',(6.99704996818703,-30.5824095673422,123.029068655138));
#99129=CARTESIAN_POINT('Ctrl Pts',(6.9993476873589,-30.5417845456429,123.01796390835));
#99130=CARTESIAN_POINT('Ctrl Pts',(7.00321676070784,-30.47337706109,122.999264895707));
#99131=CARTESIAN_POINT('Ctrl Pts',(7.00708583405677,-30.4038663884582,122.984074911669));
#99132=CARTESIAN_POINT('Ctrl Pts',(7.01095490740571,-30.3336458313534,122.972519291899));
#99133=CARTESIAN_POINT('Ctrl Pts',(7.01481821580221,-30.2635299034802,122.960980890102));
#99134=CARTESIAN_POINT('Ctrl Pts',(7.01868152419872,-30.1927066661399,122.953066181724));
#99135=CARTESIAN_POINT('Ctrl Pts',(7.02254483259522,-30.1215829758924,122.94885028765));
#99136=CARTESIAN_POINT('Ctrl Pts',(7.02640360908886,-30.0505427181911,122.944639339084));
#99137=CARTESIAN_POINT('Ctrl Pts',(7.03026238558249,-29.9792031902488,122.944118614824));
#99138=CARTESIAN_POINT('Ctrl Pts',(7.03412116207613,-29.9079780589086,122.947311634744));
#99139=CARTESIAN_POINT('Ctrl Pts',(7.03797750766506,-29.8367977971034,122.950502643165));
#99140=CARTESIAN_POINT('Ctrl Pts',(7.04183385325398,-29.7657322730734,122.957402732454));
#99141=CARTESIAN_POINT('Ctrl Pts',(7.04569019884291,-29.6951953784619,122.967983340327));
#99142=CARTESIAN_POINT('Ctrl Pts',(7.04954540508896,-29.624679323712,122.978560822198));
#99143=CARTESIAN_POINT('Ctrl Pts',(7.05340061133501,-29.5546920684666,122.992816591849));
#99144=CARTESIAN_POINT('Ctrl Pts',(7.05725581758106,-29.4856408782643,123.010670400264));
#99145=CARTESIAN_POINT('Ctrl Pts',(7.06111117443302,-29.4165869905364,123.028524906148));
#99146=CARTESIAN_POINT('Ctrl Pts',(7.06496653128498,-29.3484697102204,123.049977606121));
#99147=CARTESIAN_POINT('Ctrl Pts',(7.06882188813695,-29.2816829413656,123.074897881728));
#99148=CARTESIAN_POINT('Ctrl Pts',(7.07268128060621,-29.2148262630703,123.099844242779));
#99149=CARTESIAN_POINT('Ctrl Pts',(7.07654067307548,-29.1493033324867,123.128265254999));
#99150=CARTESIAN_POINT('Ctrl Pts',(7.08040006554475,-29.0854889450426,123.159981768335));
#99151=CARTESIAN_POINT('Ctrl Pts',(7.08426164314888,-29.0216384267712,123.191716239124));
#99152=CARTESIAN_POINT('Ctrl Pts',(7.08812322075302,-28.9594988007089,123.226749686707));
#99153=CARTESIAN_POINT('Ctrl Pts',(7.09198479835716,-28.8994186522218,123.264857856133));
#99154=CARTESIAN_POINT('Ctrl Pts',(7.09585313247272,-28.8392333829133,123.303032702526));
#99155=CARTESIAN_POINT('Ctrl Pts',(7.09972146658828,-28.7811151817515,123.344292730321));
#99156=CARTESIAN_POINT('Ctrl Pts',(7.10358980070384,-28.7253815715797,123.388371809495));
#99157=CARTESIAN_POINT('Ctrl Pts',(7.10588751986837,-28.6922768344048,123.41455397007));
#99158=CARTESIAN_POINT('Ctrl Pts',(7.10818523903291,-28.6600127586917,123.441729977376));
#99159=CARTESIAN_POINT('Ctrl Pts',(7.11048295819744,-28.6286496245686,123.469838011744));
#99160=CARTESIAN_POINT('Ctrl Pts',(7.11438261491515,-28.5754205535146,123.517542573179));
#99161=CARTESIAN_POINT('Ctrl Pts',(7.11828227163285,-28.524561791372,123.568137518425));
#99162=CARTESIAN_POINT('Ctrl Pts',(7.12218192835056,-28.4764092303526,123.621352572575));
#99163=CARTESIAN_POINT('Ctrl Pts',(7.12598698948199,-28.4294247259264,123.673276767142));
#99164=CARTESIAN_POINT('Ctrl Pts',(7.12979205061342,-28.3850169998354,123.727695018053));
#99165=CARTESIAN_POINT('Ctrl Pts',(7.13359711174485,-28.3434646904679,123.784315694445));
#99166=CARTESIAN_POINT('Ctrl Pts',(7.13739855500662,-28.3019518892276,123.840882535637));
#99167=CARTESIAN_POINT('Ctrl Pts',(7.1411999982684,-28.2632894189908,123.899647249871));
#99168=CARTESIAN_POINT('Ctrl Pts',(7.14500144153017,-28.2277166035248,123.960284113289));
#99169=CARTESIAN_POINT('Ctrl Pts',(7.14880063066554,-28.1921648815271,124.020885021112));
#99170=CARTESIAN_POINT('Ctrl Pts',(7.15259981980092,-28.1596994342751,124.08335544493));
#99171=CARTESIAN_POINT('Ctrl Pts',(7.15639900893629,-28.1305159752474,124.147341191511));
#99172=CARTESIAN_POINT('Ctrl Pts',(7.16037198481014,-28.0999975739514,124.214253845336));
#99173=CARTESIAN_POINT('Ctrl Pts',(7.16434496068397,-28.0730689420479,124.28282328704));
#99174=CARTESIAN_POINT('Ctrl Pts',(7.16831793655782,-28.0498988919779,124.352618172181));
#99175=CARTESIAN_POINT('Ctrl Pts',(7.17211850690874,-28.0277342959365,124.419384339289));
#99176=CARTESIAN_POINT('Ctrl Pts',(7.17591907725967,-28.009008924727,124.487271268717));
#99177=CARTESIAN_POINT('Ctrl Pts',(7.17971964761059,-27.9938195467489,124.555885654934));
#99178=CARTESIAN_POINT('Ctrl Pts',(7.18352169695498,-27.9786242578183,124.624526742467));
#99179=CARTESIAN_POINT('Ctrl Pts',(7.18732374629936,-27.9669677847571,124.693895355798));
#99180=CARTESIAN_POINT('Ctrl Pts',(7.19112579564375,-27.9588954503773,124.763589805614));
#99181=CARTESIAN_POINT('Ctrl Pts',(7.19493249874065,-27.9508132353665,124.833369562246));
#99182=CARTESIAN_POINT('Ctrl Pts',(7.19873920183755,-27.9463239372871,124.903475451104));
#99183=CARTESIAN_POINT('Ctrl Pts',(7.20254590493445,-27.9454208415865,124.973503881172));
#99184=CARTESIAN_POINT('Ctrl Pts',(7.20305550976377,-27.9452999438126,124.982878614437));
#99185=CARTESIAN_POINT('Ctrl Pts',(7.20356511459309,-27.9452432391408,124.992251965449));
#99186=CARTESIAN_POINT('Ctrl Pts',(7.20407471942241,-27.945250640964,125.001622972929));
#99187=CARTESIAN_POINT('Ctrl Pts',(7.20407471946233,-27.9452506409646,125.001622973663));
#99188=CARTESIAN_POINT('Ctrl Pts',(7.20992255598689,-27.9453355786831,125.109157511513));
#99189=CARTESIAN_POINT('Ctrl Pts',(7.21577039251146,-27.95386409323,125.216366166843));
#99190=CARTESIAN_POINT('Ctrl Pts',(7.22161822903602,-27.9706730699826,125.322226277026));
#99191=CARTESIAN_POINT('Ctrl Pts',(7.22548730238386,-27.9817943049358,125.392265945404));
#99192=CARTESIAN_POINT('Ctrl Pts',(7.2293563757317,-27.9965675768644,125.461866373981));
#99193=CARTESIAN_POINT('Ctrl Pts',(7.23322544907954,-28.0149451914192,125.530617535924));
#99194=CARTESIAN_POINT('Ctrl Pts',(7.23708875747494,-28.0332954231708,125.599266258047));
#99195=CARTESIAN_POINT('Ctrl Pts',(7.24095206587034,-28.055239212827,125.667067759863));
#99196=CARTESIAN_POINT('Ctrl Pts',(7.24481537426573,-28.0806775244239,125.733620335902));
#99197=CARTESIAN_POINT('Ctrl Pts',(7.24867415075823,-28.1060859952868,125.800094841597));
#99198=CARTESIAN_POINT('Ctrl Pts',(7.25253292725074,-28.1349806729059,125.86532288007));
#99199=CARTESIAN_POINT('Ctrl Pts',(7.25639170374324,-28.1672126922306,125.92891778268));
#99200=CARTESIAN_POINT('Ctrl Pts',(7.26024804933102,-28.1994244064229,125.992472622553));
#99201=CARTESIAN_POINT('Ctrl Pts',(7.26410439491881,-28.2349690720618,126.054395935445));
#99202=CARTESIAN_POINT('Ctrl Pts',(7.26796074050659,-28.2736502676501,126.114322289158));
#99203=CARTESIAN_POINT('Ctrl Pts',(7.27181594675149,-28.3123200350238,126.174230937855));
#99204=CARTESIAN_POINT('Ctrl Pts',(7.27567115299639,-28.3541242293327,126.232143390751));
#99205=CARTESIAN_POINT('Ctrl Pts',(7.27952635924128,-28.3988220533987,126.287721532715));
#99206=CARTESIAN_POINT('Ctrl Pts',(7.28338171609209,-28.4435216236116,126.343301845872));
#99207=CARTESIAN_POINT('Ctrl Pts',(7.28723707294289,-28.4911147418495,126.396547289877));
#99208=CARTESIAN_POINT('Ctrl Pts',(7.2910924297937,-28.5413202085746,126.447152662502));
#99209=CARTESIAN_POINT('Ctrl Pts',(7.2949518222618,-28.5915782281652,126.497811006596));
#99210=CARTESIAN_POINT('Ctrl Pts',(7.2988112147299,-28.6444537120632,126.545823417154));
#99211=CARTESIAN_POINT('Ctrl Pts',(7.302670607198,-28.6996290992405,126.59092208576));
#99212=CARTESIAN_POINT('Ctrl Pts',(7.30653218480097,-28.7548357259622,126.636046288611));
#99213=CARTESIAN_POINT('Ctrl Pts',(7.31039376240394,-28.8123444563731,126.678253177863));
#99214=CARTESIAN_POINT('Ctrl Pts',(7.31425534000691,-28.871807414335,126.717317399944));
#99215=CARTESIAN_POINT('Ctrl Pts',(7.31812367412132,-28.9313744132346,126.756449971774));
#99216=CARTESIAN_POINT('Ctrl Pts',(7.32199200823571,-28.992902046864,126.79242865292));
#99217=CARTESIAN_POINT('Ctrl Pts',(7.32586034235011,-29.0560170650786,126.825073637166));
#99218=CARTESIAN_POINT('Ctrl Pts',(7.32815806152493,-29.0935062227578,126.844464156196));
#99219=CARTESIAN_POINT('Ctrl Pts',(7.33045578069975,-29.1315550146588,126.862679408199));
#99220=CARTESIAN_POINT('Ctrl Pts',(7.33275349987457,-29.1700822865554,126.879689908312));
#99221=CARTESIAN_POINT('Ctrl Pts',(7.33662257322846,-29.2349574213094,126.908333475135));
#99222=CARTESIAN_POINT('Ctrl Pts',(7.34049164658234,-29.3014442652705,126.933670578712));
#99223=CARTESIAN_POINT('Ctrl Pts',(7.34436071993624,-29.3691724693324,126.955518905317));
#99224=CARTESIAN_POINT('Ctrl Pts',(7.34822402833771,-29.4367997577907,126.977334677728));
#99225=CARTESIAN_POINT('Ctrl Pts',(7.35208733673919,-29.5056642763131,126.995671843735));
#99226=CARTESIAN_POINT('Ctrl Pts',(7.35595064514066,-29.5753748210843,127.010395737145));
#99227=CARTESIAN_POINT('Ctrl Pts',(7.35980942163927,-29.6450035910178,127.025102358505));
#99228=CARTESIAN_POINT('Ctrl Pts',(7.36366819813788,-29.7154759428823,127.03620402665));
#99229=CARTESIAN_POINT('Ctrl Pts',(7.36752697463649,-29.7863862804515,127.043616094407));
#99230=CARTESIAN_POINT('Ctrl Pts',(7.37138332023038,-29.8572519467955,127.051023492802));
#99231=CARTESIAN_POINT('Ctrl Pts',(7.37523966582429,-29.9285545694183,127.054745851857));
#99232=CARTESIAN_POINT('Ctrl Pts',(7.37909601141819,-29.999880600845,127.054749996531));
#99233=CARTESIAN_POINT('Ctrl Pts',(7.3829512176692,-30.0711855592625,127.05475413998));
#99234=CARTESIAN_POINT('Ctrl Pts',(7.38680642392021,-30.1425134272324,127.051042249909));
#99235=CARTESIAN_POINT('Ctrl Pts',(7.39066163017122,-30.2134495397625,127.043633249014));
#99236=CARTESIAN_POINT('Ctrl Pts',(7.39451698702813,-30.2843884234535,127.036223958681));
#99237=CARTESIAN_POINT('Ctrl Pts',(7.39837234388504,-30.3549350383914,127.025117323432));
#99238=CARTESIAN_POINT('Ctrl Pts',(7.40222770074195,-30.4246804583584,127.010384060519));
#99239=CARTESIAN_POINT('Ctrl Pts',(7.4060870932161,-30.4944988847499,126.995635375477));
#99240=CARTESIAN_POINT('Ctrl Pts',(7.40994648569025,-30.5635139657549,126.977252585325));
#99241=CARTESIAN_POINT('Ctrl Pts',(7.41380587816441,-30.6313284701612,126.955357237249));
#99242=CARTESIAN_POINT('Ctrl Pts',(7.4176674557734,-30.6991813702056,126.93344949233));
#99243=CARTESIAN_POINT('Ctrl Pts',(7.4215290333824,-30.7658318863786,126.908025403693));
#99244=CARTESIAN_POINT('Ctrl Pts',(7.4253906109914,-30.830902013802,126.879255013552));
#99245=CARTESIAN_POINT('Ctrl Pts',(7.42925894511172,-30.8960859928938,126.850434284537));
#99246=CARTESIAN_POINT('Ctrl Pts',(7.43312727923205,-30.9596836288983,126.818255783838));
#99247=CARTESIAN_POINT('Ctrl Pts',(7.43699561335237,-31.0213414213069,126.782935574726));
#99248=CARTESIAN_POINT('Ctrl Pts',(7.43929333247263,-31.0579650127866,126.761956021956));
#99249=CARTESIAN_POINT('Ctrl Pts',(7.44159105159288,-31.0939047367783,126.739868873526));
#99250=CARTESIAN_POINT('Ctrl Pts',(7.44388877071314,-31.1290918066321,126.716726319102));
#99251=CARTESIAN_POINT('Ctrl Pts',(7.44663011023724,-31.1710724405908,126.689115633978));
#99252=CARTESIAN_POINT('Ctrl Pts',(7.44937144976133,-31.2120978673782,126.65992590008));
#99253=CARTESIAN_POINT('Ctrl Pts',(7.45211278928543,-31.2520409112987,126.629230222815));
#99254=CARTESIAN_POINT('',(7.14592528050144,-27.9452507538412,124.998239912027));
#99255=CARTESIAN_POINT('Ctrl Pts',(7.14592528053768,-27.9452507538406,124.998239912696));
#99256=CARTESIAN_POINT('Ctrl Pts',(7.14975890798157,-27.9451900689549,125.069084252562));
#99257=CARTESIAN_POINT('Ctrl Pts',(7.15359253542545,-27.9487975671426,125.139993721178));
#99258=CARTESIAN_POINT('Ctrl Pts',(7.15742616286934,-27.9560667657221,125.210557584319));
#99259=CARTESIAN_POINT('Ctrl Pts',(7.16125834634974,-27.9633332263054,125.281094869071));
#99260=CARTESIAN_POINT('Ctrl Pts',(7.16509052983015,-27.9742586004264,125.35128631759));
#99261=CARTESIAN_POINT('Ctrl Pts',(7.16892271331055,-27.9887844405883,125.420725012425));
#99262=CARTESIAN_POINT('Ctrl Pts',(7.17275477350129,-28.0033098134223,125.490161473266));
#99263=CARTESIAN_POINT('Ctrl Pts',(7.17658683369203,-28.0214353197379,125.558844747248));
#99264=CARTESIAN_POINT('Ctrl Pts',(7.18041889388276,-28.0430515099182,125.626378615269));
#99265=CARTESIAN_POINT('Ctrl Pts',(7.18425485641198,-28.0646897127202,125.6939812557));
#99266=CARTESIAN_POINT('Ctrl Pts',(7.1880908189412,-28.0898255471087,125.760431683205));
#99267=CARTESIAN_POINT('Ctrl Pts',(7.19192678147043,-28.1183001035361,125.82535026634));
#99268=CARTESIAN_POINT('Ctrl Pts',(7.19576473620619,-28.14678944822,125.890302564932));
#99269=CARTESIAN_POINT('Ctrl Pts',(7.19960269094194,-28.1786207453222,125.953720995485));
#99270=CARTESIAN_POINT('Ctrl Pts',(7.2034406456777,-28.2135887279824,126.015249885353));
#99271=CARTESIAN_POINT('Ctrl Pts',(7.20728565489047,-28.2486209846758,126.076891870389));
#99272=CARTESIAN_POINT('Ctrl Pts',(7.21113066410324,-28.2868011751739,126.136636963846));
#99273=CARTESIAN_POINT('Ctrl Pts',(7.21497567331601,-28.3278806171451,126.194158419968));
#99274=CARTESIAN_POINT('Ctrl Pts',(7.21791465037946,-28.3592801616071,126.238125607261));
#99275=CARTESIAN_POINT('Ctrl Pts',(7.22085362744291,-28.392372683204,126.280794230267));
#99276=CARTESIAN_POINT('Ctrl Pts',(7.22379260450636,-28.427032275437,126.322032563889));
#99277=CARTESIAN_POINT('Ctrl Pts',(7.22766167785529,-28.472660567764,126.376321567895));
#99278=CARTESIAN_POINT('Ctrl Pts',(7.23153075120422,-28.5211921084715,126.428351931928));
#99279=CARTESIAN_POINT('Ctrl Pts',(7.23539982455315,-28.5723747010316,126.477796862984));
#99280=CARTESIAN_POINT('Ctrl Pts',(7.23926313294966,-28.6234810310905,126.52716812067));
#99281=CARTESIAN_POINT('Ctrl Pts',(7.24312644134617,-28.6772302256488,126.57396125735));
#99282=CARTESIAN_POINT('Ctrl Pts',(7.24698974974267,-28.7333303795212,126.617883072121));
#99283=CARTESIAN_POINT('Ctrl Pts',(7.2508485262363,-28.7893647243971,126.66175336385));
#99284=CARTESIAN_POINT('Ctrl Pts',(7.25470730272993,-28.8477441699736,126.702758726121));
#99285=CARTESIAN_POINT('Ctrl Pts',(7.25856607922356,-28.9081418596759,126.74064452543));
#99286=CARTESIAN_POINT('Ctrl Pts',(7.26242242481248,-28.968501500782,126.778506457907));
#99287=CARTESIAN_POINT('Ctrl Pts',(7.2662787704014,-29.0308764529679,126.813252468867));
#99288=CARTESIAN_POINT('Ctrl Pts',(7.27013511599032,-29.09491005105,126.844670633693));
#99289=CARTESIAN_POINT('Ctrl Pts',(7.27399032223637,-29.1589247306451,126.87607951614));
#99290=CARTESIAN_POINT('Ctrl Pts',(7.27784552848242,-29.2245966473887,126.904162290511));
#99291=CARTESIAN_POINT('Ctrl Pts',(7.28170073472847,-29.291545187166,126.92875331255));
#99292=CARTESIAN_POINT('Ctrl Pts',(7.28555609158043,-29.3584963423276,126.953345295252));
#99293=CARTESIAN_POINT('Ctrl Pts',(7.28941144843239,-29.4267237627802,126.974445089378));
#99294=CARTESIAN_POINT('Ctrl Pts',(7.29326680528435,-29.4958291744837,126.991936078592));
#99295=CARTESIAN_POINT('Ctrl Pts',(7.29712619775361,-29.5650069226805,127.009445376602));
#99296=CARTESIAN_POINT('Ctrl Pts',(7.30098559022287,-29.6350640248431,127.023338209445));
#99297=CARTESIAN_POINT('Ctrl Pts',(7.30484498269213,-29.7055903192736,127.033548746009));
#99298=CARTESIAN_POINT('Ctrl Pts',(7.30870656029626,-29.7761565447209,127.043765063638));
#99299=CARTESIAN_POINT('Ctrl Pts',(7.31256813790039,-29.8471920072879,127.050294890176));
#99300=CARTESIAN_POINT('Ctrl Pts',(7.31642971550451,-29.9182824475051,127.053124400545));
#99301=CARTESIAN_POINT('Ctrl Pts',(7.32029804962007,-29.989497272992,127.055958861642));
#99302=CARTESIAN_POINT('Ctrl Pts',(7.32416638373562,-30.0607667822781,127.055080086321));
#99303=CARTESIAN_POINT('Ctrl Pts',(7.32803471785117,-30.1316784462816,127.050526359081));
#99304=CARTESIAN_POINT('Ctrl Pts',(7.33033243701576,-30.1737986676757,127.047821529033));
#99305=CARTESIAN_POINT('Ctrl Pts',(7.33263015618034,-30.2157927465829,127.043821117613));
#99306=CARTESIAN_POINT('Ctrl Pts',(7.33492787534492,-30.257575941264,127.038541683896));
#99307=CARTESIAN_POINT('Ctrl Pts',(7.33879679457318,-30.327930842686,127.029652128142));
#99308=CARTESIAN_POINT('Ctrl Pts',(7.34266571380144,-30.3979628056788,127.017098714014));
#99309=CARTESIAN_POINT('Ctrl Pts',(7.34653463302971,-30.4672605439819,127.000916076835));
#99310=CARTESIAN_POINT('Ctrl Pts',(7.35048280108411,-30.537977739268,126.984401963365));
#99311=CARTESIAN_POINT('Ctrl Pts',(7.35443096913851,-30.6079297816178,126.964108265274));
#99312=CARTESIAN_POINT('Ctrl Pts',(7.35837913719291,-30.6766848743087,126.940127610077));
#99313=CARTESIAN_POINT('Ctrl Pts',(7.36223776856797,-30.7438807368446,126.916690788933));
#99314=CARTESIAN_POINT('Ctrl Pts',(7.36609639994304,-30.8099328790602,126.889732638835));
#99315=CARTESIAN_POINT('Ctrl Pts',(7.3699550313181,-30.8744504841252,126.859390737127));
#99316=CARTESIAN_POINT('Ctrl Pts',(7.37394796771217,-30.9412137139551,126.827992743429));
#99317=CARTESIAN_POINT('Ctrl Pts',(7.37794090410625,-31.0063330884774,126.792971231739));
#99318=CARTESIAN_POINT('Ctrl Pts',(7.38193384050032,-31.0693972319678,126.754533306255));
#99319=CARTESIAN_POINT('Ctrl Pts',(7.38592677689439,-31.1324613754582,126.716095380771));
#99320=CARTESIAN_POINT('Ctrl Pts',(7.38991971328846,-31.1934697835506,126.674241325073));
#99321=CARTESIAN_POINT('Ctrl Pts',(7.39391264968254,-31.2520409112987,126.629230222815));
#99322=CARTESIAN_POINT('Ctrl Pts',(6.69398884812234,-31.2520409112987,126.629230222815));
#99323=CARTESIAN_POINT('Ctrl Pts',(6.69784694811596,-31.3084865382694,126.585852538531));
#99324=CARTESIAN_POINT('Ctrl Pts',(6.70170504810959,-31.362733689695,126.539493117966));
#99325=CARTESIAN_POINT('Ctrl Pts',(6.70556314810321,-31.4144556013838,126.490406962616));
#99326=CARTESIAN_POINT('Ctrl Pts',(6.70941911580678,-31.4661489274686,126.441347936143));
#99327=CARTESIAN_POINT('Ctrl Pts',(6.71327508351035,-31.5153194313132,126.389565498856));
#99328=CARTESIAN_POINT('Ctrl Pts',(6.71713105121391,-31.5616745617803,126.335353932704));
#99329=CARTESIAN_POINT('Ctrl Pts',(6.72098617770107,-31.6080195794303,126.281154193327));
#99330=CARTESIAN_POINT('Ctrl Pts',(6.72484130418823,-31.6515501278902,126.224526746636));
#99331=CARTESIAN_POINT('Ctrl Pts',(6.72869643067539,-31.6920127508397,126.165800331745));
#99332=CARTESIAN_POINT('Ctrl Pts',(6.7325520057066,-31.7324800816163,126.107067084033));
#99333=CARTESIAN_POINT('Ctrl Pts',(6.73640758073781,-31.7698785047534,126.046234784751));
#99334=CARTESIAN_POINT('Ctrl Pts',(6.74026315576902,-31.8039978444562,125.983661191517));
#99335=CARTESIAN_POINT('Ctrl Pts',(6.74412294979956,-31.8381545195681,125.921019126539));
#99336=CARTESIAN_POINT('Ctrl Pts',(6.74798274383009,-31.8690247189543,125.856632392983));
#99337=CARTESIAN_POINT('Ctrl Pts',(6.75184253786063,-31.8964446593591,125.790882555433));
#99338=CARTESIAN_POINT('Ctrl Pts',(6.75570478475116,-31.9238820248582,125.725090934528));
#99339=CARTESIAN_POINT('Ctrl Pts',(6.75956703164169,-31.9478646051994,125.65793494325));
#99340=CARTESIAN_POINT('Ctrl Pts',(6.76342927853222,-31.9682780607652,125.589812714351));
#99341=CARTESIAN_POINT('Ctrl Pts',(6.76729801466201,-31.9887258144484,125.521576028388));
#99342=CARTESIAN_POINT('Ctrl Pts',(6.77116675079179,-32.0055923633275,125.452370336794));
#99343=CARTESIAN_POINT('Ctrl Pts',(6.77503548692158,-32.0188143372311,125.382604540342));
#99344=CARTESIAN_POINT('Ctrl Pts',(6.7764408316651,-32.0236173092873,125.357261639707));
#99345=CARTESIAN_POINT('Ctrl Pts',(6.77784617640862,-32.027939855963,125.331844877848));
#99346=CARTESIAN_POINT('Ctrl Pts',(6.77925152115213,-32.0317806392832,125.306373948524));
#99347=CARTESIAN_POINT('Ctrl Pts',(6.78312059450033,-32.042354751044,125.236249593445));
#99348=CARTESIAN_POINT('Ctrl Pts',(6.78698966784852,-32.0493149318718,125.1654398123));
#99349=CARTESIAN_POINT('Ctrl Pts',(6.79085874119672,-32.0525826818246,125.094349863666));
#99350=CARTESIAN_POINT('Ctrl Pts',(6.79472204959248,-32.0558455628019,125.023365839665));
#99351=CARTESIAN_POINT('Ctrl Pts',(6.79858535798824,-32.0554269116062,124.952102958125));
#99352=CARTESIAN_POINT('Ctrl Pts',(6.80244866638399,-32.0512996831102,124.880974067649));
#99353=CARTESIAN_POINT('Ctrl Pts',(6.80630744287689,-32.0471772961118,124.809928615819));
#99354=CARTESIAN_POINT('Ctrl Pts',(6.81016621936978,-32.03935500117,124.739017325457));
#99355=CARTESIAN_POINT('Ctrl Pts',(6.81402499586267,-32.027857796495,124.668653776701));
#99356=CARTESIAN_POINT('Ctrl Pts',(6.81788134145086,-32.016367834688,124.598334554711));
#99357=CARTESIAN_POINT('Ctrl Pts',(6.82173768703904,-32.0012076343702,124.528562868029));
#99358=CARTESIAN_POINT('Ctrl Pts',(6.82559403262723,-31.9824539451133,124.459746431752));
#99359=CARTESIAN_POINT('Ctrl Pts',(6.82944923887254,-31.9637057965637,124.390950327033));
#99360=CARTESIAN_POINT('Ctrl Pts',(6.83330444511785,-31.941366394467,124.323109380863));
#99361=CARTESIAN_POINT('Ctrl Pts',(6.83715965136317,-31.915563046177,124.256618685585));
#99362=CARTESIAN_POINT('Ctrl Pts',(6.84101500821439,-31.8897586898639,124.190125392809));
#99363=CARTESIAN_POINT('Ctrl Pts',(6.84487036506562,-31.8604902964996,124.124982907733));
#99364=CARTESIAN_POINT('Ctrl Pts',(6.84872572191684,-31.8279336356094,124.061567164733));
#99365=CARTESIAN_POINT('Ctrl Pts',(6.85258511438538,-31.795342895844,123.998085040933));
#99366=CARTESIAN_POINT('Ctrl Pts',(6.85644450685392,-31.7594572398407,123.936333700387));
#99367=CARTESIAN_POINT('Ctrl Pts',(6.86030389932245,-31.7204984022252,123.876664426611));
#99368=CARTESIAN_POINT('Ctrl Pts',(6.86416547692587,-31.6815175066521,123.816961368915));
#99369=CARTESIAN_POINT('Ctrl Pts',(6.86802705452929,-31.6394602522201,123.759343117253));
#99370=CARTESIAN_POINT('Ctrl Pts',(6.87188863213271,-31.5945901053088,123.704129652106));
#99371=CARTESIAN_POINT('Ctrl Pts',(6.87575696624757,-31.5496414501577,123.648819581259));
#99372=CARTESIAN_POINT('Ctrl Pts',(6.87962530036242,-31.5018704020018,123.595923058158));
#99373=CARTESIAN_POINT('Ctrl Pts',(6.88349363447727,-31.4515783840471,123.545724318615));
#99374=CARTESIAN_POINT('Ctrl Pts',(6.88579135364841,-31.4217058522598,123.515907192485));
#99375=CARTESIAN_POINT('Ctrl Pts',(6.88808907281955,-31.3909445592794,123.487041142893));
#99376=CARTESIAN_POINT('Ctrl Pts',(6.89038679199069,-31.3593629475626,123.459178810084));
#99377=CARTESIAN_POINT('Ctrl Pts',(6.89425586533899,-31.3061834408045,123.412262106491));
#99378=CARTESIAN_POINT('Ctrl Pts',(6.8981249386873,-31.2504680114071,123.368009873212));
#99379=CARTESIAN_POINT('Ctrl Pts',(6.9019940120356,-31.1925145592037,123.326707859163));
#99380=CARTESIAN_POINT('Ctrl Pts',(6.90585732043148,-31.1346474581404,123.285467385469));
#99381=CARTESIAN_POINT('Ctrl Pts',(6.90972062882735,-31.074549345882,123.247168685001));
#99382=CARTESIAN_POINT('Ctrl Pts',(6.91358393722323,-31.0125524062171,123.212058393805));
#99383=CARTESIAN_POINT('Ctrl Pts',(6.91744271371623,-30.9506281928479,123.17698928918));
#99384=CARTESIAN_POINT('Ctrl Pts',(6.92130149020923,-30.8868099971837,123.145101402743));
#99385=CARTESIAN_POINT('Ctrl Pts',(6.92516026670223,-30.8214588440452,123.116598043422));
#99386=CARTESIAN_POINT('Ctrl Pts',(6.92901661229052,-30.7561488600249,123.088112640298));
#99387=CARTESIAN_POINT('Ctrl Pts',(6.93287295787882,-30.6893082787137,123.063007727904));
#99388=CARTESIAN_POINT('Ctrl Pts',(6.93672930346711,-30.6213212655347,123.041439955607));
#99389=CARTESIAN_POINT('Ctrl Pts',(6.94058450971253,-30.5533543388642,123.019878555427));
#99390=CARTESIAN_POINT('Ctrl Pts',(6.94443971595795,-30.4842421155495,123.001852367474));
#99391=CARTESIAN_POINT('Ctrl Pts',(6.94829492220338,-30.4143855768155,122.987468719193));
#99392=CARTESIAN_POINT('Ctrl Pts',(6.95215027905471,-30.3445263090946,122.973084509006));
#99393=CARTESIAN_POINT('Ctrl Pts',(6.95600563590605,-30.2739231444744,122.962343216817));
#99394=CARTESIAN_POINT('Ctrl Pts',(6.95986099275738,-30.2029872528767,122.955301064296));
#99395=CARTESIAN_POINT('Ctrl Pts',(6.96372038522603,-30.13197710872,122.94825154036));
#99396=CARTESIAN_POINT('Ctrl Pts',(6.96757977769468,-30.0606340267332,122.944908933754));
#99397=CARTESIAN_POINT('Ctrl Pts',(6.97143917016332,-29.9893733963977,122.945277479124));
#99398=CARTESIAN_POINT('Ctrl Pts',(6.97530074776684,-29.9180724192746,122.945646233159));
#99399=CARTESIAN_POINT('Ctrl Pts',(6.97916232537037,-29.8468544719533,122.949730294191));
#99400=CARTESIAN_POINT('Ctrl Pts',(6.98302390297389,-29.776131278675,122.95748185856));
#99401=CARTESIAN_POINT('Ctrl Pts',(6.98689223708884,-29.7052843426903,122.965246985658));
#99402=CARTESIAN_POINT('Ctrl Pts',(6.9907605712038,-29.634934368697,122.976692349675));
#99403=CARTESIAN_POINT('Ctrl Pts',(6.99462890531875,-29.5654836367029,122.991718871142));
#99404=CARTESIAN_POINT('Ctrl Pts',(6.99692662448891,-29.5242311818884,123.000644347952));
#99405=CARTESIAN_POINT('Ctrl Pts',(6.99922434365908,-29.4832957357481,123.010832341508));
#99406=CARTESIAN_POINT('Ctrl Pts',(7.00152206282925,-29.4427586443768,123.022253900501));
#99407=CARTESIAN_POINT('Ctrl Pts',(7.00539113617734,-29.3744992235256,123.04148638551));
#99408=CARTESIAN_POINT('Ctrl Pts',(7.00926020952544,-29.3071029468815,123.064294522592));
#99409=CARTESIAN_POINT('Ctrl Pts',(7.01312928287354,-29.2409714547277,123.090583013074));
#99410=CARTESIAN_POINT('Ctrl Pts',(7.01699259126921,-29.1749384990637,123.11683233348));
#99411=CARTESIAN_POINT('Ctrl Pts',(7.02085589966487,-29.1101670348799,123.146551535715));
#99412=CARTESIAN_POINT('Ctrl Pts',(7.02471920806054,-29.0470444364168,123.179595304243));
#99413=CARTESIAN_POINT('Ctrl Pts',(7.02857798455334,-28.9839958847178,123.212600310359));
#99414=CARTESIAN_POINT('Ctrl Pts',(7.03243676104614,-28.9225927850117,123.248921911993));
#99415=CARTESIAN_POINT('Ctrl Pts',(7.03629553753893,-28.8632017528815,123.288367063927));
#99416=CARTESIAN_POINT('Ctrl Pts',(7.04015188312703,-28.8038481351857,123.327787366689));
#99417=CARTESIAN_POINT('Ctrl Pts',(7.04400822871512,-28.7465044740008,123.370327047668));
#99418=CARTESIAN_POINT('Ctrl Pts',(7.04786457430321,-28.6915107348119,123.415748313749));
#99419=CARTESIAN_POINT('Ctrl Pts',(7.05171978054843,-28.6365332433176,123.461156160288));
#99420=CARTESIAN_POINT('Ctrl Pts',(7.05557498679364,-28.5839046698362,123.50944359257));
#99421=CARTESIAN_POINT('Ctrl Pts',(7.05943019303886,-28.5339326626447,123.560331939355));
#99422=CARTESIAN_POINT('Ctrl Pts',(7.06328554989,-28.483958703267,123.611222274124));
#99423=CARTESIAN_POINT('Ctrl Pts',(7.06714090674115,-28.4366418550176,123.664713376969));
#99424=CARTESIAN_POINT('Ctrl Pts',(7.07099626359229,-28.3922523559684,123.720490298743));
#99425=CARTESIAN_POINT('Ctrl Pts',(7.07485565606074,-28.3478163919517,123.776325605336));
#99426=CARTESIAN_POINT('Ctrl Pts',(7.07871504852919,-28.3063141971294,123.834451126329));
#99427=CARTESIAN_POINT('Ctrl Pts',(7.08257444099764,-28.267974621548,123.894520171646));
#99428=CARTESIAN_POINT('Ctrl Pts',(7.08643601860097,-28.2296133386268,123.954623227229));
#99429=CARTESIAN_POINT('Ctrl Pts',(7.0902975962043,-28.1944184793295,124.01667157494));
#99430=CARTESIAN_POINT('Ctrl Pts',(7.09415917380763,-28.1625731861594,124.080293380322));
#99431=CARTESIAN_POINT('Ctrl Pts',(7.0980275079224,-28.1306721740293,124.144026503279));
#99432=CARTESIAN_POINT('Ctrl Pts',(7.10189584203717,-28.1021326235759,124.209338135151));
#99433=CARTESIAN_POINT('Ctrl Pts',(7.10576417615195,-28.0770894760499,124.275836565835));
#99434=CARTESIAN_POINT('Ctrl Pts',(7.1080618953239,-28.0622143079571,124.315335408115));
#99435=CARTESIAN_POINT('Ctrl Pts',(7.11035961449585,-28.0485717692979,124.355252661341));
#99436=CARTESIAN_POINT('Ctrl Pts',(7.1126573336678,-28.0361816560163,124.395504280964));
#99437=CARTESIAN_POINT('Ctrl Pts',(7.11737359945866,-28.0107498851854,124.478124184637));
#99438=CARTESIAN_POINT('Ctrl Pts',(7.12208986524952,-27.9905162579432,124.562414597922));
#99439=CARTESIAN_POINT('Ctrl Pts',(7.12680613104038,-27.9756629418137,124.647782684478));
#99440=CARTESIAN_POINT('Ctrl Pts',(7.13145774527747,-27.9610132380354,124.731980527522));
#99441=CARTESIAN_POINT('Ctrl Pts',(7.13610935951457,-27.9515973927245,124.817226707599));
#99442=CARTESIAN_POINT('Ctrl Pts',(7.14076097375166,-27.9475440844172,124.902931585522));
#99443=CARTESIAN_POINT('Ctrl Pts',(7.14248240933492,-27.9460440655433,124.934648623736));
#99444=CARTESIAN_POINT('Ctrl Pts',(7.14420384491818,-27.9452780035317,124.966428274276));
#99445=CARTESIAN_POINT('Ctrl Pts',(7.14592528050144,-27.9452507538412,124.998239912027));
#99446=CARTESIAN_POINT('Origin',(-1.54592528053767,-30.,125.));
#99447=CARTESIAN_POINT('',(5.99388605066143,-31.2520409112987,126.629230222815));
#99448=CARTESIAN_POINT('',(6.05208070748271,-31.2520409112987,126.629230222815));
#99449=CARTESIAN_POINT('',(-1.54592528053767,-31.2520409112987,126.629230222815));
#99450=CARTESIAN_POINT('',(6.50407471951103,-27.9452500572952,125.000485236462));
#99451=CARTESIAN_POINT('Ctrl Pts',(6.05208070748271,-31.2520409112986,126.629230222815));
#99452=CARTESIAN_POINT('Ctrl Pts',(6.05593584186157,-31.3085914830148,126.585771889945));
#99453=CARTESIAN_POINT('Ctrl Pts',(6.05979097624043,-31.3628817184085,126.539361992874));
#99454=CARTESIAN_POINT('Ctrl Pts',(6.06364611061928,-31.4145976995229,126.490272092943));
#99455=CARTESIAN_POINT('Ctrl Pts',(6.06753106145521,-31.4667136634081,126.44080252093));
#99456=CARTESIAN_POINT('Ctrl Pts',(6.07141601229114,-31.5162150021348,126.388611638529));
#99457=CARTESIAN_POINT('Ctrl Pts',(6.07530096312706,-31.5628183594721,126.334015119029));
#99458=CARTESIAN_POINT('Ctrl Pts',(6.07916147816606,-31.6091285882156,126.279762003993));
#99459=CARTESIAN_POINT('Ctrl Pts',(6.08302199320507,-31.6525769339782,126.223133852219));
#99460=CARTESIAN_POINT('Ctrl Pts',(6.08688250824407,-31.6929272985205,126.16447186502));
#99461=CARTESIAN_POINT('Ctrl Pts',(6.09077967697846,-31.7336607699686,126.105252911047));
#99462=CARTESIAN_POINT('Ctrl Pts',(6.09467684571285,-31.7712368521271,126.043961724892));
#99463=CARTESIAN_POINT('Ctrl Pts',(6.09857401444724,-31.8054598091433,125.980975249468));
#99464=CARTESIAN_POINT('Ctrl Pts',(6.10247118318163,-31.8396827661595,125.917988774043));
#99465=CARTESIAN_POINT('Ctrl Pts',(6.10636835191603,-31.8705524401511,125.853307490443));
#99466=CARTESIAN_POINT('Ctrl Pts',(6.11026552065042,-31.8979233773648,125.787327388163));
#99467=CARTESIAN_POINT('Ctrl Pts',(6.11413459399864,-31.9250969925986,125.721822948238));
#99468=CARTESIAN_POINT('Ctrl Pts',(6.11800366734686,-31.9489286475829,125.654781756097));
#99469=CARTESIAN_POINT('Ctrl Pts',(6.12187274069508,-31.9692444247995,125.586578177139));
#99470=CARTESIAN_POINT('Ctrl Pts',(6.12573604909087,-31.9895299313342,125.518476222098));
#99471=CARTESIAN_POINT('Ctrl Pts',(6.12959935748666,-32.0063098212002,125.449215779922));
#99472=CARTESIAN_POINT('Ctrl Pts',(6.13346266588246,-32.0194582824914,125.37919099116));
#99473=CARTESIAN_POINT('Ctrl Pts',(6.13732144237538,-32.0325913198134,125.309248345864));
#99474=CARTESIAN_POINT('Ctrl Pts',(6.1411802188683,-32.0421013009361,125.238543610109));
#99475=CARTESIAN_POINT('Ctrl Pts',(6.14503899536122,-32.0479127447517,125.167484185473));
#99476=CARTESIAN_POINT('Ctrl Pts',(6.14889534094943,-32.0537205275452,125.096469525981));
#99477=CARTESIAN_POINT('Ctrl Pts',(6.15275168653764,-32.0558343561298,125.025101103938));
#99478=CARTESIAN_POINT('Ctrl Pts',(6.15660803212585,-32.0542303877085,124.95379310966));
#99479=CARTESIAN_POINT('Ctrl Pts',(6.16046323837119,-32.0526268931737,124.882506183062));
#99480=CARTESIAN_POINT('Ctrl Pts',(6.16431844461653,-32.0473077931976,124.811280134183));
#99481=CARTESIAN_POINT('Ctrl Pts',(6.16817365086187,-32.0383013546744,124.740529095981));
#99482=CARTESIAN_POINT('Ctrl Pts',(6.17202900771313,-32.0292945643094,124.669775293847));
#99483=CARTESIAN_POINT('Ctrl Pts',(6.1758843645644,-32.016600212938,124.599497020851));
#99484=CARTESIAN_POINT('Ctrl Pts',(6.17973972141566,-32.0002982194614,124.530101504876));
#99485=CARTESIAN_POINT('Ctrl Pts',(6.18359911388422,-31.983979161778,124.46063334874));
#99486=CARTESIAN_POINT('Ctrl Pts',(6.18745850635279,-31.9640450349266,124.39205026808));
#99487=CARTESIAN_POINT('Ctrl Pts',(6.19131789882135,-31.9406263111467,124.32474665274));
#99488=CARTESIAN_POINT('Ctrl Pts',(6.1951794764248,-31.9171943280077,124.25740493102));
#99489=CARTESIAN_POINT('Ctrl Pts',(6.19904105402824,-31.890274003856,124.191344566788));
#99490=CARTESIAN_POINT('Ctrl Pts',(6.20290263163169,-31.8600438601533,124.126939635073));
#99491=CARTESIAN_POINT('Ctrl Pts',(6.20677096574656,-31.8297608234797,124.062422015566));
#99492=CARTESIAN_POINT('Ctrl Pts',(6.21063929986144,-31.7961566342371,123.999566040007));
#99493=CARTESIAN_POINT('Ctrl Pts',(6.21450763397632,-31.7594552707739,123.938720247698));
#99494=CARTESIAN_POINT('Ctrl Pts',(6.21680535314721,-31.7376553372826,123.902578968454));
#99495=CARTESIAN_POINT('Ctrl Pts',(6.21910307231809,-31.7147635080566,123.867146354675));
#99496=CARTESIAN_POINT('Ctrl Pts',(6.22140079148898,-31.6908335103589,123.832489998866));
#99497=CARTESIAN_POINT('Ctrl Pts',(6.22526986483719,-31.650538370079,123.774133005415));
#99498=CARTESIAN_POINT('Ctrl Pts',(6.2291389381854,-31.60713957811,123.717750259131));
#99499=CARTESIAN_POINT('Ctrl Pts',(6.23300801153361,-31.5608573285145,123.663690918042));
#99500=CARTESIAN_POINT('Ctrl Pts',(6.23687131992939,-31.5146440398673,123.609712125835));
#99501=CARTESIAN_POINT('Ctrl Pts',(6.24073462832518,-31.4655561351378,123.558050233075));
#99502=CARTESIAN_POINT('Ctrl Pts',(6.24459793672096,-31.4138565131096,123.509024707503));
#99503=CARTESIAN_POINT('Ctrl Pts',(6.24845671321387,-31.3622175379782,123.460056691944));
#99504=CARTESIAN_POINT('Ctrl Pts',(6.25231548970678,-31.3079732818954,123.41371923322));
#99505=CARTESIAN_POINT('Ctrl Pts',(6.25617426619968,-31.2514250824289,123.370296706278));
#99506=CARTESIAN_POINT('Ctrl Pts',(6.26003061178788,-31.1949125065039,123.326901534128));
#99507=CARTESIAN_POINT('Ctrl Pts',(6.26388695737608,-31.1360992511542,123.286417945709));
#99508=CARTESIAN_POINT('Ctrl Pts',(6.26774330296428,-31.0753203642286,123.249090614345));
#99509=CARTESIAN_POINT('Ctrl Pts',(6.27159850920961,-31.0145594341977,123.211774311201));
#99510=CARTESIAN_POINT('Ctrl Pts',(6.27545371545494,-30.9518344392437,123.177612667924));
#99511=CARTESIAN_POINT('Ctrl Pts',(6.27930892170026,-30.887508641451,123.146806547106));
#99512=CARTESIAN_POINT('Ctrl Pts',(6.2831642785515,-30.8231803307329,123.115999222828));
#99513=CARTESIAN_POINT('Ctrl Pts',(6.28701963540274,-30.7572515321037,123.088547889102));
#99514=CARTESIAN_POINT('Ctrl Pts',(6.29087499225398,-30.6901077205889,123.064606268357));
#99515=CARTESIAN_POINT('Ctrl Pts',(6.29473438472254,-30.622893625897,123.04063958658));
#99516=CARTESIAN_POINT('Ctrl Pts',(6.29859377719109,-30.5544624379827,123.020190115029));
#99517=CARTESIAN_POINT('Ctrl Pts',(6.30245316965964,-30.4852162643888,123.00336214118));
#99518=CARTESIAN_POINT('Ctrl Pts',(6.30631474726306,-30.415930884565,122.986524639564));
#99519=CARTESIAN_POINT('Ctrl Pts',(6.31017632486648,-30.3458300780973,122.973312807461));
#99520=CARTESIAN_POINT('Ctrl Pts',(6.31403790246991,-30.2753249453426,122.963779546078));
#99521=CARTESIAN_POINT('Ctrl Pts',(6.31790623658477,-30.2046964514165,122.954229604571));
#99522=CARTESIAN_POINT('Ctrl Pts',(6.32177457069963,-30.1336627030745,122.948371124002));
#99523=CARTESIAN_POINT('Ctrl Pts',(6.3256429048145,-30.0626380011782,122.946204965604));
#99524=CARTESIAN_POINT('Ctrl Pts',(6.32794062398551,-30.0204506372337,122.944918307438));
#99525=CARTESIAN_POINT('Ctrl Pts',(6.33023834315652,-29.9782664489834,122.944933353137));
#99526=CARTESIAN_POINT('Ctrl Pts',(6.33253606232753,-29.9361713635724,122.946241623834));
#99527=CARTESIAN_POINT('Ctrl Pts',(6.33640513567575,-29.8652884745277,122.948444588996));
#99528=CARTESIAN_POINT('Ctrl Pts',(6.34027420902398,-29.7943809273128,122.954325827891));
#99529=CARTESIAN_POINT('Ctrl Pts',(6.3441432823722,-29.7238614901485,122.963889716671));
#99530=CARTESIAN_POINT('Ctrl Pts',(6.34800659076799,-29.6534471275495,122.973439355175));
#99531=CARTESIAN_POINT('Ctrl Pts',(6.35186989916379,-29.5834202045742,122.986660686914));
#99532=CARTESIAN_POINT('Ctrl Pts',(6.35573320755959,-29.5141917068454,123.003506106996));
#99533=CARTESIAN_POINT('Ctrl Pts',(6.35959198405251,-29.4450444184832,123.020331766345));
#99534=CARTESIAN_POINT('Ctrl Pts',(6.36345076054543,-29.3766941646795,123.040772955254));
#99535=CARTESIAN_POINT('Ctrl Pts',(6.36730953703836,-29.3095432958903,123.064730741667));
#99536=CARTESIAN_POINT('Ctrl Pts',(6.37116588262657,-29.2424347299823,123.088673435447));
#99537=CARTESIAN_POINT('Ctrl Pts',(6.37502222821478,-29.176524506499,123.116128168673));
#99538=CARTESIAN_POINT('Ctrl Pts',(6.37887857380299,-29.1121999040778,123.146946155078));
#99539=CARTESIAN_POINT('Ctrl Pts',(6.38273378004833,-29.0478943061196,123.177755036424));
#99540=CARTESIAN_POINT('Ctrl Pts',(6.38658898629367,-28.9851738370512,123.211924988476));
#99541=CARTESIAN_POINT('Ctrl Pts',(6.39044419253901,-28.9244042705948,123.249259759592));
#99542=CARTESIAN_POINT('Ctrl Pts',(6.39429954939025,-28.8636323301393,123.286595989212));
#99543=CARTESIAN_POINT('Ctrl Pts',(6.3981549062415,-28.8048118563657,123.327097027188));
#99544=CARTESIAN_POINT('Ctrl Pts',(6.40201026309274,-28.7482810659924,123.370522392683));
#99545=CARTESIAN_POINT('Ctrl Pts',(6.40586965556131,-28.6916911016837,123.413993213934));
#99546=CARTESIAN_POINT('Ctrl Pts',(6.40972904802988,-28.6373959912379,123.460394176724));
#99547=CARTESIAN_POINT('Ctrl Pts',(6.41358844049845,-28.5857014397953,123.509444014771));
#99548=CARTESIAN_POINT('Ctrl Pts',(6.4174500181019,-28.5339776196093,123.558521624161));
#99549=CARTESIAN_POINT('Ctrl Pts',(6.42131159570535,-28.4848576241844,123.610250741923));
#99550=CARTESIAN_POINT('Ctrl Pts',(6.42517317330881,-28.4386088641965,123.664314676455));
#99551=CARTESIAN_POINT('Ctrl Pts',(6.42904150742369,-28.392279183842,123.71847320538));
#99552=CARTESIAN_POINT('Ctrl Pts',(6.43290984153857,-28.3488310651752,123.774974322028));
#99553=CARTESIAN_POINT('Ctrl Pts',(6.43677817565345,-28.3084899336634,123.8334704213));
#99554=CARTESIAN_POINT('Ctrl Pts',(6.43907589482433,-28.284528045032,123.868216026185));
#99555=CARTESIAN_POINT('Ctrl Pts',(6.44137361399521,-28.2616614969002,123.903664960458));
#99556=CARTESIAN_POINT('Ctrl Pts',(6.44367133316609,-28.2399297695999,123.939740434347));
#99557=CARTESIAN_POINT('Ctrl Pts',(6.44766818401098,-28.2021277293325,124.002493224209));
#99558=CARTESIAN_POINT('Ctrl Pts',(6.45166503485587,-28.167621995408,124.067375195747));
#99559=CARTESIAN_POINT('Ctrl Pts',(6.45566188570075,-28.1366498578013,124.13401858561));
#99560=CARTESIAN_POINT('Ctrl Pts',(6.45969628851421,-28.1053867249128,124.201288116048));
#99561=CARTESIAN_POINT('Ctrl Pts',(6.46373069132768,-28.0777242453421,124.270351994449));
#99562=CARTESIAN_POINT('Ctrl Pts',(6.46776509414114,-28.0538611856038,124.340802550369));
#99563=CARTESIAN_POINT('Ctrl Pts',(6.47174648699997,-28.0303116740591,124.410327422625));
#99564=CARTESIAN_POINT('Ctrl Pts',(6.47572787985879,-28.0104625063912,124.481202326663));
#99565=CARTESIAN_POINT('Ctrl Pts',(6.47970927271762,-27.9944576731882,124.553012821362));
#99566=CARTESIAN_POINT('Ctrl Pts',(6.48377018050841,-27.9781331972702,124.626257489177));
#99567=CARTESIAN_POINT('Ctrl Pts',(6.48783108829919,-27.9658084880444,124.700475103802));
#99568=CARTESIAN_POINT('Ctrl Pts',(6.49189199608997,-27.9575832299834,124.775208318537));
#99569=CARTESIAN_POINT('Ctrl Pts',(6.49595290388076,-27.9493579719225,124.849941533272));
#99570=CARTESIAN_POINT('Ctrl Pts',(6.50001381167155,-27.9452322760607,124.9251898674));
#99571=CARTESIAN_POINT('Ctrl Pts',(6.50407471946233,-27.9452500572949,125.000485235559));
#99572=CARTESIAN_POINT('Ctrl Pts',(6.50407471951103,-27.9452500572952,125.000485236462));
#99573=CARTESIAN_POINT('Ctrl Pts',(6.50830237655216,-27.945268568698,125.078872387749));
#99574=CARTESIAN_POINT('Ctrl Pts',(6.5125300335933,-27.9497773969991,125.157140435482));
#99575=CARTESIAN_POINT('Ctrl Pts',(6.51675769063443,-27.9587077544997,125.234784009167));
#99576=CARTESIAN_POINT('Ctrl Pts',(6.52089243721856,-27.9674418511427,125.310721224023));
#99577=CARTESIAN_POINT('Ctrl Pts',(6.52502718380269,-27.9804049307438,125.386060793662));
#99578=CARTESIAN_POINT('Ctrl Pts',(6.52916193038682,-27.9974813727944,125.460344121494));
#99579=CARTESIAN_POINT('Ctrl Pts',(6.53343604265646,-28.0151333930585,125.537131241686));
#99580=CARTESIAN_POINT('Ctrl Pts',(6.5377101549261,-28.0371808331556,125.612789222111));
#99581=CARTESIAN_POINT('Ctrl Pts',(6.54198426719574,-28.0634417891516,125.686833210099));
#99582=CARTESIAN_POINT('Ctrl Pts',(6.54625837946537,-28.0897027451476,125.760877198088));
#99583=CARTESIAN_POINT('Ctrl Pts',(6.55053249173501,-28.1201769686497,125.833306828919));
#99584=CARTESIAN_POINT('Ctrl Pts',(6.55480660400465,-28.1546308748033,125.903664956868));
#99585=CARTESIAN_POINT('Ctrl Pts',(6.55867567735284,-28.1858197349993,125.967355552833));
#99586=CARTESIAN_POINT('Ctrl Pts',(6.56254475070102,-28.2203708581139,126.029554339914));
#99587=CARTESIAN_POINT('Ctrl Pts',(6.56641382404921,-28.2581183028438,126.089883349544));
#99588=CARTESIAN_POINT('Ctrl Pts',(6.57027713244497,-28.2958095035577,126.150122468432));
#99589=CARTESIAN_POINT('Ctrl Pts',(6.57414044084073,-28.3366873167936,126.208496931506));
#99590=CARTESIAN_POINT('Ctrl Pts',(6.57800374923648,-28.3805391633647,126.26465179441));
#99591=CARTESIAN_POINT('Ctrl Pts',(6.58186252572937,-28.4243395689715,126.32074078414));
#99592=CARTESIAN_POINT('Ctrl Pts',(6.58572130222225,-28.4711067805815,126.374614964572));
#99593=CARTESIAN_POINT('Ctrl Pts',(6.58958007871514,-28.5205849981015,126.425948391302));
#99594=CARTESIAN_POINT('Ctrl Pts',(6.59343642430332,-28.5700320459406,126.47724947963));
#99595=CARTESIAN_POINT('Ctrl Pts',(6.5972927698915,-28.6221863750233,126.526012640869));
#99596=CARTESIAN_POINT('Ctrl Pts',(6.60114911547968,-28.6767529565507,126.571946190079));
#99597=CARTESIAN_POINT('Ctrl Pts',(6.60500432172498,-28.7313034165857,126.617866168393));
#99598=CARTESIAN_POINT('Ctrl Pts',(6.60885952797029,-28.7882643427381,126.660957881694));
#99599=CARTESIAN_POINT('Ctrl Pts',(6.6127147342156,-28.8473063029079,126.700968783718));
#99600=CARTESIAN_POINT('Ctrl Pts',(6.61657009106682,-28.9063505695867,126.740981248792));
#99601=CARTESIAN_POINT('Ctrl Pts',(6.62042544791804,-28.9674756283068,126.777912392945));
#99602=CARTESIAN_POINT('Ctrl Pts',(6.62428080476926,-29.0303230844278,126.811552991747));
#99603=CARTESIAN_POINT('Ctrl Pts',(6.62814019723779,-29.0932363264908,126.845228804042));
#99604=CARTESIAN_POINT('Ctrl Pts',(6.63199958970633,-29.1578751358405,126.875606965472));
#99605=CARTESIAN_POINT('Ctrl Pts',(6.63585898217486,-29.2238573333875,126.902524670947));
#99606=CARTESIAN_POINT('Ctrl Pts',(6.63972055977826,-29.2898768891462,126.929457616857));
#99607=CARTESIAN_POINT('Ctrl Pts',(6.64358213738167,-29.3572408882763,126.952926046632));
#99608=CARTESIAN_POINT('Ctrl Pts',(6.64744371498507,-29.4255506327794,126.972816637957));
#99609=CARTESIAN_POINT('Ctrl Pts',(6.65131204909992,-29.4939798972346,126.992742031381));
#99610=CARTESIAN_POINT('Ctrl Pts',(6.65518038321476,-29.5633577378097,127.009076976597));
#99611=CARTESIAN_POINT('Ctrl Pts',(6.65904871732961,-29.6332745687623,127.021759140101));
#99612=CARTESIAN_POINT('Ctrl Pts',(6.66134643650081,-29.6748038777878,127.029292111492));
#99613=CARTESIAN_POINT('Ctrl Pts',(6.66364415567202,-29.7165232177419,127.035537320761));
#99614=CARTESIAN_POINT('Ctrl Pts',(6.66594187484322,-29.758346354646,127.040490401395));
#99615=CARTESIAN_POINT('Ctrl Pts',(6.66980984684839,-29.8287512695462,127.048828399126));
#99616=CARTESIAN_POINT('Ctrl Pts',(6.67367781885357,-29.899726096376,127.053534580682));
#99617=CARTESIAN_POINT('Ctrl Pts',(6.67754579085874,-29.9708636361224,127.054543412732));
#99618=CARTESIAN_POINT('Ctrl Pts',(6.6814084950816,-30.0419042938144,127.055550870856));
#99619=CARTESIAN_POINT('Ctrl Pts',(6.68527119930445,-30.1131067436655,127.052870960964));
#99620=CARTESIAN_POINT('Ctrl Pts',(6.6891339035273,-30.1840576815714,127.046489758673));
#99621=CARTESIAN_POINT('Ctrl Pts',(6.69299263972177,-30.2549357339238,127.040115111581));
#99622=CARTESIAN_POINT('Ctrl Pts',(6.69685137591624,-30.3255623057803,127.030046760409));
#99623=CARTESIAN_POINT('Ctrl Pts',(6.70071011211071,-30.3955248317993,127.016322808959));
#99624=CARTESIAN_POINT('Ctrl Pts',(6.70456617537594,-30.4654388950907,127.00260836403));
#99625=CARTESIAN_POINT('Ctrl Pts',(6.70842223864117,-30.534689350379,126.985243439873));
#99626=CARTESIAN_POINT('Ctrl Pts',(6.7122783019064,-30.6028712112944,126.964317658907));
#99627=CARTESIAN_POINT('Ctrl Pts',(6.71613400852211,-30.67104676603,126.943393813378));
#99628=CARTESIAN_POINT('Ctrl Pts',(6.71998971513781,-30.7381534547125,126.918909895311));
#99629=CARTESIAN_POINT('Ctrl Pts',(6.72384542175351,-30.8038002699191,126.891005734676));
#99630=CARTESIAN_POINT('Ctrl Pts',(6.72770090156707,-30.8694432236187,126.863103215432));
#99631=CARTESIAN_POINT('Ctrl Pts',(6.73155638138064,-30.9336260304061,126.831781050833));
#99632=CARTESIAN_POINT('Ctrl Pts',(6.7354118611942,-30.9959784867921,126.797226868358));
#99633=CARTESIAN_POINT('Ctrl Pts',(6.73927005804643,-31.058374884281,126.762648334815));
#99634=CARTESIAN_POINT('Ctrl Pts',(6.74312825489866,-31.1189379361233,126.72483348097));
#99635=CARTESIAN_POINT('Ctrl Pts',(6.74698645175089,-31.1773238863171,126.684014854212));
#99636=CARTESIAN_POINT('Ctrl Pts',(6.74865985625706,-31.2026474547853,126.666310709875));
#99637=CARTESIAN_POINT('Ctrl Pts',(6.75033326076323,-31.227561851962,126.64804204163));
#99638=CARTESIAN_POINT('Ctrl Pts',(6.75200666526939,-31.2520409112987,126.629230222815));
#99639=CARTESIAN_POINT('',(6.44592528055971,-27.9452500000201,124.999990915848));
#99640=CARTESIAN_POINT('Ctrl Pts',(6.44592528055971,-27.9452500000201,124.999990915848));
#99641=CARTESIAN_POINT('Ctrl Pts',(6.44979385262029,-27.9452496865326,125.070898847849));
#99642=CARTESIAN_POINT('Ctrl Pts',(6.45366242468087,-27.9489241543595,125.141945865788));
#99643=CARTESIAN_POINT('Ctrl Pts',(6.45753099674145,-27.9562906465005,125.212719629838));
#99644=CARTESIAN_POINT('Ctrl Pts',(6.46139380425482,-27.9636461618544,125.283387934122));
#99645=CARTESIAN_POINT('Ctrl Pts',(6.4652566117682,-27.9746827314373,125.353783313364));
#99646=CARTESIAN_POINT('Ctrl Pts',(6.46911941928157,-27.9893655868602,125.423493588143));
#99647=CARTESIAN_POINT('Ctrl Pts',(6.47297769673217,-28.0040312231345,125.493122111004));
#99648=CARTESIAN_POINT('Ctrl Pts',(6.47683597418277,-28.0223345517855,125.562066652123));
#99649=CARTESIAN_POINT('Ctrl Pts',(6.48069425163337,-28.0441892330749,125.629922063814));
#99650=CARTESIAN_POINT('Ctrl Pts',(6.48455010013137,-28.0660301558968,125.697734757588));
#99651=CARTESIAN_POINT('Ctrl Pts',(6.48840594862937,-28.0914178471182,125.764459220811));
#99652=CARTESIAN_POINT('Ctrl Pts',(6.49226179712736,-28.1202156679157,125.829703819053));
#99653=CARTESIAN_POINT('Ctrl Pts',(6.49611650899254,-28.1490049996483,125.894929184393));
#99654=CARTESIAN_POINT('Ctrl Pts',(6.49997122085771,-28.1812022691669,125.958675106488));
#99655=CARTESIAN_POINT('Ctrl Pts',(6.50382593272288,-28.2166227268674,126.020569970249));
#99656=CARTESIAN_POINT('Ctrl Pts',(6.50768079866415,-28.2520446003537,126.082467308));
#99657=CARTESIAN_POINT('Ctrl Pts',(6.51153566460542,-28.2906896745233,126.142513019873));
#99658=CARTESIAN_POINT('Ctrl Pts',(6.51539053054669,-28.3323281365673,126.200361661507));
#99659=CARTESIAN_POINT('Ctrl Pts',(6.51924943299407,-28.3740101990655,126.258270877593));
#99660=CARTESIAN_POINT('Ctrl Pts',(6.52310833544145,-28.4186916219396,126.313978035802));
#99661=CARTESIAN_POINT('Ctrl Pts',(6.52696723788883,-28.4661008194988,126.367168923929));
#99662=CARTESIAN_POINT('Ctrl Pts',(6.53082833003249,-28.5135369189414,126.420389994704));
#99663=CARTESIAN_POINT('Ctrl Pts',(6.53468942217615,-28.5637035323654,126.471091607504));
#99664=CARTESIAN_POINT('Ctrl Pts',(6.53855051431981,-28.6162924803377,126.51899672894));
#99665=CARTESIAN_POINT('Ctrl Pts',(6.5424183550777,-28.6689733459616,126.566985581396));
#99666=CARTESIAN_POINT('Ctrl Pts',(6.54628619583559,-28.7240846231536,126.612167875776));
#99667=CARTESIAN_POINT('Ctrl Pts',(6.55015403659347,-28.7812859393698,126.654307589574));
#99668=CARTESIAN_POINT('Ctrl Pts',(6.55242968422065,-28.8149403857824,126.679100528508));
#99669=CARTESIAN_POINT('Ctrl Pts',(6.55470533184783,-28.8493177651018,126.702841082516));
#99670=CARTESIAN_POINT('Ctrl Pts',(6.556980979475,-28.884344705424,126.725488576081));
#99671=CARTESIAN_POINT('Ctrl Pts',(6.56085005282323,-28.9438977749115,126.763994016338));
#99672=CARTESIAN_POINT('Ctrl Pts',(6.56471912617145,-29.0055632836948,126.799488160214));
#99673=CARTESIAN_POINT('Ctrl Pts',(6.56858819951967,-29.0690042255794,126.831732630738));
#99674=CARTESIAN_POINT('Ctrl Pts',(6.57245150791546,-29.1323506399171,126.863929056725));
#99675=CARTESIAN_POINT('Ctrl Pts',(6.57631481631125,-29.1974668067587,126.892885202362));
#99676=CARTESIAN_POINT('Ctrl Pts',(6.58017812470704,-29.2639876198692,126.918406458182));
#99677=CARTESIAN_POINT('Ctrl Pts',(6.58403690119997,-29.3304303998971,126.943897775969));
#99678=CARTESIAN_POINT('Ctrl Pts',(6.58789567769289,-29.3982741018786,126.965962034409));
#99679=CARTESIAN_POINT('Ctrl Pts',(6.59175445418582,-29.4671315275843,126.984451751393));
#99680=CARTESIAN_POINT('Ctrl Pts',(6.59561079977403,-29.535945575333,127.002929820451));
#99681=CARTESIAN_POINT('Ctrl Pts',(6.59946714536224,-29.6057716117509,127.017837689994));
#99682=CARTESIAN_POINT('Ctrl Pts',(6.60332349095046,-29.6762064784574,127.029077454881));
#99683=CARTESIAN_POINT('Ctrl Pts',(6.6071786971958,-29.7466205354462,127.040313899022));
#99684=CARTESIAN_POINT('Ctrl Pts',(6.61103390344114,-29.8176425861638,127.047884313495));
#99685=CARTESIAN_POINT('Ctrl Pts',(6.61488910968649,-29.8888601619396,127.051742064416));
#99686=CARTESIAN_POINT('Ctrl Pts',(6.61874446653774,-29.9600805198723,127.055599966043));
#99687=CARTESIAN_POINT('Ctrl Pts',(6.622599823389,-30.0314959328342,127.055744892087));
#99688=CARTESIAN_POINT('Ctrl Pts',(6.62645518024026,-30.1026914403144,127.052182260567));
#99689=CARTESIAN_POINT('Ctrl Pts',(6.63031457270883,-30.1739614721079,127.048615899841));
#99690=CARTESIAN_POINT('Ctrl Pts',(6.6341739651774,-30.245010652741,127.041334258715));
#99691=CARTESIAN_POINT('Ctrl Pts',(6.63803335764597,-30.315427563682,127.030394792785));
#99692=CARTESIAN_POINT('Ctrl Pts',(6.64189493524942,-30.3858843437084,127.01944913308));
#99693=CARTESIAN_POINT('Ctrl Pts',(6.64575651285287,-30.455707665693,127.004841625352));
#99694=CARTESIAN_POINT('Ctrl Pts',(6.64961809045631,-30.5244974581908,126.986680643398));
#99695=CARTESIAN_POINT('Ctrl Pts',(6.6534864245712,-30.5934076105692,126.9684878856));
#99696=CARTESIAN_POINT('Ctrl Pts',(6.65735475868608,-30.6612801603096,126.946729388642));
#99697=CARTESIAN_POINT('Ctrl Pts',(6.66122309280097,-30.7277319849047,126.921562832865));
#99698=CARTESIAN_POINT('Ctrl Pts',(6.66352081197183,-30.7672031440075,126.906614362552));
#99699=CARTESIAN_POINT('Ctrl Pts',(6.6658185311427,-30.8061734483555,126.890464398357));
#99700=CARTESIAN_POINT('Ctrl Pts',(6.66811625031357,-30.8445667488954,126.8731536427));
#99701=CARTESIAN_POINT('Ctrl Pts',(6.67198550524012,-30.9092193266097,126.844003114883));
#99702=CARTESIAN_POINT('Ctrl Pts',(6.67585476016666,-30.9724875642114,126.81144429552));
#99703=CARTESIAN_POINT('Ctrl Pts',(6.6797240150932,-31.0339883572384,126.775631053906));
#99704=CARTESIAN_POINT('Ctrl Pts',(6.68358710221264,-31.0953911145877,126.739874900587));
#99705=CARTESIAN_POINT('Ctrl Pts',(6.68745018933207,-31.1550316060579,126.70087486984));
#99706=CARTESIAN_POINT('Ctrl Pts',(6.6913132764515,-31.212548373772,126.658832120428));
#99707=CARTESIAN_POINT('Ctrl Pts',(6.69220513367511,-31.2258270659627,126.649125859967));
#99708=CARTESIAN_POINT('Ctrl Pts',(6.69309699089873,-31.2389926646906,126.639257620015));
#99709=CARTESIAN_POINT('Ctrl Pts',(6.69398884812234,-31.2520409112987,126.629230222815));
#99710=CARTESIAN_POINT('Ctrl Pts',(5.99388605066143,-31.2520409112987,126.629230222815));
#99711=CARTESIAN_POINT('Ctrl Pts',(5.99635890886836,-31.2880636491292,126.601547246604));
#99712=CARTESIAN_POINT('Ctrl Pts',(5.99883176707529,-31.323128886047,126.572698928905));
#99713=CARTESIAN_POINT('Ctrl Pts',(6.00130462528221,-31.3571605423516,126.542761428343));
#99714=CARTESIAN_POINT('Ctrl Pts',(6.00517369863043,-31.4104070139993,126.495920737999));
#99715=CARTESIAN_POINT('Ctrl Pts',(6.00904277197865,-31.4613299633522,126.446228460409));
#99716=CARTESIAN_POINT('Ctrl Pts',(6.01291184532687,-31.5096083664831,126.393944095846));
#99717=CARTESIAN_POINT('Ctrl Pts',(6.01677515372265,-31.5578148343798,126.341737635435));
#99718=CARTESIAN_POINT('Ctrl Pts',(6.02063846211844,-31.6033842507583,126.286947108469));
#99719=CARTESIAN_POINT('Ctrl Pts',(6.02450177051423,-31.6460300705184,126.229870956422));
#99720=CARTESIAN_POINT('Ctrl Pts',(6.02836054700715,-31.6886258640592,126.172861758278));
#99721=CARTESIAN_POINT('Ctrl Pts',(6.03221932350006,-31.7283045838958,126.113572648054));
#99722=CARTESIAN_POINT('Ctrl Pts',(6.03607809999298,-31.7648190305381,126.05233614019));
#99723=CARTESIAN_POINT('Ctrl Pts',(6.03993444558119,-31.801310474257,125.991138209351));
#99724=CARTESIAN_POINT('Ctrl Pts',(6.04379079116939,-31.8346413514289,125.927995731073));
#99725=CARTESIAN_POINT('Ctrl Pts',(6.0476471367576,-31.8646078326565,125.863270057917));
#99726=CARTESIAN_POINT('Ctrl Pts',(6.05150234300294,-31.8945654603994,125.798563507719));
#99727=CARTESIAN_POINT('Ctrl Pts',(6.05535754924827,-31.9211604615756,125.732275131846));
#99728=CARTESIAN_POINT('Ctrl Pts',(6.05921275549361,-31.9442358153368,125.664789182269));
#99729=CARTESIAN_POINT('Ctrl Pts',(6.06306811234486,-31.9673120705504,125.597300596313));
#99730=CARTESIAN_POINT('Ctrl Pts',(6.06692346919611,-31.9868682502805,125.52861480414));
#99731=CARTESIAN_POINT('Ctrl Pts',(6.07077882604736,-32.0027967472953,125.459132607776));
#99732=CARTESIAN_POINT('Ctrl Pts',(6.07463821851592,-32.0187419175574,125.389577680518));
#99733=CARTESIAN_POINT('Ctrl Pts',(6.07849761098448,-32.0310517160729,125.319225159407));
#99734=CARTESIAN_POINT('Ctrl Pts',(6.08235700345304,-32.0396695759424,125.248486586107));
#99735=CARTESIAN_POINT('Ctrl Pts',(6.08621858105648,-32.0482923151254,125.1777079616));
#99736=CARTESIAN_POINT('Ctrl Pts',(6.09008015865992,-32.0532189209048,125.10654333464));
#99737=CARTESIAN_POINT('Ctrl Pts',(6.09394173626336,-32.0544449115845,125.035407171092));
#99738=CARTESIAN_POINT('Ctrl Pts',(6.09781007037823,-32.0556730473512,124.964146542274));
#99739=CARTESIAN_POINT('Ctrl Pts',(6.10167840449311,-32.0531876576792,124.892914961944));
#99740=CARTESIAN_POINT('Ctrl Pts',(6.10554673860798,-32.0470363181878,124.822123991162));
#99741=CARTESIAN_POINT('Ctrl Pts',(6.10784445777891,-32.043382535899,124.780075459194));
#99742=CARTESIAN_POINT('Ctrl Pts',(6.11014217694984,-32.0384363455578,124.738182247743));
#99743=CARTESIAN_POINT('Ctrl Pts',(6.11243989612077,-32.0322162126119,124.696528703668));
#99744=CARTESIAN_POINT('Ctrl Pts',(6.11630896946898,-32.0217422822432,124.626389315323));
#99745=CARTESIAN_POINT('Ctrl Pts',(6.1201780428172,-32.0076124141733,124.556655420757));
#99746=CARTESIAN_POINT('Ctrl Pts',(6.12404711616541,-31.9898705140382,124.487737469786));
#99747=CARTESIAN_POINT('Ctrl Pts',(6.12791042456119,-31.9721550494862,124.418922207151));
#99748=CARTESIAN_POINT('Ctrl Pts',(6.13177373295697,-31.9508383560286,124.350920941469));
#99749=CARTESIAN_POINT('Ctrl Pts',(6.13563704135276,-31.9260157555762,124.284136275697));
#99750=CARTESIAN_POINT('Ctrl Pts',(6.13949581784567,-31.9012222735897,124.217429952524));
#99751=CARTESIAN_POINT('Ctrl Pts',(6.14335459433857,-31.8729312221434,124.151937847602));
#99752=CARTESIAN_POINT('Ctrl Pts',(6.14721337083148,-31.8412878889773,124.088047987882));
#99753=CARTESIAN_POINT('Ctrl Pts',(6.15106971641969,-31.8096644900903,124.024198376713));
#99754=CARTESIAN_POINT('Ctrl Pts',(6.15492606200789,-31.7746932144136,123.961949442476));
#99755=CARTESIAN_POINT('Ctrl Pts',(6.15878240759609,-31.736567100229,123.901668415777));
#99756=CARTESIAN_POINT('Ctrl Pts',(6.16263761384142,-31.6984522502622,123.841405198882));
#99757=CARTESIAN_POINT('Ctrl Pts',(6.16649282008675,-31.6571846717618,123.783109145601));
#99758=CARTESIAN_POINT('Ctrl Pts',(6.17034802633208,-31.6130020290764,123.727120580457));
#99759=CARTESIAN_POINT('Ctrl Pts',(6.17420338318332,-31.56881766037,123.671129828087));
#99760=CARTESIAN_POINT('Ctrl Pts',(6.17805874003457,-31.5217183040519,123.617447122804));
#99761=CARTESIAN_POINT('Ctrl Pts',(6.18191409688581,-31.4719823290648,123.566380250757));
#99762=CARTESIAN_POINT('Ctrl Pts',(6.18577348935437,-31.4221942926552,123.515259924162));
#99763=CARTESIAN_POINT('Ctrl Pts',(6.18963288182292,-31.3697644678364,123.466761245463));
#99764=CARTESIAN_POINT('Ctrl Pts',(6.19349227429148,-31.3150079288298,123.421154944393));
#99765=CARTESIAN_POINT('Ctrl Pts',(6.19735385189491,-31.2602203874248,123.375522821663));
#99766=CARTESIAN_POINT('Ctrl Pts',(6.20121542949834,-31.2031038985311,123.332786627736));
#99767=CARTESIAN_POINT('Ctrl Pts',(6.20507700710177,-31.1440042422665,123.29317491928));
#99768=CARTESIAN_POINT('Ctrl Pts',(6.20894534121664,-31.0848011807245,123.25349390315));
#99769=CARTESIAN_POINT('Ctrl Pts',(6.21281367533151,-31.0236084412548,123.216948536353));
#99770=CARTESIAN_POINT('Ctrl Pts',(6.21668200944638,-30.9607975975381,123.183722064478));
#99771=CARTESIAN_POINT('Ctrl Pts',(6.21897972861736,-30.9234891139718,123.163986152546));
#99772=CARTESIAN_POINT('Ctrl Pts',(6.22127744778835,-30.885610166226,123.145420289185));
#99773=CARTESIAN_POINT('Ctrl Pts',(6.22357516695933,-30.847241632767,123.128054707475));
#99774=CARTESIAN_POINT('Ctrl Pts',(6.22744424030755,-30.7826337937887,123.098813227393));
#99775=CARTESIAN_POINT('Ctrl Pts',(6.23131331365577,-30.7163837784896,123.072863185084));
#99776=CARTESIAN_POINT('Ctrl Pts',(6.23518238700399,-30.6488602364773,123.050390306749));
#99777=CARTESIAN_POINT('Ctrl Pts',(6.23904569539978,-30.5814373051209,123.027950913195));
#99778=CARTESIAN_POINT('Ctrl Pts',(6.24290900379558,-30.5127450708391,123.008978551621));
#99779=CARTESIAN_POINT('Ctrl Pts',(6.24677231219137,-30.4431734770939,122.993611495323));
#99780=CARTESIAN_POINT('Ctrl Pts',(6.25063108868428,-30.3736834951884,122.978262465545));
#99781=CARTESIAN_POINT('Ctrl Pts',(6.2544898651772,-30.3033166748642,122.966510444591));
#99782=CARTESIAN_POINT('Ctrl Pts',(6.25834864167012,-30.2324778133163,122.958443821783));
#99783=CARTESIAN_POINT('Ctrl Pts',(6.26220498725833,-30.1616835779659,122.950382280687));
#99784=CARTESIAN_POINT('Ctrl Pts',(6.26606133284654,-30.0904183728962,122.946001586392));
#99785=CARTESIAN_POINT('Ctrl Pts',(6.26991767843475,-30.0190954215666,122.945338731719));
#99786=CARTESIAN_POINT('Ctrl Pts',(6.27377288468009,-29.947793542336,122.944676072884));
#99787=CARTESIAN_POINT('Ctrl Pts',(6.27762809092543,-29.8764344362167,122.947729077512));
#99788=CARTESIAN_POINT('Ctrl Pts',(6.28148329717076,-29.8054329252711,122.954482653231));
#99789=CARTESIAN_POINT('Ctrl Pts',(6.28533865402201,-29.7344286406094,122.961236492783));
#99790=CARTESIAN_POINT('Ctrl Pts',(6.28919401087327,-29.6637824622511,122.971691142247));
#99791=CARTESIAN_POINT('Ctrl Pts',(6.29304936772452,-29.5939039520619,122.985779663902));
#99792=CARTESIAN_POINT('Ctrl Pts',(6.29690876019308,-29.5239522961339,122.9998829328));
#99793=CARTESIAN_POINT('Ctrl Pts',(6.30076815266165,-29.4547703896434,123.017627570876));
#99794=CARTESIAN_POINT('Ctrl Pts',(6.30462754513021,-29.386756569374,123.038895704636));
#99795=CARTESIAN_POINT('Ctrl Pts',(6.30848912273365,-29.3187042406161,123.060175880121));
#99796=CARTESIAN_POINT('Ctrl Pts',(6.31235070033709,-29.2518217703124,123.084983353613));
#99797=CARTESIAN_POINT('Ctrl Pts',(6.31621227794053,-29.1864887175937,123.113151581102));
#99798=CARTESIAN_POINT('Ctrl Pts',(6.32008061205541,-29.1210413531704,123.141369093876));
#99799=CARTESIAN_POINT('Ctrl Pts',(6.32394894617028,-29.0571492544867,123.172958885327));
#99800=CARTESIAN_POINT('Ctrl Pts',(6.32781728028516,-28.9951679023623,123.207708166046));
#99801=CARTESIAN_POINT('Ctrl Pts',(6.33011499945607,-28.9583521215156,123.228348598365));
#99802=CARTESIAN_POINT('Ctrl Pts',(6.33241271862698,-28.9222099501554,123.250102894812));
#99803=CARTESIAN_POINT('Ctrl Pts',(6.33471043779789,-28.8868106539846,123.272919503203));
#99804=CARTESIAN_POINT('Ctrl Pts',(6.33857951114609,-28.8272026413547,123.311339834345));
#99805=CARTESIAN_POINT('Ctrl Pts',(6.34244858449429,-28.7694692515095,123.352924986983));
#99806=CARTESIAN_POINT('Ctrl Pts',(6.34631765784249,-28.7139664634272,123.397465973743));
#99807=CARTESIAN_POINT('Ctrl Pts',(6.35018096623826,-28.6585463749746,123.441940594052));
#99808=CARTESIAN_POINT('Ctrl Pts',(6.35404427463404,-28.6053506667869,123.489362004667));
#99809=CARTESIAN_POINT('Ctrl Pts',(6.35790758302981,-28.5547069996118,123.539477591569));
#99810=CARTESIAN_POINT('Ctrl Pts',(6.36176635952271,-28.5041227406324,123.589534389747));
#99811=CARTESIAN_POINT('Ctrl Pts',(6.36562513601561,-28.4560849197788,123.642278746475));
#99812=CARTESIAN_POINT('Ctrl Pts',(6.3694839125085,-28.4108873442318,123.697418513191));
#99813=CARTESIAN_POINT('Ctrl Pts',(6.3733402580967,-28.3657182416993,123.752523543633));
#99814=CARTESIAN_POINT('Ctrl Pts',(6.37719660368489,-28.3233861418341,123.81002061536));
#99815=CARTESIAN_POINT('Ctrl Pts',(6.38105294927308,-28.2841462414821,123.869582624921));
#99816=CARTESIAN_POINT('Ctrl Pts',(6.3849081555184,-28.2449179344118,123.92912703711));
#99817=CARTESIAN_POINT('Ctrl Pts',(6.38876336176371,-28.2087802802567,123.990734770517));
#99818=CARTESIAN_POINT('Ctrl Pts',(6.39261856800903,-28.1759455838451,124.054049129497));
#99819=CARTESIAN_POINT('Ctrl Pts',(6.39647392486026,-28.1431096047267,124.11736596189));
#99820=CARTESIAN_POINT('Ctrl Pts',(6.40032928171149,-28.1135770612153,124.182389119962));
#99821=CARTESIAN_POINT('Ctrl Pts',(6.40418463856272,-28.087513847662,124.248738208335));
#99822=CARTESIAN_POINT('Ctrl Pts',(6.40804403103126,-28.0614233522875,124.315156748004));
#99823=CARTESIAN_POINT('Ctrl Pts',(6.41190342349981,-28.0388096142217,124.382903535505));
#99824=CARTESIAN_POINT('Ctrl Pts',(6.41576281596836,-28.0197896463736,124.451579980407));
#99825=CARTESIAN_POINT('Ctrl Pts',(6.41962439357178,-28.0007589096816,124.520295308966));
#99826=CARTESIAN_POINT('Ctrl Pts',(6.4234859711752,-27.9853260988995,124.589940868237));
#99827=CARTESIAN_POINT('Ctrl Pts',(6.42734754877862,-27.973557152391,124.660107446574));
#99828=CARTESIAN_POINT('Ctrl Pts',(6.43121588289348,-27.9617676140339,124.730396793721));
#99829=CARTESIAN_POINT('Ctrl Pts',(6.43508421700834,-27.9536547941653,124.801208497216));
#99830=CARTESIAN_POINT('Ctrl Pts',(6.43895255112319,-27.949232719164,124.872128492805));
#99831=CARTESIAN_POINT('Ctrl Pts',(6.44125027029428,-27.9466060881117,124.914253663134));
#99832=CARTESIAN_POINT('Ctrl Pts',(6.44354798946536,-27.9452806044252,124.956417024691));
#99833=CARTESIAN_POINT('Ctrl Pts',(6.44584570863644,-27.9452505240975,124.998532424289));
#99834=CARTESIAN_POINT('Ctrl Pts',(6.44587223260258,-27.9452501768621,124.999018587892));
#99835=CARTESIAN_POINT('Ctrl Pts',(6.44589875656872,-27.9452500021695,124.999504751619));
#99836=CARTESIAN_POINT('Ctrl Pts',(6.44592528053486,-27.9452500000201,124.999990915393));
#99837=CARTESIAN_POINT('Origin',(-1.54592528053767,-30.,125.));
#99838=CARTESIAN_POINT('',(5.29388025174645,-31.2520409112987,126.629230222815));
#99839=CARTESIAN_POINT('',(5.35213747652439,-31.2520409112987,126.629230222815));
#99840=CARTESIAN_POINT('',(-1.54592528053767,-31.2520409112987,126.629230222815));
#99841=CARTESIAN_POINT('',(5.80407471941279,-27.9452508587689,124.998121407386));
#99842=CARTESIAN_POINT('Ctrl Pts',(5.35213747652439,-31.2520409112987,126.629230222815));
#99843=CARTESIAN_POINT('Ctrl Pts',(5.35599720568668,-31.3084431276569,126.585885898987));
#99844=CARTESIAN_POINT('Ctrl Pts',(5.35985693484896,-31.3626623496427,126.539555122573));
#99845=CARTESIAN_POINT('Ctrl Pts',(5.36371666401124,-31.4143692255357,126.490488931981));
#99846=CARTESIAN_POINT('Ctrl Pts',(5.36757358507917,-31.4660384827823,126.44145843884));
#99847=CARTESIAN_POINT('Ctrl Pts',(5.3714305061471,-31.5151986686399,126.389696812789));
#99848=CARTESIAN_POINT('Ctrl Pts',(5.37528742721503,-31.5615540543982,126.335494851241));
#99849=CARTESIAN_POINT('Ctrl Pts',(5.37914283246657,-31.6078912219321,126.281314191717));
#99850=CARTESIAN_POINT('Ctrl Pts',(5.38299823771811,-31.6514254617369,126.224695469051));
#99851=CARTESIAN_POINT('Ctrl Pts',(5.38685364296964,-31.6918996281051,126.165964498138));
#99852=CARTESIAN_POINT('Ctrl Pts',(5.39070882268999,-31.7323714268398,126.107236962834));
#99853=CARTESIAN_POINT('Ctrl Pts',(5.39456400241034,-31.7697832332088,126.046397825505));
#99854=CARTESIAN_POINT('Ctrl Pts',(5.39841918213069,-31.803920759363,125.983802549519));
#99855=CARTESIAN_POINT('Ctrl Pts',(5.40227815589108,-31.8380918816529,125.921145670961));
#99856=CARTESIAN_POINT('Ctrl Pts',(5.40613712965147,-31.8689820537455,125.856729628919));
#99857=CARTESIAN_POINT('Ctrl Pts',(5.40999610341185,-31.8964230160968,125.790934451468));
#99858=CARTESIAN_POINT('Ctrl Pts',(5.41385692445022,-31.923877114346,125.725107778082));
#99859=CARTESIAN_POINT('Ctrl Pts',(5.4177177454886,-31.9478785498704,125.657901112266));
#99860=CARTESIAN_POINT('Ctrl Pts',(5.42157856652697,-31.9683082961627,125.589711805679));
#99861=CARTESIAN_POINT('Ctrl Pts',(5.42544650188966,-31.9887756882923,125.521396846844));
#99862=CARTESIAN_POINT('Ctrl Pts',(5.42931443725234,-32.0056581259862,125.452096102648));
#99863=CARTESIAN_POINT('Ctrl Pts',(5.43318237261502,-32.0188873920948,125.38221886471));
#99864=CARTESIAN_POINT('Ctrl Pts',(5.43660621361637,-32.0305977490355,125.320364534202));
#99865=CARTESIAN_POINT('Ctrl Pts',(5.44003005461772,-32.0394463839407,125.258058847955));
#99866=CARTESIAN_POINT('Ctrl Pts',(5.44345389561906,-32.0454200326908,125.195587454524));
#99867=CARTESIAN_POINT('Ctrl Pts',(5.44732296896727,-32.0521704878556,125.124992352924));
#99868=CARTESIAN_POINT('Ctrl Pts',(5.45119204231548,-32.0552751231039,125.053909088628));
#99869=CARTESIAN_POINT('Ctrl Pts',(5.45506111566369,-32.0546775616078,124.982746585111));
#99870=CARTESIAN_POINT('Ctrl Pts',(5.45892442405947,-32.0540808904835,124.911690114334));
#99871=CARTESIAN_POINT('Ctrl Pts',(5.46278773245525,-32.0497929763708,124.840555120507));
#99872=CARTESIAN_POINT('Ctrl Pts',(5.46665104085102,-32.0418092335023,124.769755311713));
#99873=CARTESIAN_POINT('Ctrl Pts',(5.47050981734393,-32.0338348560647,124.699038555531));
#99874=CARTESIAN_POINT('Ctrl Pts',(5.47436859383683,-32.0221733156896,124.628656683752));
#99875=CARTESIAN_POINT('Ctrl Pts',(5.47822737032974,-32.0068720328795,124.559021308739));
#99876=CARTESIAN_POINT('Ctrl Pts',(5.48208371591794,-31.9915803893839,124.489429801765));
#99877=CARTESIAN_POINT('Ctrl Pts',(5.48594006150614,-31.9726536565801,124.420584331896));
#99878=CARTESIAN_POINT('Ctrl Pts',(5.48979640709434,-31.9501906114721,124.352887844786));
#99879=CARTESIAN_POINT('Ctrl Pts',(5.49365161333966,-31.9277342029867,124.285211358349));
#99880=CARTESIAN_POINT('Ctrl Pts',(5.49750681958499,-31.9017437093025,124.218683641558));
#99881=CARTESIAN_POINT('Ctrl Pts',(5.50136202583031,-31.8723677051348,124.153692290436));
#99882=CARTESIAN_POINT('Ctrl Pts',(5.50521738268155,-31.8429905533761,124.088698400388));
#99883=CARTESIAN_POINT('Ctrl Pts',(5.50907273953279,-31.8102278306469,124.025241436929));
#99884=CARTESIAN_POINT('Ctrl Pts',(5.51292809638403,-31.7742754619648,123.963687234678));
#99885=CARTESIAN_POINT('Ctrl Pts',(5.51678748885258,-31.7382854599306,123.902068600206));
#99886=CARTESIAN_POINT('Ctrl Pts',(5.52064688132113,-31.6990993924953,123.84235712321));
#99887=CARTESIAN_POINT('Ctrl Pts',(5.52450627378969,-31.6569577433049,123.784891527722));
#99888=CARTESIAN_POINT('Ctrl Pts',(5.52836785139311,-31.6147922340929,123.727393396005));
#99889=CARTESIAN_POINT('Ctrl Pts',(5.53222942899655,-31.5696681193209,123.672144053557));
#99890=CARTESIAN_POINT('Ctrl Pts',(5.53609100659997,-31.5218658529214,123.619448701347));
#99891=CARTESIAN_POINT('Ctrl Pts',(5.53995934071484,-31.4739799480217,123.566661149321));
#99892=CARTESIAN_POINT('Ctrl Pts',(5.5438276748297,-31.4234068807599,123.516436851756));
#99893=CARTESIAN_POINT('Ctrl Pts',(5.54769600894457,-31.3704630647979,123.469043256482));
#99894=CARTESIAN_POINT('Ctrl Pts',(5.54999372811558,-31.3390154138685,123.44089233435));
#99895=CARTESIAN_POINT('Ctrl Pts',(5.5522914472866,-31.3067319607153,123.41373934893));
#99896=CARTESIAN_POINT('Ctrl Pts',(5.55458916645762,-31.2736839053951,123.387633146075));
#99897=CARTESIAN_POINT('Ctrl Pts',(5.55845823980584,-31.2180350899684,123.343673546936));
#99898=CARTESIAN_POINT('Ctrl Pts',(5.56232731315406,-31.1599987860128,123.302512198001));
#99899=CARTESIAN_POINT('Ctrl Pts',(5.56619638650228,-31.0998879711842,123.264418249305));
#99900=CARTESIAN_POINT('Ctrl Pts',(5.57005969489807,-31.0398667219847,123.22638106092));
#99901=CARTESIAN_POINT('Ctrl Pts',(5.57392300329386,-30.9777775045226,123.191402458471));
#99902=CARTESIAN_POINT('Ctrl Pts',(5.57778631168965,-30.9139654058242,123.159710675069));
#99903=CARTESIAN_POINT('Ctrl Pts',(5.58164508818257,-30.8502281627168,123.128056068114));
#99904=CARTESIAN_POINT('Ctrl Pts',(5.58550386467549,-30.7847724858286,123.099680836624));
#99905=CARTESIAN_POINT('Ctrl Pts',(5.58936264116841,-30.7179699078123,123.07476838433));
#99906=CARTESIAN_POINT('Ctrl Pts',(5.59321898675662,-30.651209413265,123.049871626077));
#99907=CARTESIAN_POINT('Ctrl Pts',(5.59707533234483,-30.5831041550974,123.028433488423));
#99908=CARTESIAN_POINT('Ctrl Pts',(5.60093167793304,-30.5140462386043,123.010589527755));
#99909=CARTESIAN_POINT('Ctrl Pts',(5.60478688417838,-30.4450087250143,122.992750839019));
#99910=CARTESIAN_POINT('Ctrl Pts',(5.60864209042371,-30.3750195819556,122.978504340595));
#99911=CARTESIAN_POINT('Ctrl Pts',(5.61249729666905,-30.3044850273202,122.967935426558));
#99912=CARTESIAN_POINT('Ctrl Pts',(5.6163526535203,-30.2339477172106,122.95736609964));
#99913=CARTESIAN_POINT('Ctrl Pts',(5.62020801037156,-30.1628654339714,122.950474712148));
#99914=CARTESIAN_POINT('Ctrl Pts',(5.62406336722281,-30.0916517938937,122.947295074499));
#99915=CARTESIAN_POINT('Ctrl Pts',(5.62792275969137,-30.0203636105222,122.944112108546));
#99916=CARTESIAN_POINT('Ctrl Pts',(5.63178215215993,-29.9489442821312,122.944648670073));
#99917=CARTESIAN_POINT('Ctrl Pts',(5.6356415446285,-29.8778088152267,122.948886430043));
#99918=CARTESIAN_POINT('Ctrl Pts',(5.63950312223194,-29.8066330724002,122.953126589374));
#99919=CARTESIAN_POINT('Ctrl Pts',(5.64336469983538,-29.7357419939932,122.961072064643));
#99920=CARTESIAN_POINT('Ctrl Pts',(5.64722627743882,-29.6655441007758,122.972652764331));
#99921=CARTESIAN_POINT('Ctrl Pts',(5.6510946115537,-29.595223383957,122.984253726497));
#99922=CARTESIAN_POINT('Ctrl Pts',(5.65496294566857,-29.5255987485067,122.999502507974));
#99923=CARTESIAN_POINT('Ctrl Pts',(5.65883127978345,-29.4570665004004,123.018278329958));
#99924=CARTESIAN_POINT('Ctrl Pts',(5.66112899895436,-29.4163596080734,123.029430822179));
#99925=CARTESIAN_POINT('Ctrl Pts',(5.66342671812527,-29.3760378167373,123.041826753286));
#99926=CARTESIAN_POINT('Ctrl Pts',(5.66572443729618,-29.336180780275,123.055432797247));
#99927=CARTESIAN_POINT('Ctrl Pts',(5.66959351064439,-29.2690664873416,123.078343683281));
#99928=CARTESIAN_POINT('Ctrl Pts',(5.6734625839926,-29.2030082382595,123.104778072836));
#99929=CARTESIAN_POINT('Ctrl Pts',(5.67733165734081,-29.1384019055373,123.134618997063));
#99930=CARTESIAN_POINT('Ctrl Pts',(5.68119496573659,-29.0738918368044,123.164415458058));
#99931=CARTESIAN_POINT('Ctrl Pts',(5.68505827413237,-29.010829827629,123.197608176431));
#99932=CARTESIAN_POINT('Ctrl Pts',(5.68892158252814,-28.9495947893972,123.234031014984));
#99933=CARTESIAN_POINT('Ctrl Pts',(5.69278035902105,-28.8884315837029,123.270411127264));
#99934=CARTESIAN_POINT('Ctrl Pts',(5.69663913551396,-28.8290915074142,123.31001358609));
#99935=CARTESIAN_POINT('Ctrl Pts',(5.70049791200687,-28.7719301519635,123.352625722295));
#99936=CARTESIAN_POINT('Ctrl Pts',(5.70435425759507,-28.7148048063227,123.395211014229));
#99937=CARTESIAN_POINT('Ctrl Pts',(5.70821060318327,-28.6598558470079,123.440801932254));
#99938=CARTESIAN_POINT('Ctrl Pts',(5.71206694877147,-28.6074098246745,123.489142572548));
#99939=CARTESIAN_POINT('Ctrl Pts',(5.7159221550168,-28.5549792973221,123.537468930781));
#99940=CARTESIAN_POINT('Ctrl Pts',(5.71977736126213,-28.5050505958757,123.588543069396));
#99941=CARTESIAN_POINT('Ctrl Pts',(5.72363256750745,-28.4579157816108,123.642070021726));
#99942=CARTESIAN_POINT('Ctrl Pts',(5.7274879243587,-28.4107791259965,123.695599065118));
#99943=CARTESIAN_POINT('Ctrl Pts',(5.73134328120994,-28.3664368936465,123.751580746428));
#99944=CARTESIAN_POINT('Ctrl Pts',(5.73519863806118,-28.3251418207865,123.809685906148));
#99945=CARTESIAN_POINT('Ctrl Pts',(5.73905803052974,-28.2838035220677,123.867851887784));
#99946=CARTESIAN_POINT('Ctrl Pts',(5.74291742299829,-28.2455190320528,123.928145388184));
#99947=CARTESIAN_POINT('Ctrl Pts',(5.74677681546684,-28.2104980363441,123.990207801292));
#99948=CARTESIAN_POINT('Ctrl Pts',(5.75063839307027,-28.1754572122299,124.052305353284));
#99949=CARTESIAN_POINT('Ctrl Pts',(5.7544999706737,-28.1436837771905,124.116173376588));
#99950=CARTESIAN_POINT('Ctrl Pts',(5.75836154827713,-28.1153404112816,124.181430639987));
#99951=CARTESIAN_POINT('Ctrl Pts',(5.762229882392,-28.0869474536525,124.246802082484));
#99952=CARTESIAN_POINT('Ctrl Pts',(5.76609821650687,-28.0619967174549,124.313567162888));
#99953=CARTESIAN_POINT('Ctrl Pts',(5.76996655062174,-28.0406016732831,124.3813274212));
#99954=CARTESIAN_POINT('Ctrl Pts',(5.77226426979274,-28.0278934113548,124.421575765819));
#99955=CARTESIAN_POINT('Ctrl Pts',(5.77456198896374,-28.0164386815439,124.462174966915));
#99956=CARTESIAN_POINT('Ctrl Pts',(5.77685970813474,-28.0062526866041,124.503040028949));
#99957=CARTESIAN_POINT('Ctrl Pts',(5.78191177765178,-27.9838564098157,124.592891363621));
#99958=CARTESIAN_POINT('Ctrl Pts',(5.78696384716883,-27.9675248955161,124.684310306518));
#99959=CARTESIAN_POINT('Ctrl Pts',(5.79201591668587,-27.9574316008725,124.776590292544));
#99960=CARTESIAN_POINT('Ctrl Pts',(5.79603551759484,-27.9494010272259,124.850011435));
#99961=CARTESIAN_POINT('Ctrl Pts',(5.80005511850382,-27.9453186463013,124.923977405746));
#99962=CARTESIAN_POINT('Ctrl Pts',(5.80407471941279,-27.9452508587689,124.998121407386));
#99963=CARTESIAN_POINT('Ctrl Pts',(5.80407471946233,-27.9452508587681,124.9981214083));
#99964=CARTESIAN_POINT('Ctrl Pts',(5.80788808427067,-27.9451865492831,125.068461258701));
#99965=CARTESIAN_POINT('Ctrl Pts',(5.81170144907901,-27.9487383877838,125.138896596668));
#99966=CARTESIAN_POINT('Ctrl Pts',(5.81551481388736,-27.9559090953207,125.209021376676));
#99967=CARTESIAN_POINT('Ctrl Pts',(5.81932566294071,-27.9630750721948,125.279099893928));
#99968=CARTESIAN_POINT('Ctrl Pts',(5.82313651199406,-27.9738551346033,125.34886776481));
#99969=CARTESIAN_POINT('Ctrl Pts',(5.82694736104741,-27.9881999804143,125.417921336731));
#99970=CARTESIAN_POINT('Ctrl Pts',(5.83075704398259,-28.0025404367087,125.486953778289));
#99971=CARTESIAN_POINT('Ctrl Pts',(5.83456672691777,-28.0204434107702,125.555271866755));
#99972=CARTESIAN_POINT('Ctrl Pts',(5.83837640985295,-28.0418083477081,125.622481337386));
#99973=CARTESIAN_POINT('Ctrl Pts',(5.84218627454128,-28.0631743039288,125.689694014461));
#99974=CARTESIAN_POINT('Ctrl Pts',(5.84599613922961,-28.0880023967571,125.755797494632));
#99975=CARTESIAN_POINT('Ctrl Pts',(5.84980600391794,-28.1161425514216,125.82041372242));
#99976=CARTESIAN_POINT('Ctrl Pts',(5.85361981396668,-28.1443118470297,125.885096864477));
#99977=CARTESIAN_POINT('Ctrl Pts',(5.85743362401542,-28.1757998467943,125.948289224173));
#99978=CARTESIAN_POINT('Ctrl Pts',(5.86124743406417,-28.2104092282852,126.009634801447));
#99979=CARTESIAN_POINT('Ctrl Pts',(5.8650635652738,-28.2450396737361,126.071017714863));
#99980=CARTESIAN_POINT('Ctrl Pts',(5.86887969648342,-28.2827950106818,126.130551190871));
#99981=CARTESIAN_POINT('Ctrl Pts',(5.87269582769305,-28.3234345959164,126.187908249121));
#99982=CARTESIAN_POINT('Ctrl Pts',(5.8765183006624,-28.3641417172158,126.245360625027));
#99983=CARTESIAN_POINT('Ctrl Pts',(5.88034077363176,-28.4077423369046,126.300628980537));
#99984=CARTESIAN_POINT('Ctrl Pts',(5.88416324660111,-28.4539562862319,126.353420259054));
#99985=CARTESIAN_POINT('Ctrl Pts',(5.88544049072517,-28.4693982516039,126.371059978374));
#99986=CARTESIAN_POINT('Ctrl Pts',(5.88671773484924,-28.4851317023621,126.388423448836));
#99987=CARTESIAN_POINT('Ctrl Pts',(5.8879949789733,-28.5011453432883,126.40550072236));
#99988=CARTESIAN_POINT('Ctrl Pts',(5.89186405232152,-28.5496544341878,126.45723180697));
#99989=CARTESIAN_POINT('Ctrl Pts',(5.89573312566973,-28.6009398356742,126.50654992552));
#99990=CARTESIAN_POINT('Ctrl Pts',(5.89960219901794,-28.6547319770886,126.553142462568));
#99991=CARTESIAN_POINT('Ctrl Pts',(5.90346550741373,-28.7084439677515,126.599665576337));
#99992=CARTESIAN_POINT('Ctrl Pts',(5.90732881580952,-28.7646549201417,126.643470854395));
#99993=CARTESIAN_POINT('Ctrl Pts',(5.9111921242053,-28.8230574377305,126.684281380179));
#99994=CARTESIAN_POINT('Ctrl Pts',(5.91505090069822,-28.8813914455059,126.725044032659));
#99995=CARTESIAN_POINT('Ctrl Pts',(5.91890967719113,-28.9419115156489,126.762818634033));
#99996=CARTESIAN_POINT('Ctrl Pts',(5.92276845368404,-29.0042774461901,126.797368676242));
#99997=CARTESIAN_POINT('Ctrl Pts',(5.92662479927225,-29.066604088207,126.831896953038));
#99998=CARTESIAN_POINT('Ctrl Pts',(5.93048114486046,-29.1307738596502,126.86320446602));
#99999=CARTESIAN_POINT('Ctrl Pts',(5.93433749044866,-29.1964191132023,126.891098971729));
#100000=CARTESIAN_POINT('Ctrl Pts',(5.93819269669399,-29.2620449721098,
126.918985236111));
#100001=CARTESIAN_POINT('Ctrl Pts',(5.94204790293932,-29.3291450008412,
126.943460305215));
#100002=CARTESIAN_POINT('Ctrl Pts',(5.94590310918465,-29.3973301517087,
126.964379448187));
#100003=CARTESIAN_POINT('Ctrl Pts',(5.9497584660359,-29.4655179662695,126.985299408379));
#100004=CARTESIAN_POINT('Ctrl Pts',(5.95361382288714,-29.5347905220617,
127.002663026264));
#100005=CARTESIAN_POINT('Ctrl Pts',(5.95746917973839,-29.6047437999571,
127.016375485575));
#100006=CARTESIAN_POINT('Ctrl Pts',(5.96132857220694,-29.674770301855,127.030102298483));
#100007=CARTESIAN_POINT('Ctrl Pts',(5.9651879646755,-29.7454784705754,127.040170229863));
#100008=CARTESIAN_POINT('Ctrl Pts',(5.96904735714406,-29.8164551747296,
127.046535819285));
#100009=CARTESIAN_POINT('Ctrl Pts',(5.97290893474749,-29.8874720649164,
127.052905012816));
#100010=CARTESIAN_POINT('Ctrl Pts',(5.97677051235093,-29.9587573075263,
127.055567673329));
#100011=CARTESIAN_POINT('Ctrl Pts',(5.98063208995436,-30.0298965035962,
127.054532492216));
#100012=CARTESIAN_POINT('Ctrl Pts',(5.98450042406923,-30.101160170243,127.053495499872));
#100013=CARTESIAN_POINT('Ctrl Pts',(5.9883687581841,-30.1722767953073,127.048747780675));
#100014=CARTESIAN_POINT('Ctrl Pts',(5.99223709229897,-30.2428365374347,
127.040349964733));
#100015=CARTESIAN_POINT('Ctrl Pts',(5.99453481146993,-30.2847477238447,
127.035361816835));
#100016=CARTESIAN_POINT('Ctrl Pts',(5.9968325306409,-30.3264625982632,127.029086849354));
#100017=CARTESIAN_POINT('Ctrl Pts',(5.99913024981186,-30.3678974432213,
127.021546198772));
#100018=CARTESIAN_POINT('Ctrl Pts',(6.00299944643829,-30.4376707925297,
127.008848276345));
#100019=CARTESIAN_POINT('Ctrl Pts',(6.00686864306471,-30.5069226418422,
126.992508916016));
#100020=CARTESIAN_POINT('Ctrl Pts',(6.01073783969114,-30.5752441048594,
126.97258505072));
#100021=CARTESIAN_POINT('Ctrl Pts',(6.01460043069505,-30.6434489271788,
126.952695200116));
#100022=CARTESIAN_POINT('Ctrl Pts',(6.01846302169896,-30.7107260565041,
126.929233137685));
#100023=CARTESIAN_POINT('Ctrl Pts',(6.02232561270287,-30.776676344021,126.902306867763));
#100024=CARTESIAN_POINT('Ctrl Pts',(6.0261843740982,-30.8425612443958,126.875407294189));
#100025=CARTESIAN_POINT('Ctrl Pts',(6.03004313549353,-30.907121465364,126.845050509387));
#100026=CARTESIAN_POINT('Ctrl Pts',(6.03390189688886,-30.9699737945266,
126.811394048911));
#100027=CARTESIAN_POINT('Ctrl Pts',(6.03775817556289,-31.0327856845946,
126.777759242952));
#100028=CARTESIAN_POINT('Ctrl Pts',(6.04161445423691,-31.0938914361431,
126.740829202853));
#100029=CARTESIAN_POINT('Ctrl Pts',(6.04547073291094,-31.1529301530049,
126.700808520908));
#100030=CARTESIAN_POINT('Ctrl Pts',(6.04767405776819,-31.1866625368388,
126.677942288774));
#100031=CARTESIAN_POINT('Ctrl Pts',(6.04987738262545,-31.2197205644288,
126.654067962738));
#100032=CARTESIAN_POINT('Ctrl Pts',(6.05208070748271,-31.2520409112986,
126.629230222815));
#100033=CARTESIAN_POINT('',(5.7459252805733,-27.9452507587439,125.001765802243));
#100034=CARTESIAN_POINT('Ctrl Pts',(5.7459252805733,-27.9452507587439,125.001765802243));
#100035=CARTESIAN_POINT('Ctrl Pts',(5.75057817989281,-27.9453246481717,
125.087746124361));
#100036=CARTESIAN_POINT('Ctrl Pts',(5.75523107921231,-27.950799087127,125.173490900306));
#100037=CARTESIAN_POINT('Ctrl Pts',(5.75988397853181,-27.9615629769852,
125.258402913494));
#100038=CARTESIAN_POINT('Ctrl Pts',(5.76460377517644,-27.9724816252832,
125.344535753992));
#100039=CARTESIAN_POINT('Ctrl Pts',(5.76932357182106,-27.9888428428069,
125.42981172288));
#100040=CARTESIAN_POINT('Ctrl Pts',(5.77404336846569,-28.0104818888308,
125.513629484969));
#100041=CARTESIAN_POINT('Ctrl Pts',(5.77570694017882,-28.018108934565,125.54317246501));
#100042=CARTESIAN_POINT('Ctrl Pts',(5.77737051189196,-28.0263912273211,
125.572534484293));
#100043=CARTESIAN_POINT('Ctrl Pts',(5.77903408360509,-28.0353201550616,
125.601689844848));
#100044=CARTESIAN_POINT('Ctrl Pts',(5.78290315695331,-28.0560867238102,
125.669498300347));
#100045=CARTESIAN_POINT('Ctrl Pts',(5.78677223030153,-28.0804085753381,
125.736363214624));
#100046=CARTESIAN_POINT('Ctrl Pts',(5.79064130364974,-28.1081813798381,
125.801885198086));
#100047=CARTESIAN_POINT('Ctrl Pts',(5.79450461204553,-28.1359128026216,
125.867309553231));
#100048=CARTESIAN_POINT('Ctrl Pts',(5.79836792044132,-28.1670847837139,
125.931394505826));
#100049=CARTESIAN_POINT('Ctrl Pts',(5.80223122883711,-28.2015433108011,
125.993756056372));
#100050=CARTESIAN_POINT('Ctrl Pts',(5.80609000533003,-28.2359614158763,
126.056044452911));
#100051=CARTESIAN_POINT('Ctrl Pts',(5.80994878182294,-28.2736581751636,
126.116613039969));
#100052=CARTESIAN_POINT('Ctrl Pts',(5.81380755831586,-28.3144323268255,
126.17509964754));
#100053=CARTESIAN_POINT('Ctrl Pts',(5.81766390390407,-28.3551807920873,
126.233549410435));
#100054=CARTESIAN_POINT('Ctrl Pts',(5.82152024949228,-28.3990025262966,
126.289919398435));
#100055=CARTESIAN_POINT('Ctrl Pts',(5.82537659508049,-28.4456521319437,
126.343875093738));
#100056=CARTESIAN_POINT('Ctrl Pts',(5.82923180132583,-28.4922879551394,
126.397814848033));
#100057=CARTESIAN_POINT('Ctrl Pts',(5.83308700757117,-28.5417496735587,
126.449341358437));
#100058=CARTESIAN_POINT('Ctrl Pts',(5.8369422138165,-28.5937517505778,126.498153337779));
#100059=CARTESIAN_POINT('Ctrl Pts',(5.84079757066776,-28.6457558590888,
126.546967223989));
#100060=CARTESIAN_POINT('Ctrl Pts',(5.84465292751901,-28.7003001675264,
126.593066037739));
#100061=CARTESIAN_POINT('Ctrl Pts',(5.84850828437026,-28.7570637140312,
126.636186710471));
#100062=CARTESIAN_POINT('Ctrl Pts',(5.85236767683882,-28.81388667811,126.679352520019));
#100063=CARTESIAN_POINT('Ctrl Pts',(5.85622706930739,-28.8729331298652,
126.719533671088));
#100064=CARTESIAN_POINT('Ctrl Pts',(5.86008646177595,-28.9338513077071,
126.756509188254));
#100065=CARTESIAN_POINT('Ctrl Pts',(5.86394803937939,-28.9948039765826,
126.793505640449));
#100066=CARTESIAN_POINT('Ctrl Pts',(5.86780961698283,-29.0576300531272,
126.827292615469));
#100067=CARTESIAN_POINT('Ctrl Pts',(5.87167119458628,-29.1219536682809,
126.85769540072));
#100068=CARTESIAN_POINT('Ctrl Pts',(5.87553952870115,-29.1863898289499,
126.888151381008));
#100069=CARTESIAN_POINT('Ctrl Pts',(5.87940786281603,-29.2523283099923,
126.915211165115));
#100070=CARTESIAN_POINT('Ctrl Pts',(5.8832761969309,-29.3193744584979,126.938748677564));
#100071=CARTESIAN_POINT('Ctrl Pts',(5.88557391610182,-29.3591986350511,
126.952729526162));
#100072=CARTESIAN_POINT('Ctrl Pts',(5.88787163527273,-29.3994133254093,
126.965468625186));
#100073=CARTESIAN_POINT('Ctrl Pts',(5.89016935444365,-29.43993406007,126.976948078587));
#100074=CARTESIAN_POINT('Ctrl Pts',(5.89403860385592,-29.5081690431589,
126.996278930193));
#100075=CARTESIAN_POINT('Ctrl Pts',(5.89790785326819,-29.5775396773508,
127.012110772205));
#100076=CARTESIAN_POINT('Ctrl Pts',(5.90177710268046,-29.6476537793551,
127.02431462557));
#100077=CARTESIAN_POINT('Ctrl Pts',(5.9056396209416,-29.7176459071555,127.036497248466));
#100078=CARTESIAN_POINT('Ctrl Pts',(5.90950213920275,-29.7883784582127,
127.045064340978));
#100079=CARTESIAN_POINT('Ctrl Pts',(5.9133646574639,-29.859445536846,127.049937073519));
#100080=CARTESIAN_POINT('Ctrl Pts',(5.91722337855584,-29.9304427507683,
127.054805015768));
#100081=CARTESIAN_POINT('Ctrl Pts',(5.92108209964779,-30.0017733579082,
127.055985769382));
#100082=CARTESIAN_POINT('Ctrl Pts',(5.92494082073974,-30.0730239449286,
127.053451987743));
#100083=CARTESIAN_POINT('Ctrl Pts',(5.92879703930301,-30.1442283232098,
127.050919849359));
#100084=CARTESIAN_POINT('Ctrl Pts',(5.93265325786629,-30.2153523000852,
127.044677973575));
#100085=CARTESIAN_POINT('Ctrl Pts',(5.93650947642956,-30.2859817782854,
127.03475108674));
#100086=CARTESIAN_POINT('Ctrl Pts',(5.94036448407856,-30.3565890777004,
127.024827317106));
#100087=CARTESIAN_POINT('Ctrl Pts',(5.94421949172756,-30.426701706177,127.011220902373));
#100088=CARTESIAN_POINT('Ctrl Pts',(5.94807449937655,-30.4959117352762,
126.994008303221));
#100089=CARTESIAN_POINT('Ctrl Pts',(5.95193183765649,-30.5651636068437,
126.976785297808));
#100090=CARTESIAN_POINT('Ctrl Pts',(5.95578917593642,-30.6335113149249,
126.955951863161));
#100091=CARTESIAN_POINT('Ctrl Pts',(5.95964651421635,-30.7005591566621,
126.931635170139));
#100092=CARTESIAN_POINT('Ctrl Pts',(5.96350485068189,-30.7676243487548,
126.907312184546));
#100093=CARTESIAN_POINT('Ctrl Pts',(5.96736318714743,-30.8333885532979,
126.879504327398));
#100094=CARTESIAN_POINT('Ctrl Pts',(5.97122152361297,-30.8974756479425,
126.848387141226));
#100095=CARTESIAN_POINT('Ctrl Pts',(5.97508578864652,-30.9616612162953,
126.81722214161));
#100096=CARTESIAN_POINT('Ctrl Pts',(5.97895005368007,-31.0241640955484,
126.782737881713));
#100097=CARTESIAN_POINT('Ctrl Pts',(5.98281431871362,-31.0846329215314,
126.745155863535));
#100098=CARTESIAN_POINT('Ctrl Pts',(5.98650489602956,-31.1423838458485,
126.709263050135));
#100099=CARTESIAN_POINT('Ctrl Pts',(5.99019547334549,-31.1982793576751,
126.670545233824));
#100100=CARTESIAN_POINT('Ctrl Pts',(5.99388605066143,-31.2520409112987,
126.629230222815));
#100101=CARTESIAN_POINT('Ctrl Pts',(5.29388025174645,-31.2520409112987,
126.629230222815));
#100102=CARTESIAN_POINT('Ctrl Pts',(5.29773979436079,-31.3086193501602,
126.585750474428));
#100103=CARTESIAN_POINT('Ctrl Pts',(5.30159933697512,-31.3629005188046,
126.539342938539));
#100104=CARTESIAN_POINT('Ctrl Pts',(5.30545887958946,-31.4145793687864,
126.49028949265));
#100105=CARTESIAN_POINT('Ctrl Pts',(5.30932071234183,-31.4662888834641,
126.441206939902));
#100106=CARTESIAN_POINT('Ctrl Pts',(5.31318254509421,-31.5153926716702,
126.389475704715));
#100107=CARTESIAN_POINT('Ctrl Pts',(5.31704437784659,-31.5616240719298,
126.335412977498));
#100108=CARTESIAN_POINT('Ctrl Pts',(5.32091286057165,-31.6079350814237,
126.281257155711));
#100109=CARTESIAN_POINT('Ctrl Pts',(5.32478134329671,-31.651363534228,126.224762213207));
#100110=CARTESIAN_POINT('Ctrl Pts',(5.32864982602178,-31.6916848663766,
126.16627607168));
#100111=CARTESIAN_POINT('Ctrl Pts',(5.3305975507648,-31.7119860702023,126.136829150736));
#100112=CARTESIAN_POINT('Ctrl Pts',(5.33254527550783,-31.731500337346,126.106877886012));
#100113=CARTESIAN_POINT('Ctrl Pts',(5.33449300025086,-31.7502034628655,
126.076468950353));
#100114=CARTESIAN_POINT('Ctrl Pts',(5.33836207359907,-31.7873564357046,
126.016062877612));
#100115=CARTESIAN_POINT('Ctrl Pts',(5.34223114694728,-31.8214512506891,
125.953612795033));
#100116=CARTESIAN_POINT('Ctrl Pts',(5.34610022029549,-31.8522571895629,
125.889460997578));
#100117=CARTESIAN_POINT('Ctrl Pts',(5.34996352869127,-31.883017227324,125.825404786851));
#100118=CARTESIAN_POINT('Ctrl Pts',(5.35382683708705,-31.9104979076632,
125.759652328628));
#100119=CARTESIAN_POINT('Ctrl Pts',(5.35769014548283,-31.9345129022425,
125.692573023989));
#100120=CARTESIAN_POINT('Ctrl Pts',(5.36154892197574,-31.958499725728,125.625572407579));
#100121=CARTESIAN_POINT('Ctrl Pts',(5.36540769846865,-31.9790287759014,
125.557248491575));
#100122=CARTESIAN_POINT('Ctrl Pts',(5.36926647496156,-31.9959613378882,
125.487991700909));
#100123=CARTESIAN_POINT('Ctrl Pts',(5.37312282054977,-32.0128832329071,
125.418778539786));
#100124=CARTESIAN_POINT('Ctrl Pts',(5.37697916613797,-32.0262130196964,
125.34863414072));
#100125=CARTESIAN_POINT('Ctrl Pts',(5.38083551172617,-32.0358619075833,
125.277963766975));
#100126=CARTESIAN_POINT('Ctrl Pts',(5.3846907179715,-32.0455079447425,125.207314272528));
#100127=CARTESIAN_POINT('Ctrl Pts',(5.38854592421683,-32.0514751763227,
125.136139592967));
#100128=CARTESIAN_POINT('Ctrl Pts',(5.39240113046216,-32.053726279784,125.06485314352));
#100129=CARTESIAN_POINT('Ctrl Pts',(5.3962564873134,-32.055977471186,124.993563909226));
#100130=CARTESIAN_POINT('Ctrl Pts',(5.40011184416465,-32.0545122331165,
124.922163381991));
#100131=CARTESIAN_POINT('Ctrl Pts',(5.40396720101589,-32.049345337888,124.851066294692));
#100132=CARTESIAN_POINT('Ctrl Pts',(5.40782659348445,-32.0441730341816,
124.779894786102));
#100133=CARTESIAN_POINT('Ctrl Pts',(5.411685985953,-32.0352913737652,124.709027837005));
#100134=CARTESIAN_POINT('Ctrl Pts',(5.41554537842156,-32.0227670734458,
124.638875465963));
#100135=CARTESIAN_POINT('Ctrl Pts',(5.41940695602499,-32.01023568204,124.568683375614));
#100136=CARTESIAN_POINT('Ctrl Pts',(5.42326853362843,-31.9940576553275,
124.499207142076));
#100137=CARTESIAN_POINT('Ctrl Pts',(5.42713011123186,-31.9743503595413,
124.43084429171));
#100138=CARTESIAN_POINT('Ctrl Pts',(5.43099844534673,-31.9546085823636,
124.362361828474));
#100139=CARTESIAN_POINT('Ctrl Pts',(5.4348667794616,-31.9313253661288,124.294997097049));
#100140=CARTESIAN_POINT('Ctrl Pts',(5.43873511357647,-31.9046669889531,
124.229129567507));
#100141=CARTESIAN_POINT('Ctrl Pts',(5.44103283274745,-31.8888324042236,
124.190005468895));
#100142=CARTESIAN_POINT('Ctrl Pts',(5.44333055191843,-31.8718079232597,
124.151409186527));
#100143=CARTESIAN_POINT('Ctrl Pts',(5.44562827108941,-31.8536359549887,
124.113415932428));
#100144=CARTESIAN_POINT('Ctrl Pts',(5.44949734443762,-31.823036620218,124.049440017222));
#100145=CARTESIAN_POINT('Ctrl Pts',(5.45336641778584,-31.7890613887607,
123.986924796112));
#100146=CARTESIAN_POINT('Ctrl Pts',(5.45723549113406,-31.7518727042285,
123.926249754049));
#100147=CARTESIAN_POINT('Ctrl Pts',(5.46109879952985,-31.7147394311548,
123.865665118319));
#100148=CARTESIAN_POINT('Ctrl Pts',(5.46496210792564,-31.6744024609846,
123.80691562988));
#100149=CARTESIAN_POINT('Ctrl Pts',(5.46882541632144,-31.6310710858574,
123.750358181165));
#100150=CARTESIAN_POINT('Ctrl Pts',(5.47268419281435,-31.587790541149,123.693867077883));
#100151=CARTESIAN_POINT('Ctrl Pts',(5.47654296930726,-31.5415228627519,
123.639563290402));
#100152=CARTESIAN_POINT('Ctrl Pts',(5.48040174580018,-31.4925208296892,
123.58777511159));
#100153=CARTESIAN_POINT('Ctrl Pts',(5.48425809138838,-31.4435496663265,
123.536019557661));
#100154=CARTESIAN_POINT('Ctrl Pts',(5.48811443697659,-31.3918478989099,
123.486776820306));
#100155=CARTESIAN_POINT('Ctrl Pts',(5.4919707825648,-31.3377078498883,123.440341296678));
#100156=CARTESIAN_POINT('Ctrl Pts',(5.49582598881013,-31.2835837963415,
123.393919492252));
#100157=CARTESIAN_POINT('Ctrl Pts',(5.49968119505546,-31.2270232598807,
123.350303571092));
#100158=CARTESIAN_POINT('Ctrl Pts',(5.5035364013008,-31.168353326242,123.309749111061));
#100159=CARTESIAN_POINT('Ctrl Pts',(5.50739175815204,-31.1096811006276,
123.269193066746));
#100160=CARTESIAN_POINT('Ctrl Pts',(5.51124711500329,-31.0488997150945,
123.231698995419));
#100161=CARTESIAN_POINT('Ctrl Pts',(5.51510247185453,-30.9863656167697,
123.197479422432));
#100162=CARTESIAN_POINT('Ctrl Pts',(5.51896186432309,-30.923766060512,123.163224029908));
#100163=CARTESIAN_POINT('Ctrl Pts',(5.52282125679164,-30.859410556091,123.132250211661));
#100164=CARTESIAN_POINT('Ctrl Pts',(5.5266806492602,-30.7936797627607,123.104724295337));
#100165=CARTESIAN_POINT('Ctrl Pts',(5.53054222686363,-30.7279117535604,
123.077182794219));
#100166=CARTESIAN_POINT('Ctrl Pts',(5.53440380446706,-30.6607673628248,
123.053093245288));
#100167=CARTESIAN_POINT('Ctrl Pts',(5.5382653820705,-30.5926442249959,123.032572648081));
#100168=CARTESIAN_POINT('Ctrl Pts',(5.54213371618537,-30.5244018937161,
123.012016146468));
#100169=CARTESIAN_POINT('Ctrl Pts',(5.54600205030024,-30.4551778682629,
122.995041179658));
#100170=CARTESIAN_POINT('Ctrl Pts',(5.54987038441511,-30.3853811412496,
122.981713861102));
#100171=CARTESIAN_POINT('Ctrl Pts',(5.55216810358607,-30.3439231717553,
122.973797679501));
#100172=CARTESIAN_POINT('Ctrl Pts',(5.55446582275702,-30.3022632866963,
122.967167450132));
#100173=CARTESIAN_POINT('Ctrl Pts',(5.55676354192797,-30.260487676048,122.961828335707));
#100174=CARTESIAN_POINT('Ctrl Pts',(5.56063261527619,-30.1901427427731,
122.952837930967));
#100175=CARTESIAN_POINT('Ctrl Pts',(5.56450168862441,-30.1191940371151,
122.947475992101));
#100176=CARTESIAN_POINT('Ctrl Pts',(5.56837076197263,-30.0480484844915,
122.945811862161));
#100177=CARTESIAN_POINT('Ctrl Pts',(5.57223407036841,-29.9770089393508,
122.944150211789));
#100178=CARTESIAN_POINT('Ctrl Pts',(5.5760973787642,-29.9057736111404,122.946175444879));
#100179=CARTESIAN_POINT('Ctrl Pts',(5.57996068715999,-29.8347558532781,
122.951905291625));
#100180=CARTESIAN_POINT('Ctrl Pts',(5.5838194636529,-29.7638214036968,122.957628416901));
#100181=CARTESIAN_POINT('Ctrl Pts',(5.58767824014582,-29.6931044993654,
122.967047484839));
#100182=CARTESIAN_POINT('Ctrl Pts',(5.59153701663873,-29.6230180516856,
122.980128179031));
#100183=CARTESIAN_POINT('Ctrl Pts',(5.59539336222694,-29.5529757562069,
122.993200632807));
#100184=CARTESIAN_POINT('Ctrl Pts',(5.59924970781514,-29.4835636058172,
123.009930047454));
#100185=CARTESIAN_POINT('Ctrl Pts',(5.60310605340335,-29.4151874815842,
123.03023050059));
#100186=CARTESIAN_POINT('Ctrl Pts',(5.60696125964868,-29.3468315588213,
123.050524956034));
#100187=CARTESIAN_POINT('Ctrl Pts',(5.61081646589401,-29.2795115199826,
123.074388217214));
#100188=CARTESIAN_POINT('Ctrl Pts',(5.61467167213934,-29.2136194867204,
123.101684101411));
#100189=CARTESIAN_POINT('Ctrl Pts',(5.61852702899058,-29.147724879347,123.128981051939));
#100190=CARTESIAN_POINT('Ctrl Pts',(5.62238238584182,-29.0832588362644,
123.159710703764));
#100191=CARTESIAN_POINT('Ctrl Pts',(5.62623774269306,-29.0205932334001,
123.193688856249));
#100192=CARTESIAN_POINT('Ctrl Pts',(5.63009713516162,-28.9578620349498,
123.227702575564));
#100193=CARTESIAN_POINT('Ctrl Pts',(5.63395652763018,-28.8969354667703,
123.264971351449));
#100194=CARTESIAN_POINT('Ctrl Pts',(5.63781592009874,-28.8381597238708,
123.305265585626));
#100195=CARTESIAN_POINT('Ctrl Pts',(5.64167749770218,-28.7793507029549,
123.345582633843));
#100196=CARTESIAN_POINT('Ctrl Pts',(5.64553907530561,-28.7226953175207,
123.388928255032));
#100197=CARTESIAN_POINT('Ctrl Pts',(5.64940065290904,-28.6685075266158,
123.435031835525));
#100198=CARTESIAN_POINT('Ctrl Pts',(5.65326898702391,-28.6142249246086,
123.481216082367));
#100199=CARTESIAN_POINT('Ctrl Pts',(5.65713732113878,-28.5624188903334,
123.530167589093));
#100200=CARTESIAN_POINT('Ctrl Pts',(5.66100565525365,-28.5133667914834,
123.581578600755));
#100201=CARTESIAN_POINT('Ctrl Pts',(5.66330337442461,-28.4842307487951,
123.612115794179));
#100202=CARTESIAN_POINT('Ctrl Pts',(5.66560109359557,-28.4560655788399,
123.64352007997));
#100203=CARTESIAN_POINT('Ctrl Pts',(5.66789881276654,-28.428922365385,123.675721846245));
#100204=CARTESIAN_POINT('Ctrl Pts',(5.6717431454675,-28.3835088333867,123.729598884259));
#100205=CARTESIAN_POINT('Ctrl Pts',(5.67558747816845,-28.3407741615803,
123.785928448142));
#100206=CARTESIAN_POINT('Ctrl Pts',(5.67943181086941,-28.3009964282984,
123.844411653812));
#100207=CARTESIAN_POINT('Ctrl Pts',(5.68327073565049,-28.2612746513583,
123.90281258968));
#100208=CARTESIAN_POINT('Ctrl Pts',(5.68710966043156,-28.2245018386301,
123.963360756745));
#100209=CARTESIAN_POINT('Ctrl Pts',(5.69094858521263,-28.1909165779052,
124.025723481551));
#100210=CARTESIAN_POINT('Ctrl Pts',(5.69478343427791,-28.1573669740336,
124.088019996998));
#100211=CARTESIAN_POINT('Ctrl Pts',(5.69861828334319,-28.1269984405786,
124.15212681733));
#100212=CARTESIAN_POINT('Ctrl Pts',(5.70245313240846,-28.1000058717301,
124.217683008596));
#100213=CARTESIAN_POINT('Ctrl Pts',(5.70628582152496,-28.0730285062352,
124.283202275849));
#100214=CARTESIAN_POINT('Ctrl Pts',(5.71011851064145,-28.0494235257518,
124.350168842791));
#100215=CARTESIAN_POINT('Ctrl Pts',(5.71395119975794,-28.0293387874971,
124.418199391512));
#100216=CARTESIAN_POINT('Ctrl Pts',(5.71778249936723,-28.0092613307849,
124.486205276366));
#100217=CARTESIAN_POINT('Ctrl Pts',(5.72161379897651,-27.9927017184503,
124.55527390418));
#100218=CARTESIAN_POINT('Ctrl Pts',(5.7254450985858,-27.9797581310329,124.625006195555));
#100219=CARTESIAN_POINT('Ctrl Pts',(5.72927810286555,-27.9668087845902,
124.694769513106));
#100220=CARTESIAN_POINT('Ctrl Pts',(5.73311110714531,-27.9574787693273,
124.765196599802));
#100221=CARTESIAN_POINT('Ctrl Pts',(5.73694411142506,-27.9518149998427,
124.835878802007));
#100222=CARTESIAN_POINT('Ctrl Pts',(5.7399378344626,-27.947391379114,124.891084307047));
#100223=CARTESIAN_POINT('Ctrl Pts',(5.74293155750014,-27.9452032175471,
124.946445182456));
#100224=CARTESIAN_POINT('Ctrl Pts',(5.74592528053768,-27.9452507587434,
125.001765801585));
#100225=CARTESIAN_POINT('Origin',(-1.54592528053767,-30.,125.));
#100226=CARTESIAN_POINT('',(4.59397334877082,-31.2520409112987,126.629230222815));
#100227=CARTESIAN_POINT('',(4.65201706724701,-31.2520409112987,126.629230222815));
#100228=CARTESIAN_POINT('',(-1.54592528053767,-31.2520409112987,126.629230222815));
#100229=CARTESIAN_POINT('',(5.10407471942417,-27.9452501074214,125.000664415721));
#100230=CARTESIAN_POINT('Ctrl Pts',(4.65201706724701,-31.2520409112987,
126.629230222815));
#100231=CARTESIAN_POINT('Ctrl Pts',(4.6558862157949,-31.3084969643693,126.585844526217));
#100232=CARTESIAN_POINT('Ctrl Pts',(4.65975536434279,-31.3626115695028,
126.539585323213));
#100233=CARTESIAN_POINT('Ctrl Pts',(4.66362451289068,-31.4140958918003,
126.49074825886));
#100234=CARTESIAN_POINT('Ctrl Pts',(4.66425200851017,-31.4224455807083,
126.482827900266));
#100235=CARTESIAN_POINT('Ctrl Pts',(4.66487950412965,-31.430726172515,126.474839810443));
#100236=CARTESIAN_POINT('Ctrl Pts',(4.66550699974914,-31.4389365354662,
126.466785331738));
#100237=CARTESIAN_POINT('Ctrl Pts',(4.66937607309736,-31.4895607876316,
126.417122245773));
#100238=CARTESIAN_POINT('Ctrl Pts',(4.67324514644558,-31.5377100925751,
126.364737957514));
#100239=CARTESIAN_POINT('Ctrl Pts',(4.6771142197938,-31.5830779920416,126.309909017304));
#100240=CARTESIAN_POINT('Ctrl Pts',(4.68097752818959,-31.6283782929492,
126.255161772684));
#100241=CARTESIAN_POINT('Ctrl Pts',(4.68484083658538,-31.6709051075679,
126.197977477701));
#100242=CARTESIAN_POINT('Ctrl Pts',(4.68870414498117,-31.7103885202681,
126.138669694088));
#100243=CARTESIAN_POINT('Ctrl Pts',(4.69256292147409,-31.7498256164506,
126.079431482223));
#100244=CARTESIAN_POINT('Ctrl Pts',(4.696421697967,-31.7862261342446,126.018075132076));
#100245=CARTESIAN_POINT('Ctrl Pts',(4.70028047445992,-31.8193612958819,
125.954946091435));
#100246=CARTESIAN_POINT('Ctrl Pts',(4.70413682004813,-31.8524755834363,
125.891856820054));
#100247=CARTESIAN_POINT('Ctrl Pts',(4.70799316563634,-31.8823283707902,
125.826997502887));
#100248=CARTESIAN_POINT('Ctrl Pts',(4.71184951122455,-31.908735752307,125.760740028108));
#100249=CARTESIAN_POINT('Ctrl Pts',(4.71570471746989,-31.9351353318617,
125.694502128851));
#100250=CARTESIAN_POINT('Ctrl Pts',(4.71955992371522,-31.9580913466996,
125.626867343081));
#100251=CARTESIAN_POINT('Ctrl Pts',(4.72341512996056,-31.9774678742001,
125.558227882684));
#100252=CARTESIAN_POINT('Ctrl Pts',(4.72727048681181,-31.9968451586562,
125.489585740846));
#100253=CARTESIAN_POINT('Ctrl Pts',(4.73112584366306,-32.0126425482943,
125.419939314573));
#100254=CARTESIAN_POINT('Ctrl Pts',(4.73498120051431,-32.0247743599364,
125.349694658015));
#100255=CARTESIAN_POINT('Ctrl Pts',(4.73884059298288,-32.0369188706232,
125.279376472452));
#100256=CARTESIAN_POINT('Ctrl Pts',(4.74269998545144,-32.0453900610247,
125.208459286247));
#100257=CARTESIAN_POINT('Ctrl Pts',(4.74655937792,-32.0501537961902,125.137357105629));
#100258=CARTESIAN_POINT('Ctrl Pts',(4.75042095552344,-32.054920228517,125.066214667936));
#100259=CARTESIAN_POINT('Ctrl Pts',(4.75428253312688,-32.0559750197405,
124.994887513286));
#100260=CARTESIAN_POINT('Ctrl Pts',(4.75814411073032,-32.0533362020555,
124.92378973935));
#100261=CARTESIAN_POINT('Ctrl Pts',(4.7620124448452,-32.0506927672933,124.852567567313));
#100262=CARTESIAN_POINT('Ctrl Pts',(4.76588077896007,-32.0443428641056,
124.781576061288));
#100263=CARTESIAN_POINT('Ctrl Pts',(4.76974911307495,-32.0343563474446,
124.71122359149));
#100264=CARTESIAN_POINT('Ctrl Pts',(4.77204683224587,-32.0284245405993,
124.669435521025));
#100265=CARTESIAN_POINT('Ctrl Pts',(4.77434455141679,-32.0212106673077,
124.627872725201));
#100266=CARTESIAN_POINT('Ctrl Pts',(4.7766422705877,-32.0127377461674,124.586618423665));
#100267=CARTESIAN_POINT('Ctrl Pts',(4.78051134393591,-31.9984704006274,
124.517151310108));
#100268=CARTESIAN_POINT('Ctrl Pts',(4.78438041728412,-31.9805745320217,
124.448287625122));
#100269=CARTESIAN_POINT('Ctrl Pts',(4.78824949063234,-31.959116270389,124.380434828612));
#100270=CARTESIAN_POINT('Ctrl Pts',(4.79211279902812,-31.9376899817499,
124.31268313335));
#100271=CARTESIAN_POINT('Ctrl Pts',(4.7959761074239,-31.9127119815917,124.245939796136));
#100272=CARTESIAN_POINT('Ctrl Pts',(4.79983941581968,-31.8842993142417,
124.180601649472));
#100273=CARTESIAN_POINT('Ctrl Pts',(4.80369819231259,-31.8559199767311,
124.115340148548));
#100274=CARTESIAN_POINT('Ctrl Pts',(4.8075569688055,-31.8241141679269,124.051481007266));
#100275=CARTESIAN_POINT('Ctrl Pts',(4.8114157452984,-31.7890480327179,123.989403790266));
#100276=CARTESIAN_POINT('Ctrl Pts',(4.81527209088661,-31.7540039880429,
123.927365679911));
#100277=CARTESIAN_POINT('Ctrl Pts',(4.81912843647481,-31.7157039302298,
123.867107688676));
#100278=CARTESIAN_POINT('Ctrl Pts',(4.82298478206301,-31.6743605549191,
123.808986022487));
#100279=CARTESIAN_POINT('Ctrl Pts',(4.82683998830834,-31.633029394354,123.750881528127));
#100280=CARTESIAN_POINT('Ctrl Pts',(4.83069519455367,-31.588656982754,123.694912501405));
#100281=CARTESIAN_POINT('Ctrl Pts',(4.834550400799,-31.5414991148619,123.641405858477));
#100282=CARTESIAN_POINT('Ctrl Pts',(4.83840575765024,-31.4943394047199,
123.587897125281));
#100283=CARTESIAN_POINT('Ctrl Pts',(4.84226111450148,-31.4443943450995,
123.536851329846));
#100284=CARTESIAN_POINT('Ctrl Pts',(4.84611647135272,-31.3919586083017,
123.488560687532));
#100285=CARTESIAN_POINT('Ctrl Pts',(4.84997586382128,-31.33946798409,123.440219496705));
#100286=CARTESIAN_POINT('Ctrl Pts',(4.85383525628983,-31.28448183635,123.394639545819));
#100287=CARTESIAN_POINT('Ctrl Pts',(4.85769464875839,-31.2273294761779,
123.352074055242));
#100288=CARTESIAN_POINT('Ctrl Pts',(4.86155622636182,-31.1701447571263,
123.309484464671));
#100289=CARTESIAN_POINT('Ctrl Pts',(4.86541780396525,-31.1107917884811,
123.269913001621));
#100290=CARTESIAN_POINT('Ctrl Pts',(4.86927938156868,-31.0496282517474,
123.233569108164));
#100291=CARTESIAN_POINT('Ctrl Pts',(4.87314771568355,-30.9883576986132,
123.197161624652));
#100292=CARTESIAN_POINT('Ctrl Pts',(4.87701604979842,-30.9252706826861,
123.163993211673));
#100293=CARTESIAN_POINT('Ctrl Pts',(4.88088438391328,-30.8607481803879,
123.134226666377));
#100294=CARTESIAN_POINT('Ctrl Pts',(4.88318210308428,-30.8224230031699,
123.116545887067));
#100295=CARTESIAN_POINT('Ctrl Pts',(4.88547982225527,-30.7835917421951,
123.100064408499));
#100296=CARTESIAN_POINT('Ctrl Pts',(4.88777754142627,-30.7443367983746,
123.084808027094));
#100297=CARTESIAN_POINT('Ctrl Pts',(4.89164661477449,-30.6782363545784,
123.059118178033));
#100298=CARTESIAN_POINT('Ctrl Pts',(4.8955156881227,-30.6106748968161,123.036804087238));
#100299=CARTESIAN_POINT('Ctrl Pts',(4.89938476147092,-30.5420306164587,
123.018031187601));
#100300=CARTESIAN_POINT('Ctrl Pts',(4.90324806986671,-30.473488616667,122.999286259746));
#100301=CARTESIAN_POINT('Ctrl Pts',(4.90711137826249,-30.4038674616248,
122.984072176635));
#100302=CARTESIAN_POINT('Ctrl Pts',(4.91097468665827,-30.3335640282405,
122.972505831928));
#100303=CARTESIAN_POINT('Ctrl Pts',(4.91483346315119,-30.2633430651896,
122.960953055269));
#100304=CARTESIAN_POINT('Ctrl Pts',(4.9186922396441,-30.1924418905883,122.953039595899));
#100305=CARTESIAN_POINT('Ctrl Pts',(4.92255101613702,-30.1212695042463,
122.948831730491));
#100306=CARTESIAN_POINT('Ctrl Pts',(4.92640736172523,-30.0501419542116,
122.944626515902));
#100307=CARTESIAN_POINT('Ctrl Pts',(4.93026370731343,-29.9787440152017,
122.944122292457));
#100308=CARTESIAN_POINT('Ctrl Pts',(4.93412005290164,-29.9074903098065,
122.947333558583));
#100309=CARTESIAN_POINT('Ctrl Pts',(4.93797525914697,-29.836257656052,122.950543875952));
#100310=CARTESIAN_POINT('Ctrl Pts',(4.94183046539231,-29.765169636342,122.957467481741));
#100311=CARTESIAN_POINT('Ctrl Pts',(4.94568567163765,-29.6946396410606,
122.968066779225));
#100312=CARTESIAN_POINT('Ctrl Pts',(4.94954102848889,-29.6241068904833,
122.978666490777));
#100313=CARTESIAN_POINT('Ctrl Pts',(4.95339638534014,-29.5541326876791,
122.992942104738));
#100314=CARTESIAN_POINT('Ctrl Pts',(4.95725174219139,-29.485122355172,123.010804541188));
#100315=CARTESIAN_POINT('Ctrl Pts',(4.96111113465995,-29.4160397856961,
123.028685675248));
#100316=CARTESIAN_POINT('Ctrl Pts',(4.96497052712851,-29.3479235718333,
123.0501610047));
#100317=CARTESIAN_POINT('Ctrl Pts',(4.96882991959707,-29.2811650615572,
123.075091198583));
#100318=CARTESIAN_POINT('Ctrl Pts',(4.97269149720051,-29.2143687535318,
123.100035507597));
#100319=CARTESIAN_POINT('Ctrl Pts',(4.97655307480395,-29.1489321251938,
123.128438381514));
#100320=CARTESIAN_POINT('Ctrl Pts',(4.98041465240738,-29.0852251315536,
123.160112910378));
#100321=CARTESIAN_POINT('Ctrl Pts',(4.98428298652226,-29.0214066712862,
123.191842859419));
#100322=CARTESIAN_POINT('Ctrl Pts',(4.98815132063713,-28.9593243110815,
123.226855653503));
#100323=CARTESIAN_POINT('Ctrl Pts',(4.992019654752,-28.8993214518444,123.264919513069));
#100324=CARTESIAN_POINT('Ctrl Pts',(4.99431737392295,-28.8636808593086,
123.287528744135));
#100325=CARTESIAN_POINT('Ctrl Pts',(4.99661509309389,-28.8287733699115,
123.311213615859));
#100326=CARTESIAN_POINT('Ctrl Pts',(4.99891281226483,-28.7946653476448,
123.335918890699));
#100327=CARTESIAN_POINT('Ctrl Pts',(5.00275064676246,-28.7376953984201,
123.377183618458));
#100328=CARTESIAN_POINT('Ctrl Pts',(5.00658848126009,-28.6827265110721,
123.421464682555));
#100329=CARTESIAN_POINT('Ctrl Pts',(5.01042631575773,-28.6300997290133,
123.468539647901));
#100330=CARTESIAN_POINT('Ctrl Pts',(5.01432833257716,-28.5765928388979,
123.516401875068));
#100331=CARTESIAN_POINT('Ctrl Pts',(5.0182303493966,-28.5255075807009,123.567152086287));
#100332=CARTESIAN_POINT('Ctrl Pts',(5.02213236621603,-28.4771716630746,
123.620510449928));
#100333=CARTESIAN_POINT('Ctrl Pts',(5.02595997436974,-28.4297574767744,
123.672851307796));
#100334=CARTESIAN_POINT('Ctrl Pts',(5.02978758252346,-28.3849890497211,
123.727701341682));
#100335=CARTESIAN_POINT('Ctrl Pts',(5.03361519067717,-28.3431406316792,
123.784757392079));
#100336=CARTESIAN_POINT('Ctrl Pts',(5.03744050268937,-28.3013173180592,
123.841779215156));
#100337=CARTESIAN_POINT('Ctrl Pts',(5.04126581470156,-28.2624108313477,
123.901004032373));
#100338=CARTESIAN_POINT('Ctrl Pts',(5.04509112671375,-28.2266549764506,
123.962095866685));
#100339=CARTESIAN_POINT('Ctrl Pts',(5.04891547573735,-28.190908122775,124.023172321666));
#100340=CARTESIAN_POINT('Ctrl Pts',(5.05273982476093,-28.1583105759944,
124.086114434041));
#100341=CARTESIAN_POINT('Ctrl Pts',(5.05656417378453,-28.1290516520466,
124.150559100472));
#100342=CARTESIAN_POINT('Ctrl Pts',(5.06052338592116,-28.0987609316954,
124.217276365006));
#100343=CARTESIAN_POINT('Ctrl Pts',(5.0644825980578,-28.0720489807084,124.285603645032));
#100344=CARTESIAN_POINT('Ctrl Pts',(5.06844181019444,-28.0490719088951,
124.355114625815));
#100345=CARTESIAN_POINT('Ctrl Pts',(5.07227054686676,-28.0268520443266,
124.422334878751));
#100346=CARTESIAN_POINT('Ctrl Pts',(5.07609928353908,-28.008124787048,124.490661515232));
#100347=CARTESIAN_POINT('Ctrl Pts',(5.0799280202114,-27.9929800396067,124.559695058984));
#100348=CARTESIAN_POINT('Ctrl Pts',(5.08395247008019,-27.9770611394396,
124.632257384334));
#100349=CARTESIAN_POINT('Ctrl Pts',(5.08797691994899,-27.9651009153752,
124.705600206819));
#100350=CARTESIAN_POINT('Ctrl Pts',(5.09200136981778,-27.9571422025377,
124.779252221195));
#100351=CARTESIAN_POINT('Ctrl Pts',(5.09602581968658,-27.9491834897002,
124.85290423557));
#100352=CARTESIAN_POINT('Ctrl Pts',(5.10005026955537,-27.9452262438764,
124.926864812609));
#100353=CARTESIAN_POINT('Ctrl Pts',(5.10407471942417,-27.9452501074214,
125.000664415721));
#100354=CARTESIAN_POINT('Ctrl Pts',(5.10407471946233,-27.9452501074216,
125.000664416421));
#100355=CARTESIAN_POINT('Ctrl Pts',(5.10606584067601,-27.9452619140691,
125.037177221924));
#100356=CARTESIAN_POINT('Ctrl Pts',(5.1080569618897,-27.9462469037348,125.073673053094));
#100357=CARTESIAN_POINT('Ctrl Pts',(5.11004808310338,-27.9482027488899,
125.110116315035));
#100358=CARTESIAN_POINT('Ctrl Pts',(5.1139171564516,-27.9520032751013,125.180931518313));
#100359=CARTESIAN_POINT('Ctrl Pts',(5.11778622979981,-27.9594816959999,
125.251688443372));
#100360=CARTESIAN_POINT('Ctrl Pts',(5.12165530314802,-27.9706330803799,
125.32197432825));
#100361=CARTESIAN_POINT('Ctrl Pts',(5.1255186115438,-27.9817678491017,125.392155486556));
#100362=CARTESIAN_POINT('Ctrl Pts',(5.12938191993959,-27.9965646425544,
125.461866521965));
#100363=CARTESIAN_POINT('Ctrl Pts',(5.13324522833537,-28.0149666018931,
125.53069762662));
#100364=CARTESIAN_POINT('Ctrl Pts',(5.13710400482828,-28.0333469745802,
125.599447988075));
#100365=CARTESIAN_POINT('Ctrl Pts',(5.14096278132119,-28.0553239878999,
125.667320002076));
#100366=CARTESIAN_POINT('Ctrl Pts',(5.1448215578141,-28.0807896635756,125.733913650957));
#100367=CARTESIAN_POINT('Ctrl Pts',(5.1486779034023,-28.1062392966971,125.800465347988));
#100368=CARTESIAN_POINT('Ctrl Pts',(5.15253424899051,-28.1351730587823,
125.865739824989));
#100369=CARTESIAN_POINT('Ctrl Pts',(5.15639059457871,-28.1674334698241,
125.929353256291));
#100370=CARTESIAN_POINT('Ctrl Pts',(5.16024580082404,-28.1996843496481,
125.992947893243));
#100371=CARTESIAN_POINT('Ctrl Pts',(5.16410100706936,-28.2352597076084,
126.05488202575));
#100372=CARTESIAN_POINT('Ctrl Pts',(5.16795621331469,-28.2739550952365,
126.114794397743));
#100373=CARTESIAN_POINT('Ctrl Pts',(5.17181157016593,-28.3126519945229,
126.174709110249));
#100374=CARTESIAN_POINT('Ctrl Pts',(5.17566692701717,-28.3544689000543,
126.232601498555));
#100375=CARTESIAN_POINT('Ctrl Pts',(5.17952228386841,-28.3991577667119,
126.288138853781));
#100376=CARTESIAN_POINT('Ctrl Pts',(5.18338167633697,-28.4438934117017,
126.343734343059));
#100377=CARTESIAN_POINT('Ctrl Pts',(5.18724106880552,-28.4915067137853,
126.396969499025));
#100378=CARTESIAN_POINT('Ctrl Pts',(5.19110046127408,-28.5417095857691,
126.447545035659));
#100379=CARTESIAN_POINT('Ctrl Pts',(5.19496203887751,-28.5919408819278,
126.498149207466));
#100380=CARTESIAN_POINT('Ctrl Pts',(5.19882361648094,-28.6447643068021,
126.546090435647));
#100381=CARTESIAN_POINT('Ctrl Pts',(5.20268519408437,-28.699857220266,126.591108517608));
#100382=CARTESIAN_POINT('Ctrl Pts',(5.20655352819924,-28.7550465285039,
126.636205366648));
#100383=CARTESIAN_POINT('Ctrl Pts',(5.2104218623141,-28.8125128614944,126.678368570638));
#100384=CARTESIAN_POINT('Ctrl Pts',(5.21429019642897,-28.8719036200696,
126.717380598495));
#100385=CARTESIAN_POINT('Ctrl Pts',(5.21658791559996,-28.907180636094,126.740553024052));
#100386=CARTESIAN_POINT('Ctrl Pts',(5.21888563477095,-28.9431361072491,
126.762614530318));
#100387=CARTESIAN_POINT('Ctrl Pts',(5.22118335394194,-28.9796923731626,
126.783527378292));
#100388=CARTESIAN_POINT('Ctrl Pts',(5.22505242729016,-29.0412485789611,
126.818742013638));
#100389=CARTESIAN_POINT('Ctrl Pts',(5.22892150063837,-29.1047505806774,
126.85083508144));
#100390=CARTESIAN_POINT('Ctrl Pts',(5.23279057398659,-29.1698489244986,
126.879586857356));
#100391=CARTESIAN_POINT('Ctrl Pts',(5.23665388238237,-29.2348502712299,
126.908295792879));
#100392=CARTESIAN_POINT('Ctrl Pts',(5.24051719077816,-29.3014427979312,
126.933673124138));
#100393=CARTESIAN_POINT('Ctrl Pts',(5.24438049917394,-29.3692513689759,
126.955544355662));
#100394=CARTESIAN_POINT('Ctrl Pts',(5.24823927566686,-29.4369803963171,
126.977389930861));
#100395=CARTESIAN_POINT('Ctrl Pts',(5.25209805215977,-29.50592217441,126.995737427486));
#100396=CARTESIAN_POINT('Ctrl Pts',(5.25595682865268,-29.5756820674499,
127.010460607576));
#100397=CARTESIAN_POINT('Ctrl Pts',(5.25981317424089,-29.6453980140077,
127.025174512538));
#100398=CARTESIAN_POINT('Ctrl Pts',(5.2636695198291,-29.7159305788037,127.036268530721));
#100399=CARTESIAN_POINT('Ctrl Pts',(5.2675258654173,-29.7868718816748,127.04366679468));
#100400=CARTESIAN_POINT('Ctrl Pts',(5.27138107166264,-29.8577922252035,
127.051062872851));
#100401=CARTESIAN_POINT('Ctrl Pts',(5.27523627790797,-29.9291205841626,
127.054765314154));
#100402=CARTESIAN_POINT('Ctrl Pts',(5.2790914841533,-30.0004425660865,127.054749952339));
#100403=CARTESIAN_POINT('Ctrl Pts',(5.28294684100455,-30.0717673342459,
127.054734589923));
#100404=CARTESIAN_POINT('Ctrl Pts',(5.28680219785579,-30.14308523909,127.051001138343));
#100405=CARTESIAN_POINT('Ctrl Pts',(5.29065755470704,-30.2139822266315,
127.04357754176));
#100406=CARTESIAN_POINT('Ctrl Pts',(5.2945169471756,-30.2849534260089,127.036146174484));
#100407=CARTESIAN_POINT('Ctrl Pts',(5.29837633964416,-30.3555023444172,
127.02501700212));
#100408=CARTESIAN_POINT('Ctrl Pts',(5.30223573211272,-30.4252212904861,
127.010269737278));
#100409=CARTESIAN_POINT('Ctrl Pts',(5.30609730971616,-30.4949797104624,
126.995514122738));
#100410=CARTESIAN_POINT('Ctrl Pts',(5.30995888731959,-30.5639067530251,
126.977136462971));
#100411=CARTESIAN_POINT('Ctrl Pts',(5.31382046492303,-30.631608822224,126.955266697458));
#100412=CARTESIAN_POINT('Ctrl Pts',(5.3176887990379,-30.6994293481398,126.933358666931));
#100413=CARTESIAN_POINT('Ctrl Pts',(5.32155713315277,-30.7660201675122,
126.907946505012));
#100414=CARTESIAN_POINT('Ctrl Pts',(5.32542546726764,-30.8310072858771,
126.879208464572));
#100415=CARTESIAN_POINT('Ctrl Pts',(5.32772318643859,-30.8696084364752,
126.862138598192));
#100416=CARTESIAN_POINT('Ctrl Pts',(5.33002090560955,-30.9076442250829,
126.843896209379));
#100417=CARTESIAN_POINT('Ctrl Pts',(5.3323186247805,-30.9450408253262,126.824526075716));
#100418=CARTESIAN_POINT('Ctrl Pts',(5.33618678852257,-31.0079972453129,
126.791916847547));
#100419=CARTESIAN_POINT('Ctrl Pts',(5.34005495226464,-31.0693871678518,
126.755981411747));
#100420=CARTESIAN_POINT('Ctrl Pts',(5.34392311600671,-31.1288367232353,
126.71689406044));
#100421=CARTESIAN_POINT('Ctrl Pts',(5.34666123617927,-31.1709187129596,
126.689225669896));
#100422=CARTESIAN_POINT('Ctrl Pts',(5.34939935635183,-31.2120287653956,
126.659979003999));
#100423=CARTESIAN_POINT('Ctrl Pts',(5.35213747652439,-31.2520409112987,
126.629230222815));
#100424=CARTESIAN_POINT('',(5.04592528049234,-27.9452502582983,124.998969719981));
#100425=CARTESIAN_POINT('Ctrl Pts',(5.04592528053768,-27.9452502582979,
124.998969720821));
#100426=CARTESIAN_POINT('Ctrl Pts',(5.04983580638859,-27.9452139274514,
125.071426584004));
#100427=CARTESIAN_POINT('Ctrl Pts',(5.0537463322395,-27.9490145212745,125.143878332677));
#100428=CARTESIAN_POINT('Ctrl Pts',(5.05765685809041,-27.9566240457995,
125.215898754732));
#100429=CARTESIAN_POINT('Ctrl Pts',(5.0615688975846,-27.9642365157353,125.28794705366));
#100430=CARTESIAN_POINT('Ctrl Pts',(5.0654809370788,-27.9756607961671,125.359563230795));
#100431=CARTESIAN_POINT('Ctrl Pts',(5.06939297657299,-27.9908172317787,
125.430327975366));
#100432=CARTESIAN_POINT('Ctrl Pts',(5.0733108311932,-28.0059961969642,125.501197909546));
#100433=CARTESIAN_POINT('Ctrl Pts',(5.07722868581341,-28.0249182944708,
125.571213427755));
#100434=CARTESIAN_POINT('Ctrl Pts',(5.08114654043362,-28.0474531999294,
125.639967621083));
#100435=CARTESIAN_POINT('Ctrl Pts',(5.08506751736911,-28.070006064472,125.708776607732));
#100436=CARTESIAN_POINT('Ctrl Pts',(5.08898849430461,-28.0961773017068,
125.776321833245));
#100437=CARTESIAN_POINT('Ctrl Pts',(5.09290947124011,-28.1257883534147,
125.842216282379));
#100438=CARTESIAN_POINT('Ctrl Pts',(5.09683849198269,-28.1554601516131,
125.908245912679));
#100439=CARTESIAN_POINT('Ctrl Pts',(5.10076751272527,-28.188585645451,125.972617587755));
#100440=CARTESIAN_POINT('Ctrl Pts',(5.10469653346786,-28.2249403918814,
126.034969057569));
#100441=CARTESIAN_POINT('Ctrl Pts',(5.10720517516982,-28.2481525454776,
126.074779867337));
#100442=CARTESIAN_POINT('Ctrl Pts',(5.10971381687178,-28.272680273511,126.113767668478));
#100443=CARTESIAN_POINT('Ctrl Pts',(5.11222245857374,-28.2984564079792,
126.151845027316));
#100444=CARTESIAN_POINT('Ctrl Pts',(5.11609153192196,-28.3382108913768,
126.210571665775));
#100445=CARTESIAN_POINT('Ctrl Pts',(5.11996060527017,-28.3810871266736,
126.267352804102));
#100446=CARTESIAN_POINT('Ctrl Pts',(5.12382967861839,-28.4268681537416,
126.321837265622));
#100447=CARTESIAN_POINT('Ctrl Pts',(5.12769298701418,-28.472580966687,126.376240544828));
#100448=CARTESIAN_POINT('Ctrl Pts',(5.13155629540996,-28.5211896701545,
126.428353571045));
#100449=CARTESIAN_POINT('Ctrl Pts',(5.13541960380575,-28.5724343269203,
126.477854462234));
#100450=CARTESIAN_POINT('Ctrl Pts',(5.13927838029866,-28.623618870492,126.527297285775));
#100451=CARTESIAN_POINT('Ctrl Pts',(5.14313715679158,-28.6774328776293,
126.574133724953));
#100452=CARTESIAN_POINT('Ctrl Pts',(5.14699593328449,-28.7335776498747,
126.618076634033));
#100453=CARTESIAN_POINT('Ctrl Pts',(5.1508522788727,-28.7896870527247,126.661991860498));
#100454=CARTESIAN_POINT('Ctrl Pts',(5.1547086244609,-28.848123925943,126.703016874631));
#100455=CARTESIAN_POINT('Ctrl Pts',(5.15856497004911,-28.9085554955759,
126.740903919308));
#100456=CARTESIAN_POINT('Ctrl Pts',(5.16242017629445,-28.9689692109278,
126.7787797704));
#100457=CARTESIAN_POINT('Ctrl Pts',(5.16627538253979,-29.0313760413579,
126.813519234689));
#100458=CARTESIAN_POINT('Ctrl Pts',(5.17013058878512,-29.0954145952796,
126.84491810335));
#100459=CARTESIAN_POINT('Ctrl Pts',(5.17398594563638,-29.1594556509053,
126.876318198626));
#100460=CARTESIAN_POINT('Ctrl Pts',(5.17784130248763,-29.2251281194314,
126.904377227293));
#100461=CARTESIAN_POINT('Ctrl Pts',(5.18169665933888,-29.2920479619282,
126.928937913539));
#100462=CARTESIAN_POINT('Ctrl Pts',(5.18555605180745,-29.3590378531612,
126.953524308828));
#100463=CARTESIAN_POINT('Ctrl Pts',(5.18941544427601,-29.4272772678516,
126.974604883981));
#100464=CARTESIAN_POINT('Ctrl Pts',(5.19327483674457,-29.4963650787203,
126.992071642428));
#100465=CARTESIAN_POINT('Ctrl Pts',(5.19713641434801,-29.5654920061563,
127.009548290314));
#100466=CARTESIAN_POINT('Ctrl Pts',(5.20099799195145,-29.6354678092435,
127.023406953932));
#100467=CARTESIAN_POINT('Ctrl Pts',(5.20485956955489,-29.7058818937099,
127.033590937739));
#100468=CARTESIAN_POINT('Ctrl Pts',(5.20872790366976,-29.7764191800424,
127.043792740222));
#100469=CARTESIAN_POINT('Ctrl Pts',(5.21259623778464,-29.8473957948873,
127.050306981797));
#100470=CARTESIAN_POINT('Ctrl Pts',(5.21646457189951,-29.9183974630044,
127.053128975115));
#100471=CARTESIAN_POINT('Ctrl Pts',(5.21876229107044,-29.9605711453068,
127.054805187137));
#100472=CARTESIAN_POINT('Ctrl Pts',(5.22106001024137,-30.0027536735455,
127.055179721477));
#100473=CARTESIAN_POINT('Ctrl Pts',(5.2233577294123,-30.0448590459357,127.054260263087));
#100474=CARTESIAN_POINT('Ctrl Pts',(5.22722618552696,-30.1157479462608,
127.052712256491));
#100475=CARTESIAN_POINT('Ctrl Pts',(5.23109464164162,-30.1866954545005,
127.047487535505));
#100476=CARTESIAN_POINT('Ctrl Pts',(5.23496309775628,-30.2572890582151,
127.038577911933));
#100477=CARTESIAN_POINT('Ctrl Pts',(5.23882613528354,-30.327783780722,127.029680768166));
#100478=CARTESIAN_POINT('Ctrl Pts',(5.2426891728108,-30.3979251045115,127.017109022759));
#100479=CARTESIAN_POINT('Ctrl Pts',(5.24655221033805,-30.4673017077463,
127.00090646369));
#100480=CARTESIAN_POINT('Ctrl Pts',(5.25049621378875,-30.5381323845454,
126.984364313005));
#100481=CARTESIAN_POINT('Ctrl Pts',(5.25444021723945,-30.6081654024678,
126.964037416808));
#100482=CARTESIAN_POINT('Ctrl Pts',(5.25838422069015,-30.6769703293199,
126.940028024468));
#100483=CARTESIAN_POINT('Ctrl Pts',(5.26224043473793,-30.7442437302688,
126.916553056158));
#100484=CARTESIAN_POINT('Ctrl Pts',(5.2660966487857,-30.8103426711026,126.889558020767));
#100485=CARTESIAN_POINT('Ctrl Pts',(5.26995286283347,-30.8748789361614,
126.859189180681));
#100486=CARTESIAN_POINT('Ctrl Pts',(5.27394076098563,-30.9416190208629,
126.827783288849));
#100487=CARTESIAN_POINT('Ctrl Pts',(5.2779286591378,-31.0066872487866,126.792769156818));
#100488=CARTESIAN_POINT('Ctrl Pts',(5.28191655728996,-31.069677830906,126.754362248958));
#100489=CARTESIAN_POINT('Ctrl Pts',(5.28590445544213,-31.1326684130254,
126.715955341098));
#100490=CARTESIAN_POINT('Ctrl Pts',(5.28989235359429,-31.1935808619265,
126.674155962877));
#100491=CARTESIAN_POINT('Ctrl Pts',(5.29388025174645,-31.2520409112987,
126.629230222815));
#100492=CARTESIAN_POINT('Ctrl Pts',(4.59397334877082,-31.2520409112987,
126.629230222815));
#100493=CARTESIAN_POINT('Ctrl Pts',(4.59782931900108,-31.3085491042728,
126.585804457422));
#100494=CARTESIAN_POINT('Ctrl Pts',(4.60168528923134,-31.3628309656863,
126.53940800709));
#100495=CARTESIAN_POINT('Ctrl Pts',(4.6055412594616,-31.4145649577858,126.490303171407));
#100496=CARTESIAN_POINT('Ctrl Pts',(4.60939638628394,-31.4662876342226,
126.441209076316));
#100497=CARTESIAN_POINT('Ctrl Pts',(4.61325151310627,-31.5154631958829,
126.389408106701));
#100498=CARTESIAN_POINT('Ctrl Pts',(4.61710663992861,-31.5618054085364,
126.335200894385));
#100499=CARTESIAN_POINT('Ctrl Pts',(4.62096221310461,-31.6081529867762,
126.280987405859));
#100500=CARTESIAN_POINT('Ctrl Pts',(4.6248177862806,-31.6516662510474,126.224367492432));
#100501=CARTESIAN_POINT('Ctrl Pts',(4.6286733594566,-31.6920989987525,126.16567514382));
#100502=CARTESIAN_POINT('Ctrl Pts',(4.63253315030944,-31.7325759765256,
126.106918590654));
#100503=CARTESIAN_POINT('Ctrl Pts',(4.63639294116229,-31.769965437958,126.046085479588));
#100504=CARTESIAN_POINT('Ctrl Pts',(4.64025273201513,-31.804064848595,125.983538298473));
#100505=CARTESIAN_POINT('Ctrl Pts',(4.64411497375936,-31.838185911688,125.920951401127));
#100506=CARTESIAN_POINT('Ctrl Pts',(4.64797721550358,-31.869012557114,125.856648705859));
#100507=CARTESIAN_POINT('Ctrl Pts',(4.65183945724781,-31.8963897053691,
125.791014315844));
#100508=CARTESIAN_POINT('Ctrl Pts',(4.65570819014413,-31.9238128655636,
125.725269616109));
#100509=CARTESIAN_POINT('Ctrl Pts',(4.65957692304045,-31.9477747978071,
125.658189212644));
#100510=CARTESIAN_POINT('Ctrl Pts',(4.66344565593677,-31.9681699974544,
125.59017321493));
#100511=CARTESIAN_POINT('Ctrl Pts',(4.66485756236435,-31.9756132907097,
125.565350559315));
#100512=CARTESIAN_POINT('Ctrl Pts',(4.66626946879192,-31.9825820204718,
125.540403390991));
#100513=CARTESIAN_POINT('Ctrl Pts',(4.66768137521949,-31.9890727647972,
125.515351432366));
#100514=CARTESIAN_POINT('Ctrl Pts',(4.6715504485677,-32.0068594717552,125.446701085897));
#100515=CARTESIAN_POINT('Ctrl Pts',(4.67541952191591,-32.0211227752711,
125.376994361718));
#100516=CARTESIAN_POINT('Ctrl Pts',(4.67928859526412,-32.0317425864935,
125.306626197068));
#100517=CARTESIAN_POINT('Ctrl Pts',(4.6831519036599,-32.0423465741063,125.236362881587));
#100518=CARTESIAN_POINT('Ctrl Pts',(4.68701521205567,-32.0493177736078,
125.165440558361));
#100519=CARTESIAN_POINT('Ctrl Pts',(4.69087852045145,-32.0525864868933,
125.094267047917));
#100520=CARTESIAN_POINT('Ctrl Pts',(4.69473729694436,-32.0558513657733,
125.023177028461));
#100521=CARTESIAN_POINT('Ctrl Pts',(4.69859607343727,-32.0554223634192,
124.951836889997));
#100522=CARTESIAN_POINT('Ctrl Pts',(4.70245484993018,-32.0512814688225,
124.880660575813));
#100523=CARTESIAN_POINT('Ctrl Pts',(4.70631119551838,-32.0471431828559,
124.809529100411));
#100524=CARTESIAN_POINT('Ctrl Pts',(4.71016754110659,-32.0392976720872,
124.738561728352));
#100525=CARTESIAN_POINT('Ctrl Pts',(4.71402388669479,-32.0277790060476,
124.668171934381));
#100526=CARTESIAN_POINT('Ctrl Pts',(4.71787909294012,-32.0162637431547,
124.597802936811));
#100527=CARTESIAN_POINT('Ctrl Pts',(4.72173429918545,-32.0010775578613,
124.528011657702));
#100528=CARTESIAN_POINT('Ctrl Pts',(4.72558950543078,-31.9823061136397,
124.459204258221));
#100529=CARTESIAN_POINT('Ctrl Pts',(4.72944486228203,-31.9635339361005,
124.390394170738));
#100530=CARTESIAN_POINT('Ctrl Pts',(4.73330021913327,-31.9411763515422,
124.32256850727));
#100531=CARTESIAN_POINT('Ctrl Pts',(4.73715557598452,-31.9153692105439,
124.256119398155));
#100532=CARTESIAN_POINT('Ctrl Pts',(4.74101496845307,-31.8895350557699,
124.189600733047));
#100533=CARTESIAN_POINT('Ctrl Pts',(4.74487436092163,-31.8602443127305,
124.124461952446));
#100534=CARTESIAN_POINT('Ctrl Pts',(4.74873375339018,-31.8276811049247,
124.0610754337));
#100535=CARTESIAN_POINT('Ctrl Pts',(4.75259533099361,-31.795099460279,123.997653026381));
#100536=CARTESIAN_POINT('Ctrl Pts',(4.75645690859704,-31.7592419067682,
123.935985276047));
#100537=CARTESIAN_POINT('Ctrl Pts',(4.76031848620047,-31.7203373198838,
123.876417751869));
#100538=CARTESIAN_POINT('Ctrl Pts',(4.76418682031534,-31.6813646625594,
123.816746003796));
#100539=CARTESIAN_POINT('Ctrl Pts',(4.76805515443021,-31.6393346142748,
123.759182211015));
#100540=CARTESIAN_POINT('Ctrl Pts',(4.77192348854507,-31.5945175083752,
123.704040325479));
#100541=CARTESIAN_POINT('Ctrl Pts',(4.77422120771607,-31.5678969734483,
123.671287061733));
#100542=CARTESIAN_POINT('Ctrl Pts',(4.77651892688706,-31.5402938708374,
123.639387615172));
#100543=CARTESIAN_POINT('Ctrl Pts',(4.77881664605806,-31.5117708171909,
123.60840143763));
#100544=CARTESIAN_POINT('Ctrl Pts',(4.78268571940627,-31.4637415418702,
123.556224567975));
#100545=CARTESIAN_POINT('Ctrl Pts',(4.78655479275449,-31.4129137901362,
123.506434921696));
#100546=CARTESIAN_POINT('Ctrl Pts',(4.7904238661027,-31.359554234086,123.459347590441));
#100547=CARTESIAN_POINT('Ctrl Pts',(4.79428717449849,-31.3062741842313,
123.412330419714));
#100548=CARTESIAN_POINT('Ctrl Pts',(4.79815048289428,-31.2504701794633,
123.368007890384));
#100549=CARTESIAN_POINT('Ctrl Pts',(4.80201379129007,-31.1924470458218,
123.326659746073));
#100550=CARTESIAN_POINT('Ctrl Pts',(4.80587256778298,-31.1344919769526,
123.285360105728));
#100551=CARTESIAN_POINT('Ctrl Pts',(4.8097313442759,-31.0743233436928,123.247028200339));
#100552=CARTESIAN_POINT('Ctrl Pts',(4.81359012076881,-31.0122791493048,
123.211903669714));
#100553=CARTESIAN_POINT('Ctrl Pts',(4.81744646635702,-30.9502740407578,
123.17680126641));
#100554=CARTESIAN_POINT('Ctrl Pts',(4.82130281194522,-30.8863961369886,
123.144902467902));
#100555=CARTESIAN_POINT('Ctrl Pts',(4.82515915753343,-30.8210112942298,
123.116402904747));
#100556=CARTESIAN_POINT('Ctrl Pts',(4.82901436377876,-30.7556457691782,
123.08791176168));
#100557=CARTESIAN_POINT('Ctrl Pts',(4.83286957002409,-30.6887746341,123.062818054167));
#100558=CARTESIAN_POINT('Ctrl Pts',(4.83672477626942,-30.6207855834735,
123.041270099822));
#100559=CARTESIAN_POINT('Ctrl Pts',(4.84058013312067,-30.5527938768144,
123.019721303693));
#100560=CARTESIAN_POINT('Ctrl Pts',(4.84443548997193,-30.4836846316522,
123.001718680408));
#100561=CARTESIAN_POINT('Ctrl Pts',(4.84829084682318,-30.4138609742382,
122.987360773387));
#100562=CARTESIAN_POINT('Ctrl Pts',(4.85215023929174,-30.3439642285028,
122.972987837143));
#100563=CARTESIAN_POINT('Ctrl Pts',(4.8560096317603,-30.2733520545136,122.962267331063));
#100564=CARTESIAN_POINT('Ctrl Pts',(4.85986902422886,-30.2024371646756,
122.955246529075));
#100565=CARTESIAN_POINT('Ctrl Pts',(4.86373060183231,-30.1314821238033,
122.948221752007));
#100566=CARTESIAN_POINT('Ctrl Pts',(4.86759217943575,-30.0602245113797,
122.944900871601));
#100567=CARTESIAN_POINT('Ctrl Pts',(4.87145375703919,-29.9890787889625,
122.945279023894));
#100568=CARTESIAN_POINT('Ctrl Pts',(4.87532209115406,-29.9178085845495,
122.945657837831));
#100569=CARTESIAN_POINT('Ctrl Pts',(4.87919042526894,-29.8466511461452,
122.949748578334));
#100570=CARTESIAN_POINT('Ctrl Pts',(4.88305875938381,-29.7760168575574,
122.957494402847));
#100571=CARTESIAN_POINT('Ctrl Pts',(4.88535647855474,-29.7340613919243,
122.962095279852));
#100572=CARTESIAN_POINT('Ctrl Pts',(4.88765419772568,-29.6922903458753,
122.967984734544));
#100573=CARTESIAN_POINT('Ctrl Pts',(4.88995191689662,-29.6507876285087,
122.975142404489));
#100574=CARTESIAN_POINT('Ctrl Pts',(4.89382099024483,-29.580902213584,122.987195030576));
#100575=CARTESIAN_POINT('Ctrl Pts',(4.89769006359304,-29.5115046159004,
123.002893522819));
#100576=CARTESIAN_POINT('Ctrl Pts',(4.90155913694124,-29.4430041910452,
123.022184732765));
#100577=CARTESIAN_POINT('Ctrl Pts',(4.90542244533703,-29.3746058324097,
123.041447198644));
#100578=CARTESIAN_POINT('Ctrl Pts',(4.90928575373282,-29.307102456889,123.064291625702));
#100579=CARTESIAN_POINT('Ctrl Pts',(4.91314906212861,-29.2408944159804,
123.0906136392));
#100580=CARTESIAN_POINT('Ctrl Pts',(4.91700783862152,-29.1747640412533,
123.116904775326));
#100581=CARTESIAN_POINT('Ctrl Pts',(4.92086661511442,-29.109926432108,123.146665216171));
#100582=CARTESIAN_POINT('Ctrl Pts',(4.92472539160733,-29.0467662412132,
123.179740962498));
#100583=CARTESIAN_POINT('Ctrl Pts',(4.92858173719554,-28.9836458392011,
123.212795872171));
#100584=CARTESIAN_POINT('Ctrl Pts',(4.93243808278374,-28.9222011882553,
123.249161718872));
#100585=CARTESIAN_POINT('Ctrl Pts',(4.93629442837195,-28.8627950734066,
123.28863723383));
#100586=CARTESIAN_POINT('Ctrl Pts',(4.94014963461728,-28.8034065098723,
123.328101085896));
#100587=CARTESIAN_POINT('Ctrl Pts',(4.94400484086261,-28.7460556911284,
123.370672513553));
#100588=CARTESIAN_POINT('Ctrl Pts',(4.94786004710794,-28.6910774968249,
123.416106239932));
#100589=CARTESIAN_POINT('Ctrl Pts',(4.95171540395919,-28.6360971547655,
123.461541741206));
#100590=CARTESIAN_POINT('Ctrl Pts',(4.95557076081044,-28.5834899942288,
123.509839452046));
#100591=CARTESIAN_POINT('Ctrl Pts',(4.9594261176617,-28.5335574470371,123.560714134941));
#100592=CARTESIAN_POINT('Ctrl Pts',(4.96328551013025,-28.48357263266,123.611642071207));
#100593=CARTESIAN_POINT('Ctrl Pts',(4.9671449025988,-28.4362683613671,123.665152016857));
#100594=CARTESIAN_POINT('Ctrl Pts',(4.97100429506736,-28.3919081904316,
123.720922873905));
#100595=CARTESIAN_POINT('Ctrl Pts',(4.97486587267079,-28.3475229033782,
123.776725307644));
#100596=CARTESIAN_POINT('Ctrl Pts',(4.97872745027421,-28.3060853173045,
123.834790805449));
#100597=CARTESIAN_POINT('Ctrl Pts',(4.98258902787764,-28.2678161348464,
123.894768522073));
#100598=CARTESIAN_POINT('Ctrl Pts',(4.9864573619925,-28.2294799937006,123.954851180295));
#100599=CARTESIAN_POINT('Ctrl Pts',(4.99032569610737,-28.1943235639811,
124.016852314539));
#100600=CARTESIAN_POINT('Ctrl Pts',(4.99419403022223,-28.1625216672204,
124.08039631413));
#100601=CARTESIAN_POINT('Ctrl Pts',(4.99649174939321,-28.1436319266522,
124.118140278774));
#100602=CARTESIAN_POINT('Ctrl Pts',(4.99878946856419,-28.1259247988859,
124.156428182751));
#100603=CARTESIAN_POINT('Ctrl Pts',(5.00108718773517,-28.1094286858362,
124.19517848652));
#100604=CARTESIAN_POINT('Ctrl Pts',(5.00537446195644,-28.0786488755259,
124.267482004074));
#100605=CARTESIAN_POINT('Ctrl Pts',(5.0096617361777,-28.0519849253725,124.341637213734));
#100606=CARTESIAN_POINT('Ctrl Pts',(5.01394901039897,-28.0296387343031,
124.417184381523));
#100607=CARTESIAN_POINT('Ctrl Pts',(5.0182226207556,-28.0073637622213,124.492490774819));
#100608=CARTESIAN_POINT('Ctrl Pts',(5.02249623111224,-27.9893792307952,
124.569180004692));
#100609=CARTESIAN_POINT('Ctrl Pts',(5.02676984146888,-27.9758386929301,
124.646774058907));
#100610=CARTESIAN_POINT('Ctrl Pts',(5.03102083154993,-27.9623698253093,
124.723957406777));
#100611=CARTESIAN_POINT('Ctrl Pts',(5.03527182163098,-27.9532981584284,
124.802035744073));
#100612=CARTESIAN_POINT('Ctrl Pts',(5.03952281171203,-27.9487267011562,
124.880520227861));
#100613=CARTESIAN_POINT('Ctrl Pts',(5.04165696797213,-27.9464316583616,
124.919922378702));
#100614=CARTESIAN_POINT('Ctrl Pts',(5.04379112423223,-27.9452700857511,
124.959426631904));
#100615=CARTESIAN_POINT('Ctrl Pts',(5.04592528049234,-27.9452502582983,
124.998969719981));
#100616=CARTESIAN_POINT('Origin',(-1.54592528053767,-30.,125.));
#100617=CARTESIAN_POINT('',(3.89394636911841,-31.2520409112987,126.629230222815));
#100618=CARTESIAN_POINT('',(3.95204573383007,-31.2520409112987,126.629230222815));
#100619=CARTESIAN_POINT('',(-1.54592528053767,-31.2520409112987,126.629230222815));
#100620=CARTESIAN_POINT('',(4.40407471951209,-27.9452505182989,125.001459434549));
#100621=CARTESIAN_POINT('Ctrl Pts',(3.95204573383007,-31.2520409112987,
126.629230222815));
#100622=CARTESIAN_POINT('Ctrl Pts',(3.95593320390404,-31.3090533867716,
126.585416923291));
#100623=CARTESIAN_POINT('Ctrl Pts',(3.95982067397802,-31.3637452867511,
126.538621370544));
#100624=CARTESIAN_POINT('Ctrl Pts',(3.963708144052,-31.4158013611643,126.489128627159));
#100625=CARTESIAN_POINT('Ctrl Pts',(3.96756865463629,-31.467496428245,126.439979114482));
#100626=CARTESIAN_POINT('Ctrl Pts',(3.97142916522058,-31.5165918191422,
126.388170101277));
#100627=CARTESIAN_POINT('Ctrl Pts',(3.97528967580487,-31.5628172576812,
126.334016409792));
#100628=CARTESIAN_POINT('Ctrl Pts',(3.97919062562369,-31.6095269123127,
126.279295452971));
#100629=CARTESIAN_POINT('Ctrl Pts',(3.98309157544251,-31.6533058234712,
126.222180809079));
#100630=CARTESIAN_POINT('Ctrl Pts',(3.98699252526133,-31.6939194848657,
126.16302809136));
#100631=CARTESIAN_POINT('Ctrl Pts',(3.99089347508015,-31.7345331462603,
126.10387537364));
#100632=CARTESIAN_POINT('Ctrl Pts',(3.99479442489897,-31.7719813499103,
126.042685046445));
#100633=CARTESIAN_POINT('Ctrl Pts',(3.99869537471779,-31.8060778097421,
125.979836980144));
#100634=CARTESIAN_POINT('Ctrl Pts',(4.002564448066,-31.8398956515833,125.917502474547));
#100635=CARTESIAN_POINT('Ctrl Pts',(4.00643352141422,-31.8705488495699,
125.853293046297));
#100636=CARTESIAN_POINT('Ctrl Pts',(4.01030259476243,-31.8978256139733,
125.78756301427));
#100637=CARTESIAN_POINT('Ctrl Pts',(4.01416590315822,-31.9250617357641,
125.721930920554));
#100638=CARTESIAN_POINT('Ctrl Pts',(4.01802921155401,-31.9489312255172,
125.654783165467));
#100639=CARTESIAN_POINT('Ctrl Pts',(4.0218925199498,-31.9692680899003,125.586498723443));
#100640=CARTESIAN_POINT('Ctrl Pts',(4.02575129644272,-31.989581097867,125.518294383349));
#100641=CARTESIAN_POINT('Ctrl Pts',(4.02961007293563,-32.0063695738438,
125.448956468227));
#100642=CARTESIAN_POINT('Ctrl Pts',(4.03346884942855,-32.0195162093905,
125.378882359722));
#100643=CARTESIAN_POINT('Ctrl Pts',(4.03732519501675,-32.032654562981,125.308852395646));
#100644=CARTESIAN_POINT('Ctrl Pts',(4.04118154060496,-32.0421555385165,
125.238087634641));
#100645=CARTESIAN_POINT('Ctrl Pts',(4.04503788619317,-32.0479524838775,
125.166997563695));
#100646=CARTESIAN_POINT('Ctrl Pts',(4.04889309243851,-32.0537477165527,
125.095928496044));
#100647=CARTESIAN_POINT('Ctrl Pts',(4.05274829868384,-32.0558410521646,
125.024534793174));
#100648=CARTESIAN_POINT('Ctrl Pts',(4.05660350492917,-32.0542176734686,
124.953231287067));
#100649=CARTESIAN_POINT('Ctrl Pts',(4.06045886178043,-32.0525942313542,
124.881924995447));
#100650=CARTESIAN_POINT('Ctrl Pts',(4.06431421863168,-32.0472537999241,
124.810709393194));
#100651=CARTESIAN_POINT('Ctrl Pts',(4.06816957548293,-32.0382336514703,
124.73999779902));
#100652=CARTESIAN_POINT('Ctrl Pts',(4.07202896795149,-32.0292040611233,
124.669212187073));
#100653=CARTESIAN_POINT('Ctrl Pts',(4.07588836042005,-32.0164871263596,
124.598932119228));
#100654=CARTESIAN_POINT('Ctrl Pts',(4.07974775288861,-32.0001717313108,
124.529563386028));
#100655=CARTESIAN_POINT('Ctrl Pts',(4.08360933049205,-31.9838470987099,
124.460155377207));
#100656=CARTESIAN_POINT('Ctrl Pts',(4.08747090809549,-31.9639200857576,
124.391660196868));
#100657=CARTESIAN_POINT('Ctrl Pts',(4.09133248569893,-31.9405294728947,
124.324468411303));
#100658=CARTESIAN_POINT('Ctrl Pts',(4.0952008198138,-31.917097934027,124.257159061853));
#100659=CARTESIAN_POINT('Ctrl Pts',(4.09906915392867,-31.8901908793727,
124.191158110285));
#100660=CARTESIAN_POINT('Ctrl Pts',(4.10293748804354,-31.8599949485487,
124.126835437118));
#100661=CARTESIAN_POINT('Ctrl Pts',(4.10523520721448,-31.8420591221495,
124.088628954722));
#100662=CARTESIAN_POINT('Ctrl Pts',(4.10753292638542,-31.8229638179775,
124.051014126221));
#100663=CARTESIAN_POINT('Ctrl Pts',(4.10983064555635,-31.8027554667188,
124.01406374967));
#100664=CARTESIAN_POINT('Ctrl Pts',(4.11369971890456,-31.768727116233,123.951843910566));
#100665=CARTESIAN_POINT('Ctrl Pts',(4.11756879225278,-31.731407172388,123.891265935903));
#100666=CARTESIAN_POINT('Ctrl Pts',(4.12143786560099,-31.6909784467623,
123.832699929288));
#100667=CARTESIAN_POINT('Ctrl Pts',(4.12530117399678,-31.6506099602841,
123.774221186524));
#100668=CARTESIAN_POINT('Ctrl Pts',(4.12916448239257,-31.607142160362,123.717748857687));
#100669=CARTESIAN_POINT('Ctrl Pts',(4.13302779078836,-31.5608034111036,
123.663627943128));
#100670=CARTESIAN_POINT('Ctrl Pts',(4.13688656728126,-31.5145190201024,
123.609570515794));
#100671=CARTESIAN_POINT('Ctrl Pts',(4.14074534377418,-31.4653706837746,
123.557859390925));
#100672=CARTESIAN_POINT('Ctrl Pts',(4.14460412026708,-31.4136286358643,
123.508808649983));
#100673=CARTESIAN_POINT('Ctrl Pts',(4.14846046585529,-31.3619191837748,
123.459788809426));
#100674=CARTESIAN_POINT('Ctrl Pts',(4.1523168114435,-31.3076196135577,123.413426361147));
#100675=CARTESIAN_POINT('Ctrl Pts',(4.1561731570317,-31.2510378033503,123.369999393531));
#100676=CARTESIAN_POINT('Ctrl Pts',(4.16002836327703,-31.1944727100272,
123.32658525625));
#100677=CARTESIAN_POINT('Ctrl Pts',(4.16388356952235,-31.1356271005012,
123.286105173458));
#100678=CARTESIAN_POINT('Ctrl Pts',(4.16773877576768,-31.0748414568478,
123.248796583734));
#100679=CARTESIAN_POINT('Ctrl Pts',(4.17159413261893,-31.014053438567,123.211486536528));
#100680=CARTESIAN_POINT('Ctrl Pts',(4.17544948947017,-30.9513256508639,
123.177348480609));
#100681=CARTESIAN_POINT('Ctrl Pts',(4.17930484632142,-30.8870255559437,
123.146575271126));
#100682=CARTESIAN_POINT('Ctrl Pts',(4.18316423878998,-30.8226581545234,
123.115769849605));
#100683=CARTESIAN_POINT('Ctrl Pts',(4.18702363125854,-30.7567155995423,
123.088336515709));
#100684=CARTESIAN_POINT('Ctrl Pts',(4.1908830237271,-30.6895870208718,123.064420680224));
#100685=CARTESIAN_POINT('Ctrl Pts',(4.19474460133053,-30.6224204349244,
123.040491303922));
#100686=CARTESIAN_POINT('Ctrl Pts',(4.19860617893397,-30.5540669542209,
123.020083529651));
#100687=CARTESIAN_POINT('Ctrl Pts',(4.2024677565374,-30.4849299800442,123.00329259105));
#100688=CARTESIAN_POINT('Ctrl Pts',(4.20633609065227,-30.4156720385312,
122.986472273739));
#100689=CARTESIAN_POINT('Ctrl Pts',(4.21020442476714,-30.3456283441291,
122.973281516649));
#100690=CARTESIAN_POINT('Ctrl Pts',(4.21407275888201,-30.2752108761994,
122.963764125618));
#100691=CARTESIAN_POINT('Ctrl Pts',(4.21637047805297,-30.2333841980406,
122.95811097075));
#100692=CARTESIAN_POINT('Ctrl Pts',(4.21866819722394,-30.1914257349887,
122.953752835488));
#100693=CARTESIAN_POINT('Ctrl Pts',(4.22096591639491,-30.1494218301973,
122.950690194441));
#100694=CARTESIAN_POINT('Ctrl Pts',(4.22483498974313,-30.0786924779759,
122.945533087776));
#100695=CARTESIAN_POINT('Ctrl Pts',(4.22870406309134,-30.0075572855653,
122.944031880373));
#100696=CARTESIAN_POINT('Ctrl Pts',(4.23257313643955,-29.9364263435634,
122.946233715169));
#100697=CARTESIAN_POINT('Ctrl Pts',(4.23643644483533,-29.8654013872744,
122.948432269213));
#100698=CARTESIAN_POINT('Ctrl Pts',(4.2402997532311,-29.7943811504204,122.954322898336));
#100699=CARTESIAN_POINT('Ctrl Pts',(4.24416306162688,-29.7237793393141,
122.963900859705));
#100700=CARTESIAN_POINT('Ctrl Pts',(4.24802183811979,-29.6532603485569,
122.973467585525));
#100701=CARTESIAN_POINT('Ctrl Pts',(4.2518806146127,-29.5831592876139,122.986712986754));
#100702=CARTESIAN_POINT('Ctrl Pts',(4.25573939110561,-29.5138865950802,
123.003580374757));
#100703=CARTESIAN_POINT('Ctrl Pts',(4.25959573669382,-29.4446575421081,
123.020437136849));
#100704=CARTESIAN_POINT('Ctrl Pts',(4.26345208228203,-29.3762562930919,
123.040911244135));
#100705=CARTESIAN_POINT('Ctrl Pts',(4.26730842787023,-29.3090834642402,
123.064894859933));
#100706=CARTESIAN_POINT('Ctrl Pts',(4.27116363411556,-29.2419304813494,
123.088871389861));
#100707=CARTESIAN_POINT('Ctrl Pts',(4.2750188403609,-29.1760056553525,123.116355206566));
#100708=CARTESIAN_POINT('Ctrl Pts',(4.27887404660623,-29.1116931339931,
123.147189034385));
#100709=CARTESIAN_POINT('Ctrl Pts',(4.28272940345749,-29.0473781002267,
123.178024066745));
#100710=CARTESIAN_POINT('Ctrl Pts',(4.28658476030875,-28.9846759332387,
123.212209158043));
#100711=CARTESIAN_POINT('Ctrl Pts',(4.29044011716001,-28.9239479573427,
123.249540184982));
#100712=CARTESIAN_POINT('Ctrl Pts',(4.29429950962857,-28.8631564140833,
123.286910288391));
#100713=CARTESIAN_POINT('Ctrl Pts',(4.29815890209712,-28.8043436017998,
123.327432646138));
#100714=CARTESIAN_POINT('Ctrl Pts',(4.30201829456568,-28.7478427364944,
123.370859198857));
#100715=CARTESIAN_POINT('Ctrl Pts',(4.30587987216911,-28.691309881177,123.414310339091));
#100716=CARTESIAN_POINT('Ctrl Pts',(4.30974144977254,-28.6370919480332,
123.460668631775));
#100717=CARTESIAN_POINT('Ctrl Pts',(4.31360302737596,-28.5854877373581,
123.509646813223));
#100718=CARTESIAN_POINT('Ctrl Pts',(4.31747136149083,-28.5337932360101,
123.558710690643));
#100719=CARTESIAN_POINT('Ctrl Pts',(4.3213396956057,-28.4847219221545,123.6104032564));
#100720=CARTESIAN_POINT('Ctrl Pts',(4.32520802972057,-28.4385340417937,
123.664402147403));
#100721=CARTESIAN_POINT('Ctrl Pts',(4.32750574889154,-28.4110992921005,
123.69647649346));
#100722=CARTESIAN_POINT('Ctrl Pts',(4.32980346806251,-28.3846810693939,
123.729363929871));
#100723=CARTESIAN_POINT('Ctrl Pts',(4.33210118723347,-28.3593266018392,
123.762992173401));
#100724=CARTESIAN_POINT('Ctrl Pts',(4.33598223894955,-28.3165006546752,
123.819793262895));
#100725=CARTESIAN_POINT('Ctrl Pts',(4.33986329066564,-28.2765427096807,
123.878933890299));
#100726=CARTESIAN_POINT('Ctrl Pts',(4.34374434238172,-28.2397168782025,
123.940093922267));
#100727=CARTESIAN_POINT('Ctrl Pts',(4.34761960540849,-28.2029459734072,
124.001162732461));
#100728=CARTESIAN_POINT('Ctrl Pts',(4.35149486843527,-28.1692981577268,
124.064244561645));
#100729=CARTESIAN_POINT('Ctrl Pts',(4.35537013146204,-28.1389961109817,
124.128987894712));
#100730=CARTESIAN_POINT('Ctrl Pts',(4.35942884712873,-28.1072595834202,
124.196796138544));
#100731=CARTESIAN_POINT('Ctrl Pts',(4.36348756279542,-28.0791938035524,
124.266426682195));
#100732=CARTESIAN_POINT('Ctrl Pts',(4.36754627846211,-28.0550020434937,
124.337443955815));
#100733=CARTESIAN_POINT('Ctrl Pts',(4.37141366678514,-28.0319506799473,
124.40511348413));
#100734=CARTESIAN_POINT('Ctrl Pts',(4.37528105510817,-28.0124165131004,
124.474041440808));
#100735=CARTESIAN_POINT('Ctrl Pts',(4.3791484434312,-27.9965263590055,124.543830149681));
#100736=CARTESIAN_POINT('Ctrl Pts',(4.38301406018575,-27.9806434838528,
124.613586889828));
#100737=CARTESIAN_POINT('Ctrl Pts',(4.38687967694029,-27.9684014102052,
124.684203129543));
#100738=CARTESIAN_POINT('Ctrl Pts',(4.39074529369484,-27.9598764862877,
124.755268287101));
#100739=CARTESIAN_POINT('Ctrl Pts',(4.39461092103577,-27.9513515390239,
124.826333639279));
#100740=CARTESIAN_POINT('Ctrl Pts',(4.3984765483767,-27.9465438214082,124.897847434114));
#100741=CARTESIAN_POINT('Ctrl Pts',(4.40234217571764,-27.9454779738572,
124.969392703581));
#100742=CARTESIAN_POINT('Ctrl Pts',(4.4029196902992,-27.9453187390298,124.980081379109));
#100743=CARTESIAN_POINT('Ctrl Pts',(4.40349720488077,-27.9452429264143,
124.990770753236));
#100744=CARTESIAN_POINT('Ctrl Pts',(4.40407471946233,-27.9452505182983,
125.001459433628));
#100745=CARTESIAN_POINT('Ctrl Pts',(4.40407471951209,-27.9452505182989,
125.001459434549));
#100746=CARTESIAN_POINT('Ctrl Pts',(4.40849095806752,-27.945308573269,125.083195487555));
#100747=CARTESIAN_POINT('Ctrl Pts',(4.41290719662295,-27.9502477237073,
125.164736898217));
#100748=CARTESIAN_POINT('Ctrl Pts',(4.41732343517838,-27.9599745962953,
125.245548192295));
#100749=CARTESIAN_POINT('Ctrl Pts',(4.42177971598686,-27.9697896629173,
125.327092206368));
#100750=CARTESIAN_POINT('Ctrl Pts',(4.42623599679533,-27.9844795567246,
125.407892614167));
#100751=CARTESIAN_POINT('Ctrl Pts',(4.43069227760381,-28.0038986271028,
125.487418579475));
#100752=CARTESIAN_POINT('Ctrl Pts',(4.43487367109322,-28.0221198249895,
125.562038956394));
#100753=CARTESIAN_POINT('Ctrl Pts',(4.43905506458263,-28.0445042064888,
125.635537342873));
#100754=CARTESIAN_POINT('Ctrl Pts',(4.44323645807204,-28.0708935156208,
125.70749256846));
#100755=CARTESIAN_POINT('Ctrl Pts',(4.44710553142024,-28.0953117323945,
125.774073254131));
#100756=CARTESIAN_POINT('Ctrl Pts',(4.45097460476845,-28.1232287475471,
125.839518723706));
#100757=CARTESIAN_POINT('Ctrl Pts',(4.45484367811666,-28.1545186966461,
125.903435842476));
#100758=CARTESIAN_POINT('Ctrl Pts',(4.45870698651244,-28.1857620234529,
125.967257724192));
#100759=CARTESIAN_POINT('Ctrl Pts',(4.46257029490822,-28.2203680964809,
126.029555342637));
#100760=CARTESIAN_POINT('Ctrl Pts',(4.466433603304,-28.2581622778487,126.089953628459));
#100761=CARTESIAN_POINT('Ctrl Pts',(4.4702923797969,-28.2959121242731,126.150281063306));
#100762=CARTESIAN_POINT('Ctrl Pts',(4.47415115628981,-28.3368423939913,
126.208713181356));
#100763=CARTESIAN_POINT('Ctrl Pts',(4.47800993278271,-28.3807324547538,
126.26489927639));
#100764=CARTESIAN_POINT('Ctrl Pts',(4.48186627837091,-28.4245948661939,
126.321049975997));
#100765=CARTESIAN_POINT('Ctrl Pts',(4.48572262395911,-28.4714130710542,
126.374957077846));
#100766=CARTESIAN_POINT('Ctrl Pts',(4.48957896954731,-28.5209238681718,
126.42629988388));
#100767=CARTESIAN_POINT('Ctrl Pts',(4.49343417579264,-28.5704200375096,
126.477627520874));
#100768=CARTESIAN_POINT('Ctrl Pts',(4.49728938203796,-28.622606882761,126.526392016628));
#100769=CARTESIAN_POINT('Ctrl Pts',(4.50114458828329,-28.6771829274427,
126.572308034404));
#100770=CARTESIAN_POINT('Ctrl Pts',(4.50499994513453,-28.7317611041698,
126.618225845917));
#100771=CARTESIAN_POINT('Ctrl Pts',(4.50885530198577,-28.7887282924879,
126.661294647469));
#100772=CARTESIAN_POINT('Ctrl Pts',(4.51271065883701,-28.8477497183853,
126.701269188288));
#100773=CARTESIAN_POINT('Ctrl Pts',(4.51657005130556,-28.9068329253051,
126.741285572692));
#100774=CARTESIAN_POINT('Ctrl Pts',(4.52042944377412,-28.9679742592167,
126.778200957744));
#100775=CARTESIAN_POINT('Ctrl Pts',(4.52428883624267,-29.0308104776631,
126.811813796253));
#100776=CARTESIAN_POINT('Ctrl Pts',(4.5281504138461,-29.0936822731112,126.845445665888));
#100777=CARTESIAN_POINT('Ctrl Pts',(4.53201199144952,-29.1582504234891,
126.875771060061));
#100778=CARTESIAN_POINT('Ctrl Pts',(4.53587356905295,-29.2241301267122,
126.902635935281));
#100779=CARTESIAN_POINT('Ctrl Pts',(4.53974190316782,-29.2901250981013,
126.929547815342));
#100780=CARTESIAN_POINT('Ctrl Pts',(4.54361023728269,-29.3574357450443,
126.952986928086));
#100781=CARTESIAN_POINT('Ctrl Pts',(4.54747857139755,-29.4256611505277,
126.972848815416));
#100782=CARTESIAN_POINT('Ctrl Pts',(4.54977629056857,-29.4661857839938,
126.984646410436));
#100783=CARTESIAN_POINT('Ctrl Pts',(4.55207400973958,-29.5070329226985,
126.995182881589));
#100784=CARTESIAN_POINT('Ctrl Pts',(4.55437172891059,-29.548117249947,127.004444946289));
#100785=CARTESIAN_POINT('Ctrl Pts',(4.55844028467461,-29.6208649897693,
127.020845221484));
#100786=CARTESIAN_POINT('Ctrl Pts',(4.56250884043863,-29.694656600035,127.033313769652));
#100787=CARTESIAN_POINT('Ctrl Pts',(4.56657739620265,-29.7690281740219,
127.041727106668));
#100788=CARTESIAN_POINT('Ctrl Pts',(4.5704397239533,-29.839629982312,127.049713986269));
#100789=CARTESIAN_POINT('Ctrl Pts',(4.57430205170395,-29.9107538314205,
127.054046646489));
#100790=CARTESIAN_POINT('Ctrl Pts',(4.5781643794546,-29.9819897223702,127.054671066716));
#100791=CARTESIAN_POINT('Ctrl Pts',(4.58202291830848,-30.0531557317731,
127.055294874394));
#100792=CARTESIAN_POINT('Ctrl Pts',(4.58588145716235,-30.1244330817512,
127.052217654959));
#100793=CARTESIAN_POINT('Ctrl Pts',(4.58973999601623,-30.195407433563,127.045437238687));
#100794=CARTESIAN_POINT('Ctrl Pts',(4.59359604056304,-30.26633590484,127.038661205536));
#100795=CARTESIAN_POINT('Ctrl Pts',(4.59745208510986,-30.3369612843276,
127.028186773298));
#100796=CARTESIAN_POINT('Ctrl Pts',(4.60130812965668,-30.4068717506067,
127.014063787733));
#100797=CARTESIAN_POINT('Ctrl Pts',(4.60516297144612,-30.4767604107765,
126.999945207337));
#100798=CARTESIAN_POINT('Ctrl Pts',(4.60901781323556,-30.5459341251056,
126.982180431198));
#100799=CARTESIAN_POINT('Ctrl Pts',(4.612872655025,-30.6139904073288,126.960870557229));
#100800=CARTESIAN_POINT('Ctrl Pts',(4.6167292826038,-30.6820782172232,126.939550811274));
#100801=CARTESIAN_POINT('Ctrl Pts',(4.6205859101826,-30.7490470959354,126.914682829204));
#100802=CARTESIAN_POINT('Ctrl Pts',(4.6244425377614,-30.814510037361,126.886417493965));
#100803=CARTESIAN_POINT('Ctrl Pts',(4.62830019961477,-30.8799905347093,
126.858144578499));
#100804=CARTESIAN_POINT('Ctrl Pts',(4.63215786146814,-30.9439638516118,
126.826472704402));
#100805=CARTESIAN_POINT('Ctrl Pts',(4.63601552332152,-31.0060654693665,
126.791599797345));
#100806=CARTESIAN_POINT('Ctrl Pts',(4.6398776444632,-31.068238873874,126.756686578735));
#100807=CARTESIAN_POINT('Ctrl Pts',(4.64373976560488,-31.1285358471724,
126.718565196641));
#100808=CARTESIAN_POINT('Ctrl Pts',(4.64760188674656,-31.1866197580259,
126.677477604131));
#100809=CARTESIAN_POINT('Ctrl Pts',(4.64907361358005,-31.2087536184256,
126.661820479406));
#100810=CARTESIAN_POINT('Ctrl Pts',(4.65054534041353,-31.2305664480703,
126.645733051043));
#100811=CARTESIAN_POINT('Ctrl Pts',(4.65201706724701,-31.2520409112987,
126.629230222815));
#100812=CARTESIAN_POINT('',(4.34592528058851,-27.945250355841,124.99879073222));
#100813=CARTESIAN_POINT('Ctrl Pts',(4.34592528058851,-27.945250355841,124.99879073222));
#100814=CARTESIAN_POINT('Ctrl Pts',(4.34974237135632,-27.945209114052,125.068867478461));
#100815=CARTESIAN_POINT('Ctrl Pts',(4.35355946212413,-27.9487570283886,
125.139087448465));
#100816=CARTESIAN_POINT('Ctrl Pts',(4.35737655289194,-27.955911683808,125.209046688822));
#100817=CARTESIAN_POINT('Ctrl Pts',(4.36118805254435,-27.9630558593865,
125.278903455801));
#100818=CARTESIAN_POINT('Ctrl Pts',(4.36499955219676,-27.9737962381263,
125.348499758144));
#100819=CARTESIAN_POINT('Ctrl Pts',(4.36881105184917,-27.988098387281,125.417431986363));
#100820=CARTESIAN_POINT('Ctrl Pts',(4.37261948474211,-28.0023890288257,
125.486308751225));
#100821=CARTESIAN_POINT('Ctrl Pts',(4.37642791763504,-28.0202356597748,
125.554522013913));
#100822=CARTESIAN_POINT('Ctrl Pts',(4.38023635052798,-28.0415522620249,
125.621675172514));
#100823=CARTESIAN_POINT('Ctrl Pts',(4.38404307118847,-28.0628592805488,
125.688798139742));
#100824=CARTESIAN_POINT('Ctrl Pts',(4.38784979184896,-28.0876330257033,
125.754861472597));
#100825=CARTESIAN_POINT('Ctrl Pts',(4.39165651250945,-28.1157372762062,
125.819482489271));
#100826=CARTESIAN_POINT('Ctrl Pts',(4.39546287300883,-28.1438388677124,
125.884097392026));
#100827=CARTESIAN_POINT('Ctrl Pts',(4.39926923350821,-28.1752701383349,
125.947269792159));
#100828=CARTESIAN_POINT('Ctrl Pts',(4.40307559400758,-28.2098469931641,
126.008637583385));
#100829=CARTESIAN_POINT('Ctrl Pts',(4.40688551323047,-28.2444561753217,
126.070062749891));
#100830=CARTESIAN_POINT('Ctrl Pts',(4.41069543245336,-28.2822165682454,
126.129679502486));
#100831=CARTESIAN_POINT('Ctrl Pts',(4.41450535167624,-28.3228989571241,
126.187151908765));
#100832=CARTESIAN_POINT('Ctrl Pts',(4.41831711300228,-28.3636010160147,
126.244652103061));
#100833=CARTESIAN_POINT('Ctrl Pts',(4.42212887432831,-28.407227572401,126.300005495645));
#100834=CARTESIAN_POINT('Ctrl Pts',(4.42594063565434,-28.4535088401647,
126.352908960371));
#100835=CARTESIAN_POINT('Ctrl Pts',(4.42975910316277,-28.4998715323924,
126.405905500254));
#100836=CARTESIAN_POINT('Ctrl Pts',(4.43357757067119,-28.5488979118458,
126.456443149054));
#100837=CARTESIAN_POINT('Ctrl Pts',(4.43739603817962,-28.6002816356027,
126.504255983159));
#100838=CARTESIAN_POINT('Ctrl Pts',(4.44006763663388,-28.6362323610338,
126.537708328479));
#100839=CARTESIAN_POINT('Ctrl Pts',(4.44273923508813,-28.6733362922242,
126.569827654898));
#100840=CARTESIAN_POINT('Ctrl Pts',(4.44541083354239,-28.7114798816252,
126.600535368882));
#100841=CARTESIAN_POINT('Ctrl Pts',(4.4492799068906,-28.7667203482161,126.645007021265));
#100842=CARTESIAN_POINT('Ctrl Pts',(4.45314898023881,-28.8243740439198,
126.686702591709));
#100843=CARTESIAN_POINT('Ctrl Pts',(4.45701805358702,-28.8841304900815,
126.725350051246));
#100844=CARTESIAN_POINT('Ctrl Pts',(4.46088136198282,-28.9437978986267,
126.763939925737));
#100845=CARTESIAN_POINT('Ctrl Pts',(4.46474467037861,-29.0055614338967,
126.799490442826));
#100846=CARTESIAN_POINT('Ctrl Pts',(4.4686079787744,-29.0690781313601,126.831770192188));
#100847=CARTESIAN_POINT('Ctrl Pts',(4.47246675526731,-29.1325203197564,
126.864012075381));
#100848=CARTESIAN_POINT('Ctrl Pts',(4.47632553176022,-29.1977111543373,
126.892990593039));
#100849=CARTESIAN_POINT('Ctrl Pts',(4.48018430825314,-29.2642808120643,
126.918518918073));
#100850=CARTESIAN_POINT('Ctrl Pts',(4.48404065384134,-29.3308085330544,
126.944031161085));
#100851=CARTESIAN_POINT('Ctrl Pts',(4.48789699942955,-29.3987129013685,
126.966097350154));
#100852=CARTESIAN_POINT('Ctrl Pts',(4.49175334501776,-29.4676030803233,
126.984578313501));
#100853=CARTESIAN_POINT('Ctrl Pts',(4.49560855126309,-29.5364729059325,
127.003053816717));
#100854=CARTESIAN_POINT('Ctrl Pts',(4.49946375750842,-29.6063274950223,
127.017946071298));
#100855=CARTESIAN_POINT('Ctrl Pts',(4.50331896375375,-29.6767614356553,
127.029165935309));
#100856=CARTESIAN_POINT('Ctrl Pts',(4.507174320605,-29.7471981278319,127.040386237632));
#100857=CARTESIAN_POINT('Ctrl Pts',(4.51102967745624,-29.8182137364021,
127.047933790311));
#100858=CARTESIAN_POINT('Ctrl Pts',(4.51488503430748,-29.8893949749596,
127.051770964542));
#100859=CARTESIAN_POINT('Ctrl Pts',(4.51874442677604,-29.9606507228947,
127.055612155357));
#100860=CARTESIAN_POINT('Ctrl Pts',(4.5226038192446,-30.0320719608351,127.055735188464));
#100861=CARTESIAN_POINT('Ctrl Pts',(4.52646321171316,-30.1032435307007,
127.052154559449));
#100862=CARTESIAN_POINT('Ctrl Pts',(4.5303247893166,-30.1744553969292,127.048571903132));
#100863=CARTESIAN_POINT('Ctrl Pts',(4.53418636692004,-30.2454168302102,
127.041281459958));
#100864=CARTESIAN_POINT('Ctrl Pts',(4.53804794452347,-30.3157186798857,
127.030349545687));
#100865=CARTESIAN_POINT('Ctrl Pts',(4.54191627863834,-30.3861435350527,
127.019398504103));
#100866=CARTESIAN_POINT('Ctrl Pts',(4.54578461275322,-30.4559060268753,
127.00479337032));
#100867=CARTESIAN_POINT('Ctrl Pts',(4.54965294686809,-30.5246087508621,
126.986651258027));
#100868=CARTESIAN_POINT('Ctrl Pts',(4.55195066603904,-30.5654169027211,
126.975875177683));
#100869=CARTESIAN_POINT('Ctrl Pts',(4.55424838520999,-30.605851453418,126.963852154995));
#100870=CARTESIAN_POINT('Ctrl Pts',(4.55654610438093,-30.6458324446947,
126.950614778956));
#100871=CARTESIAN_POINT('Ctrl Pts',(4.56041440943523,-30.7131420935789,
126.928329110068));
#100872=CARTESIAN_POINT('Ctrl Pts',(4.56428271448952,-30.7794286907234,
126.902511739844));
#100873=CARTESIAN_POINT('Ctrl Pts',(4.56815101954381,-30.8442955354996,
126.873275903661));
#100874=CARTESIAN_POINT('Ctrl Pts',(4.57201426861251,-30.9090775974502,
126.844078279553));
#100875=CARTESIAN_POINT('Ctrl Pts',(4.57587751768122,-30.9724431477123,
126.811471247143));
#100876=CARTESIAN_POINT('Ctrl Pts',(4.57974076674992,-31.0340117705029,
126.775617419649));
#100877=CARTESIAN_POINT('Ctrl Pts',(4.58359955353666,-31.0955092778802,
126.739805005454));
#100878=CARTESIAN_POINT('Ctrl Pts',(4.58745834032341,-31.1552135623627,
126.700753487884));
#100879=CARTESIAN_POINT('Ctrl Pts',(4.59131712711015,-31.2127670754802,
126.658672234991));
#100880=CARTESIAN_POINT('Ctrl Pts',(4.59220253433037,-31.2259728572141,
126.649016597817));
#100881=CARTESIAN_POINT('Ctrl Pts',(4.59308794155059,-31.2390655097594,
126.639201639586));
#100882=CARTESIAN_POINT('Ctrl Pts',(4.59397334877082,-31.2520409112987,
126.629230222815));
#100883=CARTESIAN_POINT('Ctrl Pts',(3.89394636911841,-31.2520409112987,
126.629230222815));
#100884=CARTESIAN_POINT('Ctrl Pts',(3.89781318526386,-31.3083155207066,
126.585983963165));
#100885=CARTESIAN_POINT('Ctrl Pts',(3.90168000140932,-31.3624485309783,
126.539740516924));
#100886=CARTESIAN_POINT('Ctrl Pts',(3.90554681755477,-31.4141040713363,
126.490740499862));
#100887=CARTESIAN_POINT('Ctrl Pts',(3.90951860641449,-31.4671619080732,
126.440410276089));
#100888=CARTESIAN_POINT('Ctrl Pts',(3.91349039527422,-31.5176053431718,
126.387171882628));
#100889=CARTESIAN_POINT('Ctrl Pts',(3.91746218413394,-31.5651045384085,
126.331332169803));
#100890=CARTESIAN_POINT('Ctrl Pts',(3.92131985552486,-31.6112389863935,
126.277096844048));
#100891=CARTESIAN_POINT('Ctrl Pts',(3.92517752691578,-31.6545957638065,
126.220408064187));
#100892=CARTESIAN_POINT('Ctrl Pts',(3.92903519830671,-31.6949097126747,
126.161584533463));
#100893=CARTESIAN_POINT('Ctrl Pts',(3.93289094441448,-31.7352035416938,
126.102790360333));
#100894=CARTESIAN_POINT('Ctrl Pts',(3.93674669052226,-31.7724572813979,
126.041863950583));
#100895=CARTESIAN_POINT('Ctrl Pts',(3.94060243663004,-31.8064475888168,
125.979155080341));
#100896=CARTESIAN_POINT('Ctrl Pts',(3.94445754823064,-31.8404323027414,
125.916456529562));
#100897=CARTESIAN_POINT('Ctrl Pts',(3.94831265983124,-31.8711544199303,
125.851976528084));
#100898=CARTESIAN_POINT('Ctrl Pts',(3.95216777143185,-31.8984361485015,
125.786090168214));
#100899=CARTESIAN_POINT('Ctrl Pts',(3.95622626966154,-31.927157196964,125.716727798821));
#100900=CARTESIAN_POINT('Ctrl Pts',(3.96028476789123,-31.9520645755645,
125.645807120439));
#100901=CARTESIAN_POINT('Ctrl Pts',(3.96434326612092,-31.973009012082,125.57378828913));
#100902=CARTESIAN_POINT('Ctrl Pts',(3.96820348466854,-31.9929301991169,
125.505287968898));
#100903=CARTESIAN_POINT('Ctrl Pts',(3.97206370321616,-32.0092665464193,
125.435794794154));
#100904=CARTESIAN_POINT('Ctrl Pts',(3.97592392176378,-32.0219418432179,
125.365716755351));
#100905=CARTESIAN_POINT('Ctrl Pts',(3.97978683983634,-32.0346260040949,
125.295589709631));
#100906=CARTESIAN_POINT('Ctrl Pts',(3.98364975790889,-32.0436439603416,
125.224877467475));
#100907=CARTESIAN_POINT('Ctrl Pts',(3.98751267598145,-32.0489713596993,
125.153993277879));
#100908=CARTESIAN_POINT('Ctrl Pts',(3.9913818497609,-32.0543073863818,125.08299429664));
#100909=CARTESIAN_POINT('Ctrl Pts',(3.99525102354035,-32.055940927385,125.011823296695));
#100910=CARTESIAN_POINT('Ctrl Pts',(3.9991201973198,-32.0538996768372,124.940892640152));
#100911=CARTESIAN_POINT('Ctrl Pts',(3.99970338160925,-32.0535920077279,
124.930201560636));
#100912=CARTESIAN_POINT('Ctrl Pts',(4.00028656589869,-32.0532009492814,
124.919515928032));
#100913=CARTESIAN_POINT('Ctrl Pts',(4.00086975018814,-32.052726697614,124.90883713803));
#100914=CARTESIAN_POINT('Ctrl Pts',(4.00473882353635,-32.0495803260131,
124.837989856074));
#100915=CARTESIAN_POINT('Ctrl Pts',(4.00860789688457,-32.0427556783592,
124.76716688376));
#100916=CARTESIAN_POINT('Ctrl Pts',(4.01247697023278,-32.0322538737086,
124.69678101099));
#100917=CARTESIAN_POINT('Ctrl Pts',(4.01634027862857,-32.0217677168369,
124.626500013773));
#100918=CARTESIAN_POINT('Ctrl Pts',(4.02020358702436,-32.0076153497239,
124.556655299875));
#100919=CARTESIAN_POINT('Ctrl Pts',(4.02406689542014,-31.9898498441324,
124.487657184781));
#100920=CARTESIAN_POINT('Ctrl Pts',(4.02792567191305,-31.9721051785923,
124.4187400088));
#100921=CARTESIAN_POINT('Ctrl Pts',(4.03178444840596,-31.9507559140856,
124.350667927121));
#100922=CARTESIAN_POINT('Ctrl Pts',(4.03564322489888,-31.9259063300412,
124.283841937554));
#100923=CARTESIAN_POINT('Ctrl Pts',(4.03949957048708,-31.9010724004331,
124.217058046203));
#100924=CARTESIAN_POINT('Ctrl Pts',(4.04335591607529,-31.8727426950614,
124.151519143789));
#100925=CARTESIAN_POINT('Ctrl Pts',(4.04721226166349,-31.8410711425107,
124.08761049397));
#100926=CARTESIAN_POINT('Ctrl Pts',(4.05106746790882,-31.8094089472018,
124.023720725722));
#100927=CARTESIAN_POINT('Ctrl Pts',(4.05492267415416,-31.7744070804402,
123.961460688888));
#100928=CARTESIAN_POINT('Ctrl Pts',(4.05877788039949,-31.7362666457037,
123.901193512252));
#100929=CARTESIAN_POINT('Ctrl Pts',(4.06263323725073,-31.6981247209885,
123.840923981243));
#100930=CARTESIAN_POINT('Ctrl Pts',(4.06648859410198,-31.6568442465144,
123.782647874311));
#100931=CARTESIAN_POINT('Ctrl Pts',(4.07034395095322,-31.6126701841896,
123.726700176892));
#100932=CARTESIAN_POINT('Ctrl Pts',(4.07420334342178,-31.5684498824069,
123.670693915895));
#100933=CARTESIAN_POINT('Ctrl Pts',(4.07806273589034,-31.5213302481,123.617021311814));
#100934=CARTESIAN_POINT('Ctrl Pts',(4.0819221283589,-31.4715965922107,123.565984298449));
#100935=CARTESIAN_POINT('Ctrl Pts',(4.08578370596233,-31.4218347778102,
123.514918388631));
#100936=CARTESIAN_POINT('Ctrl Pts',(4.08964528356577,-31.3694563524205,
123.46649137005));
#100937=CARTESIAN_POINT('Ctrl Pts',(4.0935068611692,-31.3147815393856,123.42096641385));
#100938=CARTESIAN_POINT('Ctrl Pts',(4.09737519528408,-31.2600110631173,
123.375361803705));
#100939=CARTESIAN_POINT('Ctrl Pts',(4.10124352939895,-31.2029365664032,
123.332669684726));
#100940=CARTESIAN_POINT('Ctrl Pts',(4.10511186351382,-31.1439086244318,
123.293110835042));
#100941=CARTESIAN_POINT('Ctrl Pts',(4.10740958268478,-31.1088471147839,
123.269613607398));
#100942=CARTESIAN_POINT('Ctrl Pts',(4.10970730185574,-31.073096919377,123.247220986002));
#100943=CARTESIAN_POINT('Ctrl Pts',(4.1120050210267,-31.036735346744,123.225971425452));
#100944=CARTESIAN_POINT('Ctrl Pts',(4.11587409437491,-30.9755069802181,
123.190189808002));
#100945=CARTESIAN_POINT('Ctrl Pts',(4.11974316772313,-30.9123040724542,
123.15751165516));
#100946=CARTESIAN_POINT('Ctrl Pts',(4.12361224107134,-30.8474740331646,
123.128159909177));
#100947=CARTESIAN_POINT('Ctrl Pts',(4.12747554946713,-30.7827405911888,
123.098851897547));
#100948=CARTESIAN_POINT('Ctrl Pts',(4.13133885786291,-30.7163852690692,
123.072860653239));
#100949=CARTESIAN_POINT('Ctrl Pts',(4.13520216625869,-30.648781574934,123.050364128734));
#100950=CARTESIAN_POINT('Ctrl Pts',(4.1390609427516,-30.5812571841689,123.027893994063));
#100951=CARTESIAN_POINT('Ctrl Pts',(4.14291971924451,-30.5124877889165,
123.008910588793));
#100952=CARTESIAN_POINT('Ctrl Pts',(4.14677849573742,-30.4428668423194,
122.993543790043));
#100953=CARTESIAN_POINT('Ctrl Pts',(4.15063484132563,-30.3732897546726,
122.978186671881));
#100954=CARTESIAN_POINT('Ctrl Pts',(4.15449118691383,-30.3028626532357,
122.966441744494));
#100955=CARTESIAN_POINT('Ctrl Pts',(4.15834753250204,-30.2319927001266,
122.958388638945));
#100956=CARTESIAN_POINT('Ctrl Pts',(4.16220273874737,-30.1611436852799,
122.950337912657));
#100957=CARTESIAN_POINT('Ctrl Pts',(4.1660579449927,-30.0898525609291,122.945976897614));
#100958=CARTESIAN_POINT('Ctrl Pts',(4.16991315123803,-30.0185334786877,
122.945333586037));
#100959=CARTESIAN_POINT('Ctrl Pts',(4.17376850808927,-29.9472116103242,
122.944690249329));
#100960=CARTESIAN_POINT('Ctrl Pts',(4.17762386494052,-29.8758622676878,
122.947764906609));
#100961=CARTESIAN_POINT('Ctrl Pts',(4.18147922179176,-29.8048997451783,
122.95453343878));
#100962=CARTESIAN_POINT('Ctrl Pts',(4.18533861426031,-29.7338629422336,
122.961309055952));
#100963=CARTESIAN_POINT('Ctrl Pts',(4.18919800672887,-29.6632142522818,
122.971786220367));
#100964=CARTESIAN_POINT('Ctrl Pts',(4.19305739919743,-29.5933620854687,
122.985888987924));
#100965=CARTESIAN_POINT('Ctrl Pts',(4.19691897680086,-29.5234703693204,
122.999999740274));
#100966=CARTESIAN_POINT('Ctrl Pts',(4.20078055440429,-29.4543765448209,
123.017740061325));
#100967=CARTESIAN_POINT('Ctrl Pts',(4.20464213200773,-29.3864753911521,
123.038983652073));
#100968=CARTESIAN_POINT('Ctrl Pts',(4.2085104661226,-29.3184554324331,123.060264412231));
#100969=CARTESIAN_POINT('Ctrl Pts',(4.21237880023747,-29.2516327664633,
123.085060510932));
#100970=CARTESIAN_POINT('Ctrl Pts',(4.21624713435234,-29.1863830179587,
123.113197156819));
#100971=CARTESIAN_POINT('Ctrl Pts',(4.21854485352331,-29.1476258698976,
123.129909805919));
#100972=CARTESIAN_POINT('Ctrl Pts',(4.22084257269429,-29.1094232312381,
123.14780014868));
#100973=CARTESIAN_POINT('Ctrl Pts',(4.22314029186526,-29.0718493387358,
123.16682409123));
#100974=CARTESIAN_POINT('Ctrl Pts',(4.22700936521348,-29.0085795763096,
123.198858044738));
#100975=CARTESIAN_POINT('Ctrl Pts',(4.2308784385617,-28.946846249431,123.234234104093));
#100976=CARTESIAN_POINT('Ctrl Pts',(4.23474751190992,-28.8870250841454,
123.272781311131));
#100977=CARTESIAN_POINT('Ctrl Pts',(4.23861082030572,-28.8272930529084,
123.311271082501));
#100978=CARTESIAN_POINT('Ctrl Pts',(4.24247412870151,-28.769467932831,123.352922361501));
#100979=CARTESIAN_POINT('Ctrl Pts',(4.2463374370973,-28.7139018069391,123.397517862719));
#100980=CARTESIAN_POINT('Ctrl Pts',(4.25019621359022,-28.6584008635953,
123.442061050619));
#100981=CARTESIAN_POINT('Ctrl Pts',(4.25405499008314,-28.6051540277779,
123.489541297822));
#100982=CARTESIAN_POINT('Ctrl Pts',(4.25791376657606,-28.5544838097656,
123.53969848789));
#100983=CARTESIAN_POINT('Ctrl Pts',(4.26177011216428,-28.503845512356,123.589824080546));
#100984=CARTESIAN_POINT('Ctrl Pts',(4.26562645775249,-28.4557809568064,
123.642622929359));
#100985=CARTESIAN_POINT('Ctrl Pts',(4.26948280334071,-28.4105778747512,
123.697796148727));
#100986=CARTESIAN_POINT('Ctrl Pts',(4.27333800958605,-28.3653881477776,
123.752953067374));
#100987=CARTESIAN_POINT('Ctrl Pts',(4.27719321583139,-28.3230585236229,
123.810482588338));
#100988=CARTESIAN_POINT('Ctrl Pts',(4.28104842207672,-28.2838371407315,
123.870051946784));
#100989=CARTESIAN_POINT('Ctrl Pts',(4.28490377892798,-28.2446142256337,
123.929623632342));
#100990=CARTESIAN_POINT('Ctrl Pts',(4.28875913577923,-28.208500058177,123.991234906642));
#100991=CARTESIAN_POINT('Ctrl Pts',(4.29261449263048,-28.1756990732597,
124.054524621582));
#100992=CARTESIAN_POINT('Ctrl Pts',(4.29647388509905,-28.1428637537198,
124.117880585401));
#100993=CARTESIAN_POINT('Ctrl Pts',(4.30033327756761,-28.1133487638009,
124.182918064874));
#100994=CARTESIAN_POINT('Ctrl Pts',(4.30419267003618,-28.0873118065517,
124.249252747495));
#100995=CARTESIAN_POINT('Ctrl Pts',(4.30805424763962,-28.0612601075358,
124.315624987901));
#100996=CARTESIAN_POINT('Ctrl Pts',(4.31191582524307,-28.0386905150577,
124.383295432486));
#100997=CARTESIAN_POINT('Ctrl Pts',(4.31577740284651,-28.0197110338736,
124.45186391002));
#100998=CARTESIAN_POINT('Ctrl Pts',(4.31964573696139,-28.0006983447381,
124.520552360206));
#100999=CARTESIAN_POINT('Ctrl Pts',(4.32351407107627,-27.9852884132221,
124.590141505975));
#101000=CARTESIAN_POINT('Ctrl Pts',(4.32738240519115,-27.9735381148485,
124.660220968086));
#101001=CARTESIAN_POINT('Ctrl Pts',(4.32968012436204,-27.9665586541724,
124.701846877017));
#101002=CARTESIAN_POINT('Ctrl Pts',(4.33197784353293,-27.9608693712244,
124.743645657191));
#101003=CARTESIAN_POINT('Ctrl Pts',(4.33427556270382,-27.9564734841712,
124.785531024144));
#101004=CARTESIAN_POINT('Ctrl Pts',(4.33815880198178,-27.9490442554462,
124.856319005628));
#101005=CARTESIAN_POINT('Ctrl Pts',(4.34204204125973,-27.9452923123651,
124.927499585747));
#101006=CARTESIAN_POINT('Ctrl Pts',(4.34592528053768,-27.9452503558416,
124.998790731287));
#101007=CARTESIAN_POINT('Origin',(-1.54592528053767,-30.,125.));
#101008=CARTESIAN_POINT('',(3.19385981518126,-31.2520409112986,126.629230222815));
#101009=CARTESIAN_POINT('',(3.25213329740746,-31.2520409112987,126.629230222815));
#101010=CARTESIAN_POINT('',(-1.54592528053767,-31.2520409112987,126.629230222815));
#101011=CARTESIAN_POINT('',(3.70407471941287,-27.9452505355246,124.998516511556));
#101012=CARTESIAN_POINT('Ctrl Pts',(3.25213329740746,-31.2520409112987,
126.629230222815));
#101013=CARTESIAN_POINT('Ctrl Pts',(3.25599022094518,-31.3085196988896,
126.585827055053));
#101014=CARTESIAN_POINT('Ctrl Pts',(3.2598471444829,-31.3627864472108,126.539447086643));
#101015=CARTESIAN_POINT('Ctrl Pts',(3.26370406802062,-31.4145168381827,
126.490348844062));
#101016=CARTESIAN_POINT('Ctrl Pts',(3.26755947426724,-31.4662268787221,
126.441269916442));
#101017=CARTESIAN_POINT('Ctrl Pts',(3.27141488051386,-31.515402190237,126.389475171135));
#101018=CARTESIAN_POINT('Ctrl Pts',(3.27527028676049,-31.561753193755,126.335261968415));
#101019=CARTESIAN_POINT('Ctrl Pts',(3.27912546600276,-31.6081014681496,
126.281051957741));
#101020=CARTESIAN_POINT('Ctrl Pts',(3.28298064524503,-31.6516254502506,
126.224424142637));
#101021=CARTESIAN_POINT('Ctrl Pts',(3.2868358244873,-31.6920751093616,126.165709821001));
#101022=CARTESIAN_POINT('Ctrl Pts',(3.29069479680136,-31.7325645664823,
126.10693773094));
#101023=CARTESIAN_POINT('Ctrl Pts',(3.29455376911542,-31.7699733821347,
126.046075434586));
#101024=CARTESIAN_POINT('Ctrl Pts',(3.29841274142948,-31.8040947549429,
125.983483440474));
#101025=CARTESIAN_POINT('Ctrl Pts',(3.30227355969859,-31.838232449848,125.920861505229));
#101026=CARTESIAN_POINT('Ctrl Pts',(3.30613437796769,-31.8690793587569,
125.85650866261));
#101027=CARTESIAN_POINT('Ctrl Pts',(3.3099951962368,-31.8964758488847,125.790807762416));
#101028=CARTESIAN_POINT('Ctrl Pts',(3.31386313027636,-31.9239228327476,
125.724985770657));
#101029=CARTESIAN_POINT('Ctrl Pts',(3.31773106431591,-31.9479065279911,
125.657811215831));
#101030=CARTESIAN_POINT('Ctrl Pts',(3.32159899835547,-31.9683165969665,
125.589684098994));
#101031=CARTESIAN_POINT('Ctrl Pts',(3.32502724879912,-31.9864065714346,
125.529301265126));
#101032=CARTESIAN_POINT('Ctrl Pts',(3.32845549924278,-32.0016898867466,
125.468170556474));
#101033=CARTESIAN_POINT('Ctrl Pts',(3.33188374968643,-32.014123551826,125.406575799181));
#101034=CARTESIAN_POINT('Ctrl Pts',(3.33575282303466,-32.0281560045215,
125.337060856283));
#101035=CARTESIAN_POINT('Ctrl Pts',(3.33962189638288,-32.0386128869442,
125.266682430377));
#101036=CARTESIAN_POINT('Ctrl Pts',(3.34349096973111,-32.0453957342306,
125.195841397287));
#101037=CARTESIAN_POINT('Ctrl Pts',(3.3473542781269,-32.0521684750165,125.125105917943));
#101038=CARTESIAN_POINT('Ctrl Pts',(3.35121758652268,-32.0552780011611,
125.053909679268));
#101039=CARTESIAN_POINT('Ctrl Pts',(3.35508089491847,-32.0546768638109,
124.982663684929));
#101040=CARTESIAN_POINT('Ctrl Pts',(3.35893967141139,-32.0540764316325,
124.911501266606));
#101041=CARTESIAN_POINT('Ctrl Pts',(3.36279844790432,-32.0497739862522,
124.840289691965));
#101042=CARTESIAN_POINT('Ctrl Pts',(3.36665722439724,-32.0417740221373,
124.769443271568));
#101043=CARTESIAN_POINT('Ctrl Pts',(3.37051356998546,-32.0337790977417,
124.69864148213));
#101044=CARTESIAN_POINT('Ctrl Pts',(3.37436991557368,-32.0220913303191,
124.628204872126));
#101045=CARTESIAN_POINT('Ctrl Pts',(3.3782262611619,-32.0067671925841,124.558544456068));
#101046=CARTESIAN_POINT('Ctrl Pts',(3.38208146740724,-31.9914475823081,
124.488904620919));
#101047=CARTESIAN_POINT('Ctrl Pts',(3.38593667365259,-31.9724938389182,
124.420040998629));
#101048=CARTESIAN_POINT('Ctrl Pts',(3.38979187989793,-31.9500135557809,
124.35235449915));
#101049=CARTESIAN_POINT('Ctrl Pts',(3.39364723674919,-31.9275323944381,
124.284665355459));
#101050=CARTESIAN_POINT('Ctrl Pts',(3.39750259360046,-31.9015245750382,
124.218153886206));
#101051=CARTESIAN_POINT('Ctrl Pts',(3.40135795045172,-31.8721470420658,
124.153204265844));
#101052=CARTESIAN_POINT('Ctrl Pts',(3.40521734292029,-31.842738757989,124.088186659088));
#101053=CARTESIAN_POINT('Ctrl Pts',(3.40907673538886,-31.809953919732,124.02473460832));
#101054=CARTESIAN_POINT('Ctrl Pts',(3.41293612785744,-31.7739966007973,
123.963209942727));
#101055=CARTESIAN_POINT('Ctrl Pts',(3.41679770546088,-31.7380189233238,
123.901650442716));
#101056=CARTESIAN_POINT('Ctrl Pts',(3.42065928306433,-31.6988654562216,
123.842020906504));
#101057=CARTESIAN_POINT('Ctrl Pts',(3.42452086066778,-31.6567835031518,
123.784653964427));
#101058=CARTESIAN_POINT('Ctrl Pts',(3.42838919478266,-31.6146279202794,
123.727186648761));
#101059=CARTESIAN_POINT('Ctrl Pts',(3.43225752889754,-31.5695339288615,
123.671990207425));
#101060=CARTESIAN_POINT('Ctrl Pts',(3.43612586301243,-31.5217885122885,
123.619363448852));
#101061=CARTESIAN_POINT('Ctrl Pts',(3.43842358218328,-31.493428614792,123.58810412417));
#101062=CARTESIAN_POINT('Ctrl Pts',(3.44072130135414,-31.4641339653978,
123.557750714455));
#101063=CARTESIAN_POINT('Ctrl Pts',(3.44301902052499,-31.4339703168494,
123.528359183464));
#101064=CARTESIAN_POINT('Ctrl Pts',(3.4468880938732,-31.3831784837289,123.478867500293));
#101065=CARTESIAN_POINT('Ctrl Pts',(3.45075716722142,-31.3297219400211,
123.431911487284));
#101066=CARTESIAN_POINT('Ctrl Pts',(3.45462624056963,-31.2738840751607,
123.387791289705));
#101067=CARTESIAN_POINT('Ctrl Pts',(3.4584895489654,-31.2181294091975,123.343736831598));
#101068=CARTESIAN_POINT('Ctrl Pts',(3.46235285736118,-31.1600008431917,
123.302510100363));
#101069=CARTESIAN_POINT('Ctrl Pts',(3.46621616575695,-31.0998179446722,
123.264373873475));
#101070=CARTESIAN_POINT('Ctrl Pts',(3.47007494224986,-31.0397056444643,
123.226282382771));
#101071=CARTESIAN_POINT('Ctrl Pts',(3.47393371874277,-30.9775442068882,
123.19127445399));
#101072=CARTESIAN_POINT('Ctrl Pts',(3.47779249523568,-30.9136841499307,
123.159571018304));
#101073=CARTESIAN_POINT('Ctrl Pts',(3.48164884082389,-30.849864322749,123.12788755476));
#101074=CARTESIAN_POINT('Ctrl Pts',(3.48550518641209,-30.7843484332854,
123.099504669707));
#101075=CARTESIAN_POINT('Ctrl Pts',(3.4893615320003,-30.7175124215067,123.074597837468));
#101076=CARTESIAN_POINT('Ctrl Pts',(3.49321673824563,-30.6506961561776,
123.049698363859));
#101077=CARTESIAN_POINT('Ctrl Pts',(3.49707194449096,-30.5825609977989,
123.028273073754));
#101078=CARTESIAN_POINT('Ctrl Pts',(3.50092715073629,-30.5135021230633,
123.010449012438));
#101079=CARTESIAN_POINT('Ctrl Pts',(3.50478250758755,-30.4444405505017,
122.992624254815));
#101080=CARTESIAN_POINT('Ctrl Pts',(3.5086378644388,-30.3744556608622,122.978401124561));
#101081=CARTESIAN_POINT('Ctrl Pts',(3.51249322129005,-30.3039553368876,
122.967856128204));
#101082=CARTESIAN_POINT('Ctrl Pts',(3.51635261375861,-30.233381216287,122.957300093811));
#101083=CARTESIAN_POINT('Ctrl Pts',(3.52021200622717,-30.1622910657463,
122.950429951004));
#101084=CARTESIAN_POINT('Ctrl Pts',(3.52407139869572,-30.0910995558632,
122.947270491901));
#101085=CARTESIAN_POINT('Ctrl Pts',(3.52793297629916,-30.0198677383272,
122.944109243955));
#101086=CARTESIAN_POINT('Ctrl Pts',(3.5317945539026,-29.9485349332081,122.94466285826));
#101087=CARTESIAN_POINT('Ctrl Pts',(3.53565613150604,-29.8775147263634,
122.948903970985));
#101088=CARTESIAN_POINT('Ctrl Pts',(3.53952446562091,-29.8063702571345,
122.953152504285));
#101089=CARTESIAN_POINT('Ctrl Pts',(3.54339279973578,-29.7355399610821,
122.961101363275));
#101090=CARTESIAN_POINT('Ctrl Pts',(3.54726113385065,-29.6654305296703,
122.972671503672));
#101091=CARTESIAN_POINT('Ctrl Pts',(3.54955885302162,-29.6237868195261,
122.97954395383));
#101092=CARTESIAN_POINT('Ctrl Pts',(3.55185657219259,-29.5823972321476,
122.987693065517));
#101093=CARTESIAN_POINT('Ctrl Pts',(3.55415429136355,-29.541344447052,122.99709394972));
#101094=CARTESIAN_POINT('Ctrl Pts',(3.55802336471178,-29.4722166621203,
123.012923869659));
#101095=CARTESIAN_POINT('Ctrl Pts',(3.56189243806001,-29.4037739608203,
123.032367785461));
#101096=CARTESIAN_POINT('Ctrl Pts',(3.56576151140823,-29.3364222085184,
123.055350397333));
#101097=CARTESIAN_POINT('Ctrl Pts',(3.56962481980402,-29.2691708109044,
123.078298764916));
#101098=CARTESIAN_POINT('Ctrl Pts',(3.57348812819982,-29.2030075916806,
123.104775206827));
#101099=CARTESIAN_POINT('Ctrl Pts',(3.57735143659561,-29.1383266436017,
123.13465376153));
#101100=CARTESIAN_POINT('Ctrl Pts',(3.58121021308853,-29.0737215703287,
123.164497266816));
#101101=CARTESIAN_POINT('Ctrl Pts',(3.58506898958144,-29.0105957532282,
123.197734754905));
#101102=CARTESIAN_POINT('Ctrl Pts',(3.58892776607436,-28.9493249145678,
123.2341915655));
#101103=CARTESIAN_POINT('Ctrl Pts',(3.59278411166257,-28.8880926745592,
123.27062540948));
#101104=CARTESIAN_POINT('Ctrl Pts',(3.59664045725078,-28.8287135110409,
123.310274304497));
#101105=CARTESIAN_POINT('Ctrl Pts',(3.60049680283899,-28.771538743971,123.352917577977));
#101106=CARTESIAN_POINT('Ctrl Pts',(3.60435200908432,-28.714380868972,123.395548252663));
#101107=CARTESIAN_POINT('Ctrl Pts',(3.60820721532965,-28.6594264866417,
123.441171259207));
#101108=CARTESIAN_POINT('Ctrl Pts',(3.61206242157498,-28.6069966629045,
123.489523497256));
#101109=CARTESIAN_POINT('Ctrl Pts',(3.61591777842622,-28.5545647909652,
123.537877624215));
#101110=CARTESIAN_POINT('Ctrl Pts',(3.61977313527747,-28.5046580290379,
123.588960863403));
#101111=CARTESIAN_POINT('Ctrl Pts',(3.62362849212871,-28.4575618745395,
123.642472029155));
#101112=CARTESIAN_POINT('Ctrl Pts',(3.62748788459728,-28.4104164218662,
123.696039208033));
#101113=CARTESIAN_POINT('Ctrl Pts',(3.63134727706584,-28.36608777116,123.75203902136));
#101114=CARTESIAN_POINT('Ctrl Pts',(3.63520666953441,-28.3248216537974,
123.810136532659));
#101115=CARTESIAN_POINT('Ctrl Pts',(3.63906824713785,-28.2835321721272,
123.868266937968));
#101116=CARTESIAN_POINT('Ctrl Pts',(3.64292982474129,-28.2453089360093,
123.928496995213));
#101117=CARTESIAN_POINT('Ctrl Pts',(3.64679140234473,-28.2103532700133,
123.990464391739));
#101118=CARTESIAN_POINT('Ctrl Pts',(3.65065973645961,-28.1753364429113,
124.05254021116));
#101119=CARTESIAN_POINT('Ctrl Pts',(3.65452807057448,-28.1435988168498,
124.116359003769));
#101120=CARTESIAN_POINT('Ctrl Pts',(3.65839640468936,-28.1152945581266,
124.181536219572));
#101121=CARTESIAN_POINT('Ctrl Pts',(3.66069412386027,-28.0984823500919,
124.220250284544));
#101122=CARTESIAN_POINT('Ctrl Pts',(3.66299184303119,-28.0828805480776,
124.259443265274));
#101123=CARTESIAN_POINT('Ctrl Pts',(3.66528956220211,-28.0685130841419,
124.299032200191));
#101124=CARTESIAN_POINT('Ctrl Pts',(3.66976608681314,-28.0405217148223,
124.376161226107));
#101125=CARTESIAN_POINT('Ctrl Pts',(3.67424261142417,-28.01712742101,124.455042428841));
#101126=CARTESIAN_POINT('Ctrl Pts',(3.67871913603519,-27.9985204841637,
124.535158833377));
#101127=CARTESIAN_POINT('Ctrl Pts',(3.68315616207655,-27.9800777254367,
124.614568331627));
#101128=CARTESIAN_POINT('Ctrl Pts',(3.68759318811791,-27.9663383039422,
124.695191164252));
#101129=CARTESIAN_POINT('Ctrl Pts',(3.69203021415927,-27.957441161254,124.77650290212));
#101130=CARTESIAN_POINT('Ctrl Pts',(3.69604504924381,-27.949390597592,124.850077682826));
#101131=CARTESIAN_POINT('Ctrl Pts',(3.70005988432834,-27.945304178903,124.924216166571));
#101132=CARTESIAN_POINT('Ctrl Pts',(3.70407471941287,-27.9452505355246,
124.998516511556));
#101133=CARTESIAN_POINT('Ctrl Pts',(3.70407471946233,-27.9452505355239,
124.998516512471));
#101134=CARTESIAN_POINT('Ctrl Pts',(3.70793830290607,-27.9451989130944,
125.070017726521));
#101135=CARTESIAN_POINT('Ctrl Pts',(3.71180188634981,-27.94888376533,125.14155223813));
#101136=CARTESIAN_POINT('Ctrl Pts',(3.71566546979354,-27.9562889262007,
125.212703101364));
#101137=CARTESIAN_POINT('Ctrl Pts',(3.719528826635,-27.9636936527526,125.283849791542));
#101138=CARTESIAN_POINT('Ctrl Pts',(3.72339218347645,-27.9748182037561,
125.354612398354));
#101139=CARTESIAN_POINT('Ctrl Pts',(3.7272555403179,-27.9895945586335,125.424579231503));
#101140=CARTESIAN_POINT('Ctrl Pts',(3.73111993975008,-28.0043749011546,
125.494564946359));
#101141=CARTESIAN_POINT('Ctrl Pts',(3.73498433918225,-28.0228089023206,
125.563753989817));
#101142=CARTESIAN_POINT('Ctrl Pts',(3.73884873861442,-28.0447778295693,
125.631746647602));
#101143=CARTESIAN_POINT('Ctrl Pts',(3.74271803189476,-28.0667745781126,
125.699825410809));
#101144=CARTESIAN_POINT('Ctrl Pts',(3.7465873251751,-28.0923150338203,125.766704306565));
#101145=CARTESIAN_POINT('Ctrl Pts',(3.75045661845545,-28.1212314339412,
125.832001344764));
#101146=CARTESIAN_POINT('Ctrl Pts',(3.75432884727638,-28.1501697722456,
125.89734792227));
#101147=CARTESIAN_POINT('Ctrl Pts',(3.75820107609731,-28.1824889322509,
125.961109825259));
#101148=CARTESIAN_POINT('Ctrl Pts',(3.76207330491825,-28.2179753493701,
126.022929961946));
#101149=CARTESIAN_POINT('Ctrl Pts',(3.76595231070743,-28.2535238729228,
126.084858292938));
#101150=CARTESIAN_POINT('Ctrl Pts',(3.76983131649661,-28.2922504492806,
126.144837675188));
#101151=CARTESIAN_POINT('Ctrl Pts',(3.77371032228579,-28.3338989370491,
126.202540980813));
#101152=CARTESIAN_POINT('Ctrl Pts',(3.77461515920409,-28.3436140783436,
126.216001151814));
#101153=CARTESIAN_POINT('Ctrl Pts',(3.77551999612238,-28.3534880425284,
126.229337625417));
#101154=CARTESIAN_POINT('Ctrl Pts',(3.77642483304068,-28.3635172836502,
126.242546530955));
#101155=CARTESIAN_POINT('Ctrl Pts',(3.78029390638889,-28.4064022154457,
126.299027675063));
#101156=CARTESIAN_POINT('Ctrl Pts',(3.7841629797371,-28.4522986437701,126.353396665213));
#101157=CARTESIAN_POINT('Ctrl Pts',(3.78803205308531,-28.500970858232,126.405314624784));
#101158=CARTESIAN_POINT('Ctrl Pts',(3.7918953614811,-28.5495705506775,126.457155226149));
#101159=CARTESIAN_POINT('Ctrl Pts',(3.79575866987688,-28.6009374899867,
126.506551694649));
#101160=CARTESIAN_POINT('Ctrl Pts',(3.79962197827266,-28.6547946429129,
126.553196738911));
#101161=CARTESIAN_POINT('Ctrl Pts',(3.80348075476557,-28.7085886180233,
126.599787065613));
#101162=CARTESIAN_POINT('Ctrl Pts',(3.80733953125848,-28.7648666388798,
126.643632062676));
#101163=CARTESIAN_POINT('Ctrl Pts',(3.81119830775139,-28.8233148545274,
126.684461228679));
#101164=CARTESIAN_POINT('Ctrl Pts',(3.81505465333959,-28.8817262496846,
126.725264673625));
#101165=CARTESIAN_POINT('Ctrl Pts',(3.8189109989278,-28.9423047299235,126.763055779299));
#101166=CARTESIAN_POINT('Ctrl Pts',(3.822767344516,-29.0047045580445,126.797605225216));
#101167=CARTESIAN_POINT('Ctrl Pts',(3.82662255076133,-29.0670859503699,
126.832144463628));
#101168=CARTESIAN_POINT('Ctrl Pts',(3.83047775700666,-29.1312871975191,
126.863443708473));
#101169=CARTESIAN_POINT('Ctrl Pts',(3.834332963252,-29.1969363517463,126.891318677366));
#101170=CARTESIAN_POINT('Ctrl Pts',(3.83818832010324,-29.2625880705965,
126.919194735211));
#101171=CARTESIAN_POINT('Ctrl Pts',(3.84204367695448,-29.3296873608155,
126.943646063685));
#101172=CARTESIAN_POINT('Ctrl Pts',(3.84589903380572,-29.3978422093966,
126.96453647401));
#101173=CARTESIAN_POINT('Ctrl Pts',(3.84975842627427,-29.4660683994638,
126.985448751494));
#101174=CARTESIAN_POINT('Ctrl Pts',(3.85361781874282,-29.535351888136,127.002792527423));
#101175=CARTESIAN_POINT('Ctrl Pts',(3.85747721121138,-29.6052862753463,
127.016481747517));
#101176=CARTESIAN_POINT('Ctrl Pts',(3.86133878881481,-29.6752602584438,
127.030178718259));
#101177=CARTESIAN_POINT('Ctrl Pts',(3.86520036641824,-29.7458853925284,
127.040216945716));
#101178=CARTESIAN_POINT('Ctrl Pts',(3.86906194402167,-29.8167486103759,
127.046562115036));
#101179=CARTESIAN_POINT('Ctrl Pts',(3.87293027813654,-29.8877358159276,
127.052918386349));
#101180=CARTESIAN_POINT('Ctrl Pts',(3.87679861225141,-29.9589614513313,
127.055568680571));
#101181=CARTESIAN_POINT('Ctrl Pts',(3.88066694636628,-30.0300115980944,
127.054530814196));
#101182=CARTESIAN_POINT('Ctrl Pts',(3.88296466553726,-30.0722140758202,
127.053914340697));
#101183=CARTESIAN_POINT('Ctrl Pts',(3.88526238470825,-30.1143546997385,
127.051997629856));
#101184=CARTESIAN_POINT('Ctrl Pts',(3.88756010387923,-30.1563480122916,
127.048793025552));
#101185=CARTESIAN_POINT('Ctrl Pts',(3.89142879128781,-30.2270524750349,
127.043397408683));
#101186=CARTESIAN_POINT('Ctrl Pts',(3.8952974786964,-30.2976157809519,127.034326880076));
#101187=CARTESIAN_POINT('Ctrl Pts',(3.89916616610498,-30.3676255076527,
127.021595668927));
#101188=CARTESIAN_POINT('Ctrl Pts',(3.90302937629839,-30.4375361158937,
127.008882482388));
#101189=CARTESIAN_POINT('Ctrl Pts',(3.9068925864918,-30.506894226168,126.992518983124));
#101190=CARTESIAN_POINT('Ctrl Pts',(3.91075579668521,-30.5752914471932,
126.97257124416));
#101191=CARTESIAN_POINT('Ctrl Pts',(3.91461452951295,-30.6436093975202,
126.952646624134));
#101192=CARTESIAN_POINT('Ctrl Pts',(3.91847326234069,-30.7109682064446,
126.929146150395));
#101193=CARTESIAN_POINT('Ctrl Pts',(3.92233199516844,-30.7769704042266,
126.902186781958));
#101194=CARTESIAN_POINT('Ctrl Pts',(3.92618810388979,-30.8429277176394,
126.875245747066));
#101195=CARTESIAN_POINT('Ctrl Pts',(3.93004421261113,-30.9075298028326,
126.844850670379));
#101196=CARTESIAN_POINT('Ctrl Pts',(3.93390032133248,-30.9703965489165,
126.811167606919));
#101197=CARTESIAN_POINT('Ctrl Pts',(3.93775577558456,-31.0332526250852,
126.777490260239));
#101198=CARTESIAN_POINT('Ctrl Pts',(3.94161122983664,-31.0943735152382,
126.740526257114));
#101199=CARTESIAN_POINT('Ctrl Pts',(3.94546668408872,-31.1534025914141,
126.700488172443));
#101200=CARTESIAN_POINT('Ctrl Pts',(3.94765970066917,-31.1869788535919,
126.677714154703));
#101201=CARTESIAN_POINT('Ctrl Pts',(3.94985271724962,-31.2198787848706,
126.653946372515));
#101202=CARTESIAN_POINT('Ctrl Pts',(3.95204573383007,-31.2520409112987,
126.629230222815));
#101203=CARTESIAN_POINT('',(3.6459252804912,-27.9452507844795,125.001795499313));
#101204=CARTESIAN_POINT('Ctrl Pts',(3.64592528053768,-27.9452507844802,
125.001795500168));
#101205=CARTESIAN_POINT('Ctrl Pts',(3.65155534725441,-27.9453413655908,
125.105455454725));
#101206=CARTESIAN_POINT('Ctrl Pts',(3.65718541397115,-27.9532796299144,
125.208784026561));
#101207=CARTESIAN_POINT('Ctrl Pts',(3.66281548068789,-27.9688964527697,
125.310831052066));
#101208=CARTESIAN_POINT('Ctrl Pts',(3.66436496634941,-27.9731944556727,
125.33891604835));
#101209=CARTESIAN_POINT('Ctrl Pts',(3.66591445201094,-27.9780738114693,
125.366904156524));
#101210=CARTESIAN_POINT('Ctrl Pts',(3.66746393767247,-27.9835304264076,
125.394775912735));
#101211=CARTESIAN_POINT('Ctrl Pts',(3.67133301102068,-27.9971556208534,
125.464371825626));
#101212=CARTESIAN_POINT('Ctrl Pts',(3.6752020843689,-28.0144147564085,125.533397845813));
#101213=CARTESIAN_POINT('Ctrl Pts',(3.67907115771711,-28.0352454688279,
125.601445920045));
#101214=CARTESIAN_POINT('Ctrl Pts',(3.6829344661129,-28.0560451433074,125.669392602063));
#101215=CARTESIAN_POINT('Ctrl Pts',(3.68679777450868,-28.0804056902298,
125.736363769799));
#101216=CARTESIAN_POINT('Ctrl Pts',(3.69066108290446,-28.1082137350865,
125.801961526748));
#101217=CARTESIAN_POINT('Ctrl Pts',(3.69451985939738,-28.1359891593639,
125.867482333417));
#101218=CARTESIAN_POINT('Ctrl Pts',(3.69837863589029,-28.167203859883,125.931632484396));
#101219=CARTESIAN_POINT('Ctrl Pts',(3.7022374123832,-28.2016952041954,125.994030896847));
#101220=CARTESIAN_POINT('Ctrl Pts',(3.70609375797141,-28.2361648200736,
126.056390000311));
#101221=CARTESIAN_POINT('Ctrl Pts',(3.70995010355962,-28.2739067499914,
126.1169991305));
#101222=CARTESIAN_POINT('Ctrl Pts',(3.71380644914783,-28.3147115970116,
126.175500132392));
#101223=CARTESIAN_POINT('Ctrl Pts',(3.71766165539316,-28.3555043883924,
126.233983850381));
#101224=CARTESIAN_POINT('Ctrl Pts',(3.72151686163849,-28.3993580225826,
126.290360278361));
#101225=CARTESIAN_POINT('Ctrl Pts',(3.72537206788382,-28.4460197348839,
126.3443001518));
#101226=CARTESIAN_POINT('Ctrl Pts',(3.72922742473507,-28.4926832700525,
126.398242132433));
#101227=CARTESIAN_POINT('Ctrl Pts',(3.73308278158632,-28.5421547816391,
126.449747003594));
#101228=CARTESIAN_POINT('Ctrl Pts',(3.73693813843757,-28.5941423085762,
126.498519841031));
#101229=CARTESIAN_POINT('Ctrl Pts',(3.74079753090613,-28.6461842537608,
126.547343731721));
#101230=CARTESIAN_POINT('Ctrl Pts',(3.74465692337469,-28.7007471166532,
126.593429546882));
#101231=CARTESIAN_POINT('Ctrl Pts',(3.74851631584325,-28.7575039387415,
126.63652103569));
#101232=CARTESIAN_POINT('Ctrl Pts',(3.75237789344669,-28.8142928957609,
126.679636922306));
#101233=CARTESIAN_POINT('Ctrl Pts',(3.75623947105013,-28.8732778829183,
126.719754834329));
#101234=CARTESIAN_POINT('Ctrl Pts',(3.76010104865356,-28.9341031682011,
126.756662035356));
#101235=CARTESIAN_POINT('Ctrl Pts',(3.76396938276844,-28.9950348780537,
126.793633812044));
#101236=CARTESIAN_POINT('Ctrl Pts',(3.76783771688331,-29.0578128866984,
126.827383431727));
#101237=CARTESIAN_POINT('Ctrl Pts',(3.77170605099818,-29.1220577374244,
126.857744585804));
#101238=CARTESIAN_POINT('Ctrl Pts',(3.77400377016912,-29.1602179947248,
126.87577855177));
#101239=CARTESIAN_POINT('Ctrl Pts',(3.77630148934007,-29.1988953899815,
126.892617941925));
#101240=CARTESIAN_POINT('Ctrl Pts',(3.77859920851102,-29.2380077640326,
126.908236199957));
#101241=CARTESIAN_POINT('Ctrl Pts',(3.78246828185923,-29.3038681380679,
126.934535404255));
#101242=CARTESIAN_POINT('Ctrl Pts',(3.78633735520744,-29.3712206395651,
126.957472487004));
#101243=CARTESIAN_POINT('Ctrl Pts',(3.79020642855565,-29.4396886210872,
126.976878529693));
#101244=CARTESIAN_POINT('Ctrl Pts',(3.79406973695143,-29.5080545847303,
126.996255657212));
#101245=CARTESIAN_POINT('Ctrl Pts',(3.79793304534722,-29.5775322656589,
127.012112056774));
#101246=CARTESIAN_POINT('Ctrl Pts',(3.801796353743,-29.6477258834258,127.024327174469));
#101247=CARTESIAN_POINT('Ctrl Pts',(3.80565513023591,-29.7178371596798,
127.036527963064));
#101248=CARTESIAN_POINT('Ctrl Pts',(3.80951390672882,-29.7886622282979,
127.04509587146));
#101249=CARTESIAN_POINT('Ctrl Pts',(3.81337268322173,-29.8597927189906,
127.049960848614));
#101250=CARTESIAN_POINT('Ctrl Pts',(3.81722902880993,-29.9308783997689,
127.054822760991));
#101251=CARTESIAN_POINT('Ctrl Pts',(3.82108537439813,-30.0022686373834,
127.05598633715));
#101252=CARTESIAN_POINT('Ctrl Pts',(3.82494171998634,-30.0735489608218,
127.05343325016));
#101253=CARTESIAN_POINT('Ctrl Pts',(3.82879692623166,-30.1448082247554,
127.05088091747));
#101254=CARTESIAN_POINT('Ctrl Pts',(3.83265213247699,-30.215957153772,127.044614118991));
#101255=CARTESIAN_POINT('Ctrl Pts',(3.83650733872232,-30.2865820279036,
127.0346666321));
#101256=CARTESIAN_POINT('Ctrl Pts',(3.84036269557357,-30.3572096610377,
127.024718756606));
#101257=CARTESIAN_POINT('Ctrl Pts',(3.84421805242481,-30.4273127179105,
127.011089977162));
#101258=CARTESIAN_POINT('Ctrl Pts',(3.84807340927605,-30.4964850706124,
126.993865626656));
#101259=CARTESIAN_POINT('Ctrl Pts',(3.85193280174461,-30.5657298298786,
126.97662324646));
#101260=CARTESIAN_POINT('Ctrl Pts',(3.85579219421316,-30.6340414678542,
126.955777899661));
#101261=CARTESIAN_POINT('Ctrl Pts',(3.85965158668172,-30.7010273665053,
126.931465297102));
#101262=CARTESIAN_POINT('Ctrl Pts',(3.86351316428515,-30.7680511916499,
126.907138929083));
#101263=CARTESIAN_POINT('Ctrl Pts',(3.86737474188858,-30.8337473356283,
126.87934158674));
#101264=CARTESIAN_POINT('Ctrl Pts',(3.87123631949202,-30.8977441330561,
126.848256755449));
#101265=CARTESIAN_POINT('Ctrl Pts',(3.87510465360688,-30.9618529041741,
126.817117535761));
#101266=CARTESIAN_POINT('Ctrl Pts',(3.87897298772175,-31.0242559669951,
126.782679577798));
#101267=CARTESIAN_POINT('Ctrl Pts',(3.88284132183662,-31.0846077947283,
126.745171479859));
#101268=CARTESIAN_POINT('Ctrl Pts',(3.88513904100761,-31.12045566812,126.722892360957));
#101269=CARTESIAN_POINT('Ctrl Pts',(3.88743676017859,-31.1555804033926,
126.699530876914));
#101270=CARTESIAN_POINT('Ctrl Pts',(3.88973447934958,-31.1899151292548,
126.675141650032));
#101271=CARTESIAN_POINT('Ctrl Pts',(3.89113844260586,-31.2108944961563,
126.660239229047));
#101272=CARTESIAN_POINT('Ctrl Pts',(3.89254240586213,-31.2316087312057,
126.644932070857));
#101273=CARTESIAN_POINT('Ctrl Pts',(3.89394636911841,-31.2520409112987,
126.629230222815));
#101274=CARTESIAN_POINT('Ctrl Pts',(3.19385981518126,-31.2520409112986,
126.629230222815));
#101275=CARTESIAN_POINT('Ctrl Pts',(3.19772164077073,-31.3085714957689,
126.585787249867));
#101276=CARTESIAN_POINT('Ctrl Pts',(3.2015834663602,-31.3627857733034,126.539439075722));
#101277=CARTESIAN_POINT('Ctrl Pts',(3.20544529194967,-31.414385544613,126.490473446154));
#101278=CARTESIAN_POINT('Ctrl Pts',(3.20931377041992,-31.4660742083699,
126.441423462052));
#101279=CARTESIAN_POINT('Ctrl Pts',(3.21318224889018,-31.5151390411146,
126.389747374098));
#101280=CARTESIAN_POINT('Ctrl Pts',(3.21705072736043,-31.5613205159542,
126.335767872409));
#101281=CARTESIAN_POINT('Ctrl Pts',(3.21900810301303,-31.5846874534069,
126.308455283453));
#101282=CARTESIAN_POINT('Ctrl Pts',(3.22096547866562,-31.6073168710985,
126.280553478093));
#101283=CARTESIAN_POINT('Ctrl Pts',(3.22292285431822,-31.6291794168833,
126.252107020228));
#101284=CARTESIAN_POINT('Ctrl Pts',(3.22679192766652,-31.6723943169508,
126.195877940321));
#101285=CARTESIAN_POINT('Ctrl Pts',(3.23066100101482,-31.71277943223,126.137298834087));
#101286=CARTESIAN_POINT('Ctrl Pts',(3.23453007436312,-31.7500698029317,
126.076686234409));
#101287=CARTESIAN_POINT('Ctrl Pts',(3.23839338275899,-31.7873046106615,
126.016163948024));
#101288=CARTESIAN_POINT('Ctrl Pts',(3.24225669115486,-31.821453574431,125.953614592888));
#101289=CARTESIAN_POINT('Ctrl Pts',(3.24611999955073,-31.8522930751951,
125.889386263715));
#101290=CARTESIAN_POINT('Ctrl Pts',(3.24997877604373,-31.883096399292,125.825233278397));
#101291=CARTESIAN_POINT('Ctrl Pts',(3.25383755253673,-31.9105977625118,
125.759405667015));
#101292=CARTESIAN_POINT('Ctrl Pts',(3.25769632902973,-31.9346187232605,
125.692277370791));
#101293=CARTESIAN_POINT('Ctrl Pts',(3.26155267461802,-31.9586245515789,
125.625191363229));
#101294=CARTESIAN_POINT('Ctrl Pts',(3.26540902020632,-31.9791541641106,
125.556806752785));
#101295=CARTESIAN_POINT('Ctrl Pts',(3.26926536579461,-31.9960772362334,
125.487517414551));
#101296=CARTESIAN_POINT('Ctrl Pts',(3.27312057204003,-32.0129953084979,
125.418248547594));
#101297=CARTESIAN_POINT('Ctrl Pts',(3.27697577828545,-32.0263088405465,
125.348075955166));
#101298=CARTESIAN_POINT('Ctrl Pts',(3.28083098453088,-32.0359378534953,
125.277406955942));
#101299=CARTESIAN_POINT('Ctrl Pts',(3.28468634138221,-32.0455672426072,
125.206735195991));
#101300=CARTESIAN_POINT('Ctrl Pts',(3.28854169823355,-32.0515117634471,
125.135567472378));
#101301=CARTESIAN_POINT('Ctrl Pts',(3.29239705508489,-32.0537431147043,
125.064317814832));
#101302=CARTESIAN_POINT('Ctrl Pts',(3.29625644755354,-32.0559768016414,
124.99299357629));
#101303=CARTESIAN_POINT('Ctrl Pts',(3.30011584002218,-32.0544895448684,
124.921587719152));
#101304=CARTESIAN_POINT('Ctrl Pts',(3.30397523249083,-32.0493051964147,
124.850514969152));
#101305=CARTESIAN_POINT('Ctrl Pts',(3.30783681009436,-32.0441179126543,
124.779401978739));
#101306=CARTESIAN_POINT('Ctrl Pts',(3.31169838769789,-32.0352294307718,
124.708622953139));
#101307=CARTESIAN_POINT('Ctrl Pts',(3.31555996530141,-32.0227152743542,
124.638585443854));
#101308=CARTESIAN_POINT('Ctrl Pts',(3.31942829941637,-32.0101792222116,
124.568425391588));
#101309=CARTESIAN_POINT('Ctrl Pts',(3.32329663353133,-31.9940049403116,
124.499009919225));
#101310=CARTESIAN_POINT('Ctrl Pts',(3.3271649676463,-31.9743184724289,124.430733689802));
#101311=CARTESIAN_POINT('Ctrl Pts',(3.32946268681646,-31.9626250733319,
124.390178867869));
#101312=CARTESIAN_POINT('Ctrl Pts',(3.33176040598662,-31.9496934720421,
124.350025665612));
#101313=CARTESIAN_POINT('Ctrl Pts',(3.33405812515678,-31.9355580520013,
124.310353286216));
#101314=CARTESIAN_POINT('Ctrl Pts',(3.33792719850498,-31.911755762472,124.243549932798));
#101315=CARTESIAN_POINT('Ctrl Pts',(3.34179627185318,-31.884444339824,124.177849434962));
#101316=CARTESIAN_POINT('Ctrl Pts',(3.34566534520138,-31.8537460124449,
124.113646073036));
#101317=CARTESIAN_POINT('Ctrl Pts',(3.34952865359714,-31.8230934258366,
124.049538374669));
#101318=CARTESIAN_POINT('Ctrl Pts',(3.35339196199291,-31.7890641595371,
123.986923818938));
#101319=CARTESIAN_POINT('Ctrl Pts',(3.35725527038868,-31.7518293801401,
123.926179072015));
#101320=CARTESIAN_POINT('Ctrl Pts',(3.36111404688158,-31.7146382794729,
123.865505582488));
#101321=CARTESIAN_POINT('Ctrl Pts',(3.36497282337447,-31.6742493875133,
123.806697957087));
#101322=CARTESIAN_POINT('Ctrl Pts',(3.36883159986737,-31.6308800882599,
123.750108924659));
#101323=CARTESIAN_POINT('Ctrl Pts',(3.37268794545556,-31.5875381102661,
123.693555541496));
#101324=CARTESIAN_POINT('Ctrl Pts',(3.37654429104375,-31.5412197448298,
123.639218363069));
#101325=CARTESIAN_POINT('Ctrl Pts',(3.38040063663193,-31.4921852201793,
123.587420504475));
#101326=CARTESIAN_POINT('Ctrl Pts',(3.38425584287725,-31.4431651825956,
123.535637949364));
#101327=CARTESIAN_POINT('Ctrl Pts',(3.38811104912256,-31.3914309127222,
123.486393577259));
#101328=CARTESIAN_POINT('Ctrl Pts',(3.39196625536788,-31.3372812390443,
123.439975496923));
#101329=CARTESIAN_POINT('Ctrl Pts',(3.39582161221911,-31.2831294499774,
123.393555603237));
#101330=CARTESIAN_POINT('Ctrl Pts',(3.39967696907034,-31.2265624400241,
123.349962535016));
#101331=CARTESIAN_POINT('Ctrl Pts',(3.40353232592156,-31.1679127039799,
123.309444624278));
#101332=CARTESIAN_POINT('Ctrl Pts',(3.40739171839011,-31.1092015759818,
123.26888430118));
#101333=CARTESIAN_POINT('Ctrl Pts',(3.41125111085865,-31.0484037704135,
123.231405837976));
#101334=CARTESIAN_POINT('Ctrl Pts',(3.41511050332719,-30.985880652913,123.197214127881));
#101335=CARTESIAN_POINT('Ctrl Pts',(3.41897208093061,-30.9233221356842,
123.16300305891));
#101336=CARTESIAN_POINT('Ctrl Pts',(3.42283365853403,-30.8590367999064,
123.13208265822));
#101337=CARTESIAN_POINT('Ctrl Pts',(3.42669523613745,-30.793408008632,123.104610516454));
#101338=CARTESIAN_POINT('Ctrl Pts',(3.4305635702523,-30.7276643882062,123.077090307328));
#101339=CARTESIAN_POINT('Ctrl Pts',(3.43443190436716,-30.6605730766348,
123.053030566895));
#101340=CARTESIAN_POINT('Ctrl Pts',(3.43830023848201,-30.5925340091425,
123.032539451346));
#101341=CARTESIAN_POINT('Ctrl Pts',(3.44059795765313,-30.5521200570071,
123.02036810636));
#101342=CARTESIAN_POINT('Ctrl Pts',(3.44289567682424,-30.5113719666559,
123.00945485306));
#101343=CARTESIAN_POINT('Ctrl Pts',(3.44519339599535,-30.4703749284779,
122.999813761381));
#101344=CARTESIAN_POINT('Ctrl Pts',(3.44906246934355,-30.4013410144278,
122.983579361925));
#101345=CARTESIAN_POINT('Ctrl Pts',(3.45293154269175,-30.3313304296167,
122.970891287314));
#101346=CARTESIAN_POINT('Ctrl Pts',(3.45680061603996,-30.2607407184091,
122.961860691645));
#101347=CARTESIAN_POINT('Ctrl Pts',(3.46066392443573,-30.1902561864759,
122.95284355164));
#101348=CARTESIAN_POINT('Ctrl Pts',(3.4645272328315,-30.1191947189178,122.947473134267));
#101349=CARTESIAN_POINT('Ctrl Pts',(3.46839054122728,-30.0479656040059,
122.945809925218));
#101350=CARTESIAN_POINT('Ctrl Pts',(3.47224931772018,-29.97682004531,122.944148667218));
#101351=CARTESIAN_POINT('Ctrl Pts',(3.47610809421308,-29.9055077131915,
122.946185990665));
#101352=CARTESIAN_POINT('Ctrl Pts',(3.47996687070598,-29.8344428517917,
122.951930569249));
#101353=CARTESIAN_POINT('Ctrl Pts',(3.48382321629417,-29.7634227589621,
122.957671528934));
#101354=CARTESIAN_POINT('Ctrl Pts',(3.48767956188236,-29.6926503106128,
122.967115071211));
#101355=CARTESIAN_POINT('Ctrl Pts',(3.49153590747056,-29.6225381082558,
122.980217813035));
#101356=CARTESIAN_POINT('Ctrl Pts',(3.49539111371587,-29.5524466202867,
122.993316683703));
#101357=CARTESIAN_POINT('Ctrl Pts',(3.49924631996119,-29.4830154683063,
123.010072518449));
#101358=CARTESIAN_POINT('Ctrl Pts',(3.50310152620651,-29.4146487788748,
123.030390518294));
#101359=CARTESIAN_POINT('Ctrl Pts',(3.50695688305774,-29.3462794186581,
123.050709311873));
#101360=CARTESIAN_POINT('Ctrl Pts',(3.51081223990897,-29.278975068579,123.07459040633));
#101361=CARTESIAN_POINT('Ctrl Pts',(3.5146675967602,-29.2131246964193,123.101889144672));
#101362=CARTESIAN_POINT('Ctrl Pts',(3.51852698922875,-29.1472053949978,
123.129216458128));
#101363=CARTESIAN_POINT('Ctrl Pts',(3.52238638169729,-29.0827435593424,
123.159968370426));
#101364=CARTESIAN_POINT('Ctrl Pts',(3.52624577416584,-29.020107320911,123.193952409274));
#101365=CARTESIAN_POINT('Ctrl Pts',(3.53010735176926,-28.9574356187039,
123.227955689417));
#101366=CARTESIAN_POINT('Ctrl Pts',(3.53396892937268,-28.8965919858927,
123.265194485332));
#101367=CARTESIAN_POINT('Ctrl Pts',(3.5378305069761,-28.8379167435928,123.305432188528));
#101368=CARTESIAN_POINT('Ctrl Pts',(3.54169884109096,-28.7791388386026,
123.345740294685));
#101369=CARTESIAN_POINT('Ctrl Pts',(3.54556717520581,-28.7225372848184,
123.389057488815));
#101370=CARTESIAN_POINT('Ctrl Pts',(3.54943550932067,-28.6684198594702,
123.435106427949));
#101371=CARTESIAN_POINT('Ctrl Pts',(3.55173322849175,-28.6362751061941,
123.462458649115));
#101372=CARTESIAN_POINT('Ctrl Pts',(3.55403094766283,-28.605006105976,123.490773938098));
#101373=CARTESIAN_POINT('Ctrl Pts',(3.55632866683391,-28.5746708837891,
123.519988353768));
#101374=CARTESIAN_POINT('Ctrl Pts',(3.56013990426075,-28.5243537103043,
123.568446440295));
#101375=CARTESIAN_POINT('Ctrl Pts',(3.5639511416876,-28.4763982156428,123.619581983347));
#101376=CARTESIAN_POINT('Ctrl Pts',(3.56776237911444,-28.4311089343795,
123.673132114069));
#101377=CARTESIAN_POINT('Ctrl Pts',(3.57156855056504,-28.3858798525731,
123.72661106484));
#101378=CARTESIAN_POINT('Ctrl Pts',(3.57537472201564,-28.343310282624,123.782497865398));
#101379=CARTESIAN_POINT('Ctrl Pts',(3.57918089346624,-28.303669205142,123.840491743489));
#101380=CARTESIAN_POINT('Ctrl Pts',(3.58298336737577,-28.2640666373578,
123.898429282882));
#101381=CARTESIAN_POINT('Ctrl Pts',(3.5867858412853,-28.2273872042862,123.958469430919));
#101382=CARTESIAN_POINT('Ctrl Pts',(3.59058831519483,-28.1938594686753,
124.020278639813));
#101383=CARTESIAN_POINT('Ctrl Pts',(3.59438845464245,-28.1603523168273,
124.082049902033));
#101384=CARTESIAN_POINT('Ctrl Pts',(3.59818859409007,-28.1299932630402,
124.145587631281));
#101385=CARTESIAN_POINT('Ctrl Pts',(3.60198873353769,-28.1029663478004,
124.210531264126));
#101386=CARTESIAN_POINT('Ctrl Pts',(3.60578956781187,-28.0759344908949,
124.27548677142));
#101387=CARTESIAN_POINT('Ctrl Pts',(3.60959040208607,-28.0522361979834,
124.341848239274));
#101388=CARTESIAN_POINT('Ctrl Pts',(3.61339123636026,-28.032007893898,124.40923385945));
#101389=CARTESIAN_POINT('Ctrl Pts',(3.61719222217678,-28.0117787832937,
124.476622166345));
#101390=CARTESIAN_POINT('Ctrl Pts',(3.6209932079933,-27.9950200700698,124.545034222851));
#101391=CARTESIAN_POINT('Ctrl Pts',(3.62479419380982,-27.9818179362867,
124.614074203757));
#101392=CARTESIAN_POINT('Ctrl Pts',(3.6285996398477,-27.9686003106176,124.683195198803));
#101393=CARTESIAN_POINT('Ctrl Pts',(3.63240508588558,-27.9589476807175,
124.752945093907));
#101394=CARTESIAN_POINT('Ctrl Pts',(3.63621053192346,-27.9528946642781,
124.822920054894));
#101395=CARTESIAN_POINT('Ctrl Pts',(3.63944878144604,-27.9477438416413,
124.882465343869));
#101396=CARTESIAN_POINT('Ctrl Pts',(3.64268703096862,-27.9451986849018,
124.942173328698));
#101397=CARTESIAN_POINT('Ctrl Pts',(3.6459252804912,-27.9452507844795,125.001795499313));
#101398=CARTESIAN_POINT('Origin',(-1.54592528053767,-30.,125.));
#101399=CARTESIAN_POINT('',(2.49394332640294,-31.2520409112987,126.629230222815));
#101400=CARTESIAN_POINT('',(2.55206159779739,-31.2520409112987,126.629230222815));
#101401=CARTESIAN_POINT('',(-1.54592528053767,-31.2520409112987,126.629230222815));
#101402=CARTESIAN_POINT('',(3.00407471949958,-27.9452500948919,124.999375533621));
#101403=CARTESIAN_POINT('Ctrl Pts',(2.55206159779739,-31.2520409112987,
126.629230222815));
#101404=CARTESIAN_POINT('Ctrl Pts',(2.5526866831371,-31.2611311656917,126.622244487936));
#101405=CARTESIAN_POINT('Ctrl Pts',(2.55331176847681,-31.2701601850064,
126.615184799744));
#101406=CARTESIAN_POINT('Ctrl Pts',(2.55393685381652,-31.2791267189991,
126.608052362096));
#101407=CARTESIAN_POINT('Ctrl Pts',(2.55780592716366,-31.334626625145,126.563904911101));
#101408=CARTESIAN_POINT('Ctrl Pts',(2.5616750005108,-31.3879470172231,126.516794349563));
#101409=CARTESIAN_POINT('Ctrl Pts',(2.56554407385794,-31.4387544190603,
126.466963968247));
#101410=CARTESIAN_POINT('Ctrl Pts',(2.56940738225263,-31.4894861174333,
126.417207834626));
#101411=CARTESIAN_POINT('Ctrl Pts',(2.57327069064732,-31.5377119140533,
126.364740262816));
#101412=CARTESIAN_POINT('Ctrl Pts',(2.57713399904201,-31.5831308416319,
126.309845143814));
#101413=CARTESIAN_POINT('Ctrl Pts',(2.5809927755338,-31.6284964899615,126.255014420228));
#101414=CARTESIAN_POINT('Ctrl Pts',(2.58485155202558,-31.6710615013615,
126.197762178345));
#101415=CARTESIAN_POINT('Ctrl Pts',(2.58871032851737,-31.7105625192321,
126.138408288049));
#101416=CARTESIAN_POINT('Ctrl Pts',(2.59256667410444,-31.7500386527355,
126.079091788789));
#101417=CARTESIAN_POINT('Ctrl Pts',(2.5964230196915,-31.7864543537217,126.01767667131));
#101418=CARTESIAN_POINT('Ctrl Pts',(2.60027936527857,-31.8195881549648,
125.954513755172));
#101419=CARTESIAN_POINT('Ctrl Pts',(2.60413457152274,-31.8527121669502,
125.891369500281));
#101420=CARTESIAN_POINT('Ctrl Pts',(2.60798977776692,-31.8825559786222,
125.826478901844));
#101421=CARTESIAN_POINT('Ctrl Pts',(2.61184498401109,-31.9089437403483,
125.760217967878));
#101422=CARTESIAN_POINT('Ctrl Pts',(2.61570034086117,-31.9353325329277,
125.693954445391));
#101423=CARTESIAN_POINT('Ctrl Pts',(2.61955569771125,-31.9582648298261,
125.626320933222));
#101424=CARTESIAN_POINT('Ctrl Pts',(2.62341105456133,-31.9776133151839,
125.557712415235));
#101425=CARTESIAN_POINT('Ctrl Pts',(2.62727044702871,-31.9969820536817,
125.489032080881));
#101426=CARTESIAN_POINT('Ctrl Pts',(2.63112983949608,-32.0127593599251,
125.419375171884));
#101427=CARTESIAN_POINT('Ctrl Pts',(2.63498923196346,-32.0248683641775,
125.34914992518));
#101428=CARTESIAN_POINT('Ctrl Pts',(2.63885080956571,-32.0369842243814,
125.278884917908));
#101429=CARTESIAN_POINT('Ctrl Pts',(2.64271238716795,-32.0454275905173,
125.208051414956));
#101430=CARTESIAN_POINT('Ctrl Pts',(2.6465739647702,-32.0501734694427,125.137063152208));
#101431=CARTESIAN_POINT('Ctrl Pts',(2.65044229888388,-32.0549276521207,
125.065950682968));
#101432=CARTESIAN_POINT('Ctrl Pts',(2.65431063299756,-32.0559714241144,
124.994683399202));
#101433=CARTESIAN_POINT('Ctrl Pts',(2.65817896711124,-32.053331929569,124.923674712497));
#101434=CARTESIAN_POINT('Ctrl Pts',(2.66047668629252,-32.0517641184474,
124.88149686108));
#101435=CARTESIAN_POINT('Ctrl Pts',(2.6627744054738,-32.0488977950344,124.839410162816));
#101436=CARTESIAN_POINT('Ctrl Pts',(2.66507212465508,-32.0447472267912,
124.797499775235));
#101437=CARTESIAN_POINT('Ctrl Pts',(2.66894119800399,-32.0377581860486,
124.726927894671));
#101438=CARTESIAN_POINT('Ctrl Pts',(2.67281027135289,-32.0270976169124,
124.656580034074));
#101439=CARTESIAN_POINT('Ctrl Pts',(2.6766793447018,-32.0127890530529,124.586868313476));
#101440=CARTESIAN_POINT('Ctrl Pts',(2.68054265309829,-31.9985018090762,
124.517260463938));
#101441=CARTESIAN_POINT('Ctrl Pts',(2.68440596149478,-31.9805774566544,
124.448287344925));
#101442=CARTESIAN_POINT('Ctrl Pts',(2.68826926989126,-31.9590912711333,
124.380355784446));
#101443=CARTESIAN_POINT('Ctrl Pts',(2.69212804638489,-31.9376302902544,
124.312503911945));
#101444=CARTESIAN_POINT('Ctrl Pts',(2.69598682287852,-31.9126159214867,
124.245691631966));
#101445=CARTESIAN_POINT('Ctrl Pts',(2.69984559937214,-31.8841740662919,
124.180313687797));
#101446=CARTESIAN_POINT('Ctrl Pts',(2.70370194496107,-31.8557501285482,
124.114976929623));
#101447=CARTESIAN_POINT('Ctrl Pts',(2.70755829055,-31.8239031815397,124.051073158967));
#101448=CARTESIAN_POINT('Ctrl Pts',(2.71141463613892,-31.7888078481915,
123.98897871202));
#101449=CARTESIAN_POINT('Ctrl Pts',(2.71526984238498,-31.7537228836281,
123.926902610645));
#101450=CARTESIAN_POINT('Ctrl Pts',(2.71912504863104,-31.7153916769383,
123.866635194417));
#101451=CARTESIAN_POINT('Ctrl Pts',(2.7229802548771,-31.6740347543116,123.808528135516));
#101452=CARTESIAN_POINT('Ctrl Pts',(2.72683561172908,-31.6326762160522,
123.750418806628));
#101453=CARTESIAN_POINT('Ctrl Pts',(2.73069096858106,-31.5882920106661,
123.694470397124));
#101454=CARTESIAN_POINT('Ctrl Pts',(2.73454632543303,-31.5411449297523,
123.641004095665));
#101455=CARTESIAN_POINT('Ctrl Pts',(2.73840571790233,-31.4939484973562,
123.587481828043));
#101456=CARTESIAN_POINT('Ctrl Pts',(2.74226511037162,-31.4439837381921,
123.536447220084));
#101457=CARTESIAN_POINT('Ctrl Pts',(2.74612450284091,-31.3915519385093,
123.488186266456));
#101458=CARTESIAN_POINT('Ctrl Pts',(2.74998608044508,-31.3390904526635,
123.439897988141));
#101459=CARTESIAN_POINT('Ctrl Pts',(2.75384765804925,-31.2841595199455,
123.394386800424));
#101460=CARTESIAN_POINT('Ctrl Pts',(2.75770923565342,-31.2270931825123,
123.351898096618));
#101461=CARTESIAN_POINT('Ctrl Pts',(2.76157756976903,-31.1699269974518,
123.309335051327));
#101462=CARTESIAN_POINT('Ctrl Pts',(2.76544590388463,-31.1106183524661,
123.269805317836));
#101463=CARTESIAN_POINT('Ctrl Pts',(2.76931423800023,-31.0495292946477,
123.233510310764));
#101464=CARTESIAN_POINT('Ctrl Pts',(2.7716119571647,-31.0132435202823,123.211951745544));
#101465=CARTESIAN_POINT('Ctrl Pts',(2.77390967632917,-30.976330061229,123.191533555241));
#101466=CARTESIAN_POINT('Ctrl Pts',(2.77620739549364,-30.9388682001961,
123.172289939525));
#101467=CARTESIAN_POINT('Ctrl Pts',(2.78007646884175,-30.8757870846558,
123.139886083632));
#101468=CARTESIAN_POINT('Ctrl Pts',(2.78394554218985,-30.8109028729085,
123.110688339052));
#101469=CARTESIAN_POINT('Ctrl Pts',(2.78781461553796,-30.7445745687621,
123.084900453226));
#101470=CARTESIAN_POINT('Ctrl Pts',(2.79167792393363,-30.6783450943571,
123.059150991572));
#101471=CARTESIAN_POINT('Ctrl Pts',(2.79554123232931,-30.6106762477178,
123.036801478187));
#101472=CARTESIAN_POINT('Ctrl Pts',(2.79940454072498,-30.5419506494207,
123.018009319877));
#101473=CARTESIAN_POINT('Ctrl Pts',(2.80326331721779,-30.4733056705576,
122.999239205947));
#101474=CARTESIAN_POINT('Ctrl Pts',(2.80712209371059,-30.4036068686827,
122.984018285609));
#101475=CARTESIAN_POINT('Ctrl Pts',(2.8109808702034,-30.3332541692576,122.972454878141));
#101476=CARTESIAN_POINT('Ctrl Pts',(2.8148372157915,-30.2629457897636,122.960898755248));
#101477=CARTESIAN_POINT('Ctrl Pts',(2.81869356137959,-30.1919848082115,
122.952995652501));
#101478=CARTESIAN_POINT('Ctrl Pts',(2.82254990696769,-30.1207821102329,
122.948802972811));
#101479=CARTESIAN_POINT('Ctrl Pts',(2.82640511321291,-30.0496004488251,
122.944611531833));
#101480=CARTESIAN_POINT('Ctrl Pts',(2.83026031945814,-29.9781776974497,
122.94412836613));
#101481=CARTESIAN_POINT('Ctrl Pts',(2.83411552570336,-29.9069289167095,
122.947358936405));
#101482=CARTESIAN_POINT('Ctrl Pts',(2.8379708825545,-29.8356773525935,122.950589632885));
#101483=CARTESIAN_POINT('Ctrl Pts',(2.84182623940564,-29.7646002577934,
122.957534329175));
#101484=CARTESIAN_POINT('Ctrl Pts',(2.84568159625677,-29.6941100056194,
122.968146443801));
#101485=CARTESIAN_POINT('Ctrl Pts',(2.84954098872523,-29.6235459673619,
122.97876966672));
#101486=CARTESIAN_POINT('Ctrl Pts',(2.85340038119368,-29.5535704793302,
122.993067898798));
#101487=CARTESIAN_POINT('Ctrl Pts',(2.85725977366213,-29.4845872249428,
123.010943129569));
#101488=CARTESIAN_POINT('Ctrl Pts',(2.86112135126546,-29.4155649131867,
123.02882848105));
#101489=CARTESIAN_POINT('Ctrl Pts',(2.86498292886879,-29.3475364169122,
123.050294716615));
#101490=CARTESIAN_POINT('Ctrl Pts',(2.86884450647212,-29.2808890741998,
123.075194285416));
#101491=CARTESIAN_POINT('Ctrl Pts',(2.87271284058689,-29.2141251202007,
123.100137420407));
#101492=CARTESIAN_POINT('Ctrl Pts',(2.87658117470166,-29.1487475902524,
123.128525688683));
#101493=CARTESIAN_POINT('Ctrl Pts',(2.88044950881643,-29.0851220628897,
123.160164158766));
#101494=CARTESIAN_POINT('Ctrl Pts',(2.88274722798835,-29.0473296722359,
123.178956826908));
#101495=CARTESIAN_POINT('Ctrl Pts',(2.88504494716027,-29.0101549265945,
123.198895338703));
#101496=CARTESIAN_POINT('Ctrl Pts',(2.8873426663322,-28.9736695586932,123.219931633968));
#101497=CARTESIAN_POINT('Ctrl Pts',(2.8912117396803,-28.9122327363575,123.255354139184));
#101498=CARTESIAN_POINT('Ctrl Pts',(2.8950808130284,-28.8525115731632,123.294030383693));
#101499=CARTESIAN_POINT('Ctrl Pts',(2.8989498863765,-28.794871956984,123.335769258055));
#101500=CARTESIAN_POINT('Ctrl Pts',(2.90281319477217,-28.7373182243266,
123.377445941135));
#101501=CARTESIAN_POINT('Ctrl Pts',(2.90667650316783,-28.6818402725019,
123.422175913361));
#101502=CARTESIAN_POINT('Ctrl Pts',(2.9105398115635,-28.6287778654823,123.469723090317));
#101503=CARTESIAN_POINT('Ctrl Pts',(2.91439858805629,-28.5757777039916,
123.517214491454));
#101504=CARTESIAN_POINT('Ctrl Pts',(2.91825736454909,-28.5251878188804,
123.567516210343));
#101505=CARTESIAN_POINT('Ctrl Pts',(2.92211614104188,-28.4773161191015,
123.62035100067));
#101506=CARTESIAN_POINT('Ctrl Pts',(2.92597248662997,-28.4294745769492,
123.673152506784));
#101507=CARTESIAN_POINT('Ctrl Pts',(2.92982883221806,-28.3843481482237,
123.728483559244));
#101508=CARTESIAN_POINT('Ctrl Pts',(2.93368517780614,-28.3422079092198,
123.78603008841));
#101509=CARTESIAN_POINT('Ctrl Pts',(2.93754038405135,-28.3000801203918,
123.843559615669));
#101510=CARTESIAN_POINT('Ctrl Pts',(2.94139559029656,-28.2609370566097,
123.90330292844));
#101511=CARTESIAN_POINT('Ctrl Pts',(2.94525079654177,-28.2250084196124,
123.96491427792));
#101512=CARTESIAN_POINT('Ctrl Pts',(2.94910615339289,-28.1890783790417,
124.026528034284));
#101513=CARTESIAN_POINT('Ctrl Pts',(2.952961510244,-28.1563632573787,124.090009551487));
#101514=CARTESIAN_POINT('Ctrl Pts',(2.95681686709512,-28.1270475759708,
124.154987112629));
#101515=CARTESIAN_POINT('Ctrl Pts',(2.96067625956356,-28.0977012082021,
124.220032689413));
#101516=CARTESIAN_POINT('Ctrl Pts',(2.96453565203199,-28.0717615842105,
124.286576992497));
#101517=CARTESIAN_POINT('Ctrl Pts',(2.96839504450043,-28.0493653045228,
124.354227712502));
#101518=CARTESIAN_POINT('Ctrl Pts',(2.97225662210374,-28.02695634437,124.421916735413));
#101519=CARTESIAN_POINT('Ctrl Pts',(2.97611819970705,-28.0080948507384,
124.490712953569));
#101520=CARTESIAN_POINT('Ctrl Pts',(2.97997977731036,-27.9928669379986,
124.560210921099));
#101521=CARTESIAN_POINT('Ctrl Pts',(2.98384811142511,-27.9776123813384,
124.629830487586));
#101522=CARTESIAN_POINT('Ctrl Pts',(2.98771644553985,-27.9660041778276,
124.700153775401));
#101523=CARTESIAN_POINT('Ctrl Pts',(2.9915847796546,-27.9580768337092,124.77076792226));
#101524=CARTESIAN_POINT('Ctrl Pts',(2.99388249882665,-27.9533681374013,
124.812711424099));
#101525=CARTESIAN_POINT('Ctrl Pts',(2.9961802179987,-27.9499571027303,124.854757479904));
#101526=CARTESIAN_POINT('Ctrl Pts',(2.99847793717075,-27.9478422574974,
124.89681975777));
#101527=CARTESIAN_POINT('Ctrl Pts',(3.00034353126794,-27.9461251447924,
124.930971510627));
#101528=CARTESIAN_POINT('Ctrl Pts',(3.00220912536513,-27.945260491498,124.965166482837));
#101529=CARTESIAN_POINT('Ctrl Pts',(3.00407471946232,-27.9452500948921,
124.999375532937));
#101530=CARTESIAN_POINT('Ctrl Pts',(3.00407471949959,-27.9452500948919,
124.999375533621));
#101531=CARTESIAN_POINT('Ctrl Pts',(3.00791348792962,-27.945228702179,125.069766312486));
#101532=CARTESIAN_POINT('Ctrl Pts',(3.01175225635965,-27.9488287016156,
125.140303260411));
#101533=CARTESIAN_POINT('Ctrl Pts',(3.01559102478968,-27.9560689985432,
125.210579257724));
#101534=CARTESIAN_POINT('Ctrl Pts',(3.01950861575716,-27.9634579625721,
125.282298252324));
#101535=CARTESIAN_POINT('Ctrl Pts',(3.02342620672465,-27.9746384824609,
125.35374494479));
#101536=CARTESIAN_POINT('Ctrl Pts',(3.02734379769213,-27.9895745963593,
125.424484698071));
#101537=CARTESIAN_POINT('Ctrl Pts',(3.03117271153808,-28.0041726219789,
125.493623212797));
#101538=CARTESIAN_POINT('Ctrl Pts',(3.03500162538402,-28.0223579037,125.562085943561));
#101539=CARTESIAN_POINT('Ctrl Pts',(3.03883053922997,-28.0440446045493,
125.629472837784));
#101540=CARTESIAN_POINT('Ctrl Pts',(3.04265730106932,-28.0657191165835,
125.696821857809));
#101541=CARTESIAN_POINT('Ctrl Pts',(3.04648406290868,-28.0908909937601,
125.763095771075));
#101542=CARTESIAN_POINT('Ctrl Pts',(3.05031082474803,-28.1194241368866,
125.827908198761));
#101543=CARTESIAN_POINT('Ctrl Pts',(3.0541367656348,-28.1479511588175,125.892706722281));
#101544=CARTESIAN_POINT('Ctrl Pts',(3.05796270652157,-28.1798378159244,
125.956043930675));
#101545=CARTESIAN_POINT('Ctrl Pts',(3.06178864740834,-28.2149000053456,
126.017553719262));
#101546=CARTESIAN_POINT('Ctrl Pts',(3.06577402745842,-28.2514233480649,
126.081626816986));
#101547=CARTESIAN_POINT('Ctrl Pts',(3.0697594075085,-28.2913924556458,126.143716319393));
#101548=CARTESIAN_POINT('Ctrl Pts',(3.07374478755858,-28.334547641787,126.20343924027));
#101549=CARTESIAN_POINT('Ctrl Pts',(3.07757550004214,-28.3760280296557,
126.260844390014));
#101550=CARTESIAN_POINT('Ctrl Pts',(3.08140621252571,-28.4204513813144,
126.316062905982));
#101551=CARTESIAN_POINT('Ctrl Pts',(3.08523692500927,-28.4675457371936,
126.368788330936));
#101552=CARTESIAN_POINT('Ctrl Pts',(3.08907026922185,-28.5146724472584,
126.421549978664));
#101553=CARTESIAN_POINT('Ctrl Pts',(3.09290361343443,-28.5644734622162,
126.471814780227));
#101554=CARTESIAN_POINT('Ctrl Pts',(3.096736957647,-28.616640920405,126.519314062135));
#101555=CARTESIAN_POINT('Ctrl Pts',(3.10057644985369,-28.6688920458064,
126.566889524342));
#101556=CARTESIAN_POINT('Ctrl Pts',(3.10441594206038,-28.7235167986926,
126.611690314675));
#101557=CARTESIAN_POINT('Ctrl Pts',(3.10825543426707,-28.7801762753519,
126.653489535282));
#101558=CARTESIAN_POINT('Ctrl Pts',(3.10870802551448,-28.7868551750185,
126.658416739291));
#101559=CARTESIAN_POINT('Ctrl Pts',(3.10916061676189,-28.7935623181573,
126.663302287644));
#101560=CARTESIAN_POINT('Ctrl Pts',(3.10961320800931,-28.800297126947,126.668145850604));
#101561=CARTESIAN_POINT('Ctrl Pts',(3.11348228135751,-28.8578710843367,
126.709552087396));
#101562=CARTESIAN_POINT('Ctrl Pts',(3.11735135470571,-28.9177039567807,
126.748055289834));
#101563=CARTESIAN_POINT('Ctrl Pts',(3.12122042805391,-28.9794709514144,
126.783400690673));
#101564=CARTESIAN_POINT('Ctrl Pts',(3.12508373644968,-29.041145912697,126.818693426562));
#101565=CARTESIAN_POINT('Ctrl Pts',(3.12894704484544,-29.1047488575628,
126.850837461135));
#101566=CARTESIAN_POINT('Ctrl Pts',(3.13281035324121,-29.1699247609725,
126.879620349979));
#101567=CARTESIAN_POINT('Ctrl Pts',(3.13666912973411,-29.2350242089628,
126.90836947469));
#101568=CARTESIAN_POINT('Ctrl Pts',(3.140527906227,-29.3016925081228,126.93376509018));
#101569=CARTESIAN_POINT('Ctrl Pts',(3.1443866827199,-29.3695502355988,126.955640728014));
#101570=CARTESIAN_POINT('Ctrl Pts',(3.14824302830809,-29.4373652148956,
126.977502584902));
#101571=CARTESIAN_POINT('Ctrl Pts',(3.15209937389628,-29.5063676746451,
126.995848714865));
#101572=CARTESIAN_POINT('Ctrl Pts',(3.15595571948447,-29.5761597972444,
127.010561375593));
#101573=CARTESIAN_POINT('Ctrl Pts',(3.15981092572979,-29.6459313000223,
127.025269689522));
#101574=CARTESIAN_POINT('Ctrl Pts',(3.16366613197511,-29.7164915273992,
127.03634656525));
#101575=CARTESIAN_POINT('Ctrl Pts',(3.16752133822043,-29.7874308248601,
127.043725007989));
#101576=CARTESIAN_POINT('Ctrl Pts',(3.17137669507166,-29.8583728936066,
127.051103738972));
#101577=CARTESIAN_POINT('Ctrl Pts',(3.17523205192289,-29.9296935784304,
127.054783702051));
#101578=CARTESIAN_POINT('Ctrl Pts',(3.17908740877412,-30.0009781593512,
127.054749767175));
#101579=CARTESIAN_POINT('Ctrl Pts',(3.18294680124266,-30.0723373578237,
127.054715796777));
#101580=CARTESIAN_POINT('Ctrl Pts',(3.18680619371121,-30.1436598901705,
127.050960168243));
#101581=CARTESIAN_POINT('Ctrl Pts',(3.19066558617975,-30.2145319980777,
127.043519900637));
#101582=CARTESIAN_POINT('Ctrl Pts',(3.19452716378317,-30.2854442327965,
127.036075420455));
#101583=CARTESIAN_POINT('Ctrl Pts',(3.19838874138659,-30.3559050553407,
127.024942224089));
#101584=CARTESIAN_POINT('Ctrl Pts',(3.20225031899001,-30.4255095200121,
127.010208748085));
#101585=CARTESIAN_POINT('Ctrl Pts',(3.20611865310487,-30.4952357699771,
126.995449493265));
#101586=CARTESIAN_POINT('Ctrl Pts',(3.20998698721973,-30.5641022010522,
126.977077507279));
#101587=CARTESIAN_POINT('Ctrl Pts',(3.21385532133458,-30.6317183549193,
126.955231311778));
#101588=CARTESIAN_POINT('Ctrl Pts',(3.21615304050568,-30.6718811041553,
126.942255074274));
#101589=CARTESIAN_POINT('Ctrl Pts',(3.21845075967678,-30.7116030891758,
126.928054022522));
#101590=CARTESIAN_POINT('Ctrl Pts',(3.22074847884788,-30.7508062394284,
126.912665039503));
#101591=CARTESIAN_POINT('Ctrl Pts',(3.22461723641773,-30.8168140815572,
126.886754020742));
#101592=CARTESIAN_POINT('Ctrl Pts',(3.22848599398759,-30.8816083107962,
126.857371254927));
#101593=CARTESIAN_POINT('Ctrl Pts',(3.23235475155745,-30.9447988250308,
126.824651403069));
#101594=CARTESIAN_POINT('Ctrl Pts',(3.23621738607661,-31.0078893281598,
126.79198333665));
#101595=CARTESIAN_POINT('Ctrl Pts',(3.24008002059578,-31.0693807290199,
126.755988893851));
#101596=CARTESIAN_POINT('Ctrl Pts',(3.24394265511494,-31.1289021815181,
126.716851020637));
#101597=CARTESIAN_POINT('Ctrl Pts',(3.24667286921245,-31.1709735470352,
126.689187317881));
#101598=CARTESIAN_POINT('Ctrl Pts',(3.24940308330995,-31.2120610722941,
126.659954176594));
#101599=CARTESIAN_POINT('Ctrl Pts',(3.25213329740746,-31.2520409112987,
126.629230222815));
#101600=CARTESIAN_POINT('',(2.94592528057306,-27.9452500017688,125.000085258451));
#101601=CARTESIAN_POINT('Ctrl Pts',(2.94592528057306,-27.9452500017688,
125.000085258451));
#101602=CARTESIAN_POINT('Ctrl Pts',(2.94997591063975,-27.9452531186627,
125.075203179717));
#101603=CARTESIAN_POINT('Ctrl Pts',(2.95402654070645,-27.9493797866667,
125.150236380527));
#101604=CARTESIAN_POINT('Ctrl Pts',(2.95807717077314,-27.9575765752318,
125.224731209355));
#101605=CARTESIAN_POINT('Ctrl Pts',(2.96213971866872,-27.9657974805201,
125.299445218067));
#101606=CARTESIAN_POINT('Ctrl Pts',(2.96620226656431,-27.9781123929221,
125.373617281608));
#101607=CARTESIAN_POINT('Ctrl Pts',(2.97026481445989,-27.9944163846029,
125.446801884677));
#101608=CARTESIAN_POINT('Ctrl Pts',(2.97433371205176,-28.0107458591575,
125.52010087409));
#101609=CARTESIAN_POINT('Ctrl Pts',(2.97840260964364,-28.0310767338203,
125.592408932705));
#101610=CARTESIAN_POINT('Ctrl Pts',(2.98247150723551,-28.0552544358625,
125.663296504791));
#101611=CARTESIAN_POINT('Ctrl Pts',(2.9865516038357,-28.0794986832723,125.734379183903));
#101612=CARTESIAN_POINT('Ctrl Pts',(2.99063170043589,-28.1076107674917,
125.804033182399));
#101613=CARTESIAN_POINT('Ctrl Pts',(2.99471179703608,-28.1393881013189,
125.871849141186));
#101614=CARTESIAN_POINT('Ctrl Pts',(2.99669196890442,-28.1548104279601,
125.904761904528));
#101615=CARTESIAN_POINT('Ctrl Pts',(2.99867214077276,-28.1710953858727,
125.937242126137));
#101616=CARTESIAN_POINT('Ctrl Pts',(3.0006523126411,-28.1882160943984,125.969245398185));
#101617=CARTESIAN_POINT('Ctrl Pts',(3.00452138598921,-28.2216683810996,
126.031776842507));
#101618=CARTESIAN_POINT('Ctrl Pts',(3.00839045933732,-28.2584272837346,
126.092696890929));
#101619=CARTESIAN_POINT('Ctrl Pts',(3.01225953268542,-28.2983134165014,
126.151633767324));
#101620=CARTESIAN_POINT('Ctrl Pts',(3.0161228410811,-28.3381401185887,126.210482827268));
#101621=CARTESIAN_POINT('Ctrl Pts',(3.01998614947677,-28.3810845315813,
126.267354181628));
#101622=CARTESIAN_POINT('Ctrl Pts',(3.02384945787244,-28.4269214872576,
126.321900735777));
#101623=CARTESIAN_POINT('Ctrl Pts',(3.02770823436524,-28.4727046733122,
126.3763833034));
#101624=CARTESIAN_POINT('Ctrl Pts',(3.03156701085805,-28.5213733511308,
126.428546117723));
#101625=CARTESIAN_POINT('Ctrl Pts',(3.03542578735085,-28.5726601990986,
126.478072615017));
#101626=CARTESIAN_POINT('Ctrl Pts',(3.03928213293895,-28.6239147380067,
126.527567912215));
#101627=CARTESIAN_POINT('Ctrl Pts',(3.04313847852704,-28.677783826134,126.574429850717));
#101628=CARTESIAN_POINT('Ctrl Pts',(3.04699482411514,-28.7339621666742,
126.618377510684));
#101629=CARTESIAN_POINT('Ctrl Pts',(3.05085003036037,-28.7901239095339,
126.662312186479));
#101630=CARTESIAN_POINT('Ctrl Pts',(3.05470523660559,-28.8485931679217,
126.703333993932));
#101631=CARTESIAN_POINT('Ctrl Pts',(3.05856044285081,-28.9090316670749,
126.741202360168));
#101632=CARTESIAN_POINT('Ctrl Pts',(3.06241579970195,-28.9694725272939,
126.779072205754));
#101633=CARTESIAN_POINT('Ctrl Pts',(3.06627115655309,-29.0318823681856,
126.813788109482));
#101634=CARTESIAN_POINT('Ctrl Pts',(3.07012651340423,-29.0958955242712,
126.845153830841));
#101635=CARTESIAN_POINT('Ctrl Pts',(3.07398590587269,-29.159975686502,126.876552384452));
#101636=CARTESIAN_POINT('Ctrl Pts',(3.07784529834114,-29.2256620770228,
126.9045935411));
#101637=CARTESIAN_POINT('Ctrl Pts',(3.08170469080959,-29.2925669254543,
126.929128302508));
#101638=CARTESIAN_POINT('Ctrl Pts',(3.08556626841292,-29.3595096544898,
126.953676955161));
#101639=CARTESIAN_POINT('Ctrl Pts',(3.08942784601626,-29.4276717503634,
126.974715117171));
#101640=CARTESIAN_POINT('Ctrl Pts',(3.09328942361959,-29.4966507084971,
126.992143833473));
#101641=CARTESIAN_POINT('Ctrl Pts',(3.09715775773436,-29.5657503574902,
127.009603044389));
#101642=CARTESIAN_POINT('Ctrl Pts',(3.10102609184912,-29.6356692455768,
127.023440106453));
#101643=CARTESIAN_POINT('Ctrl Pts',(3.10489442596389,-29.7059958155199,
127.033607410984));
#101644=CARTESIAN_POINT('Ctrl Pts',(3.10719214513581,-29.7477685019683,
127.039646602495));
#101645=CARTESIAN_POINT('Ctrl Pts',(3.10948986430774,-29.7896849274545,
127.044392046685));
#101646=CARTESIAN_POINT('Ctrl Pts',(3.11178758347966,-29.83165875689,127.047842471571));
#101647=CARTESIAN_POINT('Ctrl Pts',(3.11565566452762,-29.9023193389722,
127.053651067882));
#101648=CARTESIAN_POINT('Ctrl Pts',(3.11952374557558,-29.9734192810663,
127.05580954406));
#101649=CARTESIAN_POINT('Ctrl Pts',(3.12339182662354,-30.0445492616679,
127.054267004502));
#101650=CARTESIAN_POINT('Ctrl Pts',(3.12725460116862,-30.1155816612101,
127.052726581106));
#101651=CARTESIAN_POINT('Ctrl Pts',(3.1311173757137,-30.186643536325,127.04749522442));
#101652=CARTESIAN_POINT('Ctrl Pts',(3.13498015025878,-30.2573213267348,
127.038573839062));
#101653=CARTESIAN_POINT('Ctrl Pts',(3.13883891823638,-30.3279258083522,
127.029661707191));
#101654=CARTESIAN_POINT('Ctrl Pts',(3.14269768621397,-30.3981465164401,
127.017067202742));
#101655=CARTESIAN_POINT('Ctrl Pts',(3.14655645419157,-30.4675725071244,
127.000843200524));
#101656=CARTESIAN_POINT('Ctrl Pts',(3.15049840094071,-30.5384950295132,
126.984269477207));
#101657=CARTESIAN_POINT('Ctrl Pts',(3.15444034768985,-30.6085876520776,
126.963907977244));
#101658=CARTESIAN_POINT('Ctrl Pts',(3.15838229443899,-30.6774215865192,
126.939870499961));
#101659=CARTESIAN_POINT('Ctrl Pts',(3.16223769286971,-30.7447442216828,
126.916360783038));
#101660=CARTESIAN_POINT('Ctrl Pts',(3.16609309130044,-30.8108624124218,
126.889335069568));
#101661=CARTESIAN_POINT('Ctrl Pts',(3.16994848973117,-30.875390936098,126.858948162671));
#101662=CARTESIAN_POINT('Ctrl Pts',(3.17393371063952,-30.9420923228315,
126.827538040246));
#101663=CARTESIAN_POINT('Ctrl Pts',(3.17791893154787,-31.0070945536863,
126.792536503335));
#101664=CARTESIAN_POINT('Ctrl Pts',(3.18190415245621,-31.0699975976019,
126.754167239355));
#101665=CARTESIAN_POINT('Ctrl Pts',(3.18588937336456,-31.1329006415176,
126.715797975375));
#101666=CARTESIAN_POINT('Ctrl Pts',(3.18987459427291,-31.1937040283989,
126.674061311145));
#101667=CARTESIAN_POINT('Ctrl Pts',(3.19385981518126,-31.2520409112986,
126.629230222815));
#101668=CARTESIAN_POINT('Ctrl Pts',(2.49394332640294,-31.2520409112987,
126.629230222815));
#101669=CARTESIAN_POINT('Ctrl Pts',(2.49779845369501,-31.3085851548333,
126.585776753065));
#101670=CARTESIAN_POINT('Ctrl Pts',(2.50165358098708,-31.3628774190682,
126.539366342141));
#101671=CARTESIAN_POINT('Ctrl Pts',(2.50550870827915,-31.4146017651328,
126.49026823377));
#101672=CARTESIAN_POINT('Ctrl Pts',(2.50936427882671,-31.4663320583681,
126.441164480188));
#101673=CARTESIAN_POINT('Ctrl Pts',(2.51321984937427,-31.5154934967334,
126.389372751944));
#101674=CARTESIAN_POINT('Ctrl Pts',(2.51707541992182,-31.5618064874044,
126.335199632415));
#101675=CARTESIAN_POINT('Ctrl Pts',(2.52093520627497,-31.6081701181979,
126.280967278245));
#101676=CARTESIAN_POINT('Ctrl Pts',(2.52479499262811,-31.6516787706278,
126.224348707153));
#101677=CARTESIAN_POINT('Ctrl Pts',(2.52865477898125,-31.6920933198749,
126.16568338726));
#101678=CARTESIAN_POINT('Ctrl Pts',(2.53251701344132,-31.7325335024418,
126.10698085832));
#101679=CARTESIAN_POINT('Ctrl Pts',(2.53637924790139,-31.7698754225889,
126.046229411115));
#101680=CARTESIAN_POINT('Ctrl Pts',(2.54024148236146,-31.8039249057506,
125.983794946578));
#101681=CARTESIAN_POINT('Ctrl Pts',(2.54411021068045,-31.8380316388132,
125.921255506383));
#101682=CARTESIAN_POINT('Ctrl Pts',(2.54797893899944,-31.868834679516,125.857027839922));
#101683=CARTESIAN_POINT('Ctrl Pts',(2.55184766731844,-31.8961874947129,
125.791498924443));
#101684=CARTESIAN_POINT('Ctrl Pts',(2.55326885464125,-31.9062356218998,
125.767426708387));
#101685=CARTESIAN_POINT('Ctrl Pts',(2.55469004196406,-31.9158186332063,
125.743179043823));
#101686=CARTESIAN_POINT('Ctrl Pts',(2.55611122928687,-31.9249309694032,
125.718775573829));
#101687=CARTESIAN_POINT('Ctrl Pts',(2.55998030264048,-31.9497386049644,
125.652339000706));
#101688=CARTESIAN_POINT('Ctrl Pts',(2.56384937599409,-31.9711513321785,
125.584486481582));
#101689=CARTESIAN_POINT('Ctrl Pts',(2.5677184493477,-31.989008767343,125.515598376581));
#101690=CARTESIAN_POINT('Ctrl Pts',(2.57158175774896,-32.0068395947765,
125.446812915445));
#101691=CARTESIAN_POINT('Ctrl Pts',(2.57544506615022,-32.0211255244763,
125.376995397718));
#101692=CARTESIAN_POINT('Ctrl Pts',(2.57930837455148,-32.0317549564161,
125.306544221245));
#101693=CARTESIAN_POINT('Ctrl Pts',(2.58316715104994,-32.0423719193663,
125.236175688416));
#101694=CARTESIAN_POINT('Ctrl Pts',(2.58702592754841,-32.0493408324374,
125.165175451347));
#101695=CARTESIAN_POINT('Ctrl Pts',(2.59088470404687,-32.0526008694865,
125.09395335589));
#101696=CARTESIAN_POINT('Ctrl Pts',(2.59474104964069,-32.0558588528176,
125.022776128055));
#101697=CARTESIAN_POINT('Ctrl Pts',(2.5985973952345,-32.0554125734897,124.951377803252));
#101698=CARTESIAN_POINT('Ctrl Pts',(2.60245374082832,-32.0512530538663,
124.880173160335));
#101699=CARTESIAN_POINT('Ctrl Pts',(2.6063089470793,-32.0470947631574,124.808989554564));
#101700=CARTESIAN_POINT('Ctrl Pts',(2.61016415333028,-32.0392254384407,
124.738000001772));
#101701=CARTESIAN_POINT('Ctrl Pts',(2.61401935958127,-32.0276881762123,
124.667617355223));
#101702=CARTESIAN_POINT('Ctrl Pts',(2.61787471643819,-32.0161504632737,
124.597231959133));
#101703=CARTESIAN_POINT('Ctrl Pts',(2.62173007329512,-32.0009446090955,
124.527453995389));
#101704=CARTESIAN_POINT('Ctrl Pts',(2.62558543015205,-31.9821650814073,
124.458687564756));
#101705=CARTESIAN_POINT('Ctrl Pts',(2.6294448226263,-31.9633658961389,124.389849152461));
#101706=CARTESIAN_POINT('Ctrl Pts',(2.63330421510055,-31.9409856981956,
124.322024856521));
#101707=CARTESIAN_POINT('Ctrl Pts',(2.6371636075748,-31.915169015866,124.255604135445));
#101708=CARTESIAN_POINT('Ctrl Pts',(2.64102518518395,-31.8893377164863,
124.18914580787));
#101709=CARTESIAN_POINT('Ctrl Pts',(2.64488676279309,-31.8600662588824,
124.124093080346));
#101710=CARTESIAN_POINT('Ctrl Pts',(2.64874834040224,-31.8275464613336,
124.060813386931));
#101711=CARTESIAN_POINT('Ctrl Pts',(2.65261667452278,-31.7949697646609,
123.997422974528));
#101712=CARTESIAN_POINT('Ctrl Pts',(2.65648500864332,-31.7591336250078,
123.935812209992));
#101713=CARTESIAN_POINT('Ctrl Pts',(2.66035334276386,-31.720274372791,123.876321378321));
#101714=CARTESIAN_POINT('Ctrl Pts',(2.66265106188438,-31.6971926936896,
123.84098492155));
#101715=CARTESIAN_POINT('Ctrl Pts',(2.6649487810049,-31.6730452284487,123.806395821985));
#101716=CARTESIAN_POINT('Ctrl Pts',(2.66724650012542,-31.6478880931576,
123.772619702403));
#101717=CARTESIAN_POINT('Ctrl Pts',(2.67111557347318,-31.605526604849,123.715744916056));
#101718=CARTESIAN_POINT('Ctrl Pts',(2.67498464682093,-31.5601342422752,
123.66095438182));
#101719=CARTESIAN_POINT('Ctrl Pts',(2.67885372016868,-31.5119435761822,
123.608589138701));
#101720=CARTESIAN_POINT('Ctrl Pts',(2.68271702856402,-31.4638247145944,
123.556301920242));
#101721=CARTESIAN_POINT('Ctrl Pts',(2.68658033695935,-31.4129161520987,
123.50643317434));
#101722=CARTESIAN_POINT('Ctrl Pts',(2.69044364535468,-31.3594920722307,
123.45929273772));
#101723=CARTESIAN_POINT('Ctrl Pts',(2.69430242184715,-31.3061306621565,
123.412207599787));
#101724=CARTESIAN_POINT('Ctrl Pts',(2.69816119833963,-31.2502599586026,
123.367844733758));
#101725=CARTESIAN_POINT('Ctrl Pts',(2.7020199748321,-31.192191301005,123.326477527994));
#101726=CARTESIAN_POINT('Ctrl Pts',(2.70587632041987,-31.1341592247884,
123.285136382236));
#101727=CARTESIAN_POINT('Ctrl Pts',(2.70973266600764,-31.0739323363522,
123.246787433824));
#101728=CARTESIAN_POINT('Ctrl Pts',(2.71358901159541,-31.0118542403315,
123.211663186415));
#101729=CARTESIAN_POINT('Ctrl Pts',(2.71744421784031,-30.9497944850519,
123.176549316334));
#101730=CARTESIAN_POINT('Ctrl Pts',(2.72129942408521,-30.8858850305699,
123.144658494925));
#101731=CARTESIAN_POINT('Ctrl Pts',(2.72515463033012,-30.8204961068849,
123.116178431728));
#101732=CARTESIAN_POINT('Ctrl Pts',(2.72900998718095,-30.7551046287427,
123.08769725594));
#101733=CARTESIAN_POINT('Ctrl Pts',(2.73286534403177,-30.6882340129049,
123.062627294863));
#101734=CARTESIAN_POINT('Ctrl Pts',(2.7367207008826,-30.6202749979301,123.041108351786));
#101735=CARTESIAN_POINT('Ctrl Pts',(2.74058009335076,-30.5522448464589,
123.019566883629));
#101736=CARTESIAN_POINT('Ctrl Pts',(2.74443948581892,-30.4831244856478,
123.001584000482));
#101737=CARTESIAN_POINT('Ctrl Pts',(2.74829887828708,-30.4133195035039,
122.987249506143));
#101738=CARTESIAN_POINT('Ctrl Pts',(2.75216045589012,-30.3434749987401,
122.972906895809));
#101739=CARTESIAN_POINT('Ctrl Pts',(2.75602203349316,-30.2729455815335,
122.962216859222));
#101740=CARTESIAN_POINT('Ctrl Pts',(2.7598836110962,-30.2021439845883,122.955217524529));
#101741=CARTESIAN_POINT('Ctrl Pts',(2.7637519452107,-30.1312185077551,122.948205943264));
#101742=CARTESIAN_POINT('Ctrl Pts',(2.7676202793252,-30.0600203857999,122.9448979791));
#101743=CARTESIAN_POINT('Ctrl Pts',(2.7714886134397,-29.9889636841022,122.945279638921));
#101744=CARTESIAN_POINT('Ctrl Pts',(2.77378633261446,-29.9467573127925,
122.945506337822));
#101745=CARTESIAN_POINT('Ctrl Pts',(2.77608405178923,-29.9046007847015,
122.947033789851));
#101746=CARTESIAN_POINT('Ctrl Pts',(2.77838177096399,-29.8625796677408,
122.949850440875));
#101747=CARTESIAN_POINT('Ctrl Pts',(2.78225084431114,-29.7918213325031,
122.954593330921));
#101748=CARTESIAN_POINT('Ctrl Pts',(2.78611991765829,-29.7211702309011,
122.963013013947));
#101749=CARTESIAN_POINT('Ctrl Pts',(2.78998899100544,-29.6510390226777,
122.975099064446));
#101750=CARTESIAN_POINT('Ctrl Pts',(2.79385229940014,-29.5810123105554,
122.987167106626));
#101751=CARTESIAN_POINT('Ctrl Pts',(2.79771560779484,-29.5115044289906,
123.002890590709));
#101752=CARTESIAN_POINT('Ctrl Pts',(2.80157891618955,-29.4429243926149,
123.022207207477));
#101753=CARTESIAN_POINT('Ctrl Pts',(2.80543769268135,-29.3744248049205,
123.041501164642));
#101754=CARTESIAN_POINT('Ctrl Pts',(2.80929646917315,-29.3068513657659,
123.064379751071));
#101755=CARTESIAN_POINT('Ctrl Pts',(2.81315524566495,-29.2406026199514,
123.09072967297));
#101756=CARTESIAN_POINT('Ctrl Pts',(2.81701159125203,-29.1743956087099,
123.11706299527));
#101757=CARTESIAN_POINT('Ctrl Pts',(2.82086793683911,-29.1095120854706,
123.146863135293));
#101758=CARTESIAN_POINT('Ctrl Pts',(2.82472428242619,-29.0463337454979,
123.179967517454));
#101759=CARTESIAN_POINT('Ctrl Pts',(2.82857948867037,-28.9831740713298,
123.213062119048));
#101760=CARTESIAN_POINT('Ctrl Pts',(2.83243469491455,-28.9217190103251,
123.249458799358));
#101761=CARTESIAN_POINT('Ctrl Pts',(2.83628990115873,-28.8623270648984,
123.288948318946));
#101762=CARTESIAN_POINT('Ctrl Pts',(2.84014525800883,-28.8029327992902,
123.328439381216));
#101763=CARTESIAN_POINT('Ctrl Pts',(2.84400061485893,-28.7456022125833,
123.371023251839));
#101764=CARTESIAN_POINT('Ctrl Pts',(2.84785597170903,-28.6906646821707,
123.416447478615));
#101765=CARTESIAN_POINT('Ctrl Pts',(2.85171536417643,-28.6356696455774,
123.461919253466));
#101766=CARTESIAN_POINT('Ctrl Pts',(2.85557475664382,-28.5830730408649,
123.510237009375));
#101767=CARTESIAN_POINT('Ctrl Pts',(2.85943414911121,-28.5331702924828,
123.561108700546));
#101768=CARTESIAN_POINT('Ctrl Pts',(2.86329572671347,-28.4832392898516,
123.612009194567));
#101769=CARTESIAN_POINT('Ctrl Pts',(2.86715730431574,-28.4360055016132,
123.665466138185));
#101770=CARTESIAN_POINT('Ctrl Pts',(2.871018881918,-28.3917248122804,123.721153456014));
#101771=CARTESIAN_POINT('Ctrl Pts',(2.8748872160317,-28.3473666460677,123.776938208632));
#101772=CARTESIAN_POINT('Ctrl Pts',(2.87875555014539,-28.3059721769819,
123.834960731194));
#101773=CARTESIAN_POINT('Ctrl Pts',(2.88262388425909,-28.2677542229881,
123.894865559977));
#101774=CARTESIAN_POINT('Ctrl Pts',(2.88492160344024,-28.2450534625639,
123.930447924399));
#101775=CARTESIAN_POINT('Ctrl Pts',(2.88721932262139,-28.2234725546798,
123.966693895146));
#101776=CARTESIAN_POINT('Ctrl Pts',(2.88951704180254,-28.2030482011671,
124.003525316342));
#101777=CARTESIAN_POINT('Ctrl Pts',(2.89357123056495,-28.1670106448069,
124.068512167277));
#101778=CARTESIAN_POINT('Ctrl Pts',(2.89762541932736,-28.1344462576574,
124.135557009902));
#101779=CARTESIAN_POINT('Ctrl Pts',(2.90167960808977,-28.1055831555926,
124.204272419653));
#101780=CARTESIAN_POINT('Ctrl Pts',(2.90572241802439,-28.0768010631422,
124.272794966944));
#101781=CARTESIAN_POINT('Ctrl Pts',(2.909765227959,-28.0516997313792,124.342978361097));
#101782=CARTESIAN_POINT('Ctrl Pts',(2.91380803789362,-28.0304609874017,
124.414411714297));
#101783=CARTESIAN_POINT('Ctrl Pts',(2.91784402707238,-28.0092580759984,
124.485724549968));
#101784=CARTESIAN_POINT('Ctrl Pts',(2.92188001625114,-27.9919049147105,
124.558282753116));
#101785=CARTESIAN_POINT('Ctrl Pts',(2.9259160054299,-27.9785350595386,124.631656333046));
#101786=CARTESIAN_POINT('Ctrl Pts',(2.92994364805372,-27.9651928536556,
124.704878174062));
#101787=CARTESIAN_POINT('Ctrl Pts',(2.93397129067754,-27.9558176275984,
124.778911624366));
#101788=CARTESIAN_POINT('Ctrl Pts',(2.93799893330136,-27.9504925475499,
124.853314060484));
#101789=CARTESIAN_POINT('Ctrl Pts',(2.9406410490468,-27.946999318593,124.902121729467));
#101790=CARTESIAN_POINT('Ctrl Pts',(2.94328316479224,-27.9452479687194,
124.951087882257));
#101791=CARTESIAN_POINT('Ctrl Pts',(2.94592528053768,-27.9452500017688,
125.000085257795));
#101792=CARTESIAN_POINT('Origin',(-1.54592528053767,-30.,125.));
#101793=CARTESIAN_POINT('',(1.79398326297881,-31.2520409112987,126.629230222815));
#101794=CARTESIAN_POINT('',(1.85201788380192,-31.2520409112987,126.629230222815));
#101795=CARTESIAN_POINT('',(-1.54592528053767,-31.2520409112987,126.629230222815));
#101796=CARTESIAN_POINT('',(2.30407471949582,-27.9452508576209,125.001877336539));
#101797=CARTESIAN_POINT('Ctrl Pts',(1.85201788380192,-31.2520409112987,
126.629230222815));
#101798=CARTESIAN_POINT('Ctrl Pts',(1.85587837089731,-31.3086000947725,
126.585765271928));
#101799=CARTESIAN_POINT('Ctrl Pts',(1.85973885799271,-31.3628526586814,
126.539382921901));
#101800=CARTESIAN_POINT('Ctrl Pts',(1.86359934508811,-31.4144967675365,
126.490367893216));
#101801=CARTESIAN_POINT('Ctrl Pts',(1.86752032570428,-31.4669501354034,
126.440584802992));
#101802=CARTESIAN_POINT('Ctrl Pts',(1.87144130632046,-31.5167122299897,
126.388086186834));
#101803=CARTESIAN_POINT('Ctrl Pts',(1.87536228693663,-31.5635084223667,
126.333206276496));
#101804=CARTESIAN_POINT('Ctrl Pts',(1.87928326755281,-31.6103046147436,
126.278326366158));
#101805=CARTESIAN_POINT('Ctrl Pts',(1.88320424816899,-31.6541346429375,
126.221065613155));
#101806=CARTESIAN_POINT('Ctrl Pts',(1.88712522878516,-31.694770243634,126.161788011555));
#101807=CARTESIAN_POINT('Ctrl Pts',(1.8909943020432,-31.734867895566,126.103295148263));
#101808=CARTESIAN_POINT('Ctrl Pts',(1.89486337530124,-31.7720123219207,
126.042609395793));
#101809=CARTESIAN_POINT('Ctrl Pts',(1.89873244855929,-31.8059561429648,
125.980061208388));
#101810=CARTESIAN_POINT('Ctrl Pts',(1.90259575686323,-31.8398493874089,
125.917606218348));
#101811=CARTESIAN_POINT('Ctrl Pts',(1.90645906516718,-31.8705512629169,
125.853294725246));
#101812=CARTESIAN_POINT('Ctrl Pts',(1.91032237347112,-31.89785738344,125.787486453612));
#101813=CARTESIAN_POINT('Ctrl Pts',(1.91418114987016,-31.9251314721572,
125.721755379241));
#101814=CARTESIAN_POINT('Ctrl Pts',(1.9180399262692,-31.9490175330646,125.654531460497));
#101815=CARTESIAN_POINT('Ctrl Pts',(1.92189870266824,-31.9693576944775,
125.586197776951));
#101816=CARTESIAN_POINT('Ctrl Pts',(1.92575504816137,-31.9896850422383,
125.517907141443));
#101817=CARTESIAN_POINT('Ctrl Pts',(1.9296113936545,-32.0064707840726,125.448508592667));
#101818=CARTESIAN_POINT('Ctrl Pts',(1.93346773914762,-32.0196061767615,
125.378402501692));
#101819=CARTESIAN_POINT('Ctrl Pts',(1.93732294529681,-32.0327376886441,
125.308317123319));
#101820=CARTESIAN_POINT('Ctrl Pts',(1.941178151446,-32.0422209030551,125.237525094969));
#101821=CARTESIAN_POINT('Ctrl Pts',(1.94503335759519,-32.0479980782691,
125.166437477468));
#101822=CARTESIAN_POINT('Ctrl Pts',(1.94888871434936,-32.0537754791705,
125.095347082905));
#101823=CARTESIAN_POINT('Ctrl Pts',(1.95274407110353,-32.0558465162838,
125.023961560633));
#101824=CARTESIAN_POINT('Ctrl Pts',(1.9565994278577,-32.0542054136421,124.952695866318));
#101825=CARTESIAN_POINT('Ctrl Pts',(1.96045882022845,-32.052562593167,124.881355574233));
#101826=CARTESIAN_POINT('Ctrl Pts',(1.96431821259919,-32.0471998874065,
124.810135847147));
#101827=CARTESIAN_POINT('Ctrl Pts',(1.96817760496994,-32.0381636345743,
124.739449503553));
#101828=CARTESIAN_POINT('Ctrl Pts',(1.97203918247499,-32.0291222655413,
124.668723138333));
#101829=CARTESIAN_POINT('Ctrl Pts',(1.97590075998004,-32.0164032956312,
124.598531236013));
#101830=CARTESIAN_POINT('Ctrl Pts',(1.97976233748509,-32.0001042687789,
124.529276645457));
#101831=CARTESIAN_POINT('Ctrl Pts',(1.98363067150175,-31.9837767239016,
124.459900881767));
#101832=CARTESIAN_POINT('Ctrl Pts',(1.9874990055184,-31.9638567517517,124.39146617071));
#101833=CARTESIAN_POINT('Ctrl Pts',(1.99136733953506,-31.9404916420071,
124.324359748238));
#101834=CARTESIAN_POINT('Ctrl Pts',(1.99366505956461,-31.9266131918988,
124.284499754153));
#101835=CARTESIAN_POINT('Ctrl Pts',(1.99596277959417,-31.9115201753994,
124.24510802716));
#101836=CARTESIAN_POINT('Ctrl Pts',(1.99826049962372,-31.8952512263342,
124.206261786495));
#101837=CARTESIAN_POINT('Ctrl Pts',(2.00212957301351,-31.8678563491958,
124.140849571726));
#101838=CARTESIAN_POINT('Ctrl Pts',(2.00599864640329,-31.8370174066266,
124.076729146268));
#101839=CARTESIAN_POINT('Ctrl Pts',(2.00986771979308,-31.8028778577843,
124.014287571139));
#101840=CARTESIAN_POINT('Ctrl Pts',(2.01373102823097,-31.7687891771568,
123.951939034482));
#101841=CARTESIAN_POINT('Ctrl Pts',(2.01759433666887,-31.7314098833556,
123.891264805509));
#101842=CARTESIAN_POINT('Ctrl Pts',(2.02145764510676,-31.6909313450081,
123.832631699519));
#101843=CARTESIAN_POINT('Ctrl Pts',(2.02531642164239,-31.6505002905162,
123.774067373826));
#101844=CARTESIAN_POINT('Ctrl Pts',(2.02917519817801,-31.6069774876751,
123.717539812929));
#101845=CARTESIAN_POINT('Ctrl Pts',(2.03303397471363,-31.5605991544203,
123.663389420316));
#101846=CARTESIAN_POINT('Ctrl Pts',(2.0368903203449,-31.5142500380146,123.609273140698));
#101847=CARTESIAN_POINT('Ctrl Pts',(2.04074666597617,-31.4650492754231,
123.557531426356));
#101848=CARTESIAN_POINT('Ctrl Pts',(2.04460301160743,-31.4132742574366,
123.508472784101));
#101849=CARTESIAN_POINT('Ctrl Pts',(2.04845821789611,-31.3615145361815,
123.459428636035));
#101850=CARTESIAN_POINT('Ctrl Pts',(2.05231342418478,-31.3071824218778,
123.413066320264));
#101851=CARTESIAN_POINT('Ctrl Pts',(2.05616863047345,-31.2505919476215,
123.369657292762));
#101852=CARTESIAN_POINT('Ctrl Pts',(2.06002398736825,-31.1939992626219,
123.326246569458));
#101853=CARTESIAN_POINT('Ctrl Pts',(2.06387934426304,-31.1351484292998,
123.285789657396));
#101854=CARTESIAN_POINT('Ctrl Pts',(2.06773470115783,-31.074384937336,123.248516466271));
#101855=CARTESIAN_POINT('Ctrl Pts',(2.07159409366998,-31.0135578408318,
123.211204259214));
#101856=CARTESIAN_POINT('Ctrl Pts',(2.07545348618213,-30.9508145040071,
123.177082680198));
#101857=CARTESIAN_POINT('Ctrl Pts',(2.07931287869428,-30.8865268858702,
123.146336696396));
#101858=CARTESIAN_POINT('Ctrl Pts',(2.08317445634139,-30.8222028689681,
123.115573304641));
#101859=CARTESIAN_POINT('Ctrl Pts',(2.0870360339885,-30.7563332789708,123.088189499311));
#101860=CARTESIAN_POINT('Ctrl Pts',(2.09089761163561,-30.6893094711095,
123.064321820256));
#101861=CARTESIAN_POINT('Ctrl Pts',(2.09476594579382,-30.6221683932764,
123.040412380487));
#101862=CARTESIAN_POINT('Ctrl Pts',(2.09863427995202,-30.5538695312235,
123.020031488757));
#101863=CARTESIAN_POINT('Ctrl Pts',(2.10250261411023,-30.4848181033976,
123.003265423468));
#101864=CARTESIAN_POINT('Ctrl Pts',(2.10480033289425,-30.4438028352512,
122.993306691473));
#101865=CARTESIAN_POINT('Ctrl Pts',(2.10709805167827,-30.4025222418141,
122.984622339477));
#101866=CARTESIAN_POINT('Ctrl Pts',(2.10939577046228,-30.3610621517842,
122.977221790445));
#101867=CARTESIAN_POINT('Ctrl Pts',(2.11326484381022,-30.2912485042424,
122.964760184083));
#101868=CARTESIAN_POINT('Ctrl Pts',(2.11713391715816,-30.2206522077615,
122.955892707146));
#101869=CARTESIAN_POINT('Ctrl Pts',(2.1210029905061,-30.1496762562476,122.950708761348));
#101870=CARTESIAN_POINT('Ctrl Pts',(2.12486629890172,-30.0788060595074,
122.945532539673));
#101871=CARTESIAN_POINT('Ctrl Pts',(2.12872960729734,-30.0075578111597,
122.944028989731));
#101872=CARTESIAN_POINT('Ctrl Pts',(2.13259291569296,-29.9363434801761,
122.946236281851));
#101873=CARTESIAN_POINT('Ctrl Pts',(2.13645169218589,-29.8652126880627,
122.94844098468));
#101874=CARTESIAN_POINT('Ctrl Pts',(2.14031046867881,-29.7941162174787,
122.954347867964));
#101875=CARTESIAN_POINT('Ctrl Pts',(2.14416924517174,-29.7234681723392,
122.963943097359));
#101876=CARTESIAN_POINT('Ctrl Pts',(2.14802559076006,-29.6528646331871,
122.97353228207));
#101877=CARTESIAN_POINT('Ctrl Pts',(2.15188193634839,-29.5827094392452,
122.986805137805));
#101878=CARTESIAN_POINT('Ctrl Pts',(2.15573828193672,-29.5134122273188,
123.003695939498));
#101879=CARTESIAN_POINT('Ctrl Pts',(2.15959348818228,-29.4441354889923,
123.020581750867));
#101880=CARTESIAN_POINT('Ctrl Pts',(2.16344869442785,-29.3757167011493,
123.041083271138));
#101881=CARTESIAN_POINT('Ctrl Pts',(2.16730390067341,-29.3085542460418,
123.065083895402));
#101882=CARTESIAN_POINT('Ctrl Pts',(2.17115925752499,-29.2413891671916,
123.089085457265));
#101883=CARTESIAN_POINT('Ctrl Pts',(2.17501461437657,-29.1754809752312,
123.116586228966));
#101884=CARTESIAN_POINT('Ctrl Pts',(2.17886997122815,-29.1112102084979,
123.147420644339));
#101885=CARTESIAN_POINT('Ctrl Pts',(2.18272936369721,-29.0468721659611,
123.178287335818));
#101886=CARTESIAN_POINT('Ctrl Pts',(2.18658875616628,-28.9841754090357,
123.21249442626));
#101887=CARTESIAN_POINT('Ctrl Pts',(2.19044814863534,-28.9234770739043,
123.249829736257));
#101888=CARTESIAN_POINT('Ctrl Pts',(2.19430972623937,-28.8627443722099,
123.287186184994));
#101889=CARTESIAN_POINT('Ctrl Pts',(2.1981713038434,-28.8040127448828,123.327674103258));
#101890=CARTESIAN_POINT('Ctrl Pts',(2.20203288144743,-28.7476091620136,
123.37103875079));
#101891=CARTESIAN_POINT('Ctrl Pts',(2.20590121556304,-28.691106891121,123.414479272427));
#101892=CARTESIAN_POINT('Ctrl Pts',(2.20976954967865,-28.6369411664899,
123.460806256701));
#101893=CARTESIAN_POINT('Ctrl Pts',(2.21363788379427,-28.5854042502891,
123.509726056257));
#101894=CARTESIAN_POINT('Ctrl Pts',(2.21593560296312,-28.5547922719235,
123.53878351557));
#101895=CARTESIAN_POINT('Ctrl Pts',(2.21823332213197,-28.5251070531022,
123.568755064472));
#101896=CARTESIAN_POINT('Ctrl Pts',(2.22053104130083,-28.4964030609004,
123.599573705178));
#101897=CARTESIAN_POINT('Ctrl Pts',(2.22435385578605,-28.4486469910289,
123.650848006972));
#101898=CARTESIAN_POINT('Ctrl Pts',(2.22817667027127,-28.4034122612403,
123.704680314488));
#101899=CARTESIAN_POINT('Ctrl Pts',(2.23199948475649,-28.3609895950765,
123.760789584028));
#101900=CARTESIAN_POINT('Ctrl Pts',(2.23581710151335,-28.3186246093197,
123.816822564033));
#101901=CARTESIAN_POINT('Ctrl Pts',(2.23963471827021,-28.2790644064682,
123.875125976651));
#101902=CARTESIAN_POINT('Ctrl Pts',(2.24345233502707,-28.2425620670407,
123.935382944766));
#101903=CARTESIAN_POINT('Ctrl Pts',(2.2472661112283,-28.2060964492838,123.995579293847));
#101904=CARTESIAN_POINT('Ctrl Pts',(2.25107988742953,-28.1726828518535,
124.057724877737));
#101905=CARTESIAN_POINT('Ctrl Pts',(2.25489366363075,-28.1425321731206,
124.12147234841));
#101906=CARTESIAN_POINT('Ctrl Pts',(2.25870495117383,-28.112401169043,124.185178221031));
#101907=CARTESIAN_POINT('Ctrl Pts',(2.26251623871691,-28.0855290712528,
124.250483456995));
#101908=CARTESIAN_POINT('Ctrl Pts',(2.26632752625999,-28.0620808415638,
124.317016180378));
#101909=CARTESIAN_POINT('Ctrl Pts',(2.27013878558059,-28.0386327855083,
124.383548411087));
#101910=CARTESIAN_POINT('Ctrl Pts',(2.2739500449012,-28.0186087267518,124.451307646267));
#101911=CARTESIAN_POINT('Ctrl Pts',(2.27776130422181,-28.00212488962,124.519903545291));
#101912=CARTESIAN_POINT('Ctrl Pts',(2.28157259449292,-27.9856409186262,
124.588500001369));
#101913=CARTESIAN_POINT('Ctrl Pts',(2.28538388476404,-27.9726973326024,
124.657932647788));
#101914=CARTESIAN_POINT('Ctrl Pts',(2.28919517503516,-27.9633594769412,
124.727799812023));
#101915=CARTESIAN_POINT('Ctrl Pts',(2.29300941452562,-27.9540143955421,
124.797721040257));
#101916=CARTESIAN_POINT('Ctrl Pts',(2.29682365401607,-27.9482806627008,
124.868076961452));
#101917=CARTESIAN_POINT('Ctrl Pts',(2.30063789350653,-27.9461717409522,
124.938461029936));
#101918=CARTESIAN_POINT('Ctrl Pts',(2.30178350215846,-27.9455383252981,
124.959600918508));
#101919=CARTESIAN_POINT('Ctrl Pts',(2.3029291108104,-27.9452315484039,124.980743347371));
#101920=CARTESIAN_POINT('Ctrl Pts',(2.30407471946233,-27.9452508576204,
125.001877335921));
#101921=CARTESIAN_POINT('Ctrl Pts',(2.30407471949582,-27.9452508576209,
125.001877336539));
#101922=CARTESIAN_POINT('Ctrl Pts',(2.30909836680706,-27.9453355311479,
125.094552705721));
#101923=CARTESIAN_POINT('Ctrl Pts',(2.31412201411831,-27.9516938665571,
125.18694888772));
#101924=CARTESIAN_POINT('Ctrl Pts',(2.31914566142955,-27.9641908651484,
125.278350011594));
#101925=CARTESIAN_POINT('Ctrl Pts',(2.32331921166617,-27.9745731328905,
125.354284319586));
#101926=CARTESIAN_POINT('Ctrl Pts',(2.32749276190278,-27.989191374217,125.429532498929));
#101927=CARTESIAN_POINT('Ctrl Pts',(2.33166631213939,-28.0079438906425,
125.503696356619));
#101928=CARTESIAN_POINT('Ctrl Pts',(2.33553538549303,-28.0253283373371,
125.572449669584));
#101929=CARTESIAN_POINT('Ctrl Pts',(2.33940445884667,-28.0463104154053,
125.640436592137));
#101930=CARTESIAN_POINT('Ctrl Pts',(2.3432735322003,-28.0708056935786,125.707253059782));
#101931=CARTESIAN_POINT('Ctrl Pts',(2.34713684060158,-28.095264473578,125.77396997032));
#101932=CARTESIAN_POINT('Ctrl Pts',(2.35100014900287,-28.1232258971066,
125.839519435331));
#101933=CARTESIAN_POINT('Ctrl Pts',(2.35486345740415,-28.1545551494563,
125.903510302156));
#101934=CARTESIAN_POINT('Ctrl Pts',(2.35872223390264,-28.1858476506304,
125.967426103685));
#101935=CARTESIAN_POINT('Ctrl Pts',(2.36258101040114,-28.2204999206784,
126.029786504532));
#101936=CARTESIAN_POINT('Ctrl Pts',(2.36643978689963,-28.2583288726902,
126.090219815815));
#101937=CARTESIAN_POINT('Ctrl Pts',(2.37029613249347,-28.2961339936832,
126.150615056062));
#101938=CARTESIAN_POINT('Ctrl Pts',(2.37415247808731,-28.3371115691361,
126.209085204514));
#101939=CARTESIAN_POINT('Ctrl Pts',(2.37800882368115,-28.381033061733,126.265284005786));
#101940=CARTESIAN_POINT('Ctrl Pts',(2.38186402993216,-28.4249415778899,
126.321466203333));
#101941=CARTESIAN_POINT('Ctrl Pts',(2.38571923618317,-28.4717919854813,
126.375378003393));
#101942=CARTESIAN_POINT('Ctrl Pts',(2.38957444243417,-28.5213140123004,
126.426704353495));
#101943=CARTESIAN_POINT('Ctrl Pts',(2.39342979929112,-28.5708379737271,
126.478032708692));
#101944=CARTESIAN_POINT('Ctrl Pts',(2.39728515614807,-28.6230334227032,
126.526775065342));
#101945=CARTESIAN_POINT('Ctrl Pts',(2.40114051300502,-28.6775928133142,
126.572652789112));
#101946=CARTESIAN_POINT('Ctrl Pts',(2.4049999054793,-28.7322093142863,126.618578535658));
#101947=CARTESIAN_POINT('Ctrl Pts',(2.40885929795358,-28.789194323921,126.661633350216));
#101948=CARTESIAN_POINT('Ctrl Pts',(2.41271869042785,-28.8482074506336,
126.701579115329));
#101949=CARTESIAN_POINT('Ctrl Pts',(2.41658026803702,-28.9072539897662,
126.741547497185));
#101950=CARTESIAN_POINT('Ctrl Pts',(2.42044184564619,-28.9683305157479,
126.778403074276));
#101951=CARTESIAN_POINT('Ctrl Pts',(2.42430342325536,-29.031070268971,126.811952741886));
#101952=CARTESIAN_POINT('Ctrl Pts',(2.42817175737592,-29.0939197964628,
126.845561110559));
#101953=CARTESIAN_POINT('Ctrl Pts',(2.43204009149649,-29.1584379214406,
126.875851814768));
#101954=CARTESIAN_POINT('Ctrl Pts',(2.43590842561706,-29.2242367158349,
126.90267939744));
#101955=CARTESIAN_POINT('Ctrl Pts',(2.43820614473736,-29.2633199861162,
126.918614486741));
#101956=CARTESIAN_POINT('Ctrl Pts',(2.44050386385766,-29.3028547606617,
126.933328680147));
#101957=CARTESIAN_POINT('Ctrl Pts',(2.44280158297796,-29.3427575594249,
126.94679992213));
#101958=CARTESIAN_POINT('Ctrl Pts',(2.44667069996889,-29.4099496697731,
126.96948407477));
#101959=CARTESIAN_POINT('Ctrl Pts',(2.45053981695982,-29.4784491577362,
126.988729960308));
#101960=CARTESIAN_POINT('Ctrl Pts',(2.45440893395075,-29.5478707454889,
127.004389358312));
#101961=CARTESIAN_POINT('Ctrl Pts',(2.45827227326046,-29.6171886672618,
127.020025372426));
#101962=CARTESIAN_POINT('Ctrl Pts',(2.46213561257017,-29.6874254855223,
127.032085423932));
#101963=CARTESIAN_POINT('Ctrl Pts',(2.46599895187988,-29.7581794473605,
127.040470627777));
#101964=CARTESIAN_POINT('Ctrl Pts',(2.46985771072428,-29.8288495216491,
127.048845889928));
#101965=CARTESIAN_POINT('Ctrl Pts',(2.47371646956868,-29.9000350414532,
127.0535549026));
#101966=CARTESIAN_POINT('Ctrl Pts',(2.47757522841307,-29.9713244405029,
127.054549895911));
#101967=CARTESIAN_POINT('Ctrl Pts',(2.4814315383272,-30.0425685963087,127.055544257758));
#101968=CARTESIAN_POINT('Ctrl Pts',(2.48528784824132,-30.1139160159822,
127.052829270173));
#101969=CARTESIAN_POINT('Ctrl Pts',(2.48914415815545,-30.1849518563648,
127.046409141234));
#101970=CARTESIAN_POINT('Ctrl Pts',(2.49299931071214,-30.2559663774397,
127.039990939108));
#101971=CARTESIAN_POINT('Ctrl Pts',(2.49685446326883,-30.3266690213727,
127.029869847219));
#101972=CARTESIAN_POINT('Ctrl Pts',(2.50070961582552,-30.3966485300909,
127.016102057456));
#101973=CARTESIAN_POINT('Ctrl Pts',(2.5045649009602,-30.4666304453915,127.00233379422));
#101974=CARTESIAN_POINT('Ctrl Pts',(2.50842018609487,-30.5358886999794,
126.984918680344));
#101975=CARTESIAN_POINT('Ctrl Pts',(2.51227547122954,-30.6040224212736,
126.963963970418));
#101976=CARTESIAN_POINT('Ctrl Pts',(2.51613458281858,-30.6722237667684,
126.942988462486));
#101977=CARTESIAN_POINT('Ctrl Pts',(2.51999369440761,-30.7392978863037,
126.918466490123));
#101978=CARTESIAN_POINT('Ctrl Pts',(2.52385280599665,-30.8048601934944,
126.890554847506));
#101979=CARTESIAN_POINT('Ctrl Pts',(2.527714095329,-30.8704594982875,126.862627454012));
#101980=CARTESIAN_POINT('Ctrl Pts',(2.53157538466135,-30.9345448559496,
126.83130679581));
#101981=CARTESIAN_POINT('Ctrl Pts',(2.5354366739937,-30.9967551906669,126.796796218935));
#101982=CARTESIAN_POINT('Ctrl Pts',(2.53930424299619,-31.0590666989424,
126.762229517014));
#101983=CARTESIAN_POINT('Ctrl Pts',(2.54317181199867,-31.119496686546,126.724462799682));
#101984=CARTESIAN_POINT('Ctrl Pts',(2.54703938100116,-31.1777127385792,
126.683742934028));
#101985=CARTESIAN_POINT('Ctrl Pts',(2.54871345326657,-31.2029114817815,
126.666117392583));
#101986=CARTESIAN_POINT('Ctrl Pts',(2.55038752553198,-31.2276958470359,
126.647939068268));
#101987=CARTESIAN_POINT('Ctrl Pts',(2.55206159779739,-31.2520409112987,
126.629230222815));
#101988=CARTESIAN_POINT('',(2.24592528056747,-27.9452508239572,124.998159877293));
#101989=CARTESIAN_POINT('Ctrl Pts',(2.24592528056747,-27.9452508239572,
124.998159877293));
#101990=CARTESIAN_POINT('Ctrl Pts',(2.24973199310619,-27.9451880222813,
125.068286554887));
#101991=CARTESIAN_POINT('Ctrl Pts',(2.25353870564491,-27.9487194885961,
125.138525579213));
#101992=CARTESIAN_POINT('Ctrl Pts',(2.25734541818363,-27.9558530802283,
125.208472858876));
#101993=CARTESIAN_POINT('Ctrl Pts',(2.26114901952475,-27.9629808416296,
125.278362971152));
#101994=CARTESIAN_POINT('Ctrl Pts',(2.26495262086587,-27.9737048434681,
125.347961315223));
#101995=CARTESIAN_POINT('Ctrl Pts',(2.268756222207,-27.9879809096171,125.416865376872));
#101996=CARTESIAN_POINT('Ctrl Pts',(2.27255807181682,-28.0022504009888,
125.485737705069));
#101997=CARTESIAN_POINT('Ctrl Pts',(2.27635992142664,-28.0200686114227,
125.553915895166));
#101998=CARTESIAN_POINT('Ctrl Pts',(2.28016177103647,-28.0413399857073,
125.621006047403));
#101999=CARTESIAN_POINT('Ctrl Pts',(2.28396322582589,-28.0626091509691,
125.688089232357));
#102000=CARTESIAN_POINT('Ctrl Pts',(2.28776468061532,-28.0873306153714,
125.754084126905));
#102001=CARTESIAN_POINT('Ctrl Pts',(2.29156613540474,-28.1153590731372,
125.818612325398));
#102002=CARTESIAN_POINT('Ctrl Pts',(2.29537111048207,-28.1434134862929,
125.883200279393));
#102003=CARTESIAN_POINT('Ctrl Pts',(2.2991760855594,-28.1747808077104,125.946318364991));
#102004=CARTESIAN_POINT('Ctrl Pts',(2.30298106063673,-28.2092681474416,
126.00760954478));
#102005=CARTESIAN_POINT('Ctrl Pts',(2.30678785553211,-28.2437719815472,
126.068930038506));
#102006=CARTESIAN_POINT('Ctrl Pts',(2.3105946504275,-28.2813985348242,126.128421464577));
#102007=CARTESIAN_POINT('Ctrl Pts',(2.31440144532288,-28.3219111791817,
126.185755232729));
#102008=CARTESIAN_POINT('Ctrl Pts',(2.31821492439056,-28.3624949577879,
126.243189670551));
#102009=CARTESIAN_POINT('Ctrl Pts',(2.32202840345824,-28.4059746336492,
126.298458493979));
#102010=CARTESIAN_POINT('Ctrl Pts',(2.32584188252591,-28.4520733934073,
126.351266362751));
#102011=CARTESIAN_POINT('Ctrl Pts',(2.32850815088719,-28.4843042415268,
126.388188015456));
#102012=CARTESIAN_POINT('Ctrl Pts',(2.33117441924847,-28.5178145732298,
126.42390739227));
#102013=CARTESIAN_POINT('Ctrl Pts',(2.33384068760975,-28.5524999386655,
126.458335055787));
#102014=CARTESIAN_POINT('Ctrl Pts',(2.3377097609577,-28.6028325401845,126.50829370109));
#102015=CARTESIAN_POINT('Ctrl Pts',(2.34157883430565,-28.6558531560725,
126.555741393499));
#102016=CARTESIAN_POINT('Ctrl Pts',(2.3454479076536,-28.7112811808808,126.600375383386));
#102017=CARTESIAN_POINT('Ctrl Pts',(2.34931121604923,-28.766626617459,126.644942868247));
#102018=CARTESIAN_POINT('Ctrl Pts',(2.35317452444486,-28.8243719674648,
126.686704670265));
#102019=CARTESIAN_POINT('Ctrl Pts',(2.3570378328405,-28.8842001037992,126.7253950719));
#102020=CARTESIAN_POINT('Ctrl Pts',(2.36089660933343,-28.9439580579829,
126.764040087272));
#102021=CARTESIAN_POINT('Ctrl Pts',(2.36475538582637,-29.0057935394568,
126.79962059641));
#102022=CARTESIAN_POINT('Ctrl Pts',(2.36861416231931,-29.0693580855252,
126.831912440463));
#102023=CARTESIAN_POINT('Ctrl Pts',(2.37247050790765,-29.132882587982,126.864183941697));
#102024=CARTESIAN_POINT('Ctrl Pts',(2.37632685349599,-29.1981335618907,
126.893170668666));
#102025=CARTESIAN_POINT('Ctrl Pts',(2.38018319908433,-29.2647367038568,
126.918693682651));
#102026=CARTESIAN_POINT('Ctrl Pts',(2.3840384053299,-29.3313201681756,126.944209155958));
#102027=CARTESIAN_POINT('Ctrl Pts',(2.38789361157548,-29.3992545540755,
126.966262774159));
#102028=CARTESIAN_POINT('Ctrl Pts',(2.39174881782105,-29.4681458750043,
126.98472384785));
#102029=CARTESIAN_POINT('Ctrl Pts',(2.39560417467265,-29.5370398872153,
127.003185642735));
#102030=CARTESIAN_POINT('Ctrl Pts',(2.39945953152424,-29.6068904388744,
127.01805449086));
#102031=CARTESIAN_POINT('Ctrl Pts',(2.40331488837584,-29.677290371186,127.029250122082));
#102032=CARTESIAN_POINT('Ctrl Pts',(2.40717428084491,-29.7477639950412,
127.040457472397));
#102033=CARTESIAN_POINT('Ctrl Pts',(2.41103367331399,-29.8187876667723,
127.047983853952));
#102034=CARTESIAN_POINT('Ctrl Pts',(2.41489306578306,-29.8899469624257,
127.051800646121));
#102035=CARTESIAN_POINT('Ctrl Pts',(2.4187546433871,-29.9611465474941,127.055619599305));
#102036=CARTESIAN_POINT('Ctrl Pts',(2.42261622099113,-30.0324814233311,
127.055724781301));
#102037=CARTESIAN_POINT('Ctrl Pts',(2.42647779859517,-30.1035377690062,
127.052139735225));
#102038=CARTESIAN_POINT('Ctrl Pts',(2.43034613271079,-30.1747184402994,
127.048548416478));
#102039=CARTESIAN_POINT('Ctrl Pts',(2.43421446682641,-30.2456191250582,
127.041254028392));
#102040=CARTESIAN_POINT('Ctrl Pts',(2.43808280094203,-30.3158324191724,
127.030331856003));
#102041=CARTESIAN_POINT('Ctrl Pts',(2.44038052011079,-30.3575378217996,
127.023844286906));
#102042=CARTESIAN_POINT('Ctrl Pts',(2.44267823927955,-30.3990009027221,
127.016077763855));
#102043=CARTESIAN_POINT('Ctrl Pts',(2.44497595844831,-30.440138756094,127.007056411236));
#102044=CARTESIAN_POINT('Ctrl Pts',(2.44884535140181,-30.5094155076324,
126.991864320432));
#102045=CARTESIAN_POINT('Ctrl Pts',(2.45271474435532,-30.5780404729772,
126.973051462176));
#102046=CARTESIAN_POINT('Ctrl Pts',(2.45658413730882,-30.645607008178,126.95068940467));
#102047=CARTESIAN_POINT('Ctrl Pts',(2.46044683557589,-30.7130566421563,
126.928366037202));
#102048=CARTESIAN_POINT('Ctrl Pts',(2.46430953384297,-30.7794510271505,
126.902505823078));
#102049=CARTESIAN_POINT('Ctrl Pts',(2.46817223211004,-30.8443951111531,
126.873231021193));
#102050=CARTESIAN_POINT('Ctrl Pts',(2.47203108524621,-30.9092745464342,
126.84398536097));
#102051=CARTESIAN_POINT('Ctrl Pts',(2.47588993838239,-30.9727061043097,
126.81133205486));
#102052=CARTESIAN_POINT('Ctrl Pts',(2.47974879151856,-31.0343124417274,
126.775442292891));
#102053=CARTESIAN_POINT('Ctrl Pts',(2.48360488023206,-31.0958746453184,
126.739578241793));
#102054=CARTESIAN_POINT('Ctrl Pts',(2.48746096894557,-31.1556138066068,
126.70048258348));
#102055=CARTESIAN_POINT('Ctrl Pts',(2.49131705765907,-31.2131766508907,
126.658372689185));
#102056=CARTESIAN_POINT('Ctrl Pts',(2.49219248057369,-31.2262447716371,
126.648812751865));
#102057=CARTESIAN_POINT('Ctrl Pts',(2.49306790348832,-31.2392008355424,
126.639097643592));
#102058=CARTESIAN_POINT('Ctrl Pts',(2.49394332640294,-31.2520409112987,
126.629230222815));
#102059=CARTESIAN_POINT('Ctrl Pts',(1.79398326297881,-31.2520409112987,
126.629230222815));
#102060=CARTESIAN_POINT('Ctrl Pts',(1.79795477719867,-31.3100239000484,
126.584671097249));
#102061=CARTESIAN_POINT('Ctrl Pts',(1.80192629141854,-31.3657081646153,
126.53694901864));
#102062=CARTESIAN_POINT('Ctrl Pts',(1.8058978056384,-31.4187339253545,126.486334959405));
#102063=CARTESIAN_POINT('Ctrl Pts',(1.80975547492232,-31.4702396828908,
126.43717177105));
#102064=CARTESIAN_POINT('Ctrl Pts',(1.81361314420623,-31.5192369238096,
126.385280532738));
#102065=CARTESIAN_POINT('Ctrl Pts',(1.81747081349015,-31.5654288977993,
126.330950761086));
#102066=CARTESIAN_POINT('Ctrl Pts',(1.82132655812563,-31.6115978259278,
126.276648095363));
#102067=CARTESIAN_POINT('Ctrl Pts',(1.8251823027611,-31.6549639501939,126.219909680033));
#102068=CARTESIAN_POINT('Ctrl Pts',(1.82903804739658,-31.6952688910805,
126.16106026951));
#102069=CARTESIAN_POINT('Ctrl Pts',(1.83289315815994,-31.7355672059634,
126.102220533643));
#102070=CARTESIAN_POINT('Ctrl Pts',(1.83674826892331,-31.7728050628913,
126.041270892824));
#102071=CARTESIAN_POINT('Ctrl Pts',(1.84060337968667,-31.8067667655206,
125.97856600059));
#102072=CARTESIAN_POINT('Ctrl Pts',(1.84466139840074,-31.8425159912344,
125.912560730762));
#102073=CARTESIAN_POINT('Ctrl Pts',(1.84871941711481,-31.8746343923033,
125.844610859921));
#102074=CARTESIAN_POINT('Ctrl Pts',(1.85277743582888,-31.902925891643,125.775158444071));
#102075=CARTESIAN_POINT('Ctrl Pts',(1.85663765431487,-31.9298383768834,
125.709091351125));
#102076=CARTESIAN_POINT('Ctrl Pts',(1.86049787280086,-31.9532882097898,
125.64166526996));
#102077=CARTESIAN_POINT('Ctrl Pts',(1.86435809128686,-31.9731573139482,
125.57327809736));
#102078=CARTESIAN_POINT('Ctrl Pts',(1.86822100972785,-31.9930403151663,
125.504843092678));
#102079=CARTESIAN_POINT('Ctrl Pts',(1.87208392816884,-32.0093374949156,
125.435446131666));
#102080=CARTESIAN_POINT('Ctrl Pts',(1.87594684660983,-32.0219818112365,
125.365495714789));
#102081=CARTESIAN_POINT('Ctrl Pts',(1.87981602035975,-32.0346466027773,
125.29543202566));
#102082=CARTESIAN_POINT('Ctrl Pts',(1.88368519410967,-32.0436466744898,
125.224813573776));
#102083=CARTESIAN_POINT('Ctrl Pts',(1.88755436785959,-32.0489668424968,
125.154053370131));
#102084=CARTESIAN_POINT('Ctrl Pts',(1.88813611332489,-32.0497667506458,
125.143414295679));
#102085=CARTESIAN_POINT('Ctrl Pts',(1.8887178587902,-32.0504835657235,125.132772013456));
#102086=CARTESIAN_POINT('Ctrl Pts',(1.88929960425551,-32.0511173377636,
125.122127921564));
#102087=CARTESIAN_POINT('Ctrl Pts',(1.8931686779118,-32.0553324298458,125.051336178452));
#102088=CARTESIAN_POINT('Ctrl Pts',(1.89703775156808,-32.0558865433681,
124.980187299047));
#102089=CARTESIAN_POINT('Ctrl Pts',(1.90090682522436,-32.0527379987999,
124.909091965246));
#102090=CARTESIAN_POINT('Ctrl Pts',(1.90477013393189,-32.0495941455867,
124.838102564025));
#102091=CARTESIAN_POINT('Ctrl Pts',(1.90863344263941,-32.0427586066674,
124.767167031397));
#102092=CARTESIAN_POINT('Ctrl Pts',(1.91249675134693,-32.0322416318168,
124.696698973937));
#102093=CARTESIAN_POINT('Ctrl Pts',(1.9163555281555,-32.021736994025,124.626313579847));
#102094=CARTESIAN_POINT('Ctrl Pts',(1.92021430496407,-32.0075595697636,
124.556395049793));
#102095=CARTESIAN_POINT('Ctrl Pts',(1.92407308177264,-31.9897715065036,
124.487353031408));
#102096=CARTESIAN_POINT('Ctrl Pts',(1.92792942767875,-31.9719946491384,
124.418354507224));
#102097=CARTESIAN_POINT('Ctrl Pts',(1.93178577358485,-31.950611786426,124.350231868515));
#102098=CARTESIAN_POINT('Ctrl Pts',(1.93564211949096,-31.9257360785957,
124.283384260503));
#102099=CARTESIAN_POINT('Ctrl Pts',(1.93949732605596,-31.9008677201881,
124.216556402334));
#102100=CARTESIAN_POINT('Ctrl Pts',(1.94335253262096,-31.8725087346924,
124.151003282038));
#102101=CARTESIAN_POINT('Ctrl Pts',(1.94720773918597,-31.8408214977065,
124.087106919688));
#102102=CARTESIAN_POINT('Ctrl Pts',(1.95106309635817,-31.8091330228294,
124.023208061167));
#102103=CARTESIAN_POINT('Ctrl Pts',(1.95491845353038,-31.7741162561223,
123.960966523321));
#102104=CARTESIAN_POINT('Ctrl Pts',(1.95877381070259,-31.7359801128372,
123.900740881169));
#102105=CARTESIAN_POINT('Ctrl Pts',(1.96263320349186,-31.697804050327,123.840452197483));
#102106=CARTESIAN_POINT('Ctrl Pts',(1.96649259628114,-31.6565023535359,
123.782184033088));
#102107=CARTESIAN_POINT('Ctrl Pts',(1.97035198907041,-31.6123274957083,
123.726266272299));
#102108=CARTESIAN_POINT('Ctrl Pts',(1.9742135669949,-31.5681276266825,123.670316851641));
#102109=CARTESIAN_POINT('Ctrl Pts',(1.97807514491939,-31.5210516790099,
123.616720848893));
#102110=CARTESIAN_POINT('Ctrl Pts',(1.98193672284388,-31.4713908686318,
123.565773213816));
#102111=CARTESIAN_POINT('Ctrl Pts',(1.98580505727686,-31.4216431679479,
123.514736436908));
#102112=CARTESIAN_POINT('Ctrl Pts',(1.98967339170984,-31.3693019317678,
123.466357608996));
#102113=CARTESIAN_POINT('Ctrl Pts',(1.99354172614282,-31.3146929590917,
123.420892661718));
#102114=CARTESIAN_POINT('Ctrl Pts',(1.9958394424599,-31.282256278719,123.393887356716));
#102115=CARTESIAN_POINT('Ctrl Pts',(1.99813715877699,-31.2490201142081,
123.367909310058));
#102116=CARTESIAN_POINT('Ctrl Pts',(2.00043487509407,-31.2150573708127,
123.34300478331));
#102117=CARTESIAN_POINT('Ctrl Pts',(2.00430394846991,-31.1578682629736,
123.301068604913));
#102118=CARTESIAN_POINT('Ctrl Pts',(2.00817302184574,-31.0983935262999,
123.262014475619));
#102119=CARTESIAN_POINT('Ctrl Pts',(2.01204209522157,-31.0369555869914,
123.226100151331));
#102120=CARTESIAN_POINT('Ctrl Pts',(2.01590540364641,-30.9756091907153,
123.19023933968));
#102121=CARTESIAN_POINT('Ctrl Pts',(2.01976871207125,-30.9123058141906,
123.157509289833));
#102122=CARTESIAN_POINT('Ctrl Pts',(2.02363202049609,-30.8473985053611,
123.128125715863));
#102123=CARTESIAN_POINT('Ctrl Pts',(2.02749079702005,-30.7825673368385,
123.098776610652));
#102124=CARTESIAN_POINT('Ctrl Pts',(2.03134957354402,-30.7161364137331,
123.072766383073));
#102125=CARTESIAN_POINT('Ctrl Pts',(2.03520835006799,-30.6484836053586,
123.050264998498));
#102126=CARTESIAN_POINT('Ctrl Pts',(2.03906469568848,-30.5808734160492,
123.027777789063));
#102127=CARTESIAN_POINT('Ctrl Pts',(2.04292104130896,-30.5120433285063,
123.008795190075));
#102128=CARTESIAN_POINT('Ctrl Pts',(2.04677738692944,-30.4423900560028,
122.993438612738));
#102129=CARTESIAN_POINT('Ctrl Pts',(2.05063259320823,-30.3727573622766,
122.97808657244));
#102130=CARTESIAN_POINT('Ctrl Pts',(2.05448779948702,-30.3023024405569,
122.966358531514));
#102131=CARTESIAN_POINT('Ctrl Pts',(2.0583430057658,-30.2314343091854,122.958325265124));
#102132=CARTESIAN_POINT('Ctrl Pts',(2.06219836265164,-30.1605634092877,
122.950291684907));
#102133=CARTESIAN_POINT('Ctrl Pts',(2.06605371953747,-30.0892797506324,
122.945953218321));
#102134=CARTESIAN_POINT('Ctrl Pts',(2.0699090764233,-30.0179978957906,122.945328824788));
#102135=CARTESIAN_POINT('Ctrl Pts',(2.07376846892795,-29.9466414262238,
122.944703777667));
#102136=CARTESIAN_POINT('Ctrl Pts',(2.07762786143259,-29.8752872510023,
122.947800568642));
#102137=CARTESIAN_POINT('Ctrl Pts',(2.08148725393723,-29.8043494526783,
122.95458600136));
#102138=CARTESIAN_POINT('Ctrl Pts',(2.08534883157766,-29.7333714903335,
122.961375275898));
#102139=CARTESIAN_POINT('Ctrl Pts',(2.08921040921808,-29.6628108549264,
122.97185727824));
#102140=CARTESIAN_POINT('Ctrl Pts',(2.0930719868585,-29.5930732916184,122.98594731536));
#102141=CARTESIAN_POINT('Ctrl Pts',(2.09694032101139,-29.52321371012,123.000062005489));
#102142=CARTESIAN_POINT('Ctrl Pts',(2.10080865516429,-29.4541805465985,
123.017797213357));
#102143=CARTESIAN_POINT('Ctrl Pts',(2.10467698931718,-29.3863655219985,
123.039018029173));
#102144=CARTESIAN_POINT('Ctrl Pts',(2.106974708189,-29.346084652855,123.051622800904));
#102145=CARTESIAN_POINT('Ctrl Pts',(2.10927242706081,-29.3062332176237,
123.065456404863));
#102146=CARTESIAN_POINT('Ctrl Pts',(2.11157014593263,-29.266889624117,123.080482680653));
#102147=CARTESIAN_POINT('Ctrl Pts',(2.11543921919095,-29.2006398981864,
123.105785063179));
#102148=CARTESIAN_POINT('Ctrl Pts',(2.11930829244926,-29.1355718640553,
123.134570821762));
#102149=CARTESIAN_POINT('Ctrl Pts',(2.12317736570758,-29.0720769460634,
123.16670886969));
#102150=CARTESIAN_POINT('Ctrl Pts',(2.12704067401181,-29.0086766360726,
123.198799031637));
#102151=CARTESIAN_POINT('Ctrl Pts',(2.13090398231604,-28.946845219429,123.234231350518));
#102152=CARTESIAN_POINT('Ctrl Pts',(2.13476729062027,-28.88695540744,123.272826210981));
#102153=CARTESIAN_POINT('Ctrl Pts',(2.1386260670196,-28.8271358499872,123.311375797234));
#102154=CARTESIAN_POINT('Ctrl Pts',(2.14248484341893,-28.7692537794135,
123.353080294159));
#102155=CARTESIAN_POINT('Ctrl Pts',(2.14634361981825,-28.7136569337726,
123.397714420439));
#102156=CARTESIAN_POINT('Ctrl Pts',(2.15019996531167,-28.658095112369,123.442320428645));
#102157=CARTESIAN_POINT('Ctrl Pts',(2.15405631080509,-28.6048160376363,
123.489852101218));
#102158=CARTESIAN_POINT('Ctrl Pts',(2.15791265629851,-28.5541368754454,
123.540041991168));
#102159=CARTESIAN_POINT('Ctrl Pts',(2.16176786244799,-28.5034726862377,
123.590217052689));
#102160=CARTESIAN_POINT('Ctrl Pts',(2.16562306859748,-28.4554072295875,
123.643048430781));
#102161=CARTESIAN_POINT('Ctrl Pts',(2.16947827474696,-28.4102218036538,
123.698230877259));
#102162=CARTESIAN_POINT('Ctrl Pts',(2.17333363150144,-28.3650346125353,
123.753415479459));
#102163=CARTESIAN_POINT('Ctrl Pts',(2.17718898825592,-28.3227279815673,
123.810950955138));
#102164=CARTESIAN_POINT('Ctrl Pts',(2.1810443450104,-28.2835426832373,123.870499295161));
#102165=CARTESIAN_POINT('Ctrl Pts',(2.18490373738144,-28.2443163674738,
123.930109967747));
#102166=CARTESIAN_POINT('Ctrl Pts',(2.18876312975249,-28.2082181741437,
123.991737304038));
#102167=CARTESIAN_POINT('Ctrl Pts',(2.19262252212353,-28.175444797052,124.055015410763));
#102168=CARTESIAN_POINT('Ctrl Pts',(2.19648409962889,-28.1426528641299,
124.118329344672));
#102169=CARTESIAN_POINT('Ctrl Pts',(2.20034567713425,-28.11318969559,124.183295466976));
#102170=CARTESIAN_POINT('Ctrl Pts',(2.20420725463961,-28.0872041987393,
124.249526959059));
#102171=CARTESIAN_POINT('Ctrl Pts',(2.20807558865656,-28.061173235674,124.315874334831));
#102172=CARTESIAN_POINT('Ctrl Pts',(2.21194392267352,-28.0386322464595,
124.383491039674));
#102173=CARTESIAN_POINT('Ctrl Pts',(2.21581225669047,-28.0196803428808,
124.451974801558));
#102174=CARTESIAN_POINT('Ctrl Pts',(2.21810997671738,-28.0084232569597,
124.492652910147));
#102175=CARTESIAN_POINT('Ctrl Pts',(2.22040769674429,-27.9984314773309,
124.533636707412));
#102176=CARTESIAN_POINT('Ctrl Pts',(2.22270541677119,-27.98971714967,124.5748407073));
#102177=CARTESIAN_POINT('Ctrl Pts',(2.22812785149404,-27.9691520362785,
124.672078837751));
#102178=CARTESIAN_POINT('Ctrl Pts',(2.23355028621689,-27.9556362047534,
124.770855989234));
#102179=CARTESIAN_POINT('Ctrl Pts',(2.23897272093974,-27.9493462562119,
124.870320450387));
#102180=CARTESIAN_POINT('Ctrl Pts',(2.24129024080572,-27.946657965537,124.912831034001));
#102181=CARTESIAN_POINT('Ctrl Pts',(2.2436077606717,-27.9452890575184,124.95546687936));
#102182=CARTESIAN_POINT('Ctrl Pts',(2.24592528053768,-27.9452508239577,
124.998159876744));
#102183=CARTESIAN_POINT('Origin',(-1.54592528053767,-30.,125.));
#102184=CARTESIAN_POINT('',(1.09386069669771,-31.2520409112987,126.629230222815));
#102185=CARTESIAN_POINT('',(1.15210970423049,-31.2520409112987,126.629230222815));
#102186=CARTESIAN_POINT('',(-1.54592528053767,-31.2520409112987,126.629230222815));
#102187=CARTESIAN_POINT('',(1.60407471941018,-27.9452500663321,124.999477896899));
#102188=CARTESIAN_POINT('Ctrl Pts',(1.15210970423049,-31.2520409112987,
126.629230222815));
#102189=CARTESIAN_POINT('Ctrl Pts',(1.1559651187354,-31.308569673581,126.585788650193));
#102190=CARTESIAN_POINT('Ctrl Pts',(1.15982053324031,-31.3628595945105,
126.539382601305));
#102191=CARTESIAN_POINT('Ctrl Pts',(1.16367594774522,-31.4145917589832,
126.490277731806));
#102192=CARTESIAN_POINT('Ctrl Pts',(1.16753113264579,-31.4663208426124,
126.441175786685));
#102193=CARTESIAN_POINT('Ctrl Pts',(1.17138631754637,-31.5154921209874,
126.389375675649));
#102194=CARTESIAN_POINT('Ctrl Pts',(1.17524150244695,-31.5618224856364,
126.335180918775));
#102195=CARTESIAN_POINT('Ctrl Pts',(1.17910047876147,-31.6081984142713,
126.280932863612));
#102196=CARTESIAN_POINT('Ctrl Pts',(1.18295945507599,-31.6517275316966,
126.224285828409));
#102197=CARTESIAN_POINT('Ctrl Pts',(1.18681843139052,-31.6921666883546,
126.165576879199));
#102198=CARTESIAN_POINT('Ctrl Pts',(1.19067925130637,-31.7326251645619,
126.106839882162));
#102199=CARTESIAN_POINT('Ctrl Pts',(1.19454007122222,-31.7699904843435,
126.046039423183));
#102200=CARTESIAN_POINT('Ctrl Pts',(1.19840089113807,-31.8040640891954,
125.983539691408));
#102201=CARTESIAN_POINT('Ctrl Pts',(1.202268829534,-31.8382005180801,125.920924724242));
#102202=CARTESIAN_POINT('Ctrl Pts',(1.20613676792992,-31.8690328951808,
125.856604663548));
#102203=CARTESIAN_POINT('Ctrl Pts',(1.21000470632584,-31.8964099070394,
125.790965882313));
#102204=CARTESIAN_POINT('Ctrl Pts',(1.2134410054685,-31.9207318048435,125.732652004325));
#102205=CARTESIAN_POINT('Ctrl Pts',(1.21687730461115,-31.9423271335707,
125.673297808585));
#102206=CARTESIAN_POINT('Ctrl Pts',(1.2203136037538,-31.9611231636045,125.613183088216));
#102207=CARTESIAN_POINT('Ctrl Pts',(1.22418267030921,-31.9822863651068,
125.545497521735));
#102208=CARTESIAN_POINT('Ctrl Pts',(1.22805173686462,-31.9999827911828,
125.476582456271));
#102209=CARTESIAN_POINT('Ctrl Pts',(1.23192080342002,-32.0140729490346,
125.406826398439));
#102210=CARTESIAN_POINT('Ctrl Pts',(1.23578410490835,-32.0281421119762,
125.33717427998));
#102211=CARTESIAN_POINT('Ctrl Pts',(1.23964740639668,-32.0386155775137,
125.266684128839));
#102212=CARTESIAN_POINT('Ctrl Pts',(1.24351070788501,-32.0454035440006,
125.195759813777));
#102213=CARTESIAN_POINT('Ctrl Pts',(1.24736947733365,-32.0521835475227,
125.124918700042));
#102214=CARTESIAN_POINT('Ctrl Pts',(1.25122824678228,-32.0552865937895,
125.053644915294));
#102215=CARTESIAN_POINT('Ctrl Pts',(1.25508701623091,-32.0546742017609,
124.982351002343));
#102216=CARTESIAN_POINT('Ctrl Pts',(1.25894335469421,-32.054062195533,124.91110200383));
#102217=CARTESIAN_POINT('Ctrl Pts',(1.2627996931575,-32.0497393990592,124.839833386893));
#102218=CARTESIAN_POINT('Ctrl Pts',(1.2666560316208,-32.0417193711735,124.768959804634));
#102219=CARTESIAN_POINT('Ctrl Pts',(1.2705112306712,-32.0337017129251,124.698107163035));
#102220=CARTESIAN_POINT('Ctrl Pts',(1.27436642972161,-32.0219890465787,
124.627649806838));
#102221=CARTESIAN_POINT('Ctrl Pts',(1.27822162877202,-32.0066468237053,
124.557997638679));
#102222=CARTESIAN_POINT('Ctrl Pts',(1.28207697836888,-31.9913040017144,
124.488342750586));
#102223=CARTESIAN_POINT('Ctrl Pts',(1.28593232796574,-31.9723314484503,
124.419493586897));
#102224=CARTESIAN_POINT('Ctrl Pts',(1.2897876775626,-31.9498454356419,124.351848521095));
#102225=CARTESIAN_POINT('Ctrl Pts',(1.29364706273577,-31.9273358856629,
124.284132648011));
#102226=CARTESIAN_POINT('Ctrl Pts',(1.29750644790895,-31.9013056881675,
124.217623850758));
#102227=CARTESIAN_POINT('Ctrl Pts',(1.30136583308213,-31.8719203064661,
124.152703163738));
#102228=CARTESIAN_POINT('Ctrl Pts',(1.30522740335605,-31.8425182873948,
124.087745720024));
#102229=CARTESIAN_POINT('Ctrl Pts',(1.30908897362996,-31.8097575257402,
124.024378608213));
#102230=CARTESIAN_POINT('Ctrl Pts',(1.31295054390387,-31.7738495090303,
123.962958302761));
#102231=CARTESIAN_POINT('Ctrl Pts',(1.31681887071462,-31.7378786645533,
123.901430531038));
#102232=CARTESIAN_POINT('Ctrl Pts',(1.32068719752537,-31.6987498374917,
123.841856772617));
#102233=CARTESIAN_POINT('Ctrl Pts',(1.32455552433612,-31.6567174875471,
123.784563975787));
#102234=CARTESIAN_POINT('Ctrl Pts',(1.32685330775487,-31.6317503010919,
123.75053209456));
#102235=CARTESIAN_POINT('Ctrl Pts',(1.32915109117362,-31.6057594272786,
123.717304388655));
#102236=CARTESIAN_POINT('Ctrl Pts',(1.33144887459236,-31.5788044682051,
123.684943342028));
#102237=CARTESIAN_POINT('Ctrl Pts',(1.33531795015095,-31.5334169123184,
123.630452856314));
#102238=CARTESIAN_POINT('Ctrl Pts',(1.33918702570954,-31.485116135623,123.578208140709));
#102239=CARTESIAN_POINT('Ctrl Pts',(1.34305610126813,-31.434152886149,123.528537101504));
#102240=CARTESIAN_POINT('Ctrl Pts',(1.34691941189731,-31.3832655720066,
123.478940072234));
#102241=CARTESIAN_POINT('Ctrl Pts',(1.35078272252649,-31.3297240046965,
123.431909443729));
#102242=CARTESIAN_POINT('Ctrl Pts',(1.35464603315567,-31.2738187891828,
123.387739706243));
#102243=CARTESIAN_POINT('Ctrl Pts',(1.35850481190518,-31.2179791536169,
123.343621782332));
#102244=CARTESIAN_POINT('Ctrl Pts',(1.36236359065469,-31.1597817566726,
123.302358383013));
#102245=CARTESIAN_POINT('Ctrl Pts',(1.36622236940421,-31.0995523250525,
123.264205586202));
#102246=CARTESIAN_POINT('Ctrl Pts',(1.37007871726209,-31.039360835805,123.226076824279));
#102247=CARTESIAN_POINT('Ctrl Pts',(1.37393506511997,-30.9771402610041,
123.191055036457));
#102248=CARTESIAN_POINT('Ctrl Pts',(1.37779141297786,-30.9132463246948,
123.159353724114));
#102249=CARTESIAN_POINT('Ctrl Pts',(1.38164662150252,-30.8493712654389,
123.127661777721));
#102250=CARTESIAN_POINT('Ctrl Pts',(1.38550183002718,-30.7838242610932,
123.099288575016));
#102251=CARTESIAN_POINT('Ctrl Pts',(1.38935703855185,-30.7169851892392,
123.07440144347));
#102252=CARTESIAN_POINT('Ctrl Pts',(1.39321239768867,-30.6501435061704,
123.049513339653));
#102253=CARTESIAN_POINT('Ctrl Pts',(1.3970677568255,-30.5820101113969,123.02811174483));
#102254=CARTESIAN_POINT('Ctrl Pts',(1.40092311596233,-30.5129827592616,
123.010315037198));
#102255=CARTESIAN_POINT('Ctrl Pts',(1.40478251071016,-30.4438831524978,
122.992499700798));
#102256=CARTESIAN_POINT('Ctrl Pts',(1.40864190545801,-30.3738881917653,
122.978296905729));
#102257=CARTESIAN_POINT('Ctrl Pts',(1.41250130020584,-30.3034077437419,
122.967774298082));
#102258=CARTESIAN_POINT('Ctrl Pts',(1.41636288008844,-30.2328873906851,
122.957245732682));
#102259=CARTESIAN_POINT('Ctrl Pts',(1.42022445997104,-30.1618814869173,
122.950401549279));
#102260=CARTESIAN_POINT('Ctrl Pts',(1.42408603985364,-30.0908042270566,
122.947257406578));
#102261=CARTESIAN_POINT('Ctrl Pts',(1.42795437622264,-30.0196026055215,
122.944107762668));
#102262=CARTESIAN_POINT('Ctrl Pts',(1.43182271259164,-29.9483298645522,
122.944671080841));
#102263=CARTESIAN_POINT('Ctrl Pts',(1.43569104896064,-29.8773986990648,
122.948910903079));
#102264=CARTESIAN_POINT('Ctrl Pts',(1.43798874778407,-29.8352672916747,
122.951429255579));
#102265=CARTESIAN_POINT('Ctrl Pts',(1.44028644660749,-29.7932562886806,
122.955243712123));
#102266=CARTESIAN_POINT('Ctrl Pts',(1.44258414543092,-29.7514505019871,
122.960338089404));
#102267=CARTESIAN_POINT('Ctrl Pts',(1.44645321925166,-29.68105412401,122.96891646424));
#102268=CARTESIAN_POINT('Ctrl Pts',(1.45032229307241,-29.6109644877276,
122.981160384507));
#102269=CARTESIAN_POINT('Ctrl Pts',(1.45419136689315,-29.5415930779158,
122.997037030725));
#102270=CARTESIAN_POINT('Ctrl Pts',(1.45805467577709,-29.472325031806,123.012890020672));
#102271=CARTESIAN_POINT('Ctrl Pts',(1.46191798466102,-29.4037735576123,
123.032364884866));
#102272=CARTESIAN_POINT('Ctrl Pts',(1.46578129354496,-29.336343682847,123.05537719462));
#102273=CARTESIAN_POINT('Ctrl Pts',(1.46964007054697,-29.2689929071752,
123.078362509621));
#102274=CARTESIAN_POINT('Ctrl Pts',(1.47349884754898,-29.2027615750243,
123.104876871482));
#102275=CARTESIAN_POINT('Ctrl Pts',(1.47735762455099,-29.1380414908253,
123.134785510736));
#102276=CARTESIAN_POINT('Ctrl Pts',(1.48121397066095,-29.0733621779736,
123.164675308612));
#102277=CARTESIAN_POINT('Ctrl Pts',(1.48507031677091,-29.0101926641901,
123.197954938277));
#102278=CARTESIAN_POINT('Ctrl Pts',(1.48892666288088,-28.9489052530017,
123.234441336196));
#102279=CARTESIAN_POINT('Ctrl Pts',(1.49278186965987,-28.887635948758,123.27091695446));
#102280=CARTESIAN_POINT('Ctrl Pts',(1.49663707643886,-28.8282480603753,
123.310597211726));
#102281=CARTESIAN_POINT('Ctrl Pts',(1.50049228321786,-28.7710881986911,
123.353253708945));
#102282=CARTESIAN_POINT('Ctrl Pts',(1.50434764061392,-28.713926103858,123.395911872688));
#102283=CARTESIAN_POINT('Ctrl Pts',(1.50820299800997,-28.6589925965489,
123.441546214932));
#102284=CARTESIAN_POINT('Ctrl Pts',(1.51205835540603,-28.6066028589048,
123.489886769249));
#102285=CARTESIAN_POINT('Ctrl Pts',(1.51591774843277,-28.5541582818228,
123.538277924485));
#102286=CARTESIAN_POINT('Ctrl Pts',(1.51977714145951,-28.5042631475354,
123.5893806165));
#102287=CARTESIAN_POINT('Ctrl Pts',(1.52363653448625,-28.4571965852293,
123.642887187493));
#102288=CARTESIAN_POINT('Ctrl Pts',(1.52749811265627,-28.410103374385,123.696424053281));
#102289=CARTESIAN_POINT('Ctrl Pts',(1.53135969082629,-28.3658422251813,
123.752367126325));
#102290=CARTESIAN_POINT('Ctrl Pts',(1.53522126899631,-28.324650937252,123.810376916646));
#102291=CARTESIAN_POINT('Ctrl Pts',(1.53908960368497,-28.2833875778295,
123.868488205424));
#102292=CARTESIAN_POINT('Ctrl Pts',(1.54295793837363,-28.2452050638975,
123.928673020778));
#102293=CARTESIAN_POINT('Ctrl Pts',(1.54682627306229,-28.2102965961721,
123.990564866459));
#102294=CARTESIAN_POINT('Ctrl Pts',(1.54912398746468,-28.1895616558131,
124.027327400381));
#102295=CARTESIAN_POINT('Ctrl Pts',(1.55142170186708,-28.1699809474435,
124.064691745944));
#102296=CARTESIAN_POINT('Ctrl Pts',(1.55371941626948,-28.1515868743254,
124.102577870044));
#102297=CARTESIAN_POINT('Ctrl Pts',(1.5579156915312,-28.1179941032189,124.171768629853));
#102298=CARTESIAN_POINT('Ctrl Pts',(1.56211196679293,-28.0882444501088,
124.242941993068));
#102299=CARTESIAN_POINT('Ctrl Pts',(1.56630824205465,-28.0625573661179,
124.315665576698));
#102300=CARTESIAN_POINT('Ctrl Pts',(1.57045672473061,-28.037162839714,124.38756089052));
#102301=CARTESIAN_POINT('Ctrl Pts',(1.57460520740658,-28.0157389964659,
124.460970953742));
#102302=CARTESIAN_POINT('Ctrl Pts',(1.57875369008254,-27.9984520816046,
124.535453454574));
#102303=CARTESIAN_POINT('Ctrl Pts',(1.58297386163715,-27.9808664359451,
124.611223068642));
#102304=CARTESIAN_POINT('Ctrl Pts',(1.58719403319175,-27.9675622691549,
124.688102209931));
#102305=CARTESIAN_POINT('Ctrl Pts',(1.59141420474636,-27.9586631076518,
124.765604491429));
#102306=CARTESIAN_POINT('Ctrl Pts',(1.59563437630097,-27.9497639461487,
124.843106772928));
#102307=CARTESIAN_POINT('Ctrl Pts',(1.59985454785558,-27.9452699483265,
124.921231805876));
#102308=CARTESIAN_POINT('Ctrl Pts',(1.60407471941018,-27.9452500663321,
124.999477896899));
#102309=CARTESIAN_POINT('Ctrl Pts',(1.60407471946233,-27.9452500663318,
124.999477897865));
#102310=CARTESIAN_POINT('Ctrl Pts',(1.60804279144092,-27.9452313720589,
125.073049817208));
#102311=CARTESIAN_POINT('Ctrl Pts',(1.6120108634195,-27.9491684627898,125.1465793535));
#102312=CARTESIAN_POINT('Ctrl Pts',(1.61597893539809,-27.9570216303455,
125.219629104683));
#102313=CARTESIAN_POINT('Ctrl Pts',(1.62005191470725,-27.9650824188439,
125.294610134945));
#102314=CARTESIAN_POINT('Ctrl Pts',(1.62412489401641,-27.9772692208633,
125.369085156028));
#102315=CARTESIAN_POINT('Ctrl Pts',(1.62819787332558,-27.9934830709017,
125.442591658012));
#102316=CARTESIAN_POINT('Ctrl Pts',(1.63217761780573,-28.0093257686653,
125.514415517974));
#102317=CARTESIAN_POINT('Ctrl Pts',(1.63615736228589,-28.0290128981694,
125.585314321825));
#102318=CARTESIAN_POINT('Ctrl Pts',(1.64013710676604,-28.0524017569215,
125.654872999945));
#102319=CARTESIAN_POINT('Ctrl Pts',(1.64425670348971,-28.0766125238101,
125.726876040321));
#102320=CARTESIAN_POINT('Ctrl Pts',(1.64837630021338,-28.1047898157325,
125.797442528993));
#102321=CARTESIAN_POINT('Ctrl Pts',(1.65249589693704,-28.1367223437685,
125.86613736687));
#102322=CARTESIAN_POINT('Ctrl Pts',(1.65661549366071,-28.1686548718044,
125.934832204747));
#102323=CARTESIAN_POINT('Ctrl Pts',(1.66073509038437,-28.2043423228842,
126.00165497065));
#102324=CARTESIAN_POINT('Ctrl Pts',(1.66485468710804,-28.2435236961586,
126.066202868381));
#102325=CARTESIAN_POINT('Ctrl Pts',(1.66872376076535,-28.280322351309,126.126825445661));
#102326=CARTESIAN_POINT('Ctrl Pts',(1.67259283442267,-28.3203352379876,
126.185659440808));
#102327=CARTESIAN_POINT('Ctrl Pts',(1.67646190807999,-28.3633630459669,
126.24234336767));
#102328=CARTESIAN_POINT('Ctrl Pts',(1.68032521678857,-28.40632674219,126.298942835056));
#102329=CARTESIAN_POINT('Ctrl Pts',(1.68418852549714,-28.4522961513903,
126.353398209465));
#102330=CARTESIAN_POINT('Ctrl Pts',(1.68805183420572,-28.5010275887913,
126.405375136017));
#102331=CARTESIAN_POINT('Ctrl Pts',(1.69191061101535,-28.5497018612162,
126.457291090434));
#102332=CARTESIAN_POINT('Ctrl Pts',(1.69576938782498,-28.6011313954007,
126.50673401935));
#102333=CARTESIAN_POINT('Ctrl Pts',(1.69962816463461,-28.6550320733385,
126.553402342844));
#102334=CARTESIAN_POINT('Ctrl Pts',(1.70348451054179,-28.7088987956224,
126.600041266829));
#102335=CARTESIAN_POINT('Ctrl Pts',(1.70734085644897,-28.7652332067255,
126.643908735991));
#102336=CARTESIAN_POINT('Ctrl Pts',(1.71119720235615,-28.8237152051057,
126.684740823925));
#102337=CARTESIAN_POINT('Ctrl Pts',(1.71505240892223,-28.8821799252267,
126.725560848192));
#102338=CARTESIAN_POINT('Ctrl Pts',(1.71890761548831,-28.9427905748845,
126.763346993663));
#102339=CARTESIAN_POINT('Ctrl Pts',(1.72276282205439,-29.0051963142589,
126.79787741221));
#102340=CARTESIAN_POINT('Ctrl Pts',(1.72661817922768,-29.0676044915714,
126.832409179721));
#102341=CARTESIAN_POINT('Ctrl Pts',(1.73047353640098,-29.131807471706,126.863684734528));
#102342=CARTESIAN_POINT('Ctrl Pts',(1.73432889357427,-29.1974294719842,
126.891527982891));
#102343=CARTESIAN_POINT('Ctrl Pts',(1.73818828636462,-29.2631201624646,
126.919400376333));
#102344=CARTESIAN_POINT('Ctrl Pts',(1.74204767915498,-29.3302323901025,
126.943833101187));
#102345=CARTESIAN_POINT('Ctrl Pts',(1.74590707194533,-29.3983708653951,
126.96469843663));
#102346=CARTESIAN_POINT('Ctrl Pts',(1.74976864987091,-29.4665479197571,
126.985575585739));
#102347=CARTESIAN_POINT('Ctrl Pts',(1.75363022779649,-29.5357519069623,
127.002881206717));
#102348=CARTESIAN_POINT('Ctrl Pts',(1.75749180572206,-29.6055755426125,
127.016538348238));
#102349=CARTESIAN_POINT('Ctrl Pts',(1.76136014015612,-29.6755213469706,
127.030219385325));
#102350=CARTESIAN_POINT('Ctrl Pts',(1.76522847459017,-29.7460884832636,
127.040239129489));
#102351=CARTESIAN_POINT('Ctrl Pts',(1.76909680902422,-29.8168634161222,
127.046572391621));
#102352=CARTESIAN_POINT('Ctrl Pts',(1.77139452533168,-29.8589023660013,
127.050334227607));
#102353=CARTESIAN_POINT('Ctrl Pts',(1.77369224163914,-29.9010145865438,
127.052796422883));
#102354=CARTESIAN_POINT('Ctrl Pts',(1.7759899579466,-29.9431138013116,127.053962395688));
#102355=CARTESIAN_POINT('Ctrl Pts',(1.77985822425498,-30.0139889452827,
127.055925341811));
#102356=CARTESIAN_POINT('Ctrl Pts',(1.78372649056337,-30.0851046067981,
127.054219342807));
#102357=CARTESIAN_POINT('Ctrl Pts',(1.78759475687176,-30.156049245216,127.048815803231));
#102358=CARTESIAN_POINT('Ctrl Pts',(1.79145765803492,-30.2268954859906,
127.043419758168));
#102359=CARTESIAN_POINT('Ctrl Pts',(1.79532055919808,-30.2975706942403,
127.034336383239));
#102360=CARTESIAN_POINT('Ctrl Pts',(1.79918346036124,-30.3676619284924,
127.021589045488));
#102361=CARTESIAN_POINT('Ctrl Pts',(1.80304229660246,-30.4376794059011,
127.008855121732));
#102362=CARTESIAN_POINT('Ctrl Pts',(1.80690113284367,-30.5071136534782,
126.992464974016));
#102363=CARTESIAN_POINT('Ctrl Pts',(1.81075996908489,-30.5755571841383,
126.972493723764));
#102364=CARTESIAN_POINT('Ctrl Pts',(1.81461644855471,-30.6439589131398,
126.952534670886));
#102365=CARTESIAN_POINT('Ctrl Pts',(1.81847292802453,-30.711370660064,126.928998989314));
#102366=CARTESIAN_POINT('Ctrl Pts',(1.82232940749435,-30.7773970319467,
126.902012465054));
#102367=CARTESIAN_POINT('Ctrl Pts',(1.826184465167,-30.8433990613924,126.875035890117));
#102368=CARTESIAN_POINT('Ctrl Pts',(1.83003952283965,-30.9080162820449,
126.844611186077));
#102369=CARTESIAN_POINT('Ctrl Pts',(1.83389458051229,-30.9708720641262,
126.810912752619));
#102370=CARTESIAN_POINT('Ctrl Pts',(1.83775080895679,-31.0337469353589,
126.777204085028));
#102371=CARTESIAN_POINT('Ctrl Pts',(1.84160703740129,-31.0948588704673,
126.740219930774));
#102372=CARTESIAN_POINT('Ctrl Pts',(1.84546326584578,-31.1538558705416,
126.700180635261));
#102373=CARTESIAN_POINT('Ctrl Pts',(1.84764813849783,-31.1872825551559,
126.677495059696));
#102374=CARTESIAN_POINT('Ctrl Pts',(1.84983301114987,-31.220030802175,126.653829549317));
#102375=CARTESIAN_POINT('Ctrl Pts',(1.85201788380192,-31.2520409112987,
126.629230222815));
#102376=CARTESIAN_POINT('',(1.54592528048733,-27.9452502737908,125.001060727663));
#102377=CARTESIAN_POINT('Ctrl Pts',(1.54592528053768,-27.9452502737913,
125.001060728586));
#102378=CARTESIAN_POINT('Ctrl Pts',(1.54924811760506,-27.9452817531205,
125.062039704646));
#102379=CARTESIAN_POINT('Ctrl Pts',(1.55257095467244,-27.9480275057199,
125.122946605554));
#102380=CARTESIAN_POINT('Ctrl Pts',(1.55589379173983,-27.9534698466372,
125.183607989687));
#102381=CARTESIAN_POINT('Ctrl Pts',(1.55976286729176,-27.9598068495541,
125.254241449448));
#102382=CARTESIAN_POINT('Ctrl Pts',(1.56363194284369,-27.9698172975719,
125.324684804351));
#102383=CARTESIAN_POINT('Ctrl Pts',(1.56750101839562,-27.9834814636208,
125.394525734191));
#102384=CARTESIAN_POINT('Ctrl Pts',(1.57136432901806,-27.9971252700379,
125.464262600921));
#102385=CARTESIAN_POINT('Ctrl Pts',(1.57522763964051,-28.0144118956924,
125.533398351465));
#102386=CARTESIAN_POINT('Ctrl Pts',(1.57909095026296,-28.0352698251771,
125.601525479627));
#102387=CARTESIAN_POINT('Ctrl Pts',(1.58294972900565,-28.0561032871422,
125.669572690851));
#102388=CARTESIAN_POINT('Ctrl Pts',(1.58680850774834,-28.0804995899692,
125.736613167621));
#102389=CARTESIAN_POINT('Ctrl Pts',(1.59066728649103,-28.108336482699,125.80225102045));
#102390=CARTESIAN_POINT('Ctrl Pts',(1.59452363434205,-28.1361558391885,
125.867847523794));
#102391=CARTESIAN_POINT('Ctrl Pts',(1.59837998219306,-28.167411296179,125.932042710079));
#102392=CARTESIAN_POINT('Ctrl Pts',(1.60223633004407,-28.2019317133454,
125.994458646213));
#102393=CARTESIAN_POINT('Ctrl Pts',(1.60609153856183,-28.2364419316758,
126.056856141957));
#102394=CARTESIAN_POINT('Ctrl Pts',(1.60994674707959,-28.2742149601786,
126.117475006278));
#102395=CARTESIAN_POINT('Ctrl Pts',(1.61380195559734,-28.3150335294589,
126.175961545142));
#102396=CARTESIAN_POINT('Ctrl Pts',(1.61765731472724,-28.3558536934058,
126.23445036891));
#102397=CARTESIAN_POINT('Ctrl Pts',(1.62151267385714,-28.3997193545229,
126.290806304734));
#102398=CARTESIAN_POINT('Ctrl Pts',(1.62536803298704,-28.4463706982994,
126.344705750489));
#102399=CARTESIAN_POINT('Ctrl Pts',(1.62922742772796,-28.4930708745375,
126.398661615682));
#102400=CARTESIAN_POINT('Ctrl Pts',(1.63308682246887,-28.5425622357055,
126.450155489772));
#102401=CARTESIAN_POINT('Ctrl Pts',(1.63694621720978,-28.5945461492713,
126.498898607636));
#102402=CARTESIAN_POINT('Ctrl Pts',(1.64080779708544,-28.6465594953941,
126.547669323163));
#102403=CARTESIAN_POINT('Ctrl Pts',(1.6446693769611,-28.7010678319009,126.593685868565));
#102404=CARTESIAN_POINT('Ctrl Pts',(1.64853095683675,-28.757739396791,126.636699775834));
#102405=CARTESIAN_POINT('Ctrl Pts',(1.65239929319888,-28.8145101181594,
126.679788943202));
#102406=CARTESIAN_POINT('Ctrl Pts',(1.65626762956101,-28.8734512227913,
126.719864710197));
#102407=CARTESIAN_POINT('Ctrl Pts',(1.66013596592313,-28.9342025387947,
126.756722327002));
#102408=CARTESIAN_POINT('Ctrl Pts',(1.66243366480822,-28.9702873613079,
126.778614866097));
#102409=CARTESIAN_POINT('Ctrl Pts',(1.6647313636933,-29.0070103617168,126.799372895577));
#102410=CARTESIAN_POINT('Ctrl Pts',(1.66702906257839,-29.0442925786996,
126.81896148595));
#102411=CARTESIAN_POINT('Ctrl Pts',(1.67089813639869,-29.1070717577412,
126.851946531416));
#102412=CARTESIAN_POINT('Ctrl Pts',(1.67476721021898,-29.1716835652525,
126.881742253025));
#102413=CARTESIAN_POINT('Ctrl Pts',(1.67863628403928,-29.2377708942199,
126.908141596633));
#102414=CARTESIAN_POINT('Ctrl Pts',(1.68249959292275,-29.3037597527794,
126.934501605104));
#102415=CARTESIAN_POINT('Ctrl Pts',(1.68636290180621,-29.3712193213189,
126.95747510202));
#102416=CARTESIAN_POINT('Ctrl Pts',(1.69022621068968,-29.4397684491177,
126.9769011538));
#102417=CARTESIAN_POINT('Ctrl Pts',(1.69408498769117,-29.5082371648743,
126.996304417712));
#102418=CARTESIAN_POINT('Ctrl Pts',(1.69794376469266,-29.5777924360088,
127.012168370542));
#102419=CARTESIAN_POINT('Ctrl Pts',(1.70180254169415,-29.6480353543373,
127.024381004333));
#102420=CARTESIAN_POINT('Ctrl Pts',(1.70565888780357,-29.7182340221292,
127.0365859446));
#102421=CARTESIAN_POINT('Ctrl Pts',(1.70951523391299,-29.7891190001922,
127.045144046375));
#102422=CARTESIAN_POINT('Ctrl Pts',(1.71337158002241,-29.8602799504348,
127.049994114687));
#102423=CARTESIAN_POINT('Ctrl Pts',(1.71722678680084,-29.931419876663,127.054842750079));
#102424=CARTESIAN_POINT('Ctrl Pts',(1.72108199357926,-30.0028351288057,
127.05598549389));
#102425=CARTESIAN_POINT('Ctrl Pts',(1.72493720035769,-30.0741107142985,
127.053413052585));
#102426=CARTESIAN_POINT('Ctrl Pts',(1.72879255775315,-30.1453890844195,
127.050840510778));
#102427=CARTESIAN_POINT('Ctrl Pts',(1.73264791514862,-30.216527291667,127.044552515409));
#102428=CARTESIAN_POINT('Ctrl Pts',(1.73650327254409,-30.2871125500495,
127.034591837717));
#102429=CARTESIAN_POINT('Ctrl Pts',(1.74036266557021,-30.3577716941975,
127.024620733594));
#102430=CARTESIAN_POINT('Ctrl Pts',(1.74422205859634,-30.4278762520515,
127.010969340854));
#102431=CARTESIAN_POINT('Ctrl Pts',(1.74808145162246,-30.4970216521958,
126.993731937786));
#102432=CARTESIAN_POINT('Ctrl Pts',(1.75194302979184,-30.566206201658,126.976484775102));
#102433=CARTESIAN_POINT('Ctrl Pts',(1.75580460796121,-30.6344300475182,
126.955647702241));
#102434=CARTESIAN_POINT('Ctrl Pts',(1.75966618613059,-30.7013045054973,
126.93136468671));
#102435=CARTESIAN_POINT('Ctrl Pts',(1.76353452081859,-30.7682959722487,
126.907039183719));
#102436=CARTESIAN_POINT('Ctrl Pts',(1.76740285550659,-30.833932889824,126.879255889827));
#102437=CARTESIAN_POINT('Ctrl Pts',(1.77127119019459,-30.8978478950008,
126.8482063521));
#102438=CARTESIAN_POINT('Ctrl Pts',(1.77356890460204,-30.9358121457939,
126.829763539899));
#102439=CARTESIAN_POINT('Ctrl Pts',(1.7758666190095,-30.9731693624293,126.810169233763));
#102440=CARTESIAN_POINT('Ctrl Pts',(1.77816433341695,-31.0098473718615,
126.789470829057));
#102441=CARTESIAN_POINT('Ctrl Pts',(1.78203306930039,-31.0716033197561,
126.75462025722));
#102442=CARTESIAN_POINT('Ctrl Pts',(1.78590180518384,-31.1316740256028,
126.716500811245));
#102443=CARTESIAN_POINT('Ctrl Pts',(1.78977054106728,-31.1896919472856,
126.67530016208));
#102444=CARTESIAN_POINT('Ctrl Pts',(1.79117478170446,-31.2107507959034,
126.660345503096));
#102445=CARTESIAN_POINT('Ctrl Pts',(1.79257902234163,-31.2315393936004,
126.644985355848));
#102446=CARTESIAN_POINT('Ctrl Pts',(1.79398326297881,-31.2520409112987,
126.629230222815));
#102447=CARTESIAN_POINT('Ctrl Pts',(1.09386069669771,-31.2520409112987,
126.629230222815));
#102448=CARTESIAN_POINT('Ctrl Pts',(1.09772924491478,-31.3085426350283,
126.585809428947));
#102449=CARTESIAN_POINT('Ctrl Pts',(1.10159779313184,-31.3627072268892,
126.539504236734));
#102450=CARTESIAN_POINT('Ctrl Pts',(1.1054663413489,-31.4142430475397,126.49060865588));
#102451=CARTESIAN_POINT('Ctrl Pts',(1.10742846369447,-31.4403819450334,
126.465808884388));
#102452=CARTESIAN_POINT('Ctrl Pts',(1.10939058604003,-31.4658452042217,
126.440343298387));
#102453=CARTESIAN_POINT('Ctrl Pts',(1.1113527083856,-31.4905987617337,126.414253475873));
#102454=CARTESIAN_POINT('Ctrl Pts',(1.11522172489627,-31.5394091343021,
126.36280818537));
#102455=CARTESIAN_POINT('Ctrl Pts',(1.11909074140694,-31.5856487050198,
126.308732229566));
#102456=CARTESIAN_POINT('Ctrl Pts',(1.12295975791762,-31.6290211273891,
126.25231295171));
#102457=CARTESIAN_POINT('Ctrl Pts',(1.12682300855902,-31.6723289132502,
126.195977753665));
#102458=CARTESIAN_POINT('Ctrl Pts',(1.13068625920042,-31.7127777385068,
126.137306547442));
#102459=CARTESIAN_POINT('Ctrl Pts',(1.13454950984182,-31.7501091015278,
126.076622354983));
#102460=CARTESIAN_POINT('Ctrl Pts',(1.13840822749898,-31.7873966614162,
126.016009366936));
#102461=CARTESIAN_POINT('Ctrl Pts',(1.14226694515614,-31.8215737715933,
125.953388496063));
#102462=CARTESIAN_POINT('Ctrl Pts',(1.1461256628133,-31.8524241841776,125.889113156113));
#102463=CARTESIAN_POINT('Ctrl Pts',(1.14998194893019,-31.8832551566196,
125.824878318758));
#102464=CARTESIAN_POINT('Ctrl Pts',(1.15383823504708,-31.9107633807586,
125.758991517657));
#102465=CARTESIAN_POINT('Ctrl Pts',(1.15769452116397,-31.9347783993041,
125.691830982312));
#102466=CARTESIAN_POINT('Ctrl Pts',(1.16154966739118,-31.9587863191875,
125.624690299124));
#102467=CARTESIAN_POINT('Ctrl Pts',(1.1654048136184,-31.9793029199239,125.556277086349));
#102468=CARTESIAN_POINT('Ctrl Pts',(1.16925995984561,-31.9962064246485,
125.486988164838));
#102469=CARTESIAN_POINT('Ctrl Pts',(1.17311525622009,-32.0131105877178,
125.417696544715));
#102470=CARTESIAN_POINT('Ctrl Pts',(1.17697055259457,-32.026401262396,125.347529620626));
#102471=CARTESIAN_POINT('Ctrl Pts',(1.18082584896905,-32.0360073750409,
125.276896246415));
#102472=CARTESIAN_POINT('Ctrl Pts',(1.18468518067613,-32.0456235423888,
125.206188940364));
#102473=CARTESIAN_POINT('Ctrl Pts',(1.18854451238321,-32.0515473834114,
125.135014691927));
#102474=CARTESIAN_POINT('Ctrl Pts',(1.19240384409029,-32.0537596245863,
125.063788454434));
#102475=CARTESIAN_POINT('Ctrl Pts',(1.19626536067988,-32.0559731181767,
124.99252189365));
#102476=CARTESIAN_POINT('Ctrl Pts',(1.20012687726946,-32.0544708392241,
124.921203771145));
#102477=CARTESIAN_POINT('Ctrl Pts',(1.20398839385904,-32.0492856511186,
124.85024726173));
#102478=CARTESIAN_POINT('Ctrl Pts',(1.20785666722236,-32.044091390116,124.779166594599));
#102479=CARTESIAN_POINT('Ctrl Pts',(1.21172494058567,-32.035201414441,124.708449286005));
#102480=CARTESIAN_POINT('Ctrl Pts',(1.21559321394899,-32.022700171652,124.638500929325));
#102481=CARTESIAN_POINT('Ctrl Pts',(1.21789146904071,-32.0152728152596,
124.596942551259));
#102482=CARTESIAN_POINT('Ctrl Pts',(1.22018972413243,-32.0065716934448,
124.555655383917));
#102483=CARTESIAN_POINT('Ctrl Pts',(1.22248797922415,-31.9966228130601,
124.514721827332));
#102484=CARTESIAN_POINT('Ctrl Pts',(1.22635706752053,-31.9798739774771,
124.445810614958));
#102485=CARTESIAN_POINT('Ctrl Pts',(1.23022615581692,-31.959520558601,124.377632550889));
#102486=CARTESIAN_POINT('Ctrl Pts',(1.23409524411331,-31.9356432554691,
124.310592464462));
#102487=CARTESIAN_POINT('Ctrl Pts',(1.23795856758115,-31.9118015288215,
124.243652265805));
#102488=CARTESIAN_POINT('Ctrl Pts',(1.24182189104898,-31.8844465016466,
124.177847133058));
#102489=CARTESIAN_POINT('Ctrl Pts',(1.24568521451682,-31.8537093734378,
124.113569449235));
#102490=CARTESIAN_POINT('Ctrl Pts',(1.24954400619125,-31.8230083007953,
124.049367165049));
#102491=CARTESIAN_POINT('Ctrl Pts',(1.25340279786567,-31.7889332160827,
123.986689206902));
#102492=CARTESIAN_POINT('Ctrl Pts',(1.2572615895401,-31.7516637685877,123.925908940398));
#102493=CARTESIAN_POINT('Ctrl Pts',(1.26111795036892,-31.7144177989791,
123.865166962419));
#102494=CARTESIAN_POINT('Ctrl Pts',(1.26497431119774,-31.6739817122725,
123.806320717475));
#102495=CARTESIAN_POINT('Ctrl Pts',(1.26883067202656,-31.6305808409948,
123.749718558291));
#102496=CARTESIAN_POINT('Ctrl Pts',(1.27268589354858,-31.5871927918853,
123.693133121408));
#102497=CARTESIAN_POINT('Ctrl Pts',(1.2765411150706,-31.5408419925447,123.63879083937));
#102498=CARTESIAN_POINT('Ctrl Pts',(1.28039633659263,-31.4917957966719,
123.587009248603));
#102499=CARTESIAN_POINT('Ctrl Pts',(1.28425170873368,-31.4427476846212,
123.53522563479));
#102500=CARTESIAN_POINT('Ctrl Pts',(1.28810708087473,-31.3910043026237,
123.486003262045));
#102501=CARTESIAN_POINT('Ctrl Pts',(1.29196245301577,-31.3368706127427,
123.439623594358));
#102502=CARTESIAN_POINT('Ctrl Pts',(1.29582186068773,-31.2826802595433,
123.393195379714));
#102503=CARTESIAN_POINT('Ctrl Pts',(1.29968126835969,-31.2260949735539,
123.349616126688));
#102504=CARTESIAN_POINT('Ctrl Pts',(1.30354067603165,-31.1674529352236,
123.309127087408));
#102505=CARTESIAN_POINT('Ctrl Pts',(1.30740226881264,-31.1087776951022,
123.268615124152));
#102506=CARTESIAN_POINT('Ctrl Pts',(1.31126386159363,-31.04804379829,123.231197112506));
#102507=CARTESIAN_POINT('Ctrl Pts',(1.31512545437463,-30.9856162078359,
123.197069537295));
#102508=CARTESIAN_POINT('Ctrl Pts',(1.31899380346042,-30.9230793930662,
123.162882251929));
#102509=CARTESIAN_POINT('Ctrl Pts',(1.32286215254621,-30.8588434062568,
123.131997107583));
#102510=CARTESIAN_POINT('Ctrl Pts',(1.326730501632,-30.793294818061,123.104563138974));
#102511=CARTESIAN_POINT('Ctrl Pts',(1.32902808444224,-30.7543626260239,
123.088268897348));
#102512=CARTESIAN_POINT('Ctrl Pts',(1.33132566725247,-30.7149677308598,
123.073191186264));
#102513=CARTESIAN_POINT('Ctrl Pts',(1.33362325006271,-30.6751933900766,
123.059352827406));
#102514=CARTESIAN_POINT('Ctrl Pts',(1.33749232926178,-30.608214270153,123.036049333765));
#102515=CARTESIAN_POINT('Ctrl Pts',(1.34136140846086,-30.5398961063051,
123.016171823758));
#102516=CARTESIAN_POINT('Ctrl Pts',(1.34523048765993,-30.470622779717,122.999872063664));
#102517=CARTESIAN_POINT('Ctrl Pts',(1.3490938020638,-30.4014526680079,122.983596589653));
#102518=CARTESIAN_POINT('Ctrl Pts',(1.35295711646766,-30.3313306875089,
122.970888394575));
#102519=CARTESIAN_POINT('Ctrl Pts',(1.35682043087152,-30.2606576524422,
122.961850066672));
#102520=CARTESIAN_POINT('Ctrl Pts',(1.36067921357757,-30.1900675173948,
122.952822340799));
#102521=CARTESIAN_POINT('Ctrl Pts',(1.36453799628361,-30.1189280912524,
122.947455992673));
#102522=CARTESIAN_POINT('Ctrl Pts',(1.36839677898966,-30.0476504883975,
122.945802591411));
#102523=CARTESIAN_POINT('Ctrl Pts',(1.37225313091432,-29.9764177857827,
122.944150231683));
#102524=CARTESIAN_POINT('Ctrl Pts',(1.37610948283898,-29.9050475636516,
122.946206189691));
#102525=CARTESIAN_POINT('Ctrl Pts',(1.37996583476364,-29.8339546989679,
122.951970087986));
#102526=CARTESIAN_POINT('Ctrl Pts',(1.38382104745943,-29.7628828362689,
122.957732283532));
#102527=CARTESIAN_POINT('Ctrl Pts',(1.38767626015522,-29.6920886522836,
122.967200205486));
#102528=CARTESIAN_POINT('Ctrl Pts',(1.39153147285101,-29.6219839246391,
122.980321458927));
#102529=CARTESIAN_POINT('Ctrl Pts',(1.39538683625752,-29.5518764564108,
122.993443225315));
#102530=CARTESIAN_POINT('Ctrl Pts',(1.39924219966403,-29.4824589751218,
123.010218515202));
#102531=CARTESIAN_POINT('Ctrl Pts',(1.40309756307054,-29.4141333497697,
123.030543772853));
#102532=CARTESIAN_POINT('Ctrl Pts',(1.40695696221005,-29.3457362022413,
123.05089030666));
#102533=CARTESIAN_POINT('Ctrl Pts',(1.41081636134956,-29.2784336587827,
123.074794087508));
#102534=CARTESIAN_POINT('Ctrl Pts',(1.41467576048908,-29.2126118210786,
123.102101841986));
#102535=CARTESIAN_POINT('Ctrl Pts',(1.41853734483883,-29.1467527147353,
123.129425058245));
#102536=CARTESIAN_POINT('Ctrl Pts',(1.42239892918858,-29.0823764217114,
123.160155875513));
#102537=CARTESIAN_POINT('Ctrl Pts',(1.42626051353833,-29.0198459585534,
123.194094239021));
#102538=CARTESIAN_POINT('Ctrl Pts',(1.43012885444623,-28.9572060867505,
123.228091983992));
#102539=CARTESIAN_POINT('Ctrl Pts',(1.43399719535414,-28.8964189072815,
123.265308226385));
#102540=CARTESIAN_POINT('Ctrl Pts',(1.43786553626204,-28.8378192908918,
123.305499022757));
#102541=CARTESIAN_POINT('Ctrl Pts',(1.44016319780845,-28.8030131327949,
123.329370974465));
#102542=CARTESIAN_POINT('Ctrl Pts',(1.44246085935486,-28.7689781332935,
123.354291537304));
#102543=CARTESIAN_POINT('Ctrl Pts',(1.44475852090127,-28.7357786282846,
123.380203134403));
#102544=CARTESIAN_POINT('Ctrl Pts',(1.44858235651619,-28.680527040056,123.423325972916));
#102545=CARTESIAN_POINT('Ctrl Pts',(1.45240619213111,-28.6273638365409,
123.46937333891));
#102546=CARTESIAN_POINT('Ctrl Pts',(1.45623002774603,-28.5766205720042,
123.518113173532));
#102547=CARTESIAN_POINT('Ctrl Pts',(1.46004735844195,-28.5259636293858,
123.566770094372));
#102548=CARTESIAN_POINT('Ctrl Pts',(1.46386468913786,-28.4777188079647,
123.61811004743));
#102549=CARTESIAN_POINT('Ctrl Pts',(1.46768201983378,-28.4321857652817,
123.671859914047));
#102550=CARTESIAN_POINT('Ctrl Pts',(1.47149571672727,-28.3866960665198,
123.725558614965));
#102551=CARTESIAN_POINT('Ctrl Pts',(1.47530941362077,-28.3439133504474,
123.781662304536));
#102552=CARTESIAN_POINT('Ctrl Pts',(1.47912311051427,-28.3041004409665,
123.839861108242));
#102553=CARTESIAN_POINT('Ctrl Pts',(1.48293452525575,-28.2643113559042,
123.898025085237));
#102554=CARTESIAN_POINT('Ctrl Pts',(1.48674593999724,-28.227488834142,123.95828127991));
#102555=CARTESIAN_POINT('Ctrl Pts',(1.49055735473872,-28.1938542112394,
124.020288332088));
#102556=CARTESIAN_POINT('Ctrl Pts',(1.49436783584484,-28.1602278273964,
124.082280195162));
#102557=CARTESIAN_POINT('Ctrl Pts',(1.49817831695096,-28.1297880293746,
124.146021626344));
#102558=CARTESIAN_POINT('Ctrl Pts',(1.50198879805707,-28.1027107834153,
124.211145646439));
#102559=CARTESIAN_POINT('Ctrl Pts',(1.50580209425412,-28.0756135334441,
124.276317778579));
#102560=CARTESIAN_POINT('Ctrl Pts',(1.50961539045116,-28.0518839927297,
124.342874080217));
#102561=CARTESIAN_POINT('Ctrl Pts',(1.51342868664821,-28.0316499531354,
124.410427565512));
#102562=CARTESIAN_POINT('Ctrl Pts',(1.51724331848722,-28.0114088263831,
124.478004712035));
#102563=CARTESIAN_POINT('Ctrl Pts',(1.52105795032623,-27.9946657595528,
124.546579253509));
#102564=CARTESIAN_POINT('Ctrl Pts',(1.52487258216524,-27.9814978720417,
124.615751744405));
#102565=CARTESIAN_POINT('Ctrl Pts',(1.52869351667211,-27.9683082280873,
124.685038524504));
#102566=CARTESIAN_POINT('Ctrl Pts',(1.53251445117898,-27.9587056314373,
124.75492473284));
#102567=CARTESIAN_POINT('Ctrl Pts',(1.53633538568585,-27.9527154435004,
124.825004265143));
#102568=CARTESIAN_POINT('Ctrl Pts',(1.53953201728634,-27.9477039930247,
124.883633495009));
#102569=CARTESIAN_POINT('Ctrl Pts',(1.54272864888684,-27.9452199901119,
124.942397808631));
#102570=CARTESIAN_POINT('Ctrl Pts',(1.54592528048734,-27.9452502737908,
125.001060727663));
#102571=CARTESIAN_POINT('Origin',(-1.54592528053767,-30.,125.));
#102572=CARTESIAN_POINT('',(0.39390276451725,-31.2520409112987,126.629230222815));
#102573=CARTESIAN_POINT('',(0.452117106605179,-31.2520409112987,126.629230222815));
#102574=CARTESIAN_POINT('',(-1.54592528053767,-31.2520409112987,126.629230222815));
#102575=CARTESIAN_POINT('',(0.145925136774057,-27.9455707835906,124.9977750384));
#102576=CARTESIAN_POINT('Ctrl Pts',(0.145925280537678,-27.9452512021367,
124.997777348617));
#102577=CARTESIAN_POINT('Ctrl Pts',(0.149742855972762,-27.945174835179,
125.068375426051));
#102578=CARTESIAN_POINT('Ctrl Pts',(0.153560431407846,-27.948741212299,
125.13903804764));
#102579=CARTESIAN_POINT('Ctrl Pts',(0.15737800684293,-27.955943445049,125.209357022003));
#102580=CARTESIAN_POINT('Ctrl Pts',(0.161194301449952,-27.9631432613905,
125.27965240377));
#102581=CARTESIAN_POINT('Ctrl Pts',(0.165010596056974,-27.9739764629279,
125.349603873899));
#102582=CARTESIAN_POINT('Ctrl Pts',(0.168826890663996,-27.9883842021359,
125.418807168377));
#102583=CARTESIAN_POINT('Ctrl Pts',(0.17264324173275,-28.0027921545051,
125.48801148671));
#102584=CARTESIAN_POINT('Ctrl Pts',(0.176459592801504,-28.0207746461243,
125.556467122227));
#102585=CARTESIAN_POINT('Ctrl Pts',(0.180275943870259,-28.0422218624211,
125.623780671806));
#102586=CARTESIAN_POINT('Ctrl Pts',(0.184096399549484,-28.063692145901,
125.69116661931));
#102587=CARTESIAN_POINT('Ctrl Pts',(0.187916855228711,-28.0886344413074,
125.757407555328));
#102588=CARTESIAN_POINT('Ctrl Pts',(0.191737310907937,-28.1168895501514,
125.822126873524));
#102589=CARTESIAN_POINT('Ctrl Pts',(0.195559946017952,-28.1451607775057,
125.886883111735));
#102590=CARTESIAN_POINT('Ctrl Pts',(0.199382581127968,-28.1767483553683,
125.9501155618));
#102591=CARTESIAN_POINT('Ctrl Pts',(0.203205216237984,-28.2114468676046,
126.011471826152));
#102592=CARTESIAN_POINT('Ctrl Pts',(0.207034920453413,-28.2462095469491,
126.072941555139));
#102593=CARTESIAN_POINT('Ctrl Pts',(0.210864624668841,-28.2840943777579,
126.132527754396));
#102594=CARTESIAN_POINT('Ctrl Pts',(0.214694328884269,-28.3248527725902,
126.189907277481));
#102595=CARTESIAN_POINT('Ctrl Pts',(0.217219733148553,-28.3517298937267,
126.227744792894));
#102596=CARTESIAN_POINT('Ctrl Pts',(0.219745137412836,-28.3798557023373,
126.264623409239));
#102597=CARTESIAN_POINT('Ctrl Pts',(0.22227054167712,-28.4091499875841,
126.30045907298));
#102598=CARTESIAN_POINT('Ctrl Pts',(0.226141673197727,-28.4540544936058,
126.355390700931));
#102599=CARTESIAN_POINT('Ctrl Pts',(0.230012804718335,-28.5018955096994,
126.40810145461));
#102600=CARTESIAN_POINT('Ctrl Pts',(0.233883936238942,-28.5524251572329,
126.458260826151));
#102601=CARTESIAN_POINT('Ctrl Pts',(0.237749257978822,-28.602878970047,
126.508344918682));
#102602=CARTESIAN_POINT('Ctrl Pts',(0.241614579718701,-28.6560130630199,
126.555884890918));
#102603=CARTESIAN_POINT('Ctrl Pts',(0.245479901458581,-28.7115393876318,
126.600583272709));
#102604=CARTESIAN_POINT('Ctrl Pts',(0.249340613883586,-28.7669994982696,
126.64522835262));
#102605=CARTESIAN_POINT('Ctrl Pts',(0.25320132630859,-28.8248457976965,
126.687038270525));
#102606=CARTESIAN_POINT('Ctrl Pts',(0.257062038733595,-28.8847547571072,
126.725753635576));
#102607=CARTESIAN_POINT('Ctrl Pts',(0.260920271211504,-28.9446252337112,
126.764444131627));
#102608=CARTESIAN_POINT('Ctrl Pts',(0.264778503689414,-29.0065553349753,
126.800043756038));
#102609=CARTESIAN_POINT('Ctrl Pts',(0.268636736167323,-29.0701911223101,
126.832335398738));
#102610=CARTESIAN_POINT('Ctrl Pts',(0.272493777200255,-29.1338072585379,
126.864617069588));
#102611=CARTESIAN_POINT('Ctrl Pts',(0.276350818233187,-29.1991276026886,
126.893592567357));
#102612=CARTESIAN_POINT('Ctrl Pts',(0.280207859266119,-29.2657736075305,
126.91909071362));
#102613=CARTESIAN_POINT('Ctrl Pts',(0.284064995690883,-29.3324212606527,
126.944589490499));
#102614=CARTESIAN_POINT('Ctrl Pts',(0.287922132115646,-29.4003941856134,
126.966610573799));
#102615=CARTESIAN_POINT('Ctrl Pts',(0.291779268540409,-29.4692954678159,
126.985031551895));
#102616=CARTESIAN_POINT('Ctrl Pts',(0.295640343039968,-29.538267097129,
127.003471337517));
#102617=CARTESIAN_POINT('Ctrl Pts',(0.299501417539527,-29.6081685061665,
127.018303554646));
#102618=CARTESIAN_POINT('Ctrl Pts',(0.303362492039085,-29.6785901633433,
127.029456399975));
#102619=CARTESIAN_POINT('Ctrl Pts',(0.307225699100924,-29.7490507160582,
127.040615405283));
#102620=CARTESIAN_POINT('Ctrl Pts',(0.311088906162763,-29.8200316062018,
127.048090941898));
#102621=CARTESIAN_POINT('Ctrl Pts',(0.314952113224602,-29.8911184336103,
127.05186314529));
#102622=CARTESIAN_POINT('Ctrl Pts',(0.318821975145273,-29.9623277169973,
127.055641846777));
#102623=CARTESIAN_POINT('Ctrl Pts',(0.322691837065945,-30.0336428166044,
127.055704477394));
#102624=CARTESIAN_POINT('Ctrl Pts',(0.326561698986616,-30.1046502956107,
127.052083301947));
#102625=CARTESIAN_POINT('Ctrl Pts',(0.328843070162972,-30.1465108113685,
127.049948537074));
#102626=CARTESIAN_POINT('Ctrl Pts',(0.331124441339327,-30.1882645132298,
127.046534501362));
#102627=CARTESIAN_POINT('Ctrl Pts',(0.333405812515682,-30.2298282324623,
127.041856152148));
#102628=CARTESIAN_POINT('Ctrl Pts',(0.337280820021117,-30.3004260052618,
127.033909773887));
#102629=CARTESIAN_POINT('Ctrl Pts',(0.341155827526552,-30.370744503116,
127.022282695611));
#102630=CARTESIAN_POINT('Ctrl Pts',(0.345030835031987,-30.4403708785773,
127.007005493715));
#102631=CARTESIAN_POINT('Ctrl Pts',(0.349103495822425,-30.5135487005361,
126.990949044517));
#102632=CARTESIAN_POINT('Ctrl Pts',(0.353176156612864,-30.5859613704907,
126.970860133849));
#102633=CARTESIAN_POINT('Ctrl Pts',(0.357248817403303,-30.6571349812852,
126.946836197237));
#102634=CARTESIAN_POINT('Ctrl Pts',(0.361113777721505,-30.7246788292949,
126.924037450552));
#102635=CARTESIAN_POINT('Ctrl Pts',(0.364978738039707,-30.7911063722484,
126.897695373647));
#102636=CARTESIAN_POINT('Ctrl Pts',(0.368843698357909,-30.8560246926624,
126.867945204778));
#102637=CARTESIAN_POINT('Ctrl Pts',(0.372706164963254,-30.9209011270965,
126.838214231029));
#102638=CARTESIAN_POINT('Ctrl Pts',(0.376568631568599,-30.9842698337519,
126.805079733099));
#102639=CARTESIAN_POINT('Ctrl Pts',(0.380431098173944,-31.0457575024229,
126.768725193077));
#102640=CARTESIAN_POINT('Ctrl Pts',(0.384292618222436,-31.1072301025949,
126.732379562295));
#102641=CARTESIAN_POINT('Ctrl Pts',(0.388154138270928,-31.1668221635663,
126.692815701947));
#102642=CARTESIAN_POINT('Ctrl Pts',(0.392015658319421,-31.2241860666473,
126.650262414505));
#102643=CARTESIAN_POINT('Ctrl Pts',(0.392644693718697,-31.2335305541096,
126.643330552486));
#102644=CARTESIAN_POINT('Ctrl Pts',(0.393273729117974,-31.2428159780343,
126.636319456546));
#102645=CARTESIAN_POINT('Ctrl Pts',(0.393902764517251,-31.2520409112987,
126.629230222815));
#102646=CARTESIAN_POINT('',(0.,-29.4698297828114,123.014825674328));
#102647=CARTESIAN_POINT('Ctrl Pts',(-2.77555756156289E-16,-29.4698297828114,
123.014825674328));
#102648=CARTESIAN_POINT('Ctrl Pts',(0.0370450902795195,-28.8097276504723,
123.191115729233));
#102649=CARTESIAN_POINT('Ctrl Pts',(0.0856865378424994,-28.0750900177817,
123.887375885199));
#102650=CARTESIAN_POINT('Ctrl Pts',(0.134327985405479,-27.9457241577746,
124.783527527238));
#102651=CARTESIAN_POINT('Ctrl Pts',(0.145924342688939,-27.9473360067712,
124.997762277807));
#102652=CARTESIAN_POINT('',(7.76923664291829E-9,-30.530363345704,123.014877262224));
#102653=CARTESIAN_POINT('Origin',(0.,-30.,125.));
#102654=CARTESIAN_POINT('',(0.20407471941795,-27.945250548143,125.001500864184));
#102655=CARTESIAN_POINT('Ctrl Pts',(7.76923658740714E-9,-30.530363345704,
123.014877262224));
#102656=CARTESIAN_POINT('Ctrl Pts',(0.00385760787619837,-30.4620546494468,
122.996627293092));
#102657=CARTESIAN_POINT('Ctrl Pts',(0.00771520798316006,-30.3926645715971,
122.981870325238));
#102658=CARTESIAN_POINT('Ctrl Pts',(0.0115728080901218,-30.3225847520692,
122.970730022833));
#102659=CARTESIAN_POINT('Ctrl Pts',(0.0154246241661233,-30.25261000923,
122.959606424039));
#102660=CARTESIAN_POINT('Ctrl Pts',(0.0192764402421246,-30.1819480560963,
122.952088804636));
#102661=CARTESIAN_POINT('Ctrl Pts',(0.0231282563181261,-30.1110039601888,
122.948250579792));
#102662=CARTESIAN_POINT('Ctrl Pts',(0.0269755322799582,-30.0401434856922,
122.944416879043));
#102663=CARTESIAN_POINT('Ctrl Pts',(0.0308228082417903,-29.9690020148071,
122.944253985825));
#102664=CARTESIAN_POINT('Ctrl Pts',(0.0346700842036225,-29.8979912511057,
122.947783691311));
#102665=CARTESIAN_POINT('Ctrl Pts',(0.0385149443694312,-29.8270250767507,
122.951311180411));
#102666=CARTESIAN_POINT('Ctrl Pts',(0.0423598045352404,-29.7561899340426,
122.958526644498));
#102667=CARTESIAN_POINT('Ctrl Pts',(0.046204664701049,-29.6858975330341,
122.969399792488));
#102668=CARTESIAN_POINT('Ctrl Pts',(0.0500484171687816,-29.6156253831542,
122.980269807942));
#102669=CARTESIAN_POINT('Ctrl Pts',(0.0538921696365139,-29.5458961475966,
122.99479534066));
#102670=CARTESIAN_POINT('Ctrl Pts',(0.0577359221042466,-29.4771146500438,
123.012894448374));
#102671=CARTESIAN_POINT('Ctrl Pts',(0.0615798733729778,-29.4083295950741,
123.030994492184));
#102672=CARTESIAN_POINT('Ctrl Pts',(0.0654238246417088,-29.3404928476682,
123.052668350937));
#102673=CARTESIAN_POINT('Ctrl Pts',(0.0692677759104399,-29.2739955743463,
123.077783795607));
#102674=CARTESIAN_POINT('Ctrl Pts',(0.0731156987411403,-29.2074295961883,
123.102925189499));
#102675=CARTESIAN_POINT('Ctrl Pts',(0.0769636215718412,-29.1422063121485,
123.131515092081));
#102676=CARTESIAN_POINT('Ctrl Pts',(0.0808115444025417,-29.0786974170051,
123.163372897655));
#102677=CARTESIAN_POINT('Ctrl Pts',(0.0846617298495252,-29.0151511780099,
123.195249435931));
#102678=CARTESIAN_POINT('Ctrl Pts',(0.0885119152965084,-28.9533217589085,
123.23039745915));
#102679=CARTESIAN_POINT('Ctrl Pts',(0.0923621007434918,-28.8935543097556,
123.268591470207));
#102680=CARTESIAN_POINT('Ctrl Pts',(0.0962187336365197,-28.833686775189,
123.306849440216));
#102681=CARTESIAN_POINT('Ctrl Pts',(0.100075366529548,-28.7758884983343,
123.348163292566));
#102682=CARTESIAN_POINT('Ctrl Pts',(0.103931999422576,-28.7204731275101,
123.39226602167));
#102683=CARTESIAN_POINT('Ctrl Pts',(0.105608298071121,-28.6963866474645,
123.411435423386));
#102684=CARTESIAN_POINT('Ctrl Pts',(0.107284596719665,-28.6727498971189,
123.431131223205));
#102685=CARTESIAN_POINT('Ctrl Pts',(0.10896089536821,-28.6495864180097,
123.451329370048));
#102686=CARTESIAN_POINT('Ctrl Pts',(0.112923971370282,-28.5948237250601,
123.499081476219));
#102687=CARTESIAN_POINT('Ctrl Pts',(0.116887047372355,-28.5424737288281,
123.549849695004));
#102688=CARTESIAN_POINT('Ctrl Pts',(0.120850123374427,-28.4928909201467,
123.603354095011));
#102689=CARTESIAN_POINT('Ctrl Pts',(0.12466130497301,-28.4452084916609,
123.654807810418));
#102690=CARTESIAN_POINT('Ctrl Pts',(0.128472486571594,-28.4000854002298,
123.708791396722));
#102691=CARTESIAN_POINT('Ctrl Pts',(0.132283668170177,-28.3578035821471,
123.7650147824));
#102692=CARTESIAN_POINT('Ctrl Pts',(0.136091357608174,-28.3155605066157,
123.82118665096));
#102693=CARTESIAN_POINT('Ctrl Pts',(0.139899047046172,-28.2761538430259,
123.879593853435));
#102694=CARTESIAN_POINT('Ctrl Pts',(0.143706736484169,-28.2398264892347,
123.939911902482));
#102695=CARTESIAN_POINT('Ctrl Pts',(0.147512291348494,-28.2035195003957,
124.000196137499));
#102696=CARTESIAN_POINT('Ctrl Pts',(0.151317846212819,-28.1702886550489,
124.062388667107));
#102697=CARTESIAN_POINT('Ctrl Pts',(0.155123401077145,-28.1403334844351,
124.126136158554));
#102698=CARTESIAN_POINT('Ctrl Pts',(0.158928175891731,-28.1103844539307,
124.189870583256));
#102699=CARTESIAN_POINT('Ctrl Pts',(0.162732950706317,-28.0837099762376,
124.255158884088));
#102700=CARTESIAN_POINT('Ctrl Pts',(0.166537725520903,-28.0604627032384,
124.321625002693));
#102701=CARTESIAN_POINT('Ctrl Pts',(0.170344988314308,-28.037200228624,
124.388134584133));
#102702=CARTESIAN_POINT('Ctrl Pts',(0.174152251107713,-28.0173695981176,
124.455823048431));
#102703=CARTESIAN_POINT('Ctrl Pts',(0.177959513901117,-28.001074099642,
124.524297564251));
#102704=CARTESIAN_POINT('Ctrl Pts',(0.181768282834312,-27.9847721547245,
124.592799168348));
#102705=CARTESIAN_POINT('Ctrl Pts',(0.185577051767507,-27.9720082170426,
124.662086951351));
#102706=CARTESIAN_POINT('Ctrl Pts',(0.189385820700702,-27.9628342584875,
124.731758869471));
#102707=CARTESIAN_POINT('Ctrl Pts',(0.193199633430934,-27.9536481512339,
124.801523051264));
#102708=CARTESIAN_POINT('Ctrl Pts',(0.197013446161167,-27.9480615453774,
124.871671885187));
#102709=CARTESIAN_POINT('Ctrl Pts',(0.200827258891399,-27.9460743989428,
124.941800448267));
#102710=CARTESIAN_POINT('Ctrl Pts',(0.201909745733583,-27.9455103807225,
124.961705265877));
#102711=CARTESIAN_POINT('Ctrl Pts',(0.202992232575767,-27.9452360180092,
124.981608468297));
#102712=CARTESIAN_POINT('Ctrl Pts',(0.20407471941795,-27.945250548143,125.001500864184));
#102713=CARTESIAN_POINT('Ctrl Pts',(0.204074719462324,-27.9452505481436,
125.001500864999));
#102714=CARTESIAN_POINT('Ctrl Pts',(0.209415201710473,-27.9453222330462,
125.099640614109));
#102715=CARTESIAN_POINT('Ctrl Pts',(0.214755683958622,-27.9524256421758,
125.197525919788));
#102716=CARTESIAN_POINT('Ctrl Pts',(0.220096166206771,-27.9664486897963,
125.294391968757));
#102717=CARTESIAN_POINT('Ctrl Pts',(0.223961505846526,-27.9765983053776,
125.364501775592));
#102718=CARTESIAN_POINT('Ctrl Pts',(0.227826845486281,-27.9903981515537,
125.434225968574));
#102719=CARTESIAN_POINT('Ctrl Pts',(0.231692185126037,-28.0078069756633,
125.503154565004));
#102720=CARTESIAN_POINT('Ctrl Pts',(0.235551705855852,-28.0251895924046,
125.571979395832));
#102721=CARTESIAN_POINT('Ctrl Pts',(0.239411226585667,-28.0461702853158,
125.640010539238));
#102722=CARTESIAN_POINT('Ctrl Pts',(0.243270747315482,-28.0706563372835,
125.706845523177));
#102723=CARTESIAN_POINT('Ctrl Pts',(0.247125674239539,-28.0951132446568,
125.773600956583));
#102724=CARTESIAN_POINT('Ctrl Pts',(0.250980601163595,-28.1230670573192,
125.83916260352));
#102725=CARTESIAN_POINT('Ctrl Pts',(0.254835528087652,-28.1543750051239,
125.903142259441));
#102726=CARTESIAN_POINT('Ctrl Pts',(0.25868798791371,-28.1856629162906,
125.967080969299));
#102727=CARTESIAN_POINT('Ctrl Pts',(0.262540447739768,-28.2203004906343,
126.029439260421));
#102728=CARTESIAN_POINT('Ctrl Pts',(0.266392907565826,-28.258097084805,
126.089849437553));
#102729=CARTESIAN_POINT('Ctrl Pts',(0.270244197575565,-28.2958822018742,
126.150241270871));
#102730=CARTESIAN_POINT('Ctrl Pts',(0.274095487585303,-28.3368241764601,
126.208685751987));
#102731=CARTESIAN_POINT('Ctrl Pts',(0.277946777595041,-28.3806875867483,
126.264841836274));
#102732=CARTESIAN_POINT('Ctrl Pts',(0.281798193422183,-28.4245524300058,
126.320999755118));
#102733=CARTESIAN_POINT('Ctrl Pts',(0.285649609249325,-28.4713385969919,
126.374868746374));
#102734=CARTESIAN_POINT('Ctrl Pts',(0.289501025076467,-28.5207697854712,
126.426140082504));
#102735=CARTESIAN_POINT('Ctrl Pts',(0.293356465647466,-28.5702526297261,
126.477464997371));
#102736=CARTESIAN_POINT('Ctrl Pts',(0.297211906218466,-28.6223856745522,
126.526186486988));
#102737=CARTESIAN_POINT('Ctrl Pts',(0.301067346789465,-28.6768557205867,
126.572032689977));
#102738=CARTESIAN_POINT('Ctrl Pts',(0.304924960312611,-28.7313564663043,
126.617904732193));
#102739=CARTESIAN_POINT('Ctrl Pts',(0.308782573835757,-28.7881964466043,
126.660897968169));
#102740=CARTESIAN_POINT('Ctrl Pts',(0.312640187358902,-28.8470315508531,
126.700782560403));
#102741=CARTESIAN_POINT('Ctrl Pts',(0.316504581130456,-28.9059700653112,
126.740737254902));
#102742=CARTESIAN_POINT('Ctrl Pts',(0.320368974902009,-28.9669102880165,
126.777572145162));
#102743=CARTESIAN_POINT('Ctrl Pts',(0.324233368673562,-29.0294820987998,
126.811102582945));
#102744=CARTESIAN_POINT('Ctrl Pts',(0.326566058130818,-29.0672527329443,
126.831342781884));
#102745=CARTESIAN_POINT('Ctrl Pts',(0.328898747588075,-29.1056174416194,
126.850379828498));
#102746=CARTESIAN_POINT('Ctrl Pts',(0.331231437045331,-29.1444916043112,
126.868181722265));
#102747=CARTESIAN_POINT('Ctrl Pts',(0.335101017067839,-29.2089779777015,
126.897712379366));
#102748=CARTESIAN_POINT('Ctrl Pts',(0.338970597090347,-29.275121315827,
126.923957950765));
#102749=CARTESIAN_POINT('Ctrl Pts',(0.342840177112856,-29.3425536894351,
126.946731083438));
#102750=CARTESIAN_POINT('Ctrl Pts',(0.346703991075797,-29.4098855820916,
126.969470281876));
#102751=CARTESIAN_POINT('Ctrl Pts',(0.350567805038738,-29.4785022411153,
126.988747158347));
#102752=CARTESIAN_POINT('Ctrl Pts',(0.354431619001679,-29.5480142396889,
127.00442172084));
#102753=CARTESIAN_POINT('Ctrl Pts',(0.358290896853122,-29.6174446312858,
127.020077881422));
#102754=CARTESIAN_POINT('Ctrl Pts',(0.362150174704567,-29.6877678030683,
127.032140022251));
#102755=CARTESIAN_POINT('Ctrl Pts',(0.36600945255601,-29.7585792591669,
127.040517970613));
#102756=CARTESIAN_POINT('Ctrl Pts',(0.369866296612965,-29.8293460591048,
127.048890635551));
#102757=CARTESIAN_POINT('Ctrl Pts',(0.37372314066992,-29.9006000512908,
127.053583660692));
#102758=CARTESIAN_POINT('Ctrl Pts',(0.377579984726875,-29.9719280890738,
127.054558232399));
#102759=CARTESIAN_POINT('Ctrl Pts',(0.38143568578439,-30.0432349883545,
127.055532515285));
#102760=CARTESIAN_POINT('Ctrl Pts',(0.385291386841906,-30.1146154043383,
127.052790525874));
#102761=CARTESIAN_POINT('Ctrl Pts',(0.389147087899421,-30.1856543622022,
127.046345528081));
#102762=CARTESIAN_POINT('Ctrl Pts',(0.393002935136099,-30.2566960133287,
127.039900285941));
#102763=CARTESIAN_POINT('Ctrl Pts',(0.396858782372778,-30.3273956971792,
127.029751802762));
#102764=CARTESIAN_POINT('Ctrl Pts',(0.400714629609457,-30.397343468581,
127.015965210631));
#102765=CARTESIAN_POINT('Ctrl Pts',(0.404574502226595,-30.4673642632056,
127.002164225742));
#102766=CARTESIAN_POINT('Ctrl Pts',(0.408434374843733,-30.5366311009456,
126.984717644176));
#102767=CARTESIAN_POINT('Ctrl Pts',(0.412294247460872,-30.6047450347016,
126.963741583178));
#102768=CARTESIAN_POINT('Ctrl Pts',(0.416156300156607,-30.6728974396053,
126.942753674779));
#102769=CARTESIAN_POINT('Ctrl Pts',(0.420018352852343,-30.7398951879513,
126.918232485479));
#102770=CARTESIAN_POINT('Ctrl Pts',(0.423880405548079,-30.8053578897072,
126.890342887411));
#102771=CARTESIAN_POINT('Ctrl Pts',(0.427749201512576,-30.870934891455,
126.862404593204));
#102772=CARTESIAN_POINT('Ctrl Pts',(0.431617997477072,-30.9349710590033,
126.831086361316));
#102773=CARTESIAN_POINT('Ctrl Pts',(0.435486793441568,-30.9971098712046,
126.796599417579));
#102774=CARTESIAN_POINT('Ctrl Pts',(0.437780098255676,-31.0339438729126,
126.776156604151));
#102775=CARTESIAN_POINT('Ctrl Pts',(0.440073403069785,-31.0701117139769,
126.75460123076));
#102776=CARTESIAN_POINT('Ctrl Pts',(0.442366707883893,-31.1055442987138,
126.731984228012));
#102777=CARTESIAN_POINT('Ctrl Pts',(0.445616840790988,-31.1557603052944,
126.699930806923));
#102778=CARTESIAN_POINT('Ctrl Pts',(0.448866973698083,-31.204663376369,
126.665639203681));
#102779=CARTESIAN_POINT('Ctrl Pts',(0.452117106605179,-31.2520409112987,
126.629230222815));
#102780=CARTESIAN_POINT('Origin',(5.,30.,55.));
#102781=CARTESIAN_POINT('',(9.56912139758663,31.5634376777551,55.575515966569));
#102782=CARTESIAN_POINT('',(9.76070772053754,31.5634376782623,55.5755159651912));
#102783=CARTESIAN_POINT('',(5.,31.5634376782623,55.5755159651912));
#102784=CARTESIAN_POINT('',(10.,28.6653082844465,55.9970727277551));
#102785=CARTESIAN_POINT('Ctrl Pts',(9.76070772053754,31.5634376782623,55.5755159651912));
#102786=CARTESIAN_POINT('Ctrl Pts',(9.76500822046156,31.5412735069596,55.6357268066236));
#102787=CARTESIAN_POINT('Ctrl Pts',(9.76930872038559,31.5156588479085,55.6945694832879));
#102788=CARTESIAN_POINT('Ctrl Pts',(9.77360922030962,31.4867958201399,55.7516609536318));
#102789=CARTESIAN_POINT('Ctrl Pts',(9.7749826329807,31.4775780899309,55.7698937521823));
#102790=CARTESIAN_POINT('Ctrl Pts',(9.77635604565179,31.4680293913545,55.7879481540697));
#102791=CARTESIAN_POINT('Ctrl Pts',(9.77772945832288,31.4581572365982,55.8058123065306));
#102792=CARTESIAN_POINT('Ctrl Pts',(9.78176791912768,31.4291285907429,55.8583410774113));
#102793=CARTESIAN_POINT('Ctrl Pts',(9.78580637993247,31.3971912918331,55.9094193856562));
#102794=CARTESIAN_POINT('Ctrl Pts',(9.78984484073727,31.3625153003126,55.9587012341778));
#102795=CARTESIAN_POINT('Ctrl Pts',(9.79397066942161,31.3270891299501,56.0090492439953));
#102796=CARTESIAN_POINT('Ctrl Pts',(9.79809649810595,31.2888045450285,56.0575216187083));
#102797=CARTESIAN_POINT('Ctrl Pts',(9.80222232679029,31.2478929598246,56.1037749593193));
#102798=CARTESIAN_POINT('Ctrl Pts',(9.80624967600004,31.2079578939394,56.1489242781614));
#102799=CARTESIAN_POINT('Ctrl Pts',(9.81027702520978,31.1655202145113,56.1919589071941));
#102800=CARTESIAN_POINT('Ctrl Pts',(9.81430437441952,31.1208378861853,56.2325901317517));
#102801=CARTESIAN_POINT('Ctrl Pts',(9.81832937588719,31.0761816054098,56.2731976703486));
#102802=CARTESIAN_POINT('Ctrl Pts',(9.82235437735485,31.0292836539648,56.3114042292453));
#102803=CARTESIAN_POINT('Ctrl Pts',(9.82637937882252,30.9804387670977,56.346957988941));
#102804=CARTESIAN_POINT('Ctrl Pts',(9.83040359871507,30.9316033649346,56.3825048448048));
#102805=CARTESIAN_POINT('Ctrl Pts',(9.83442781860763,30.8808221998901,56.4153996160489));
#102806=CARTESIAN_POINT('Ctrl Pts',(9.83845203850019,30.8284212102314,56.4454322185557));
#102807=CARTESIAN_POINT('Ctrl Pts',(9.8426530960553,30.7737175460733,56.4767845539223));
#102808=CARTESIAN_POINT('Ctrl Pts',(9.8468541536104,30.717248904141,56.505016989362));
#102809=CARTESIAN_POINT('Ctrl Pts',(9.85105521116551,30.6594148160633,56.5299438226145));
#102810=CARTESIAN_POINT('Ctrl Pts',(9.85508552229091,30.6039313180275,56.5538575376876));
#102811=CARTESIAN_POINT('Ctrl Pts',(9.85911583341631,30.5471917684168,56.574729072882));
#102812=CARTESIAN_POINT('Ctrl Pts',(9.86314614454171,30.4895667884119,56.5924447744534));
#102813=CARTESIAN_POINT('Ctrl Pts',(9.86717971472583,30.4318952107157,56.6101748015968));
#102814=CARTESIAN_POINT('Ctrl Pts',(9.87121328490995,30.3733372865983,56.62474380153));
#102815=CARTESIAN_POINT('Ctrl Pts',(9.87524685509407,30.3142743232612,56.6360891325777));
#102816=CARTESIAN_POINT('Ctrl Pts',(9.87928790344763,30.2551018582104,56.6474554976731));
#102817=CARTESIAN_POINT('Ctrl Pts',(9.8833289518012,30.1954230035822,56.6555862179572));
#102818=CARTESIAN_POINT('Ctrl Pts',(9.88737000015477,30.1356231791982,56.6604705216487));
#102819=CARTESIAN_POINT('Ctrl Pts',(9.88786824315699,30.1282501310614,56.6610727342237));
#102820=CARTESIAN_POINT('Ctrl Pts',(9.88836648615922,30.1208752406347,56.6616256604532));
#102821=CARTESIAN_POINT('Ctrl Pts',(9.88886472916144,30.1134992263197,56.6621293348067));
#102822=CARTESIAN_POINT('Ctrl Pts',(9.89305224182562,30.0515070794814,56.6663624955822));
#102823=CARTESIAN_POINT('Ctrl Pts',(9.89723975448979,29.9891721256139,56.6671303991492));
#102824=CARTESIAN_POINT('Ctrl Pts',(9.90142726715397,29.9269022972419,56.6643956037708));
#102825=CARTESIAN_POINT('Ctrl Pts',(9.90560583628048,29.8647654625107,56.6616666492691));
#102826=CARTESIAN_POINT('Ctrl Pts',(9.90978440540699,29.8026939512104,56.6554498951321));
#102827=CARTESIAN_POINT('Ctrl Pts',(9.91396297453351,29.7410974011908,56.6457598379866));
#102828=CARTESIAN_POINT('Ctrl Pts',(9.91813627185461,29.679578563186,56.6360820061016));
#102829=CARTESIAN_POINT('Ctrl Pts',(9.92230956917571,29.6185339664344,56.622939646519));
#102830=CARTESIAN_POINT('Ctrl Pts',(9.92648286649681,29.5583688605115,56.606399058962));
#102831=CARTESIAN_POINT('Ctrl Pts',(9.93065213828524,29.4982617894182,56.5898744263372));
#102832=CARTESIAN_POINT('Ctrl Pts',(9.93482141007368,29.4390329837869,56.56995820315));
#102833=CARTESIAN_POINT('Ctrl Pts',(9.93899068186211,29.3810765727086,56.5467675297697));
#102834=CARTESIAN_POINT('Ctrl Pts',(9.94315716884789,29.3231588727472,56.5235923462524));
#102835=CARTESIAN_POINT('Ctrl Pts',(9.94732365583366,29.2665123218583,56.497147236304));
#102836=CARTESIAN_POINT('Ctrl Pts',(9.95149014281944,29.2115133833492,56.4675983290269));
#102837=CARTESIAN_POINT('Ctrl Pts',(9.95565639117634,29.1565175948163,56.4380511141162));
#102838=CARTESIAN_POINT('Ctrl Pts',(9.95982263953323,29.1031696592298,56.4054006693019));
#102839=CARTESIAN_POINT('Ctrl Pts',(9.96398888789013,29.0518224621395,56.3698596120394));
#102840=CARTESIAN_POINT('Ctrl Pts',(9.96815464396323,29.0004813322328,56.3343227543074));
#102841=CARTESIAN_POINT('Ctrl Pts',(9.97232040003632,28.9511408610854,56.2958962407257));
#102842=CARTESIAN_POINT('Ctrl Pts',(9.97648615610942,28.9041241251909,56.2548354740807));
#102843=CARTESIAN_POINT('Ctrl Pts',(9.98065518728645,28.8570704248908,56.2137424255939));
#102844=CARTESIAN_POINT('Ctrl Pts',(9.98482421846348,28.8123444693646,56.1700113037728));
#102845=CARTESIAN_POINT('Ctrl Pts',(9.98899324964051,28.7702347417616,56.1239365683302));
#102846=CARTESIAN_POINT('Ctrl Pts',(9.99266216642701,28.7331764709268,56.0833889295335));
#102847=CARTESIAN_POINT('Ctrl Pts',(9.9963310832135,28.6981440032315,56.0410269555827));
#102848=CARTESIAN_POINT('Ctrl Pts',(10.,28.6653082844465,55.9970727277551));
#102849=CARTESIAN_POINT('',(10.,29.207701741744,53.534455913333));
#102850=CARTESIAN_POINT('Origin',(10.,30.,55.));
#102851=CARTESIAN_POINT('Ctrl Pts',(10.,29.207701741744,53.534455913333));
#102852=CARTESIAN_POINT('Ctrl Pts',(9.9999921334966,29.2076011593475,53.5345102899009));
#102853=CARTESIAN_POINT('Ctrl Pts',(9.99998428041792,29.2075007614304,53.5345645801173));
#102854=CARTESIAN_POINT('Ctrl Pts',(9.99924409863901,29.1980390851774,53.5396822377603));
#102855=CARTESIAN_POINT('Ctrl Pts',(9.99850690240549,29.1887266307341,53.5448351356371));
#102856=CARTESIAN_POINT('Ctrl Pts',(9.98871049730391,29.0663555033177,53.6140869791279));
#102857=CARTESIAN_POINT('Ctrl Pts',(9.97908838697546,28.9611311285857,53.6911087323511));
#102858=CARTESIAN_POINT('Ctrl Pts',(9.96547087946054,28.8230334408968,53.8194344968611));
#102859=CARTESIAN_POINT('Ctrl Pts',(9.96129063692594,28.7822640983707,53.8615336559987));
#102860=CARTESIAN_POINT('Ctrl Pts',(9.95536217401458,28.7265932318676,53.92544106697));
#102861=CARTESIAN_POINT('Ctrl Pts',(9.95354765844531,28.7098603486707,53.9455894979658));
#102862=CARTESIAN_POINT('Ctrl Pts',(9.9502902850344,28.6803877058669,53.982830757882));
#102863=CARTESIAN_POINT('Ctrl Pts',(9.94884150801389,28.6674879769311,53.9997891949158));
#102864=CARTESIAN_POINT('Ctrl Pts',(9.94657711500799,28.6476679566286,54.0269095813354));
#102865=CARTESIAN_POINT('Ctrl Pts',(9.94575320398035,28.6405291332994,54.0369081586646));
#102866=CARTESIAN_POINT('Ctrl Pts',(9.94421115893203,28.6273090069964,54.0558640875259));
#102867=CARTESIAN_POINT('Ctrl Pts',(9.94349212969346,28.6212031894676,54.0648034708836));
#102868=CARTESIAN_POINT('Ctrl Pts',(9.94187407736825,28.6075992945117,54.0851434830152));
#102869=CARTESIAN_POINT('Ctrl Pts',(9.94097700410683,28.6001532151457,54.0965780784546));
#102870=CARTESIAN_POINT('Ctrl Pts',(9.93865937760413,28.581176216018,54.1265182189766));
#102871=CARTESIAN_POINT('Ctrl Pts',(9.93724674340839,28.5698663821802,54.1451612691884));
#102872=CARTESIAN_POINT('Ctrl Pts',(9.92880290084574,28.5039289990767,54.2588253280436));
#102873=CARTESIAN_POINT('Ctrl Pts',(9.92209637357502,28.4584200902975,54.3588269039648));
#102874=CARTESIAN_POINT('Ctrl Pts',(9.90957491399275,28.3925433534241,54.5521284972471));
#102875=CARTESIAN_POINT('Ctrl Pts',(9.90377823975221,28.369712852453,54.6440997978177));
#102876=CARTESIAN_POINT('Ctrl Pts',(9.89667275096164,28.3525038873702,54.7519538800272));
#102877=CARTESIAN_POINT('Ctrl Pts',(9.89571196948037,28.3503879452385,54.7664398308436));
#102878=CARTESIAN_POINT('Ctrl Pts',(9.8942461764201,28.3474812667112,54.7883549751589));
#102879=CARTESIAN_POINT('Ctrl Pts',(9.89374843852431,28.3465490980117,54.7957651110021));
#102880=CARTESIAN_POINT('Ctrl Pts',(9.89283834932606,28.34494466509,54.8092509423548));
#102881=CARTESIAN_POINT('Ctrl Pts',(9.89242689546626,28.3442559718041,54.8153244055713));
#102882=CARTESIAN_POINT('Ctrl Pts',(9.89148437809254,28.3427617626,54.829182354735));
#102883=CARTESIAN_POINT('Ctrl Pts',(9.89095220180115,28.3419776746004,54.8369686968788));
#102884=CARTESIAN_POINT('Ctrl Pts',(9.88930777585709,28.3397361169874,54.860919926778));
#102885=CARTESIAN_POINT('Ctrl Pts',(9.88818650237146,28.3384600395756,54.8771002860524));
#102886=CARTESIAN_POINT('Ctrl Pts',(9.88143658466501,28.3322568641657,54.973753328602));
#102887=CARTESIAN_POINT('Ctrl Pts',(9.87558979249202,28.3329407862813,55.0544720596489));
#102888=CARTESIAN_POINT('Ctrl Pts',(9.86438828937606,28.3454057313998,55.208003988834));
#102889=CARTESIAN_POINT('Ctrl Pts',(9.85904784155947,28.3561803189986,55.2807240357849));
#102890=CARTESIAN_POINT('Ctrl Pts',(9.85078615767219,28.3806875041675,55.3939287792899));
#102891=CARTESIAN_POINT('Ctrl Pts',(9.84779849883295,28.3912348448639,55.4350034609071));
#102892=CARTESIAN_POINT('Ctrl Pts',(9.84273624168451,28.4120610560996,55.5049152269595));
#102893=CARTESIAN_POINT('Ctrl Pts',(9.84064051823436,28.4215880117049,55.533952509169));
#102894=CARTESIAN_POINT('Ctrl Pts',(9.83762117921648,28.4366419197326,55.5759026667076));
#102895=CARTESIAN_POINT('Ctrl Pts',(9.83667736323895,28.4415413894456,55.5890323832796));
#102896=CARTESIAN_POINT('Ctrl Pts',(9.83501642720591,28.4505062074001,55.6121612908367));
#102897=CARTESIAN_POINT('Ctrl Pts',(9.83429711970387,28.4545040982892,55.6221855723715));
#102898=CARTESIAN_POINT('Ctrl Pts',(9.83279079984806,28.4631184296286,55.6431896166631));
#102899=CARTESIAN_POINT('Ctrl Pts',(9.8320045368151,28.4677557923953,55.6541601829281));
#102900=CARTESIAN_POINT('Ctrl Pts',(9.82992068834927,28.480419579384,55.6832450934806));
#102901=CARTESIAN_POINT('Ctrl Pts',(9.82863012633181,28.4886523055433,55.7012679323898));
#102902=CARTESIAN_POINT('Ctrl Pts',(9.82166564186228,28.5351693697122,55.7984751409863));
#102903=CARTESIAN_POINT('Ctrl Pts',(9.81620162899176,28.5793586830698,55.8746841845705));
#102904=CARTESIAN_POINT('Ctrl Pts',(9.80490794400726,28.6840408201953,56.026186466088));
#102905=CARTESIAN_POINT('Ctrl Pts',(9.79911265478617,28.7454635057324,56.1004286345801));
#102906=CARTESIAN_POINT('Ctrl Pts',(9.79133331747189,28.8324496410791,56.1887619974792));
#102907=CARTESIAN_POINT('Ctrl Pts',(9.78956928065937,28.8524484059355,56.2080786786343));
#102908=CARTESIAN_POINT('Ctrl Pts',(9.78654535833426,28.8869700316724,56.2397920352963));
#102909=CARTESIAN_POINT('Ctrl Pts',(9.78530112692813,28.9012401155837,56.2524562436854));
#102910=CARTESIAN_POINT('Ctrl Pts',(9.78349882617448,28.9219422404081,56.2702025633031));
#102911=CARTESIAN_POINT('Ctrl Pts',(9.78295440190788,28.9281997786776,56.2754871083198));
#102912=CARTESIAN_POINT('Ctrl Pts',(9.78200208682903,28.9391465516507,56.2845943174286));
#102913=CARTESIAN_POINT('Ctrl Pts',(9.78159570555835,28.9438180690526,56.2884379406307));
#102914=CARTESIAN_POINT('Ctrl Pts',(9.78071919834293,28.9538921187521,56.2966350437827));
#102915=CARTESIAN_POINT('Ctrl Pts',(9.78024854822626,28.9593008614875,56.3009801822757));
#102916=CARTESIAN_POINT('Ctrl Pts',(9.7789359381167,28.9743880307589,56.3129462438892));
#102917=CARTESIAN_POINT('Ctrl Pts',(9.7780891580952,28.9841238541162,56.320493613994));
#102918=CARTESIAN_POINT('Ctrl Pts',(9.77161173858368,29.0586842643619,56.3769815114018));
#102919=CARTESIAN_POINT('Ctrl Pts',(9.76573180447678,29.1269198814428,56.4212253838409));
#102920=CARTESIAN_POINT('Ctrl Pts',(9.75291363113925,29.2813131213122,56.5060071409655));
#102921=CARTESIAN_POINT('Ctrl Pts',(9.74599280184867,29.3682876933211,56.5445100250906));
#102922=CARTESIAN_POINT('Ctrl Pts',(9.7356583718456,29.5064217705223,56.5920271868783));
#102923=CARTESIAN_POINT('Ctrl Pts',(9.73210263381972,29.5555127458148,56.606425246884));
#102924=CARTESIAN_POINT('Ctrl Pts',(9.72747810644054,29.6214674384418,56.6225133937519));
#102925=CARTESIAN_POINT('Ctrl Pts',(9.72634490236115,29.6378012218125,56.6262375884116));
#102926=CARTESIAN_POINT('Ctrl Pts',(9.72446881266807,29.6651226433057,56.632034952004));
#102927=CARTESIAN_POINT('Ctrl Pts',(9.7237215868202,29.6760796489352,56.6342449465537));
#102928=CARTESIAN_POINT('Ctrl Pts',(9.72225894172217,29.6976712846713,56.6383742255235));
#102929=CARTESIAN_POINT('Ctrl Pts',(9.72154332754521,29.7083039696301,56.6403006402005));
#102930=CARTESIAN_POINT('Ctrl Pts',(9.71981549057166,29.7341376432104,56.6447220057654));
#102931=CARTESIAN_POINT('Ctrl Pts',(9.71880671242831,29.7493561355462,56.6471098774975));
#102932=CARTESIAN_POINT('Ctrl Pts',(9.71537206282122,29.8016080993668,56.6545675266043));
#102933=CARTESIAN_POINT('Ctrl Pts',(9.71297862446614,29.8387794100014,56.6586022123196));
#102934=CARTESIAN_POINT('Ctrl Pts',(9.702975055107,29.9966288627798,56.6703781122689));
#102935=CARTESIAN_POINT('Ctrl Pts',(9.69571902315179,30.1178188968901,56.6662215698574));
#102936=CARTESIAN_POINT('Ctrl Pts',(9.685218760115,30.2871537633829,56.6418330608564));
#102937=CARTESIAN_POINT('Ctrl Pts',(9.68211195186999,30.3364601418657,56.6324420203433));
#102938=CARTESIAN_POINT('Ctrl Pts',(9.6771040355738,30.4130889463502,56.6142278331624));
#102939=CARTESIAN_POINT('Ctrl Pts',(9.67525946604597,30.4407370908712,56.6068990504903));
#102940=CARTESIAN_POINT('Ctrl Pts',(9.6727539684467,30.4772828515812,56.5961976784617));
#102941=CARTESIAN_POINT('Ctrl Pts',(9.67212594439946,30.4863616153848,56.5934548370253));
#102942=CARTESIAN_POINT('Ctrl Pts',(9.67107703854111,30.5013788504092,56.58877759629));
#102943=CARTESIAN_POINT('Ctrl Pts',(9.67065865726054,30.5073309349506,56.5868869912357));
#102944=CARTESIAN_POINT('Ctrl Pts',(9.66980524836908,30.5193917341402,56.5829812388149));
#102945=CARTESIAN_POINT('Ctrl Pts',(9.66937013269844,30.5254996044484,56.5809641166416));
#102946=CARTESIAN_POINT('Ctrl Pts',(9.66823795423821,30.541289573384,56.5756478747855));
#102947=CARTESIAN_POINT('Ctrl Pts',(9.66753789391651,30.5509530713428,56.5722949238469));
#102948=CARTESIAN_POINT('Ctrl Pts',(9.66462500577775,30.590776069752,56.558065316548));
#102949=CARTESIAN_POINT('Ctrl Pts',(9.66237347034805,30.6206474170141,56.5464088600235));
#102950=CARTESIAN_POINT('Ctrl Pts',(9.6531773800464,30.7397117547678,56.4959420103337));
#102951=CARTESIAN_POINT('Ctrl Pts',(9.64603165138362,30.8257630429656,56.4502174096908));
#102952=CARTESIAN_POINT('Ctrl Pts',(9.63431974001052,30.9613407943762,56.3621772499679));
#102953=CARTESIAN_POINT('Ctrl Pts',(9.62970407341772,31.0132751120928,56.3240007484282));
#102954=CARTESIAN_POINT('Ctrl Pts',(9.62232836234123,31.094278698707,56.2568903873615));
#102955=CARTESIAN_POINT('Ctrl Pts',(9.61951036125195,31.1247205053202,56.2297250084522));
#102956=CARTESIAN_POINT('Ctrl Pts',(9.6156798326698,31.1653669870621,56.1906797535968));
#102957=CARTESIAN_POINT('Ctrl Pts',(9.61462830541647,31.1764456152332,56.1797348147418));
#102958=CARTESIAN_POINT('Ctrl Pts',(9.61284485989911,31.1950932890359,56.1607882117486));
#102959=CARTESIAN_POINT('Ctrl Pts',(9.61210959425413,31.2027392501759,56.1528640631639));
#102960=CARTESIAN_POINT('Ctrl Pts',(9.61071538918272,31.2171540195357,56.1376253296534));
#102961=CARTESIAN_POINT('Ctrl Pts',(9.61005586610363,31.2239368255041,56.1303247110512));
#102962=CARTESIAN_POINT('Ctrl Pts',(9.60835166070601,31.2413658924711,56.1112242259723));
#102963=CARTESIAN_POINT('Ctrl Pts',(9.60731129854455,31.2519097063717,56.0993319221415));
#102964=CARTESIAN_POINT('Ctrl Pts',(9.60367941479996,31.2883535708544,56.0570226703431));
#102965=CARTESIAN_POINT('Ctrl Pts',(9.60112506719479,31.3133294369489,56.0258255369275));
#102966=CARTESIAN_POINT('Ctrl Pts',(9.59049652839227,31.413827073112,55.8905999988086));
#102967=CARTESIAN_POINT('Ctrl Pts',(9.5828136701822,31.4782952439529,55.7789212372678));
#102968=CARTESIAN_POINT('Ctrl Pts',(9.57297165895243,31.5414547301015,55.6327830043088));
#102969=CARTESIAN_POINT('Ctrl Pts',(9.57106030652439,31.5528431753127,55.6042968262802));
#102970=CARTESIAN_POINT('Ctrl Pts',(9.56912139758663,31.5634376777551,55.575515966569));
#102971=CARTESIAN_POINT('Origin',(5.,30.,55.));
#102972=CARTESIAN_POINT('',(8.86797183897061,31.5634375186471,55.575516398799));
#102973=CARTESIAN_POINT('',(9.06224863102698,31.5634376784282,55.5755159647402));
#102974=CARTESIAN_POINT('',(5.,31.5634376782623,55.5755159651912));
#102975=CARTESIAN_POINT('',(9.72158833090148,31.6659999998112,55.0000015226055));
#102976=CARTESIAN_POINT('Ctrl Pts',(9.06224863102697,31.5634376784283,55.5755159647401));
#102977=CARTESIAN_POINT('Ctrl Pts',(9.06293928128569,31.5597675361453,55.5854862159268));
#102978=CARTESIAN_POINT('Ctrl Pts',(9.06362691885452,31.5560019522037,55.5954215478723));
#102979=CARTESIAN_POINT('Ctrl Pts',(9.07227369261313,31.5072540733995,55.7204191142712));
#102980=CARTESIAN_POINT('Ctrl Pts',(9.07977931942399,31.4497036442719,55.8301699251228));
#102981=CARTESIAN_POINT('Ctrl Pts',(9.09272378845509,31.3311181141229,56.0057216985928));
#102982=CARTESIAN_POINT('Ctrl Pts',(9.09813272625667,31.2759635575033,56.0748324046651));
#102983=CARTESIAN_POINT('Ctrl Pts',(9.10491873848209,31.2043377353272,56.1512593088233));
#102984=CARTESIAN_POINT('Ctrl Pts',(9.10599655431006,31.19289571438,56.1631109755843));
#102985=CARTESIAN_POINT('Ctrl Pts',(9.10759798742486,31.1758371962787,56.1802637300698));
#102986=CARTESIAN_POINT('Ctrl Pts',(9.10811173698039,31.1703561771518,56.1856989488918));
#102987=CARTESIAN_POINT('Ctrl Pts',(9.10903052724184,31.1605435552389,56.195295248907));
#102988=CARTESIAN_POINT('Ctrl Pts',(9.10943440023325,31.1562269354538,56.1994712781793));
#102989=CARTESIAN_POINT('Ctrl Pts',(9.11033221764584,31.1466246925319,56.2086607810446));
#102990=CARTESIAN_POINT('Ctrl Pts',(9.1108269550082,31.1413287935606,56.2136629058821));
#102991=CARTESIAN_POINT('Ctrl Pts',(9.11229679390002,31.1255764231085,56.2283471813861));
#102992=CARTESIAN_POINT('Ctrl Pts',(9.11327876789436,31.1150286382456,56.2379297978141));
#102993=CARTESIAN_POINT('Ctrl Pts',(9.11557758347753,31.0902529116233,56.2598649031498));
#102994=CARTESIAN_POINT('Ctrl Pts',(9.1169002135782,31.0759359162082,56.2721135269541));
#102995=CARTESIAN_POINT('Ctrl Pts',(9.1216112363507,31.0246277780649,56.3145234173586));
#102996=CARTESIAN_POINT('Ctrl Pts',(9.12505479880484,30.9865531261056,56.3433340096796));
#102997=CARTESIAN_POINT('Ctrl Pts',(9.13668862231103,30.8547290214093,56.4344536269194));
#102998=CARTESIAN_POINT('Ctrl Pts',(9.14492219155174,30.755904048157,56.4889034494751));
#102999=CARTESIAN_POINT('Ctrl Pts',(9.1560675588748,30.6103743046556,56.5508316952402));
#103000=CARTESIAN_POINT('Ctrl Pts',(9.15923110531494,30.5676929085884,56.566959216064));
#103001=CARTESIAN_POINT('Ctrl Pts',(9.16347228959737,30.5085835509555,56.5865611973252));
#103002=CARTESIAN_POINT('Ctrl Pts',(9.16459934446256,30.492689104707,56.5915687677051));
#103003=CARTESIAN_POINT('Ctrl Pts',(9.16639595110731,30.4670590358538,56.5992227957994));
#103004=CARTESIAN_POINT('Ctrl Pts',(9.16707039746375,30.4573702030699,56.602020661119));
#103005=CARTESIAN_POINT('Ctrl Pts',(9.16846536848271,30.4371936504265,56.6076491219757));
#103006=CARTESIAN_POINT('Ctrl Pts',(9.16918540206304,30.4267024257003,56.6104654720852));
#103007=CARTESIAN_POINT('Ctrl Pts',(9.17088149007747,30.4018130523105,56.616886683418));
#103008=CARTESIAN_POINT('Ctrl Pts',(9.17185462937672,30.3873926425779,56.6204021846428));
#103009=CARTESIAN_POINT('Ctrl Pts',(9.17516181891229,30.3379309813643,56.6317622257666));
#103010=CARTESIAN_POINT('Ctrl Pts',(9.17746609259214,30.302682675301,56.6386667761133));
#103011=CARTESIAN_POINT('Ctrl Pts',(9.18311688138339,30.2146517914985,56.6529727156887));
#103012=CARTESIAN_POINT('Ctrl Pts',(9.18642450480134,30.1616849501031,56.6589914994885));
#103013=CARTESIAN_POINT('Ctrl Pts',(9.1931045230721,30.0532834277847,56.6660674302036));
#103014=CARTESIAN_POINT('Ctrl Pts',(9.19647019781724,29.9979034581181,56.6669179602142));
#103015=CARTESIAN_POINT('Ctrl Pts',(9.20070013024026,29.9287972729098,56.6645349114707));
#103016=CARTESIAN_POINT('Ctrl Pts',(9.20154517656372,29.9150170858926,56.6638882770147));
#103017=CARTESIAN_POINT('Ctrl Pts',(9.20691140084649,29.8278006458662,56.658709352287));
#103018=CARTESIAN_POINT('Ctrl Pts',(9.2114851009775,29.7547331623437,56.6494880319336));
#103019=CARTESIAN_POINT('Ctrl Pts',(9.2170916499667,29.6704756082838,56.6331320577941));
#103020=CARTESIAN_POINT('Ctrl Pts',(9.21789968334496,29.6584535006396,56.6306601761097));
#103021=CARTESIAN_POINT('Ctrl Pts',(9.21917627988038,29.6396719364905,56.6265816735425));
#103022=CARTESIAN_POINT('Ctrl Pts',(9.21963996527995,29.6328930736158,56.6250651538587));
#103023=CARTESIAN_POINT('Ctrl Pts',(9.22051226721762,29.6202254395123,56.62214793468));
#103024=CARTESIAN_POINT('Ctrl Pts',(9.22092031075189,29.6143345610657,56.6207574782435));
#103025=CARTESIAN_POINT('Ctrl Pts',(9.22188648273589,29.6004660433869,56.6174041279162));
#103026=CARTESIAN_POINT('Ctrl Pts',(9.22244609695882,29.5924951987902,56.6154142890924));
#103027=CARTESIAN_POINT('Ctrl Pts',(9.22433020439821,29.5658544997367,56.6085539996208));
#103028=CARTESIAN_POINT('Ctrl Pts',(9.22566823457467,29.5472553652699,56.6034183800581));
#103029=CARTESIAN_POINT('Ctrl Pts',(9.22899864395205,29.5016456753128,56.589967779792));
#103030=CARTESIAN_POINT('Ctrl Pts',(9.23100558775403,29.4747499649182,56.5812864364313));
#103031=CARTESIAN_POINT('Ctrl Pts',(9.24019387779678,29.3537610240141,56.5388066657188));
#103032=CARTESIAN_POINT('Ctrl Pts',(9.24754721382004,29.2626056634811,56.497264435469));
#103033=CARTESIAN_POINT('Ctrl Pts',(9.26073727958948,29.1036603813908,56.4067720877262));
#103034=CARTESIAN_POINT('Ctrl Pts',(9.26660347042933,29.0347520069989,56.360416286323));
#103035=CARTESIAN_POINT('Ctrl Pts',(9.27362333424604,28.9541520129957,56.2969746240103));
#103036=CARTESIAN_POINT('Ctrl Pts',(9.27495582875827,28.9389452618019,56.2845637730119));
#103037=CARTESIAN_POINT('Ctrl Pts',(9.27707452383162,28.914925732336,56.2642428144208));
#103038=CARTESIAN_POINT('Ctrl Pts',(9.27786751495595,28.9059721887577,56.2565027739306));
#103039=CARTESIAN_POINT('Ctrl Pts',(9.27937300013986,28.8890479467531,56.241554268009));
#103040=CARTESIAN_POINT('Ctrl Pts',(9.28008614719488,28.8810630694573,56.234362839572));
#103041=CARTESIAN_POINT('Ctrl Pts',(9.2817198949902,28.862849079093,56.2176367698139));
#103042=CARTESIAN_POINT('Ctrl Pts',(9.28263820707428,28.8526692186604,56.2080495097675));
#103043=CARTESIAN_POINT('Ctrl Pts',(9.28554909999279,28.8206026065786,56.1770785836723));
#103044=CARTESIAN_POINT('Ctrl Pts',(9.2875210425452,28.7991829570915,56.1552189495418));
#103045=CARTESIAN_POINT('Ctrl Pts',(9.29217893993317,28.7494800660016,56.1016179042624));
#103046=CARTESIAN_POINT('Ctrl Pts',(9.29484235655604,28.7217853574685,56.069359536966));
#103047=CARTESIAN_POINT('Ctrl Pts',(9.30204530464079,28.6495387928007,55.9783852237224));
#103048=CARTESIAN_POINT('Ctrl Pts',(9.30651745083815,28.6076004530641,55.9177183576028));
#103049=CARTESIAN_POINT('Ctrl Pts',(9.31186054882374,28.5628111182578,55.8427518034916));
#103050=CARTESIAN_POINT('Ctrl Pts',(9.31269722941317,28.5559515872971,55.8309432352984));
#103051=CARTESIAN_POINT('Ctrl Pts',(9.31805984532966,28.5130327468991,55.754922374555));
#103052=CARTESIAN_POINT('Ctrl Pts',(9.32263808235209,28.4811238448674,55.6884706863783));
#103053=CARTESIAN_POINT('Ctrl Pts',(9.32824990129537,28.4491448636682,55.608732541227));
#103054=CARTESIAN_POINT('Ctrl Pts',(9.32905877137347,28.4446978697281,55.5972790155644));
#103055=CARTESIAN_POINT('Ctrl Pts',(9.3303368815668,28.4379320189691,55.5792650700017));
#103056=CARTESIAN_POINT('Ctrl Pts',(9.33080124643702,28.4355267895186,55.5727372591254));
#103057=CARTESIAN_POINT('Ctrl Pts',(9.33167549849056,28.4310989439311,55.5604840290776));
#103058=CARTESIAN_POINT('Ctrl Pts',(9.33208481850921,28.4290666513074,55.5547623633094));
#103059=CARTESIAN_POINT('Ctrl Pts',(9.33305483032973,28.4243457156412,55.5412371935046));
#103060=CARTESIAN_POINT('Ctrl Pts',(9.3336170225781,28.4216837310813,55.53342466345));
#103061=CARTESIAN_POINT('Ctrl Pts',(9.33551298120203,28.4129499800598,55.5071545934103));
#103062=CARTESIAN_POINT('Ctrl Pts',(9.33686042197716,28.4071433423331,55.4886114356529));
#103063=CARTESIAN_POINT('Ctrl Pts',(9.34021857972493,28.3936172014157,55.4426101064415));
#103064=CARTESIAN_POINT('Ctrl Pts',(9.34224406405335,28.3862761427188,55.4150476252237));
#103065=CARTESIAN_POINT('Ctrl Pts',(9.35160860557777,28.3558912858513,55.2879299189499));
#103066=CARTESIAN_POINT('Ctrl Pts',(9.35912300282084,28.3413294135802,55.186573554496));
#103067=CARTESIAN_POINT('Ctrl Pts',(9.37220621381704,28.3321092200796,55.0050654559412));
#103068=CARTESIAN_POINT('Ctrl Pts',(9.37782459907529,28.3337690258278,54.9254146775234));
#103069=CARTESIAN_POINT('Ctrl Pts',(9.38460402308866,28.3429177027656,54.8267521393244));
#103070=CARTESIAN_POINT('Ctrl Pts',(9.38592822619664,28.3450599923048,54.8073599523512));
#103071=CARTESIAN_POINT('Ctrl Pts',(9.38803771301508,28.3490465822965,54.7762846959257));
#103072=CARTESIAN_POINT('Ctrl Pts',(9.38882965584497,28.3506754590439,54.7645763483789));
#103073=CARTESIAN_POINT('Ctrl Pts',(9.39033565813448,28.3540263238609,54.7422352846733));
#103074=CARTESIAN_POINT('Ctrl Pts',(9.39105034530193,28.3557270719483,54.7316000403139));
#103075=CARTESIAN_POINT('Ctrl Pts',(9.39269122752458,28.3598871765332,54.7071111580265));
#103076=CARTESIAN_POINT('Ctrl Pts',(9.39361508286203,28.3624191561991,54.6932705629591));
#103077=CARTESIAN_POINT('Ctrl Pts',(9.39655903638998,28.3710954800286,54.649017607785));
#103078=CARTESIAN_POINT('Ctrl Pts',(9.39855784591758,28.3779143118231,54.6187431433732));
#103079=CARTESIAN_POINT('Ctrl Pts',(9.4099350245357,28.4220179381688,54.4456390954479));
#103080=CARTESIAN_POINT('Ctrl Pts',(9.41870203428594,28.477304108859,54.3080897440184));
#103081=CARTESIAN_POINT('Ctrl Pts',(9.43134065343489,28.5777528360631,54.130547089414));
#103082=CARTESIAN_POINT('Ctrl Pts',(9.43488985288649,28.6079891438743,54.0829178102258));
#103083=CARTESIAN_POINT('Ctrl Pts',(9.43935430827129,28.6474654603177,54.0271956565969));
#103084=CARTESIAN_POINT('Ctrl Pts',(9.44013925237602,28.654457255636,54.0175476221827));
#103085=CARTESIAN_POINT('Ctrl Pts',(9.44138741222215,28.6656420234885,54.0024570296437));
#103086=CARTESIAN_POINT('Ctrl Pts',(9.44184610499773,28.6697663642701,53.9969637806512));
#103087=CARTESIAN_POINT('Ctrl Pts',(9.44271278265618,28.6775822968313,53.9866866570922));
#103088=CARTESIAN_POINT('Ctrl Pts',(9.44312024102352,28.6812660848524,53.9818971716314));
#103089=CARTESIAN_POINT('Ctrl Pts',(9.44409173264595,28.6900717686854,53.9705764139777));
#103090=CARTESIAN_POINT('Ctrl Pts',(9.44465732957572,28.6952164879157,53.9640632886545));
#103091=CARTESIAN_POINT('Ctrl Pts',(9.44659809780187,28.7129383854756,53.9419691141793));
#103092=CARTESIAN_POINT('Ctrl Pts',(9.44798808105683,28.7257471612771,53.9265771712717));
#103093=CARTESIAN_POINT('Ctrl Pts',(9.45148133423516,28.758294527602,53.888869511172));
#103094=CARTESIAN_POINT('Ctrl Pts',(9.45360111481002,28.7783598370672,53.8668457524919));
#103095=CARTESIAN_POINT('Ctrl Pts',(9.46387144260097,28.8774946323081,53.763729723926));
#103096=CARTESIAN_POINT('Ctrl Pts',(9.47222581443075,28.9641069803916,53.6903014162346));
#103097=CARTESIAN_POINT('Ctrl Pts',(9.48531563202135,29.1147225511038,53.5869696312445));
#103098=CARTESIAN_POINT('Ctrl Pts',(9.49019306822294,29.1743438227994,53.5513229644445));
#103099=CARTESIAN_POINT('Ctrl Pts',(9.49622371898402,29.2527443836546,53.5108663189698));
#103100=CARTESIAN_POINT('Ctrl Pts',(9.49750006791159,29.2696117482676,53.5025210757432));
#103101=CARTESIAN_POINT('Ctrl Pts',(9.49954793400567,29.2971115278384,53.4894906005289));
#103102=CARTESIAN_POINT('Ctrl Pts',(9.50032556481102,29.3076574818053,53.484627867628));
#103103=CARTESIAN_POINT('Ctrl Pts',(9.50181338288449,29.3280303158158,53.4754910456978));
#103104=CARTESIAN_POINT('Ctrl Pts',(9.50252409959971,29.3378492395932,53.4712007365601));
#103105=CARTESIAN_POINT('Ctrl Pts',(9.50416871529685,29.3607683112844,53.4614486459508));
#103106=CARTESIAN_POINT('Ctrl Pts',(9.50510012806694,29.3738983459009,53.4560588870174));
#103107=CARTESIAN_POINT('Ctrl Pts',(9.50812329622769,29.4169869333384,53.4390115039924));
#103108=CARTESIAN_POINT('Ctrl Pts',(9.51019175471155,29.447215307859,53.4280526019688));
#103109=CARTESIAN_POINT('Ctrl Pts',(9.51513454339689,29.5210272682812,53.4036858791511));
#103110=CARTESIAN_POINT('Ctrl Pts',(9.51798193817156,29.5648811646825,53.3911787860515));
#103111=CARTESIAN_POINT('Ctrl Pts',(9.52509598764719,29.6767720585325,53.3641784262859));
#103112=CARTESIAN_POINT('Ctrl Pts',(9.52931399503807,29.7453043411834,53.3521168466163));
#103113=CARTESIAN_POINT('Ctrl Pts',(9.53434103965144,29.8269811132401,53.3429601687225));
#103114=CARTESIAN_POINT('Ctrl Pts',(9.53511708763151,29.839588182171,53.3416922536186));
#103115=CARTESIAN_POINT('Ctrl Pts',(9.54041152767559,29.9254787169282,53.3340427070248));
#103116=CARTESIAN_POINT('Ctrl Pts',(9.54498322551238,29.999091844044,53.3323778784447));
#103117=CARTESIAN_POINT('Ctrl Pts',(9.5505868677634,30.0847941746212,53.3361142412321));
#103118=CARTESIAN_POINT('Ctrl Pts',(9.55139286450664,30.0970180179242,53.3367822292992));
#103119=CARTESIAN_POINT('Ctrl Pts',(9.55266584410028,30.1161402967374,53.33803870412));
#103120=CARTESIAN_POINT('Ctrl Pts',(9.55312794535591,30.1230445979865,53.3385356037256));
#103121=CARTESIAN_POINT('Ctrl Pts',(9.55399890063669,30.1359830999371,53.339547870928));
#103122=CARTESIAN_POINT('Ctrl Pts',(9.55440719738167,30.1420178669402,53.3400531342943));
#103123=CARTESIAN_POINT('Ctrl Pts',(9.55537431830951,30.1562422845859,53.3413222125061));
#103124=CARTESIAN_POINT('Ctrl Pts',(9.5559346382882,30.1644292226808,53.342113792247));
#103125=CARTESIAN_POINT('Ctrl Pts',(9.55781829539099,30.1917821508138,53.3449630891386));
#103126=CARTESIAN_POINT('Ctrl Pts',(9.55915511183033,30.2109174498649,53.347292730092));
#103127=CARTESIAN_POINT('Ctrl Pts',(9.56247984889537,30.2579316078467,53.3538462335772));
#103128=CARTESIAN_POINT('Ctrl Pts',(9.56448223031771,30.2857514051568,53.3584468049578));
#103129=CARTESIAN_POINT('Ctrl Pts',(9.57360822445225,30.4108354900165,53.3824078746661));
#103130=CARTESIAN_POINT('Ctrl Pts',(9.58090199874208,30.5063703582634,53.4097234631507));
#103131=CARTESIAN_POINT('Ctrl Pts',(9.59414466477184,30.6776067192957,53.4756911215899));
#103132=CARTESIAN_POINT('Ctrl Pts',(9.60011509632396,30.7538980002194,53.5119441748055));
#103133=CARTESIAN_POINT('Ctrl Pts',(9.6072444541771,30.8442980617198,53.5636476236931));
#103134=CARTESIAN_POINT('Ctrl Pts',(9.60858795697425,30.8612950058578,53.5737747943839));
#103135=CARTESIAN_POINT('Ctrl Pts',(9.61072253968059,30.8882262619261,53.5904781433869));
#103136=CARTESIAN_POINT('Ctrl Pts',(9.61152050508331,30.8982769915131,53.5968620111175));
#103137=CARTESIAN_POINT('Ctrl Pts',(9.61303453680375,30.9173100591049,53.6092394773106));
#103138=CARTESIAN_POINT('Ctrl Pts',(9.61375126878156,30.9263042080106,53.6152136989617));
#103139=CARTESIAN_POINT('Ctrl Pts',(9.61539209895532,30.9468529024029,53.629152633958));
#103140=CARTESIAN_POINT('Ctrl Pts',(9.61631391074184,30.9583662676364,53.6371768138606));
#103141=CARTESIAN_POINT('Ctrl Pts',(9.61923223901578,30.9946993618172,53.6631871440359));
#103142=CARTESIAN_POINT('Ctrl Pts',(9.6212081772296,31.0191255948057,53.6817137479796));
#103143=CARTESIAN_POINT('Ctrl Pts',(9.62587587064451,31.0762244665977,53.7275577481859));
#103144=CARTESIAN_POINT('Ctrl Pts',(9.62854516136255,31.1083886019676,53.7554745998401));
#103145=CARTESIAN_POINT('Ctrl Pts',(9.63571344019281,31.1926820468283,53.8345001976203));
#103146=CARTESIAN_POINT('Ctrl Pts',(9.64014781064916,31.2425793870167,53.8878502460746));
#103147=CARTESIAN_POINT('Ctrl Pts',(9.64532676979143,31.2961694168032,53.9532739545163));
#103148=CARTESIAN_POINT('Ctrl Pts',(9.6460379820886,31.3034263651314,53.9623245792557));
#103149=CARTESIAN_POINT('Ctrl Pts',(9.65139201868645,31.3572323658479,54.0308847082958));
#103150=CARTESIAN_POINT('Ctrl Pts',(9.65608516034864,31.3997738872444,54.0934161255742));
#103151=CARTESIAN_POINT('Ctrl Pts',(9.6618257008195,31.4441601149845,54.1692712942414));
#103152=CARTESIAN_POINT('Ctrl Pts',(9.66263892300595,31.4502803016499,54.1800026554667));
#103153=CARTESIAN_POINT('Ctrl Pts',(9.6639246942477,31.4596841040202,54.1969262645773));
#103154=CARTESIAN_POINT('Ctrl Pts',(9.66439237439429,31.4630490880941,54.203073109093));
#103155=CARTESIAN_POINT('Ctrl Pts',(9.66527785028223,31.4693135982272,54.2146899483029));
#103156=CARTESIAN_POINT('Ctrl Pts',(9.66569511987698,31.4722215700353,54.220155162289));
#103157=CARTESIAN_POINT('Ctrl Pts',(9.666688503862,31.4790417852602,54.233147109499));
#103158=CARTESIAN_POINT('Ctrl Pts',(9.66726620417077,31.4829271100746,54.2406877211072));
#103159=CARTESIAN_POINT('Ctrl Pts',(9.66923214447231,31.4958821909095,54.2663095598047));
#103160=CARTESIAN_POINT('Ctrl Pts',(9.67063484700283,31.5046797883318,54.2845254454026));
#103161=CARTESIAN_POINT('Ctrl Pts',(9.68050126631705,31.5636329629896,54.4124899746156));
#103162=CARTESIAN_POINT('Ctrl Pts',(9.6893817068692,31.6020652382261,54.5272401423611));
#103163=CARTESIAN_POINT('Ctrl Pts',(9.70405552931875,31.6455025616253,54.7264852314741));
#103164=CARTESIAN_POINT('Ctrl Pts',(9.7099398458228,31.6571167822441,54.8090637802794));
#103165=CARTESIAN_POINT('Ctrl Pts',(9.71695427045445,31.6637537404347,54.9113969690014));
#103166=CARTESIAN_POINT('Ctrl Pts',(9.71826169886316,31.6646669638397,54.9306389267541));
#103167=CARTESIAN_POINT('Ctrl Pts',(9.72022163497542,31.6655422914515,54.9597294550104));
#103168=CARTESIAN_POINT('Ctrl Pts',(9.7208816490184,31.665751111934,54.9695684112151));
#103169=CARTESIAN_POINT('Ctrl Pts',(9.72199553663507,31.6659572261724,54.9862435190925));
#103170=CARTESIAN_POINT('Ctrl Pts',(9.72245078595099,31.6659996453322,54.99307873824));
#103171=CARTESIAN_POINT('Ctrl Pts',(9.72290474287967,31.6659999977852,54.9999140956723));
#103172=CARTESIAN_POINT('Ctrl Pts',(9.72148036344425,31.6659999999773,55.0000086930536));
#103173=CARTESIAN_POINT('Ctrl Pts',(9.72575162903862,31.6659996648664,55.0642317834644));
#103174=CARTESIAN_POINT('Ctrl Pts',(9.73002289463299,31.6622813967003,55.128381221177));
#103175=CARTESIAN_POINT('Ctrl Pts',(9.73429416022736,31.6548963909707,55.192025871049));
#103176=CARTESIAN_POINT('Ctrl Pts',(9.73869642027905,31.6472848962072,55.2576224239783));
#103177=CARTESIAN_POINT('Ctrl Pts',(9.74309868033075,31.6357781724688,55.3226822259613));
#103178=CARTESIAN_POINT('Ctrl Pts',(9.74750094038244,31.6204884723869,55.3867468304473));
#103179=CARTESIAN_POINT('Ctrl Pts',(9.75190320043414,31.6051987723051,55.4508114349334));
#103180=CARTESIAN_POINT('Ctrl Pts',(9.75630546048584,31.5861263069399,55.5138803910486));
#103181=CARTESIAN_POINT('Ctrl Pts',(9.76070772053754,31.5634376782623,55.5755159651912));
#103182=CARTESIAN_POINT('Ctrl Pts',(9.56912139758663,31.5634376777551,55.575515966569));
#103183=CARTESIAN_POINT('Ctrl Pts',(9.56843888003858,31.5671670606512,55.5653847832946));
#103184=CARTESIAN_POINT('Ctrl Pts',(9.56775294050477,31.5707980645885,55.5552170859515));
#103185=CARTESIAN_POINT('Ctrl Pts',(9.56544857079703,31.5825951755981,55.5211399118735));
#103186=CARTESIAN_POINT('Ctrl Pts',(9.56381286286895,31.5903155367117,55.497082113429));
#103187=CARTESIAN_POINT('Ctrl Pts',(9.56154741322078,31.6000746418027,55.4641124419768));
#103188=CARTESIAN_POINT('Ctrl Pts',(9.56094266118142,31.60259188435,55.4553443323174));
#103189=CARTESIAN_POINT('Ctrl Pts',(9.55991911091215,31.6067025944225,55.4405693928223));
#103190=CARTESIAN_POINT('Ctrl Pts',(9.55950248788842,31.608334734456,55.4345733506667));
#103191=CARTESIAN_POINT('Ctrl Pts',(9.55864070723962,31.6116256346078,55.4222109598002));
#103192=CARTESIAN_POINT('Ctrl Pts',(9.55819534445324,31.613280284311,55.4158437220623));
#103193=CARTESIAN_POINT('Ctrl Pts',(9.55700795882038,31.6175712483432,55.3989205861298));
#103194=CARTESIAN_POINT('Ctrl Pts',(9.55626240405005,31.620141888435,55.3883485845622));
#103195=CARTESIAN_POINT('Ctrl Pts',(9.55284758840529,31.6313657656347,55.3401372294056));
#103196=CARTESIAN_POINT('Ctrl Pts',(9.55012186546077,31.6388114398416,55.3022319369514));
#103197=CARTESIAN_POINT('Ctrl Pts',(9.54075737098301,31.6595734472879,55.1729196813758));
#103198=CARTESIAN_POINT('Ctrl Pts',(9.53397689092433,31.6666062158077,55.0806761496393));
#103199=CARTESIAN_POINT('Ctrl Pts',(9.52052986714115,31.665304347461,54.8948864531111));
#103200=CARTESIAN_POINT('Ctrl Pts',(9.51389078321266,31.6567896110581,54.8016547613869));
#103201=CARTESIAN_POINT('Ctrl Pts',(9.50615114195072,31.637077577199,54.6902936245822));
#103202=CARTESIAN_POINT('Ctrl Pts',(9.50481893139739,31.6333161965664,54.6710329927547));
#103203=CARTESIAN_POINT('Ctrl Pts',(9.50270074440271,31.6267427763886,54.6402724353493));
#103204=CARTESIAN_POINT('Ctrl Pts',(9.50190798132002,31.6241470459172,54.6287287150432));
#103205=CARTESIAN_POINT('Ctrl Pts',(9.50040296692266,31.6189604179501,54.6067589135398));
#103206=CARTESIAN_POINT('Ctrl Pts',(9.49969006264807,31.6163912322436,54.5963283753965));
#103207=CARTESIAN_POINT('Ctrl Pts',(9.49807234840389,31.6103053245132,54.5726106520954));
#103208=CARTESIAN_POINT('Ctrl Pts',(9.4971696425408,31.6067246720497,54.5593405625229));
#103209=CARTESIAN_POINT('Ctrl Pts',(9.49430651218749,31.5947806685594,54.5171579812168));
#103210=CARTESIAN_POINT('Ctrl Pts',(9.49236607054106,31.585797656029,54.4884261834884));
#103211=CARTESIAN_POINT('Ctrl Pts',(9.48140346894314,31.5300586917328,54.3257612329878));
#103212=CARTESIAN_POINT('Ctrl Pts',(9.47294360003098,31.4671304458004,54.1979985341477));
#103213=CARTESIAN_POINT('Ctrl Pts',(9.4615268026904,31.3649473971391,54.0437911004344));
#103214=CARTESIAN_POINT('Ctrl Pts',(9.45883671393636,31.3397333148186,54.0087729812608));
#103215=CARTESIAN_POINT('Ctrl Pts',(9.45442793195575,31.2972308252152,53.9543323593697));
#103216=CARTESIAN_POINT('Ctrl Pts',(9.45275013384337,31.280796721428,53.9342663512118));
#103217=CARTESIAN_POINT('Ctrl Pts',(9.45043645746936,31.257912358809,53.9076186461381));
#103218=CARTESIAN_POINT('Ctrl Pts',(9.44982710834959,31.2518651386115,53.9006937688619));
#103219=CARTESIAN_POINT('Ctrl Pts',(9.44879894430112,31.2416349493708,53.8891727091354));
#103220=CARTESIAN_POINT('Ctrl Pts',(9.44838237362555,31.2374828987417,53.8845491085432));
#103221=CARTESIAN_POINT('Ctrl Pts',(9.44752388156461,31.2289139827507,53.8751137463673));
#103222=CARTESIAN_POINT('Ctrl Pts',(9.44708178493124,31.2244945505675,53.8703045753224));
#103223=CARTESIAN_POINT('Ctrl Pts',(9.44591017285661,31.2127619320424,53.8576870174266));
#103224=CARTESIAN_POINT('Ctrl Pts',(9.44517726954991,31.205401752765,53.8499230228377));
#103225=CARTESIAN_POINT('Ctrl Pts',(9.4419086217738,31.1724632434546,53.815840873813));
#103226=CARTESIAN_POINT('Ctrl Pts',(9.43932186275907,31.146095950254,53.790303131795));
#103227=CARTESIAN_POINT('Ctrl Pts',(9.4291357477657,31.040401505385,53.6944928888983));
#103228=CARTESIAN_POINT('Ctrl Pts',(9.42133169317932,30.9552842901963,53.6309797720966));
#103229=CARTESIAN_POINT('Ctrl Pts',(9.40776036305137,30.7943870075803,53.5332777156577));
#103230=CARTESIAN_POINT('Ctrl Pts',(9.40194190944326,30.7209881840826,53.49583754913));
#103231=CARTESIAN_POINT('Ctrl Pts',(9.39496986376498,30.6270551730021,53.456386905623));
#103232=CARTESIAN_POINT('Ctrl Pts',(9.39364024069968,30.6088650410454,53.4491218636671));
#103233=CARTESIAN_POINT('Ctrl Pts',(9.39152582848276,30.5795035616891,53.4379912964515));
#103234=CARTESIAN_POINT('Ctrl Pts',(9.39073427172936,30.5684123186592,53.4339211333964));
#103235=CARTESIAN_POINT('Ctrl Pts',(9.3892313680882,30.5471678441394,53.4263804608205));
#103236=CARTESIAN_POINT('Ctrl Pts',(9.38851937083619,30.5370225952394,53.4228893998384));
#103237=CARTESIAN_POINT('Ctrl Pts',(9.38688810182456,30.5135974057995,53.4150808606403));
#103238=CARTESIAN_POINT('Ctrl Pts',(9.38597111633698,30.5002953753401,53.4108318117179));
#103239=CARTESIAN_POINT('Ctrl Pts',(9.38306412352662,30.4577162315701,53.397818447542));
#103240=CARTESIAN_POINT('Ctrl Pts',(9.38109473540321,30.4282497422575,53.3896918860816));
#103241=CARTESIAN_POINT('Ctrl Pts',(9.37644358074709,30.3573718268691,53.3722278625199));
#103242=CARTESIAN_POINT('Ctrl Pts',(9.37378431901489,30.3157941132131,53.3636530896065));
#103243=CARTESIAN_POINT('Ctrl Pts',(9.36657904545865,30.2011535168197,53.3445432215242));
#103244=CARTESIAN_POINT('Ctrl Pts',(9.3621011029355,30.1276478641984,53.3372594080665));
#103245=CARTESIAN_POINT('Ctrl Pts',(9.35677683137713,30.0406492200486,53.3344432033744));
#103246=CARTESIAN_POINT('Ctrl Pts',(9.35596473417298,30.0273925757854,53.3341724448094));
#103247=CARTESIAN_POINT('Ctrl Pts',(9.35059047955145,29.9398679825883,53.3334298663247));
#103248=CARTESIAN_POINT('Ctrl Pts',(9.34597604659209,29.8656518036035,53.3377666764457));
#103249=CARTESIAN_POINT('Ctrl Pts',(9.34032435664034,29.7798052221407,53.3485700427747));
#103250=CARTESIAN_POINT('Ctrl Pts',(9.33951634068205,29.7676453136079,53.350237010425));
#103251=CARTESIAN_POINT('Ctrl Pts',(9.3382399143794,29.7486362021598,53.3530572367882));
#103252=CARTESIAN_POINT('Ctrl Pts',(9.33777638380629,29.7417736231372,53.3541192758634));
#103253=CARTESIAN_POINT('Ctrl Pts',(9.3369044207251,29.7289446926024,53.3561868634161));
#103254=CARTESIAN_POINT('Ctrl Pts',(9.33649656133541,29.7229769187949,53.3571820504258));
#103255=CARTESIAN_POINT('Ctrl Pts',(9.33553096125169,29.7089239966555,53.3596042653874));
#103256=CARTESIAN_POINT('Ctrl Pts',(9.33497173761227,29.7008438253787,53.3610585788428));
#103257=CARTESIAN_POINT('Ctrl Pts',(9.33308971579237,29.6738347132591,53.3661262083867));
#103258=CARTESIAN_POINT('Ctrl Pts',(9.33175341910263,29.654958551408,53.3700080733511));
#103259=CARTESIAN_POINT('Ctrl Pts',(9.32842800910045,29.6086213823301,53.3803781777075));
#103260=CARTESIAN_POINT('Ctrl Pts',(9.32642438356216,29.5812502419328,53.3872382289343));
#103261=CARTESIAN_POINT('Ctrl Pts',(9.31726138820989,29.4580283564345,53.4214696076344));
#103262=CARTESIAN_POINT('Ctrl Pts',(9.30993080677071,29.3645774991331,53.4567145074392));
#103263=CARTESIAN_POINT('Ctrl Pts',(9.29674505771154,29.1999744623092,53.536295961376));
#103264=CARTESIAN_POINT('Ctrl Pts',(9.29086227013496,29.1279178614349,53.5780482122596));
#103265=CARTESIAN_POINT('Ctrl Pts',(9.28382707217414,29.0430754109903,53.6360951543477));
#103266=CARTESIAN_POINT('Ctrl Pts',(9.28249476205126,29.0270758684549,53.6474617238605));
#103267=CARTESIAN_POINT('Ctrl Pts',(9.2803765684037,29.0017586477555,53.6661296327067));
#103268=CARTESIAN_POINT('Ctrl Pts',(9.27958389327735,28.9923118638365,53.6732518751466));
#103269=CARTESIAN_POINT('Ctrl Pts',(9.27807914126751,28.9744356032813,53.6870304640742));
#103270=CARTESIAN_POINT('Ctrl Pts',(9.27736641054238,28.9659931027749,53.6936688475787));
#103271=CARTESIAN_POINT('Ctrl Pts',(9.275733813904,28.9467160331359,53.7091304872602));
#103272=CARTESIAN_POINT('Ctrl Pts',(9.27481623204606,28.9359269925767,53.7180094117578));
#103273=CARTESIAN_POINT('Ctrl Pts',(9.27190856507873,28.9019004751943,53.7467373341465));
#103274=CARTESIAN_POINT('Ctrl Pts',(9.26993906691906,28.8790960704118,53.7670910641118));
#103275=CARTESIAN_POINT('Ctrl Pts',(9.26528794143432,28.8259978657113,53.8171748896573));
#103276=CARTESIAN_POINT('Ctrl Pts',(9.2626287733219,28.7962544587725,53.8474578953481));
#103277=CARTESIAN_POINT('Ctrl Pts',(9.25542782535457,28.718098548194,53.9333618940862));
#103278=CARTESIAN_POINT('Ctrl Pts',(9.25095375909464,28.6721702728705,53.9911111238162));
#103279=CARTESIAN_POINT('Ctrl Pts',(9.24560870912098,28.6224417280865,54.0629430129494));
#103280=CARTESIAN_POINT('Ctrl Pts',(9.24477185811805,28.6148050548724,54.0742691817106));
#103281=CARTESIAN_POINT('Ctrl Pts',(9.23940295840345,28.5668343355864,54.1473387693496));
#103282=CARTESIAN_POINT('Ctrl Pts',(9.23481861962066,28.5305033768844,54.2116016775694));
#103283=CARTESIAN_POINT('Ctrl Pts',(9.22920030444782,28.4932316031709,54.2891162044358));
#103284=CARTESIAN_POINT('Ctrl Pts',(9.22839192343974,28.4880333004404,54.3002404340435));
#103285=CARTESIAN_POINT('Ctrl Pts',(9.22711468537034,28.4800856671172,54.3177502381017));
#103286=CARTESIAN_POINT('Ctrl Pts',(9.22665070295415,28.477252420096,54.3240975510956));
#103287=CARTESIAN_POINT('Ctrl Pts',(9.22577804538881,28.4720260580494,54.3360058109906));
#103288=CARTESIAN_POINT('Ctrl Pts',(9.22536994515191,28.4696234271096,54.3415623106149));
#103289=CARTESIAN_POINT('Ctrl Pts',(9.22440363460769,28.4640311513545,54.3546913813091));
#103290=CARTESIAN_POINT('Ctrl Pts',(9.22384393950127,28.4608671887328,54.3622745892069));
#103291=CARTESIAN_POINT('Ctrl Pts',(9.22195873761799,28.4504561077155,54.3877560975347));
#103292=CARTESIAN_POINT('Ctrl Pts',(9.22061967377745,28.443464393955,54.405756196596));
#103293=CARTESIAN_POINT('Ctrl Pts',(9.21728584882126,28.427003252466,54.4504203963385));
#103294=CARTESIAN_POINT('Ctrl Pts',(9.21527648876348,28.4178974297132,54.4772115295083));
#103295=CARTESIAN_POINT('Ctrl Pts',(9.20606239155674,28.3796302092884,54.5999773096793));
#103296=CARTESIAN_POINT('Ctrl Pts',(9.19868506082896,28.3584903070569,54.6982338519756));
#103297=CARTESIAN_POINT('Ctrl Pts',(9.18551250193248,28.3363151657845,54.8795889060205));
#103298=CARTESIAN_POINT('Ctrl Pts',(9.17968479460354,28.3323947406802,54.9620206181944));
#103299=CARTESIAN_POINT('Ctrl Pts',(9.17270303743105,28.335114636498,55.0640062432877));
#103300=CARTESIAN_POINT('Ctrl Pts',(9.1713725345938,28.3359827694484,55.0835869972811));
#103301=CARTESIAN_POINT('Ctrl Pts',(9.16925664323324,28.3379282236735,55.1149486240861));
#103302=CARTESIAN_POINT('Ctrl Pts',(9.16846448496528,28.3387858146876,55.1267407544119));
#103303=CARTESIAN_POINT('Ctrl Pts',(9.16696037153546,28.3406616825418,55.1492234730349));
#103304=CARTESIAN_POINT('Ctrl Pts',(9.16624776626329,28.3416579304798,55.1599152474169));
#103305=CARTESIAN_POINT('Ctrl Pts',(9.16461498515638,28.3441887078215,55.1845001768978));
#103306=CARTESIAN_POINT('Ctrl Pts',(9.16369709896174,28.3457948571069,55.1983852704428));
#103307=CARTESIAN_POINT('Ctrl Pts',(9.16078658377417,28.3514739313462,55.2425986556928));
#103308=CARTESIAN_POINT('Ctrl Pts',(9.15881461336789,28.3562078475767,55.2728366814595));
#103309=CARTESIAN_POINT('Ctrl Pts',(9.15415646784814,28.3695008319836,55.3447246616848));
#103310=CARTESIAN_POINT('Ctrl Pts',(9.1514928616421,28.3788264265774,55.386211411117));
#103311=CARTESIAN_POINT('Ctrl Pts',(9.14428667114999,28.4086385240908,55.4985580819379));
#103312=CARTESIAN_POINT('Ctrl Pts',(9.13981172065586,28.432257672762,55.5684855928086));
#103313=CARTESIAN_POINT('Ctrl Pts',(9.13445242938353,28.4657334458135,55.6494418264753));
#103314=CARTESIAN_POINT('Ctrl Pts',(9.1336023629126,28.4711957836392,55.6621980122535));
#103315=CARTESIAN_POINT('Ctrl Pts',(9.12823491606235,28.5065940840286,55.7420903600135));
#103316=CARTESIAN_POINT('Ctrl Pts',(9.12366503966482,28.5407830448044,55.8072437517862));
#103317=CARTESIAN_POINT('Ctrl Pts',(9.11806275655161,28.5855660190547,55.8803881055));
#103318=CARTESIAN_POINT('Ctrl Pts',(9.11725456451468,28.5920914028662,55.8907862050594));
#103319=CARTESIAN_POINT('Ctrl Pts',(9.11597769365475,28.6024891000288,55.9069551058199));
#103320=CARTESIAN_POINT('Ctrl Pts',(9.11551389048466,28.6062837810931,55.9127756440087));
#103321=CARTESIAN_POINT('Ctrl Pts',(9.11464155862745,28.6134514022043,55.923620923263));
#103322=CARTESIAN_POINT('Ctrl Pts',(9.11423360457744,28.6168154536837,55.9286512424472));
#103323=CARTESIAN_POINT('Ctrl Pts',(9.11326772223332,28.6248093842379,55.9404648953807));
#103324=CARTESIAN_POINT('Ctrl Pts',(9.11270831054794,28.6294620984284,55.9472324437079));
#103325=CARTESIAN_POINT('Ctrl Pts',(9.11082467040578,28.6452108640997,55.9697806709638));
#103326=CARTESIAN_POINT('Ctrl Pts',(9.10948690974453,28.6565304853925,55.9854023221984));
#103327=CARTESIAN_POINT('Ctrl Pts',(9.1061569511322,28.6850933062422,56.0234133393425));
#103328=CARTESIAN_POINT('Ctrl Pts',(9.10415019034259,28.7026395100741,56.0455668584097));
#103329=CARTESIAN_POINT('Ctrl Pts',(9.09495878113625,28.7848160281203,56.1440667175974));
#103330=CARTESIAN_POINT('Ctrl Pts',(9.08760211413387,28.8556785008973,56.2149442318511));
#103331=CARTESIAN_POINT('Ctrl Pts',(9.07442321463585,28.9959932289217,56.332055660511));
#103332=CARTESIAN_POINT('Ctrl Pts',(9.06857067622661,29.0633839453631,56.3802738727036));
#103333=CARTESIAN_POINT('Ctrl Pts',(9.06156504909387,29.1508395707369,56.4334807276759));
#103334=CARTESIAN_POINT('Ctrl Pts',(9.06023391260802,29.1677692533702,56.4433753748076));
#103335=CARTESIAN_POINT('Ctrl Pts',(9.05811732988295,29.1951820795511,56.4587542335006));
#103336=CARTESIAN_POINT('Ctrl Pts',(9.05732510356771,29.2055553641059,56.4644294219276));
#103337=CARTESIAN_POINT('Ctrl Pts',(9.05582105718531,29.2254609657391,56.4750459441564));
#103338=CARTESIAN_POINT('Ctrl Pts',(9.05510858502812,29.2349823040467,56.4800064820965));
#103339=CARTESIAN_POINT('Ctrl Pts',(9.05347638824164,29.2570022340538,56.4912094011162));
#103340=CARTESIAN_POINT('Ctrl Pts',(9.05255894933391,29.2695328345439,56.4973873573875));
#103341=CARTESIAN_POINT('Ctrl Pts',(9.04965103860313,29.3097227232626,56.5165775777828));
#103342=CARTESIAN_POINT('Ctrl Pts',(9.04768117630316,29.33766395817,56.52898705805));
#103343=CARTESIAN_POINT('Ctrl Pts',(9.04302895226361,29.4051809371577,56.5567747655664));
#103344=CARTESIAN_POINT('Ctrl Pts',(9.04036908224021,29.4450343113215,56.5714231929296));
#103345=CARTESIAN_POINT('Ctrl Pts',(9.03316538820894,29.5555417829254,56.6073116505606));
#103346=CARTESIAN_POINT('Ctrl Pts',(9.02868941773754,29.6271141542294,56.6254077529749));
#103347=CARTESIAN_POINT('Ctrl Pts',(9.02334928855865,29.7129769827958,56.6411451365426));
#103348=CARTESIAN_POINT('Ctrl Pts',(9.02251931711529,29.7263330487208,56.6434250716013));
#103349=CARTESIAN_POINT('Ctrl Pts',(9.01714811733028,29.8127171604241,56.6570889356044));
#103350=CARTESIAN_POINT('Ctrl Pts',(9.01255456462187,29.8863976007119,56.6637639027963));
#103351=CARTESIAN_POINT('Ctrl Pts',(9.00692601924097,29.9725405802788,56.6658189279834));
#103352=CARTESIAN_POINT('Ctrl Pts',(9.00611778419574,29.9848163379132,56.665976036805));
#103353=CARTESIAN_POINT('Ctrl Pts',(9.0048408787324,30.0040404844589,56.6660095895311));
#103354=CARTESIAN_POINT('Ctrl Pts',(9.00437708521899,30.0109885561357,56.6659782487136));
#103355=CARTESIAN_POINT('Ctrl Pts',(9.00350474681917,30.0239877560037,56.6658382918829));
#103356=CARTESIAN_POINT('Ctrl Pts',(9.00309677635804,30.0300387503311,56.6657401645936));
#103357=CARTESIAN_POINT('Ctrl Pts',(9.00213085668382,30.0443001382684,56.6654311611487));
#103358=CARTESIAN_POINT('Ctrl Pts',(9.00157142392235,30.0525096553228,56.6651925365575));
#103359=CARTESIAN_POINT('Ctrl Pts',(8.99968783654224,30.0799943028688,56.6641902011967));
#103360=CARTESIAN_POINT('Ctrl Pts',(8.99835015287118,30.0992570805142,56.6631524485093));
#103361=CARTESIAN_POINT('Ctrl Pts',(8.99502048223286,30.1466794286389,56.6597709073216));
#103362=CARTESIAN_POINT('Ctrl Pts',(8.99301393749694,30.1748051958208,56.6570447437967));
#103363=CARTESIAN_POINT('Ctrl Pts',(8.9838247306023,30.3020994262158,56.6414296646917));
#103364=CARTESIAN_POINT('Ctrl Pts',(8.9764701309106,30.4000540267934,56.6203433649102));
#103365=CARTESIAN_POINT('Ctrl Pts',(8.96328635188567,30.5746117732985,56.5659625293287));
#103366=CARTESIAN_POINT('Ctrl Pts',(8.95742726746579,30.6517580524963,56.5354584023196));
#103367=CARTESIAN_POINT('Ctrl Pts',(8.9504177634592,30.7439419965077,56.4908016294299));
#103368=CARTESIAN_POINT('Ctrl Pts',(8.94908882301312,30.7614078520939,56.4819572638775));
#103369=CARTESIAN_POINT('Ctrl Pts',(8.94697480182236,30.7891619710384,56.4672828793185));
#103370=CARTESIAN_POINT('Ctrl Pts',(8.94618297255658,30.799550657379,56.4616478451445));
#103371=CARTESIAN_POINT('Ctrl Pts',(8.94467910690707,30.8192634211448,56.4506821747156));
#103372=CARTESIAN_POINT('Ctrl Pts',(8.94396642434882,30.8285975896672,56.4453710142629));
#103373=CARTESIAN_POINT('Ctrl Pts',(8.94233293297492,30.8499689450331,56.432935594311));
#103374=CARTESIAN_POINT('Ctrl Pts',(8.94141442063563,30.8619691818833,56.4257491975129));
#103375=CARTESIAN_POINT('Ctrl Pts',(8.93849966168582,30.8999774049968,56.4023324931049));
#103376=CARTESIAN_POINT('Ctrl Pts',(8.93652416040779,30.925629419124,56.385534596638));
#103377=CARTESIAN_POINT('Ctrl Pts',(8.93185579651994,30.9857963952058,56.3437177313079));
#103378=CARTESIAN_POINT('Ctrl Pts',(8.92918564263991,31.0198438113091,56.3180632977824));
#103379=CARTESIAN_POINT('Ctrl Pts',(8.92197730699959,31.1099594331494,56.2445771229049));
#103380=CARTESIAN_POINT('Ctrl Pts',(8.91750625392741,31.1638978437474,56.1942882093984));
#103381=CARTESIAN_POINT('Ctrl Pts',(8.91212697571873,31.2240950862085,56.1301993700254));
#103382=CARTESIAN_POINT('Ctrl Pts',(8.9112531958362,31.2337251221126,56.1196792901001));
#103383=CARTESIAN_POINT('Ctrl Pts',(8.90589476105488,31.2917844259517,56.0545954180717));
#103384=CARTESIAN_POINT('Ctrl Pts',(8.90135742289196,31.3367156392568,55.9970291447507));
#103385=CARTESIAN_POINT('Ctrl Pts',(8.8957912748277,31.3846258643009,55.9265623944582));
#103386=CARTESIAN_POINT('Ctrl Pts',(8.89498320837052,31.3914144077802,55.9163364987807));
#103387=CARTESIAN_POINT('Ctrl Pts',(8.89370646796057,31.4018678646251,55.9002059592704));
#103388=CARTESIAN_POINT('Ctrl Pts',(8.89324266701334,31.4056100290262,55.8943515644891));
#103389=CARTESIAN_POINT('Ctrl Pts',(8.89237028226156,31.4125432127131,55.883354009506));
#103390=CARTESIAN_POINT('Ctrl Pts',(8.89196227251172,31.4157429668173,55.8782166481709));
#103391=CARTESIAN_POINT('Ctrl Pts',(8.89099617160445,31.4232197242359,55.8660653006766));
#103392=CARTESIAN_POINT('Ctrl Pts',(8.8904365957617,31.4274729184495,55.859036989024));
#103393=CARTESIAN_POINT('Ctrl Pts',(8.88855200720881,31.4415450468792,55.835390010543));
#103394=CARTESIAN_POINT('Ctrl Pts',(8.88721344657906,31.451126702301,55.8186328886552));
#103395=CARTESIAN_POINT('Ctrl Pts',(8.88388110120536,31.4740232419693,55.7769242005239));
#103396=CARTESIAN_POINT('Ctrl Pts',(8.88187273069933,31.4869977951015,55.7517932615117));
#103397=CARTESIAN_POINT('Ctrl Pts',(8.87592640617201,31.523178718102,55.6771084654667));
#103398=CARTESIAN_POINT('Ctrl Pts',(8.87194751235138,31.544570813737,55.6267693507067));
#103399=CARTESIAN_POINT('Ctrl Pts',(8.86797183897061,31.5634375186471,55.575516398799));
#103400=CARTESIAN_POINT('Origin',(5.,30.,55.));
#103401=CARTESIAN_POINT('',(8.16625307517082,31.5634376782623,55.5755159651912));
#103402=CARTESIAN_POINT('',(8.36103882979909,31.5634376856231,55.5755159451947));
#103403=CARTESIAN_POINT('',(5.,31.5634376782623,55.5755159651912));
#103404=CARTESIAN_POINT('Ctrl Pts',(8.36103882979909,31.5634376856231,55.5755159451947));
#103405=CARTESIAN_POINT('Ctrl Pts',(8.36205627649009,31.5585956668143,55.5886696983504));
#103406=CARTESIAN_POINT('Ctrl Pts',(8.36307222991977,31.5535870872764,55.6017638659151));
#103407=CARTESIAN_POINT('Ctrl Pts',(8.36843576746039,31.5262117404169,55.6707109554684));
#103408=CARTESIAN_POINT('Ctrl Pts',(8.37273595310039,31.5009962748264,55.7253873979175));
#103409=CARTESIAN_POINT('Ctrl Pts',(8.3788042038508,31.4604844203644,55.8020251027462));
#103410=CARTESIAN_POINT('Ctrl Pts',(8.38064270991459,31.4475349235036,55.8251677328212));
#103411=CARTESIAN_POINT('Ctrl Pts',(8.38393356177099,31.4231244565934,55.8664482070297));
#103412=CARTESIAN_POINT('Ctrl Pts',(8.38539217101872,31.4118553526886,55.8846921791763));
#103413=CARTESIAN_POINT('Ctrl Pts',(8.3876615210663,31.3936183896671,55.9129802718727));
#103414=CARTESIAN_POINT('Ctrl Pts',(8.38848086408679,31.3868871992046,55.9231733874505));
#103415=CARTESIAN_POINT('Ctrl Pts',(8.39000823057807,31.3740658124173,55.942132176784));
#103416=CARTESIAN_POINT('Ctrl Pts',(8.39071720763343,31.3680023442971,55.9509150805632));
#103417=CARTESIAN_POINT('Ctrl Pts',(8.3923041953239,31.3541798214715,55.9705310642995));
#103418=CARTESIAN_POINT('Ctrl Pts',(8.39318037718018,31.3463742998671,55.9813306259722));
#103419=CARTESIAN_POINT('Ctrl Pts',(8.39542499448463,31.325935616332,56.0089061962745));
#103420=CARTESIAN_POINT('Ctrl Pts',(8.39678606958796,31.3131130949825,56.0255393870726));
#103421=CARTESIAN_POINT('Ctrl Pts',(8.4063894878014,31.2196827289862,56.1421095478402));
#103422=CARTESIAN_POINT('Ctrl Pts',(8.41415207298269,31.128075389506,56.2326758698676));
#103423=CARTESIAN_POINT('Ctrl Pts',(8.42714731700296,30.9608330099099,56.3636019305316));
#103424=CARTESIAN_POINT('Ctrl Pts',(8.43232045910536,30.8908860865237,56.4102938096875));
#103425=CARTESIAN_POINT('Ctrl Pts',(8.43870216532561,30.8054625641133,56.4584184117172));
#103426=CARTESIAN_POINT('Ctrl Pts',(8.43962655498679,30.7931099673625,56.4651726019063));
#103427=CARTESIAN_POINT('Ctrl Pts',(8.44104140069344,30.7742656185709,56.4751682514421));
#103428=CARTESIAN_POINT('Ctrl Pts',(8.44152498915339,30.767835489199,56.4785253716999));
#103429=CARTESIAN_POINT('Ctrl Pts',(8.44241414991067,30.7560372658783,56.4845874122119));
#103430=CARTESIAN_POINT('Ctrl Pts',(8.44281890556004,30.7506761896033,56.4873054113144));
#103431=CARTESIAN_POINT('Ctrl Pts',(8.4437507378028,30.7383554763966,56.4934682763078));
#103432=CARTESIAN_POINT('Ctrl Pts',(8.44427896811244,30.7313864012709,56.4968935258967));
#103433=CARTESIAN_POINT('Ctrl Pts',(8.44591343049007,30.7098614556466,56.5072866811455));
#103434=CARTESIAN_POINT('Ctrl Pts',(8.44702867678168,30.6952285709147,56.5140916787555));
#103435=CARTESIAN_POINT('Ctrl Pts',(8.45379903316783,30.6065904147532,56.5537569224189));
#103436=CARTESIAN_POINT('Ctrl Pts',(8.45967662653935,30.5303749060301,56.5813957418237));
#103437=CARTESIAN_POINT('Ctrl Pts',(8.47093284823899,30.3815331505376,56.6233976049849));
#103438=CARTESIAN_POINT('Ctrl Pts',(8.47629712669906,30.3093511513442,56.6386856027348));
#103439=CARTESIAN_POINT('Ctrl Pts',(8.48459249075474,30.1942878553428,56.6551789267522));
#103440=CARTESIAN_POINT('Ctrl Pts',(8.48759132509216,30.1519669194229,56.6595998339502));
#103441=CARTESIAN_POINT('Ctrl Pts',(8.49266871781459,30.0789710662695,56.6644088632391));
#103442=CARTESIAN_POINT('Ctrl Pts',(8.49476880563511,30.0483707606269,56.6655791114978));
#103443=CARTESIAN_POINT('Ctrl Pts',(8.49779003535032,30.0037726874795,56.6660543987042));
#103444=CARTESIAN_POINT('Ctrl Pts',(8.49873164972401,29.9897899359217,56.6660273911016));
#103445=CARTESIAN_POINT('Ctrl Pts',(8.50038688120911,29.9650691642587,56.6656683946309));
#103446=CARTESIAN_POINT('Ctrl Pts',(8.50110270600235,29.9543310751578,56.6654085753201));
#103447=CARTESIAN_POINT('Ctrl Pts',(8.50259985222612,29.9317773424905,56.664644559856));
#103448=CARTESIAN_POINT('Ctrl Pts',(8.50338044663311,29.9199630046799,56.6641183651334));
#103449=CARTESIAN_POINT('Ctrl Pts',(8.50544465656957,29.8885837964544,56.6623858245411));
#103450=CARTESIAN_POINT('Ctrl Pts',(8.50672139226859,29.8690325433054,56.6609598965471));
#103451=CARTESIAN_POINT('Ctrl Pts',(8.51331372961258,29.7674414121054,56.651745506146));
#103452=CARTESIAN_POINT('Ctrl Pts',(8.51844679840904,29.686032601836,56.6382227151438));
#103453=CARTESIAN_POINT('Ctrl Pts',(8.52967070183395,29.5084836991051,56.5950017036998));
#103454=CARTESIAN_POINT('Ctrl Pts',(8.53570216748055,29.4133655981144,56.5625224609065));
#103455=CARTESIAN_POINT('Ctrl Pts',(8.54376391854017,29.2959083315333,56.5101693734412));
#103456=CARTESIAN_POINT('Ctrl Pts',(8.545557656361,29.2703632579819,56.4979942116819));
#103457=CARTESIAN_POINT('Ctrl Pts',(8.54862650761194,29.2279266813487,56.4764253187738));
#103458=CARTESIAN_POINT('Ctrl Pts',(8.54988527641027,29.2108656149202,56.467377175633));
#103459=CARTESIAN_POINT('Ctrl Pts',(8.55170421024368,29.1867743938961,56.4540590254996));
#103460=CARTESIAN_POINT('Ctrl Pts',(8.55225031257358,29.1796119134909,56.4500299709209));
#103461=CARTESIAN_POINT('Ctrl Pts',(8.55320454506792,29.167225112612,56.4429409694294));
#103462=CARTESIAN_POINT('Ctrl Pts',(8.55361114476291,29.1619871883431,56.4399052678831));
#103463=CARTESIAN_POINT('Ctrl Pts',(8.5544885743513,29.1507717538263,56.4333233020826));
#103464=CARTESIAN_POINT('Ctrl Pts',(8.55495992992316,29.1447999424607,56.4297682188284));
#103465=CARTESIAN_POINT('Ctrl Pts',(8.55627020811848,29.1283409314513,56.419829987886));
#103466=CARTESIAN_POINT('Ctrl Pts',(8.5571138777114,29.1179020249927,56.4133682700058));
#103467=CARTESIAN_POINT('Ctrl Pts',(8.56302674093423,29.0457739172337,56.3676104409821));
#103468=CARTESIAN_POINT('Ctrl Pts',(8.56829783249204,28.986665831434,56.3244082556172));
#103469=CARTESIAN_POINT('Ctrl Pts',(8.57463991073829,28.9197268208185,56.2683716770691));
#103470=CARTESIAN_POINT('Ctrl Pts',(8.57567095620926,28.9089762791907,56.2591362474495));
#103471=CARTESIAN_POINT('Ctrl Pts',(8.58206622320197,28.8430616759172,56.2010331907677));
#103472=CARTESIAN_POINT('Ctrl Pts',(8.58743037033348,28.7910693122629,56.1486839919751));
#103473=CARTESIAN_POINT('Ctrl Pts',(8.59572623647197,28.7148007825884,56.0609565121179));
#103474=CARTESIAN_POINT('Ctrl Pts',(8.5987256730966,28.6881277174367,56.0277924725809));
#103475=CARTESIAN_POINT('Ctrl Pts',(8.60380396940839,28.6444893757952,55.9690637294101));
#103476=CARTESIAN_POINT('Ctrl Pts',(8.60590436855001,28.6269071670899,55.9439861493138));
#103477=CARTESIAN_POINT('Ctrl Pts',(8.60892596337948,28.602316716161,55.906770618742));
#103478=CARTESIAN_POINT('Ctrl Pts',(8.60986763814666,28.5947552561777,55.895007680189));
#103479=CARTESIAN_POINT('Ctrl Pts',(8.61152294507793,28.581648757723,55.8740429751129));
#103480=CARTESIAN_POINT('Ctrl Pts',(8.61223878544998,28.576043033867,55.8648803019511));
#103481=CARTESIAN_POINT('Ctrl Pts',(8.61373593447631,28.5644527037283,55.8455174728347));
#103482=CARTESIAN_POINT('Ctrl Pts',(8.61451651638392,28.5584872802521,55.8353064872514));
#103483=CARTESIAN_POINT('Ctrl Pts',(8.61658062428933,28.5429248722342,55.8080050848434));
#103484=CARTESIAN_POINT('Ctrl Pts',(8.61785727193711,28.5335197151259,55.7908070382551));
#103485=CARTESIAN_POINT('Ctrl Pts',(8.62444643346127,28.4861850338615,55.7005019933978));
#103486=CARTESIAN_POINT('Ctrl Pts',(8.62957665226229,28.4534090839173,55.6248182193147));
#103487=CARTESIAN_POINT('Ctrl Pts',(8.64080026141045,28.3934132303803,55.4522229888109));
#103488=CARTESIAN_POINT('Ctrl Pts',(8.64683403084159,28.3690975507752,55.3546569237867));
#103489=CARTESIAN_POINT('Ctrl Pts',(8.65489854654159,28.3493687251707,55.227537462718));
#103490=CARTESIAN_POINT('Ctrl Pts',(8.65669259725022,28.3457420320228,55.1994675340614));
#103491=CARTESIAN_POINT('Ctrl Pts',(8.65976193398912,28.3408460214315,55.1521088679756));
#103492=CARTESIAN_POINT('Ctrl Pts',(8.66102086942313,28.3391942281276,55.1328651286049));
#103493=CARTESIAN_POINT('Ctrl Pts',(8.66284000985164,28.3373170226287,55.1053985864034));
#103494=CARTESIAN_POINT('Ctrl Pts',(8.66338614849168,28.336817324566,55.0971953002256));
#103495=CARTESIAN_POINT('Ctrl Pts',(8.66434043647391,28.3360549507858,55.0829429384075));
#103496=CARTESIAN_POINT('Ctrl Pts',(8.6647470551388,28.3357645221633,55.0768955837515));
#103497=CARTESIAN_POINT('Ctrl Pts',(8.66562452871365,28.3352114920588,55.0639025155719));
#103498=CARTESIAN_POINT('Ctrl Pts',(8.66609590933853,28.3349593922591,55.0569568067692));
#103499=CARTESIAN_POINT('Ctrl Pts',(8.6674062362673,28.3343822228256,55.0377379867326));
#103500=CARTESIAN_POINT('Ctrl Pts',(8.66824992930461,28.3341493592813,55.0254628354024));
#103501=CARTESIAN_POINT('Ctrl Pts',(8.67416389953594,28.333473131712,54.9400312543727));
#103502=CARTESIAN_POINT('Ctrl Pts',(8.67943614048649,28.3377134140135,54.8669248783947));
#103503=CARTESIAN_POINT('Ctrl Pts',(8.68577826874258,28.3484899467498,54.780293416415));
#103504=CARTESIAN_POINT('Ctrl Pts',(8.68680824145774,28.3504166264213,54.7662669714259));
#103505=CARTESIAN_POINT('Ctrl Pts',(8.6932021576332,28.3634798461617,54.6793937769295));
#103506=CARTESIAN_POINT('Ctrl Pts',(8.69856601264265,28.379261587988,54.6073234484704));
#103507=CARTESIAN_POINT('Ctrl Pts',(8.70686093306862,28.4115969197425,54.4956780143239));
#103508=CARTESIAN_POINT('Ctrl Pts',(8.70985972455127,28.4249899914488,54.4552899976558));
#103509=CARTESIAN_POINT('Ctrl Pts',(8.71493706540982,28.4506571189974,54.3867872130853));
#103510=CARTESIAN_POINT('Ctrl Pts',(8.71703714167927,28.4621877079846,54.3584184749675));
#103511=CARTESIAN_POINT('Ctrl Pts',(8.72005838896884,28.4801142091657,54.3175788054269));
#103512=CARTESIAN_POINT('Ctrl Pts',(8.72100003067838,28.485895227142,54.3048465913996));
#103513=CARTESIAN_POINT('Ctrl Pts',(8.72265532552244,28.496399527294,54.2824646390722));
#103514=CARTESIAN_POINT('Ctrl Pts',(8.72337118620915,28.5010570673973,54.2727851281822));
#103515=CARTESIAN_POINT('Ctrl Pts',(8.72486842380179,28.5110386027274,54.2525444368429));
#103516=CARTESIAN_POINT('Ctrl Pts',(8.72564907347848,28.5163821150826,54.2419935058615));
#103517=CARTESIAN_POINT('Ctrl Pts',(8.72771347101432,28.5308802208721,54.2141072885434));
#103518=CARTESIAN_POINT('Ctrl Pts',(8.72899033767368,28.5402293682744,54.1968748324737));
#103519=CARTESIAN_POINT('Ctrl Pts',(8.7355856539571,28.5904717925098,54.1080447156981));
#103520=CARTESIAN_POINT('Ctrl Pts',(8.74072136238261,28.6363367066296,54.0393861859714));
#103521=CARTESIAN_POINT('Ctrl Pts',(8.75194552477794,28.7488329683305,53.8953768822272));
#103522=CARTESIAN_POINT('Ctrl Pts',(8.75797484606344,28.8175673694881,53.8220942727128));
#103523=CARTESIAN_POINT('Ctrl Pts',(8.76603401967559,28.9136019400408,53.7366332231265));
#103524=CARTESIAN_POINT('Ctrl Pts',(8.76782748247126,28.9352104450464,53.7183684691837));
#103525=CARTESIAN_POINT('Ctrl Pts',(8.77089591604756,28.9723317549512,53.6885783185242));
#103526=CARTESIAN_POINT('Ctrl Pts',(8.77215454880021,28.9875995200781,53.6767562436189));
#103527=CARTESIAN_POINT('Ctrl Pts',(8.77397332815621,29.0096525779383,53.6602852855893));
#103528=CARTESIAN_POINT('Ctrl Pts',(8.77451941604781,29.0162728008566,53.6554166730715));
#103529=CARTESIAN_POINT('Ctrl Pts',(8.77547362680052,29.0278322707947,53.6470467268552));
#103530=CARTESIAN_POINT('Ctrl Pts',(8.77588021930316,29.0327550240435,53.6435230159822));
#103531=CARTESIAN_POINT('Ctrl Pts',(8.77675761398086,29.0433700381244,53.6360119455495));
#103532=CARTESIAN_POINT('Ctrl Pts',(8.77722894166771,29.0490679875311,53.6320334068777));
#103533=CARTESIAN_POINT('Ctrl Pts',(8.77853918054754,29.0649002422733,53.6211253990517));
#103534=CARTESIAN_POINT('Ctrl Pts',(8.77938283919927,29.0750862709956,53.6142722872705));
#103535=CARTESIAN_POINT('Ctrl Pts',(8.78530376321517,29.1465771447837,53.5673129378853));
#103536=CARTESIAN_POINT('Ctrl Pts',(8.79058358863294,29.2103872518454,53.5311800256463));
#103537=CARTESIAN_POINT('Ctrl Pts',(8.79692823295547,29.2890494401745,53.4932472709247));
#103538=CARTESIAN_POINT('Ctrl Pts',(8.79795319720536,29.3018165494048,53.4872890723419));
#103539=CARTESIAN_POINT('Ctrl Pts',(8.80434326283068,29.3818391817626,53.4511727286867));
#103540=CARTESIAN_POINT('Ctrl Pts',(8.80970823356939,29.4509631091155,53.4253417773784));
#103541=CARTESIAN_POINT('Ctrl Pts',(8.81800323613674,29.5623025569032,53.3919624209005));
#103542=CARTESIAN_POINT('Ctrl Pts',(8.82100109501396,29.6034862089017,53.3813149708069));
#103543=CARTESIAN_POINT('Ctrl Pts',(8.82607700920438,29.6749402197358,53.3657328917174));
#103544=CARTESIAN_POINT('Ctrl Pts',(8.82817657985738,29.7050208974012,53.3600364684965));
#103545=CARTESIAN_POINT('Ctrl Pts',(8.83119716665653,29.7490454986412,53.3529501294377));
#103546=CARTESIAN_POINT('Ctrl Pts',(8.8321386461157,29.7628755183767,53.3509022349246));
#103547=CARTESIAN_POINT('Ctrl Pts',(8.83379367495203,29.7873729445972,53.3475893131375));
#103548=CARTESIAN_POINT('Ctrl Pts',(8.83450943126546,29.7980297143815,53.346252934769));
#103549=CARTESIAN_POINT('Ctrl Pts',(8.83600646603725,29.8204455117738,53.3436618664201));
#103550=CARTESIAN_POINT('Ctrl Pts',(8.83678701723942,29.8322065133456,53.3424291312385));
#103551=CARTESIAN_POINT('Ctrl Pts',(8.83885118222315,29.8634948138343,53.3394860628645));
#103552=CARTESIAN_POINT('Ctrl Pts',(8.8401279152448,29.8830412323286,53.3379949156085));
#103553=CARTESIAN_POINT('Ctrl Pts',(8.8467222078802,29.984905580873,53.3320299982524));
#103554=CARTESIAN_POINT('Ctrl Pts',(8.85185707068511,30.06745050934,53.3333252636355));
#103555=CARTESIAN_POINT('Ctrl Pts',(8.86308118628233,30.2494532078754,53.3497312312895));
#103556=CARTESIAN_POINT('Ctrl Pts',(8.86911122386991,30.3483136382028,53.367734955653));
#103557=CARTESIAN_POINT('Ctrl Pts',(8.8771712662145,30.4722125859457,53.4020726878313));
#103558=CARTESIAN_POINT('Ctrl Pts',(8.87896479071521,30.4992782165408,53.4103215723689));
#103559=CARTESIAN_POINT('Ctrl Pts',(8.88203330015515,30.5444404486352,53.4253529115653));
#103560=CARTESIAN_POINT('Ctrl Pts',(8.88329194289921,30.562653424005,53.4317685433296));
#103561=CARTESIAN_POINT('Ctrl Pts',(8.88511070348003,30.5884517182196,53.4413633842885));
#103562=CARTESIAN_POINT('Ctrl Pts',(8.88565676015999,30.5961321227428,53.4442847272902));
#103563=CARTESIAN_POINT('Ctrl Pts',(8.88661092159961,30.6094327224263,53.4494567382818));
#103564=CARTESIAN_POINT('Ctrl Pts',(8.88701749610584,30.6150627705936,53.4516814163397));
#103565=CARTESIAN_POINT('Ctrl Pts',(8.88789488641821,30.6271301870447,53.456525987319));
#103566=CARTESIAN_POINT('Ctrl Pts',(8.88836622801419,30.6335632277531,53.4591554486718));
#103567=CARTESIAN_POINT('Ctrl Pts',(8.8896764567769,30.6513140726288,53.4665409390363));
#103568=CARTESIAN_POINT('Ctrl Pts',(8.89052009068216,30.6625957812576,53.4713818261564));
#103569=CARTESIAN_POINT('Ctrl Pts',(8.89642020845009,30.7405469393167,53.5058550554763));
#103570=CARTESIAN_POINT('Ctrl Pts',(8.90167759448997,30.8052538295571,53.5397113998074));
#103571=CARTESIAN_POINT('Ctrl Pts',(8.90801559435536,30.8797364771311,53.5851416012652));
#103572=CARTESIAN_POINT('Ctrl Pts',(8.90905610408381,30.891850295866,53.5927460771268));
#103573=CARTESIAN_POINT('Ctrl Pts',(8.91545986324786,30.9657593255029,53.6404802841695));
#103574=CARTESIAN_POINT('Ctrl Pts',(8.92082315572547,31.0249378234739,53.6845195943871));
#103575=CARTESIAN_POINT('Ctrl Pts',(8.92912216116893,31.1134180458005,53.7599716080982));
#103576=CARTESIAN_POINT('Ctrl Pts',(8.93212539735323,31.1447574534946,53.7888431005033));
#103577=CARTESIAN_POINT('Ctrl Pts',(8.93720937597408,31.1966854596676,53.8405004664004));
#103578=CARTESIAN_POINT('Ctrl Pts',(8.93931172232874,31.2178135270761,53.862711256745));
#103579=CARTESIAN_POINT('Ctrl Pts',(8.94233557728322,31.2476755165954,53.8958906461361));
#103580=CARTESIAN_POINT('Ctrl Pts',(8.94327760729109,31.2569019163401,53.9064053523242));
#103581=CARTESIAN_POINT('Ctrl Pts',(8.94493333658898,31.2729777268657,53.9251981129967));
#103582=CARTESIAN_POINT('Ctrl Pts',(8.94564924744788,31.2798814345576,53.9334284308271));
#103583=CARTESIAN_POINT('Ctrl Pts',(8.94714634714123,31.2942156155117,53.9508566674604));
#103584=CARTESIAN_POINT('Ctrl Pts',(8.9479268110971,31.3016287706111,53.9600681044917));
#103585=CARTESIAN_POINT('Ctrl Pts',(8.94999014895215,31.3210620786838,53.984748932016));
#103586=CARTESIAN_POINT('Ctrl Pts',(8.95126615464385,31.3329087470012,54.0003530265854));
#103587=CARTESIAN_POINT('Ctrl Pts',(8.95783371841241,31.392920719157,54.0823633260575));
#103588=CARTESIAN_POINT('Ctrl Pts',(8.9629445804669,31.4364112935496,54.1520552825639));
#103589=CARTESIAN_POINT('Ctrl Pts',(8.97416638327103,31.5214237126474,54.3137409249979));
#103590=CARTESIAN_POINT('Ctrl Pts',(8.98021596675857,31.5600845942449,54.4068597668906));
#103591=CARTESIAN_POINT('Ctrl Pts',(8.98829946599533,31.5985611533171,54.5299349960784));
#103592=CARTESIAN_POINT('Ctrl Pts',(8.99009564512755,31.6063240843312,54.5571889525425));
#103593=CARTESIAN_POINT('Ctrl Pts',(8.99316827400936,31.6182077206386,54.6033471469372));
#103594=CARTESIAN_POINT('Ctrl Pts',(8.99442833093867,31.6227011031554,54.6221498119952));
#103595=CARTESIAN_POINT('Ctrl Pts',(8.99624884499023,31.6286376972994,54.6490543438868));
#103596=CARTESIAN_POINT('Ctrl Pts',(8.99679520997813,31.6303498096392,54.6570960866291));
#103597=CARTESIAN_POINT('Ctrl Pts',(8.9977498283048,31.633219510297,54.6710825208833));
#103598=CARTESIAN_POINT('Ctrl Pts',(8.99815654944529,31.634404322585,54.6770213848546));
#103599=CARTESIAN_POINT('Ctrl Pts',(8.99903423950952,31.6368797218294,54.689791830915));
#103600=CARTESIAN_POINT('Ctrl Pts',(8.99950573412987,31.6381599180794,54.6966249675829));
#103601=CARTESIAN_POINT('Ctrl Pts',(9.00081619383511,31.6415826321533,54.7155475315672));
#103602=CARTESIAN_POINT('Ctrl Pts',(9.0016599028148,31.643634280061,54.727652655071));
#103603=CARTESIAN_POINT('Ctrl Pts',(9.00754905743618,31.6569229221559,54.8116856160863));
#103604=CARTESIAN_POINT('Ctrl Pts',(9.0127943932279,31.6635672820153,54.8842527319199));
#103605=CARTESIAN_POINT('Ctrl Pts',(9.01908762315329,31.6658027503877,54.9708607651056));
#103606=CARTESIAN_POINT('Ctrl Pts',(9.02009528315077,31.6659874532099,54.9847127389741));
#103607=CARTESIAN_POINT('Ctrl Pts',(9.03044946508363,31.6661099731375,55.1269885512871));
#103608=CARTESIAN_POINT('Ctrl Pts',(9.03975371819533,31.6513708722469,55.2550189113104));
#103609=CARTESIAN_POINT('Ctrl Pts',(9.05003537295159,31.6172724846976,55.4005322823692));
#103610=CARTESIAN_POINT('Ctrl Pts',(9.05146704967117,31.6120987630031,55.4208729580537));
#103611=CARTESIAN_POINT('Ctrl Pts',(9.05378749781389,31.6030145318558,55.4539580287628));
#103612=CARTESIAN_POINT('Ctrl Pts',(9.05468350440069,31.5993331225526,55.4667623187593));
#103613=CARTESIAN_POINT('Ctrl Pts',(9.05628847251154,31.5924259068171,55.4897445084674));
#103614=CARTESIAN_POINT('Ctrl Pts',(9.05699917740378,31.5892551434346,55.4999380466049));
#103615=CARTESIAN_POINT('Ctrl Pts',(9.05851677195906,31.5822442987145,55.5217359139965));
#103616=CARTESIAN_POINT('Ctrl Pts',(9.05932262640994,31.5783740304096,55.5333299337659));
#103617=CARTESIAN_POINT('Ctrl Pts',(9.06083570059036,31.5708299486596,55.5551277827587));
#103618=CARTESIAN_POINT('Ctrl Pts',(9.06154373499386,31.5671835233094,55.5653400610581));
#103619=CARTESIAN_POINT('Ctrl Pts',(9.06224863102697,31.5634376784283,55.5755159647401));
#103620=CARTESIAN_POINT('',(8.82705497355655,31.6659999398532,54.9995523290613));
#103621=CARTESIAN_POINT('Ctrl Pts',(8.86797183897061,31.5634375186471,55.575516398799));
#103622=CARTESIAN_POINT('Ctrl Pts',(8.86184835557125,31.5924967353516,55.4965746523031));
#103623=CARTESIAN_POINT('Ctrl Pts',(8.85573816968857,31.6155646837455,55.4154644668671));
#103624=CARTESIAN_POINT('Ctrl Pts',(8.84631919559105,31.6421995656765,55.28484965997));
#103625=CARTESIAN_POINT('Ctrl Pts',(8.84291221592427,31.6498699883968,55.2364077125598));
#103626=CARTESIAN_POINT('Ctrl Pts',(8.83841122193728,31.6573110519839,55.1707800307525));
#103627=CARTESIAN_POINT('Ctrl Pts',(8.83725933668326,31.658969484026,55.1538376753291));
#103628=CARTESIAN_POINT('Ctrl Pts',(8.83535763833246,31.661294759191,55.125630272975));
#103629=CARTESIAN_POINT('Ctrl Pts',(8.83460332395891,31.6621073148942,55.1143788747463));
#103630=CARTESIAN_POINT('Ctrl Pts',(8.83317998162107,31.6634310863907,55.0930330850496));
#103631=CARTESIAN_POINT('Ctrl Pts',(8.83251028085413,31.6639648402148,55.082940655086));
#103632=CARTESIAN_POINT('Ctrl Pts',(8.83105713180266,31.6649277509197,55.0609391251755));
#103633=CARTESIAN_POINT('Ctrl Pts',(8.83027483098005,31.6653210400976,55.0490289545022));
#103634=CARTESIAN_POINT('Ctrl Pts',(8.82867835061849,31.665865484226,55.0245964937025));
#103635=CARTESIAN_POINT('Ctrl Pts',(8.82786462710371,31.6660033047414,55.0120747044674));
#103636=CARTESIAN_POINT('Ctrl Pts',(8.82705497355655,31.6659999398532,54.9995523290613));
#103637=CARTESIAN_POINT('Ctrl Pts',(8.82705505845663,31.6659999402055,54.9995536421544));
#103638=CARTESIAN_POINT('Ctrl Pts',(8.82553610359139,31.6659936460075,54.9760609811571));
#103639=CARTESIAN_POINT('Ctrl Pts',(8.82403175635443,31.6654904404392,54.9525700214294));
#103640=CARTESIAN_POINT('Ctrl Pts',(8.81396003855586,31.6587392066447,54.7940820609814));
#103641=CARTESIAN_POINT('Ctrl Pts',(8.80588759280819,31.6365833860729,54.6602746920782));
#103642=CARTESIAN_POINT('Ctrl Pts',(8.79388677069296,31.5817697377278,54.4736064599062));
#103643=CARTESIAN_POINT('Ctrl Pts',(8.79017179395581,31.5619953544911,54.4175442576192));
#103644=CARTESIAN_POINT('Ctrl Pts',(8.78533510573124,31.5335120722739,54.3487523994713));
#103645=CARTESIAN_POINT('Ctrl Pts',(8.78434795440504,31.5275638649981,54.3349200705605));
#103646=CARTESIAN_POINT('Ctrl Pts',(8.78285664760139,31.5183948032396,54.3143698643188));
#103647=CARTESIAN_POINT('Ctrl Pts',(8.78236052743893,31.515314849947,54.3075894558272));
#103648=CARTESIAN_POINT('Ctrl Pts',(8.78145963817243,31.5096713422155,54.2953834760889));
#103649=CARTESIAN_POINT('Ctrl Pts',(8.78105583435059,31.5071237951953,54.2899507973767));
#103650=CARTESIAN_POINT('Ctrl Pts',(8.78014062095601,31.5013096242896,54.2777242654838));
#103651=CARTESIAN_POINT('Ctrl Pts',(8.7796282258575,31.4980262302407,54.2709388004939));
#103652=CARTESIAN_POINT('Ctrl Pts',(8.77805247463645,31.4878396145204,54.2502464825534));
#103653=CARTESIAN_POINT('Ctrl Pts',(8.77698075865629,31.4807881631426,54.2364140989553));
#103654=CARTESIAN_POINT('Ctrl Pts',(8.76869598900977,31.4252696380621,54.1311687196831));
#103655=CARTESIAN_POINT('Ctrl Pts',(8.76111592793846,31.3685784785411,54.0443583821508));
#103656=CARTESIAN_POINT('Ctrl Pts',(8.74555632899655,31.2354270282251,53.8768367646623));
#103657=CARTESIAN_POINT('Ctrl Pts',(8.73763023200618,31.1581918838061,53.7973465458893));
#103658=CARTESIAN_POINT('Ctrl Pts',(8.72900065786744,31.0619743711026,53.7162558433822));
#103659=CARTESIAN_POINT('Ctrl Pts',(8.72796105483216,31.0501770810135,53.7065871696235));
#103660=CARTESIAN_POINT('Ctrl Pts',(8.72598363199649,31.0273454410484,53.6883934655784));
#103661=CARTESIAN_POINT('Ctrl Pts',(8.72504482586285,31.0163336496218,53.6798423239843));
#103662=CARTESIAN_POINT('Ctrl Pts',(8.72339295013933,30.9966566009004,53.6649543786674));
#103663=CARTESIAN_POINT('Ctrl Pts',(8.72267769972337,30.9880351360616,53.658561305787));
#103664=CARTESIAN_POINT('Ctrl Pts',(8.72118021452816,30.9697742945875,53.6452919144908));
#103665=CARTESIAN_POINT('Ctrl Pts',(8.72039872111644,30.9601221502674,53.6384341190626));
#103666=CARTESIAN_POINT('Ctrl Pts',(8.71832853385494,30.934234190799,53.6204530577542));
#103667=CARTESIAN_POINT('Ctrl Pts',(8.71704679639953,30.9178726980463,53.6095133756436));
#103668=CARTESIAN_POINT('Ctrl Pts',(8.71044161629415,30.8319045157143,53.5542118242739));
#103669=CARTESIAN_POINT('Ctrl Pts',(8.7053011840619,30.7592616308765,53.5147751583784));
#103670=CARTESIAN_POINT('Ctrl Pts',(8.69408423991596,30.5927258897614,53.439792016934));
#103671=CARTESIAN_POINT('Ctrl Pts',(8.68806591503792,30.4979543025982,53.4070115811314));
#103672=CARTESIAN_POINT('Ctrl Pts',(8.68002004403746,30.3733864048549,53.3761350176207));
#103673=CARTESIAN_POINT('Ctrl Pts',(8.6782281655632,30.3457849104645,53.3700345083538));
#103674=CARTESIAN_POINT('Ctrl Pts',(8.67516224622675,30.2991029521632,53.3609558497359));
#103675=CARTESIAN_POINT('Ctrl Pts',(8.67390451237128,30.280101087901,53.3576018737098));
#103676=CARTESIAN_POINT('Ctrl Pts',(8.67208691732575,30.2529339655181,53.353291806335));
#103677=CARTESIAN_POINT('Ctrl Pts',(8.67154109405221,30.2448124584464,53.3520648316177));
#103678=CARTESIAN_POINT('Ctrl Pts',(8.67058728555508,30.2306916733415,53.3500381882641));
#103679=CARTESIAN_POINT('Ctrl Pts',(8.6701808286422,30.2246965726348,53.3492110742926));
#103680=CARTESIAN_POINT('Ctrl Pts',(8.66930364431018,30.2118085646209,53.347504489152));
#103681=CARTESIAN_POINT('Ctrl Pts',(8.6688323909263,30.2049147267133,53.3466354812707));
#103682=CARTESIAN_POINT('Ctrl Pts',(8.66752228513739,30.185826776063,53.3443505471011));
#103683=CARTESIAN_POINT('Ctrl Pts',(8.66667868599297,30.1736224257632,53.3430262727635));
#103684=CARTESIAN_POINT('Ctrl Pts',(8.6607400783166,30.0882358483373,53.3347147727091));
#103685=CARTESIAN_POINT('Ctrl Pts',(8.65544110967738,30.0146832630126,53.3324441660386));
#103686=CARTESIAN_POINT('Ctrl Pts',(8.64909088675572,29.9273340514737,53.3355274088435));
#103687=CARTESIAN_POINT('Ctrl Pts',(8.6480792702371,29.9134445347966,53.336191869634));
#103688=CARTESIAN_POINT('Ctrl Pts',(8.64170115626646,29.8259723798899,53.3414747452173));
#103689=CARTESIAN_POINT('Ctrl Pts',(8.63633492771701,29.7527512672942,53.3507998868397));
#103690=CARTESIAN_POINT('Ctrl Pts',(8.62804290047012,29.6387091217188,53.3730924525723));
#103691=CARTESIAN_POINT('Ctrl Pts',(8.6250490546401,29.5973570852291,53.3828301107252));
#103692=CARTESIAN_POINT('Ctrl Pts',(8.61997918816134,29.5269451683638,53.4022797052534));
#103693=CARTESIAN_POINT('Ctrl Pts',(8.61788172043162,29.497699133649,53.4112315880915));
#103694=CARTESIAN_POINT('Ctrl Pts',(8.61486367308045,29.4554710290015,53.4254399215573));
#103695=CARTESIAN_POINT('Ctrl Pts',(8.61392267684296,29.44228395252,53.430062398717));
#103696=CARTESIAN_POINT('Ctrl Pts',(8.61226832343055,29.4190693113459,53.4385292780688));
#103697=CARTESIAN_POINT('Ctrl Pts',(8.61155276327038,29.4090179904489,53.4423056929766));
#103698=CARTESIAN_POINT('Ctrl Pts',(8.61005597357871,29.3879757368174,53.4504445441467));
#103699=CARTESIAN_POINT('Ctrl Pts',(8.60927547247432,29.3769932900719,53.4548273685418));
#103700=CARTESIAN_POINT('Ctrl Pts',(8.60721106582747,29.3479275418711,53.466787071259));
#103701=CARTESIAN_POINT('Ctrl Pts',(8.60593404573643,29.3299294045247,53.4745670040198));
#103702=CARTESIAN_POINT('Ctrl Pts',(8.59932454190857,29.2367812274761,53.5167983797557));
#103703=CARTESIAN_POINT('Ctrl Pts',(8.59417587667596,29.1641305092543,53.5564922479013));
#103704=CARTESIAN_POINT('Ctrl Pts',(8.58295044249539,29.0106939113296,53.6558095623349));
#103705=CARTESIAN_POINT('Ctrl Pts',(8.57693165756953,28.9317460849413,53.7176561685824));
#103706=CARTESIAN_POINT('Ctrl Pts',(8.5688852400486,28.8382373814483,53.8055701933716));
#103707=CARTESIAN_POINT('Ctrl Pts',(8.56709329829167,28.8181412185335,53.825451326926));
#103708=CARTESIAN_POINT('Ctrl Pts',(8.56402727886024,28.785194025901,53.8597479361411));
#103709=CARTESIAN_POINT('Ctrl Pts',(8.5627695090207,28.7720698560035,53.8738935185878));
#103710=CARTESIAN_POINT('Ctrl Pts',(8.56095186516394,28.7537137636402,53.8943806775853));
#103711=CARTESIAN_POINT('Ctrl Pts',(8.56040602957827,28.7482779775385,53.9005385679675));
#103712=CARTESIAN_POINT('Ctrl Pts',(8.55945220306337,28.7389164986006,53.9113030578484));
#103713=CARTESIAN_POINT('Ctrl Pts',(8.5590457405223,28.7349700120069,53.9158912612256));
#103714=CARTESIAN_POINT('Ctrl Pts',(8.55816855126101,28.7265461748394,53.9257934851969));
#103715=CARTESIAN_POINT('Ctrl Pts',(8.55769729863433,28.7220771094003,53.9311139618555));
#103716=CARTESIAN_POINT('Ctrl Pts',(8.55638719524231,28.7098048090319,53.9459112607604));
#103717=CARTESIAN_POINT('Ctrl Pts',(8.55554359775215,28.702073021989,53.9554463926474));
#103718=CARTESIAN_POINT('Ctrl Pts',(8.54960515949182,28.6487809308619,54.022673481444));
#103719=CARTESIAN_POINT('Ctrl Pts',(8.54430637170586,28.6069821324187,54.0832345327938));
#103720=CARTESIAN_POINT('Ctrl Pts',(8.53795623954585,28.5621975538289,54.1582913174384));
#103721=CARTESIAN_POINT('Ctrl Pts',(8.5369445349373,28.5552219473771,54.1703218963868));
#103722=CARTESIAN_POINT('Ctrl Pts',(8.53056636141165,28.512217831074,54.2466768334407));
#103723=CARTESIAN_POINT('Ctrl Pts',(8.52520015924222,28.4803396438246,54.3132501962001));
#103724=CARTESIAN_POINT('Ctrl Pts',(8.51690810723396,28.4372155934243,54.4211526794455));
#103725=CARTESIAN_POINT('Ctrl Pts',(8.51391421336267,28.4229683669556,54.4611762335098));
#103726=CARTESIAN_POINT('Ctrl Pts',(8.50884427917112,28.4011193705922,54.5308819288071));
#103727=CARTESIAN_POINT('Ctrl Pts',(8.50674679078772,28.3927780522181,54.5603082267925));
#103728=CARTESIAN_POINT('Ctrl Pts',(8.50372872344318,28.3818118683094,54.6034922304952));
#103729=CARTESIAN_POINT('Ctrl Pts',(8.50278772726036,28.3785431708655,54.6170783203686));
#103730=CARTESIAN_POINT('Ctrl Pts',(8.50113337778597,28.3730657096828,54.6411740056661));
#103731=CARTESIAN_POINT('Ctrl Pts',(8.50041782146082,28.370786941366,54.6516666853801));
#103732=CARTESIAN_POINT('Ctrl Pts',(8.49892104370957,28.3662121421728,54.6737592266454));
#103733=CARTESIAN_POINT('Ctrl Pts',(8.49814055066797,28.3639378412726,54.6853630163244));
#103734=CARTESIAN_POINT('Ctrl Pts',(8.4960761750838,28.3582214629008,54.7162684423323));
#103735=CARTESIAN_POINT('Ctrl Pts',(8.49479917774291,28.3549961604493,54.7356086571121));
#103736=CARTESIAN_POINT('Ctrl Pts',(8.48819039339495,28.3399575555467,54.8367601825694));
#103737=CARTESIAN_POINT('Ctrl Pts',(8.48304237366808,28.3339025974047,54.9193148422241));
#103738=CARTESIAN_POINT('Ctrl Pts',(8.47181688524308,28.3341205591325,55.1020901699696));
#103739=CARTESIAN_POINT('Ctrl Pts',(8.4657974650397,28.3432617835874,55.2019724125215));
#103740=CARTESIAN_POINT('Ctrl Pts',(8.45775027725041,28.3664082481482,55.3282270770604));
#103741=CARTESIAN_POINT('Ctrl Pts',(8.45595824904168,28.3722120477668,55.3558949680674));
#103742=CARTESIAN_POINT('Ctrl Pts',(8.45289209763865,28.3831571896435,55.4021786629869));
#103743=CARTESIAN_POINT('Ctrl Pts',(8.45163428439331,28.3879235934513,55.4208775736203));
#103744=CARTESIAN_POINT('Ctrl Pts',(8.44981659164693,28.3951802673527,55.447411550849));
#103745=CARTESIAN_POINT('Ctrl Pts',(8.44927075186763,28.397405624294,55.4553182733951));
#103746=CARTESIAN_POINT('Ctrl Pts',(8.44831692322422,28.4013720257761,55.4690215656168));
#103747=CARTESIAN_POINT('Ctrl Pts',(8.44791046283195,28.4030863358875,55.474825628007));
#103748=CARTESIAN_POINT('Ctrl Pts',(8.4470332836435,28.4068368002712,55.487273330573));
#103749=CARTESIAN_POINT('Ctrl Pts',(8.44656203899971,28.4088828710595,55.4939135119102));
#103750=CARTESIAN_POINT('Ctrl Pts',(8.44525197541004,28.4146584994855,55.5122489789224));
#103751=CARTESIAN_POINT('Ctrl Pts',(8.44440841015877,28.418475788029,55.5239158658659));
#103752=CARTESIAN_POINT('Ctrl Pts',(8.43847834899337,28.4460135369473,55.6050359240063));
#103753=CARTESIAN_POINT('Ctrl Pts',(8.43318856979112,28.4741696063173,55.6728904955669));
#103754=CARTESIAN_POINT('Ctrl Pts',(8.42684061355435,28.5129091604143,55.7512075613265));
#103755=CARTESIAN_POINT('Ctrl Pts',(8.42582217631955,28.5192737127025,55.7636763868469));
#103756=CARTESIAN_POINT('Ctrl Pts',(8.41943779376698,28.560134796905,55.8412958516943));
#103757=CARTESIAN_POINT('Ctrl Pts',(8.41407206409622,28.5987690156022,55.9041811520905));
#103758=CARTESIAN_POINT('Ctrl Pts',(8.40577891398666,28.6660352119208,55.9989489437549));
#103759=CARTESIAN_POINT('Ctrl Pts',(8.4027835333492,28.6919444326111,56.0326432986966));
#103760=CARTESIAN_POINT('Ctrl Pts',(8.39771139040445,28.7386753921521,56.0888305268553));
#103761=CARTESIAN_POINT('Ctrl Pts',(8.39561315459719,28.7588803043475,56.1118065465268));
#103762=CARTESIAN_POINT('Ctrl Pts',(8.39259422869578,28.7892216466417,56.1444505543991));
#103763=CARTESIAN_POINT('Ctrl Pts',(8.39165310491,28.7988642995752,56.1545667335652));
#103764=CARTESIAN_POINT('Ctrl Pts',(8.38999861211679,28.8161387251966,56.1722387837488));
#103765=CARTESIAN_POINT('Ctrl Pts',(8.38928303876903,28.8237182877485,56.1798443231228));
#103766=CARTESIAN_POINT('Ctrl Pts',(8.38778630448792,28.8397974140994,56.1956695797933));
#103767=CARTESIAN_POINT('Ctrl Pts',(8.38700587117656,28.8483120466164,56.2038731887268));
#103768=CARTESIAN_POINT('Ctrl Pts',(8.38494183873673,28.8711726813434,56.2254342390859));
#103769=CARTESIAN_POINT('Ctrl Pts',(8.38366512064124,28.8856685750143,56.2386305815535));
#103770=CARTESIAN_POINT('Ctrl Pts',(8.37706593008509,28.9623810134926,56.3060287464395));
#103771=CARTESIAN_POINT('Ctrl Pts',(8.37192651587782,29.0283316036291,56.3558123985024));
#103772=CARTESIAN_POINT('Ctrl Pts',(8.36070163156955,29.1819640516161,56.4547917565012));
#103773=CARTESIAN_POINT('Ctrl Pts',(8.35467498637628,29.2709417606716,56.5013572548453));
#103774=CARTESIAN_POINT('Ctrl Pts',(8.34661911115974,29.3896958950261,56.5504466517915));
#103775=CARTESIAN_POINT('Ctrl Pts',(8.3448261167064,29.4161030991972,56.5605832722019));
#103776=CARTESIAN_POINT('Ctrl Pts',(8.34175847907943,29.4609462904271,56.5764992076295));
#103777=CARTESIAN_POINT('Ctrl Pts',(8.3405001664206,29.4792485523437,56.5826390950878));
#103778=CARTESIAN_POINT('Ctrl Pts',(8.33868187673522,29.5054853486663,56.5909364384793));
#103779=CARTESIAN_POINT('Ctrl Pts',(8.33813595197105,29.5133363259476,56.5933555639042));
#103780=CARTESIAN_POINT('Ctrl Pts',(8.33718202714467,29.5270016971516,56.5974558637262));
#103781=CARTESIAN_POINT('Ctrl Pts',(8.33677555650413,29.5328078811856,56.5991635794459));
#103782=CARTESIAN_POINT('Ctrl Pts',(8.3358984170954,29.5452993124806,56.6027637238111));
#103783=CARTESIAN_POINT('Ctrl Pts',(8.33542722307885,29.5519870291935,56.6046459557121));
#103784=CARTESIAN_POINT('Ctrl Pts',(8.33411743648922,29.5705200713913,56.6097371214792));
#103785=CARTESIAN_POINT('Ctrl Pts',(8.3332741007402,29.5823891040885,56.6128570075721));
#103786=CARTESIAN_POINT('Ctrl Pts',(8.32739914873105,29.6647052897696,56.6335250811979));
#103787=CARTESIAN_POINT('Ctrl Pts',(8.32216859223985,29.736192395319,56.6465812906607));
#103788=CARTESIAN_POINT('Ctrl Pts',(8.31584409808381,29.8226801139109,56.656599950404));
#103789=CARTESIAN_POINT('Ctrl Pts',(8.31479054129817,29.837087283724,56.6580787617991));
#103790=CARTESIAN_POINT('Ctrl Pts',(8.30828554897284,29.9261080965898,56.666044762055));
#103791=CARTESIAN_POINT('Ctrl Pts',(8.30283399774223,30.0010744490843,56.6676826436863));
#103792=CARTESIAN_POINT('Ctrl Pts',(8.29449542297255,30.1178583240142,56.6623566260043));
#103793=CARTESIAN_POINT('Ctrl Pts',(8.29153546152786,30.1597316104884,56.6588569665739));
#103794=CARTESIAN_POINT('Ctrl Pts',(8.28651598891549,30.2315431115093,56.6501102955644));
#103795=CARTESIAN_POINT('Ctrl Pts',(8.2844356050796,30.261551155552,56.6456206735221));
#103796=CARTESIAN_POINT('Ctrl Pts',(8.28143720769942,30.3051371854474,56.6378770869985));
#103797=CARTESIAN_POINT('Ctrl Pts',(8.28049915137323,30.3188219848497,56.6352683622274));
#103798=CARTESIAN_POINT('Ctrl Pts',(8.27884811207615,30.3429884248197,56.6303466210606));
#103799=CARTESIAN_POINT('Ctrl Pts',(8.27813295600121,30.353483293679,56.6281034164687));
#103800=CARTESIAN_POINT('Ctrl Pts',(8.27663519437453,30.3755153415698,56.6231711382093));
#103801=CARTESIAN_POINT('Ctrl Pts',(8.27585333477465,30.3870470287705,56.6204600968204));
#103802=CARTESIAN_POINT('Ctrl Pts',(8.27378105964955,30.4176832014621,56.6129119883268));
#103803=CARTESIAN_POINT('Ctrl Pts',(8.27249762586325,30.4367328000111,56.6078584681774));
#103804=CARTESIAN_POINT('Ctrl Pts',(8.26561050712643,30.5392549450564,56.5787045584924));
#103805=CARTESIAN_POINT('Ctrl Pts',(8.26021198918261,30.6208393787416,56.548439607445));
#103806=CARTESIAN_POINT('Ctrl Pts',(8.24896487390345,30.7872638936493,56.4714215111499));
#103807=CARTESIAN_POINT('Ctrl Pts',(8.24315368639412,30.8711368192315,56.4233706845726));
#103808=CARTESIAN_POINT('Ctrl Pts',(8.2345134171551,30.9842578537331,56.3448027210113));
#103809=CARTESIAN_POINT('Ctrl Pts',(8.23188284765405,31.0172520705503,56.3200210167398));
#103810=CARTESIAN_POINT('Ctrl Pts',(8.22847293717646,31.0576364318827,56.2872748949067));
#103811=CARTESIAN_POINT('Ctrl Pts',(8.22776317725223,31.0659173145016,56.2804263902247));
#103812=CARTESIAN_POINT('Ctrl Pts',(8.22661217809893,31.0791339109638,56.2692788643662));
#103813=CARTESIAN_POINT('Ctrl Pts',(8.22617444525673,31.0841117080983,56.2650298945001));
#103814=CARTESIAN_POINT('Ctrl Pts',(8.22532202885754,31.0937081824508,56.2567402557315));
#103815=CARTESIAN_POINT('Ctrl Pts',(8.22490760163971,31.0983297747668,56.2527032210022));
#103816=CARTESIAN_POINT('Ctrl Pts',(8.22397306221718,31.1086553385317,56.2435826145211));
#103817=CARTESIAN_POINT('Ctrl Pts',(8.22345195668135,31.1143468473354,56.2384851541254));
#103818=CARTESIAN_POINT('Ctrl Pts',(8.22160692658806,31.1342735092486,56.2203897708179));
#103819=CARTESIAN_POINT('Ctrl Pts',(8.22026919250675,31.1483173356322,56.2071846605633));
#103820=CARTESIAN_POINT('Ctrl Pts',(8.2113606105704,31.2394020687851,56.1185119452913));
#103821=CARTESIAN_POINT('Ctrl Pts',(8.20343273451831,31.3091840589787,56.035963837881));
#103822=CARTESIAN_POINT('Ctrl Pts',(8.18941145024412,31.4190509845364,55.8770079186528));
#103823=CARTESIAN_POINT('Ctrl Pts',(8.18329625522762,31.4621384129286,55.8031210712222));
#103824=CARTESIAN_POINT('Ctrl Pts',(8.17529348338707,31.5124376277498,55.699275698788));
#103825=CARTESIAN_POINT('Ctrl Pts',(8.1732388582997,31.5247719209036,55.6719560035575));
#103826=CARTESIAN_POINT('Ctrl Pts',(8.17027012358035,31.5417257004153,55.6315299870337));
#103827=CARTESIAN_POINT('Ctrl Pts',(8.16933652897778,31.5469285119554,55.6186763765713));
#103828=CARTESIAN_POINT('Ctrl Pts',(8.16769050166197,31.5558694711451,55.5957694041656));
#103829=CARTESIAN_POINT('Ctrl Pts',(8.16697594118911,31.5596720925595,55.5857422360674));
#103830=CARTESIAN_POINT('Ctrl Pts',(8.16626075047351,31.5633977026734,55.5756245535268));
#103831=CARTESIAN_POINT('Ctrl Pts',(8.166256912775,31.5634176918823,55.5755702598786));
#103832=CARTESIAN_POINT('Ctrl Pts',(8.16625307517082,31.5634376782623,55.5755159651912));
#103833=CARTESIAN_POINT('Origin',(5.,30.,55.));
#103834=CARTESIAN_POINT('',(7.46827878691259,31.5634376230276,55.5755161152408));
#103835=CARTESIAN_POINT('',(7.65925614416276,31.563437678903,55.5755159634506));
#103836=CARTESIAN_POINT('',(5.,31.5634376782623,55.5755159651912));
#103837=CARTESIAN_POINT('',(8.32030902926138,31.665999673445,55.0010431112818));
#103838=CARTESIAN_POINT('Ctrl Pts',(7.65925614416276,31.563437678903,55.5755159634506));
#103839=CARTESIAN_POINT('Ctrl Pts',(7.65963159048,31.5614376460338,55.5809492215099));
#103840=CARTESIAN_POINT('Ctrl Pts',(7.66000838851873,31.559409165902,55.5863723927665));
#103841=CARTESIAN_POINT('Ctrl Pts',(7.66118870360561,31.5529906532224,55.6032634618152));
#103842=CARTESIAN_POINT('Ctrl Pts',(7.66199708032709,31.5485023898747,55.6146926875642));
#103843=CARTESIAN_POINT('Ctrl Pts',(7.66327427744762,31.5412764375556,55.6325118591142));
#103844=CARTESIAN_POINT('Ctrl Pts',(7.66373822044195,31.5386242822467,55.6389363212319));
#103845=CARTESIAN_POINT('Ctrl Pts',(7.66461086647291,31.5335868428309,55.6509255339244));
#103846=CARTESIAN_POINT('Ctrl Pts',(7.66501899500722,31.5312113248434,55.6564941197066));
#103847=CARTESIAN_POINT('Ctrl Pts',(7.66598537297125,31.5255400249626,55.6695902916737));
#103848=CARTESIAN_POINT('Ctrl Pts',(7.66654510793023,31.5222188419567,55.6771065769736));
#103849=CARTESIAN_POINT('Ctrl Pts',(7.66843020185025,31.5109083480086,55.7021999336251));
#103850=CARTESIAN_POINT('Ctrl Pts',(7.66976911520282,31.5026694377293,55.7196619097496));
#103851=CARTESIAN_POINT('Ctrl Pts',(7.6731023784322,31.4816161755155,55.762344854778));
#103852=CARTESIAN_POINT('Ctrl Pts',(7.67511132091524,31.4684595478875,55.7873897032115));
#103853=CARTESIAN_POINT('Ctrl Pts',(7.68432087457773,31.405809189489,55.8996139705159));
#103854=CARTESIAN_POINT('Ctrl Pts',(7.69169395322286,31.3491462429622,55.9825526201571));
#103855=CARTESIAN_POINT('Ctrl Pts',(7.70486795675479,31.2329021130264,56.1235257660179));
#103856=CARTESIAN_POINT('Ctrl Pts',(7.71070090930999,31.1757749373198,56.1831799307067));
#103857=CARTESIAN_POINT('Ctrl Pts',(7.71768797249666,31.099883362438,56.2514778811915));
#103858=CARTESIAN_POINT('Ctrl Pts',(7.71901887146961,31.0850809177853,56.2643337205403));
#103859=CARTESIAN_POINT('Ctrl Pts',(7.72113538275762,31.0609902010117,56.2845215645147));
#103860=CARTESIAN_POINT('Ctrl Pts',(7.72192776914359,31.0518451368708,56.2920207726157));
#103861=CARTESIAN_POINT('Ctrl Pts',(7.72343231646594,31.0342433609175,56.3061439562762));
#103862=CARTESIAN_POINT('Ctrl Pts',(7.72414512787151,31.0258009637973,56.3127847333081));
#103863=CARTESIAN_POINT('Ctrl Pts',(7.72577839130045,31.0062228416963,56.3278806659074));
#103864=CARTESIAN_POINT('Ctrl Pts',(7.7266965521399,30.9950436246061,56.3362782924647));
#103865=CARTESIAN_POINT('Ctrl Pts',(7.7296080445694,30.9590559778833,56.3626094873501));
#103866=CARTESIAN_POINT('Ctrl Pts',(7.73158070212546,30.933857630097,56.3800011228142));
#103867=CARTESIAN_POINT('Ctrl Pts',(7.73624069398871,30.8725434888767,56.4198704547853));
#103868=CARTESIAN_POINT('Ctrl Pts',(7.73890543768339,30.8360178803313,56.4416791364344));
#103869=CARTESIAN_POINT('Ctrl Pts',(7.746111352965,30.7340132570919,56.4974020469629));
#103870=CARTESIAN_POINT('Ctrl Pts',(7.75058501916957,30.6670558228482,56.5284061126924));
#103871=CARTESIAN_POINT('Ctrl Pts',(7.75594783055933,30.5852424146112,56.5598852581263));
#103872=CARTESIAN_POINT('Ctrl Pts',(7.75680266838987,30.5721572274757,56.564732182654));
#103873=CARTESIAN_POINT('Ctrl Pts',(7.7621675047063,30.4898843024883,56.5940371430003));
#103874=CARTESIAN_POINT('Ctrl Pts',(7.76673002896838,30.4192128321675,56.6140628616324));
#103875=CARTESIAN_POINT('Ctrl Pts',(7.77232427557083,30.3354539449594,56.6319244461285));
#103876=CARTESIAN_POINT('Ctrl Pts',(7.77313258334213,30.3234185255547,56.6343522211045));
#103877=CARTESIAN_POINT('Ctrl Pts',(7.77440969496384,30.3045300481083,56.6379455898641));
#103878=CARTESIAN_POINT('Ctrl Pts',(7.77487362246632,30.2976943777533,56.6392017443362));
#103879=CARTESIAN_POINT('Ctrl Pts',(7.77574625672221,30.2848897735902,56.6414720444637));
#103880=CARTESIAN_POINT('Ctrl Pts',(7.77615438917134,30.2789229137948,56.6424964716342));
#103881=CARTESIAN_POINT('Ctrl Pts',(7.77712080008715,30.2648438704207,56.6448347204768));
#103882=CARTESIAN_POINT('Ctrl Pts',(7.77768056439062,30.2567274036312,56.6461210667904));
#103883=CARTESIAN_POINT('Ctrl Pts',(7.77956586335291,30.2295080461111,56.6502287530831));
#103884=CARTESIAN_POINT('Ctrl Pts',(7.78090495626985,30.2103664672671,56.6527778891059));
#103885=CARTESIAN_POINT('Ctrl Pts',(7.78423876687398,30.1630805058365,56.6582403947546));
#103886=CARTESIAN_POINT('Ctrl Pts',(7.78624808290117,30.1348984375856,56.6607705106326));
#103887=CARTESIAN_POINT('Ctrl Pts',(7.79546095714804,30.0065889503532,56.669002543238));
#103888=CARTESIAN_POINT('Ctrl Pts',(7.80283707374235,29.906135983675,56.666374182863));
#103889=CARTESIAN_POINT('Ctrl Pts',(7.81601039326826,29.7246594348859,56.6451558201465));
#103890=CARTESIAN_POINT('Ctrl Pts',(7.82183993394843,29.6436042322961,56.6295201240762));
#103891=CARTESIAN_POINT('Ctrl Pts',(7.82882370036997,29.5451096955661,56.6028147282216));
#103892=CARTESIAN_POINT('Ctrl Pts',(7.83015450015074,29.5262820226596,56.5973514256298));
#103893=CARTESIAN_POINT('Ctrl Pts',(7.83227089236381,29.4962570743077,56.5880613697007));
#103894=CARTESIAN_POINT('Ctrl Pts',(7.83306325751763,29.4849970068625,56.5844455745345));
#103895=CARTESIAN_POINT('Ctrl Pts',(7.83456778818429,29.4635851656586,56.5773174985461));
#103896=CARTESIAN_POINT('Ctrl Pts',(7.83528060391883,29.4534270424619,56.5738263490694));
#103897=CARTESIAN_POINT('Ctrl Pts',(7.83691391060792,29.4301251991416,56.565565137015));
#103898=CARTESIAN_POINT('Ctrl Pts',(7.83783210995017,29.417006227852,56.5607273202801));
#103899=CARTESIAN_POINT('Ctrl Pts',(7.84074386437779,29.3753620795096,56.5447720429243));
#103900=CARTESIAN_POINT('Ctrl Pts',(7.84271673999939,29.3470807928504,56.5330329069656));
#103901=CARTESIAN_POINT('Ctrl Pts',(7.84737735812253,29.2803212895614,56.5031391707893));
#103902=CARTESIAN_POINT('Ctrl Pts',(7.85004250136094,29.2421830169955,56.4842771350868));
#103903=CARTESIAN_POINT('Ctrl Pts',(7.85724861653753,29.1400418520056,56.4287966740701));
#103904=CARTESIAN_POINT('Ctrl Pts',(7.8617221095835,29.0776817179599,56.3893585939889));
#103905=CARTESIAN_POINT('Ctrl Pts',(7.8670863453393,29.0068442276365,56.3376819636178));
#103906=CARTESIAN_POINT('Ctrl Pts',(7.8679427701454,28.9956548321545,56.3293013961326));
#103907=CARTESIAN_POINT('Ctrl Pts',(7.87330713273971,28.9264229477285,56.276075336891));
#103908=CARTESIAN_POINT('Ctrl Pts',(7.8778676100798,28.8712964649854,56.2275836275946));
#103909=CARTESIAN_POINT('Ctrl Pts',(7.88345958440012,28.8108869492878,56.1669262600644));
#103910=CARTESIAN_POINT('Ctrl Pts',(7.88426788362659,28.8023197858966,56.1581316103053));
#103911=CARTESIAN_POINT('Ctrl Pts',(7.88554498458273,28.7890565239385,56.1442116075763));
#103912=CARTESIAN_POINT('Ctrl Pts',(7.88600891009339,28.7842937736759,56.1391499778476));
#103913=CARTESIAN_POINT('Ctrl Pts',(7.88688154272525,28.7754416570285,56.1296236189867));
#103914=CARTESIAN_POINT('Ctrl Pts',(7.88728967556645,28.7713447778844,56.1251662083443));
#103915=CARTESIAN_POINT('Ctrl Pts',(7.88825609025736,28.7617443109088,56.1146059315397));
#103916=CARTESIAN_POINT('Ctrl Pts',(7.88881585798119,28.7562614837534,56.1084845647622));
#103917=CARTESIAN_POINT('Ctrl Pts',(7.89070118111609,28.7380474101835,56.0878439931072));
#103918=CARTESIAN_POINT('Ctrl Pts',(7.89204029524548,28.7255238784898,56.0731446447318));
#103919=CARTESIAN_POINT('Ctrl Pts',(7.89537417052015,28.6952878378115,56.0363795955823));
#103920=CARTESIAN_POINT('Ctrl Pts',(7.89738353068785,28.6778768937669,56.0140743579871));
#103921=CARTESIAN_POINT('Ctrl Pts',(7.90659679602378,28.6013673418907,55.9107362670062));
#103922=CARTESIAN_POINT('Ctrl Pts',(7.91397327037209,28.5490914909691,55.8249114052757));
#103923=CARTESIAN_POINT('Ctrl Pts',(7.92714651609673,28.4684935822616,55.6609366863721));
#103924=CARTESIAN_POINT('Ctrl Pts',(7.93297566143948,28.4376708299431,55.5843632888298));
#103925=CARTESIAN_POINT('Ctrl Pts',(7.93995904599438,28.4066890555883,55.4871349608446));
#103926=CARTESIAN_POINT('Ctrl Pts',(7.94128983442738,28.4010676185352,55.4683540670327));
#103927=CARTESIAN_POINT('Ctrl Pts',(7.94340621305111,28.392588212488,55.4380903944065));
#103928=CARTESIAN_POINT('Ctrl Pts',(7.94419857580865,28.3895189570306,55.4266692759289));
#103929=CARTESIAN_POINT('Ctrl Pts',(7.94570310465096,28.3838945651968,55.4048142654578));
#103930=CARTESIAN_POINT('Ctrl Pts',(7.94641592092891,28.3813182326309,55.3943864996689));
#103931=CARTESIAN_POINT('Ctrl Pts',(7.94804923270478,28.3756207451255,55.3703289418695));
#103932=CARTESIAN_POINT('Ctrl Pts',(7.94896743654092,28.3725699378383,55.3566831946801));
#103933=CARTESIAN_POINT('Ctrl Pts',(7.95187922135973,28.3633882966704,55.3130420953412));
#103934=CARTESIAN_POINT('Ctrl Pts',(7.95385212225296,28.357912056782,55.2829144681088));
#103935=CARTESIAN_POINT('Ctrl Pts',(7.95851281304256,28.3468190423902,55.210612440084));
#103936=CARTESIAN_POINT('Ctrl Pts',(7.96117800267659,28.3419810253693,55.1683399499645));
#103937=CARTESIAN_POINT('Ctrl Pts',(7.96838413995461,28.3331951505188,55.0524356415399));
#103938=CARTESIAN_POINT('Ctrl Pts',(7.97285761186704,28.332507077862,54.9786547129672));
#103939=CARTESIAN_POINT('Ctrl Pts',(7.97822200202179,28.3375034759265,54.8911110165375));
#103940=CARTESIAN_POINT('Ctrl Pts',(7.97907860112277,28.338475890721,54.8771621738888));
#103941=CARTESIAN_POINT('Ctrl Pts',(7.98444290711716,28.3456450689222,54.7901306500289));
#103942=CARTESIAN_POINT('Ctrl Pts',(7.98900315506913,28.3564861301249,54.7175202272039));
#103943=CARTESIAN_POINT('Ctrl Pts',(7.99459487478488,28.3746822581407,54.6338729981434));
#103944=CARTESIAN_POINT('Ctrl Pts',(7.99540317319719,28.377424503538,54.6219054615397));
#103945=CARTESIAN_POINT('Ctrl Pts',(7.99668027322735,28.38192578622,54.6032127222205));
#103946=CARTESIAN_POINT('Ctrl Pts',(7.99714419864135,28.3835951376044,54.5964660837598));
#103947=CARTESIAN_POINT('Ctrl Pts',(7.99801683169108,28.3867975795262,54.5838622745005));
#103948=CARTESIAN_POINT('Ctrl Pts',(7.99842496505287,28.3883204469311,54.5780027612128));
#103949=CARTESIAN_POINT('Ctrl Pts',(7.99939138163754,28.3919856559909,54.5642094494099));
#103950=CARTESIAN_POINT('Ctrl Pts',(7.99995115074493,28.3941548008729,54.5562830588268));
#103951=CARTESIAN_POINT('Ctrl Pts',(8.00183648090793,28.4016172170938,54.5297858203319));
#103952=CARTESIAN_POINT('Ctrl Pts',(8.0031756007797,28.4071744942746,54.5112917800015));
#103953=CARTESIAN_POINT('Ctrl Pts',(8.00650949305517,28.4216635586059,54.4659488984786));
#103954=CARTESIAN_POINT('Ctrl Pts',(8.00851886462424,28.430960153971,54.4392235007593));
#103955=CARTESIAN_POINT('Ctrl Pts',(8.01773223287277,28.4762835290226,54.3188963137295));
#103956=CARTESIAN_POINT('Ctrl Pts',(8.0251088010293,28.5200369046607,54.2284276963778));
#103957=CARTESIAN_POINT('Ctrl Pts',(8.03828200312867,28.6140860174395,54.0717805433387));
#103958=CARTESIAN_POINT('Ctrl Pts',(8.04411102165076,28.6617006017761,54.0043558239765));
#103959=CARTESIAN_POINT('Ctrl Pts',(8.05109428420104,28.7265818096801,53.9255948872316));
#103960=CARTESIAN_POINT('Ctrl Pts',(8.05242506928609,28.7393115561493,53.9106860240202));
#103961=CARTESIAN_POINT('Ctrl Pts',(8.0545414443727,28.7601384195485,53.8871482086335));
#103962=CARTESIAN_POINT('Ctrl Pts',(8.05533380688427,28.7680691399381,53.8783751889618));
#103963=CARTESIAN_POINT('Ctrl Pts',(8.05683833638183,28.783380020198,53.8617965072268));
#103964=CARTESIAN_POINT('Ctrl Pts',(8.05755115354964,28.7907435373651,53.8539763601888));
#103965=CARTESIAN_POINT('Ctrl Pts',(8.05918446897586,28.8078652608931,53.8361416521534));
#103966=CARTESIAN_POINT('Ctrl Pts',(8.06010267554918,28.8176750265233,53.8261775403098));
#103967=CARTESIAN_POINT('Ctrl Pts',(8.06301447597311,28.8493601880155,53.7947941021487));
#103968=CARTESIAN_POINT('Ctrl Pts',(8.06498738944223,28.8717017492147,53.7738529945338));
#103969=CARTESIAN_POINT('Ctrl Pts',(8.06964811551408,28.92642981198,53.7253188786076));
#103970=CARTESIAN_POINT('Ctrl Pts',(8.07231332739492,28.9593211036829,53.6983269515445));
#103971=CARTESIAN_POINT('Ctrl Pts',(8.07951947700207,29.051932462727,53.6280831556815));
#103972=CARTESIAN_POINT('Ctrl Pts',(8.08399294042461,29.1135457644703,53.5874890672456));
#103973=CARTESIAN_POINT('Ctrl Pts',(8.08935742332851,29.1898062382662,53.5442055029688));
#103974=CARTESIAN_POINT('Ctrl Pts',(8.09021412316998,29.2020541217334,53.5374563533158));
#103975=CARTESIAN_POINT('Ctrl Pts',(8.09557840540333,29.2790611418513,53.4962772073723));
#103976=CARTESIAN_POINT('Ctrl Pts',(8.100138529637,29.3459422554202,53.4660049473089));
#103977=CARTESIAN_POINT('Ctrl Pts',(8.10573011210905,29.4260848868553,53.4359257734126));
#103978=CARTESIAN_POINT('Ctrl Pts',(8.10653841020586,29.4376266254109,53.4317388899915));
#103979=CARTESIAN_POINT('Ctrl Pts',(8.10781550993127,29.4557725380248,53.42538234014));
#103980=CARTESIAN_POINT('Ctrl Pts',(8.10827943536346,29.462346078788,53.4231256988139));
#103981=CARTESIAN_POINT('Ctrl Pts',(8.10915206783548,29.474671968237,53.4189803559276));
#103982=CARTESIAN_POINT('Ctrl Pts',(8.10956020059574,29.4804207402492,53.4170817948946));
#103983=CARTESIAN_POINT('Ctrl Pts',(8.1105266154132,29.4939969540745,53.4126801041525));
#103984=CARTESIAN_POINT('Ctrl Pts',(8.11108638334695,29.5018327092095,53.4102035106509));
#103985=CARTESIAN_POINT('Ctrl Pts',(8.11297170966746,29.5281414838758,53.4021018697337));
#103986=CARTESIAN_POINT('Ctrl Pts',(8.11431082685165,29.5466931610663,53.3967402817212));
#103987=CARTESIAN_POINT('Ctrl Pts',(8.11764471193652,29.5926459342696,53.3843208354584));
#103988=CARTESIAN_POINT('Ctrl Pts',(8.11965407898041,29.6201411785841,53.3776364178605));
#103989=CARTESIAN_POINT('Ctrl Pts',(8.12886740901152,29.7458145175515,53.3504534683223));
#103990=CARTESIAN_POINT('Ctrl Pts',(8.13624394312168,29.845550915368,53.3381456237804));
#103991=CARTESIAN_POINT('Ctrl Pts',(8.14941717408802,30.0281661795857,53.3322003346614));
#103992=CARTESIAN_POINT('Ctrl Pts',(8.15524625111241,30.1106378609247,53.3356346558013));
#103993=CARTESIAN_POINT('Ctrl Pts',(8.16222956843385,30.2119983827531,53.347427181732));
#103994=CARTESIAN_POINT('Ctrl Pts',(8.1635603538566,30.2314281299664,53.3500359665824));
#103995=CARTESIAN_POINT('Ctrl Pts',(8.16567672825,30.2624990063343,53.3547674573025));
#103996=CARTESIAN_POINT('Ctrl Pts',(8.16646908975953,30.2741709254493,53.3566722286782));
#103997=CARTESIAN_POINT('Ctrl Pts',(8.16797361654901,30.2964034297831,53.3605438790621));
#103998=CARTESIAN_POINT('Ctrl Pts',(8.16868643201802,30.306967158092,53.3624889195073));
#103999=CARTESIAN_POINT('Ctrl Pts',(8.17031974235481,30.3312370056854,53.3672007059445));
#104000=CARTESIAN_POINT('Ctrl Pts',(8.17123794555848,30.3449287044924,53.3700381301506));
#104001=CARTESIAN_POINT('Ctrl Pts',(8.17414972987248,30.3884799510167,53.3796369083406));
#104002=CARTESIAN_POINT('Ctrl Pts',(8.17612263085626,30.4181905599041,53.3870492675355));
#104003=CARTESIAN_POINT('Ctrl Pts',(8.18078332244457,30.4886482006191,53.4067053581101));
#104004=CARTESIAN_POINT('Ctrl Pts',(8.18344851273002,30.5291640231085,53.4196991751695));
#104005=CARTESIAN_POINT('Ctrl Pts',(8.19065465245124,30.6384078458108,53.4594081231101));
#104006=CARTESIAN_POINT('Ctrl Pts',(8.19512812596855,30.7059297372772,53.489155375738));
#104007=CARTESIAN_POINT('Ctrl Pts',(8.20459019166356,30.8430245666284,53.5607569553848));
#104008=CARTESIAN_POINT('Ctrl Pts',(8.20957425962665,30.9119530789412,53.6034150939223));
#104009=CARTESIAN_POINT('Ctrl Pts',(8.21586588284626,30.9905750436725,53.6603814656874));
#104010=CARTESIAN_POINT('Ctrl Pts',(8.21692241484219,31.0035117618374,53.6700448009833));
#104011=CARTESIAN_POINT('Ctrl Pts',(8.21850515162858,31.02246010189,53.6846324954647));
#104012=CARTESIAN_POINT('Ctrl Pts',(8.21902203001787,31.0285814445675,53.6894136663841));
#104013=CARTESIAN_POINT('Ctrl Pts',(8.21994425270688,31.0393802837109,53.6979705230566));
#104014=CARTESIAN_POINT('Ctrl Pts',(8.2203483954664,31.0440711053927,53.7017289737103));
#104015=CARTESIAN_POINT('Ctrl Pts',(8.22122422841557,31.0541465867422,53.7098917244783));
#104016=CARTESIAN_POINT('Ctrl Pts',(8.22169647569926,31.059523986063,53.7143043488144));
#104017=CARTESIAN_POINT('Ctrl Pts',(8.22301300035022,31.074366712232,53.7266404506612));
#104018=CARTESIAN_POINT('Ctrl Pts',(8.2238620600468,31.0837716269391,53.7346354625719));
#104019=CARTESIAN_POINT('Ctrl Pts',(8.22585941747524,31.1055272088131,53.7535501006916));
#104020=CARTESIAN_POINT('Ctrl Pts',(8.22701241427171,31.1178062031414,53.7645498763099));
#104021=CARTESIAN_POINT('Ctrl Pts',(8.23090037176596,31.1583448860011,53.80196435963));
#104022=CARTESIAN_POINT('Ctrl Pts',(8.23367346168671,31.1858463297726,53.8291796121029));
#104023=CARTESIAN_POINT('Ctrl Pts',(8.24157338291223,31.260819089416,53.9087254589146));
#104024=CARTESIAN_POINT('Ctrl Pts',(8.24674141994125,31.3059463004509,53.9631541828364));
#104025=CARTESIAN_POINT('Ctrl Pts',(8.25869915466466,31.4030484747042,54.0967065416247));
#104026=CARTESIAN_POINT('Ctrl Pts',(8.2654185770515,31.4520193026704,54.177729112473));
#104027=CARTESIAN_POINT('Ctrl Pts',(8.27325583122943,31.5026906660689,54.2803649597529));
#104028=CARTESIAN_POINT('Ctrl Pts',(8.2746104905053,31.5111988111378,54.2984074955985));
#104029=CARTESIAN_POINT('Ctrl Pts',(8.27675548501441,31.5242621508798,54.3274507632539));
#104030=CARTESIAN_POINT('Ctrl Pts',(8.27755292125273,31.5290267873699,54.3383545687644));
#104031=CARTESIAN_POINT('Ctrl Pts',(8.27906145396482,31.5378625644788,54.3591804274129));
#104032=CARTESIAN_POINT('Ctrl Pts',(8.27977325974764,31.5419554960087,54.3690925191919));
#104033=CARTESIAN_POINT('Ctrl Pts',(8.28139642352814,31.5511111355222,54.3918866878254));
#104034=CARTESIAN_POINT('Ctrl Pts',(8.28230558977907,31.5561096327392,54.404793829628));
#104035=CARTESIAN_POINT('Ctrl Pts',(8.28515654498737,31.5713647523713,54.4456919408238));
#104036=CARTESIAN_POINT('Ctrl Pts',(8.2870788921486,31.5810316497581,54.4738976270498));
#104037=CARTESIAN_POINT('Ctrl Pts',(8.29851342700332,31.6345903129926,54.6450113106569));
#104038=CARTESIAN_POINT('Ctrl Pts',(8.30738782332018,31.6598381214884,54.7930240966322));
#104039=CARTESIAN_POINT('Ctrl Pts',(8.3178623416834,31.6656802062543,54.9619538784274));
#104040=CARTESIAN_POINT('Ctrl Pts',(8.31908056412801,31.6660119108601,54.9814981883682));
#104041=CARTESIAN_POINT('Ctrl Pts',(8.32030902926138,31.665999673445,55.0010431112818));
#104042=CARTESIAN_POINT('Ctrl Pts',(8.32030918176878,31.665999671924,55.0010455376788));
#104043=CARTESIAN_POINT('Ctrl Pts',(8.32194772557573,31.6659833115337,55.0271148085817));
#104044=CARTESIAN_POINT('Ctrl Pts',(8.32360410126614,31.6653550622253,55.0531790328534));
#104045=CARTESIAN_POINT('Ctrl Pts',(8.32632096570275,31.663353304605,55.0952302538716));
#104046=CARTESIAN_POINT('Ctrl Pts',(8.32736521618276,31.6623599366694,55.1112313530609));
#104047=CARTESIAN_POINT('Ctrl Pts',(8.32888514943137,31.6605977381666,55.1342416336321));
#104048=CARTESIAN_POINT('Ctrl Pts',(8.32935150877709,31.6600150430196,55.1412647049778));
#104049=CARTESIAN_POINT('Ctrl Pts',(8.3301984943843,31.6588816762545,55.1539477901932));
#104050=CARTESIAN_POINT('Ctrl Pts',(8.33057828611858,31.6583465443042,55.1596091304013));
#104051=CARTESIAN_POINT('Ctrl Pts',(8.331364323057,31.6571840392508,55.1712701061304));
#104052=CARTESIAN_POINT('Ctrl Pts',(8.33177078463885,31.6565530628952,55.1772691024171));
#104053=CARTESIAN_POINT('Ctrl Pts',(8.33271294974264,31.655021827187,55.1911046102106));
#104054=CARTESIAN_POINT('Ctrl Pts',(8.33324989138303,31.6540984780162,55.1989382799917));
#104055=CARTESIAN_POINT('Ctrl Pts',(8.33496704599849,31.6509841690874,55.2238376950734));
#104056=CARTESIAN_POINT('Ctrl Pts',(8.33615772225577,31.6485845261539,55.2408755760136));
#104057=CARTESIAN_POINT('Ctrl Pts',(8.34123780411159,31.6373256422381,55.3127376313061));
#104058=CARTESIAN_POINT('Ctrl Pts',(8.34522559574536,31.6259924777415,55.367134109977));
#104059=CARTESIAN_POINT('Ctrl Pts',(8.35316770311035,31.5983070033082,55.4731747447218));
#104060=CARTESIAN_POINT('Ctrl Pts',(8.35711503915216,31.5821109667713,55.5247883994072));
#104061=CARTESIAN_POINT('Ctrl Pts',(8.36103882979909,31.5634376856231,55.5755159451947));
#104062=CARTESIAN_POINT('Ctrl Pts',(8.16625307517082,31.5634376782623,55.5755159651912));
#104063=CARTESIAN_POINT('Ctrl Pts',(8.1654689857109,31.5675212442298,55.5644226136918));
#104064=CARTESIAN_POINT('Ctrl Pts',(8.16468883772099,31.5714867118766,55.5532858795883));
#104065=CARTESIAN_POINT('Ctrl Pts',(8.16260806743168,31.5817969750552,55.5233248517541));
#104066=CARTESIAN_POINT('Ctrl Pts',(8.16131461585613,31.5879243263064,55.5044273578505));
#104067=CARTESIAN_POINT('Ctrl Pts',(8.15400399036986,31.6208982766069,55.3961694593425));
#104068=CARTESIAN_POINT('Ctrl Pts',(8.14822701968199,31.6405400220761,55.3047836819981));
#104069=CARTESIAN_POINT('Ctrl Pts',(8.13814300282262,31.6615214613163,55.1414169030305));
#104070=CARTESIAN_POINT('Ctrl Pts',(8.13381644262068,31.6660544910231,55.0701010364573));
#104071=CARTESIAN_POINT('Ctrl Pts',(8.12585887029341,31.6659555137899,54.9416043706985));
#104072=CARTESIAN_POINT('Ctrl Pts',(8.12226599904631,31.6629747266091,54.8845381260349));
#104073=CARTESIAN_POINT('Ctrl Pts',(8.11775192226371,31.6558348957875,54.8158541241578));
#104074=CARTESIAN_POINT('Ctrl Pts',(8.116964457239,31.6544709846876,54.8039779442338));
#104075=CARTESIAN_POINT('Ctrl Pts',(8.1157132948838,31.6521214343764,54.7852954399317));
#104076=CARTESIAN_POINT('Ctrl Pts',(8.11525415990859,31.6512212179353,54.7784785174439));
#104077=CARTESIAN_POINT('Ctrl Pts',(8.11438520856184,31.6494469295648,54.7656548029881));
#104078=CARTESIAN_POINT('Ctrl Pts',(8.11397590597296,31.6485821958361,54.7596469606278));
#104079=CARTESIAN_POINT('Ctrl Pts',(8.11299940032779,31.6464503390475,54.745388614632));
#104080=CARTESIAN_POINT('Ctrl Pts',(8.11243061602187,31.6451540150343,54.7371427461048));
#104081=CARTESIAN_POINT('Ctrl Pts',(8.1104809578297,31.6405237814545,54.709066905393));
#104082=CARTESIAN_POINT('Ctrl Pts',(8.10908528283463,31.6368929876308,54.6892885564858));
#104083=CARTESIAN_POINT('Ctrl Pts',(8.10557742183999,31.6269706917297,54.6402531997301));
#104084=CARTESIAN_POINT('Ctrl Pts',(8.10344875669529,31.6202472823083,54.611091361287));
#104085=CARTESIAN_POINT('Ctrl Pts',(8.09308104129543,31.5840151716182,54.4712564451794));
#104086=CARTESIAN_POINT('Ctrl Pts',(8.08463859021491,31.5439310907534,54.3636407458044));
#104087=CARTESIAN_POINT('Ctrl Pts',(8.07164485655367,31.4633667547676,54.2008673942762));
#104088=CARTESIAN_POINT('Ctrl Pts',(8.06693618237087,31.4300063988784,54.1425975605253));
#104089=CARTESIAN_POINT('Ctrl Pts',(8.06106914896445,31.3829351224479,54.0708077848959));
#104090=CARTESIAN_POINT('Ctrl Pts',(8.05979718372886,31.3723872133398,54.0552984005117));
#104091=CARTESIAN_POINT('Ctrl Pts',(8.0577515382181,31.3548699013491,54.0304541709546));
#104092=CARTESIAN_POINT('Ctrl Pts',(8.05697186744231,31.3480608094352,54.0210088712497));
#104093=CARTESIAN_POINT('Ctrl Pts',(8.05547689974625,31.3347509474218,54.0029481627606));
#104094=CARTESIAN_POINT('Ctrl Pts',(8.05476110354745,31.3282644069587,53.9943230477293));
#104095=CARTESIAN_POINT('Ctrl Pts',(8.05309976503262,31.3129465568645,53.9743617523121));
#104096=CARTESIAN_POINT('Ctrl Pts',(8.05215679196557,31.3040513940417,53.9630754803865));
#104097=CARTESIAN_POINT('Ctrl Pts',(8.04907205991135,31.2743030595855,53.9263188524834));
#104098=CARTESIAN_POINT('Ctrl Pts',(8.04695473140637,31.2528402793171,53.9013503924657));
#104099=CARTESIAN_POINT('Ctrl Pts',(8.04187226920585,31.1989388084011,53.8422802082121));
#104100=CARTESIAN_POINT('Ctrl Pts',(8.03893601871442,31.1657677515346,53.8088848029491));
#104101=CARTESIAN_POINT('Ctrl Pts',(8.03183109530371,31.0813128232839,53.7307714702887));
#104102=CARTESIAN_POINT('Ctrl Pts',(8.02770383043196,31.0286208109519,53.6877051010575));
#104103=CARTESIAN_POINT('Ctrl Pts',(8.02330839097962,30.9703415362762,53.6457445147084));
#104104=CARTESIAN_POINT('Ctrl Pts',(8.02307428604218,30.9672312328613,53.6435213387096));
#104105=CARTESIAN_POINT('Ctrl Pts',(8.01786325416568,30.8978654754573,53.5943001068665));
#104106=CARTESIAN_POINT('Ctrl Pts',(8.01284055411631,30.828276649342,53.5522055090314));
#104107=CARTESIAN_POINT('Ctrl Pts',(8.00673014466067,30.7449018940282,53.5097551631353));
#104108=CARTESIAN_POINT('Ctrl Pts',(8.0059172404046,30.7338353469973,53.5042747020569));
#104109=CARTESIAN_POINT('Ctrl Pts',(8.00463451755969,30.7164339056545,53.4958966232369));
#104110=CARTESIAN_POINT('Ctrl Pts',(8.00416964681807,30.7101397647097,53.4929147272504));
#104111=CARTESIAN_POINT('Ctrl Pts',(8.00329646715863,30.6983448255102,53.4874170794146));
#104112=CARTESIAN_POINT('Ctrl Pts',(8.00288874618628,30.6928487860687,53.4848917061889));
#104113=CARTESIAN_POINT('Ctrl Pts',(8.00192499500437,30.6798830351813,53.4790193765771));
#104114=CARTESIAN_POINT('Ctrl Pts',(8.0013675017544,30.6724022788147,53.4756974818622));
#104115=CARTESIAN_POINT('Ctrl Pts',(7.99949736146867,30.6473623553941,53.4647984763812));
#104116=CARTESIAN_POINT('Ctrl Pts',(7.99817143679796,30.6296979525992,53.4574689149167));
#104117=CARTESIAN_POINT('Ctrl Pts',(7.99487752301475,30.58594264874,53.4401901383625));
#104118=CARTESIAN_POINT('Ctrl Pts',(7.99289534718539,30.5597207339902,53.4305898824676));
#104119=CARTESIAN_POINT('Ctrl Pts',(7.98391876482938,30.4409895401603,53.3904745019434));
#104120=CARTESIAN_POINT('Ctrl Pts',(7.97675825528527,30.3461520196638,53.3674489068411));
#104121=CARTESIAN_POINT('Ctrl Pts',(7.96353282865088,30.1650345494987,53.3399764974163));
#104122=CARTESIAN_POINT('Ctrl Pts',(7.95745689652306,30.0793459343204,53.3336798727251));
#104123=CARTESIAN_POINT('Ctrl Pts',(7.95023686437213,29.9738569247563,53.3340888317368));
#104124=CARTESIAN_POINT('Ctrl Pts',(7.94890033864265,29.9541747406982,53.3345140096057));
#104125=CARTESIAN_POINT('Ctrl Pts',(7.94677724438336,29.9226722503671,53.3357534361846));
#104126=CARTESIAN_POINT('Ctrl Pts',(7.94598382328304,29.9108455841279,53.3363450752348));
#104127=CARTESIAN_POINT('Ctrl Pts',(7.94447876027205,29.8883130992987,53.3377132543517));
#104128=CARTESIAN_POINT('Ctrl Pts',(7.94376645311238,29.8776065655324,53.3384672603463));
#104129=CARTESIAN_POINT('Ctrl Pts',(7.94213638941917,29.8530130060767,53.3404382716168));
#104130=CARTESIAN_POINT('Ctrl Pts',(7.94122089630504,29.8391323503871,53.3417262211645));
#104131=CARTESIAN_POINT('Ctrl Pts',(7.93832645307775,29.7950500179682,53.3463752370039));
#104132=CARTESIAN_POINT('Ctrl Pts',(7.93636783144652,29.7649223644249,53.3503885179102));
#104133=CARTESIAN_POINT('Ctrl Pts',(7.93174786958889,29.6933554502602,53.361922594837));
#104134=CARTESIAN_POINT('Ctrl Pts',(7.92910857597325,29.6520580891277,53.3701947161593));
#104135=CARTESIAN_POINT('Ctrl Pts',(7.92182834702889,29.537915408683,53.3975952555952));
#104136=CARTESIAN_POINT('Ctrl Pts',(7.91726069360868,29.465989456128,53.4201087851613));
#104137=CARTESIAN_POINT('Ctrl Pts',(7.91182546623245,29.3832075900958,53.4523221870205));
#104138=CARTESIAN_POINT('Ctrl Pts',(7.91099544123318,29.3706443366304,53.457388275337));
#104139=CARTESIAN_POINT('Ctrl Pts',(7.90567968819271,29.2907998741095,53.4907230292039));
#104140=CARTESIAN_POINT('Ctrl Pts',(7.90114104059178,29.2253837157161,53.5232303091945));
#104141=CARTESIAN_POINT('Ctrl Pts',(7.89557344041552,29.1517081007515,53.5660866471952));
#104142=CARTESIAN_POINT('Ctrl Pts',(7.89476538875152,29.1411674520313,53.5723749503135));
#104143=CARTESIAN_POINT('Ctrl Pts',(7.89348868359969,29.1247704703638,53.5824043082926));
#104144=CARTESIAN_POINT('Ctrl Pts',(7.89302490339176,29.1188661852279,53.5860666667806));
#104145=CARTESIAN_POINT('Ctrl Pts',(7.89215255437734,29.1078619074573,53.5929881823327));
#104146=CARTESIAN_POINT('Ctrl Pts',(7.89174455957917,29.1027565440904,53.5962383366924));
#104147=CARTESIAN_POINT('Ctrl Pts',(7.89077850427102,29.0907635966205,53.6039653858493));
#104148=CARTESIAN_POINT('Ctrl Pts',(7.89021895922887,29.0838912910393,53.6084654846419));
#104149=CARTESIAN_POINT('Ctrl Pts',(7.88833455896171,29.0609847291038,53.6237083067728));
#104150=CARTESIAN_POINT('Ctrl Pts',(7.8869961590687,29.0451045840916,53.6346783642134));
#104151=CARTESIAN_POINT('Ctrl Pts',(7.88366429711673,29.0064383045922,53.6623936924725));
#104152=CARTESIAN_POINT('Ctrl Pts',(7.8816562540726,28.9838814840546,53.6794476694942));
#104153=CARTESIAN_POINT('Ctrl Pts',(7.87245368498565,28.883438273511,53.7594847953962));
#104154=CARTESIAN_POINT('Ctrl Pts',(7.86508685287616,28.8108946114786,53.8288395110735));
#104155=CARTESIAN_POINT('Ctrl Pts',(7.85191064759957,28.6907075943827,53.9664968781553));
#104156=CARTESIAN_POINT('Ctrl Pts',(7.8460699207212,28.6410898827901,54.0326622629877));
#104157=CARTESIAN_POINT('Ctrl Pts',(7.83907560558779,28.586015027664,54.1187583868265));
#104158=CARTESIAN_POINT('Ctrl Pts',(7.83774473231254,28.5757434266787,54.1354576048071));
#104159=CARTESIAN_POINT('Ctrl Pts',(7.83562841568059,28.5597527033934,54.1625135695074));
#104160=CARTESIAN_POINT('Ctrl Pts',(7.83483619698365,28.5538452411562,54.1727562495912));
#104161=CARTESIAN_POINT('Ctrl Pts',(7.83333206963248,28.5427822325502,54.1924186357606));
#104162=CARTESIAN_POINT('Ctrl Pts',(7.83261950983348,28.5376077585574,54.2018269467011));
#104163=CARTESIAN_POINT('Ctrl Pts',(7.83098697502548,28.5259090781151,54.2235933933471));
#104164=CARTESIAN_POINT('Ctrl Pts',(7.83006928771538,28.5194486209281,54.235985014234));
#104165=CARTESIAN_POINT('Ctrl Pts',(7.82715999420424,28.499348342297,54.2757514645404));
#104166=CARTESIAN_POINT('Ctrl Pts',(7.82518902217089,28.4863055795109,54.3034221304657));
#104167=CARTESIAN_POINT('Ctrl Pts',(7.82053366010357,28.4569860168231,54.3703429413191));
#104168=CARTESIAN_POINT('Ctrl Pts',(7.81787180120431,28.4414340112721,54.4098876361963));
#104169=CARTESIAN_POINT('Ctrl Pts',(7.81066718054126,28.4030696126762,54.519578403903));
#104170=CARTESIAN_POINT('Ctrl Pts',(7.80619212603821,28.3833754575499,54.5907115595036));
#104171=CARTESIAN_POINT('Ctrl Pts',(7.80083999972846,28.365674043276,54.6763891874583));
#104172=CARTESIAN_POINT('Ctrl Pts',(7.79999715780075,28.3630573359335,54.6898967919067));
#104173=CARTESIAN_POINT('Ctrl Pts',(7.79462855671414,28.3474981570939,54.7759069487567));
#104174=CARTESIAN_POINT('Ctrl Pts',(7.79005037509517,28.3392096945153,54.849159523034));
#104175=CARTESIAN_POINT('Ctrl Pts',(7.78443889153302,28.3352242827534,54.9349729039652));
#104176=CARTESIAN_POINT('Ctrl Pts',(7.7836306765562,28.3347903296891,54.94724164423));
#104177=CARTESIAN_POINT('Ctrl Pts',(7.78235376890748,28.3343231527469,54.9664601267501));
#104178=CARTESIAN_POINT('Ctrl Pts',(7.78188995201852,28.3341977561378,54.9734074720215));
#104179=CARTESIAN_POINT('Ctrl Pts',(7.78101757531465,28.334044459824,54.9864070663611));
#104180=CARTESIAN_POINT('Ctrl Pts',(7.78060958997865,28.3340060751918,54.9924589446918));
#104181=CARTESIAN_POINT('Ctrl Pts',(7.77964361330082,28.3339933235609,55.0067244867441));
#104182=CARTESIAN_POINT('Ctrl Pts',(7.7790841381583,28.3340467243174,55.0149378993074));
#104183=CARTESIAN_POINT('Ctrl Pts',(7.77720022499056,28.3344289637405,55.0424428408602));
#104184=CARTESIAN_POINT('Ctrl Pts',(7.77586225146258,28.335032185937,55.0617281979107));
#104185=CARTESIAN_POINT('Ctrl Pts',(7.77253168870701,28.3373442259207,55.1092271396294));
#104186=CARTESIAN_POINT('Ctrl Pts',(7.77052453208001,28.3394363660621,55.1374155321467));
#104187=CARTESIAN_POINT('Ctrl Pts',(7.76132982801723,28.352186751437,55.2651043857725));
#104188=CARTESIAN_POINT('Ctrl Pts',(7.75397018978691,28.3710792193116,55.3635744377672));
#104189=CARTESIAN_POINT('Ctrl Pts',(7.74079234931782,28.4215131404336,55.5392335084213));
#104190=CARTESIAN_POINT('Ctrl Pts',(7.73494352531683,28.450220534493,55.6169123619868));
#104191=CARTESIAN_POINT('Ctrl Pts',(7.7279413928737,28.4927292041249,55.7099825073175));
#104192=CARTESIAN_POINT('Ctrl Pts',(7.72661028936251,28.5011892805688,55.7276722456543));
#104193=CARTESIAN_POINT('Ctrl Pts',(7.72449369664643,28.5152490291249,55.7557846040994));
#104194=CARTESIAN_POINT('Ctrl Pts',(7.72370142896215,28.520650627779,55.7663036347916));
#104195=CARTESIAN_POINT('Ctrl Pts',(7.72219726366893,28.5311698397171,55.7862628301204));
#104196=CARTESIAN_POINT('Ctrl Pts',(7.72148471433916,28.5362675973549,55.7957127248184));
#104197=CARTESIAN_POINT('Ctrl Pts',(7.71985228109367,28.5482087299234,55.8173452964194));
#104198=CARTESIAN_POINT('Ctrl Pts',(7.71893468387943,28.5551147847291,55.8294925917958));
#104199=CARTESIAN_POINT('Ctrl Pts',(7.71602600126338,28.5776175765787,55.8679395633482));
#104200=CARTESIAN_POINT('Ctrl Pts',(7.7140555374062,28.5937863325539,55.8938982903509));
#104201=CARTESIAN_POINT('Ctrl Pts',(7.70940163380587,28.6340932381776,55.9548076085145));
#104202=CARTESIAN_POINT('Ctrl Pts',(7.70674070511053,28.6588713621722,55.9893094596976));
#104203=CARTESIAN_POINT('Ctrl Pts',(7.69953660422257,28.7302092053187,56.0810290057603));
#104204=CARTESIAN_POINT('Ctrl Pts',(7.69506119862694,28.7792910431705,56.136161249065));
#104205=CARTESIAN_POINT('Ctrl Pts',(7.68971384706615,28.8416141478796,56.1974494682131));
#104206=CARTESIAN_POINT('Ctrl Pts',(7.68887610742027,28.8514822141496,56.2069175205105));
#104207=CARTESIAN_POINT('Ctrl Pts',(7.68350640208746,28.9153086857956,56.266664988286));
#104208=CARTESIAN_POINT('Ctrl Pts',(7.67892205798069,28.9724326667835,56.3134298829397));
#104209=CARTESIAN_POINT('Ctrl Pts',(7.67330373076348,29.0424519722074,56.3633812731262));
#104210=CARTESIAN_POINT('Ctrl Pts',(7.67249549090482,29.0525244255663,56.3704002099891));
#104211=CARTESIAN_POINT('Ctrl Pts',(7.67121855238707,29.0684177150572,56.3812163951233));
#104212=CARTESIAN_POINT('Ctrl Pts',(7.67075472989186,29.074186541949,56.3850897878103));
#104213=CARTESIAN_POINT('Ctrl Pts',(7.66988234892712,29.0850249786524,56.3922691333822));
#104214=CARTESIAN_POINT('Ctrl Pts',(7.66947436500813,29.0900885896202,56.3955836951057));
#104215=CARTESIAN_POINT('Ctrl Pts',(7.66850840022717,29.1020666301471,56.4033314382105));
#104216=CARTESIAN_POINT('Ctrl Pts',(7.66794893567573,29.1089959078184,56.4077411561836));
#104217=CARTESIAN_POINT('Ctrl Pts',(7.66606509637627,29.1323104077254,56.4223371638982));
#104218=CARTESIAN_POINT('Ctrl Pts',(7.66472718751596,29.148839245191,56.432289609872));
#104219=CARTESIAN_POINT('Ctrl Pts',(7.66139682181687,29.1899967056376,56.4561076025831));
#104220=CARTESIAN_POINT('Ctrl Pts',(7.65938979963948,29.2148120346619,56.4696374947641));
#104221=CARTESIAN_POINT('Ctrl Pts',(7.65019628783019,29.3289894363844,56.5281723556831));
#104222=CARTESIAN_POINT('Ctrl Pts',(7.64283774004886,29.4219507307493,56.5657028485786));
#104223=CARTESIAN_POINT('Ctrl Pts',(7.62965965141574,29.5968835102083,56.6186084781));
#104224=CARTESIAN_POINT('Ctrl Pts',(7.62380959960134,29.6777308583614,56.636625376748));
#104225=CARTESIAN_POINT('Ctrl Pts',(7.6168062820679,29.7789953504499,56.651392556983));
#104226=CARTESIAN_POINT('Ctrl Pts',(7.61547514387438,29.7984462042601,56.6538792449243));
#104227=CARTESIAN_POINT('Ctrl Pts',(7.61335850955488,29.8296907233105,56.6573142629258));
#104228=CARTESIAN_POINT('Ctrl Pts',(7.61256623447685,29.8414579573358,56.6584813080072));
#104229=CARTESIAN_POINT('Ctrl Pts',(7.61106206342974,29.8639318676572,56.6604688315574));
#104230=CARTESIAN_POINT('Ctrl Pts',(7.61034951565319,29.8746359493407,56.6613112716227));
#104231=CARTESIAN_POINT('Ctrl Pts',(7.60871709763415,29.8992866176447,56.6630117360234));
#104232=CARTESIAN_POINT('Ctrl Pts',(7.60779951394328,29.9132374737514,56.6637979153967));
#104233=CARTESIAN_POINT('Ctrl Pts',(7.60489092310531,29.9577417273879,56.6657445807025));
#104234=CARTESIAN_POINT('Ctrl Pts',(7.60292053560572,29.9883189198263,56.6662396316288));
#104235=CARTESIAN_POINT('Ctrl Pts',(7.59826685115947,30.0613489739135,56.6654113478274));
#104236=CARTESIAN_POINT('Ctrl Pts',(7.59560606224221,30.1037719356854,56.6633070727821));
#104237=CARTESIAN_POINT('Ctrl Pts',(7.5884020407577,30.2195191601238,56.6531194237627));
#104238=CARTESIAN_POINT('Ctrl Pts',(7.5839265836452,30.2924592504376,56.6417857489463));
#104239=CARTESIAN_POINT('Ctrl Pts',(7.57445467251241,30.443540894953,56.6079191556948));
#104240=CARTESIAN_POINT('Ctrl Pts',(7.56946273537542,30.521263070193,56.5844286638284));
#104241=CARTESIAN_POINT('Ctrl Pts',(7.56316349761809,30.6120132481413,56.5495986261994));
#104242=CARTESIAN_POINT('Ctrl Pts',(7.56210818590097,30.6269851299292,56.543601541247));
#104243=CARTESIAN_POINT('Ctrl Pts',(7.5605270334629,30.6490298464412,56.5343977677214));
#104244=CARTESIAN_POINT('Ctrl Pts',(7.56001049509019,30.6561716210186,56.5313572571304));
#104245=CARTESIAN_POINT('Ctrl Pts',(7.55908875504542,30.6688038841038,56.5258746580552));
#104246=CARTESIAN_POINT('Ctrl Pts',(7.55868475218502,30.6743027874232,56.5234526104147));
#104247=CARTESIAN_POINT('Ctrl Pts',(7.55778909175074,30.6864092545777,56.5180418058125));
#104248=CARTESIAN_POINT('Ctrl Pts',(7.55729666711525,30.6930103757568,56.515039670468));
#104249=CARTESIAN_POINT('Ctrl Pts',(7.55584127124922,30.712365933217,56.5060839612423));
#104250=CARTESIAN_POINT('Ctrl Pts',(7.55487163049218,30.7250643985567,56.5000119020881));
#104251=CARTESIAN_POINT('Ctrl Pts',(7.54806868534156,30.812897954201,56.4566364384869));
#104252=CARTESIAN_POINT('Ctrl Pts',(7.5419820788777,30.8851917534359,56.4138689761082));
#104253=CARTESIAN_POINT('Ctrl Pts',(7.52652525687139,31.059306011282,56.2922620594852));
#104254=CARTESIAN_POINT('Ctrl Pts',(7.51721420295268,31.1558146621214,56.2067206892762));
#104255=CARTESIAN_POINT('Ctrl Pts',(7.50692676486953,31.2555294624945,56.0952817309755));
#104256=CARTESIAN_POINT('Ctrl Pts',(7.50549524115868,31.2692253941626,56.0793809659869));
#104257=CARTESIAN_POINT('Ctrl Pts',(7.50317527755965,31.2911168019607,56.0529723425865));
#104258=CARTESIAN_POINT('Ctrl Pts',(7.50227959898613,31.2994927431455,56.0426178489473));
#104259=CARTESIAN_POINT('Ctrl Pts',(7.50067538230539,31.3143534398637,56.0237894563849));
#104260=CARTESIAN_POINT('Ctrl Pts',(7.49996510007983,31.3208825747504,56.0153516871969));
#104261=CARTESIAN_POINT('Ctrl Pts',(7.49844859792349,31.3347107506058,55.99712203234));
#104262=CARTESIAN_POINT('Ctrl Pts',(7.49764341020147,31.3419841177594,55.9873113876414));
#104263=CARTESIAN_POINT('Ctrl Pts',(7.49543578745122,31.3617286385748,55.9600577363322));
#104264=CARTESIAN_POINT('Ctrl Pts',(7.49404207498355,31.373972216678,55.9424522047077));
#104265=CARTESIAN_POINT('Ctrl Pts',(7.48818256773555,31.4244297145494,55.8668231942112));
#104266=CARTESIAN_POINT('Ctrl Pts',(7.48383762888856,31.4593363503408,55.8066730894563));
#104267=CARTESIAN_POINT('Ctrl Pts',(7.47576622236848,31.5178498003253,55.6895391775552));
#104268=CARTESIAN_POINT('Ctrl Pts',(7.47203390583422,31.5422332525998,55.6331195595607));
#104269=CARTESIAN_POINT('Ctrl Pts',(7.46827878691259,31.5634376230276,55.5755161152408));
#104270=CARTESIAN_POINT('Origin',(5.,30.,55.));
#104271=CARTESIAN_POINT('',(6.76892549910492,31.5634376526692,55.5755160347169));
#104272=CARTESIAN_POINT('',(6.9616842973919,31.5634376940719,55.5755159222429));
#104273=CARTESIAN_POINT('',(5.,31.5634376782623,55.5755159651912));
#104274=CARTESIAN_POINT('Ctrl Pts',(6.9616842973919,31.5634376940719,55.5755159222429));
#104275=CARTESIAN_POINT('Ctrl Pts',(6.96605878096345,31.5391991836305,55.6413618865466));
#104276=CARTESIAN_POINT('Ctrl Pts',(6.97033680726182,31.510818319282,55.7056294995728));
#104277=CARTESIAN_POINT('Ctrl Pts',(6.97960774088078,31.4408418132267,55.8403512155861));
#104278=CARTESIAN_POINT('Ctrl Pts',(6.984589699559,31.3979601620666,55.9099011867989));
#104279=CARTESIAN_POINT('Ctrl Pts',(6.99144683607502,31.335035920585,55.9969461669099));
#104280=CARTESIAN_POINT('Ctrl Pts',(6.99311723203387,31.3194271468703,56.0175138320948));
#104281=CARTESIAN_POINT('Ctrl Pts',(6.99542234375112,31.2976299855697,56.0448907550862));
#104282=CARTESIAN_POINT('Ctrl Pts',(6.99603078389574,31.2918529972518,56.0520247589419));
#104283=CARTESIAN_POINT('Ctrl Pts',(6.99705796587303,31.282067579129,56.0639066349479));
#104284=CARTESIAN_POINT('Ctrl Pts',(6.9974744751748,31.2780908961335,56.0686806187769));
#104285=CARTESIAN_POINT('Ctrl Pts',(6.99833373373159,31.2698713889729,56.0784365887687));
#104286=CARTESIAN_POINT('Ctrl Pts',(6.99877666510884,31.2656257893292,56.0834159765248));
#104287=CARTESIAN_POINT('Ctrl Pts',(6.99995165755948,31.2543377663635,56.0964980701339));
#104288=CARTESIAN_POINT('Ctrl Pts',(7.00068713337997,31.247246302718,56.1045577826216));
#104289=CARTESIAN_POINT('Ctrl Pts',(7.00398200111639,31.2153421053471,56.1401191053309));
#104290=CARTESIAN_POINT('Ctrl Pts',(7.00659333309507,31.189695929694,56.1668552344542));
#104291=CARTESIAN_POINT('Ctrl Pts',(7.0159177694808,31.0962272142633,56.2580098117355));
#104292=CARTESIAN_POINT('Ctrl Pts',(7.02278600539818,31.0238941437296,56.3175519507439));
#104293=CARTESIAN_POINT('Ctrl Pts',(7.0341056887045,30.8952550118401,56.4064217150446));
#104294=CARTESIAN_POINT('Ctrl Pts',(7.03860457923511,30.8415786141611,56.439183928949));
#104295=CARTESIAN_POINT('Ctrl Pts',(7.04581928682043,30.7508075133655,56.4877678797704));
#104296=CARTESIAN_POINT('Ctrl Pts',(7.04858991700207,30.7147656914341,56.5054154459738));
#104297=CARTESIAN_POINT('Ctrl Pts',(7.05236697558147,30.6639937743315,56.5280403830164));
#104298=CARTESIAN_POINT('Ctrl Pts',(7.05341107596881,30.6497811328394,56.5341380811063));
#104299=CARTESIAN_POINT('Ctrl Pts',(7.05518486167894,30.6253375094143,56.5442245657764));
#104300=CARTESIAN_POINT('Ctrl Pts',(7.05591782820855,30.6151484536999,56.5483116288662));
#104301=CARTESIAN_POINT('Ctrl Pts',(7.05739747670118,30.5944038861428,56.5563956410507));
#104302=CARTESIAN_POINT('Ctrl Pts',(7.05814392764579,30.5838466606964,56.5603866375819));
#104303=CARTESIAN_POINT('Ctrl Pts',(7.06000839099854,30.5572523199332,56.5701325193655));
#104304=CARTESIAN_POINT('Ctrl Pts',(7.0611217945913,30.5411657210251,56.5757493372613));
#104305=CARTESIAN_POINT('Ctrl Pts',(7.06539707030997,30.4786449668356,56.5965087553796));
#104306=CARTESIAN_POINT('Ctrl Pts',(7.06850073577216,30.4316374986171,56.6098543291492));
#104307=CARTESIAN_POINT('Ctrl Pts',(7.07842143390615,30.2774277896715,56.6463928384726));
#104308=CARTESIAN_POINT('Ctrl Pts',(7.08501078287782,30.1685156231981,56.6610774527979));
#104309=CARTESIAN_POINT('Ctrl Pts',(7.09464516483473,30.0120876145971,56.6666159316788));
#104310=CARTESIAN_POINT('Ctrl Pts',(7.09755918558406,29.9651798272095,56.6662958103886));
#104311=CARTESIAN_POINT('Ctrl Pts',(7.10229181881558,29.8909824314054,56.6626551172728));
#104312=CARTESIAN_POINT('Ctrl Pts',(7.10406177420637,29.8636525155922,56.660637235264));
#104313=CARTESIAN_POINT('Ctrl Pts',(7.10648301761513,29.8270506616555,56.6570252071521));
#104314=CARTESIAN_POINT('Ctrl Pts',(7.10710451205596,29.8177228245269,56.6560250698242));
#104315=CARTESIAN_POINT('Ctrl Pts',(7.10814743850237,29.8021924527981,56.6542270936239));
#104316=CARTESIAN_POINT('Ctrl Pts',(7.10856648284714,29.7959848885515,56.6534729920111));
#104317=CARTESIAN_POINT('Ctrl Pts',(7.10937087599066,29.7841343500284,56.6519656263791));
#104318=CARTESIAN_POINT('Ctrl Pts',(7.10975585986795,29.7784907378013,56.6512183543889));
#104319=CARTESIAN_POINT('Ctrl Pts',(7.11080105572772,29.7632414859407,56.6491196140163));
#104320=CARTESIAN_POINT('Ctrl Pts',(7.11146421154153,29.7536438187596,56.6477131776893));
#104321=CARTESIAN_POINT('Ctrl Pts',(7.11403693553516,29.7166867423936,56.6419674065242));
#104322=CARTESIAN_POINT('Ctrl Pts',(7.11597515316308,29.6894264594142,56.6370300022833));
#104323=CARTESIAN_POINT('Ctrl Pts',(7.12580958903916,29.5534118974173,56.6088755691168));
#104324=CARTESIAN_POINT('Ctrl Pts',(7.13400651215752,29.4470536890573,56.5754907915846));
#104325=CARTESIAN_POINT('Ctrl Pts',(7.1462941521345,29.2906872324615,56.5086077636068));
#104326=CARTESIAN_POINT('Ctrl Pts',(7.15049845842193,29.2378194372421,56.482600399395));
#104327=CARTESIAN_POINT('Ctrl Pts',(7.15730693364231,29.1528992881794,56.4350795179289));
#104328=CARTESIAN_POINT('Ctrl Pts',(7.15995817737944,29.1200206041347,56.4151570649151));
#104329=CARTESIAN_POINT('Ctrl Pts',(7.16360271723309,29.0751177173069,56.3857779630177));
#104330=CARTESIAN_POINT('Ctrl Pts',(7.16463026714366,29.0624919315407,56.3772677473651));
#104331=CARTESIAN_POINT('Ctrl Pts',(7.16638460604484,29.041001669676,56.362350089912));
#104332=CARTESIAN_POINT('Ctrl Pts',(7.1671144980028,29.0320805579173,56.3560263745625));
#104333=CARTESIAN_POINT('Ctrl Pts',(7.168595283171,29.014026257364,56.3429596565791));
#104334=CARTESIAN_POINT('Ctrl Pts',(7.16934587683821,29.0048984257147,56.3362102110101));
#104335=CARTESIAN_POINT('Ctrl Pts',(7.17123509513117,28.9819906784605,56.3189064668498));
#104336=CARTESIAN_POINT('Ctrl Pts',(7.17236884621399,28.9683051799836,56.3082289869823));
#104337=CARTESIAN_POINT('Ctrl Pts',(7.17685749519357,28.9144154583463,56.2648123164017));
#104338=CARTESIAN_POINT('Ctrl Pts',(7.18014600508872,28.8755801182253,56.2304164826193));
#104339=CARTESIAN_POINT('Ctrl Pts',(7.19151845194387,28.7450558894532,56.1034630283681));
#104340=CARTESIAN_POINT('Ctrl Pts',(7.19926377393868,28.6626774574071,56.0020383521461));
#104341=CARTESIAN_POINT('Ctrl Pts',(7.20935364639527,28.5761500002311,55.8655587257811));
#104342=CARTESIAN_POINT('Ctrl Pts',(7.21133530491899,28.5601004609697,55.8385879878787));
#104343=CARTESIAN_POINT('Ctrl Pts',(7.21469136474507,28.5346917797679,55.7930074224237));
#104344=CARTESIAN_POINT('Ctrl Pts',(7.21604517200548,28.5249024562239,55.774645785246));
#104345=CARTESIAN_POINT('Ctrl Pts',(7.21797734270721,28.5116204247047,55.7485678440223));
#104346=CARTESIAN_POINT('Ctrl Pts',(7.21853915511936,28.5078383231723,55.7410000673838));
#104347=CARTESIAN_POINT('Ctrl Pts',(7.21951131419237,28.5014341441487,55.7279377978301));
#104348=CARTESIAN_POINT('Ctrl Pts',(7.21991995363518,28.4987842643689,55.7224571791995));
#104349=CARTESIAN_POINT('Ctrl Pts',(7.22079069355832,28.4932278908324,55.7108026252196));
#104350=CARTESIAN_POINT('Ctrl Pts',(7.22125321463698,28.4903293103046,55.7046254079117));
#104351=CARTESIAN_POINT('Ctrl Pts',(7.22253673186184,28.482428658832,55.6875156478742));
#104352=CARTESIAN_POINT('Ctrl Pts',(7.22336229199063,28.4775069727751,55.6765467483983));
#104353=CARTESIAN_POINT('Ctrl Pts',(7.22805529647081,28.4504016172849,55.6143434870941));
#104354=CARTESIAN_POINT('Ctrl Pts',(7.23204072404014,28.4306877802332,55.5620773311299));
#104355=CARTESIAN_POINT('Ctrl Pts',(7.24439011190475,28.3784717475078,55.3993158572814));
#104356=CARTESIAN_POINT('Ctrl Pts',(7.25285272177008,28.3547585893054,55.2863426391698));
#104357=CARTESIAN_POINT('Ctrl Pts',(7.26500701822658,28.3371014018802,55.1160525750548));
#104358=CARTESIAN_POINT('Ctrl Pts',(7.26891717713879,28.3341372015599,55.0600194059551));
#104359=CARTESIAN_POINT('Ctrl Pts',(7.27392176472738,28.3339637216004,54.9866192144537));
#104360=CARTESIAN_POINT('Ctrl Pts',(7.27509418772777,28.3341928317121,54.9693007528494));
#104361=CARTESIAN_POINT('Ctrl Pts',(7.27702062649477,28.3350188641001,54.9406493602572));
#104362=CARTESIAN_POINT('Ctrl Pts',(7.27777938644573,28.33546158406,54.929313691585));
#104363=CARTESIAN_POINT('Ctrl Pts',(7.27925453116482,28.3365525225946,54.907180428105));
#104364=CARTESIAN_POINT('Ctrl Pts',(7.27997120774794,28.337190182243,54.8963829050674));
#104365=CARTESIAN_POINT('Ctrl Pts',(7.28168499835746,28.3389744470515,54.8704618918199));
#104366=CARTESIAN_POINT('Ctrl Pts',(7.28267889926956,28.340222513103,54.8553461787118));
#104367=CARTESIAN_POINT('Ctrl Pts',(7.28596061648191,28.345054365208,54.8051882331202));
#104368=CARTESIAN_POINT('Ctrl Pts',(7.288220365409,28.3495431062944,54.7702414336188));
#104369=CARTESIAN_POINT('Ctrl Pts',(7.29820377937337,28.3745634184298,54.6146688501553));
#104370=CARTESIAN_POINT('Ctrl Pts',(7.30555594387433,28.4072355480808,54.4963860829649));
#104371=CARTESIAN_POINT('Ctrl Pts',(7.31616835007085,28.4712510215176,54.3359023028214));
#104372=CARTESIAN_POINT('Ctrl Pts',(7.31929271379768,28.4920514171192,54.2899369352619));
#104373=CARTESIAN_POINT('Ctrl Pts',(7.32432615251511,28.5279176976066,54.2193883910628));
#104374=CARTESIAN_POINT('Ctrl Pts',(7.32617870871891,28.5415917477417,54.1941303300494));
#104375=CARTESIAN_POINT('Ctrl Pts',(7.32869595031607,28.5606681658887,54.1609702656021));
#104376=CARTESIAN_POINT('Ctrl Pts',(7.32932775507096,28.5654964703236,54.1527416943151));
#104377=CARTESIAN_POINT('Ctrl Pts',(7.33038319056283,28.5736226210392,54.1391614065089));
#104378=CARTESIAN_POINT('Ctrl Pts',(7.33080430929422,28.5768806536416,54.1337859185545));
#104379=CARTESIAN_POINT('Ctrl Pts',(7.33166108525565,28.5835387476352,54.1229395627342));
#104380=CARTESIAN_POINT('Ctrl Pts',(7.33209682305247,28.5869402500874,54.1174697570728));
#104381=CARTESIAN_POINT('Ctrl Pts',(7.33323220332089,28.5958451431336,54.1033336572343));
#104382=CARTESIAN_POINT('Ctrl Pts',(7.33393487326718,28.6013969746332,54.0946984168727));
#104383=CARTESIAN_POINT('Ctrl Pts',(7.33687296088697,28.6247929819851,54.0590374830235));
#104384=CARTESIAN_POINT('Ctrl Pts',(7.33914789212967,28.6433423261855,54.0324854359747));
#104385=CARTESIAN_POINT('Ctrl Pts',(7.34834777601949,28.7204685121623,53.9286668015828));
#104386=CARTESIAN_POINT('Ctrl Pts',(7.35547038268582,28.7849661406488,53.856038653126));
#104387=CARTESIAN_POINT('Ctrl Pts',(7.36714653526506,28.9020787083574,53.7453089585798));
#104388=CARTESIAN_POINT('Ctrl Pts',(7.37174946631868,28.9512622934629,53.7039168865007));
#104389=CARTESIAN_POINT('Ctrl Pts',(7.37910617768451,29.0353124021925,53.6411072341496));
#104390=CARTESIAN_POINT('Ctrl Pts',(7.38191764461866,29.0687907301478,53.617950254636));
#104391=CARTESIAN_POINT('Ctrl Pts',(7.38573984266054,29.1161852243322,53.5876724686091));
#104392=CARTESIAN_POINT('Ctrl Pts',(7.38678945020077,29.1294011300752,53.5794876805362));
#104393=CARTESIAN_POINT('Ctrl Pts',(7.38856972450322,29.1521554437231,53.5658324922275));
#104394=CARTESIAN_POINT('Ctrl Pts',(7.3893037322654,29.1616367778829,53.5602694871104));
#104395=CARTESIAN_POINT('Ctrl Pts',(7.39069557057181,29.1798024914372,53.5498513815655));
#104396=CARTESIAN_POINT('Ctrl Pts',(7.39135398399864,29.1884766182542,53.5449794583038));
#104397=CARTESIAN_POINT('Ctrl Pts',(7.39288876624656,29.208881895304,53.533757842432));
#104398=CARTESIAN_POINT('Ctrl Pts',(7.39376289455994,29.2206468049796,53.5274707016041));
#104399=CARTESIAN_POINT('Ctrl Pts',(7.39679048882461,29.2618781161244,53.506069374918));
#104400=CARTESIAN_POINT('Ctrl Pts',(7.39891846956236,29.291719745271,53.4916923580391));
#104401=CARTESIAN_POINT('Ctrl Pts',(7.408925649166,29.4356832938722,53.4275497492198));
#104402=CARTESIAN_POINT('Ctrl Pts',(7.41640732848865,29.5547127289888,53.3897906887562));
#104403=CARTESIAN_POINT('Ctrl Pts',(7.42718355791543,29.7268812733978,53.3557482091025));
#104404=CARTESIAN_POINT('Ctrl Pts',(7.43034218624413,29.7773448750178,53.3481580698023));
#104405=CARTESIAN_POINT('Ctrl Pts',(7.43483335889778,29.8476023668032,53.3408687653566));
#104406=CARTESIAN_POINT('Ctrl Pts',(7.43609392040169,29.8671649106243,53.3391880717044));
#104407=CARTESIAN_POINT('Ctrl Pts',(7.43832620579238,29.901425354632,53.3368537779799));
#104408=CARTESIAN_POINT('Ctrl Pts',(7.4392909648623,29.9161110195968,53.3360484023967));
#104409=CARTESIAN_POINT('Ctrl Pts',(7.44075509085872,29.938178340151,53.3351310725891));
#104410=CARTESIAN_POINT('Ctrl Pts',(7.44124684945115,29.9455536630292,53.3348735620677));
#104411=CARTESIAN_POINT('Ctrl Pts',(7.44214365629856,29.9589321079609,53.3344954281089));
#104412=CARTESIAN_POINT('Ctrl Pts',(7.4425477914177,29.9649344951484,53.3343582444591));
#104413=CARTESIAN_POINT('Ctrl Pts',(7.44346871877992,29.9785526676406,53.3341206466661));
#104414=CARTESIAN_POINT('Ctrl Pts',(7.44398655380007,29.9861684379261,53.3340400094495));
#104415=CARTESIAN_POINT('Ctrl Pts',(7.44559552250121,30.0097113275793,53.3339521724374));
#104416=CARTESIAN_POINT('Ctrl Pts',(7.44669551210689,30.0256376692242,53.3341211516941));
#104417=CARTESIAN_POINT('Ctrl Pts',(7.4547521473933,30.1412379710788,53.3370057005297));
#104418=CARTESIAN_POINT('Ctrl Pts',(7.46204710573607,30.2404844424247,53.3484364400081));
#104419=CARTESIAN_POINT('Ctrl Pts',(7.47209091130659,30.375687687993,53.3764582060482));
#104420=CARTESIAN_POINT('Ctrl Pts',(7.47487542062039,30.4129918543761,53.3855443343301));
#104421=CARTESIAN_POINT('Ctrl Pts',(7.48142394225165,30.5006069290069,53.41012052554));
#104422=CARTESIAN_POINT('Ctrl Pts',(7.48516417682383,30.5505660896669,53.4267225604054));
#104423=CARTESIAN_POINT('Ctrl Pts',(7.49131977273814,30.6328770553442,53.4584779438754));
#104424=CARTESIAN_POINT('Ctrl Pts',(7.49377120946707,30.6656770074748,53.4723553843643));
#104425=CARTESIAN_POINT('Ctrl Pts',(7.49719204794729,30.7114491227021,53.4934757773371));
#104426=CARTESIAN_POINT('Ctrl Pts',(7.49819032687666,30.7248060840215,53.4998562559568));
#104427=CARTESIAN_POINT('Ctrl Pts',(7.49991050409725,30.7478145783698,53.5112262290877));
#104428=CARTESIAN_POINT('Ctrl Pts',(7.50063519516233,30.7575054332946,53.5161335933682));
#104429=CARTESIAN_POINT('Ctrl Pts',(7.50202767702168,30.776117710957,53.5257885467199));
#104430=CARTESIAN_POINT('Ctrl Pts',(7.50269588195686,30.7850452631518,53.530523204451));
#104431=CARTESIAN_POINT('Ctrl Pts',(7.50446396467172,30.808652193802,53.5433194991129));
#104432=CARTESIAN_POINT('Ctrl Pts',(7.50555881244014,30.8232542824333,53.5515218772777));
#104433=CARTESIAN_POINT('Ctrl Pts',(7.50964783892518,30.877688395064,53.5831880779939));
#104434=CARTESIAN_POINT('Ctrl Pts',(7.51259047533527,30.9166637316682,53.608087239961));
#104435=CARTESIAN_POINT('Ctrl Pts',(7.52375852737322,31.0625812368592,53.7100969648281));
#104436=CARTESIAN_POINT('Ctrl Pts',(7.53160205882745,31.1612562487365,53.798163654094));
#104437=CARTESIAN_POINT('Ctrl Pts',(7.54195588990297,31.2714675064711,53.9229078164203));
#104438=CARTESIAN_POINT('Ctrl Pts',(7.54413620160729,31.2935973853703,53.9495892715032));
#104439=CARTESIAN_POINT('Ctrl Pts',(7.54779202977871,31.3285865406652,53.9945587194966));
#104440=CARTESIAN_POINT('Ctrl Pts',(7.54924193474332,31.3419390328605,54.0124505683885));
#104441=CARTESIAN_POINT('Ctrl Pts',(7.55128795984955,31.3599850376022,54.0376735199897));
#104442=CARTESIAN_POINT('Ctrl Pts',(7.55186481112744,31.3649873057471,54.0447821172259));
#104443=CARTESIAN_POINT('Ctrl Pts',(7.5528544600751,31.3734189482748,54.0569655870034));
#104444=CARTESIAN_POINT('Ctrl Pts',(7.55326539092743,31.3768764612798,54.0620209379647));
#104445=CARTESIAN_POINT('Ctrl Pts',(7.55413123934494,31.3840688521163,54.0726626463423));
#104446=CARTESIAN_POINT('Ctrl Pts',(7.55458649931756,31.3877978816186,54.0782526427193));
#104447=CARTESIAN_POINT('Ctrl Pts',(7.55582957068282,31.3978400775973,54.0935054638303));
#104448=CARTESIAN_POINT('Ctrl Pts',(7.55662150217171,31.4040866684626,54.1032113763642));
#104449=CARTESIAN_POINT('Ctrl Pts',(7.56067180433702,31.4352978770733,54.1528326793087));
#104450=CARTESIAN_POINT('Ctrl Pts',(7.56401422468317,31.4586612315519,54.1937252209994));
#104451=CARTESIAN_POINT('Ctrl Pts',(7.57465828076498,31.5265704721966,54.3252223764167));
#104452=CARTESIAN_POINT('Ctrl Pts',(7.58207951644744,31.5646372979801,54.4189203581647));
#104453=CARTESIAN_POINT('Ctrl Pts',(7.59484875179544,31.6162990247435,54.5888825997773));
#104454=CARTESIAN_POINT('Ctrl Pts',(7.60025566188861,31.6335144953173,54.6637360100342));
#104455=CARTESIAN_POINT('Ctrl Pts',(7.60679056684221,31.6484616321655,54.758160325794));
#104456=CARTESIAN_POINT('Ctrl Pts',(7.6080707447755,31.6510955416035,54.7768503997537));
#104457=CARTESIAN_POINT('Ctrl Pts',(7.61012640958847,31.6548433975342,54.807164482254));
#104458=CARTESIAN_POINT('Ctrl Pts',(7.61090799260652,31.6561536847005,54.8187620571968));
#104459=CARTESIAN_POINT('Ctrl Pts',(7.61240458861309,31.658440303052,54.8411034419004));
#104460=CARTESIAN_POINT('Ctrl Pts',(7.61312012179271,31.6594343619786,54.8518448024095));
#104461=CARTESIAN_POINT('Ctrl Pts',(7.6147616322004,31.6614846358644,54.8766191989005));
#104462=CARTESIAN_POINT('Ctrl Pts',(7.61568527563044,31.6624675267487,54.8906576025065));
#104463=CARTESIAN_POINT('Ctrl Pts',(7.61869408056788,31.6651048252023,54.9366898637379));
#104464=CARTESIAN_POINT('Ctrl Pts',(7.62075616911904,31.6660144207487,54.9687203207882));
#104465=CARTESIAN_POINT('Ctrl Pts',(7.62567552230028,31.6659791981065,55.0460479865259));
#104466=CARTESIAN_POINT('Ctrl Pts',(7.62850644731632,31.6641118616799,55.09131954637));
#104467=CARTESIAN_POINT('Ctrl Pts',(7.63562981808123,31.6546777507552,55.2061096596105));
#104468=CARTESIAN_POINT('Ctrl Pts',(7.63987218161648,31.6445769255838,55.2753300566623));
#104469=CARTESIAN_POINT('Ctrl Pts',(7.64492146248019,31.6275528375619,55.3560720941749));
#104470=CARTESIAN_POINT('Ctrl Pts',(7.64569548756865,31.6248061902719,55.3684025174323));
#104471=CARTESIAN_POINT('Ctrl Pts',(7.65064046933885,31.6064087226453,55.4467822927442));
#104472=CARTESIAN_POINT('Ctrl Pts',(7.65485616124645,31.5868767434299,55.5118417667872));
#104473=CARTESIAN_POINT('Ctrl Pts',(7.65925614416276,31.563437678903,55.5755159634506));
#104474=CARTESIAN_POINT('',(7.42924477180836,31.6659997297127,55.0012652267279));
#104475=CARTESIAN_POINT('Ctrl Pts',(7.46827878691259,31.5634376230276,55.5755161152408));
#104476=CARTESIAN_POINT('Ctrl Pts',(7.4656539658509,31.5782594380647,55.535251416031));
#104477=CARTESIAN_POINT('Ctrl Pts',(7.46301743683412,31.5915279306235,55.494408327742));
#104478=CARTESIAN_POINT('Ctrl Pts',(7.45745227979136,31.6157720974862,55.4086205039906));
#104479=CARTESIAN_POINT('Ctrl Pts',(7.45452076845838,31.6264799160976,55.3636652849397));
#104480=CARTESIAN_POINT('Ctrl Pts',(7.45074649398307,31.6374954372626,55.3070766712269));
#104481=CARTESIAN_POINT('Ctrl Pts',(7.44999047643321,31.6395693643978,55.2958034320809));
#104482=CARTESIAN_POINT('Ctrl Pts',(7.44878249270745,31.642671099076,55.2779074742279));
#104483=CARTESIAN_POINT('Ctrl Pts',(7.44833467699693,31.6437755938566,55.2712981700257));
#104484=CARTESIAN_POINT('Ctrl Pts',(7.4474728606743,31.645813982304,55.2586308315242));
#104485=CARTESIAN_POINT('Ctrl Pts',(7.44705921983653,31.6467543571502,55.2525740554654));
#104486=CARTESIAN_POINT('Ctrl Pts',(7.44622483485821,31.6485756845497,55.2404005066046));
#104487=CARTESIAN_POINT('Ctrl Pts',(7.44580407019775,31.6494560722221,55.2342837042026));
#104488=CARTESIAN_POINT('Ctrl Pts',(7.44479672650825,31.6514738932723,55.2196887628783));
#104489=CARTESIAN_POINT('Ctrl Pts',(7.44420856977113,31.652580088181,55.2112065751816));
#104490=CARTESIAN_POINT('Ctrl Pts',(7.44212392557101,31.6562502390306,55.1812680196867));
#104491=CARTESIAN_POINT('Ctrl Pts',(7.44061140200932,31.6584619054565,55.1597715769524));
#104492=CARTESIAN_POINT('Ctrl Pts',(7.43585342418317,31.6640485999887,55.0926753967592));
#104493=CARTESIAN_POINT('Ctrl Pts',(7.43256029705638,31.6659648561359,55.0469779281573));
#104494=CARTESIAN_POINT('Ctrl Pts',(7.4292449970585,31.6659995210235,55.0012633089186));
#104495=CARTESIAN_POINT('Ctrl Pts',(7.42924513422323,31.6659995195882,55.0012652002811));
#104496=CARTESIAN_POINT('Ctrl Pts',(7.41936135371292,31.6661030194695,54.8649778827319));
#104497=CARTESIAN_POINT('Ctrl Pts',(7.40938169123781,31.6494818328085,54.7291573370653));
#104498=CARTESIAN_POINT('Ctrl Pts',(7.39771728103842,31.6088565340369,54.56625860823));
#104499=CARTESIAN_POINT('Ctrl Pts',(7.39555200428979,31.6003558274504,54.5358745847821));
#104500=CARTESIAN_POINT('Ctrl Pts',(7.39245617925532,31.5868023520165,54.4922459184446));
#104501=CARTESIAN_POINT('Ctrl Pts',(7.3915036984892,31.5824359088968,54.4787970382474));
#104502=CARTESIAN_POINT('Ctrl Pts',(7.38983635145403,31.5744463334028,54.4552151853474));
#104503=CARTESIAN_POINT('Ctrl Pts',(7.38911916494136,31.5708953101027,54.4450588453925));
#104504=CARTESIAN_POINT('Ctrl Pts',(7.38762589435441,31.5632627843851,54.4238894277458));
#104505=CARTESIAN_POINT('Ctrl Pts',(7.38685047238517,31.5591626986701,54.4128836440023));
#104506=CARTESIAN_POINT('Ctrl Pts',(7.3848154294815,31.5480432973963,54.3839742527801));
#104507=CARTESIAN_POINT('Ctrl Pts',(7.38356233987784,31.5408296700018,54.3661469021415));
#104508=CARTESIAN_POINT('Ctrl Pts',(7.3775013159638,31.5041719301216,54.2798796232642));
#104509=CARTESIAN_POINT('Ctrl Pts',(7.37283973460155,31.470466657887,54.2133384866256));
#104510=CARTESIAN_POINT('Ctrl Pts',(7.36163437503957,31.377608980505,54.0569893057153));
#104511=CARTESIAN_POINT('Ctrl Pts',(7.35519975023623,31.3140164567546,53.9702262801732));
#104512=CARTESIAN_POINT('Ctrl Pts',(7.34664975305962,31.2230466447546,53.8683781648411));
#104513=CARTESIAN_POINT('Ctrl Pts',(7.34479825774764,31.2029974935462,53.8470872073387));
#104514=CARTESIAN_POINT('Ctrl Pts',(7.34166016428255,31.1686790866063,53.8125133616532));
#104515=CARTESIAN_POINT('Ctrl Pts',(7.34039159863371,31.1547178449358,53.7989329981939));
#104516=CARTESIAN_POINT('Ctrl Pts',(7.33858416214926,31.1347654542844,53.7801943838589));
#104517=CARTESIAN_POINT('Ctrl Pts',(7.33805981535908,31.1289701718512,53.7748286967522));
#104518=CARTESIAN_POINT('Ctrl Pts',(7.33752869710769,31.1230960305806,53.7694670629413));
#104519=CARTESIAN_POINT('Ctrl Pts',(7.33752498343876,31.1230549573915,53.7694295770779));
#104520=CARTESIAN_POINT('Ctrl Pts',(7.33751748310661,31.1229720033011,53.7693538757969));
#104521=CARTESIAN_POINT('Ctrl Pts',(7.33751369643611,31.1229301223116,53.7693156604476));
#104522=CARTESIAN_POINT('Ctrl Pts',(7.33750604627074,31.1228455102381,53.7692384619741));
#104523=CARTESIAN_POINT('Ctrl Pts',(7.33750218276933,31.1228027790735,53.7691994789364));
#104524=CARTESIAN_POINT('Ctrl Pts',(7.33749437487349,31.1227164216271,53.769120704498));
#104525=CARTESIAN_POINT('Ctrl Pts',(7.33749043047031,31.1226727952395,53.7690809131727));
#104526=CARTESIAN_POINT('Ctrl Pts',(7.33748245644921,31.122584599523,53.769000479061));
#104527=CARTESIAN_POINT('Ctrl Pts',(7.33747842681846,31.1225400300429,53.7689598363215));
#104528=CARTESIAN_POINT('Ctrl Pts',(7.33747027774098,31.1224498972236,53.7688776535111));
#104529=CARTESIAN_POINT('Ctrl Pts',(7.3374661582819,31.1224043337378,53.7688361135055));
#104530=CARTESIAN_POINT('Ctrl Pts',(7.33745782463336,31.1223121585232,53.768752087186));
#104531=CARTESIAN_POINT('Ctrl Pts',(7.33745361044804,31.1222655468294,53.7687096011187));
#104532=CARTESIAN_POINT('Ctrl Pts',(7.337445082118,31.1221712173329,53.7686236305835));
#104533=CARTESIAN_POINT('Ctrl Pts',(7.33744076796644,31.1221234994429,53.7685801462677));
#104534=CARTESIAN_POINT('Ctrl Pts',(7.33743203411954,31.122026895754,53.7684921236232));
#104535=CARTESIAN_POINT('Ctrl Pts',(7.33742761441807,31.1219780098749,53.7684475854716));
#104536=CARTESIAN_POINT('Ctrl Pts',(7.3374186635088,31.1218790042225,53.7683573957999));
#104537=CARTESIAN_POINT('Ctrl Pts',(7.33741413227305,31.1218288841266,53.7683117442569));
#104538=CARTESIAN_POINT('Ctrl Pts',(7.33740495188074,31.1217273390527,53.7682192639682));
#104539=CARTESIAN_POINT('Ctrl Pts',(7.33740030272578,31.121675914078,53.7681724355192));
#104540=CARTESIAN_POINT('Ctrl Pts',(7.33739087962831,31.1215716832527,53.7680775331113));
#104541=CARTESIAN_POINT('Ctrl Pts',(7.33738610567137,31.1215188772269,53.7680294593119));
#104542=CARTESIAN_POINT('Ctrl Pts',(7.33737642560051,31.1214118027413,53.7679319929252));
#104543=CARTESIAN_POINT('Ctrl Pts',(7.33737151946792,31.1213575340581,53.7678826004817));
#104544=CARTESIAN_POINT('Ctrl Pts',(7.3373615671032,31.1212474463556,53.7677824178594));
#104545=CARTESIAN_POINT('Ctrl Pts',(7.33735652086198,31.1211916272173,53.7677316279506));
#104546=CARTESIAN_POINT('Ctrl Pts',(7.33734627972727,31.1210783439482,53.7676285654216));
#104547=CARTESIAN_POINT('Ctrl Pts',(7.33734108481863,31.1210208796301,53.7675762930437));
#104548=CARTESIAN_POINT('Ctrl Pts',(7.33733053712263,31.1209042038868,53.7674701739453));
#104549=CARTESIAN_POINT('Ctrl Pts',(7.33732518431461,31.120844992212,53.7674163274492));
#104550=CARTESIAN_POINT('Ctrl Pts',(7.33731431084044,31.1207247113062,53.7673069610485));
#104551=CARTESIAN_POINT('Ctrl Pts',(7.33730879015368,31.1206636418241,53.7672514414102));
#104552=CARTESIAN_POINT('Ctrl Pts',(7.33729757011571,31.1205395257016,53.7671386214993));
#104553=CARTESIAN_POINT('Ctrl Pts',(7.33729187073861,31.1204764787494,53.7670813214864));
#104554=CARTESIAN_POINT('Ctrl Pts',(7.33728028158943,31.1203482778526,53.7669648244831));
#104555=CARTESIAN_POINT('Ctrl Pts',(7.33727439179787,31.1202831236652,53.7669056278693));
#104556=CARTESIAN_POINT('Ctrl Pts',(7.337262409071,31.1201505671927,53.7667852112836));
#104557=CARTESIAN_POINT('Ctrl Pts',(7.33725631611415,31.1200831646392,53.7667239917266));
#104558=CARTESIAN_POINT('Ctrl Pts',(7.33724391318314,31.1199459578779,53.7665993917941));
#104559=CARTESIAN_POINT('Ctrl Pts',(7.33723760317389,31.1198761532488,53.7665360117643));
#104560=CARTESIAN_POINT('Ctrl Pts',(7.33722475099225,31.1197339746944,53.7664069408965));
#104561=CARTESIAN_POINT('Ctrl Pts',(7.33721820878539,31.1196616003518,53.7663412504866));
#104562=CARTESIAN_POINT('Ctrl Pts',(7.33720487564038,31.1195140989835,53.7662073948723));
#104563=CARTESIAN_POINT('Ctrl Pts',(7.33719808466971,31.1194389715584,53.7661392302019));
#104564=CARTESIAN_POINT('Ctrl Pts',(7.33718423584509,31.1192857631039,53.7660002465054));
#104565=CARTESIAN_POINT('Ctrl Pts',(7.3371771779531,31.1192076816101,53.7659294280565));
#104566=CARTESIAN_POINT('Ctrl Pts',(7.33716277536024,31.119048344462,53.7657849398154));
#104567=CARTESIAN_POINT('Ctrl Pts',(7.33715543060139,31.1189670881182,53.7657112705133));
#104568=CARTESIAN_POINT('Ctrl Pts',(7.33714043232229,31.1188011582741,53.7655608636701));
#104569=CARTESIAN_POINT('Ctrl Pts',(7.33713277875259,31.1187164841733,53.7654841268347));
#104570=CARTESIAN_POINT('Ctrl Pts',(7.3371171386195,31.1185434505803,53.7653273456586));
#104571=CARTESIAN_POINT('Ctrl Pts',(7.33710915200722,31.1184550904877,53.7652473021788));
#104572=CARTESIAN_POINT('Ctrl Pts',(7.33709281899485,31.1182743883132,53.765083643334));
#104573=CARTESIAN_POINT('Ctrl Pts',(7.33708447252312,31.1181820453727,53.7650000287754));
#104574=CARTESIAN_POINT('Ctrl Pts',(7.33706739005771,31.1179930483544,53.76482893459));
#104575=CARTESIAN_POINT('Ctrl Pts',(7.33705865398962,31.1178963933797,53.764741455944));
#104576=CARTESIAN_POINT('Ctrl Pts',(7.33704075924674,31.1176984060491,53.7645623076064));
#104577=CARTESIAN_POINT('Ctrl Pts',(7.3370316004879,31.117597072681,53.764470639035));
#104578=CARTESIAN_POINT('Ctrl Pts',(7.33661963579285,31.1130390161951,53.7603483324531));
#104579=CARTESIAN_POINT('Ctrl Pts',(7.33621501173573,31.1085607628729,53.756342032666));
#104580=CARTESIAN_POINT('Ctrl Pts',(7.33528349452633,31.0982475395454,53.7472156601709));
#104581=CARTESIAN_POINT('Ctrl Pts',(7.33475544850223,31.0923984060726,53.7421120969548));
#104582=CARTESIAN_POINT('Ctrl Pts',(7.33312162651768,31.074285378687,53.7265294903765));
#104583=CARTESIAN_POINT('Ctrl Pts',(7.33200684366963,31.061905192542,53.7161878922637));
#104584=CARTESIAN_POINT('Ctrl Pts',(7.32522946465763,30.9864025441923,53.6549572148642));
#104585=CARTESIAN_POINT('Ctrl Pts',(7.31934375050404,30.9197892594001,53.6085563923883));
#104586=CARTESIAN_POINT('Ctrl Pts',(7.30807741906914,30.7866631560088,53.5295739389255));
#104587=CARTESIAN_POINT('Ctrl Pts',(7.30271115037753,30.7208242667557,53.4962030009142));
#104588=CARTESIAN_POINT('Ctrl Pts',(7.29441923114099,30.6139225091634,53.4506587670401));
#104589=CARTESIAN_POINT('Ctrl Pts',(7.29142552549945,30.5742326464151,53.435513991074));
#104590=CARTESIAN_POINT('Ctrl Pts',(7.28635587043202,30.5050408717769,53.4121005485957));
#104591=CARTESIAN_POINT('Ctrl Pts',(7.28425847615295,30.4758113654081,53.4030984039399));
#104592=CARTESIAN_POINT('Ctrl Pts',(7.28124051673948,30.432887065572,53.3911619028423));
#104593=CARTESIAN_POINT('Ctrl Pts',(7.28029953645357,30.4193783395296,53.3875878121911));
#104594=CARTESIAN_POINT('Ctrl Pts',(7.27864520465512,30.3954125095825,53.3815685909063));
#104595=CARTESIAN_POINT('Ctrl Pts',(7.27792965027376,30.384973893948,53.3790538599535));
#104596=CARTESIAN_POINT('Ctrl Pts',(7.27643286654219,30.3629900068715,53.3739821451141));
#104597=CARTESIAN_POINT('Ctrl Pts',(7.27565236567342,30.3514403177188,53.3714468001591));
#104598=CARTESIAN_POINT('Ctrl Pts',(7.2735879457731,30.3206709415822,53.3650350061602));
#104599=CARTESIAN_POINT('Ctrl Pts',(7.2723109124728,30.3014077955811,53.3613744243243));
#104600=CARTESIAN_POINT('Ctrl Pts',(7.26570085748255,30.2006015240896,53.3440560529881));
#104601=CARTESIAN_POINT('Ctrl Pts',(7.26055169692385,30.1181850272333,53.3361411953126));
#104602=CARTESIAN_POINT('Ctrl Pts',(7.24932615985716,29.9354491086202,53.3322450857504));
#104603=CARTESIAN_POINT('Ctrl Pts',(7.24330772727876,29.8354035698146,53.3391330739407));
#104604=CARTESIAN_POINT('Ctrl Pts',(7.23526172914461,29.7086784113402,53.3594249074209));
#104605=CARTESIAN_POINT('Ctrl Pts',(7.23346983411112,29.6808888727648,53.3646031641164));
#104606=CARTESIAN_POINT('Ctrl Pts',(7.2304038875109,29.6343733939767,53.3745014630549));
#104607=CARTESIAN_POINT('Ctrl Pts',(7.22914614300898,29.6155728345928,53.3788448608118));
#104608=CARTESIAN_POINT('Ctrl Pts',(7.2273285319046,29.5888832143918,53.3855011750096));
#104609=CARTESIAN_POINT('Ctrl Pts',(7.22678270326308,29.5809284966649,53.3875476641457));
#104610=CARTESIAN_POINT('Ctrl Pts',(7.2258288866033,29.5671394418894,53.3912040632634));
#104611=CARTESIAN_POINT('Ctrl Pts',(7.22542242692411,29.5612982173978,53.392787079001));
#104612=CARTESIAN_POINT('Ctrl Pts',(7.22454524027695,29.5487690208073,53.3962559790522));
#104613=CARTESIAN_POINT('Ctrl Pts',(7.22407398737323,29.5420842835327,53.3981518569107));
#104614=CARTESIAN_POINT('Ctrl Pts',(7.22276388077397,29.5236226667169,53.4035128129715));
#104615=CARTESIAN_POINT('Ctrl Pts',(7.22192028030396,29.5118722035352,53.4070662492671));
#104616=CARTESIAN_POINT('Ctrl Pts',(7.21598088644478,29.4300234107072,53.4328086249645));
#104617=CARTESIAN_POINT('Ctrl Pts',(7.21068106986272,29.3614290365905,53.4594848761912));
#104618=CARTESIAN_POINT('Ctrl Pts',(7.2043306767875,29.2822392106961,53.4964812803225));
#104619=CARTESIAN_POINT('Ctrl Pts',(7.20331972864838,29.2697237864708,53.5025202039802));
#104620=CARTESIAN_POINT('Ctrl Pts',(7.1969422456024,29.1912900315833,53.541583086263));
#104621=CARTESIAN_POINT('Ctrl Pts',(7.19157598349826,29.1275450601664,53.5787979027861));
#104622=CARTESIAN_POINT('Ctrl Pts',(7.18328404853701,29.0313014756086,53.6439091856491));
#104623=CARTESIAN_POINT('Ctrl Pts',(7.18029032177354,28.9970510838288,53.6690405338959));
#104624=CARTESIAN_POINT('Ctrl Pts',(7.17522063532679,28.9398529346135,53.714473197895));
#104625=CARTESIAN_POINT('Ctrl Pts',(7.17312323042974,28.9164366852389,53.7341478304714));
#104626=CARTESIAN_POINT('Ctrl Pts',(7.17010525881311,28.8831275755497,53.763736588488));
#104627=CARTESIAN_POINT('Ctrl Pts',(7.16916427670842,28.8727981580041,53.7731474158654));
#104628=CARTESIAN_POINT('Ctrl Pts',(7.16750994286101,28.854742919506,53.790017562803));
#104629=CARTESIAN_POINT('Ctrl Pts',(7.16679438823088,28.8469686512666,53.7974236004051));
#104630=CARTESIAN_POINT('Ctrl Pts',(7.1652976051002,28.8307844177705,53.8131424974093));
#104631=CARTESIAN_POINT('Ctrl Pts',(7.16451710507027,28.8223902360731,53.8214708042556));
#104632=CARTESIAN_POINT('Ctrl Pts',(7.16245269001489,28.800315254679,53.8438439148331));
#104633=CARTESIAN_POINT('Ctrl Pts',(7.16117566066175,28.786792242434,53.858042307682));
#104634=CARTESIAN_POINT('Ctrl Pts',(7.15456574329001,28.7175700548323,53.9333395950971));
#104635=CARTESIAN_POINT('Ctrl Pts',(7.14941670621357,28.6662218487224,53.998286806429));
#104636=CARTESIAN_POINT('Ctrl Pts',(7.13819117751702,28.563838711539,54.1496974733098));
#104637=CARTESIAN_POINT('Ctrl Pts',(7.13217264094968,28.5153634203465,54.2374873646948));
#104638=CARTESIAN_POINT('Ctrl Pts',(7.12412651774114,28.4636793968143,54.3549620789907));
#104639=CARTESIAN_POINT('Ctrl Pts',(7.1223346087697,28.4529577285925,54.3811179872377));
#104640=CARTESIAN_POINT('Ctrl Pts',(7.11926864072834,28.4360452612514,54.4255664632346));
#104641=CARTESIAN_POINT('Ctrl Pts',(7.11801088902014,28.4294975488458,54.4437174404057));
#104642=CARTESIAN_POINT('Ctrl Pts',(7.1161932693053,28.4206142719863,54.4697508229514));
#104643=CARTESIAN_POINT('Ctrl Pts',(7.11564743944051,28.4180192569503,54.4775438877387));
#104644=CARTESIAN_POINT('Ctrl Pts',(7.11469362140238,28.4136124617742,54.4911117928085));
#104645=CARTESIAN_POINT('Ctrl Pts',(7.11428716158187,28.4117743508658,54.4968778329816));
#104646=CARTESIAN_POINT('Ctrl Pts',(7.11340997553306,28.4078933405523,54.5092855554374));
#104647=CARTESIAN_POINT('Ctrl Pts',(7.11293872337768,28.4058605914589,54.5159299400975));
#104648=CARTESIAN_POINT('Ctrl Pts',(7.11162862083806,28.4003516617981,54.5343478820785));
#104649=CARTESIAN_POINT('Ctrl Pts',(7.11078502372491,28.3969640411088,54.5461471678704));
#104650=CARTESIAN_POINT('Ctrl Pts',(7.10484654088162,28.3742029633798,54.6288609597439));
#104651=CARTESIAN_POINT('Ctrl Pts',(7.09954770427299,28.3594135002388,54.700945267841));
#104652=CARTESIAN_POINT('Ctrl Pts',(7.09319754130338,28.3475444176817,54.7875384218401));
#104653=CARTESIAN_POINT('Ctrl Pts',(7.09218585424388,28.345828608473,54.8013385351312));
#104654=CARTESIAN_POINT('Ctrl Pts',(7.08580768599559,28.3361058679432,54.8884297715622));
#104655=CARTESIAN_POINT('Ctrl Pts',(7.0804414722535,28.3327982581748,54.9621679190801));
#104656=CARTESIAN_POINT('Ctrl Pts',(7.07214942250059,28.3353012656139,55.0783417573029));
#104657=CARTESIAN_POINT('Ctrl Pts',(7.06915554129466,28.3378389444276,55.1207494660266));
#104658=CARTESIAN_POINT('Ctrl Pts',(7.06408562539641,28.3449867833987,55.1934483901222));
#104659=CARTESIAN_POINT('Ctrl Pts',(7.06198814285379,28.3488162459197,55.223793319982));
#104660=CARTESIAN_POINT('Ctrl Pts',(7.05897008198878,28.3556095415329,55.2678269228894));
#104661=CARTESIAN_POINT('Ctrl Pts',(7.05802908657451,28.3579137034547,55.2816094030332));
#104662=CARTESIAN_POINT('Ctrl Pts',(7.05637473772187,28.3622945595824,55.3059283734798));
#104663=CARTESIAN_POINT('Ctrl Pts',(7.05565918126057,28.3643002089105,55.3164766689362));
#104664=CARTESIAN_POINT('Ctrl Pts',(7.05416240249325,28.3687285654756,55.3385990457935));
#104665=CARTESIAN_POINT('Ctrl Pts',(7.05338190857903,28.371172808747,55.350168245385));
#104666=CARTESIAN_POINT('Ctrl Pts',(7.05131752889043,28.377996614594,55.3808482393211));
#104667=CARTESIAN_POINT('Ctrl Pts',(7.05004052835716,28.3825907787712,55.3999097740509));
#104668=CARTESIAN_POINT('Ctrl Pts',(7.04343161517723,28.4083036029674,55.4988898249042));
#104669=CARTESIAN_POINT('Ctrl Pts',(7.03828347913053,28.4350130610867,55.5772407237078));
#104670=CARTESIAN_POINT('Ctrl Pts',(7.02705801160689,28.5066852030141,55.7453772133003));
#104671=CARTESIAN_POINT('Ctrl Pts',(7.02103871636445,28.5541548375283,55.8337299911078));
#104672=CARTESIAN_POINT('Ctrl Pts',(7.01299168066608,28.6248265325165,55.9408788146017));
#104673=CARTESIAN_POINT('Ctrl Pts',(7.01119967001764,28.6409870709111,55.9640740054108));
#104674=CARTESIAN_POINT('Ctrl Pts',(7.0081335455616,28.6691588513973,56.0023922296672));
#104675=CARTESIAN_POINT('Ctrl Pts',(7.0068757412808,28.6808575139882,56.0177383596366));
#104676=CARTESIAN_POINT('Ctrl Pts',(7.00505805874144,28.6979119064701,56.0393219263367));
#104677=CARTESIAN_POINT('Ctrl Pts',(7.0045122199458,28.7030518396532,56.0457288999806));
#104678=CARTESIAN_POINT('Ctrl Pts',(7.00355839183945,28.7120608339707,56.0567901086185));
#104679=CARTESIAN_POINT('Ctrl Pts',(7.00315193098186,28.7159082194527,56.0614616935405));
#104680=CARTESIAN_POINT('Ctrl Pts',(7.00227474928508,28.7242275245877,56.0714517586226));
#104681=CARTESIAN_POINT('Ctrl Pts',(7.00180350258308,28.7287072188928,56.0767631774803));
#104682=CARTESIAN_POINT('Ctrl Pts',(7.00049342962972,28.7411928041527,56.0913803809645));
#104683=CARTESIAN_POINT('Ctrl Pts',(6.9996498569816,28.7492683373594,56.1006257212308));
#104684=CARTESIAN_POINT('Ctrl Pts',(6.99371799094271,28.8063513016481,56.164538102448));
#104685=CARTESIAN_POINT('Ctrl Pts',(6.98842627154945,28.8588185625995,56.2159970168365));
#104686=CARTESIAN_POINT('Ctrl Pts',(6.98207783193072,28.9251053585262,56.2729308396778));
#104687=CARTESIAN_POINT('Ctrl Pts',(6.9810608300407,28.9358239663894,56.2819051363999));
#104688=CARTESIAN_POINT('Ctrl Pts',(6.97467776353723,29.0037698176388,56.3373541713216));
#104689=CARTESIAN_POINT('Ctrl Pts',(6.96931192600109,29.0639198853448,56.3801253889907));
#104690=CARTESIAN_POINT('Ctrl Pts',(6.96101902013396,29.162885727613,56.4410414137333));
#104691=CARTESIAN_POINT('Ctrl Pts',(6.95802397280665,29.1999037731808,56.4619190095447));
#104692=CARTESIAN_POINT('Ctrl Pts',(6.95295232449897,29.2648788890727,56.4953556397664));
#104693=CARTESIAN_POINT('Ctrl Pts',(6.95085425575586,29.2924572810486,56.5086003616544));
#104694=CARTESIAN_POINT('Ctrl Pts',(6.94783552110862,29.3331450845323,56.5267795528042));
#104695=CARTESIAN_POINT('Ctrl Pts',(6.94689442522416,29.3459753432158,56.5323195000149));
#104696=CARTESIAN_POINT('Ctrl Pts',(6.9452399630988,29.3687842577523,56.5418294231166));
#104697=CARTESIAN_POINT('Ctrl Pts',(6.94452439281197,29.3787342861965,56.5458655198237));
#104698=CARTESIAN_POINT('Ctrl Pts',(6.94302764696574,29.3997215015171,56.5541433376583));
#104699=CARTESIAN_POINT('Ctrl Pts',(6.94224719920249,29.4107662604548,56.5583643354625));
#104700=CARTESIAN_POINT('Ctrl Pts',(6.9401830863956,29.4402388992497,56.5692698110047));
#104701=CARTESIAN_POINT('Ctrl Pts',(6.93890630334014,29.4587417514493,56.5757473752566));
#104702=CARTESIAN_POINT('Ctrl Pts',(6.93230491513963,29.5557334685815,56.6077925756956));
#104703=CARTESIAN_POINT('Ctrl Pts',(6.92716353017965,29.635932808174,56.6278290094954));
#104704=CARTESIAN_POINT('Ctrl Pts',(6.91593851664298,29.8160427756509,56.6588417077554));
#104705=CARTESIAN_POINT('Ctrl Pts',(6.90991353420581,29.9161157124277,56.6669004632127));
#104706=CARTESIAN_POINT('Ctrl Pts',(6.9018596587187,30.0445772531729,56.6656435942839));
#104707=CARTESIAN_POINT('Ctrl Pts',(6.90006688643726,30.0728419352257,56.6646469856563));
#104708=CARTESIAN_POINT('Ctrl Pts',(6.89699959035963,30.1203327782595,56.6617606946654));
#104709=CARTESIAN_POINT('Ctrl Pts',(6.89574139231349,30.1395768529188,56.6602550430834));
#104710=CARTESIAN_POINT('Ctrl Pts',(6.89392323923254,30.1669670377126,56.6576324970088));
#104711=CARTESIAN_POINT('Ctrl Pts',(6.89337733355555,30.175138559673,56.6567890525774));
#104712=CARTESIAN_POINT('Ctrl Pts',(6.89242343004667,30.1893188763338,56.6552193189123));
#104713=CARTESIAN_POINT('Ctrl Pts',(6.89201696141894,30.1953304928817,56.6545206640732));
#104714=CARTESIAN_POINT('Ctrl Pts',(6.89113981230245,30.2082352267473,56.6529495946015));
#104715=CARTESIAN_POINT('Ctrl Pts',(6.89066860642839,30.2151266293412,56.6520668270076));
#104716=CARTESIAN_POINT('Ctrl Pts',(6.88935875496266,30.2341757532931,56.6495054849027));
#104717=CARTESIAN_POINT('Ctrl Pts',(6.88851536546236,30.2463204716164,56.647735667917));
#104718=CARTESIAN_POINT('Ctrl Pts',(6.88262969400869,30.3303171094864,56.6345457222853));
#104719=CARTESIAN_POINT('Ctrl Pts',(6.87738763181497,30.401366034414,56.6185648188023));
#104720=CARTESIAN_POINT('Ctrl Pts',(6.87109326932466,30.4844775195886,56.5940611789448));
#104721=CARTESIAN_POINT('Ctrl Pts',(6.87008132834552,30.4977705925252,56.5899603588245));
#104722=CARTESIAN_POINT('Ctrl Pts',(6.86359730198435,30.5825668622907,56.5626336417741));
#104723=CARTESIAN_POINT('Ctrl Pts',(6.85812428195912,30.6524847319064,56.5347550690545));
#104724=CARTESIAN_POINT('Ctrl Pts',(6.84975947777016,30.7582232870142,56.484056524513));
#104725=CARTESIAN_POINT('Ctrl Pts',(6.84679413727263,30.7954625197656,56.4644337435514));
#104726=CARTESIAN_POINT('Ctrl Pts',(6.84176665891241,30.8582369938003,56.4282534127869));
#104727=CARTESIAN_POINT('Ctrl Pts',(6.83968355767121,30.884134231174,56.4123687262163));
#104728=CARTESIAN_POINT('Ctrl Pts',(6.83668203430711,30.9212607597868,56.3881746486524));
#104729=CARTESIAN_POINT('Ctrl Pts',(6.8357435101111,30.9328416894826,56.3804190108606));
#104730=CARTESIAN_POINT('Ctrl Pts',(6.83409194485034,30.9531659548508,56.3664354521437));
#104731=CARTESIAN_POINT('Ctrl Pts',(6.83337672591566,30.9619488489477,56.3602667398843));
#104732=CARTESIAN_POINT('Ctrl Pts',(6.83187912442134,30.9802961078255,56.3471138684557));
#104733=CARTESIAN_POINT('Ctrl Pts',(6.8310974849964,30.9898468808998,56.3401117110762));
#104734=CARTESIAN_POINT('Ctrl Pts',(6.82902648110482,31.0150768851456,56.3211974170714));
#104735=CARTESIAN_POINT('Ctrl Pts',(6.82774408281731,31.0306212690898,56.3091079216888));
#104736=CARTESIAN_POINT('Ctrl Pts',(6.82091056443519,31.1129362713106,56.2427130537237));
#104737=CARTESIAN_POINT('Ctrl Pts',(6.81556036864427,31.1756411298718,56.1835681352485));
#104738=CARTESIAN_POINT('Ctrl Pts',(6.80431808609745,31.2988208924428,56.0478854006752));
#104739=CARTESIAN_POINT('Ctrl Pts',(6.7984670929878,31.3577160787612,55.9703629809232));
#104740=CARTESIAN_POINT('Ctrl Pts',(6.7906228232605,31.4243845589283,55.8645591368767));
#104741=CARTESIAN_POINT('Ctrl Pts',(6.78885380496981,31.4386573981902,55.8405941882899));
#104742=CARTESIAN_POINT('Ctrl Pts',(6.78582307910406,31.4616839088293,55.7996257246469));
#104743=CARTESIAN_POINT('Ctrl Pts',(6.78457719509404,31.4707588344152,55.7828087404315));
#104744=CARTESIAN_POINT('Ctrl Pts',(6.78277376261574,31.4833035174229,55.7585734185253));
#104745=CARTESIAN_POINT('Ctrl Pts',(6.78222995566122,31.4870113073347,55.7512791232499));
#104746=CARTESIAN_POINT('Ctrl Pts',(6.7812784142699,31.4933660117108,55.7385462322214));
#104747=CARTESIAN_POINT('Ctrl Pts',(6.78087218547185,31.4960372853206,55.7331200594789));
#104748=CARTESIAN_POINT('Ctrl Pts',(6.77999399613911,31.5017218074526,55.721412602477));
#104749=CARTESIAN_POINT('Ctrl Pts',(6.77952149508007,31.5047251793298,55.7151270238548));
#104750=CARTESIAN_POINT('Ctrl Pts',(6.77820461129838,31.5129460086804,55.6976410579305));
#104751=CARTESIAN_POINT('Ctrl Pts',(6.77735540540176,31.5180782928327,55.6864014460978));
#104752=CARTESIAN_POINT('Ctrl Pts',(6.77401858093961,31.5376086796873,55.6423395834222));
#104753=CARTESIAN_POINT('Ctrl Pts',(6.7714867893049,31.5510657685036,55.6091252973127));
#104754=CARTESIAN_POINT('Ctrl Pts',(6.76892549910492,31.5634376526692,55.5755160347169));
#104755=CARTESIAN_POINT('Origin',(5.,30.,55.));
#104756=CARTESIAN_POINT('',(6.06643882015546,31.5634376718251,55.5755159826781));
#104757=CARTESIAN_POINT('',(6.26189397015589,31.5634377553307,55.5755157558283));
#104758=CARTESIAN_POINT('',(5.,31.5634376782623,55.5755159651912));
#104759=CARTESIAN_POINT('',(6.92208051667986,31.665999351236,54.9985297343455));
#104760=CARTESIAN_POINT('Ctrl Pts',(6.26189397015589,31.5634377553307,55.5755157558282));
#104761=CARTESIAN_POINT('Ctrl Pts',(6.26454446910789,31.5505005284184,55.6106608388241));
#104762=CARTESIAN_POINT('Ctrl Pts',(6.26716434398739,31.5363749856231,55.6453785376556));
#104763=CARTESIAN_POINT('Ctrl Pts',(6.27128114969912,31.5120082168646,55.6999156178218));
#104764=CARTESIAN_POINT('Ctrl Pts',(6.27280066409409,31.5025288324042,55.7200402144111));
#104765=CARTESIAN_POINT('Ctrl Pts',(6.27523278931301,31.4865707133745,55.7522305388054));
#104766=CARTESIAN_POINT('Ctrl Pts',(6.27615385824067,31.4803415632221,55.7644162118716));
#104767=CARTESIAN_POINT('Ctrl Pts',(6.27778610711501,31.4689728440355,55.7859957995209));
#104768=CARTESIAN_POINT('Ctrl Pts',(6.27849928604317,31.4638915984733,55.7954193928292));
#104769=CARTESIAN_POINT('Ctrl Pts',(6.28000407604947,31.4529300348091,55.8152876555579));
#104770=CARTESIAN_POINT('Ctrl Pts',(6.28079483181936,31.4470271076433,55.8257192075521));
#104771=CARTESIAN_POINT('Ctrl Pts',(6.28291780609597,31.430797396761,55.8536914463546));
#104772=CARTESIAN_POINT('Ctrl Pts',(6.28424241371186,31.4202606939117,55.8711084296106));
#104773=CARTESIAN_POINT('Ctrl Pts',(6.29309777851616,31.3471139573512,55.9871618018824));
#104774=CARTESIAN_POINT('Ctrl Pts',(6.30023260538611,31.2745965825394,56.0791720623636));
#104775=CARTESIAN_POINT('Ctrl Pts',(6.31334400596743,31.1247264743723,56.2329336508886));
#104776=CARTESIAN_POINT('Ctrl Pts',(6.31930587690848,31.0503782129085,56.296856046941));
#104777=CARTESIAN_POINT('Ctrl Pts',(6.32668323572236,30.9579381238079,56.3631447112663));
#104778=CARTESIAN_POINT('Ctrl Pts',(6.32772465881346,30.9448818417876,56.3722270995284));
#104779=CARTESIAN_POINT('Ctrl Pts',(6.32928199749853,30.9253877519606,56.3853777286699));
#104780=CARTESIAN_POINT('Ctrl Pts',(6.32978880196477,30.9190484240044,56.3895912820912));
#104781=CARTESIAN_POINT('Ctrl Pts',(6.33070053847853,30.9076576361282,56.3970503443272));
#104782=CARTESIAN_POINT('Ctrl Pts',(6.33110438354637,30.9026171944378,56.4003121961606));
#104783=CARTESIAN_POINT('Ctrl Pts',(6.33200898553347,30.8913385735679,56.4075248017062));
#104784=CARTESIAN_POINT('Ctrl Pts',(6.33251060968784,30.8850917710684,56.4114613249073));
#104785=CARTESIAN_POINT('Ctrl Pts',(6.33402030053552,30.8663076021315,56.4231247413204));
#104786=CARTESIAN_POINT('Ctrl Pts',(6.33503577436208,30.8536941119497,56.4307268142366));
#104787=CARTESIAN_POINT('Ctrl Pts',(6.33742713999119,30.8240036485659,56.4480886800526));
#104788=CARTESIAN_POINT('Ctrl Pts',(6.33880943489345,30.8068515265934,56.4577151231761));
#104789=CARTESIAN_POINT('Ctrl Pts',(6.34382784273806,30.7444902529549,56.4912769187487));
#104790=CARTESIAN_POINT('Ctrl Pts',(6.34752594371102,30.6983567311009,56.5134298214047));
#104791=CARTESIAN_POINT('Ctrl Pts',(6.3603275807005,30.5362156595595,56.5822948592716));
#104792=CARTESIAN_POINT('Ctrl Pts',(6.36944846596878,30.415995421047,56.6180671883888));
#104793=CARTESIAN_POINT('Ctrl Pts',(6.38042235669413,30.2608017692666,56.6457828247175));
#104794=CARTESIAN_POINT('Ctrl Pts',(6.38266379850855,30.2285478146143,56.6505710594049));
#104795=CARTESIAN_POINT('Ctrl Pts',(6.38577515583164,30.1830098682816,56.6559707327709));
#104796=CARTESIAN_POINT('Ctrl Pts',(6.38666951785534,30.1698291795518,56.6573743533363));
#104797=CARTESIAN_POINT('Ctrl Pts',(6.38829176844728,30.1457602698896,56.6596473149358));
#104798=CARTESIAN_POINT('Ctrl Pts',(6.38902119924368,30.134877684636,56.6605671580019));
#104799=CARTESIAN_POINT('Ctrl Pts',(6.390491444365,30.1128247724441,56.6622129380143));
#104800=CARTESIAN_POINT('Ctrl Pts',(6.39123205219052,30.1016545961667,56.662933442449));
#104801=CARTESIAN_POINT('Ctrl Pts',(6.39306106574678,30.0739228494996,56.6644417347846));
#104802=CARTESIAN_POINT('Ctrl Pts',(6.39414523447107,30.0573549430988,56.665094988));
#104803=CARTESIAN_POINT('Ctrl Pts',(6.39840371105517,29.9918098899949,56.6666998490327));
#104804=CARTESIAN_POINT('Ctrl Pts',(6.40151881609411,29.9428081657521,56.6657386500724));
#104805=CARTESIAN_POINT('Ctrl Pts',(6.41006368516231,29.8066567670543,56.6570514779924));
#104806=CARTESIAN_POINT('Ctrl Pts',(6.41537171933191,29.7199699196642,56.6446231657939));
#104807=CARTESIAN_POINT('Ctrl Pts',(6.42592259687318,29.5515755374984,56.6067739525485));
#104808=CARTESIAN_POINT('Ctrl Pts',(6.43115064643243,29.470059040529,56.5817604281636));
#104809=CARTESIAN_POINT('Ctrl Pts',(6.43771151061711,29.3758321436095,56.5447426549644));
#104810=CARTESIAN_POINT('Ctrl Pts',(6.43876536389152,29.3609289023786,56.538636886488));
#104811=CARTESIAN_POINT('Ctrl Pts',(6.44034482983503,29.3389807224503,56.5292709760042));
#104812=CARTESIAN_POINT('Ctrl Pts',(6.44086117112911,29.3318657861061,56.5261758973357));
#104813=CARTESIAN_POINT('Ctrl Pts',(6.44178282691114,29.319278120031,56.5205952286167));
#104814=CARTESIAN_POINT('Ctrl Pts',(6.44218694594865,29.3137968439858,56.5181295575934));
#104815=CARTESIAN_POINT('Ctrl Pts',(6.44308321191695,29.3017251270598,56.5126205387022));
#104816=CARTESIAN_POINT('Ctrl Pts',(6.44357613005769,29.2951412642526,56.5095637945923));
#104817=CARTESIAN_POINT('Ctrl Pts',(6.44503397754371,29.2758244845402,56.5004415153977));
#104818=CARTESIAN_POINT('Ctrl Pts',(6.44600560684886,29.2631487373168,56.4942573748045));
#104819=CARTESIAN_POINT('Ctrl Pts',(6.44827568555491,29.2339561352245,56.4795533652609));
#104820=CARTESIAN_POINT('Ctrl Pts',(6.44957972780327,29.217500477524,56.4709166525838));
#104821=CARTESIAN_POINT('Ctrl Pts',(6.45419605412011,29.1602319945494,56.4396264876734));
#104822=CARTESIAN_POINT('Ctrl Pts',(6.45756136787187,29.1202316004384,56.415535851681));
#104823=CARTESIAN_POINT('Ctrl Pts',(6.46884788794875,28.990478027427,56.3297645834281));
#104824=CARTESIAN_POINT('Ctrl Pts',(6.47681751322673,28.9057507187853,56.2609645375228));
#104825=CARTESIAN_POINT('Ctrl Pts',(6.48803071237488,28.7929972894757,56.1494223992228));
#104826=CARTESIAN_POINT('Ctrl Pts',(6.49148758115324,28.7592352638556,56.1128931405395));
#104827=CARTESIAN_POINT('Ctrl Pts',(6.49604405202577,28.7161035616119,56.0618188669129));
#104828=CARTESIAN_POINT('Ctrl Pts',(6.49720329321096,28.7052546358374,56.0485627547598));
#104829=CARTESIAN_POINT('Ctrl Pts',(6.49911395594621,28.6875878488317,56.0262836533291));
#104830=CARTESIAN_POINT('Ctrl Pts',(6.49986996430184,28.6806541798109,56.0173546133259));
#104831=CARTESIAN_POINT('Ctrl Pts',(6.50135219851044,28.6671751897656,55.9996270580687));
#104832=CARTESIAN_POINT('Ctrl Pts',(6.50207859914733,28.6606247995773,55.9908331404722));
#104833=CARTESIAN_POINT('Ctrl Pts',(6.50381679899227,28.6450878940491,55.9695391520569));
#104834=CARTESIAN_POINT('Ctrl Pts',(6.50482527981346,28.6361867781769,55.9569777971918));
#104835=CARTESIAN_POINT('Ctrl Pts',(6.50840621747789,28.6050070847161,55.9116578775794));
#104836=CARTESIAN_POINT('Ctrl Pts',(6.51094160109677,28.5837233407896,55.878228974684));
#104837=CARTESIAN_POINT('Ctrl Pts',(6.51733465407905,28.5324220010151,55.7909298246603));
#104838=CARTESIAN_POINT('Ctrl Pts',(6.52113766321207,28.5041652730762,55.7360940590507));
#104839=CARTESIAN_POINT('Ctrl Pts',(6.53046096434747,28.4420461664146,55.597111564984));
#104840=CARTESIAN_POINT('Ctrl Pts',(6.53592963512186,28.4118905269714,55.5115356666956));
#104841=CARTESIAN_POINT('Ctrl Pts',(6.5441871821628,28.3783803045492,55.3841817741611));
#104842=CARTESIAN_POINT('Ctrl Pts',(6.54680688343859,28.3693952104421,55.3440544764472));
#104843=CARTESIAN_POINT('Ctrl Pts',(6.55022846062596,28.3598779541345,55.2927101588169));
#104844=CARTESIAN_POINT('Ctrl Pts',(6.55096210681504,28.3579615179349,55.281760837159));
#104845=CARTESIAN_POINT('Ctrl Pts',(6.55214261794786,28.3550777166994,55.2642547958385));
#104846=CARTESIAN_POINT('Ctrl Pts',(6.55258565012885,28.3540396268147,55.2577098393394));
#104847=CARTESIAN_POINT('Ctrl Pts',(6.55344528518027,28.3521109466256,55.2450626405104));
#104848=CARTESIAN_POINT('Ctrl Pts',(6.55386159937029,28.3512151508746,55.2389613907362));
#104849=CARTESIAN_POINT('Ctrl Pts',(6.55488547629687,28.3491048139549,55.224010871304));
#104850=CARTESIAN_POINT('Ctrl Pts',(6.55549504762872,28.347927541058,55.2151566108729));
#104851=CARTESIAN_POINT('Ctrl Pts',(6.55775468789567,28.343851205502,55.1824900073672));
#104852=CARTESIAN_POINT('Ctrl Pts',(6.55942630127973,28.3413954934318,55.1586265363298));
#104853=CARTESIAN_POINT('Ctrl Pts',(6.56382548643563,28.3363473855281,55.0964040797225));
#104854=CARTESIAN_POINT('Ctrl Pts',(6.56658085768375,28.3345661070411,55.057994391017));
#104855=CARTESIAN_POINT('Ctrl Pts',(6.57445564284476,28.3332866279909,54.9490241308927));
#104856=CARTESIAN_POINT('Ctrl Pts',(6.57961695443758,28.336939103798,54.8785070727554));
#104857=CARTESIAN_POINT('Ctrl Pts',(6.59159850107301,28.3559608983907,54.714176993236));
#104858=CARTESIAN_POINT('Ctrl Pts',(6.59834763788879,28.3749053093943,54.6210118211431));
#104859=CARTESIAN_POINT('Ctrl Pts',(6.60621506602963,28.4073224590016,54.5107827219602));
#104860=CARTESIAN_POINT('Ctrl Pts',(6.60757227508838,28.4133049482404,54.4917144820485));
#104861=CARTESIAN_POINT('Ctrl Pts',(6.60972032538783,28.4233973722518,54.4614631672848));
#104862=CARTESIAN_POINT('Ctrl Pts',(6.61051830306708,28.4272865159286,54.4502090617554));
#104863=CARTESIAN_POINT('Ctrl Pts',(6.61202727250786,28.4349064538417,54.4289018062784));
#104864=CARTESIAN_POINT('Ctrl Pts',(6.61273897981658,28.4386142852798,54.4188411455231));
#104865=CARTESIAN_POINT('Ctrl Pts',(6.61436110699777,28.4473251782979,54.3958906956219));
#104866=CARTESIAN_POINT('Ctrl Pts',(6.61526934536675,28.4523921346682,54.3830258774828));
#104867=CARTESIAN_POINT('Ctrl Pts',(6.61811410739145,28.4688563564685,54.3427033520321));
#104868=CARTESIAN_POINT('Ctrl Pts',(6.62003131306179,28.4808290646567,54.3154858779349));
#104869=CARTESIAN_POINT('Ctrl Pts',(6.62754512384627,28.5311349856975,54.2089567012364));
#104870=CARTESIAN_POINT('Ctrl Pts',(6.63295707053892,28.5750038857815,54.1324158898279));
#104871=CARTESIAN_POINT('Ctrl Pts',(6.64524356702567,28.6884929689743,53.9664280889392));
#104872=CARTESIAN_POINT('Ctrl Pts',(6.6520649630289,28.7615759199393,53.8799017507475));
#104873=CARTESIAN_POINT('Ctrl Pts',(6.66036616825373,28.8534552610495,53.7911952029906));
#104874=CARTESIAN_POINT('Ctrl Pts',(6.66133432016541,28.8642096675191,53.7810848431364));
#104875=CARTESIAN_POINT('Ctrl Pts',(6.66280258186005,28.8805478499893,53.7661290579411));
#104876=CARTESIAN_POINT('Ctrl Pts',(6.6632950194684,28.8860321876878,53.7611754257529));
#104877=CARTESIAN_POINT('Ctrl Pts',(6.6641924778081,28.8960313416976,53.7522639508771));
#104878=CARTESIAN_POINT('Ctrl Pts',(6.66459657746125,28.9005348362815,53.7482938055264));
#104879=CARTESIAN_POINT('Ctrl Pts',(6.66551666969061,28.91079132902,53.7393500475988));
#104880=CARTESIAN_POINT('Ctrl Pts',(6.66603369637194,28.9165569479355,53.7343914591472));
#104881=CARTESIAN_POINT('Ctrl Pts',(6.66763762445608,28.9344559307134,53.7192097881502));
#104882=CARTESIAN_POINT('Ctrl Pts',(6.66873330520163,28.9467011399438,53.7091207663099));
#104883=CARTESIAN_POINT('Ctrl Pts',(6.67447905426606,29.0110979182744,53.6575895359064));
#104884=CARTESIAN_POINT('Ctrl Pts',(6.67928051055774,29.065552294662,53.6191310925398));
#104885=CARTESIAN_POINT('Ctrl Pts',(6.69275118747356,29.2231754402455,53.5214105296857));
#104886=CARTESIAN_POINT('Ctrl Pts',(6.70143597850424,29.3306226233818,53.4697632686658));
#104887=CARTESIAN_POINT('Ctrl Pts',(6.71247881518522,29.4792055752419,53.4170177042953));
#104888=CARTESIAN_POINT('Ctrl Pts',(6.71515692767405,29.5161940289344,53.4053238602658));
#104889=CARTESIAN_POINT('Ctrl Pts',(6.71886141760123,29.5686923505188,53.3907217689671));
#104890=CARTESIAN_POINT('Ctrl Pts',(6.71992231224148,29.5838842042955,53.3867268094654));
#104891=CARTESIAN_POINT('Ctrl Pts',(6.72170853920639,29.6097230589536,53.3803213277282));
#104892=CARTESIAN_POINT('Ctrl Pts',(6.72243740440672,29.6203411259396,53.3777995681036));
#104893=CARTESIAN_POINT('Ctrl Pts',(6.72390771829576,29.6419079726874,53.3729008625591));
#104894=CARTESIAN_POINT('Ctrl Pts',(6.72464894932268,29.6528574887926,53.3705296595572));
#104895=CARTESIAN_POINT('Ctrl Pts',(6.72648177991336,29.6801170785309,53.3649136311013));
#104896=CARTESIAN_POINT('Ctrl Pts',(6.72756910283182,29.6964536197185,53.3618021655201));
#104897=CARTESIAN_POINT('Ctrl Pts',(6.73185891907859,29.7615180864653,53.3504167066448));
#104898=CARTESIAN_POINT('Ctrl Pts',(6.73500104308888,29.810559647094,53.3440677170322));
#104899=CARTESIAN_POINT('Ctrl Pts',(6.74366052336572,29.948374881642,53.3324300146838));
#104900=CARTESIAN_POINT('Ctrl Pts',(6.74905156999228,30.0373922657802,53.3320498827654));
#104901=CARTESIAN_POINT('Ctrl Pts',(6.75955273346603,30.2086239896618,53.3450392765063));
#104902=CARTESIAN_POINT('Ctrl Pts',(6.76464545837968,30.2906376243938,53.3574576335264));
#104903=CARTESIAN_POINT('Ctrl Pts',(6.77108085283034,30.3874783324586,53.3796020973636));
#104904=CARTESIAN_POINT('Ctrl Pts',(6.77216146633097,30.4035236290371,53.383523136123));
#104905=CARTESIAN_POINT('Ctrl Pts',(6.77376626251121,30.42698514929,53.3896275625658));
#104906=CARTESIAN_POINT('Ctrl Pts',(6.77428051695907,30.4344492606985,53.3916251870434));
#104907=CARTESIAN_POINT('Ctrl Pts',(6.7751999762385,30.4476925808438,53.395268415404));
#104908=CARTESIAN_POINT('Ctrl Pts',(6.77560400927407,30.4534771725202,53.3968934666513));
#104909=CARTESIAN_POINT('Ctrl Pts',(6.77650198477888,30.4662556828926,53.4005580007246));
#104910=CARTESIAN_POINT('Ctrl Pts',(6.77699671860619,30.4732449875346,53.4026120547537));
#104911=CARTESIAN_POINT('Ctrl Pts',(6.77846529892519,30.4938490503898,53.4088143773793));
#104912=CARTESIAN_POINT('Ctrl Pts',(6.77944598902457,30.5074239810572,53.4130912313705));
#104913=CARTESIAN_POINT('Ctrl Pts',(6.78611282510082,30.5985838192819,53.4431008466858));
#104914=CARTESIAN_POINT('Ctrl Pts',(6.79203860541199,30.6742316553096,53.4743373562673));
#104915=CARTESIAN_POINT('Ctrl Pts',(6.80751906645864,30.8643624055347,53.5697565017614));
#104916=CARTESIAN_POINT('Ctrl Pts',(6.81701846628112,30.9741349591643,53.6421367851628));
#104917=CARTESIAN_POINT('Ctrl Pts',(6.82745087359127,31.0900955840493,53.7399704108144));
#104918=CARTESIAN_POINT('Ctrl Pts',(6.82886000950821,31.1056398069442,53.7535876959437));
#104919=CARTESIAN_POINT('Ctrl Pts',(6.83115152309085,31.1307114469955,53.7763895496966));
#104920=CARTESIAN_POINT('Ctrl Pts',(6.83204083996111,31.1403895244257,53.7854043221947));
#104921=CARTESIAN_POINT('Ctrl Pts',(6.83363841356968,31.1576763151014,53.8018951252541));
#104922=CARTESIAN_POINT('Ctrl Pts',(6.83434834825031,31.1653224387397,53.8093307074249));
#104923=CARTESIAN_POINT('Ctrl Pts',(6.83516741448436,31.1741003032443,53.8180324243905));
#104924=CARTESIAN_POINT('Ctrl Pts',(6.83527963444615,31.1753019998948,53.8192273373126));
#104925=CARTESIAN_POINT('Ctrl Pts',(6.83544884750548,31.1771125480504,53.8210331670805));
#104926=CARTESIAN_POINT('Ctrl Pts',(6.83550589996095,31.1777227489705,53.8216427237616));
#104927=CARTESIAN_POINT('Ctrl Pts',(6.83560860012256,31.1788207204448,53.8227412408269));
#104928=CARTESIAN_POINT('Ctrl Pts',(6.83565425526253,31.179308660484,53.823230030843));
#104929=CARTESIAN_POINT('Ctrl Pts',(6.83573741773183,31.1801971665912,53.8241211923311));
#104930=CARTESIAN_POINT('Ctrl Pts',(6.8357749293641,31.1805978309797,53.8245234652099));
#104931=CARTESIAN_POINT('Ctrl Pts',(6.83584390436646,31.181334356579,53.8252637040641));
#104932=CARTESIAN_POINT('Ctrl Pts',(6.83587537038675,31.1816702784592,53.8256016093207));
#104933=CARTESIAN_POINT('Ctrl Pts',(6.83593367511896,31.1822925792425,53.826228121663));
#104934=CARTESIAN_POINT('Ctrl Pts',(6.83596051554893,31.1825789974935,53.8265166895118));
#104935=CARTESIAN_POINT('Ctrl Pts',(6.83601056864273,31.1831130163785,53.8270551103278));
#104936=CARTESIAN_POINT('Ctrl Pts',(6.83603378245821,31.1833606434847,53.8273049368296));
#104937=CARTESIAN_POINT('Ctrl Pts',(6.83607730787514,31.1838248598031,53.8277735730241));
#104938=CARTESIAN_POINT('Ctrl Pts',(6.83609762027836,31.1840414674615,53.8279923643081));
#104939=CARTESIAN_POINT('Ctrl Pts',(6.83613588347032,31.1844494378197,53.8284046759575));
#104940=CARTESIAN_POINT('Ctrl Pts',(6.83615383483775,31.1846408137845,53.8285981832071));
#104941=CARTESIAN_POINT('Ctrl Pts',(6.83618778774809,31.1850027309763,53.8289643103386));
#104942=CARTESIAN_POINT('Ctrl Pts',(6.83620378971336,31.1851732819139,53.8291369205926));
#104943=CARTESIAN_POINT('Ctrl Pts',(6.83623416348085,31.1854969709265,53.8294646611739));
#104944=CARTESIAN_POINT('Ctrl Pts',(6.83624853559594,31.1856501162387,53.8296197842668));
#104945=CARTESIAN_POINT('Ctrl Pts',(6.83627590190537,31.185941693009,53.8299152425401));
#104946=CARTESIAN_POINT('Ctrl Pts',(6.8362888963381,31.1860801299844,53.8300555722115));
#104947=CARTESIAN_POINT('Ctrl Pts',(6.83631370920196,31.1863444497915,53.8303236009039));
#104948=CARTESIAN_POINT('Ctrl Pts',(6.83632552782,31.1864703369218,53.8304512956879));
#104949=CARTESIAN_POINT('Ctrl Pts',(6.8363481527537,31.1867113073393,53.8306958052231));
#104950=CARTESIAN_POINT('Ctrl Pts',(6.83635895921926,31.1868263940369,53.8308126166831));
#104951=CARTESIAN_POINT('Ctrl Pts',(6.83637969407458,31.1870471983068,53.8310367962609));
#104952=CARTESIAN_POINT('Ctrl Pts',(6.83638962257781,31.1871529185312,53.8311441617004));
#104953=CARTESIAN_POINT('Ctrl Pts',(6.83640871267701,31.1873561777663,53.8313506400732));
#104954=CARTESIAN_POINT('Ctrl Pts',(6.83641787437143,31.1874537189872,53.8314497509304));
#104955=CARTESIAN_POINT('Ctrl Pts',(6.83646162549998,31.1879194894079,53.8319231350813));
#104956=CARTESIAN_POINT('Ctrl Pts',(6.83649620782555,31.1882875543859,53.8322975705405));
#104957=CARTESIAN_POINT('Ctrl Pts',(6.83656536217928,31.1890233837649,53.8330468438649));
#104958=CARTESIAN_POINT('Ctrl Pts',(6.83659993420023,31.1893911480616,53.8334216817259));
#104959=CARTESIAN_POINT('Ctrl Pts',(6.83771236570147,31.2012216974717,53.8454911891868));
#104960=CARTESIAN_POINT('Ctrl Pts',(6.83878273897157,31.2125119319482,53.8573543826887));
#104961=CARTESIAN_POINT('Ctrl Pts',(6.84310574479034,31.2576969066564,53.9062564182439));
#104962=CARTESIAN_POINT('Ctrl Pts',(6.84629563101873,31.2900859938941,53.9446538966336));
#104963=CARTESIAN_POINT('Ctrl Pts',(6.85518459504228,31.3766862732671,54.0572760669948));
#104964=CARTESIAN_POINT('Ctrl Pts',(6.86074737879746,31.4265610848228,54.1345995941727));
#104965=CARTESIAN_POINT('Ctrl Pts',(6.86673819339692,31.4726450709742,54.2209565011216));
#104966=CARTESIAN_POINT('Ctrl Pts',(6.8671070829813,31.4754519351859,54.2262856698189));
#104967=CARTESIAN_POINT('Ctrl Pts',(6.87233807994812,31.5148072795536,54.3019995035082));
#104968=CARTESIAN_POINT('Ctrl Pts',(6.8772486017718,31.5463086025132,54.3748822613228));
#104969=CARTESIAN_POINT('Ctrl Pts',(6.88323164472075,31.5765647727414,54.4613431812816));
#104970=CARTESIAN_POINT('Ctrl Pts',(6.88404231908957,31.5805031617025,54.4730110201292));
#104971=CARTESIAN_POINT('Ctrl Pts',(6.88532236569692,31.5864638871805,54.4913382709559));
#104972=CARTESIAN_POINT('Ctrl Pts',(6.88578682527168,31.5885745438602,54.4979687916753));
#104973=CARTESIAN_POINT('Ctrl Pts',(6.88665986328564,31.5924433051095,54.5103910192878));
#104974=CARTESIAN_POINT('Ctrl Pts',(6.88706786060929,31.5942114644677,54.5161793349988));
#104975=CARTESIAN_POINT('Ctrl Pts',(6.88803314046332,31.5983018160076,54.5298355594006));
#104976=CARTESIAN_POINT('Ctrl Pts',(6.88859189828572,31.6005974776023,54.5377111250451));
#104977=CARTESIAN_POINT('Ctrl Pts',(6.89047019066464,31.6080779994046,54.5640978394452));
#104978=CARTESIAN_POINT('Ctrl Pts',(6.89180315187381,31.6130004002564,54.5826809661126));
#104979=CARTESIAN_POINT('Ctrl Pts',(6.90252368276676,31.6496326427416,54.7313212070418));
#104980=CARTESIAN_POINT('Ctrl Pts',(6.91245003382505,31.6658812228862,54.8646751798091));
#104981=CARTESIAN_POINT('Ctrl Pts',(6.92208051667986,31.665999351236,54.9985297343455));
#104982=CARTESIAN_POINT('Ctrl Pts',(6.92208062419127,31.6659993525541,54.998531228652));
#104983=CARTESIAN_POINT('Ctrl Pts',(6.92752430250826,31.6660660573411,55.0741931974836));
#104984=CARTESIAN_POINT('Ctrl Pts',(6.93286713313332,31.6609784705008,55.1497823894655));
#104985=CARTESIAN_POINT('Ctrl Pts',(6.9390761915014,31.6487537501628,55.2395615832835));
#104986=CARTESIAN_POINT('Ctrl Pts',(6.94009265401845,31.6465417946736,55.2543203183327));
#104987=CARTESIAN_POINT('Ctrl Pts',(6.94184206420286,31.6423685301795,55.2798228409888));
#104988=CARTESIAN_POINT('Ctrl Pts',(6.94257785034269,31.640499366719,55.2905805377481));
#104989=CARTESIAN_POINT('Ctrl Pts',(6.94404681408289,31.6365387213767,55.3121178717952));
#104990=CARTESIAN_POINT('Ctrl Pts',(6.94477991743677,31.6344461590539,55.3228967568165));
#104991=CARTESIAN_POINT('Ctrl Pts',(6.9461716460916,31.630252263745,55.3434134165066));
#104992=CARTESIAN_POINT('Ctrl Pts',(6.94683083937543,31.6281698637739,55.3531545272042));
#104993=CARTESIAN_POINT('Ctrl Pts',(6.94853761732648,31.622528699819,55.3784318107188));
#104994=CARTESIAN_POINT('Ctrl Pts',(6.94958082868873,31.6188340829349,55.3939368704649));
#104995=CARTESIAN_POINT('Ctrl Pts',(6.95324032441697,31.6050054202772,55.4484870871939));
#104996=CARTESIAN_POINT('Ctrl Pts',(6.95581850255506,31.5936761217487,55.4872164720534));
#104997=CARTESIAN_POINT('Ctrl Pts',(6.9594761742502,31.5753775740763,55.5422672213609));
#104998=CARTESIAN_POINT('Ctrl Pts',(6.96058317929051,31.5695388628525,55.5589415810635));
#104999=CARTESIAN_POINT('Ctrl Pts',(6.9616842973919,31.5634376940719,55.5755159222429));
#105000=CARTESIAN_POINT('Ctrl Pts',(6.76892549910492,31.5634376526692,55.5755160347169));
#105001=CARTESIAN_POINT('Ctrl Pts',(6.76565911937185,31.5792153539615,55.5326545838016));
#105002=CARTESIAN_POINT('Ctrl Pts',(6.76234507064774,31.5932281209808,55.4891507352691));
#105003=CARTESIAN_POINT('Ctrl Pts',(6.75469116315526,31.6213380402814,55.3877638984053));
#105004=CARTESIAN_POINT('Ctrl Pts',(6.75035204169247,31.6341546959461,55.3296008909939));
#105005=CARTESIAN_POINT('Ctrl Pts',(6.74215950402389,31.6526440596059,55.21739656209));
#105006=CARTESIAN_POINT('Ctrl Pts',(6.73830181290237,31.6588421481276,55.1635155351563));
#105007=CARTESIAN_POINT('Ctrl Pts',(6.731979587325,31.6647892737022,55.073164757906));
#105008=CARTESIAN_POINT('Ctrl Pts',(6.729476324338,31.665989175487,55.0368351927104));
#105009=CARTESIAN_POINT('Ctrl Pts',(6.72609830067245,31.6660038990593,54.9870677159392));
#105010=CARTESIAN_POINT('Ctrl Pts',(6.72519211718745,31.6658455943011,54.9736426591224));
#105011=CARTESIAN_POINT('Ctrl Pts',(6.72362203442421,31.665287049257,54.95025689691));
#105012=CARTESIAN_POINT('Ctrl Pts',(6.72295589879717,31.6649596662987,54.9402953119165));
#105013=CARTESIAN_POINT('Ctrl Pts',(6.72156261528189,31.6640843147945,54.9193794498966));
#105014=CARTESIAN_POINT('Ctrl Pts',(6.72083608895692,31.6635175280787,54.9084264045131));
#105015=CARTESIAN_POINT('Ctrl Pts',(6.71909601998206,31.66189363788,54.8820875302484));
#105016=CARTESIAN_POINT('Ctrl Pts',(6.71808581757055,31.6607309719811,54.8667090434471));
#105017=CARTESIAN_POINT('Ctrl Pts',(6.71448946446047,31.6558012336014,54.8116797662985));
#105018=CARTESIAN_POINT('Ctrl Pts',(6.71194083465546,31.6508260289116,54.7721490582995));
#105019=CARTESIAN_POINT('Ctrl Pts',(6.70550331699152,31.634471834921,54.6714877923803));
#105020=CARTESIAN_POINT('Ctrl Pts',(6.70167015351356,31.6210801107925,54.6107461511771));
#105021=CARTESIAN_POINT('Ctrl Pts',(6.6922398465037,31.5795632922062,54.4624378796174));
#105022=CARTESIAN_POINT('Ctrl Pts',(6.68669531528131,31.5475306897353,54.3761892385126));
#105023=CARTESIAN_POINT('Ctrl Pts',(6.6784524895859,31.4918423034467,54.2573601384714));
#105024=CARTESIAN_POINT('Ctrl Pts',(6.67593864523918,31.4738696561359,54.2223013987281));
#105025=CARTESIAN_POINT('Ctrl Pts',(6.67263998774119,31.4493409894124,54.1783636009939));
#105026=CARTESIAN_POINT('Ctrl Pts',(6.6719177215886,31.4439147299853,54.168864684572));
#105027=CARTESIAN_POINT('Ctrl Pts',(6.67075131951546,31.4350720159899,54.1537330811792));
#105028=CARTESIAN_POINT('Ctrl Pts',(6.67031085987238,31.4317149046991,54.1480658377198));
#105029=CARTESIAN_POINT('Ctrl Pts',(6.66945254843252,31.4251407450083,54.1371163998416));
#105030=CARTESIAN_POINT('Ctrl Pts',(6.66903494887247,31.4219277565512,54.1318319859096));
#105031=CARTESIAN_POINT('Ctrl Pts',(6.66800257927938,31.4139478307814,54.1188705009532));
#105032=CARTESIAN_POINT('Ctrl Pts',(6.66738572271682,31.4091477495981,54.1112141580838));
#105033=CARTESIAN_POINT('Ctrl Pts',(6.66506535594283,31.3909645148401,54.0827286768571));
#105034=CARTESIAN_POINT('Ctrl Pts',(6.66333882225146,31.3771805728924,54.062160742341));
#105035=CARTESIAN_POINT('Ctrl Pts',(6.65875260611361,31.3397877795645,54.008967156546));
#105036=CARTESIAN_POINT('Ctrl Pts',(6.65586239213901,31.3154458447325,53.9768777123148));
#105037=CARTESIAN_POINT('Ctrl Pts',(6.64436139454279,31.2148356054583,53.8537776904426));
#105038=CARTESIAN_POINT('Ctrl Pts',(6.63564038080289,31.130082447412,53.7701340003028));
#105039=CARTESIAN_POINT('Ctrl Pts',(6.62373805248037,30.9983233553895,53.6653208906011));
#105040=CARTESIAN_POINT('Ctrl Pts',(6.62028806826645,30.9581301561778,53.6361798785766));
#105041=CARTESIAN_POINT('Ctrl Pts',(6.61573914320249,30.902401031623,53.599456784676));
#105042=CARTESIAN_POINT('Ctrl Pts',(6.61458081120952,30.8879652151375,53.5902600471949));
#105043=CARTESIAN_POINT('Ctrl Pts',(6.612671402862,30.8637676441831,53.5753635092416));
#105044=CARTESIAN_POINT('Ctrl Pts',(6.61191574892079,30.8540853141077,53.5695378505429));
#105045=CARTESIAN_POINT('Ctrl Pts',(6.61043403987332,30.8348940315954,53.5582551785704));
#105046=CARTESIAN_POINT('Ctrl Pts',(6.60970781168411,30.8253890158533,53.5527926353211));
#105047=CARTESIAN_POINT('Ctrl Pts',(6.60796975446231,30.8024080148902,53.5398854925403));
#105048=CARTESIAN_POINT('Ctrl Pts',(6.6069612457587,30.7888812495336,53.5325329995176));
#105049=CARTESIAN_POINT('Ctrl Pts',(6.60337871521551,30.7401684892407,53.5069233623563));
#105050=CARTESIAN_POINT('Ctrl Pts',(6.60084181978597,30.7044338006731,53.4897349082269));
#105051=CARTESIAN_POINT('Ctrl Pts',(6.59444342688585,30.6115965395116,53.4490929936117));
#105052=CARTESIAN_POINT('Ctrl Pts',(6.59063672421522,30.5537417353607,53.4275071431035));
#105053=CARTESIAN_POINT('Ctrl Pts',(6.58130056451441,30.4081745374395,53.3822289141359));
#105054=CARTESIAN_POINT('Ctrl Pts',(6.57582285166048,30.3194778677749,53.3624036892467));
#105055=CARTESIAN_POINT('Ctrl Pts',(6.56756727858888,30.1891027090245,53.3442617500192));
#105056=CARTESIAN_POINT('Ctrl Pts',(6.56496038142273,30.1484005818776,53.3401187835617));
#105057=CARTESIAN_POINT('Ctrl Pts',(6.56155351888063,30.0965170860123,53.3367611114426));
#105058=CARTESIAN_POINT('Ctrl Pts',(6.56082107744078,30.085436514906,53.3361551352871));
#105059=CARTESIAN_POINT('Ctrl Pts',(6.55964214016954,30.0677362383127,53.3353644105716));
#105060=CARTESIAN_POINT('Ctrl Pts',(6.55919946114745,30.0611198290855,53.3351083499998));
#105061=CARTESIAN_POINT('Ctrl Pts',(6.55834020611756,30.048339109485,53.3346900123259));
#105062=CARTESIAN_POINT('Ctrl Pts',(6.55792391555715,30.042175165848,53.3345225084346));
#105063=CARTESIAN_POINT('Ctrl Pts',(6.55689967433441,30.0270748031653,53.3341960376499));
#105064=CARTESIAN_POINT('Ctrl Pts',(6.55628971008174,30.0181378367476,53.3340747628306));
#105065=CARTESIAN_POINT('Ctrl Pts',(6.55402604735073,29.9851604253147,53.3338926403799));
#105066=CARTESIAN_POINT('Ctrl Pts',(6.55235070368922,29.9611216913236,53.3342802522857));
#105067=CARTESIAN_POINT('Ctrl Pts',(6.54793869623674,29.8985613394167,53.336643859521));
#105068=CARTESIAN_POINT('Ctrl Pts',(6.54517404443425,29.8600858198119,53.3394377143644));
#105069=CARTESIAN_POINT('Ctrl Pts',(6.53729996037453,29.7517517887729,53.3510959588226));
#105070=CARTESIAN_POINT('Ctrl Pts',(6.53214929795718,29.6823071173561,53.363056806371));
#105071=CARTESIAN_POINT('Ctrl Pts',(6.5201809781779,29.5215606120598,53.4013605059429));
#105072=CARTESIAN_POINT('Ctrl Pts',(6.51343458450082,29.4313275791278,53.4311884795724));
#105073=CARTESIAN_POINT('Ctrl Pts',(6.50557024582169,29.3257496561618,53.4764050854349));
#105074=CARTESIAN_POINT('Ctrl Pts',(6.50421356553821,29.3075302802036,53.4845988196997));
#105075=CARTESIAN_POINT('Ctrl Pts',(6.50206631270421,29.2786962642302,53.4981948894288));
#105076=CARTESIAN_POINT('Ctrl Pts',(6.50126860944032,29.267985044698,53.5033865604917));
#105077=CARTESIAN_POINT('Ctrl Pts',(6.4997601429042,29.2477357702683,53.5134706831928));
#105078=CARTESIAN_POINT('Ctrl Pts',(6.4990486646831,29.2381875488748,53.5183412405233));
#105079=CARTESIAN_POINT('Ctrl Pts',(6.49742704632043,29.216435768787,53.5297027067191));
#105080=CARTESIAN_POINT('Ctrl Pts',(6.49651908639284,29.2042645461572,53.536254072028));
#105081=CARTESIAN_POINT('Ctrl Pts',(6.49367519742556,29.1661848905766,53.5573664530873));
#105082=CARTESIAN_POINT('Ctrl Pts',(6.4917585743462,29.1405828876277,53.572470109689));
#105083=CARTESIAN_POINT('Ctrl Pts',(6.4842386787959,29.0406725829616,53.6350739762306));
#105084=CARTESIAN_POINT('Ctrl Pts',(6.47882060970477,28.9697799096292,53.6877573026117));
#105085=CARTESIAN_POINT('Ctrl Pts',(6.46653434034759,28.8184077546284,53.8201111708132));
#105086=CARTESIAN_POINT('Ctrl Pts',(6.45971886838307,28.7412135004261,53.9028458848058));
#105087=CARTESIAN_POINT('Ctrl Pts',(6.45142396345215,28.6640547366363,54.004497893463));
#105088=CARTESIAN_POINT('Ctrl Pts',(6.45045512728118,28.6552812290801,54.0163813842829));
#105089=CARTESIAN_POINT('Ctrl Pts',(6.44898612506668,28.6423567356201,54.034383412082));
#105090=CARTESIAN_POINT('Ctrl Pts',(6.4484936450737,28.6380863162184,54.0404158500107));
#105091=CARTESIAN_POINT('Ctrl Pts',(6.44759628634361,28.6304211764548,54.0513979401307));
#105092=CARTESIAN_POINT('Ctrl Pts',(6.4471923304685,28.6270128742458,54.056337787586));
#105093=CARTESIAN_POINT('Ctrl Pts',(6.44627281039241,28.6193499759925,54.0675734624939));
#105094=CARTESIAN_POINT('Ctrl Pts',(6.44575621553459,28.6151117398446,54.0738800089329));
#105095=CARTESIAN_POINT('Ctrl Pts',(6.44415446716409,28.6021713282531,54.0934229569121));
#105096=CARTESIAN_POINT('Ctrl Pts',(6.44306056479699,28.5936149701943,54.1067542146976));
#105097=CARTESIAN_POINT('Ctrl Pts',(6.43733185489244,28.5501872798413,54.1765878640327));
#105098=CARTESIAN_POINT('Ctrl Pts',(6.43254655963957,28.5185294192158,54.2350113267309));
#105099=CARTESIAN_POINT('Ctrl Pts',(6.41913802495707,28.4404252015248,54.4022873427279));
#105100=CARTESIAN_POINT('Ctrl Pts',(6.41049803460797,28.4019441682706,54.5144501612296));
#105101=CARTESIAN_POINT('Ctrl Pts',(6.39944598388614,28.3668968193069,54.668208240349));
#105102=CARTESIAN_POINT('Ctrl Pts',(6.39672077394952,28.3594989288619,54.7069668026118));
#105103=CARTESIAN_POINT('Ctrl Pts',(6.39296414188989,28.3510742048676,54.761568999204));
#105104=CARTESIAN_POINT('Ctrl Pts',(6.3918968625506,28.3488871573478,54.7772175260533));
#105105=CARTESIAN_POINT('Ctrl Pts',(6.39010327499326,28.3455645516379,54.8037380373539));
#105106=CARTESIAN_POINT('Ctrl Pts',(6.38937336182883,28.3443128076106,54.8145941167331));
#105107=CARTESIAN_POINT('Ctrl Pts',(6.38790366461216,28.3419970009609,54.8365773047733));
#105108=CARTESIAN_POINT('Ctrl Pts',(6.38716407286781,28.340937922559,54.8477043807266));
#105109=CARTESIAN_POINT('Ctrl Pts',(6.3853404269031,28.3385918278208,54.8752942094089));
#105110=CARTESIAN_POINT('Ctrl Pts',(6.38426055741512,28.3374374129943,54.8917672642455));
#105111=CARTESIAN_POINT('Ctrl Pts',(6.38004253353108,28.3338615649757,54.9566028351024));
#105112=CARTESIAN_POINT('Ctrl Pts',(6.37696210588774,28.3333039267688,55.0050466381535));
#105113=CARTESIAN_POINT('Ctrl Pts',(6.368561479618,28.3376050930823,55.1390428267351));
#105114=CARTESIAN_POINT('Ctrl Pts',(6.36335742185344,28.3469479333945,55.2242980747015));
#105115=CARTESIAN_POINT('Ctrl Pts',(6.35276793898048,28.3790327232282,55.3945923478807));
#105116=CARTESIAN_POINT('Ctrl Pts',(6.34739549126449,28.4020304205631,55.479298902742));
#105117=CARTESIAN_POINT('Ctrl Pts',(6.34067251035354,28.4370129153623,55.5769636757493));
#105118=CARTESIAN_POINT('Ctrl Pts',(6.33961800815994,28.4426668373582,55.5920549666972));
#105119=CARTESIAN_POINT('Ctrl Pts',(6.33803784431309,28.4513660024572,55.614287354525));
#105120=CARTESIAN_POINT('Ctrl Pts',(6.33752146838993,28.4542438664272,55.621493509088));
#105121=CARTESIAN_POINT('Ctrl Pts',(6.33659990001523,28.4594393648644,55.6342436717513));
#105122=CARTESIAN_POINT('Ctrl Pts',(6.33619590453659,28.4617368048074,55.6397956281614));
#105123=CARTESIAN_POINT('Ctrl Pts',(6.3353001140434,28.4668740894821,55.6520226685981));
#105124=CARTESIAN_POINT('Ctrl Pts',(6.33480755042212,28.4697274800136,55.6586916027032));
#105125=CARTESIAN_POINT('Ctrl Pts',(6.33335133501082,28.4782494672888,55.6782549036394));
#105126=CARTESIAN_POINT('Ctrl Pts',(6.33238100279907,28.4840379845453,55.6910958928343));
#105127=CARTESIAN_POINT('Ctrl Pts',(6.32545203338066,28.52619062429,55.7815270143243));
#105128=CARTESIAN_POINT('Ctrl Pts',(6.31922931046621,28.5683272794901,55.8562761213077));
#105129=CARTESIAN_POINT('Ctrl Pts',(6.3038021595715,28.6863168726329,56.0323461573861));
#105130=CARTESIAN_POINT('Ctrl Pts',(6.29465972233035,28.7683263673373,56.1289345966134));
#105131=CARTESIAN_POINT('Ctrl Pts',(6.28450763392295,28.8759438515739,56.2298387186755));
#105132=CARTESIAN_POINT('Ctrl Pts',(6.28306088197729,28.8916861289083,56.2440441847461));
#105133=CARTESIAN_POINT('Ctrl Pts',(6.28072148724295,28.9177995605363,56.266719093448));
#105134=CARTESIAN_POINT('Ctrl Pts',(6.27982140021284,28.9280087725843,56.2753704870971));
#105135=CARTESIAN_POINT('Ctrl Pts',(6.27821240442564,28.9465469255068,56.290700021231));
#105136=CARTESIAN_POINT('Ctrl Pts',(6.27750170701223,28.9548378129768,56.297422805751));
#105137=CARTESIAN_POINT('Ctrl Pts',(6.27598761537083,28.9727176351743,56.3116382921029));
#105138=CARTESIAN_POINT('Ctrl Pts',(6.27518522019695,28.9823252497917,56.3191065849153));
#105139=CARTESIAN_POINT('Ctrl Pts',(6.2729938780674,29.0089194431084,56.3393155540326));
#105140=CARTESIAN_POINT('Ctrl Pts',(6.27161343546043,29.0260694672255,56.35183808465));
#105141=CARTESIAN_POINT('Ctrl Pts',(6.26855642918643,29.064892904632,56.3790635678446));
#105142=CARTESIAN_POINT('Ctrl Pts',(6.26688632111294,29.0866832011447,56.3935903768461));
#105143=CARTESIAN_POINT('Ctrl Pts',(6.2615042687905,29.158628006576,56.4391407726055));
#105144=CARTESIAN_POINT('Ctrl Pts',(6.25785899503546,29.2100902538788,56.4680178304589));
#105145=CARTESIAN_POINT('Ctrl Pts',(6.24742248065099,29.3627474015405,56.543321458361));
#105146=CARTESIAN_POINT('Ctrl Pts',(6.24074553007785,29.4671848368141,56.5824143597914));
#105147=CARTESIAN_POINT('Ctrl Pts',(6.23191086951282,29.6013760188719,56.6178425926378));
#105148=CARTESIAN_POINT('Ctrl Pts',(6.23013206342855,29.6281948301113,56.6242156387382));
#105149=CARTESIAN_POINT('Ctrl Pts',(6.22768265384676,29.6646282298012,56.6319238603171));
#105150=CARTESIAN_POINT('Ctrl Pts',(6.22704180413422,29.674115987311,56.633844946517));
#105151=CARTESIAN_POINT('Ctrl Pts',(6.2260171602238,29.6892040773609,56.6367633448034));
#105152=CARTESIAN_POINT('Ctrl Pts',(6.22563635378028,29.6947938804587,56.6378148779908));
#105153=CARTESIAN_POINT('Ctrl Pts',(6.22483333731474,29.7065412603464,56.6399625255993));
#105154=CARTESIAN_POINT('Ctrl Pts',(6.22441077834105,29.7126997680553,56.6410526162936));
#105155=CARTESIAN_POINT('Ctrl Pts',(6.22334882668066,29.7281228583254,56.6436931152702));
#105156=CARTESIAN_POINT('Ctrl Pts',(6.22270708178892,29.7373945923247,56.64519987444));
#105157=CARTESIAN_POINT('Ctrl Pts',(6.22017041484111,29.7738727907375,56.6508117787616));
#105158=CARTESIAN_POINT('Ctrl Pts',(6.21824680728647,29.8011649110137,56.654320839445));
#105159=CARTESIAN_POINT('Ctrl Pts',(6.21296146290074,29.8754694158971,56.6620093530622));
#105160=CARTESIAN_POINT('Ctrl Pts',(6.20955799413574,29.9225918069228,56.6648694765281));
#105161=CARTESIAN_POINT('Ctrl Pts',(6.19810119341712,30.0804216959721,56.6677339254671));
#105162=CARTESIAN_POINT('Ctrl Pts',(6.19000189333466,30.1910132467543,56.6587112659582));
#105163=CARTESIAN_POINT('Ctrl Pts',(6.17882658687335,30.3467522340408,56.6302109205204));
#105164=CARTESIAN_POINT('Ctrl Pts',(6.17551844198579,30.3932199502535,56.6196306997463));
#105165=CARTESIAN_POINT('Ctrl Pts',(6.17112079763952,30.4554817863482,56.602616026593));
#105166=CARTESIAN_POINT('Ctrl Pts',(6.16997698582802,30.4717207796462,56.597911552317));
#105167=CARTESIAN_POINT('Ctrl Pts',(6.1681604924861,30.4975734324719,56.5899935003967));
#105168=CARTESIAN_POINT('Ctrl Pts',(6.16748272079862,30.5072338900197,56.5869380708327));
#105169=CARTESIAN_POINT('Ctrl Pts',(6.16608581986091,30.527170545936,56.5804318101603));
#105170=CARTESIAN_POINT('Ctrl Pts',(6.16536714054307,30.5374421681683,56.576968425935));
#105171=CARTESIAN_POINT('Ctrl Pts',(6.16368292459527,30.5615422396621,56.5685795403138));
#105172=CARTESIAN_POINT('Ctrl Pts',(6.16272018016313,30.5753409844888,56.5635709883225));
#105173=CARTESIAN_POINT('Ctrl Pts',(6.15949230060128,30.6216562736052,56.5460636829091));
#105174=CARTESIAN_POINT('Ctrl Pts',(6.15725495077937,30.6538477697883,56.5327272423187));
#105175=CARTESIAN_POINT('Ctrl Pts',(6.15181098270919,30.7320684874088,56.4974082162702));
#105176=CARTESIAN_POINT('Ctrl Pts',(6.1486393830375,30.77755207393,56.4743028799099));
#105177=CARTESIAN_POINT('Ctrl Pts',(6.13929137637149,30.9095844175477,56.3994185827939));
#105178=CARTESIAN_POINT('Ctrl Pts',(6.133235355052,30.992563141032,56.3418393336228));
#105179=CARTESIAN_POINT('Ctrl Pts',(6.12399828956644,31.1060969094595,56.246733504011));
#105180=CARTESIAN_POINT('Ctrl Pts',(6.12099855308623,31.1410539128376,56.214820928005));
#105181=CARTESIAN_POINT('Ctrl Pts',(6.11714665268529,31.1827865586526,56.1733307935841));
#105182=CARTESIAN_POINT('Ctrl Pts',(6.11638557168548,31.1908859652968,56.1651093484501));
#105183=CARTESIAN_POINT('Ctrl Pts',(6.11517135017654,31.2035638049652,56.151970181987));
#105184=CARTESIAN_POINT('Ctrl Pts',(6.11472243326801,31.2081991974774,56.1471075921828));
#105185=CARTESIAN_POINT('Ctrl Pts',(6.11386000623778,31.2170025944169,56.1377601551767));
#105186=CARTESIAN_POINT('Ctrl Pts',(6.11344687141477,31.221175460885,56.1332801834442));
#105187=CARTESIAN_POINT('Ctrl Pts',(6.11244304877632,31.2312096707202,56.1223877328082));
#105188=CARTESIAN_POINT('Ctrl Pts',(6.11185053108079,31.2370456781989,56.1159522650149));
#105189=CARTESIAN_POINT('Ctrl Pts',(6.1098116416017,31.2568414084029,56.0937770736268));
#105190=CARTESIAN_POINT('Ctrl Pts',(6.10834919186775,31.2705525696277,56.0778194097897));
#105191=CARTESIAN_POINT('Ctrl Pts',(6.10181417219437,31.329841177883,56.0061130208916));
#105192=CARTESIAN_POINT('Ctrl Pts',(6.09658992949722,31.3720755896651,55.947706645059));
#105193=CARTESIAN_POINT('Ctrl Pts',(6.08493504205352,31.4573181988525,55.8121274161216));
#105194=CARTESIAN_POINT('Ctrl Pts',(6.07851905786425,31.4982468554402,55.7338843670799));
#105195=CARTESIAN_POINT('Ctrl Pts',(6.07031018813179,31.5436497110356,55.6272713353825));
#105196=CARTESIAN_POINT('Ctrl Pts',(6.06836462738581,31.5538675993448,55.6015138911432));
#105197=CARTESIAN_POINT('Ctrl Pts',(6.06643882015545,31.5634376718252,55.5755159826781));
#105198=CARTESIAN_POINT('Origin',(5.,30.,55.));
#105199=CARTESIAN_POINT('',(5.36787289354565,31.5634376782623,55.5755159651912));
#105200=CARTESIAN_POINT('',(5.55935725065089,31.5634376826058,55.5755159533916));
#105201=CARTESIAN_POINT('',(5.,31.5634376782623,55.5755159651912));
#105202=CARTESIAN_POINT('Ctrl Pts',(5.55935725065089,31.5634376826058,55.5755159533915));
#105203=CARTESIAN_POINT('Ctrl Pts',(5.56438142617607,31.5386334334857,55.642898790539));
#105204=CARTESIAN_POINT('Ctrl Pts',(5.56958176175285,31.5094976695741,55.7086108847468));
#105205=CARTESIAN_POINT('Ctrl Pts',(5.57506597430681,31.474553496052,55.7754100768546));
#105206=CARTESIAN_POINT('Ctrl Pts',(5.57532629573884,31.4728849165893,55.7785748663058));
#105207=CARTESIAN_POINT('Ctrl Pts',(5.58228131114254,31.428039808155,55.8629723445646));
#105208=CARTESIAN_POINT('Ctrl Pts',(5.58897634642658,31.3782145606548,55.9405034253079));
#105209=CARTESIAN_POINT('Ctrl Pts',(5.59903261293475,31.2916697514238,56.0534087962369));
#105210=CARTESIAN_POINT('Ctrl Pts',(5.60252539582477,31.259310001581,56.0918883030689));
#105211=CARTESIAN_POINT('Ctrl Pts',(5.6070645053916,31.2141584933073,56.1408958946897));
#105212=CARTESIAN_POINT('Ctrl Pts',(5.60817273521232,31.20288265202,56.1527782302515));
#105213=CARTESIAN_POINT('Ctrl Pts',(5.60930874773144,31.1910659530328,56.1648683064411));
#105214=CARTESIAN_POINT('Ctrl Pts',(5.60934403107992,31.1906986800897,56.1652437208836));
#105215=CARTESIAN_POINT('Ctrl Pts',(5.60941457768895,31.1899638260067,56.1659941545953));
#105216=CARTESIAN_POINT('Ctrl Pts',(5.60944984094736,31.1895962449558,56.1663691738652));
#105217=CARTESIAN_POINT('Ctrl Pts',(5.60949443673807,31.1891310553628,56.1668433281837));
#105218=CARTESIAN_POINT('Ctrl Pts',(5.609503776488,31.1890336119965,56.1669426245097));
#105219=CARTESIAN_POINT('Ctrl Pts',(5.60952323637707,31.1888305454974,56.1671495006305));
#105220=CARTESIAN_POINT('Ctrl Pts',(5.60953335642456,31.1887249201563,56.1672570783376));
#105221=CARTESIAN_POINT('Ctrl Pts',(5.60955448972941,31.1885043023187,56.1674817130455));
#105222=CARTESIAN_POINT('Ctrl Pts',(5.60956550287016,31.1883893071048,56.1675987674217));
#105223=CARTESIAN_POINT('Ctrl Pts',(5.60958855851705,31.1881485155607,56.1678437982768));
#105224=CARTESIAN_POINT('Ctrl Pts',(5.60960060087439,31.188022715836,56.1679717714313));
#105225=CARTESIAN_POINT('Ctrl Pts',(5.60962588093001,31.1877585659453,56.1682403981834));
#105226=CARTESIAN_POINT('Ctrl Pts',(5.60963911843756,31.1876202114697,56.1683810475324));
#105227=CARTESIAN_POINT('Ctrl Pts',(5.6096669934003,31.1873287938332,56.1686771936434));
#105228=CARTESIAN_POINT('Ctrl Pts',(5.60968163061705,31.1871757250234,56.1688326849994));
#105229=CARTESIAN_POINT('Ctrl Pts',(5.60971256045189,31.1868521817154,56.1691612197481));
#105230=CARTESIAN_POINT('Ctrl Pts',(5.60972885273997,31.1866816999834,56.169334255861));
#105231=CARTESIAN_POINT('Ctrl Pts',(5.60976341621427,31.1863199120729,56.1697013039481));
#105232=CARTESIAN_POINT('Ctrl Pts',(5.6097816869726,31.186128596093,56.1698953063284));
#105233=CARTESIAN_POINT('Ctrl Pts',(5.60982062380237,31.1857207341308,56.1703086924712));
#105234=CARTESIAN_POINT('Ctrl Pts',(5.60984128928755,31.1855041748085,56.1705280631122));
#105235=CARTESIAN_POINT('Ctrl Pts',(5.60988556177281,31.1850400404178,56.1709979618531));
#105236=CARTESIAN_POINT('Ctrl Pts',(5.609909167954,31.1847924467195,56.1712484716124));
#105237=CARTESIAN_POINT('Ctrl Pts',(5.60996005416152,31.1842584755389,56.1717883891228));
#105238=CARTESIAN_POINT('Ctrl Pts',(5.60998733301112,31.183972071315,56.1720777705064));
#105239=CARTESIAN_POINT('Ctrl Pts',(5.61004657226197,31.1833497733272,56.172706076415));
#105240=CARTESIAN_POINT('Ctrl Pts',(5.61007853091724,31.1830138398797,56.173044961776));
#105241=CARTESIAN_POINT('Ctrl Pts',(5.61014856038942,31.1822772575612,56.1737873783654));
#105242=CARTESIAN_POINT('Ctrl Pts',(5.61018662850561,31.1818765474767,56.174190849003));
#105243=CARTESIAN_POINT('Ctrl Pts',(5.61027098724686,31.1809879049234,56.1750846977867));
#105244=CARTESIAN_POINT('Ctrl Pts',(5.61031727349049,31.1804998732521,56.1755749775331));
#105245=CARTESIAN_POINT('Ctrl Pts',(5.6104213355967,31.1794016585379,56.1766768775831));
#105246=CARTESIAN_POINT('Ctrl Pts',(5.61047910390184,31.1787913044448,56.1772883278837));
#105247=CARTESIAN_POINT('Ctrl Pts',(5.61068048993553,31.1766611140632,56.1794190267513));
#105248=CARTESIAN_POINT('Ctrl Pts',(5.6108239984544,31.1751388090333,56.1809358143395));
#105249=CARTESIAN_POINT('Ctrl Pts',(5.61168020060985,31.1660306523415,56.1899759085126));
#105250=CARTESIAN_POINT('Ctrl Pts',(5.61238979142832,31.1583753687793,56.1974291875225));
#105251=CARTESIAN_POINT('Ctrl Pts',(5.61398643714876,31.1409117657192,56.2141077500461));
#105252=CARTESIAN_POINT('Ctrl Pts',(5.61487156491238,31.1310621662562,56.2232888782436));
#105253=CARTESIAN_POINT('Ctrl Pts',(5.61756513883188,31.1005834127957,56.2510162280415));
#105254=CARTESIAN_POINT('Ctrl Pts',(5.61935716118375,31.0796008549319,56.2691680692193));
#105255=CARTESIAN_POINT('Ctrl Pts',(5.62950549158411,30.9569847370767,56.3699998499438));
#105256=CARTESIAN_POINT('Ctrl Pts',(5.63738327934517,30.8463360884268,56.4409847635265));
#105257=CARTESIAN_POINT('Ctrl Pts',(5.64865786447829,30.68105782887,56.5213480949747));
#105258=CARTESIAN_POINT('Ctrl Pts',(5.65192040425943,30.6325418896573,56.5421510212462));
#105259=CARTESIAN_POINT('Ctrl Pts',(5.65714970409301,30.5554406712294,56.5709599175612));
#105260=CARTESIAN_POINT('Ctrl Pts',(5.6590544903043,30.5274883564841,56.5805648302918));
#105261=CARTESIAN_POINT('Ctrl Pts',(5.66163228132368,30.4901027419031,56.5923090746656));
#105262=CARTESIAN_POINT('Ctrl Pts',(5.66227037439265,30.4808833488748,56.5951175758118));
#105263=CARTESIAN_POINT('Ctrl Pts',(5.6633334671081,30.4655923155106,56.5996310705523));
#105264=CARTESIAN_POINT('Ctrl Pts',(5.66375587808909,30.4595342638098,56.6013819106883));
#105265=CARTESIAN_POINT('Ctrl Pts',(5.66461225681819,30.4472919072846,56.6048448916062));
#105266=CARTESIAN_POINT('Ctrl Pts',(5.66504627975323,30.4411073892707,56.6065557705979));
#105267=CARTESIAN_POINT('Ctrl Pts',(5.66617220095384,30.4251114320976,56.6108815514161));
#105268=CARTESIAN_POINT('Ctrl Pts',(5.66686703662255,30.415285864413,56.6134425122357));
#105269=CARTESIAN_POINT('Ctrl Pts',(5.66972852073009,30.3749847753909,56.6235541836016));
#105270=CARTESIAN_POINT('Ctrl Pts',(5.67193225510594,30.3443240648373,56.6303319931451));
#105271=CARTESIAN_POINT('Ctrl Pts',(5.68190384758507,30.2065197041298,56.6567344030723));
#105272=CARTESIAN_POINT('Ctrl Pts',(5.6899298328273,30.0977973217312,56.6666897565582));
#105273=CARTESIAN_POINT('Ctrl Pts',(5.701935769797,29.9314878439444,56.6655798774498));
#105274=CARTESIAN_POINT('Ctrl Pts',(5.70603035474739,29.874147400891,56.6622311703427));
#105275=CARTESIAN_POINT('Ctrl Pts',(5.71268592042958,29.7795369284339,56.6517806833118));
#105276=CARTESIAN_POINT('Ctrl Pts',(5.71529124385533,29.7421340745683,56.6463562654311));
#105277=CARTESIAN_POINT('Ctrl Pts',(5.71888458789381,29.6900542301858,56.6369845888825));
#105278=CARTESIAN_POINT('Ctrl Pts',(5.71990558846127,29.675199940804,56.634102160897));
#105279=CARTESIAN_POINT('Ctrl Pts',(5.72165225607404,29.6496978885732,56.6287920774072));
#105280=CARTESIAN_POINT('Ctrl Pts',(5.72238095613864,29.6390311566344,56.6264614058104));
#105281=CARTESIAN_POINT('Ctrl Pts',(5.72377262678835,29.6186113271342,56.6217889091472));
#105282=CARTESIAN_POINT('Ctrl Pts',(5.72443608874799,29.6088549940349,56.6194635461721));
#105283=CARTESIAN_POINT('Ctrl Pts',(5.72617229731467,29.5832727184829,56.6131214913951));
#105284=CARTESIAN_POINT('Ctrl Pts',(5.72724035843151,29.5674835349375,56.6089599471674));
#105285=CARTESIAN_POINT('Ctrl Pts',(5.73109742565772,29.5103151782821,56.5929897300078));
#105286=CARTESIAN_POINT('Ctrl Pts',(5.73384244620543,29.469334450681,56.5798107680502));
#105287=CARTESIAN_POINT('Ctrl Pts',(5.74377246347529,29.3210246398426,56.5256922428114));
#105288=CARTESIAN_POINT('Ctrl Pts',(5.75067322552188,29.2175036662022,56.4752777756366));
#105289=CARTESIAN_POINT('Ctrl Pts',(5.76070931432902,29.0789266853458,56.3890711197075));
#105290=CARTESIAN_POINT('Ctrl Pts',(5.76371069612895,29.0389987543043,56.3617527631369));
#105291=CARTESIAN_POINT('Ctrl Pts',(5.76799841422418,28.9851201218553,56.3213386331694));
#105292=CARTESIAN_POINT('Ctrl Pts',(5.76921949673666,28.9701186509693,56.3096798437433));
#105293=CARTESIAN_POINT('Ctrl Pts',(5.77138841407432,28.9441472004133,56.2887732951251));
#105294=CARTESIAN_POINT('Ctrl Pts',(5.77232981992269,28.9330909685501,56.2796354267453));
#105295=CARTESIAN_POINT('Ctrl Pts',(5.77376545365181,28.9165826084727,56.2656287576805));
#105296=CARTESIAN_POINT('Ctrl Pts',(5.77425250593635,28.9110419553616,56.260864690804));
#105297=CARTESIAN_POINT('Ctrl Pts',(5.77514486379189,28.9010036773915,56.2521178748903));
#105298=CARTESIAN_POINT('Ctrl Pts',(5.77554931159352,28.8964960184456,56.248147046171));
#105299=CARTESIAN_POINT('Ctrl Pts',(5.77647632172216,28.8862596628727,56.2390309725505));
#105300=CARTESIAN_POINT('Ctrl Pts',(5.77699998919003,28.8805451189608,56.2338703549874));
#105301=CARTESIAN_POINT('Ctrl Pts',(5.77864562373789,28.8627921127189,56.217613352367));
#105302=CARTESIAN_POINT('Ctrl Pts',(5.77977701361075,28.8508817321547,56.2063793811396));
#105303=CARTESIAN_POINT('Ctrl Pts',(5.78634064111896,28.783359353779,56.1407844956635));
#105304=CARTESIAN_POINT('Ctrl Pts',(5.79197758969326,28.7314470682383,56.0827626165985));
#105305=CARTESIAN_POINT('Ctrl Pts',(5.80248998111074,28.6428816280932,55.9686261851671));
#105306=CARTESIAN_POINT('Ctrl Pts',(5.80735135535522,28.6051830279587,55.9135060851548));
#105307=CARTESIAN_POINT('Ctrl Pts',(5.81560742853956,28.5460286048384,55.8147779025804));
#105308=CARTESIAN_POINT('Ctrl Pts',(5.81903484700217,28.5229841407807,55.7722180445302));
#105309=CARTESIAN_POINT('Ctrl Pts',(5.82474099980228,28.4871379370471,55.698520964106));
#105310=CARTESIAN_POINT('Ctrl Pts',(5.82704921748487,28.4733680782871,55.6678910202404));
#105311=CARTESIAN_POINT('Ctrl Pts',(5.83030816087445,28.4549973061191,55.6234840279199));
#105312=CARTESIAN_POINT('Ctrl Pts',(5.83128417573571,28.4496367125943,55.610032259169));
#105313=CARTESIAN_POINT('Ctrl Pts',(5.83297861701718,28.4405811674031,55.5864177526218));
#105314=CARTESIAN_POINT('Ctrl Pts',(5.83369960416216,28.4368085817856,55.5762859321121));
#105315=CARTESIAN_POINT('Ctrl Pts',(5.83518768648709,28.4291916236937,55.5552041988846));
#105316=CARTESIAN_POINT('Ctrl Pts',(5.83595424319227,28.4253624900285,55.544249374108));
#105317=CARTESIAN_POINT('Ctrl Pts',(5.83793710918573,28.4157076973509,55.5156726982956));
#105318=CARTESIAN_POINT('Ctrl Pts',(5.83914750209038,28.4100613779089,55.4979916213125));
#105319=CARTESIAN_POINT('Ctrl Pts',(5.84448122561573,28.3863106233631,55.4190916139728));
#105320=CARTESIAN_POINT('Ctrl Pts',(5.84850014935065,28.3714370626358,55.3569528054532));
#105321=CARTESIAN_POINT('Ctrl Pts',(5.86142117325569,28.3346224186023,55.1516881745476));
#105322=CARTESIAN_POINT('Ctrl Pts',(5.86996417475767,28.3277445217982,55.0065688996762));
#105323=CARTESIAN_POINT('Ctrl Pts',(5.88069467302052,28.3415639148894,54.8398135534096));
#105324=CARTESIAN_POINT('Ctrl Pts',(5.88216648745376,28.343897092926,54.8172625233612));
#105325=CARTESIAN_POINT('Ctrl Pts',(5.8842383858517,28.3477665979335,54.7860905946412));
#105326=CARTESIAN_POINT('Ctrl Pts',(5.88481855284784,28.3489119586705,54.7774225527197));
#105327=CARTESIAN_POINT('Ctrl Pts',(5.88581209580855,28.3509767504594,54.7626902020593));
#105328=CARTESIAN_POINT('Ctrl Pts',(5.88622356714983,28.3518615602632,54.7566210772582));
#105329=CARTESIAN_POINT('Ctrl Pts',(5.88708850889559,28.3537828453135,54.7439336931603));
#105330=CARTESIAN_POINT('Ctrl Pts',(5.88754230336582,28.3548257434434,54.7373166631237));
#105331=CARTESIAN_POINT('Ctrl Pts',(5.88877725004576,28.3577586396373,54.7194107528596));
#105332=CARTESIAN_POINT('Ctrl Pts',(5.88956243544875,28.3597250777891,54.7081350094737));
#105333=CARTESIAN_POINT('Ctrl Pts',(5.89352306029839,28.3701568976936,54.6517567576427));
#105334=CARTESIAN_POINT('Ctrl Pts',(5.89677840882485,28.3803664221921,54.6070010649619));
#105335=CARTESIAN_POINT('Ctrl Pts',(5.90634436388976,28.4153022520344,54.4785625148006));
#105336=CARTESIAN_POINT('Ctrl Pts',(5.91274379238227,28.4447698051571,54.3963253200586));
#105337=CARTESIAN_POINT('Ctrl Pts',(5.92341360657095,28.5052842518092,54.261744454002));
#105338=CARTESIAN_POINT('Ctrl Pts',(5.92772673531838,28.5330010181555,54.2080961884032));
#105339=CARTESIAN_POINT('Ctrl Pts',(5.9346860010844,28.5833573841249,54.1223864666511));
#105340=CARTESIAN_POINT('Ctrl Pts',(5.93738200309132,28.6043242335547,54.0894115050606));
#105341=CARTESIAN_POINT('Ctrl Pts',(5.94107632232717,28.6350999362334,54.0445742356365));
#105342=CARTESIAN_POINT('Ctrl Pts',(5.94211015684279,28.6439412168671,54.0320665419653));
#105343=CARTESIAN_POINT('Ctrl Pts',(5.94387187026964,28.659397719978,54.0108278983088));
#105344=CARTESIAN_POINT('Ctrl Pts',(5.94460291957702,28.6659287268419,54.00203719109));
#105345=CARTESIAN_POINT('Ctrl Pts',(5.94599451631321,28.6785832486332,53.985350508075));
#105346=CARTESIAN_POINT('Ctrl Pts',(5.9466555968881,28.6846920237563,53.977444007766));
#105347=CARTESIAN_POINT('Ctrl Pts',(5.94820463325613,28.6992327173627,53.9589701133856));
#105348=CARTESIAN_POINT('Ctrl Pts',(5.94909023768516,28.7077229435511,53.948449347169));
#105349=CARTESIAN_POINT('Ctrl Pts',(5.95220101933214,28.7381609783025,53.9116571810827));
#105350=CARTESIAN_POINT('Ctrl Pts',(5.95439877066066,28.7607902713254,53.8859590163247));
#105351=CARTESIAN_POINT('Ctrl Pts',(5.96517498497581,28.8769610361903,53.7619575309283));
#105352=CARTESIAN_POINT('Ctrl Pts',(5.97327247946438,28.9814689877015,53.6746470661402));
#105353=CARTESIAN_POINT('Ctrl Pts',(5.98427000393146,29.1310246177015,53.577946344057));
#105354=CARTESIAN_POINT('Ctrl Pts',(5.98691667608192,29.1675046059302,53.556287509775));
#105355=CARTESIAN_POINT('Ctrl Pts',(5.99126211897766,29.2273006583769,53.5238058271616));
#105356=CARTESIAN_POINT('Ctrl Pts',(5.99292143313435,29.2501109620411,53.512088790314));
#105357=CARTESIAN_POINT('Ctrl Pts',(5.99521358779847,29.2814204052399,53.4969087813291));
#105358=CARTESIAN_POINT('Ctrl Pts',(5.9958205305972,29.2896923519451,53.4929821231137));
#105359=CARTESIAN_POINT('Ctrl Pts',(5.99684591417611,29.3036267402538,53.4865077361036));
#105360=CARTESIAN_POINT('Ctrl Pts',(5.99726214006056,29.3092719775985,53.4839230404561));
#105361=CARTESIAN_POINT('Ctrl Pts',(5.99812161867224,29.3209030209689,53.4786761656712));
#105362=CARTESIAN_POINT('Ctrl Pts',(5.99856506046589,29.3268902601006,53.4760176542543));
#105363=CARTESIAN_POINT('Ctrl Pts',(5.99974286314159,29.3427606139052,53.4690825119363));
#105364=CARTESIAN_POINT('Ctrl Pts',(6.00048066687747,29.3526695918747,53.4648663597796));
#105365=CARTESIAN_POINT('Ctrl Pts',(6.00380368503843,29.3971838991493,53.4464336561704));
#105366=CARTESIAN_POINT('Ctrl Pts',(6.00644190064862,29.4322188698263,53.4332901519454));
#105367=CARTESIAN_POINT('Ctrl Pts',(6.01665735794077,29.5677149746606,53.3875998441156));
#105368=CARTESIAN_POINT('Ctrl Pts',(6.02443255821359,29.6707462143277,53.3634496752657));
#105369=CARTESIAN_POINT('Ctrl Pts',(6.03600598498834,29.8298438700515,53.341800635542));
#105370=CARTESIAN_POINT('Ctrl Pts',(6.03992106520626,29.8846543195539,53.3370885173216));
#105371=CARTESIAN_POINT('Ctrl Pts',(6.04632454628363,29.9762716849743,53.3337649026414));
#105372=CARTESIAN_POINT('Ctrl Pts',(6.04885299567858,30.0129775326438,53.333646381974));
#105373=CARTESIAN_POINT('Ctrl Pts',(6.05236034792536,30.0646215755687,53.335186466547));
#105374=CARTESIAN_POINT('Ctrl Pts',(6.0533701491903,30.0795769124824,53.3358342661861));
#105375=CARTESIAN_POINT('Ctrl Pts',(6.05510373452009,30.1053943551225,53.3373014039075));
#105376=CARTESIAN_POINT('Ctrl Pts',(6.05583043273052,30.1162606846872,53.3380258562676));
#105377=CARTESIAN_POINT('Ctrl Pts',(6.05722238753816,30.1371551828384,53.3396248124423));
#105378=CARTESIAN_POINT('Ctrl Pts',(6.0578880980002,30.147184025289,53.3404837518537));
#105379=CARTESIAN_POINT('Ctrl Pts',(6.05963950851647,30.1736583288824,53.3429930777817));
#105380=CARTESIAN_POINT('Ctrl Pts',(6.0607203596329,30.190088344681,53.3447974115597));
#105381=CARTESIAN_POINT('Ctrl Pts',(6.06468452423232,30.2506454151043,53.3523613688104));
#105382=CARTESIAN_POINT('Ctrl Pts',(6.06752045822625,30.2945654122062,53.3596439621735));
#105383=CARTESIAN_POINT('Ctrl Pts',(6.07744498142532,30.4492649245558,53.3917104224484));
#105384=CARTESIAN_POINT('Ctrl Pts',(6.08426439881451,30.5577391625354,53.4260362396723));
#105385=CARTESIAN_POINT('Ctrl Pts',(6.09419585415679,30.7059133693824,53.4901840333163));
#105386=CARTESIAN_POINT('Ctrl Pts',(6.09717458968547,30.7490960585087,53.5111372124569));
#105387=CARTESIAN_POINT('Ctrl Pts',(6.10143292372959,30.8079481485887,53.5429024705863));
#105388=CARTESIAN_POINT('Ctrl Pts',(6.1026482146318,30.8244302406474,53.5521643270762));
#105389=CARTESIAN_POINT('Ctrl Pts',(6.10480781772517,30.8530872632819,53.5689156823011));
#105390=CARTESIAN_POINT('Ctrl Pts',(6.10574577770904,30.8653303183613,53.5762852779555));
#105391=CARTESIAN_POINT('Ctrl Pts',(6.10717720349427,30.883678972499,53.5876541809736));
#105392=CARTESIAN_POINT('Ctrl Pts',(6.10766355656535,30.8898559296141,53.5915378391746));
#105393=CARTESIAN_POINT('Ctrl Pts',(6.10855526382174,30.9010722246558,53.5986931302238));
#105394=CARTESIAN_POINT('Ctrl Pts',(6.10895976851424,30.9061196373273,53.6019516115001));
#105395=CARTESIAN_POINT('Ctrl Pts',(6.10988772833993,30.9176065205782,53.6094555877559));
#105396=CARTESIAN_POINT('Ctrl Pts',(6.11041229823292,30.9240341830352,53.6137185308529));
#105397=CARTESIAN_POINT('Ctrl Pts',(6.11206365320363,30.9440707129814,53.6272083820125));
#105398=CARTESIAN_POINT('Ctrl Pts',(6.1131999510721,30.9575722628004,53.6365918995358));
#105399=CARTESIAN_POINT('Ctrl Pts',(6.12047552777701,31.0423588623688,53.6973988153171));
#105400=CARTESIAN_POINT('Ctrl Pts',(6.12687573452939,31.1096132770386,53.7541920552121));
#105401=CARTESIAN_POINT('Ctrl Pts',(6.13683136810198,31.2068083295225,53.8504090807581));
#105402=CARTESIAN_POINT('Ctrl Pts',(6.14038599273035,31.2400193819456,53.8863133897986));
#105403=CARTESIAN_POINT('Ctrl Pts',(6.14771407543596,31.3057951880298,53.9640195562467));
#105404=CARTESIAN_POINT('Ctrl Pts',(6.15147708698704,31.3380445123024,54.0060209611816));
#105405=CARTESIAN_POINT('Ctrl Pts',(6.15766510767683,31.3886372630467,54.0788483141074));
#105406=CARTESIAN_POINT('Ctrl Pts',(6.16012669806253,31.4080834187329,54.10885730668));
#105407=CARTESIAN_POINT('Ctrl Pts',(6.16355896420394,31.4342071195242,54.1521641169793));
#105408=CARTESIAN_POINT('Ctrl Pts',(6.16455877995208,31.4416944415924,54.1649593375249));
#105409=CARTESIAN_POINT('Ctrl Pts',(6.16628074228329,31.4543722876095,54.1873036770456));
#105410=CARTESIAN_POINT('Ctrl Pts',(6.16700569777559,31.459641895636,54.1968066170301));
#105411=CARTESIAN_POINT('Ctrl Pts',(6.16839809479899,31.4696293959761,54.2152405222175));
#105412=CARTESIAN_POINT('Ctrl Pts',(6.16906595583971,31.4743597685916,54.2241641411716));
#105413=CARTESIAN_POINT('Ctrl Pts',(6.17083175085771,31.4867035600154,54.2479707647085));
#105414=CARTESIAN_POINT('Ctrl Pts',(6.17192467978531,31.4941747486084,54.262926530197));
#105415=CARTESIAN_POINT('Ctrl Pts',(6.17599588874745,31.521346224349,54.3194298229548));
#105416=CARTESIAN_POINT('Ctrl Pts',(6.17892323530642,31.5395498953674,54.3616765719644));
#105417=CARTESIAN_POINT('Ctrl Pts',(6.18884425669667,31.5960594324387,54.5093616280592));
#105418=CARTESIAN_POINT('Ctrl Pts',(6.1955834187822,31.6254574578055,54.6178740724291));
#105419=CARTESIAN_POINT('Ctrl Pts',(6.20541143011197,31.6514884380471,54.7754832350751));
#105420=CARTESIAN_POINT('Ctrl Pts',(6.20836769698654,31.6572282965008,54.8227555652822));
#105421=CARTESIAN_POINT('Ctrl Pts',(6.21316100842611,31.6630920843164,54.8977922958354));
#105422=CARTESIAN_POINT('Ctrl Pts',(6.21494786037152,31.6645601052876,54.9254269459025));
#105423=CARTESIAN_POINT('Ctrl Pts',(6.21738876580524,31.6656043790455,54.9624941829058));
#105424=CARTESIAN_POINT('Ctrl Pts',(6.2180124066811,31.6657897214408,54.9719068075026));
#105425=CARTESIAN_POINT('Ctrl Pts',(6.21905793229511,31.665965463337,54.9875797775692));
#105426=CARTESIAN_POINT('Ctrl Pts',(6.21947740362127,31.6660003704114,54.9938395883496));
#105427=CARTESIAN_POINT('Ctrl Pts',(6.22033485673021,31.6659996108333,55.006574221476));
#105428=CARTESIAN_POINT('Ctrl Pts',(6.22077295319821,31.6659614782214,55.0130488755287));
#105429=CARTESIAN_POINT('Ctrl Pts',(6.22192132873125,31.6657634983231,55.029942377));
#105430=CARTESIAN_POINT('Ctrl Pts',(6.22263476050851,31.6655436442829,55.0403600466417));
#105431=CARTESIAN_POINT('Ctrl Pts',(6.22592344924527,31.6640892228774,55.0880598623975));
#105432=CARTESIAN_POINT('Ctrl Pts',(6.2285521248893,31.6617005110438,55.1252933180455));
#105433=CARTESIAN_POINT('Ctrl Pts',(6.23683766796736,31.650388174945,55.2407811107911));
#105434=CARTESIAN_POINT('Ctrl Pts',(6.24259887178799,31.6371654375801,55.3185046605562));
#105435=CARTESIAN_POINT('Ctrl Pts',(6.25289734072264,31.603563647212,55.4561870396466));
#105436=CARTESIAN_POINT('Ctrl Pts',(6.25743983383605,31.5851786325435,55.5164548041091));
#105437=CARTESIAN_POINT('Ctrl Pts',(6.26189397015589,31.5634377553307,55.5755157558282));
#105438=CARTESIAN_POINT('',(6.02851963656332,31.6659993037065,54.9984768292001));
#105439=CARTESIAN_POINT('Ctrl Pts',(6.06643882015545,31.5634376718252,55.5755159826781));
#105440=CARTESIAN_POINT('Ctrl Pts',(6.06472934739696,31.571932695597,55.5524385346354));
#105441=CARTESIAN_POINT('Ctrl Pts',(6.06303542075663,31.5799172711098,55.5291716135343));
#105442=CARTESIAN_POINT('Ctrl Pts',(6.06017046701639,31.5926705752753,55.4891417128373));
#105443=CARTESIAN_POINT('Ctrl Pts',(6.0589915588576,31.5976959179968,55.4724690150401));
#105444=CARTESIAN_POINT('Ctrl Pts',(6.05705752028612,31.6055667482191,55.4447926286377));
#105445=CARTESIAN_POINT('Ctrl Pts',(6.0562975660611,31.608562580033,55.4338334964505));
#105446=CARTESIAN_POINT('Ctrl Pts',(6.05481403277105,31.614218559563,55.4122787407976));
#105447=CARTESIAN_POINT('Ctrl Pts',(6.05409021742884,31.6168870540454,55.4016859249121));
#105448=CARTESIAN_POINT('Ctrl Pts',(6.05265582349213,31.6219917817132,55.3805467114568));
#105449=CARTESIAN_POINT('Ctrl Pts',(6.05194521956491,31.6244298025128,55.3700013046029));
#105450=CARTESIAN_POINT('Ctrl Pts',(6.05027908981712,31.6299294334358,55.3451103938039));
#105451=CARTESIAN_POINT('Ctrl Pts',(6.04932629407405,31.6329047289416,55.3307465946524));
#105452=CARTESIAN_POINT('Ctrl Pts',(6.04149014513026,31.6559460428788,55.2116094284625));
#105453=CARTESIAN_POINT('Ctrl Pts',(6.03493536642089,31.6660964531918,55.1051698531878));
#105454=CARTESIAN_POINT('Ctrl Pts',(6.02841825655256,31.665999309357,54.9984830221305));
#105455=CARTESIAN_POINT('Ctrl Pts',(6.02851963656332,31.6659993037066,54.9984768292001));
#105456=CARTESIAN_POINT('Ctrl Pts',(6.02319560874737,31.6659265050777,54.9188518357291));
#105457=CARTESIAN_POINT('Ctrl Pts',(6.01787158093143,31.6601415384276,54.8394810237068));
#105458=CARTESIAN_POINT('Ctrl Pts',(6.01254755311548,31.6487752899906,54.7610522167576));
#105459=CARTESIAN_POINT('Ctrl Pts',(6.00879991050439,31.6407744608358,54.7058453040553));
#105460=CARTESIAN_POINT('Ctrl Pts',(6.0050522678933,31.6300091693766,54.651104499668));
#105461=CARTESIAN_POINT('Ctrl Pts',(6.00130462528222,31.6165387634104,54.597062751298));
#105462=CARTESIAN_POINT('Ctrl Pts',(5.99722727558211,31.6018832688966,54.5382665614325));
#105463=CARTESIAN_POINT('Ctrl Pts',(5.993149925882,31.5839855577694,54.4801495795245));
#105464=CARTESIAN_POINT('Ctrl Pts',(5.98907257618189,31.5629257672557,54.4230952885891));
#105465=CARTESIAN_POINT('Ctrl Pts',(5.98495160860947,31.5416406874435,54.3654306534447));
#105466=CARTESIAN_POINT('Ctrl Pts',(5.98083064103704,31.5171255131336,54.3088521143315));
#105467=CARTESIAN_POINT('Ctrl Pts',(5.97670967346462,31.4895158984509,54.2537437516095));
#105468=CARTESIAN_POINT('Ctrl Pts',(5.97264355643921,31.4622737708795,54.1993688874622));
#105469=CARTESIAN_POINT('Ctrl Pts',(5.96857743941381,31.4320193111664,54.1464257733204));
#105470=CARTESIAN_POINT('Ctrl Pts',(5.96451132238841,31.3989316336097,54.095264522368));
#105471=CARTESIAN_POINT('Ctrl Pts',(5.96044769316903,31.3658642003606,54.0441345738271));
#105472=CARTESIAN_POINT('Ctrl Pts',(5.95638406394966,31.3299672636836,53.994784755908));
#105473=CARTESIAN_POINT('Ctrl Pts',(5.95232043473028,31.2914648767165,53.9475388500246));
#105474=CARTESIAN_POINT('Ctrl Pts',(5.9482577821136,31.2529717429399,53.9003042986414));
#105475=CARTESIAN_POINT('Ctrl Pts',(5.94419512949692,31.21187472517,53.8551730522363));
#105476=CARTESIAN_POINT('Ctrl Pts',(5.94013247688024,31.1684387532835,53.8124365786093));
#105477=CARTESIAN_POINT('Ctrl Pts',(5.93596888334386,31.1239235685369,53.7686382718994));
#105478=CARTESIAN_POINT('Ctrl Pts',(5.93180528980747,31.0769520072831,53.7273557654103));
#105479=CARTESIAN_POINT('Ctrl Pts',(5.92764169627109,31.0278483005124,53.6888616125162));
#105480=CARTESIAN_POINT('Ctrl Pts',(5.92357385644512,30.9798738735519,53.6512527424761));
#105481=CARTESIAN_POINT('Ctrl Pts',(5.91950601661914,30.9298648035666,53.6163055754419));
#105482=CARTESIAN_POINT('Ctrl Pts',(5.91543817679317,30.8781537564999,53.5842309581202));
#105483=CARTESIAN_POINT('Ctrl Pts',(5.91122670640158,30.8246168541251,53.551023824371));
#105484=CARTESIAN_POINT('Ctrl Pts',(5.90701523600999,30.769256040786,53.520896213991));
#105485=CARTESIAN_POINT('Ctrl Pts',(5.9028037656184,30.7124665881183,53.4940294289678));
#105486=CARTESIAN_POINT('Ctrl Pts',(5.89859229522682,30.6556771354505,53.4671626439445));
#105487=CARTESIAN_POINT('Ctrl Pts',(5.89438082483523,30.5974596275331,53.4435568429065));
#105488=CARTESIAN_POINT('Ctrl Pts',(5.89016935444364,30.5382274340246,53.4233366785318));
#105489=CARTESIAN_POINT('Ctrl Pts',(5.88609200474353,30.4808815799681,53.4037604561002));
#105490=CARTESIAN_POINT('Ctrl Pts',(5.88201465504341,30.4223478962537,53.3872765390741));
#105491=CARTESIAN_POINT('Ctrl Pts',(5.87793730534329,30.36299202722,53.3740255880935));
#105492=CARTESIAN_POINT('Ctrl Pts',(5.87381633777087,30.3030011926064,53.3606328836871));
#105493=CARTESIAN_POINT('Ctrl Pts',(5.86969537019844,30.2421709473292,53.3505429818469));
#105494=CARTESIAN_POINT('Ctrl Pts',(5.86557440262602,30.1808975479542,53.3438502250267));
#105495=CARTESIAN_POINT('Ctrl Pts',(5.86150828560061,30.1204397044928,53.3372465495608));
#105496=CARTESIAN_POINT('Ctrl Pts',(5.8574421685752,30.0595509558089,53.3339501953221));
#105497=CARTESIAN_POINT('Ctrl Pts',(5.85337605154979,29.9986225924009,53.3340005694034));
#105498=CARTESIAN_POINT('Ctrl Pts',(5.84931242233042,29.9377315072978,53.3340509126639));
#105499=CARTESIAN_POINT('Ctrl Pts',(5.84524879311104,29.8768013664309,53.3374439239197));
#105500=CARTESIAN_POINT('Ctrl Pts',(5.84118516389166,29.8162257110446,53.3441669737806));
#105501=CARTESIAN_POINT('Ctrl Pts',(5.83712251127498,29.7556646136666,53.3508884079063));
#105502=CARTESIAN_POINT('Ctrl Pts',(5.8330598586583,29.6954583412569,53.3609382354768));
#105503=CARTESIAN_POINT('Ctrl Pts',(5.82899720604162,29.6359954570605,53.3742519590295));
#105504=CARTESIAN_POINT('Ctrl Pts',(5.82483361250524,29.5750551543435,53.387896476186));
#105505=CARTESIAN_POINT('Ctrl Pts',(5.82067001896886,29.5148962345786,53.404969181928));
#105506=CARTESIAN_POINT('Ctrl Pts',(5.81650642543249,29.455923532972,53.4253454988391));
#105507=CARTESIAN_POINT('Ctrl Pts',(5.81243858560651,29.3983070768638,53.4452532042176));
#105508=CARTESIAN_POINT('Ctrl Pts',(5.80837074578053,29.3418233160874,53.4683139139436));
#105509=CARTESIAN_POINT('Ctrl Pts',(5.80430290595455,29.2868298182051,53.4943624965489));
#105510=CARTESIAN_POINT('Ctrl Pts',(5.80009143556298,29.2298945655972,53.5213308234933));
#105511=CARTESIAN_POINT('Ctrl Pts',(5.7958799651714,29.1745573309091,53.5515017203615));
#105512=CARTESIAN_POINT('Ctrl Pts',(5.79166849477982,29.1211848149767,53.5846414339212));
#105513=CARTESIAN_POINT('Ctrl Pts',(5.78745702438825,29.0678122990444,53.617781147481));
#105514=CARTESIAN_POINT('Ctrl Pts',(5.78324555399667,29.0164049519221,53.6538892730567));
#105515=CARTESIAN_POINT('Ctrl Pts',(5.7790340836051,28.9672916966112,53.6926861279281));
#105516=CARTESIAN_POINT('Ctrl Pts',(5.77495673390498,28.9197425277474,53.7302474378429));
#105517=CARTESIAN_POINT('Ctrl Pts',(5.77087938420487,28.8741471032048,53.7704838505866));
#105518=CARTESIAN_POINT('Ctrl Pts',(5.76680203450475,28.8308219104712,53.8131644617026));
#105519=CARTESIAN_POINT('Ctrl Pts',(5.76268106693233,28.7870332419841,53.8563016530932));
#105520=CARTESIAN_POINT('Ctrl Pts',(5.7585600993599,28.745564135601,53.901935391439));
#105521=CARTESIAN_POINT('Ctrl Pts',(5.75443913178748,28.7067087678565,53.9497839322973));
#105522=CARTESIAN_POINT('Ctrl Pts',(5.75037301476207,28.6683705694754,53.9969956036356));
#105523=CARTESIAN_POINT('Ctrl Pts',(5.74630689773666,28.6325772882021,54.0463630694733));
#105524=CARTESIAN_POINT('Ctrl Pts',(5.74224078071126,28.5995742535652,54.0975789626109));
#105525=CARTESIAN_POINT('Ctrl Pts',(5.73817715149188,28.5665914114481,54.1487635199047));
#105526=CARTESIAN_POINT('Ctrl Pts',(5.7341135222725,28.5363957078717,54.201793832717));
#105527=CARTESIAN_POINT('Ctrl Pts',(5.73004989305313,28.5091899749724,54.2563324201787));
#105528=CARTESIAN_POINT('Ctrl Pts',(5.72598724043645,28.4819907803645,54.3108579005067));
#105529=CARTESIAN_POINT('Ctrl Pts',(5.72192458781976,28.4577803583886,54.36689047799));
#105530=CARTESIAN_POINT('Ctrl Pts',(5.71786193520308,28.436715264666,54.4240687226137));
#105531=CARTESIAN_POINT('Ctrl Pts',(5.7136983416667,28.4151267863141,54.4826676214611));
#105532=CARTESIAN_POINT('Ctrl Pts',(5.70953474813032,28.3968422725698,54.5424693728215));
#105533=CARTESIAN_POINT('Ctrl Pts',(5.70537115459394,28.3819766285954,54.6030662906876));
#105534=CARTESIAN_POINT('Ctrl Pts',(5.70130331476797,28.3674528625098,54.6622696095691));
#105535=CARTESIAN_POINT('Ctrl Pts',(5.69723547494199,28.3561924059843,54.7222313780833));
#105536=CARTESIAN_POINT('Ctrl Pts',(5.69316763511601,28.3482504566835,54.7825616267682));
#105537=CARTESIAN_POINT('Ctrl Pts',(5.68895616472443,28.3400280866387,54.8450220644753));
#105538=CARTESIAN_POINT('Ctrl Pts',(5.68474469433285,28.3353630426135,54.9078768966285));
#105539=CARTESIAN_POINT('Ctrl Pts',(5.68053322394127,28.3342578236991,54.9706912625246));
#105540=CARTESIAN_POINT('Ctrl Pts',(5.67632175354969,28.3331526047847,55.0335056284206));
#105541=CARTESIAN_POINT('Ctrl Pts',(5.67211028315811,28.3356071150888,55.0962789304679));
#105542=CARTESIAN_POINT('Ctrl Pts',(5.66789881276653,28.3415647769982,55.1585831362628));
#105543=CARTESIAN_POINT('Ctrl Pts',(5.66382146306642,28.3473327080867,55.2189031696937));
#105544=CARTESIAN_POINT('Ctrl Pts',(5.6597441133663,28.3564077503369,55.2790326571175));
#105545=CARTESIAN_POINT('Ctrl Pts',(5.65566676366619,28.3687675623041,55.3385804693256));
#105546=CARTESIAN_POINT('Ctrl Pts',(5.65154579609376,28.3812595946448,55.3987653004457));
#105547=CARTESIAN_POINT('Ctrl Pts',(5.64742482852134,28.3971071320074,55.4583554038117));
#105548=CARTESIAN_POINT('Ctrl Pts',(5.64330386094891,28.4162330194006,55.5169508208359));
#105549=CARTESIAN_POINT('Ctrl Pts',(5.63923774392351,28.4351043390575,55.5747663261962));
#105550=CARTESIAN_POINT('Ctrl Pts',(5.6351716268981,28.4571671072163,55.6316129613537));
#105551=CARTESIAN_POINT('Ctrl Pts',(5.6311055098727,28.4822961492295,55.6871179093549));
#105552=CARTESIAN_POINT('Ctrl Pts',(5.62704188065332,28.5074098163328,55.7425888973045));
#105553=CARTESIAN_POINT('Ctrl Pts',(5.62297825143395,28.5355858268912,55.7967193602662));
#105554=CARTESIAN_POINT('Ctrl Pts',(5.61891462221457,28.5666506573924,55.8491558526245));
#105555=CARTESIAN_POINT('Ctrl Pts',(5.61485196959789,28.5977080221541,55.9015797430408));
#105556=CARTESIAN_POINT('Ctrl Pts',(5.61078931698121,28.6316525678179,55.9523100307528));
#105557=CARTESIAN_POINT('Ctrl Pts',(5.60672666436454,28.6682655514314,56.0010191599044));
#105558=CARTESIAN_POINT('Ctrl Pts',(5.60256307082815,28.7057882235139,56.0509385191097));
#105559=CARTESIAN_POINT('Ctrl Pts',(5.59839947729177,28.7461134161297,56.0987344577357));
#105560=CARTESIAN_POINT('Ctrl Pts',(5.59423588375539,28.7889609349392,56.1440893247018));
#105561=CARTESIAN_POINT('Ctrl Pts',(5.59016804392942,28.8308230528272,56.1884011271232));
#105562=CARTESIAN_POINT('Ctrl Pts',(5.58610020410344,28.8750922791935,56.2303826368797));
#105563=CARTESIAN_POINT('Ctrl Pts',(5.58203236427747,28.9214709209376,56.2697759745785));
#105564=CARTESIAN_POINT('Ctrl Pts',(5.57782089388588,28.9694871371267,56.3105602439798));
#105565=CARTESIAN_POINT('Ctrl Pts',(5.5736094234943,29.0197640671424,56.3485697542235));
#105566=CARTESIAN_POINT('Ctrl Pts',(5.56939795310272,29.0719377209833,56.3835665528866));
#105567=CARTESIAN_POINT('Ctrl Pts',(5.56518648271114,29.1241113748243,56.4185633515496));
#105568=CARTESIAN_POINT('Ctrl Pts',(5.56097501231955,29.1781811984192,56.4505471950831));
#105569=CARTESIAN_POINT('Ctrl Pts',(5.55676354192797,29.2337568974359,56.4793334674011));
#105570=CARTESIAN_POINT('Ctrl Pts',(5.55268619222786,29.287562703639,56.5072029970166));
#105571=CARTESIAN_POINT('Ctrl Pts',(5.54860884252774,29.3430020821623,56.5321907331816));
#105572=CARTESIAN_POINT('Ctrl Pts',(5.54453149282763,29.3997343111234,56.5541033114814));
#105573=CARTESIAN_POINT('Ctrl Pts',(5.5404105252552,29.4570734390018,56.5762503018657));
#105574=CARTESIAN_POINT('Ctrl Pts',(5.53628955768277,29.5157328156011,56.595255627346));
#105575=CARTESIAN_POINT('Ctrl Pts',(5.53216859011035,29.5753345721937,56.6109671860178));
#105576=CARTESIAN_POINT('Ctrl Pts',(5.52810247308494,29.6341430226283,56.626469622057));
#105577=CARTESIAN_POINT('Ctrl Pts',(5.52403635605954,29.6938684100509,56.6387653027937));
#105578=CARTESIAN_POINT('Ctrl Pts',(5.51997023903413,29.7541296244664,56.6477571903757));
#105579=CARTESIAN_POINT('Ctrl Pts',(5.51590660981475,29.8143539687644,56.6567435763768));
#105580=CARTESIAN_POINT('Ctrl Pts',(5.51184298059538,29.8751129847361,56.6624301016414));
#105581=CARTESIAN_POINT('Ctrl Pts',(5.507779351376,29.9360156144035,56.6647708546223));
#105582=CARTESIAN_POINT('Ctrl Pts',(5.50371669875932,29.9969036074814,56.6671110450554));
#105583=CARTESIAN_POINT('Ctrl Pts',(5.49965404614264,30.0579346343862,56.6661070397697));
#105584=CARTESIAN_POINT('Ctrl Pts',(5.49559139352596,30.1187148628539,56.6617649597153));
#105585=CARTESIAN_POINT('Ctrl Pts',(5.49142779998958,30.18100524066,56.6573149960696));
#105586=CARTESIAN_POINT('Ctrl Pts',(5.4872642064532,30.2430316268305,56.64935884579));
#105587=CARTESIAN_POINT('Ctrl Pts',(5.48310061291682,30.3043751815094,56.6379596298081));
#105588=CARTESIAN_POINT('Ctrl Pts',(5.47903277309084,30.3643079661603,56.626822571315));
#105589=CARTESIAN_POINT('Ctrl Pts',(5.47496493326487,30.423588499628,56.6123993290894));
#105590=CARTESIAN_POINT('Ctrl Pts',(5.47089709343889,30.4818386681553,56.594800143551));
#105591=CARTESIAN_POINT('Ctrl Pts',(5.46668562304731,30.5421455805589,56.5765795517918));
#105592=CARTESIAN_POINT('Ctrl Pts',(5.46247415265573,30.601347426917,56.5549547061609));
#105593=CARTESIAN_POINT('Ctrl Pts',(5.45826268226415,30.6590468779299,56.5301023536649));
#105594=CARTESIAN_POINT('Ctrl Pts',(5.45405121187257,30.7167463289428,56.5052500011689));
#105595=CARTESIAN_POINT('Ctrl Pts',(5.44983974148099,30.772942879486,56.477170475215));
#105596=CARTESIAN_POINT('Ctrl Pts',(5.44562827108941,30.8272697439158,56.4460915499378));
#105597=CARTESIAN_POINT('Ctrl Pts',(5.44155183030141,30.879854761844,56.4160090877886));
#105598=CARTESIAN_POINT('Ctrl Pts',(5.43747538951342,30.9309053356807,56.3829925194285));
#105599=CARTESIAN_POINT('Ctrl Pts',(5.43339894872543,30.9800744459655,56.3472230997001));
#105600=CARTESIAN_POINT('Ctrl Pts',(5.42932840892906,31.0291723798188,56.3115054592216));
#105601=CARTESIAN_POINT('Ctrl Pts',(5.4252578691327,31.0763938387612,56.2730431653455));
#105602=CARTESIAN_POINT('Ctrl Pts',(5.42118732933634,31.1214179744792,56.2320623874281));
#105603=CARTESIAN_POINT('Ctrl Pts',(5.41712116909536,31.1663936680481,56.1911257013499));
#105604=CARTESIAN_POINT('Ctrl Pts',(5.41305500885438,31.2091763505024,56.1476762483517));
#105605=CARTESIAN_POINT('Ctrl Pts',(5.4089888486134,31.2494773543157,56.101981098319));
#105606=CARTESIAN_POINT('Ctrl Pts',(5.40492500374107,31.2897554097759,56.0563119681949));
#105607=CARTESIAN_POINT('Ctrl Pts',(5.40086115886875,31.3275542482263,56.0084000576379));
#105608=CARTESIAN_POINT('Ctrl Pts',(5.39679731399643,31.3626226620096,55.9585486325575));
#105609=CARTESIAN_POINT('Ctrl Pts',(5.39273479857776,31.3976796034478,55.9087135159637));
#105610=CARTESIAN_POINT('Ctrl Pts',(5.38867228315909,31.4300076027422,55.8569405655971));
#105611=CARTESIAN_POINT('Ctrl Pts',(5.38460976774043,31.4593976665616,55.8035635947668));
#105612=CARTESIAN_POINT('Ctrl Pts',(5.38054576406626,31.4887984970907,55.7501670699011));
#105613=CARTESIAN_POINT('Ctrl Pts',(5.37648176039209,31.5152589994234,55.6951658017929));
#105614=CARTESIAN_POINT('Ctrl Pts',(5.37241775671792,31.5386160469458,55.6389183516546));
#105615=CARTESIAN_POINT('Ctrl Pts',(5.37090280232716,31.5473229440197,55.6179507718028));
#105616=CARTESIAN_POINT('Ctrl Pts',(5.3693878479364,31.555599061099,55.5968102300939));
#105617=CARTESIAN_POINT('Ctrl Pts',(5.36787289354565,31.5634376782623,55.5755159651912));
#105618=CARTESIAN_POINT('Origin',(5.,30.,55.));
#105619=CARTESIAN_POINT('',(4.66781602428403,31.5660238537031,55.5764683070372));
#105620=CARTESIAN_POINT('',(4.86076605062571,31.563437683379,55.5755159512911));
#105621=CARTESIAN_POINT('',(5.,31.5634376782623,55.5755159651912));
#105622=CARTESIAN_POINT('',(5.52206895547911,31.6659994155302,55.0013955117896));
#105623=CARTESIAN_POINT('Ctrl Pts',(4.86076605062571,31.563437683379,55.575515951291));
#105624=CARTESIAN_POINT('Ctrl Pts',(4.86235663650181,31.5544423538878,55.5999525234998));
#105625=CARTESIAN_POINT('Ctrl Pts',(4.86394540308067,31.5448739300461,55.6241786808564));
#105626=CARTESIAN_POINT('Ctrl Pts',(4.86634047276108,31.5296416355314,55.6602455418293));
#105627=CARTESIAN_POINT('Ctrl Pts',(4.86714313447064,31.5244012764948,55.6722562398718));
#105628=CARTESIAN_POINT('Ctrl Pts',(4.87251833492517,31.4884500562448,55.7520725425401));
#105629=CARTESIAN_POINT('Ctrl Pts',(4.87714293081916,31.4533698782181,55.8178079565178));
#105630=CARTESIAN_POINT('Ctrl Pts',(4.88280612972829,31.4075242765575,55.8913934335003));
#105631=CARTESIAN_POINT('Ctrl Pts',(4.88361468741238,31.4009149122755,55.9017451021056));
#105632=CARTESIAN_POINT('Ctrl Pts',(4.88489210896611,31.3903866965534,55.9178393931811));
#105633=CARTESIAN_POINT('Ctrl Pts',(4.88535609265786,31.3865451634237,55.923632406879));
#105634=CARTESIAN_POINT('Ctrl Pts',(4.88622876943183,31.3792901511753,55.9344256698058));
#105635=CARTESIAN_POINT('Ctrl Pts',(4.88663688748976,31.3758855231996,55.9394315706274));
#105636=CARTESIAN_POINT('Ctrl Pts',(4.88760317836795,31.3677960797829,55.9511873592213));
#105637=CARTESIAN_POINT('Ctrl Pts',(4.88816283590673,31.3630885313786,55.9579212685606));
#105638=CARTESIAN_POINT('Ctrl Pts',(4.89004739048439,31.3471561890903,55.9803564289671));
#105639=CARTESIAN_POINT('Ctrl Pts',(4.89138583176619,31.335708847404,55.9958967422528));
#105640=CARTESIAN_POINT('Ctrl Pts',(4.89471765645642,31.3068330198224,56.0337034720899));
#105641=CARTESIAN_POINT('Ctrl Pts',(4.89672561742635,31.2891029932193,56.0557313589832));
#105642=CARTESIAN_POINT('Ctrl Pts',(4.90592645439317,31.2060698470409,56.1536806195336));
#105643=CARTESIAN_POINT('Ctrl Pts',(4.91329155941284,31.134563286062,56.2240710967319));
#105644=CARTESIAN_POINT('Ctrl Pts',(4.92646737058855,30.9933318201047,56.3400260584977));
#105645=CARTESIAN_POINT('Ctrl Pts',(4.93230929159736,30.9256791495063,56.3876237797659));
#105646=CARTESIAN_POINT('Ctrl Pts',(4.93930501687842,30.8379345535513,56.4400715703094));
#105647=CARTESIAN_POINT('Ctrl Pts',(4.94063617362945,30.8209278042958,56.4498337976376));
#105648=CARTESIAN_POINT('Ctrl Pts',(4.94275299396792,30.7933925546242,56.4649997028176));
#105649=CARTESIAN_POINT('Ctrl Pts',(4.94354543514238,30.7829723901156,56.4705951597197));
#105650=CARTESIAN_POINT('Ctrl Pts',(4.94505002476253,30.7629771240952,56.4810595085514));
#105651=CARTESIAN_POINT('Ctrl Pts',(4.94576282432307,30.7534128385819,56.4859476651747));
#105652=CARTESIAN_POINT('Ctrl Pts',(4.94739597361152,30.7312928664252,56.4969843584031));
#105653=CARTESIAN_POINT('Ctrl Pts',(4.94831403327499,30.7187056127938,56.5030680914914));
#105654=CARTESIAN_POINT('Ctrl Pts',(4.9512248397847,30.6783257533892,56.5219614318327));
#105655=CARTESIAN_POINT('Ctrl Pts',(4.95319692678012,30.6502552341312,56.5341645109156));
#105656=CARTESIAN_POINT('Ctrl Pts',(4.95785528068165,30.5824290333054,56.5614541919447));
#105657=CARTESIAN_POINT('Ctrl Pts',(4.96051897956434,30.5424005024078,56.5758060944509));
#105658=CARTESIAN_POINT('Ctrl Pts',(4.96772435997881,30.4315771743691,56.6108167218702));
#105659=CARTESIAN_POINT('Ctrl Pts',(4.97219846733111,30.3598920182885,56.6283327268158));
#105660=CARTESIAN_POINT('Ctrl Pts',(4.97755725133607,30.2736090208458,56.6434374930756));
#105661=CARTESIAN_POINT('Ctrl Pts',(4.97840764802541,30.259906398373,56.6456601557228));
#105662=CARTESIAN_POINT('Ctrl Pts',(4.98377372505517,30.1735058138186,56.6585689086929));
#105663=CARTESIAN_POINT('Ctrl Pts',(4.98834189284911,30.1002040276405,56.6646055127479));
#105664=CARTESIAN_POINT('Ctrl Pts',(4.99394240468856,30.0144768926542,56.6659823454786));
#105665=CARTESIAN_POINT('Ctrl Pts',(4.99475073555195,30.0021988454305,56.666043786695));
#105666=CARTESIAN_POINT('Ctrl Pts',(4.99602787579493,29.9829715155292,56.6659274706254));
#105667=CARTESIAN_POINT('Ctrl Pts',(4.99649180847242,29.9760218314703,56.6658419341962));
#105668=CARTESIAN_POINT('Ctrl Pts',(4.99736444665823,29.9630196971493,56.665600526189));
#105669=CARTESIAN_POINT('Ctrl Pts',(4.99777257779605,29.9569672993867,56.6654551442883));
#105670=CARTESIAN_POINT('Ctrl Pts',(4.99873897767125,29.9427017624914,56.6650346672203));
#105671=CARTESIAN_POINT('Ctrl Pts',(4.99929873214277,29.9344897185266,56.66473178831));
#105672=CARTESIAN_POINT('Ctrl Pts',(5.00118396234252,29.9069901123561,56.6635137536867));
#105673=CARTESIAN_POINT('Ctrl Pts',(5.00252299503156,29.8877170753713,56.6623240698753));
#105674=CARTESIAN_POINT('Ctrl Pts',(5.00585662201406,29.8402677783128,56.6585662418381));
#105675=CARTESIAN_POINT('Ctrl Pts',(5.00786581272343,29.81212843595,56.6556148271649));
#105676=CARTESIAN_POINT('Ctrl Pts',(5.01707757252619,29.6846547490511,56.6389531863565));
#105677=CARTESIAN_POINT('Ctrl Pts',(5.0244526694838,29.5866068564928,56.6170085804126));
#105678=CARTESIAN_POINT('Ctrl Pts',(5.03762621900644,29.4126241659588,56.5611989952842));
#105679=CARTESIAN_POINT('Ctrl Pts',(5.04345690518757,29.3360901828385,56.5302222415589));
#105680=CARTESIAN_POINT('Ctrl Pts',(5.05044177860603,29.2445792350055,56.4850184270763));
#105681=CARTESIAN_POINT('Ctrl Pts',(5.05177261180772,29.2271579603793,56.4760269305421));
#105682=CARTESIAN_POINT('Ctrl Pts',(5.05388904417198,29.19948737997,56.4611212806397));
#105683=CARTESIAN_POINT('Ctrl Pts',(5.05468141651019,29.1891357749937,56.4554020312796));
#105684=CARTESIAN_POINT('Ctrl Pts',(5.05618595286663,29.1695002115588,56.4442788742467));
#105685=CARTESIAN_POINT('Ctrl Pts',(5.05689876718966,29.1602059467897,56.4388944793154));
#105686=CARTESIAN_POINT('Ctrl Pts',(5.05853205943992,29.1389346158975,56.4262951607404));
#105687=CARTESIAN_POINT('Ctrl Pts',(5.05945024589866,29.1269948967195,56.4190185307593));
#105688=CARTESIAN_POINT('Ctrl Pts',(5.0623619124653,29.0892100928351,56.3953332469326));
#105689=CARTESIAN_POINT('Ctrl Pts',(5.06433471493293,29.0637241660238,56.3783616638133));
#105690=CARTESIAN_POINT('Ctrl Pts',(5.06899512294395,29.0039846144587,56.3361579155534));
#105691=CARTESIAN_POINT('Ctrl Pts',(5.07166013212919,28.9702009022567,56.3102972266712));
#105692=CARTESIAN_POINT('Ctrl Pts',(5.07886618036332,28.880675439424,56.2361636681823));
#105693=CARTESIAN_POINT('Ctrl Pts',(5.08333973163574,28.8270894971359,56.1854405943642));
#105694=CARTESIAN_POINT('Ctrl Pts',(5.08870349548183,28.7675510834482,56.1210802167872));
#105695=CARTESIAN_POINT('Ctrl Pts',(5.08955939369601,28.758193311437,56.1107057785937));
#105696=CARTESIAN_POINT('Ctrl Pts',(5.09492391492343,28.7005209677286,56.0451276905725));
#105697=CARTESIAN_POINT('Ctrl Pts',(5.09948507290607,28.6557720421935,55.986907351982));
#105698=CARTESIAN_POINT('Ctrl Pts',(5.10507780280791,28.6081863491954,55.9157300400978));
#105699=CARTESIAN_POINT('Ctrl Pts',(5.10588610492336,28.6014758125052,55.905448408324));
#105700=CARTESIAN_POINT('Ctrl Pts',(5.10716320951199,28.5911456251963,55.8892320596307));
#105701=CARTESIAN_POINT('Ctrl Pts',(5.10762713572351,28.5874482853521,55.883347018079));
#105702=CARTESIAN_POINT('Ctrl Pts',(5.10849976902017,28.5805992579069,55.8722924906557));
#105703=CARTESIAN_POINT('Ctrl Pts',(5.10890790181771,28.577438787206,55.8671287373172));
#105704=CARTESIAN_POINT('Ctrl Pts',(5.1098743155168,28.5700548366442,55.85491541322));
#105705=CARTESIAN_POINT('Ctrl Pts',(5.11043408228111,28.5658552951224,55.8478516924311));
#105706=CARTESIAN_POINT('Ctrl Pts',(5.11231939817491,28.551963216115,55.8240863797617));
#105707=CARTESIAN_POINT('Ctrl Pts',(5.11365850587876,28.5425092294102,55.8072480801908));
#105708=CARTESIAN_POINT('Ctrl Pts',(5.11699236148828,28.5199301492602,55.7653428766653));
#105709=CARTESIAN_POINT('Ctrl Pts',(5.11900170820245,28.5071471452543,55.7400990847667));
#105710=CARTESIAN_POINT('Ctrl Pts',(5.12821485489357,28.452000748355,55.6239486258526));
#105711=CARTESIAN_POINT('Ctrl Pts',(5.13559122067235,28.4172558720462,55.5296556087123));
#105712=CARTESIAN_POINT('Ctrl Pts',(5.14876448388332,28.3697891449328,55.3532167014955));
#105713=CARTESIAN_POINT('Ctrl Pts',(5.15459374451775,28.3543100239748,55.2721353545114));
#105714=CARTESIAN_POINT('Ctrl Pts',(5.1615772404742,28.3426579610005,55.1707559758881));
#105715=CARTESIAN_POINT('Ctrl Pts',(5.16290803222408,28.3407635223316,55.1512435309539));
#105716=CARTESIAN_POINT('Ctrl Pts',(5.16502441488257,28.3382789666538,55.1199127011607));
#105717=CARTESIAN_POINT('Ctrl Pts',(5.16581677840161,28.3374696371733,55.1081140773727));
#105718=CARTESIAN_POINT('Ctrl Pts',(5.1673213079361,28.3361650836573,55.0855846776702));
#105719=CARTESIAN_POINT('Ctrl Pts',(5.1680341241527,28.3356478796665,55.074855825759));
#105720=CARTESIAN_POINT('Ctrl Pts',(5.16966743472992,28.3346963188003,55.0501511489765));
#105721=CARTESIAN_POINT('Ctrl Pts',(5.17058563744198,28.3343340655208,55.0361732334579));
#105722=CARTESIAN_POINT('Ctrl Pts',(5.17349741426955,28.3337400167845,54.991580811281));
#105723=CARTESIAN_POINT('Ctrl Pts',(5.17547030846364,28.3341760311844,54.960962736805));
#105724=CARTESIAN_POINT('Ctrl Pts',(5.18013097984319,28.3372331129386,54.8878789036314));
#105725=CARTESIAN_POINT('Ctrl Pts',(5.18279615703603,28.3406372269072,54.845467062748));
#105726=CARTESIAN_POINT('Ctrl Pts',(5.19000228883895,28.3543658854286,54.7300439330904));
#105727=CARTESIAN_POINT('Ctrl Pts',(5.19447576684108,28.3679178182753,54.6575149154913));
#105728=CARTESIAN_POINT('Ctrl Pts',(5.19984011989559,28.3897012342677,54.5725782307036));
#105729=CARTESIAN_POINT('Ctrl Pts',(5.20069667615469,28.3933449462772,54.5590793539671));
#105730=CARTESIAN_POINT('Ctrl Pts',(5.20606099815161,28.4171617269136,54.4750633097786));
#105731=CARTESIAN_POINT('Ctrl Pts',(5.21062130456655,28.4418010098706,54.4059051296081));
#105732=CARTESIAN_POINT('Ctrl Pts',(5.21621308917605,28.475785663444,54.3273355964502));
#105733=CARTESIAN_POINT('Ctrl Pts',(5.21702138778401,28.4807841352829,54.3161214448463));
#105734=CARTESIAN_POINT('Ctrl Pts',(5.21829848802258,28.4888054471132,54.2986475005859));
#105735=CARTESIAN_POINT('Ctrl Pts',(5.21876241344514,28.4917444177771,54.2923493803947));
#105736=CARTESIAN_POINT('Ctrl Pts',(5.21963504614521,28.4973171378532,54.2805996443204));
#105737=CARTESIAN_POINT('Ctrl Pts',(5.22004317914523,28.4999413076421,54.275143758569));
#105738=CARTESIAN_POINT('Ctrl Pts',(5.22100959453115,28.5061974749979,54.2623160903091));
#105739=CARTESIAN_POINT('Ctrl Pts',(5.2215693627954,28.5098543441761,54.2549567451017));
#105740=CARTESIAN_POINT('Ctrl Pts',(5.22345468914561,28.5222861242735,54.2303958190944));
#105741=CARTESIAN_POINT('Ctrl Pts',(5.22479380600284,28.5313052743471,54.2133205118007));
#105742=CARTESIAN_POINT('Ctrl Pts',(5.22812768950991,28.5542657806628,54.1716226320691));
#105743=CARTESIAN_POINT('Ctrl Pts',(5.23013705526025,28.5685412927402,54.1471915306869));
#105744=CARTESIAN_POINT('Ctrl Pts',(5.23935037120251,28.6362162396475,54.0378628786241));
#105745=CARTESIAN_POINT('Ctrl Pts',(5.24672689182591,28.6965930003308,53.9575295465222));
#105746=CARTESIAN_POINT('Ctrl Pts',(5.2599001201097,28.8190831724509,53.8219573327791));
#105747=CARTESIAN_POINT('Ctrl Pts',(5.26572920679015,28.8788062375034,53.7649788243938));
#105748=CARTESIAN_POINT('Ctrl Pts',(5.27271253465233,28.9576579358876,53.7002064563712));
#105749=CARTESIAN_POINT('Ctrl Pts',(5.27404332133784,28.9730236603695,53.6880320547133));
#105750=CARTESIAN_POINT('Ctrl Pts',(5.27615969792345,28.9979984534086,53.668952011073));
#105751=CARTESIAN_POINT('Ctrl Pts',(5.27695206036505,29.0074720282609,53.6618729185927));
#105752=CARTESIAN_POINT('Ctrl Pts',(5.27845658906621,29.0256924072131,53.6485577775517));
#105753=CARTESIAN_POINT('Ctrl Pts',(5.27916940551415,29.0344256739778,53.6423043065102));
#105754=CARTESIAN_POINT('Ctrl Pts',(5.28080271833059,29.0546650866662,53.6281059112081));
#105755=CARTESIAN_POINT('Ctrl Pts',(5.28172092302855,29.0662120958323,53.62022043101));
#105756=CARTESIAN_POINT('Ctrl Pts',(5.28463271332843,29.1033541196631,53.5955359062602));
#105757=CARTESIAN_POINT('Ctrl Pts',(5.28660561873014,29.1293143327372,53.5792959904505));
#105758=CARTESIAN_POINT('Ctrl Pts',(5.29126632228987,29.1923737612445,53.5422260983115));
#105759=CARTESIAN_POINT('Ctrl Pts',(5.29393152001118,29.2298523818477,53.5220832510944));
#105760=CARTESIAN_POINT('Ctrl Pts',(5.30113766199339,29.3342705475308,53.4710159606947));
#105761=CARTESIAN_POINT('Ctrl Pts',(5.3056111310124,29.402555312167,53.4430645147566));
#105762=CARTESIAN_POINT('Ctrl Pts',(5.31097555531217,29.4857299830408,53.4152988074354));
#105763=CARTESIAN_POINT('Ctrl Pts',(5.31183219125765,29.4990484399682,53.4110383741189));
#105764=CARTESIAN_POINT('Ctrl Pts',(5.31719648891537,29.5825509913188,53.3854810017439));
#105765=CARTESIAN_POINT('Ctrl Pts',(5.32175669199643,29.6540155697621,53.3686731396946));
#105766=CARTESIAN_POINT('Ctrl Pts',(5.32734836190012,29.7384555793296,53.3546121249323));
#105767=CARTESIAN_POINT('Ctrl Pts',(5.32815666008225,29.7505880616639,53.3527294069703));
#105768=CARTESIAN_POINT('Ctrl Pts',(5.32943375979257,29.7696191468434,53.3499912219665));
#105769=CARTESIAN_POINT('Ctrl Pts',(5.32989768511939,29.7765044626304,53.3490445052972));
#105770=CARTESIAN_POINT('Ctrl Pts',(5.33077031774719,29.7893983698063,53.3473537555467));
#105771=CARTESIAN_POINT('Ctrl Pts',(5.3311784507719,29.795405352857,53.3465993584057));
#105772=CARTESIAN_POINT('Ctrl Pts',(5.33214486636234,29.8095755591308,53.3448981702983));
#105773=CARTESIAN_POINT('Ctrl Pts',(5.33270463480862,29.8177418227126,53.3439790206355));
#105774=CARTESIAN_POINT('Ctrl Pts',(5.33458996242873,29.8451190957674,53.3411025348467));
#105775=CARTESIAN_POINT('Ctrl Pts',(5.33592908039743,29.8643564839536,53.339418881393));
#105776=CARTESIAN_POINT('Ctrl Pts',(5.33926296729188,29.9118416903326,53.3360935690707));
#105777=CARTESIAN_POINT('Ctrl Pts',(5.34127233535368,29.9401098795163,53.3348364971635));
#105778=CARTESIAN_POINT('Ctrl Pts',(5.35048567184742,30.0686663857335,53.3323972406065));
#105779=CARTESIAN_POINT('Ctrl Pts',(5.35786221127302,30.1689043533885,53.339552523285));
#105780=CARTESIAN_POINT('Ctrl Pts',(5.37103725007931,30.3492635363559,53.368936493002));
#105781=CARTESIAN_POINT('Ctrl Pts',(5.37686805330178,30.4295491680146,53.3882170197411));
#105782=CARTESIAN_POINT('Ctrl Pts',(5.38385203872933,30.5267432920322,53.4193415230747));
#105783=CARTESIAN_POINT('Ctrl Pts',(5.38518190713605,30.5452926178412,53.4256443431887));
#105784=CARTESIAN_POINT('Ctrl Pts',(5.38729718258022,30.5748527040983,53.4362736331698));
#105785=CARTESIAN_POINT('Ctrl Pts',(5.38808934964544,30.5859355717253,53.4403925814524));
#105786=CARTESIAN_POINT('Ctrl Pts',(5.38959372734781,30.6070021964862,53.4484782583155));
#105787=CARTESIAN_POINT('Ctrl Pts',(5.39030658587293,30.6169932230632,53.4524242333991));
#105788=CARTESIAN_POINT('Ctrl Pts',(5.39194030534308,30.6399047730358,53.4617303459898));
#105789=CARTESIAN_POINT('Ctrl Pts',(5.39285887062399,30.6527974677927,53.4671571728283));
#105790=CARTESIAN_POINT('Ctrl Pts',(5.39577310790037,30.6937148995898,53.4849901488772));
#105791=CARTESIAN_POINT('Ctrl Pts',(5.39774804903468,30.7214672687489,53.4980078628039));
#105792=CARTESIAN_POINT('Ctrl Pts',(5.40241459905559,30.7868939522836,53.5309295206623));
#105793=CARTESIAN_POINT('Ctrl Pts',(5.40508352673329,30.8241952869313,53.55152746792));
#105794=CARTESIAN_POINT('Ctrl Pts',(5.41233927746679,30.9244107189907,53.611993133956));
#105795=CARTESIAN_POINT('Ctrl Pts',(5.41685664461958,30.9855040234186,53.6546820401439));
#105796=CARTESIAN_POINT('Ctrl Pts',(5.4222283522364,31.0539381406431,53.7096712117875));
#105797=CARTESIAN_POINT('Ctrl Pts',(5.42304582824291,31.0642370360891,53.7181523055947));
#105798=CARTESIAN_POINT('Ctrl Pts',(5.42835820140213,31.1303248987084,53.7739208609916));
#105799=CARTESIAN_POINT('Ctrl Pts',(5.43290598065822,31.183043878114,53.8247090086364));
#105800=CARTESIAN_POINT('Ctrl Pts',(5.43848386119012,31.2405120390993,53.8878684409762));
#105801=CARTESIAN_POINT('Ctrl Pts',(5.43929210777578,31.2486734655022,53.8970397656657));
#105802=CARTESIAN_POINT('Ctrl Pts',(5.44056914349405,31.2612950510678,53.9115427905758));
#105803=CARTESIAN_POINT('Ctrl Pts',(5.44103305721563,31.265824655015,53.9168138474957));
#105804=CARTESIAN_POINT('Ctrl Pts',(5.44190568106951,31.2742382215263,53.9267294790082));
#105805=CARTESIAN_POINT('Ctrl Pts',(5.44231381707429,31.2781300170575,53.9313670830248));
#105806=CARTESIAN_POINT('Ctrl Pts',(5.44328025748123,31.2872448883106,53.9423497094576));
#105807=CARTESIAN_POINT('Ctrl Pts',(5.44384004799494,31.2924463870803,53.9487122805771));
#105808=CARTESIAN_POINT('Ctrl Pts',(5.44572552945688,31.3097128574698,53.9701547695029));
#105809=CARTESIAN_POINT('Ctrl Pts',(5.44706478209705,31.3215621547659,53.9854053226042));
#105810=CARTESIAN_POINT('Ctrl Pts',(5.45451787189272,31.3853822330601,54.0705596400865));
#105811=CARTESIAN_POINT('Ctrl Pts',(5.46086903257902,31.4320703266873,54.144245665123));
#105812=CARTESIAN_POINT('Ctrl Pts',(5.47371934623301,31.5145970471616,54.3003183880402));
#105813=CARTESIAN_POINT('Ctrl Pts',(5.48019534484159,31.5499802940644,54.382648356998));
#105814=CARTESIAN_POINT('Ctrl Pts',(5.48939999497811,31.5918823640378,54.5068495656644));
#105815=CARTESIAN_POINT('Ctrl Pts',(5.49227859868952,31.6037012827997,54.5467566533317));
#105816=CARTESIAN_POINT('Ctrl Pts',(5.49620663499285,31.6180111360496,54.6026890801662));
#105817=CARTESIAN_POINT('Ctrl Pts',(5.49729641366454,31.6217808763644,54.6183682085881));
#105818=CARTESIAN_POINT('Ctrl Pts',(5.4990497623105,31.6275173367581,54.6438494887592));
#105819=CARTESIAN_POINT('Ctrl Pts',(5.49971778261907,31.6296244398868,54.6536186198092));
#105820=CARTESIAN_POINT('Ctrl Pts',(5.50111179637471,31.6338555992209,54.6741292353459));
#105821=CARTESIAN_POINT('Ctrl Pts',(5.50183719467011,31.6359619306563,54.6848739212149));
#105822=CARTESIAN_POINT('Ctrl Pts',(5.50327581299805,31.6399471560584,54.7063209682102));
#105823=CARTESIAN_POINT('Ctrl Pts',(5.50398904821198,31.6418275749237,54.7170224887864));
#105824=CARTESIAN_POINT('Ctrl Pts',(5.50566479121968,31.6460181664571,54.7423207939145));
#105825=CARTESIAN_POINT('Ctrl Pts',(5.50662450582426,31.6482391033695,54.756931577679));
#105826=CARTESIAN_POINT('Ctrl Pts',(5.51254171926052,31.6608060215381,54.8477199279824));
#105827=CARTESIAN_POINT('Ctrl Pts',(5.5173393256724,31.6660638176322,54.9245105544638));
#105828=CARTESIAN_POINT('Ctrl Pts',(5.52206895547911,31.6659994155302,55.0013955117896));
#105829=CARTESIAN_POINT('Ctrl Pts',(5.5220688677794,31.6659994167237,55.0013940861415));
#105830=CARTESIAN_POINT('Ctrl Pts',(5.53026528752143,31.6658879223103,55.1346352268217));
#105831=CARTESIAN_POINT('Ctrl Pts',(5.53818966990361,31.6497930141248,55.2673674871747));
#105832=CARTESIAN_POINT('Ctrl Pts',(5.54801370322328,31.6135136075547,55.4153259430768));
#105833=CARTESIAN_POINT('Ctrl Pts',(5.54926067071279,31.6086395532938,55.4338208298432));
#105834=CARTESIAN_POINT('Ctrl Pts',(5.55106550065771,31.6012261259723,55.4601064243879));
#105835=CARTESIAN_POINT('Ctrl Pts',(5.55160959587991,31.5989457914207,55.4679694193285));
#105836=CARTESIAN_POINT('Ctrl Pts',(5.55256157280845,31.5948796144338,55.4816135628806));
#105837=CARTESIAN_POINT('Ctrl Pts',(5.55296794664354,31.5931200835991,55.487402304405));
#105838=CARTESIAN_POINT('Ctrl Pts',(5.55384638297178,31.5892663307709,55.4998370543067));
#105839=CARTESIAN_POINT('Ctrl Pts',(5.55431898567185,31.5871619689062,55.506479447757));
#105840=CARTESIAN_POINT('Ctrl Pts',(5.55563602444341,31.581210309918,55.5248644069739));
#105841=CARTESIAN_POINT('Ctrl Pts',(5.55648528359108,31.5772740324032,55.5365773887186));
#105842=CARTESIAN_POINT('Ctrl Pts',(5.55800937646137,31.5700298200513,55.5573649041467));
#105843=CARTESIAN_POINT('Ctrl Pts',(5.55868169084271,31.5667729072001,55.5664555341626));
#105844=CARTESIAN_POINT('Ctrl Pts',(5.55935725065089,31.5634376826058,55.5755159533915));
#105845=CARTESIAN_POINT('',(5.3285190759848,31.667962423648,55.0005309979303));
#105846=CARTESIAN_POINT('Ctrl Pts',(5.36787289354565,31.5634376782623,55.5755159651912));
#105847=CARTESIAN_POINT('Ctrl Pts',(5.36380422315238,31.5844896318861,55.5183265569258));
#105848=CARTESIAN_POINT('Ctrl Pts',(5.3597355527591,31.6023823060254,55.4600275789832));
#105849=CARTESIAN_POINT('Ctrl Pts',(5.35566688236583,31.6170202081189,55.4010008061526));
#105850=CARTESIAN_POINT('Ctrl Pts',(5.35159065514323,31.6316852975039,55.341864401623));
#105851=CARTESIAN_POINT('Ctrl Pts',(5.34751442792064,31.6430834450864,55.2819980062784));
#105852=CARTESIAN_POINT('Ctrl Pts',(5.34343820069804,31.6511704975579,55.2217926689373));
#105853=CARTESIAN_POINT('Ctrl Pts',(5.34045646721565,31.6570861234078,55.1777528594847));
#105854=CARTESIAN_POINT('Ctrl Pts',(5.33747473373325,31.6612311284502,55.1335318674855));
#105855=CARTESIAN_POINT('Ctrl Pts',(5.33449300025085,31.6636058986979,55.0892827744734));
#105856=CARTESIAN_POINT('Ctrl Pts',(5.33250187903717,31.6651917062309,55.0597344233873));
#105857=CARTESIAN_POINT('Ctrl Pts',(5.33051075782348,31.6659903400224,55.0301434489476));
#105858=CARTESIAN_POINT('Ctrl Pts',(5.32851963660979,31.6659999129021,55.0005387116472));
#105859=CARTESIAN_POINT('Ctrl Pts',(5.32851891017001,31.6685428710302,55.0005287164616));
#105860=CARTESIAN_POINT('Ctrl Pts',(5.29346518325078,31.6663312333053,54.4785404025847));
#105861=CARTESIAN_POINT('Ctrl Pts',(5.22136636605202,31.1216350812794,53.4009406959792));
#105862=CARTESIAN_POINT('Ctrl Pts',(5.11222245857373,29.2866759464458,53.1646043774385));
#105863=CARTESIAN_POINT('Ctrl Pts',(5.00108718773517,28.0711228425453,54.60384194045));
#105864=CARTESIAN_POINT('Ctrl Pts',(4.88995191689661,28.6210166627157,56.4056718152503));
#105865=CARTESIAN_POINT('Ctrl Pts',(4.77886152907957,30.4323232756296,56.9207217847491));
#105866=CARTESIAN_POINT('Ctrl Pts',(4.70481623154204,31.3756950548499,56.0933234118257));
#105867=CARTESIAN_POINT('Ctrl Pts',(4.66781602428403,31.5660238537031,55.5764683070371));
#105868=CARTESIAN_POINT('Origin',(5.,30.,55.));
#105869=CARTESIAN_POINT('',(3.96712534830139,31.5634376767977,55.5755159691697));
#105870=CARTESIAN_POINT('',(4.16232242021249,31.5634376783907,55.5755159648424));
#105871=CARTESIAN_POINT('',(5.,31.5634376782623,55.5755159651912));
#105872=CARTESIAN_POINT('Ctrl Pts',(4.16232242021249,31.5634376783906,55.5755159648424));
#105873=CARTESIAN_POINT('Ctrl Pts',(4.16283813385309,31.5608103487311,55.5826533275469));
#105874=CARTESIAN_POINT('Ctrl Pts',(4.16335223587354,31.558134084724,55.5897728603756));
#105875=CARTESIAN_POINT('Ctrl Pts',(4.16467335641337,31.5511094127128,55.6080786290433));
#105876=CARTESIAN_POINT('Ctrl Pts',(4.16547790768569,31.5466887235781,55.6192366548532));
#105877=CARTESIAN_POINT('Ctrl Pts',(4.1669923035432,31.5380982316544,55.640253372118));
#105878=CARTESIAN_POINT('Ctrl Pts',(4.16770293852686,31.533953262297,55.6501214878334));
#105879=CARTESIAN_POINT('Ctrl Pts',(4.16931310081107,31.5243033729042,55.6724892180871));
#105880=CARTESIAN_POINT('Ctrl Pts',(4.17021056532531,31.5187392231987,55.6849625620775));
#105881=CARTESIAN_POINT('Ctrl Pts',(4.17255011010829,31.503751708711,55.7174798186707));
#105882=CARTESIAN_POINT('Ctrl Pts',(4.1739837145369,31.4940807657592,55.7374070995912));
#105883=CARTESIAN_POINT('Ctrl Pts',(4.18231018932071,31.4351168494857,55.8529785284581));
#105884=CARTESIAN_POINT('Ctrl Pts',(4.18888569401557,31.3770479724169,55.9438617677663));
#105885=CARTESIAN_POINT('Ctrl Pts',(4.19994051564531,31.2652800543895,56.0862847435557));
#105886=CARTESIAN_POINT('Ctrl Pts',(4.20441636953415,31.2161800806057,56.1409875951416));
#105887=CARTESIAN_POINT('Ctrl Pts',(4.21057609909438,31.1462864271764,56.209202703844));
#105888=CARTESIAN_POINT('Ctrl Pts',(4.21212154010923,31.1285698790687,56.225754322193));
#105889=CARTESIAN_POINT('Ctrl Pts',(4.21447114938599,31.1014974278408,56.2499620983466));
#105890=CARTESIAN_POINT('Ctrl Pts',(4.21525804145268,31.0924084289675,56.2579132069522));
#105891=CARTESIAN_POINT('Ctrl Pts',(4.21668095986283,31.0759529832811,56.27199568374));
#105892=CARTESIAN_POINT('Ctrl Pts',(4.2173145811575,31.0686184508188,56.2781636974812));
#105893=CARTESIAN_POINT('Ctrl Pts',(4.21837162823822,31.0563802200761,56.2882765359056));
#105894=CARTESIAN_POINT('Ctrl Pts',(4.21879252918983,31.0515065381851,56.2922575591554));
#105895=CARTESIAN_POINT('Ctrl Pts',(4.21962651068774,31.0418516552295,56.3000532835367));
#105896=CARTESIAN_POINT('Ctrl Pts',(4.22003948862542,31.0370718359291,56.3038694006139));
#105897=CARTESIAN_POINT('Ctrl Pts',(4.22096668045426,31.0263409611412,56.3123403960948));
#105898=CARTESIAN_POINT('Ctrl Pts',(4.22148183785593,31.0203790381539,56.3169812818609));
#105899=CARTESIAN_POINT('Ctrl Pts',(4.22330440495648,30.9992803693504,56.333175663116));
#105900=CARTESIAN_POINT('Ctrl Pts',(4.22462532274783,30.9839779421821,56.3445095531925));
#105901=CARTESIAN_POINT('Ctrl Pts',(4.23352540274032,30.8805947515072,56.4183711170017));
#105902=CARTESIAN_POINT('Ctrl Pts',(4.24146563824476,30.7868113674687,56.4724636038578));
#105903=CARTESIAN_POINT('Ctrl Pts',(4.25552570786375,30.6103777985771,56.5525292819306));
#105904=CARTESIAN_POINT('Ctrl Pts',(4.26166650033521,30.5296684763962,56.5818859575669));
#105905=CARTESIAN_POINT('Ctrl Pts',(4.26969064508329,30.418213223528,56.6129319967477));
#105906=CARTESIAN_POINT('Ctrl Pts',(4.27174274776361,30.3891662298304,56.6201857214714));
#105907=CARTESIAN_POINT('Ctrl Pts',(4.27470875501087,30.3464031821576,56.6296481191194));
#105908=CARTESIAN_POINT('Ctrl Pts',(4.2756420881411,30.3328313138985,56.6324740406557));
#105909=CARTESIAN_POINT('Ctrl Pts',(4.27728801600493,30.3086981128824,56.6371855492519));
#105910=CARTESIAN_POINT('Ctrl Pts',(4.27800273409458,30.2981510264143,56.6391391101038));
#105911=CARTESIAN_POINT('Ctrl Pts',(4.27950274847185,30.2758768179673,56.6430426918769));
#105912=CARTESIAN_POINT('Ctrl Pts',(4.28028726759658,30.264146169273,56.6449693369796));
#105913=CARTESIAN_POINT('Ctrl Pts',(4.28237414750275,30.2327339204768,56.649783800005));
#105914=CARTESIAN_POINT('Ctrl Pts',(4.28366935014773,30.2130191597457,56.6524450238862));
#105915=CARTESIAN_POINT('Ctrl Pts',(4.29126959631204,30.0961570901069,56.6660935004305));
#105916=CARTESIAN_POINT('Ctrl Pts',(4.29730806518718,29.998238368268,56.6688661167145));
#105917=CARTESIAN_POINT('Ctrl Pts',(4.30780756501426,29.8268872674085,56.6586276046746));
#105918=CARTESIAN_POINT('Ctrl Pts',(4.31228607655116,29.7535214093718,56.6493213728924));
#105919=CARTESIAN_POINT('Ctrl Pts',(4.3190359910938,29.6470136912755,56.6285444440918));
#105920=CARTESIAN_POINT('Ctrl Pts',(4.32121556005548,29.6132259851334,56.6208522154244));
#105921=CARTESIAN_POINT('Ctrl Pts',(4.32487027445901,29.5581082088159,56.6064824187245));
#105922=CARTESIAN_POINT('Ctrl Pts',(4.32631982815338,29.5366281545712,56.6004188617187));
#105923=CARTESIAN_POINT('Ctrl Pts',(4.3283654381972,29.5069621656253,56.5913972590653));
#105924=CARTESIAN_POINT('Ctrl Pts',(4.32894223598817,29.4986668103672,56.5888035017117));
#105925=CARTESIAN_POINT('Ctrl Pts',(4.32993182223119,29.4845613866193,56.5842716136195));
#105926=CARTESIAN_POINT('Ctrl Pts',(4.330342744475,29.4787408835318,56.582366089832));
#105927=CARTESIAN_POINT('Ctrl Pts',(4.3312086080303,29.4665561011166,56.5783024951669));
#105928=CARTESIAN_POINT('Ctrl Pts',(4.33166389204858,29.4601942478669,56.5761379715815));
#105929=CARTESIAN_POINT('Ctrl Pts',(4.33290709675902,29.4429397718215,56.5701506823678));
#105930=CARTESIAN_POINT('Ctrl Pts',(4.33369913897965,29.4320737424715,56.5662531757526));
#105931=CARTESIAN_POINT('Ctrl Pts',(4.33776675198897,29.3768689185041,56.5458019294094));
#105932=CARTESIAN_POINT('Ctrl Pts',(4.341127303514,29.3332132351503,56.5274784747139));
#105933=CARTESIAN_POINT('Ctrl Pts',(4.35178349107516,29.1991770843532,56.4643786347515));
#105934=CARTESIAN_POINT('Ctrl Pts',(4.35919710277712,29.112039175885,56.4132405648925));
#105935=CARTESIAN_POINT('Ctrl Pts',(4.37010694540066,28.9886320596101,56.324872385041));
#105936=CARTESIAN_POINT('Ctrl Pts',(4.37372443638217,28.9485865934312,56.2933223135008));
#105937=CARTESIAN_POINT('Ctrl Pts',(4.37970460196693,28.8837135110756,56.2372036460356));
#105938=CARTESIAN_POINT('Ctrl Pts',(4.38210068635491,28.8580989567626,56.2136023676452));
#105939=CARTESIAN_POINT('Ctrl Pts',(4.38545911184596,28.8227631202627,56.1789337568608));
#105940=CARTESIAN_POINT('Ctrl Pts',(4.38644891703554,28.8124210657607,56.1685152001527));
#105941=CARTESIAN_POINT('Ctrl Pts',(4.388159270635,28.7946818832143,56.1501659834469));
#105942=CARTESIAN_POINT('Ctrl Pts',(4.38888252313148,28.7872221238133,56.1422974151812));
#105943=CARTESIAN_POINT('Ctrl Pts',(4.3902755579086,28.7729379533952,56.1269327736997));
#105944=CARTESIAN_POINT('Ctrl Pts',(4.3909457243175,28.7661041192247,56.1194461602688));
#105945=CARTESIAN_POINT('Ctrl Pts',(4.39272679567373,28.7480482258861,56.0992992993217));
#105946=CARTESIAN_POINT('Ctrl Pts',(4.39383252817931,28.7369497667524,56.0865294919277));
#105947=CARTESIAN_POINT('Ctrl Pts',(4.39802779174855,28.6953009920132,56.0371079776084));
#105948=CARTESIAN_POINT('Ctrl Pts',(4.4010620449907,28.6661342113754,55.9993173451037));
#105949=CARTESIAN_POINT('Ctrl Pts',(4.41161197917421,28.5690732551866,55.8617219988201));
#105950=CARTESIAN_POINT('Ctrl Pts',(4.41882941762728,28.51043930039,55.7558600777894));
#105951=CARTESIAN_POINT('Ctrl Pts',(4.42879877015058,28.4480718271118,55.6072212452058));
#105952=CARTESIAN_POINT('Ctrl Pts',(4.43133266424086,28.4337602849347,55.5692902751069));
#105953=CARTESIAN_POINT('Ctrl Pts',(4.43551305552126,28.4129221615758,55.5073050537952));
#105954=CARTESIAN_POINT('Ctrl Pts',(4.43712370485106,28.4055267713564,55.4835591468595));
#105955=CARTESIAN_POINT('Ctrl Pts',(4.43935888308449,28.3961681492935,55.450956052531));
#105956=CARTESIAN_POINT('Ctrl Pts',(4.4399591414771,28.3937412754614,55.4422339508539));
#105957=CARTESIAN_POINT('Ctrl Pts',(4.44097651753335,28.3897752590063,55.4275167707363));
#105958=CARTESIAN_POINT('Ctrl Pts',(4.44139149864227,28.3881981742691,55.4215319429374));
#105959=CARTESIAN_POINT('Ctrl Pts',(4.44219695605938,28.3852161284823,55.409954026074));
#105960=CARTESIAN_POINT('Ctrl Pts',(4.44258714227081,28.383806805956,55.4043622289235));
#105961=CARTESIAN_POINT('Ctrl Pts',(4.4436638038028,28.3800137041978,55.3889756071637));
#105962=CARTESIAN_POINT('Ctrl Pts',(4.4443535275396,28.3776897991491,55.3791664820515));
#105963=CARTESIAN_POINT('Ctrl Pts',(4.44716620852365,28.3686339095457,55.3393337770422));
#105964=CARTESIAN_POINT('Ctrl Pts',(4.44932474667618,28.3626456894253,55.3091493350984));
#105965=CARTESIAN_POINT('Ctrl Pts',(4.45927229540769,28.3392059774649,55.1710675564686));
#105966=CARTESIAN_POINT('Ctrl Pts',(4.467326343228,28.331562481225,55.0617807114785));
#105967=CARTESIAN_POINT('Ctrl Pts',(4.47937924976396,28.3363187689734,54.8949095859488));
#105968=CARTESIAN_POINT('Ctrl Pts',(4.48349254313625,28.3409510942873,54.8374051946401));
#105969=CARTESIAN_POINT('Ctrl Pts',(4.49017424374649,28.353554219054,54.7426906207558));
#105970=CARTESIAN_POINT('Ctrl Pts',(4.49278745376725,28.3598325925154,54.7053084635835));
#105971=CARTESIAN_POINT('Ctrl Pts',(4.49638959945624,28.3703978054925,54.6533270880344));
#105972=CARTESIAN_POINT('Ctrl Pts',(4.49741173223651,28.3736170374182,54.6385253735316));
#105973=CARTESIAN_POINT('Ctrl Pts',(4.49915972496514,28.3795040031089,54.6131305293424));
#105974=CARTESIAN_POINT('Ctrl Pts',(4.49988863000191,28.3820748236023,54.602516168089));
#105975=CARTESIAN_POINT('Ctrl Pts',(4.50128028366652,28.3872056032259,54.5822072890153));
#105976=CARTESIAN_POINT('Ctrl Pts',(4.50194352740437,28.3897490614654,54.5725091369312));
#105977=CARTESIAN_POINT('Ctrl Pts',(4.50367825069259,28.3966591101202,54.5470983280366));
#105978=CARTESIAN_POINT('Ctrl Pts',(4.50474506063968,28.4011691949799,54.531425543359));
#105979=CARTESIAN_POINT('Ctrl Pts',(4.5085918602712,28.4183732362959,54.4747836548872));
#105980=CARTESIAN_POINT('Ctrl Pts',(4.5113281820529,28.4324183756111,54.4342405467219));
#105981=CARTESIAN_POINT('Ctrl Pts',(4.5212588097925,28.4898145665806,54.2871785699899));
#105982=CARTESIAN_POINT('Ctrl Pts',(4.52816741711857,28.5425886254987,54.184691960459));
#105983=CARTESIAN_POINT('Ctrl Pts',(4.53821358558086,28.6319761328701,54.047944923547));
#105984=CARTESIAN_POINT('Ctrl Pts',(4.54121714447261,28.6602066222092,54.0086114641782));
#105985=CARTESIAN_POINT('Ctrl Pts',(4.54550768627988,28.7018517190081,53.9556206002979));
#105986=CARTESIAN_POINT('Ctrl Pts',(4.54672932414605,28.7138510657058,53.9408785979324));
#105987=CARTESIAN_POINT('Ctrl Pts',(4.54889913437573,28.7353465380309,53.9153740232821));
#105988=CARTESIAN_POINT('Ctrl Pts',(4.54984087037637,28.7447346106193,53.9045226352961));
#105989=CARTESIAN_POINT('Ctrl Pts',(4.55127690722263,28.7591139242739,53.8883295638116));
#105990=CARTESIAN_POINT('Ctrl Pts',(4.55176402643552,28.7640023640918,53.8828969382277));
#105991=CARTESIAN_POINT('Ctrl Pts',(4.55265644671194,28.7729738973071,53.8730576623736));
#105992=CARTESIAN_POINT('Ctrl Pts',(4.55306088921458,28.7770452890834,53.8686407022879));
#105993=CARTESIAN_POINT('Ctrl Pts',(4.55398780908502,28.7863889142307,53.8586133858283));
#105994=CARTESIAN_POINT('Ctrl Pts',(4.55451139067789,28.7916761851476,53.8530175140435));
#105995=CARTESIAN_POINT('Ctrl Pts',(4.5561564815387,28.808323780469,53.8356411093869));
#105996=CARTESIAN_POINT('Ctrl Pts',(4.5572874050676,28.8198186419073,53.8239916027553));
#105997=CARTESIAN_POINT('Ctrl Pts',(4.56382731770072,28.88667630101,53.7582019232234));
#105998=CARTESIAN_POINT('Ctrl Pts',(4.56943929196914,28.9455842249568,53.707809143538));
#105999=CARTESIAN_POINT('Ctrl Pts',(4.5818394987114,29.0824801690206,53.6063136056006));
#106000=CARTESIAN_POINT('Ctrl Pts',(4.58861071367887,29.1616984072832,53.5572741027483));
#106001=CARTESIAN_POINT('Ctrl Pts',(4.59876767631203,29.2897341042386,53.4921397667207));
#106002=CARTESIAN_POINT('Ctrl Pts',(4.60228799551275,29.3358938115403,53.4712475593601));
#106003=CARTESIAN_POINT('Ctrl Pts',(4.60687963580261,29.3985088147929,53.4462801574541));
#106004=CARTESIAN_POINT('Ctrl Pts',(4.60801359176219,29.4141728045458,53.4403065917489));
#106005=CARTESIAN_POINT('Ctrl Pts',(4.60989403373137,29.4404767928441,53.4307275917063));
#106006=CARTESIAN_POINT('Ctrl Pts',(4.6106448093776,29.4510675902408,53.4269916303602));
#106007=CARTESIAN_POINT('Ctrl Pts',(4.61211679218591,29.4720033701583,53.4198436168642));
#106008=CARTESIAN_POINT('Ctrl Pts',(4.61283817238461,29.4823456260084,53.4164253743687));
#106009=CARTESIAN_POINT('Ctrl Pts',(4.61458430228583,29.5075739706603,53.4083606676544));
#106010=CARTESIAN_POINT('Ctrl Pts',(4.61560551709185,29.5224933943488,53.403821242057));
#106011=CARTESIAN_POINT('Ctrl Pts',(4.61910123917343,29.5741032202546,53.3889067002341));
#106012=CARTESIAN_POINT('Ctrl Pts',(4.62154214149323,29.6110861792708,53.3795815125446));
#106013=CARTESIAN_POINT('Ctrl Pts',(4.63224061350549,29.7766003060196,53.3438414151382));
#106014=CARTESIAN_POINT('Ctrl Pts',(4.64007488303997,29.9076578018976,53.3313953490188));
#106015=CARTESIAN_POINT('Ctrl Pts',(4.65076679503384,30.0806818671835,53.3354280125569));
#106016=CARTESIAN_POINT('Ctrl Pts',(4.65338125590551,30.1224905347588,53.3379816282574));
#106017=CARTESIAN_POINT('Ctrl Pts',(4.65767966430228,30.1894550353858,53.3446120923456));
#106018=CARTESIAN_POINT('Ctrl Pts',(4.65932520263956,30.2146921705761,53.3476957181483));
#106019=CARTESIAN_POINT('Ctrl Pts',(4.66160124143916,30.2488799056959,53.3526693989337));
#106020=CARTESIAN_POINT('Ctrl Pts',(4.66220631015672,30.2579014071987,53.3540576646166));
#106021=CARTESIAN_POINT('Ctrl Pts',(4.66322944520891,30.2730339393776,53.3565137820419));
#106022=CARTESIAN_POINT('Ctrl Pts',(4.66364531867461,30.2791514112839,53.3575417908756));
#106023=CARTESIAN_POINT('Ctrl Pts',(4.664505084181,30.2917263325982,53.3597272227256));
#106024=CARTESIAN_POINT('Ctrl Pts',(4.66494917406099,30.2981828767792,53.3608886537988));
#106025=CARTESIAN_POINT('Ctrl Pts',(4.66613054539578,30.3152610073173,53.3640649843135));
#106026=CARTESIAN_POINT('Ctrl Pts',(4.66687130551921,30.3258699218904,53.3661451542912));
#106027=CARTESIAN_POINT('Ctrl Pts',(4.67023045957177,30.3735652898927,53.3759801376771));
#106028=CARTESIAN_POINT('Ctrl Pts',(4.67290323259024,30.4103982062694,53.3848949387347));
#106029=CARTESIAN_POINT('Ctrl Pts',(4.68225111857294,30.5364039318481,53.4199808700875));
#106030=CARTESIAN_POINT('Ctrl Pts',(4.68907425729419,30.6236718886279,53.4523493183181));
#106031=CARTESIAN_POINT('Ctrl Pts',(4.70033061720281,30.7644370784319,53.518410230628));
#106032=CARTESIAN_POINT('Ctrl Pts',(4.70481090948164,30.8195504984283,53.5481699040625));
#106033=CARTESIAN_POINT('Ctrl Pts',(4.71200015265218,30.9069428990667,53.6019258126873));
#106034=CARTESIAN_POINT('Ctrl Pts',(4.71476341073818,30.9402585659378,53.6241107771918));
#106035=CARTESIAN_POINT('Ctrl Pts',(4.71853231031078,30.9852883320304,53.6564965206022));
#106036=CARTESIAN_POINT('Ctrl Pts',(4.71957540826618,30.9977053512757,53.66569165619));
#106037=CARTESIAN_POINT('Ctrl Pts',(4.72134801380106,31.0187213183329,53.6817119709214));
#106038=CARTESIAN_POINT('Ctrl Pts',(4.72208079173014,31.0273838158864,53.6884516948168));
#106039=CARTESIAN_POINT('Ctrl Pts',(4.72356049512437,31.0448207568923,53.7022970127118));
#106040=CARTESIAN_POINT('Ctrl Pts',(4.72430718551478,31.0535908417358,53.7094071881195));
#106041=CARTESIAN_POINT('Ctrl Pts',(4.72617308716575,31.0754271947817,53.7274815295486));
#106042=CARTESIAN_POINT('Ctrl Pts',(4.72728767434761,31.0883988252924,53.7385583877239));
#106043=CARTESIAN_POINT('Ctrl Pts',(4.73157557281459,31.1379806346987,53.7822320773032));
#106044=CARTESIAN_POINT('Ctrl Pts',(4.73469020703579,31.1733172842122,53.816240785988));
#106045=CARTESIAN_POINT('Ctrl Pts',(4.74610174471999,31.2989754937157,53.9483410807389));
#106046=CARTESIAN_POINT('Ctrl Pts',(4.75402222409377,31.3789162251238,54.0555896581443));
#106047=CARTESIAN_POINT('Ctrl Pts',(4.76431596960786,31.4609555750366,54.1986479453005));
#106048=CARTESIAN_POINT('Ctrl Pts',(4.76631264686039,31.4759040505895,54.2265251762463));
#106049=CARTESIAN_POINT('Ctrl Pts',(4.76969150464396,31.499408569833,54.2735237283791));
#106050=CARTESIAN_POINT('Ctrl Pts',(4.77105273055319,31.5084140153461,54.2924119183667));
#106051=CARTESIAN_POINT('Ctrl Pts',(4.77299371296883,31.5205649939473,54.319184321938));
#106052=CARTESIAN_POINT('Ctrl Pts',(4.77355671586167,31.5240100474343,54.326931462642));
#106053=CARTESIAN_POINT('Ctrl Pts',(4.77453024877183,31.5298279311554,54.3402882473822));
#106054=CARTESIAN_POINT('Ctrl Pts',(4.7749390581352,31.5322293897791,54.3458851848185));
#106055=CARTESIAN_POINT('Ctrl Pts',(4.77580936103992,31.5372528818615,54.3577726116578));
#106056=CARTESIAN_POINT('Ctrl Pts',(4.77627126775305,31.5398669901336,54.364065970673));
#106057=CARTESIAN_POINT('Ctrl Pts',(4.77755134910518,31.5469705624184,54.3814681570488));
#106058=CARTESIAN_POINT('Ctrl Pts',(4.77837404928239,31.5513788054187,54.3926093982103));
#106059=CARTESIAN_POINT('Ctrl Pts',(4.78299495638825,31.5752898401613,54.4550001942932));
#106060=CARTESIAN_POINT('Ctrl Pts',(4.78690699088596,31.5923714556087,54.5071361526437));
#106061=CARTESIAN_POINT('Ctrl Pts',(4.80157606841262,31.6460178008095,54.7030548853134));
#106062=CARTESIAN_POINT('Ctrl Pts',(4.81249360620914,31.6659176429962,54.8507206310839));
#106063=CARTESIAN_POINT('Ctrl Pts',(4.82499129265967,31.6660171922899,55.0306050153185));
#106064=CARTESIAN_POINT('Ctrl Pts',(4.82715546894155,31.6651397279086,55.0621278657168));
#106065=CARTESIAN_POINT('Ctrl Pts',(4.8302399093024,31.6625821967124,55.1075735692989));
#106066=CARTESIAN_POINT('Ctrl Pts',(4.83118219986254,31.6616204529125,55.1215282881547));
#106067=CARTESIAN_POINT('Ctrl Pts',(4.83284059726982,31.6596069630516,55.1462081081664));
#106068=CARTESIAN_POINT('Ctrl Pts',(4.83355889530278,31.6586267024974,55.1569380573531));
#106069=CARTESIAN_POINT('Ctrl Pts',(4.83505103387841,31.6563640485858,55.1793076766305));
#106070=CARTESIAN_POINT('Ctrl Pts',(4.83582424471099,31.6550628889343,55.1909448868516));
#106071=CARTESIAN_POINT('Ctrl Pts',(4.83784570684523,31.6513224308644,55.2214797094866));
#106072=CARTESIAN_POINT('Ctrl Pts',(4.8390875916497,31.6486814045713,55.2403512160899));
#106073=CARTESIAN_POINT('Ctrl Pts',(4.84549601455918,31.6332682194872,55.338222727906));
#106074=CARTESIAN_POINT('Ctrl Pts',(4.8504904266267,31.6151394352568,55.4162771223049));
#106075=CARTESIAN_POINT('Ctrl Pts',(4.85720460833585,31.5828485078716,55.5205726360054));
#106076=CARTESIAN_POINT('Ctrl Pts',(4.85898648174111,31.5735017790748,55.5481759854316));
#106077=CARTESIAN_POINT('Ctrl Pts',(4.86076605062571,31.563437683379,55.575515951291));
#106078=CARTESIAN_POINT('',(4.62852046321459,31.6642316419507,55.0011944504675));
#106079=CARTESIAN_POINT('Ctrl Pts',(4.66781602428403,31.5660238537031,55.5764683070371));
#106080=CARTESIAN_POINT('Ctrl Pts',(4.66777114126252,31.5662547316415,55.5758413370685));
#106081=CARTESIAN_POINT('Ctrl Pts',(4.65467262090604,31.6335127243303,55.3928239797156));
#106082=CARTESIAN_POINT('Ctrl Pts',(4.64157410054956,31.6655128862826,55.1968759451668));
#106083=CARTESIAN_POINT('Ctrl Pts',(4.62852046321459,31.6642316419507,55.0011944504675));
#106084=CARTESIAN_POINT('Ctrl Pts',(4.62750288773491,31.6659995270476,55.0012553395138));
#106085=CARTESIAN_POINT('Ctrl Pts',(4.62392608253606,31.6660375735313,54.9507626853719));
#106086=CARTESIAN_POINT('Ctrl Pts',(4.62040756350042,31.6637801570908,54.9002895119885));
#106087=CARTESIAN_POINT('Ctrl Pts',(4.61603290565177,31.6580121437699,54.8364900498272));
#106088=CARTESIAN_POINT('Ctrl Pts',(4.61511224377004,31.6566267453367,54.8230039035159));
#106089=CARTESIAN_POINT('Ctrl Pts',(4.6134917819864,31.653883489832,54.7991658327399));
#106090=CARTESIAN_POINT('Ctrl Pts',(4.61278992858583,31.6525926679084,54.7888070946701));
#106091=CARTESIAN_POINT('Ctrl Pts',(4.61140045450403,31.6498325545355,54.7682350462989));
#106092=CARTESIAN_POINT('Ctrl Pts',(4.61071279398538,31.6483655722525,54.7580219013712));
#106093=CARTESIAN_POINT('Ctrl Pts',(4.60924923531365,31.6450271562619,54.7362208940149));
#106094=CARTESIAN_POINT('Ctrl Pts',(4.6084742537118,31.6431279418675,54.7246378019317));
#106095=CARTESIAN_POINT('Ctrl Pts',(4.60644175916033,31.6378002899008,54.6941655218651));
#106096=CARTESIAN_POINT('Ctrl Pts',(4.60519074714566,31.6341674474727,54.6753135038796));
#106097=CARTESIAN_POINT('Ctrl Pts',(4.59879713054056,31.6137835864916,54.5785663258725));
#106098=CARTESIAN_POINT('Ctrl Pts',(4.59382466559208,31.5917854667709,54.5018783785038));
#106099=CARTESIAN_POINT('Ctrl Pts',(4.58406222880871,31.5371924023319,54.3528173416392));
#106100=CARTESIAN_POINT('Ctrl Pts',(4.57928269727814,31.5047557353687,54.280614389318));
#106101=CARTESIAN_POINT('Ctrl Pts',(4.57074277749213,31.4391902586471,54.1586829738244));
#106102=CARTESIAN_POINT('Ctrl Pts',(4.56702916256826,31.4082904411514,54.107924055398));
#106103=CARTESIAN_POINT('Ctrl Pts',(4.56219410992613,31.3662473081641,54.0465059381401));
#106104=CARTESIAN_POINT('Ctrl Pts',(4.56120712878124,31.3575759560073,54.0341997525652));
#106105=CARTESIAN_POINT('Ctrl Pts',(4.55971602666297,31.3443679615188,54.0159846351031));
#106106=CARTESIAN_POINT('Ctrl Pts',(4.55921993762499,31.3399562435075,54.0099854978386));
#106107=CARTESIAN_POINT('Ctrl Pts',(4.55831907440673,31.3319171794065,53.9992059975433));
#106108=CARTESIAN_POINT('Ctrl Pts',(4.55791526509758,31.3283040251912,53.9944153831105));
#106109=CARTESIAN_POINT('Ctrl Pts',(4.55699999935006,31.320093024641,53.9836500399698));
#106110=CARTESIAN_POINT('Ctrl Pts',(4.55648755692153,31.3154804915835,53.9776869825341));
#106111=CARTESIAN_POINT('Ctrl Pts',(4.55491153162744,31.3012432123387,53.9595369974291));
#106112=CARTESIAN_POINT('Ctrl Pts',(4.55383958501061,31.2914887151701,53.947453557862));
#106113=CARTESIAN_POINT('Ctrl Pts',(4.54555837142807,31.215492287527,53.8559595870152));
#106114=CARTESIAN_POINT('Ctrl Pts',(4.53798250483419,31.1421599526536,53.7827419212522));
#106115=CARTESIAN_POINT('Ctrl Pts',(4.52242343743735,30.9773435228809,53.6462697939842));
#106116=CARTESIAN_POINT('Ctrl Pts',(4.51449384916197,30.8853404804869,53.5843848509661));
#106117=CARTESIAN_POINT('Ctrl Pts',(4.5054639809538,30.7693265223364,53.5221179080577));
#106118=CARTESIAN_POINT('Ctrl Pts',(4.50403310547343,30.7505984152836,53.5125186169315));
#106119=CARTESIAN_POINT('Ctrl Pts',(4.50179705062597,30.7207967755109,53.4979497003995));
#106120=CARTESIAN_POINT('Ctrl Pts',(4.50098367920247,30.7098427638429,53.4927421062698));
#106121=CARTESIAN_POINT('Ctrl Pts',(4.49946192721021,30.6891387653193,53.4831750933216));
#106122=CARTESIAN_POINT('Ctrl Pts',(4.49875265578805,30.6794018941504,53.478788932895));
#106123=CARTESIAN_POINT('Ctrl Pts',(4.49715781781391,30.6573155951919,53.4690940996785));
#106124=CARTESIAN_POINT('Ctrl Pts',(4.49627416406383,30.644942645305,53.4638406107462));
#106125=CARTESIAN_POINT('Ctrl Pts',(4.49399584933292,30.6127020940637,53.4506096542735));
#106126=CARTESIAN_POINT('Ctrl Pts',(4.49260893958195,30.5927415276213,53.4428642167012));
#106127=CARTESIAN_POINT('Ctrl Pts',(4.48326972852482,30.4562294387731,53.3928980497413));
#106128=CARTESIAN_POINT('Ctrl Pts',(4.47575849343676,30.3354299973551,53.3634144047361));
#106129=CARTESIAN_POINT('Ctrl Pts',(4.46282136053429,30.1255626529175,53.3364293276458));
#106130=CARTESIAN_POINT('Ctrl Pts',(4.45743786002316,30.0379224568773,53.3321297403098));
#106131=CARTESIAN_POINT('Ctrl Pts',(4.45081904007182,29.9362743243497,53.3351595481324));
#106132=CARTESIAN_POINT('Ctrl Pts',(4.44989354294296,29.9221912371156,53.3357582939663));
#106133=CARTESIAN_POINT('Ctrl Pts',(4.44847743663394,29.900873134756,53.3369358060815));
#106134=CARTESIAN_POINT('Ctrl Pts',(4.44799371586475,29.8936311105201,53.3373832964499));
#106135=CARTESIAN_POINT('Ctrl Pts',(4.44710458076348,29.8803977120386,53.3382878116181));
#106136=CARTESIAN_POINT('Ctrl Pts',(4.44669998600041,29.874405586259,53.3387299605948));
#106137=CARTESIAN_POINT('Ctrl Pts',(4.44576889385398,29.8606832045598,53.3398171782372));
#106138=CARTESIAN_POINT('Ctrl Pts',(4.44524124784759,29.8529549944233,53.3404838260823));
#106139=CARTESIAN_POINT('Ctrl Pts',(4.44360983622891,29.8291994143394,53.3427002568481));
#106140=CARTESIAN_POINT('Ctrl Pts',(4.44249710017374,29.8131901648763,53.3444284018405));
#106141=CARTESIAN_POINT('Ctrl Pts',(4.43541681984961,29.7123855200508,53.3567905848384));
#106142=CARTESIAN_POINT('Ctrl Pts',(4.42920132067106,29.6284956954561,53.3737032468747));
#106143=CARTESIAN_POINT('Ctrl Pts',(4.41663266173739,29.4623614360909,53.420725604156));
#106144=CARTESIAN_POINT('Ctrl Pts',(4.41030008263312,29.3804277776422,53.4510339207596));
#106145=CARTESIAN_POINT('Ctrl Pts',(4.40068671476945,29.256833463031,53.50813800948));
#106146=CARTESIAN_POINT('Ctrl Pts',(4.39728956770065,29.2133503121205,53.5306015484871));
#106147=CARTESIAN_POINT('Ctrl Pts',(4.39283004687733,29.1565437583529,53.5631937910363));
#106148=CARTESIAN_POINT('Ctrl Pts',(4.39170954924573,29.1422960154746,53.5716532553097));
#106149=CARTESIAN_POINT('Ctrl Pts',(4.38984533407847,29.1186424326813,53.5861789316156));
#106150=CARTESIAN_POINT('Ctrl Pts',(4.38909748101786,29.1091675090358,53.5921297437398));
#106151=CARTESIAN_POINT('Ctrl Pts',(4.38762676660182,29.0905661171268,53.6040754962339));
#106152=CARTESIAN_POINT('Ctrl Pts',(4.38690377456692,29.0814372252639,53.6100655964997));
#106153=CARTESIAN_POINT('Ctrl Pts',(4.38531048022611,29.0613587925301,53.6235246689107));
#106154=CARTESIAN_POINT('Ctrl Pts',(4.38444179719749,29.0504380916647,53.6310354816876));
#106155=CARTESIAN_POINT('Ctrl Pts',(4.38142986492495,29.0126826937431,53.657671304738));
#106156=CARTESIAN_POINT('Ctrl Pts',(4.37931187430215,28.9863256488539,53.6774621630467));
#106157=CARTESIAN_POINT('Ctrl Pts',(4.36929390308862,28.863059580359,53.7758711637061));
#106158=CARTESIAN_POINT('Ctrl Pts',(4.36179479820369,28.7746031192559,53.8644256573008));
#106159=CARTESIAN_POINT('Ctrl Pts',(4.35099642222793,28.6650308349105,54.0019903543665));
#106160=CARTESIAN_POINT('Ctrl Pts',(4.34783306114754,28.6350588214409,54.0433910007479));
#106161=CARTESIAN_POINT('Ctrl Pts',(4.34333586572791,28.596258330771,54.1025305024615));
#106162=CARTESIAN_POINT('Ctrl Pts',(4.34207422642964,28.5857704738276,54.1191498709518));
#106163=CARTESIAN_POINT('Ctrl Pts',(4.33984026983917,28.5679468775651,54.1485327745743));
#106164=CARTESIAN_POINT('Ctrl Pts',(4.33887493339831,28.5604816227675,54.1612155302659));
#106165=CARTESIAN_POINT('Ctrl Pts',(4.33741019689928,28.5495265170467,54.18040428022));
#106166=CARTESIAN_POINT('Ctrl Pts',(4.3369184169902,28.5459100776486,54.1868376784591));
#106167=CARTESIAN_POINT('Ctrl Pts',(4.33602173067697,28.5394302446526,54.1985463110036));
#106168=CARTESIAN_POINT('Ctrl Pts',(4.33561773895219,28.536552454398,54.2038132732765));
#106169=CARTESIAN_POINT('Ctrl Pts',(4.33469736098629,28.5300902719843,54.2157938348754));
#106170=CARTESIAN_POINT('Ctrl Pts',(4.33417993517464,28.526523402679,54.2225164764516));
#106171=CARTESIAN_POINT('Ctrl Pts',(4.3325730084847,28.5156453803827,54.2433625128973));
#106172=CARTESIAN_POINT('Ctrl Pts',(4.33147468020476,28.5084905503534,54.2575658687918));
#106173=CARTESIAN_POINT('Ctrl Pts',(4.32340649147518,28.4578768202241,54.3617265292075));
#106174=CARTESIAN_POINT('Ctrl Pts',(4.31609683987139,28.4223880497606,54.455321923888));
#106175=CARTESIAN_POINT('Ctrl Pts',(4.30052825652344,28.3647719229351,54.6614532026222));
#106176=CARTESIAN_POINT('Ctrl Pts',(4.29233432248276,28.3454187492353,54.774268640264));
#106177=CARTESIAN_POINT('Ctrl Pts',(4.28308877247625,28.3363668961022,54.9088448001041));
#106178=CARTESIAN_POINT('Ctrl Pts',(4.28168188633582,28.3353627898426,54.9295202129776));
#106179=CARTESIAN_POINT('Ctrl Pts',(4.27947451735669,28.3343838914722,54.962259914996));
#106180=CARTESIAN_POINT('Ctrl Pts',(4.27866619208725,28.3341543979604,54.9743138480727));
#106181=CARTESIAN_POINT('Ctrl Pts',(4.27714884811469,28.3339683038534,54.9970585883093));
#106182=CARTESIAN_POINT('Ctrl Pts',(4.27643899431975,28.3339837232162,55.0077484873008));
#106183=CARTESIAN_POINT('Ctrl Pts',(4.27483616983301,28.334252052041,55.0319927317074));
#106184=CARTESIAN_POINT('Ctrl Pts',(4.27394519241046,28.33456751408,55.0455457341369));
#106185=CARTESIAN_POINT('Ctrl Pts',(4.27163420195255,28.335821732058,55.0808830319278));
#106186=CARTESIAN_POINT('Ctrl Pts',(4.27022232481575,28.3370227829073,55.1026558232917));
#106187=CARTESIAN_POINT('Ctrl Pts',(4.25945157065493,28.3495484657367,55.2699355554147));
#106188=CARTESIAN_POINT('Ctrl Pts',(4.25073123579656,28.3795199573312,55.4134026828032));
#106189=CARTESIAN_POINT('Ctrl Pts',(4.23888477965579,28.4431716993595,55.5949791414188));
#106190=CARTESIAN_POINT('Ctrl Pts',(4.23599642303174,28.4603676042876,55.638158313174));
#106191=CARTESIAN_POINT('Ctrl Pts',(4.23130081349718,28.4904696140823,55.70541887716));
#106192=CARTESIAN_POINT('Ctrl Pts',(4.22954130058974,28.5022025123248,55.7300001794339));
#106193=CARTESIAN_POINT('Ctrl Pts',(4.22713233276354,28.5187690120197,55.7626259570023));
#106194=CARTESIAN_POINT('Ctrl Pts',(4.22651229393094,28.5230763965082,55.7709346596035));
#106195=CARTESIAN_POINT('Ctrl Pts',(4.22547122306904,28.5303753668707,55.7847282756772));
#106196=CARTESIAN_POINT('Ctrl Pts',(4.22505256213403,28.5333283000348,55.7902336056585));
#106197=CARTESIAN_POINT('Ctrl Pts',(4.22419505914448,28.5394105582043,55.801421591165));
#106198=CARTESIAN_POINT('Ctrl Pts',(4.22375608795675,28.5425422181252,55.8071027782687));
#106199=CARTESIAN_POINT('Ctrl Pts',(4.222602492518,28.5508210851472,55.8219162767302));
#106200=CARTESIAN_POINT('Ctrl Pts',(4.22188466310825,28.5560213541198,55.8310183808447));
#106201=CARTESIAN_POINT('Ctrl Pts',(4.21879032494597,28.5786592927831,55.8697877979095));
#106202=CARTESIAN_POINT('Ctrl Pts',(4.21636909449108,28.5969268202498,55.8989580020446));
#106203=CARTESIAN_POINT('Ctrl Pts',(4.20627824297224,28.6757617551641,56.0165821637736));
#106204=CARTESIAN_POINT('Ctrl Pts',(4.19838199190649,28.7438938263939,56.0996561404667));
#106205=CARTESIAN_POINT('Ctrl Pts',(4.18659668922015,28.8591809156105,56.2154194875824));
#106206=CARTESIAN_POINT('Ctrl Pts',(4.18259195852655,28.9008189178275,56.2532017804535));
#106207=CARTESIAN_POINT('Ctrl Pts',(4.17688945201212,28.9639432052222,56.3049090825147));
#106208=CARTESIAN_POINT('Ctrl Pts',(4.1751303495383,28.9839626288232,56.3205565398546));
#106209=CARTESIAN_POINT('Ctrl Pts',(4.17196686941235,29.0209624903413,56.3481363969568));
#106210=CARTESIAN_POINT('Ctrl Pts',(4.17055693786601,29.0378225686264,56.3602208820861));
#106211=CARTESIAN_POINT('Ctrl Pts',(4.16834592575701,29.0648401846509,56.3788319976896));
#106212=CARTESIAN_POINT('Ctrl Pts',(4.16753695872247,29.0748500411115,56.385568159611));
#106213=CARTESIAN_POINT('Ctrl Pts',(4.16601906048028,29.0938638582634,56.3980656371764));
#106214=CARTESIAN_POINT('Ctrl Pts',(4.1653092870467,29.1028517526657,56.4038501574643));
#106215=CARTESIAN_POINT('Ctrl Pts',(4.16370750953633,29.123351374253,56.4167662272335));
#106216=CARTESIAN_POINT('Ctrl Pts',(4.16281748822097,29.1348957235678,56.4238447824599));
#106217=CARTESIAN_POINT('Ctrl Pts',(4.16051077259799,29.1652056817379,56.4419249514623));
#106218=CARTESIAN_POINT('Ctrl Pts',(4.15910216336266,29.1841030626167,56.4527014066301));
#106219=CARTESIAN_POINT('Ctrl Pts',(4.14831717175063,29.3316054957921,56.5330298376717));
#106220=CARTESIAN_POINT('Ctrl Pts',(4.13958228448592,29.4686438069036,56.5857471895375));
#106221=CARTESIAN_POINT('Ctrl Pts',(4.12772570974535,29.6558758464832,56.6307307658874));
#106222=CARTESIAN_POINT('Ctrl Pts',(4.12484394740102,29.7013720150023,56.6396722244861));
#106223=CARTESIAN_POINT('Ctrl Pts',(4.12015783416611,29.7740565259787,56.6508316127432));
#106224=CARTESIAN_POINT('Ctrl Pts',(4.11840098765949,29.8010299262758,56.6542993004619));
#106225=CARTESIAN_POINT('Ctrl Pts',(4.11599512508008,29.8373779317457,56.6580704309633));
#106226=CARTESIAN_POINT('Ctrl Pts',(4.11537542860821,29.8466893566352,56.6589573013335));
#106227=CARTESIAN_POINT('Ctrl Pts',(4.11433477180292,29.8622303635508,56.6603055571012));
#106228=CARTESIAN_POINT('Ctrl Pts',(4.1139161784708,29.8684561419605,56.6608104127609));
#106229=CARTESIAN_POINT('Ctrl Pts',(4.11305863934986,29.8811548986549,56.6617683188711));
#106230=CARTESIAN_POINT('Ctrl Pts',(4.11261956294185,29.8876279111249,56.6622185818125));
#106231=CARTESIAN_POINT('Ctrl Pts',(4.11146538821747,29.9045718950883,56.6632977827065));
#106232=CARTESIAN_POINT('Ctrl Pts',(4.11074707908674,29.9150462725682,56.6638656457732));
#106233=CARTESIAN_POINT('Ctrl Pts',(4.10764767817032,29.9599688341473,56.6658758240063));
#106234=CARTESIAN_POINT('Ctrl Pts',(4.10522169057012,29.9944495579494,56.6663473718565));
#106235=CARTESIAN_POINT('Ctrl Pts',(4.09512817233281,30.1360569264897,56.6638890916981));
#106236=CARTESIAN_POINT('Ctrl Pts',(4.08723467045153,30.242765518535,56.6516971358001));
#106237=CARTESIAN_POINT('Ctrl Pts',(4.07545411476279,30.4024865823204,56.6176261236222));
#106238=CARTESIAN_POINT('Ctrl Pts',(4.07145135730114,30.4567855538752,56.6031399568175));
#106239=CARTESIAN_POINT('Ctrl Pts',(4.06492459590977,30.5456914129049,56.5745357146169));
#106240=CARTESIAN_POINT('Ctrl Pts',(4.06235846771108,30.5807393178021,56.5619488017357));
#106241=CARTESIAN_POINT('Ctrl Pts',(4.05880911804395,30.6293200576447,56.5426401485739));
#106242=CARTESIAN_POINT('Ctrl Pts',(4.05779398319049,30.6432260278243,56.5368938368909));
#106243=CARTESIAN_POINT('Ctrl Pts',(4.05605435132113,30.6670695858688,56.5266607312253));
#106244=CARTESIAN_POINT('Ctrl Pts',(4.05532688203491,30.6770442841548,56.5222634028574));
#106245=CARTESIAN_POINT('Ctrl Pts',(4.05393555121215,30.6961250642125,56.5136270227263));
#106246=CARTESIAN_POINT('Ctrl Pts',(4.05327121696123,30.7052373440137,56.5094029167318));
#106247=CARTESIAN_POINT('Ctrl Pts',(4.05152820542748,30.729144118317,56.4980568855487));
#106248=CARTESIAN_POINT('Ctrl Pts',(4.05045428949456,30.7438727333469,56.4907980968879));
#106249=CARTESIAN_POINT('Ctrl Pts',(4.04654723815605,30.7974153589723,56.4634192523556));
#106250=CARTESIAN_POINT('Ctrl Pts',(4.04375966293906,30.8355423989993,56.4419904879222));
#106251=CARTESIAN_POINT('Ctrl Pts',(4.03383220710234,30.9700645711245,56.3592548342384));
#106252=CARTESIAN_POINT('Ctrl Pts',(4.02696948416452,31.0609325213869,56.2895820159823));
#106253=CARTESIAN_POINT('Ctrl Pts',(4.01698214615392,31.1789897627733,56.1780750529946));
#106254=CARTESIAN_POINT('Ctrl Pts',(4.0139911860069,31.2125646951688,56.1434876089795));
#106255=CARTESIAN_POINT('Ctrl Pts',(4.00914824256803,31.2631306896512,56.0866621582956));
#106256=CARTESIAN_POINT('Ctrl Pts',(4.00734773464094,31.2811428128532,56.0653669145895));
#106257=CARTESIAN_POINT('Ctrl Pts',(4.00489106618436,31.3045238026577,56.0362734911865));
#106258=CARTESIAN_POINT('Ctrl Pts',(4.00426582520555,31.3103740416305,56.0288658614668));
#106259=CARTESIAN_POINT('Ctrl Pts',(4.00321845409541,31.3200009941074,56.016460824661));
#106260=CARTESIAN_POINT('Ctrl Pts',(4.00279875747084,31.3238131480955,56.0114909684755));
#106261=CARTESIAN_POINT('Ctrl Pts',(4.00194175962675,31.3315029012076,56.0013480014726));
#106262=CARTESIAN_POINT('Ctrl Pts',(4.0015043515384,31.3353785602897,55.9961736259792));
#106263=CARTESIAN_POINT('Ctrl Pts',(4.00035936345872,31.3453987905753,55.9826321079127));
#106264=CARTESIAN_POINT('Ctrl Pts',(3.99964866193045,31.3514953338419,55.9742300108421));
#106265=CARTESIAN_POINT('Ctrl Pts',(3.99662839559915,31.3769039654457,55.9385150075283));
#106266=CARTESIAN_POINT('Ctrl Pts',(3.99427661623603,31.395468372566,55.9106825001384));
#106267=CARTESIAN_POINT('Ctrl Pts',(3.98422441648481,31.4702356091155,55.790929419651));
#106268=CARTESIAN_POINT('Ctrl Pts',(3.97628760402876,31.5182909273427,55.6942296257175));
#106269=CARTESIAN_POINT('Ctrl Pts',(3.96805081481214,31.55896341148,55.5875630831849));
#106270=CARTESIAN_POINT('Ctrl Pts',(3.96758775221476,31.5612180395373,55.5815458010209));
#106271=CARTESIAN_POINT('Ctrl Pts',(3.96712534830139,31.5634376767977,55.5755159691697));
#106272=CARTESIAN_POINT('Origin',(5.,30.,55.));
#106273=CARTESIAN_POINT('',(3.26653908718979,31.5634376777881,55.5755159664792));
#106274=CARTESIAN_POINT('',(3.46016014030872,31.5634377287949,55.5755158279149));
#106275=CARTESIAN_POINT('',(5.,31.5634376782623,55.5755159651912));
#106276=CARTESIAN_POINT('',(4.12032061737785,31.6659997582528,54.999102502649));
#106277=CARTESIAN_POINT('Ctrl Pts',(3.46016014030872,31.5634377287949,55.5755158279149));
#106278=CARTESIAN_POINT('Ctrl Pts',(3.46533508665415,31.5387976594635,55.6424526733747));
#106279=CARTESIAN_POINT('Ctrl Pts',(3.47055209472285,31.5098738865113,55.7077663328729));
#106280=CARTESIAN_POINT('Ctrl Pts',(3.48167284141879,31.43849959412,55.8444735671295));
#106281=CARTESIAN_POINT('Ctrl Pts',(3.48753195065647,31.3947381704652,55.914945819601));
#106282=CARTESIAN_POINT('Ctrl Pts',(3.49454426464309,31.3343484856101,55.9977248299006));
#106283=CARTESIAN_POINT('Ctrl Pts',(3.49587590576348,31.3225092538315,56.0133657029079));
#106284=CARTESIAN_POINT('Ctrl Pts',(3.49799330691346,31.3030918251546,56.0380980711248));
#106285=CARTESIAN_POINT('Ctrl Pts',(3.49878585113611,31.2956885016182,56.0473238416662));
#106286=CARTESIAN_POINT('Ctrl Pts',(3.5002905205491,31.2813766440671,56.0647747403505));
#106287=CARTESIAN_POINT('Ctrl Pts',(3.50100329806649,31.2744856282455,56.0730133942589));
#106288=CARTESIAN_POINT('Ctrl Pts',(3.50263623362298,31.2584449385539,56.0918185194894));
#106289=CARTESIAN_POINT('Ctrl Pts',(3.50355410369704,31.249240921583,56.1023377351952));
#106290=CARTESIAN_POINT('Ctrl Pts',(3.50646362457264,31.2194779302772,56.1355020755035));
#106291=CARTESIAN_POINT('Ctrl Pts',(3.50843464210021,31.1984266293029,56.1576982284507));
#106292=CARTESIAN_POINT('Ctrl Pts',(3.51308992617994,31.1467094549826,56.2093045248518));
#106293=CARTESIAN_POINT('Ctrl Pts',(3.51575166701474,31.1155062043054,56.2381463142057));
#106294=CARTESIAN_POINT('Ctrl Pts',(3.52295599516635,31.0272205083045,56.3137005683529));
#106295=CARTESIAN_POINT('Ctrl Pts',(3.52743088156339,30.9680867638358,56.3578658035549));
#106296=CARTESIAN_POINT('Ctrl Pts',(3.53278087428709,30.8947040643059,56.4054355367462));
#106297=CARTESIAN_POINT('Ctrl Pts',(3.53362175135898,30.8830943621304,56.4127592691422));
#106298=CARTESIAN_POINT('Ctrl Pts',(3.53899015858684,30.8085994909791,56.4584756820157));
#106299=CARTESIAN_POINT('Ctrl Pts',(3.54357009394533,30.7433237598665,56.4927998824545));
#106300=CARTESIAN_POINT('Ctrl Pts',(3.54918367207347,30.6647779423351,56.5276704688808));
#106301=CARTESIAN_POINT('Ctrl Pts',(3.54999205075681,30.6535008555704,56.5325284284833));
#106302=CARTESIAN_POINT('Ctrl Pts',(3.55126925030795,30.6357581397266,56.5399402250574));
#106303=CARTESIAN_POINT('Ctrl Pts',(3.55173319374091,30.6293282080846,56.5425791101632));
#106304=CARTESIAN_POINT('Ctrl Pts',(3.55260584006009,30.6172668219132,56.5474412188377));
#106305=CARTESIAN_POINT('Ctrl Pts',(3.55301396843795,30.6116395184423,56.5496740786344));
#106306=CARTESIAN_POINT('Ctrl Pts',(3.55398034532309,30.5983457314973,56.5548652391269));
#106307=CARTESIAN_POINT('Ctrl Pts',(3.55454007935012,30.5906693931238,56.557797543712));
#106308=CARTESIAN_POINT('Ctrl Pts',(3.55642516703632,30.5648850221224,56.5674290069065));
#106309=CARTESIAN_POINT('Ctrl Pts',(3.55776407497309,30.5466830282125,56.5738698698242));
#106310=CARTESIAN_POINT('Ctrl Pts',(3.56109732175184,30.5015474379016,56.5889639165221));
#106311=CARTESIAN_POINT('Ctrl Pts',(3.56310625303131,30.4744979832408,56.5972500254272));
#106312=CARTESIAN_POINT('Ctrl Pts',(3.5723157071,30.3506897651624,56.6317540310309));
#106313=CARTESIAN_POINT('Ctrl Pts',(3.57968869467792,30.2518961893848,56.6498949366246));
#106314=CARTESIAN_POINT('Ctrl Pts',(3.5928627206271,30.0699400603664,56.6665732474566));
#106315=CARTESIAN_POINT('Ctrl Pts',(3.59869577729024,29.9873546364215,56.6679933394905));
#106316=CARTESIAN_POINT('Ctrl Pts',(3.60568294097849,29.8854206476869,56.6621708311039));
#106317=CARTESIAN_POINT('Ctrl Pts',(3.60701384290961,29.8658695534124,56.6607074938125));
#106318=CARTESIAN_POINT('Ctrl Pts',(3.60913035768893,29.8345724024207,56.6578086640202));
#106319=CARTESIAN_POINT('Ctrl Pts',(3.60992274464965,29.8228084032032,56.6565925893377));
#106320=CARTESIAN_POINT('Ctrl Pts',(3.61142729231794,29.8003866142317,56.6540332101452));
#106321=CARTESIAN_POINT('Ctrl Pts',(3.61214010350258,29.7897269682926,56.6527119003));
#106322=CARTESIAN_POINT('Ctrl Pts',(3.61377336537157,29.7652230562985,56.6494336167819));
#106323=CARTESIAN_POINT('Ctrl Pts',(3.61469152488574,29.7513890330395,56.6474052556401));
#106324=CARTESIAN_POINT('Ctrl Pts',(3.61760300867053,29.7073538613577,56.6403814234232));
#106325=CARTESIAN_POINT('Ctrl Pts',(3.61957565908218,29.6772631290063,56.6347275239019));
#106326=CARTESIAN_POINT('Ctrl Pts',(3.62423563051579,29.605784004053,56.6192461142565));
#106327=CARTESIAN_POINT('Ctrl Pts',(3.62690036120363,29.564582278122,56.6086565878944));
#106328=CARTESIAN_POINT('Ctrl Pts',(3.63410626988643,29.4531986702559,56.5754353907735));
#106329=CARTESIAN_POINT('Ctrl Pts',(3.63857994163612,29.38404296712,56.5497050243978));
#106330=CARTESIAN_POINT('Ctrl Pts',(3.64394270453551,29.3040926545885,56.513758119578));
#106331=CARTESIAN_POINT('Ctrl Pts',(3.64479748866411,29.2914395285092,56.5078768949202));
#106332=CARTESIAN_POINT('Ctrl Pts',(3.65016234028007,29.2127088940172,56.4700727628586));
#106333=CARTESIAN_POINT('Ctrl Pts',(3.65472493308989,29.1487349860253,56.4339757202959));
#106334=CARTESIAN_POINT('Ctrl Pts',(3.66031925577431,29.0770852193275,56.3870598598369));
#106335=CARTESIAN_POINT('Ctrl Pts',(3.661127563792,29.0668884777912,56.3802208564271));
#106336=CARTESIAN_POINT('Ctrl Pts',(3.66240467570083,29.0510396165593,56.3693350562313));
#106337=CARTESIAN_POINT('Ctrl Pts',(3.66286860323989,29.0453354170697,56.3653643599008));
#106338=CARTESIAN_POINT('Ctrl Pts',(3.66374123754035,29.0347090494322,56.357868195594));
#106339=CARTESIAN_POINT('Ctrl Pts',(3.66414936999714,29.029781038941,56.3543514384286));
#106340=CARTESIAN_POINT('Ctrl Pts',(3.66511578085771,29.018209260603,56.3459979485143));
#106341=CARTESIAN_POINT('Ctrl Pts',(3.665675545098,29.0115819916774,56.3411388321555));
#106342=CARTESIAN_POINT('Ctrl Pts',(3.66756084339686,28.9895032609136,56.3246981621082));
#106343=CARTESIAN_POINT('Ctrl Pts',(3.66889993569834,28.9742178946141,56.312897510548));
#106344=CARTESIAN_POINT('Ctrl Pts',(3.67223374436468,28.9370508779154,56.2831584551422));
#106345=CARTESIAN_POINT('Ctrl Pts',(3.6742430590468,28.9154149006627,56.2649234912472));
#106346=CARTESIAN_POINT('Ctrl Pts',(3.6834559209495,28.8192437790371,56.179587902602));
#106347=CARTESIAN_POINT('Ctrl Pts',(3.69083202618176,28.750395952079,56.1063919124717));
#106348=CARTESIAN_POINT('Ctrl Pts',(3.70400534816922,28.637714151063,55.9625629296919));
#106349=CARTESIAN_POINT('Ctrl Pts',(3.70983490151272,28.5917596889583,55.893987154749));
#106350=CARTESIAN_POINT('Ctrl Pts',(3.71681868031431,28.5413908424466,55.8052326172279));
#106351=CARTESIAN_POINT('Ctrl Pts',(3.71814948058291,28.5320172084058,55.7880144813866));
#106352=CARTESIAN_POINT('Ctrl Pts',(3.72026587345646,28.5174790784654,55.7601496999893));
#106353=CARTESIAN_POINT('Ctrl Pts',(3.72105823878788,28.5121205482233,55.7496069627771));
#106354=CARTESIAN_POINT('Ctrl Pts',(3.72256276972427,28.5021101606159,55.7293815152714));
#106355=CARTESIAN_POINT('Ctrl Pts',(3.72327558555169,28.4974388251294,55.7197091709414));
#106356=CARTESIAN_POINT('Ctrl Pts',(3.72490889236232,28.4869027563188,55.6973436871903));
#106357=CARTESIAN_POINT('Ctrl Pts',(3.72582709173406,28.4811035669327,55.6846204293308));
#106358=CARTESIAN_POINT('Ctrl Pts',(3.72873884590078,28.4631199289388,55.643811185987));
#106359=CARTESIAN_POINT('Ctrl Pts',(3.73071172124312,28.4515487083012,55.615460788233));
#106360=CARTESIAN_POINT('Ctrl Pts',(3.73537233849443,28.4257845846137,55.5470014973659));
#106361=CARTESIAN_POINT('Ctrl Pts',(3.73803748115778,28.4123334374677,55.5066360417781));
#106362=CARTESIAN_POINT('Ctrl Pts',(3.7452435958232,28.3798348511975,55.3950352422274));
#106363=CARTESIAN_POINT('Ctrl Pts',(3.74971708892027,28.3639464814892,55.3229817340117));
#106364=CARTESIAN_POINT('Ctrl Pts',(3.75508132177096,28.3507827396229,55.236291876073));
#106365=CARTESIAN_POINT('Ctrl Pts',(3.75593774364295,28.348858105026,55.22244518258));
#106366=CARTESIAN_POINT('Ctrl Pts',(3.76130210658127,28.3379250955385,55.1358049058926));
#106367=CARTESIAN_POINT('Ctrl Pts',(3.76586258715842,28.3335591700475,55.0625156050565));
#106368=CARTESIAN_POINT('Ctrl Pts',(3.77145456509739,28.3341147717062,54.976909959023));
#106369=CARTESIAN_POINT('Ctrl Pts',(3.772262864423,28.334330171417,54.9646341375197));
#106370=CARTESIAN_POINT('Ctrl Pts',(3.77353996555152,28.334879952118,54.945414917008));
#106371=CARTESIAN_POINT('Ctrl Pts',(3.77400389113555,28.3351221541964,54.9384690377012));
#106372=CARTESIAN_POINT('Ctrl Pts',(3.77487652395781,28.3356566489741,54.9254757366308));
#106373=CARTESIAN_POINT('Ctrl Pts',(3.77528465691647,28.3359384551154,54.9194281309053));
#106374=CARTESIAN_POINT('Ctrl Pts',(3.77625107195705,28.336680474099,54.9051754831087));
#106375=CARTESIAN_POINT('Ctrl Pts',(3.77681083991436,28.3371684415244,54.8969721624713));
#106376=CARTESIAN_POINT('Ctrl Pts',(3.77869616412535,28.3390062855521,54.8695056578784));
#106377=CARTESIAN_POINT('Ctrl Pts',(3.78003527910983,28.3406303303832,54.8502631880619));
#106378=CARTESIAN_POINT('Ctrl Pts',(3.7833691569091,28.345457487882,54.8029072065176));
#106379=CARTESIAN_POINT('Ctrl Pts',(3.78537851876467,28.349043019405,54.7748392549013));
#106380=CARTESIAN_POINT('Ctrl Pts',(3.79459180007811,28.3685785299282,54.6477530873025));
#106381=CARTESIAN_POINT('Ctrl Pts',(3.80196828902024,28.3927349615413,54.5502073094739));
#106382=CARTESIAN_POINT('Ctrl Pts',(3.81514152444983,28.4524590790366,54.3775321234921));
#106383=CARTESIAN_POINT('Ctrl Pts',(3.82097064672097,28.4851466357642,54.3017363519848));
#106384=CARTESIAN_POINT('Ctrl Pts',(3.82795400897509,28.5323921862791,54.2112874158683));
#106385=CARTESIAN_POINT('Ctrl Pts',(3.82928479669688,28.5417738910934,54.1940738821026));
#106386=CARTESIAN_POINT('Ctrl Pts',(3.83140117452513,28.5572992479177,54.1667471042869));
#106387=CARTESIAN_POINT('Ctrl Pts',(3.83219353718721,28.5632503696404,54.1565272023256));
#106388=CARTESIAN_POINT('Ctrl Pts',(3.8336980660589,28.5748133640607,54.1371475104627));
#106389=CARTESIAN_POINT('Ctrl Pts',(3.83441088245948,28.5804059644971,54.127976978778));
#106390=CARTESIAN_POINT('Ctrl Pts',(3.83604419481766,28.593481847257,54.1069948628052));
#106391=CARTESIAN_POINT('Ctrl Pts',(3.83696239910928,28.6010259835407,54.0952220106202));
#106392=CARTESIAN_POINT('Ctrl Pts',(3.83987418665241,28.6255582267854,54.0579792809409));
#106393=CARTESIAN_POINT('Ctrl Pts',(3.84184708976075,28.6431010893036,54.0328812079989));
#106394=CARTESIAN_POINT('Ctrl Pts',(3.84650778673558,28.6866440214969,53.9741048017639));
#106395=CARTESIAN_POINT('Ctrl Pts',(3.84917298025618,28.7132619733805,53.940910525331));
#106396=CARTESIAN_POINT('Ctrl Pts',(3.85637912015602,28.7893971622503,53.8530786121888));
#106397=CARTESIAN_POINT('Ctrl Pts',(3.86085259101378,28.8413150506234,53.800651238141));
#106398=CARTESIAN_POINT('Ctrl Pts',(3.8662170007479,28.9070097061631,53.7425725745712));
#106399=CARTESIAN_POINT('Ctrl Pts',(3.86707362039982,28.9176015479757,53.7334436066009));
#106400=CARTESIAN_POINT('Ctrl Pts',(3.87243792303791,28.9844617265538,53.6772689849089));
#106401=CARTESIAN_POINT('Ctrl Pts',(3.87699814725148,29.0436639965253,53.6338543078848));
#106402=CARTESIAN_POINT('Ctrl Pts',(3.88258984061333,29.1158826912752,53.5878940096969));
#106403=CARTESIAN_POINT('Ctrl Pts',(3.88339813888248,29.1263129550086,53.5814170207238));
#106404=CARTESIAN_POINT('Ctrl Pts',(3.88467523870082,29.1427580236849,53.5714551112631));
#106405=CARTESIAN_POINT('Ctrl Pts',(3.8851391640472,29.1487249180685,53.5678914023021));
#106406=CARTESIAN_POINT('Ctrl Pts',(3.88601179668975,29.1599310446839,53.5612933564278));
#106407=CARTESIAN_POINT('Ctrl Pts',(3.8864199297094,29.1651647439661,53.5582501095731));
#106408=CARTESIAN_POINT('Ctrl Pts',(3.88738634525808,29.1775414651067,53.5511433843424));
#106409=CARTESIAN_POINT('Ctrl Pts',(3.88794611366717,29.1846980938452,53.5471041575202));
#106410=CARTESIAN_POINT('Ctrl Pts',(3.88983144102737,29.208770721434,53.5337513433923));
#106411=CARTESIAN_POINT('Ctrl Pts',(3.89117055876866,29.2258180170275,53.5246793324716));
#106412=CARTESIAN_POINT('Ctrl Pts',(3.89450444497027,29.2682220233958,53.5030506050495));
#106413=CARTESIAN_POINT('Ctrl Pts',(3.89651381255923,29.2937478685106,53.4908398878478));
#106414=CARTESIAN_POINT('Ctrl Pts',(3.90572714484882,29.4111145052723,53.4383252901231));
#106415=CARTESIAN_POINT('Ctrl Pts',(3.91310368042812,29.5061691616486,53.4057147067374));
#106416=CARTESIAN_POINT('Ctrl Pts',(3.92627690533863,29.6836332936735,53.3622389830126));
#106417=CARTESIAN_POINT('Ctrl Pts',(3.93210597521771,29.7650404821818,53.348592495939));
#106418=CARTESIAN_POINT('Ctrl Pts',(3.93908928684428,29.8666541304664,53.3392293615676));
#106419=CARTESIAN_POINT('Ctrl Pts',(3.94042007304057,29.8862042478938,53.3377753406513));
#106420=CARTESIAN_POINT('Ctrl Pts',(3.94253644903959,29.9175830336683,53.3359978089487));
#106421=CARTESIAN_POINT('Ctrl Pts',(3.94332881137708,29.9293968885114,53.3354546983357));
#106422=CARTESIAN_POINT('Ctrl Pts',(3.94483333999774,29.9519499612372,53.3346584254991));
#106423=CARTESIAN_POINT('Ctrl Pts',(3.94554615646801,29.962687751182,53.3343832459746));
#106424=CARTESIAN_POINT('Ctrl Pts',(3.94717946950067,29.9874076405158,53.3339889190656));
#106425=CARTESIAN_POINT('Ctrl Pts',(3.94809767439053,30.0013902043818,53.3339419048581));
#106426=CARTESIAN_POINT('Ctrl Pts',(3.95100946599199,30.0459849145829,53.3343533946195));
#106427=CARTESIAN_POINT('Ctrl Pts',(3.95298237247646,30.0765855711247,53.3354796290588));
#106428=CARTESIAN_POINT('Ctrl Pts',(3.9576430791451,30.1495824683159,53.3401837517527));
#106429=CARTESIAN_POINT('Ctrl Pts',(3.9603082788496,30.1919071482605,53.3445432896958));
#106430=CARTESIAN_POINT('Ctrl Pts',(3.96751442181486,30.3069916107435,53.3608709491741));
#106431=CARTESIAN_POINT('Ctrl Pts',(3.9719878899657,30.379196483283,53.3760547160427));
#106432=CARTESIAN_POINT('Ctrl Pts',(3.98145089247296,30.5281247722577,53.4178502988029));
#106433=CARTESIAN_POINT('Ctrl Pts',(3.98643591211819,30.6043826998837,53.4453836941138));
#106434=CARTESIAN_POINT('Ctrl Pts',(3.99272799625555,30.6930659031125,53.4849171433578));
#106435=CARTESIAN_POINT('Ctrl Pts',(3.99378388267648,30.7077080098458,53.4917010460959));
#106436=CARTESIAN_POINT('Ctrl Pts',(3.9953658315541,30.7292463088972,53.5020627109277));
#106437=CARTESIAN_POINT('Ctrl Pts',(3.99588258090173,30.7362202232012,53.505477976739));
#106438=CARTESIAN_POINT('Ctrl Pts',(3.99680466777476,30.7485496024603,53.5116231578253));
#106439=CARTESIAN_POINT('Ctrl Pts',(3.99720880522894,30.75391454024,53.5143334844259));
#106440=CARTESIAN_POINT('Ctrl Pts',(3.99810474396323,30.7657216264186,53.5203787611708));
#106441=CARTESIAN_POINT('Ctrl Pts',(3.9985973125665,30.7721566307778,53.5237267352773));
#106442=CARTESIAN_POINT('Ctrl Pts',(4.000053098539,30.7910165133656,53.5336961104309));
#106443=CARTESIAN_POINT('Ctrl Pts',(4.00102298844109,30.8033792035477,53.540432925965));
#106444=CARTESIAN_POINT('Ctrl Pts',(4.00784036257214,30.8889764114697,53.5884944430012));
#106445=CARTESIAN_POINT('Ctrl Pts',(4.01394234123824,30.9590688230319,53.6351516189576));
#106446=CARTESIAN_POINT('Ctrl Pts',(4.02939497361657,31.1264124677434,53.7658210616265));
#106447=CARTESIAN_POINT('Ctrl Pts',(4.0386861009998,31.218060330235,53.8561715340597));
#106448=CARTESIAN_POINT('Ctrl Pts',(4.04895779111851,31.3116069335795,53.9725347874851));
#106449=CARTESIAN_POINT('Ctrl Pts',(4.05039132668525,31.3244617220503,53.989159395468));
#106450=CARTESIAN_POINT('Ctrl Pts',(4.05271401000041,31.3449508888141,54.0167193982816));
#106451=CARTESIAN_POINT('Ctrl Pts',(4.05361042175633,31.352774245051,54.0275106710706));
#106452=CARTESIAN_POINT('Ctrl Pts',(4.05521563714506,31.3666275113448,54.0471101083771));
#106453=CARTESIAN_POINT('Ctrl Pts',(4.05592619045449,31.3727037942888,54.0558844336824));
#106454=CARTESIAN_POINT('Ctrl Pts',(4.05744294394216,31.3855510569989,54.074822506494));
#106455=CARTESIAN_POINT('Ctrl Pts',(4.05824811450683,31.3922954767459,54.0850035820852));
#106456=CARTESIAN_POINT('Ctrl Pts',(4.06045485056925,31.4105643138374,54.1132511732276));
#106457=CARTESIAN_POINT('Ctrl Pts',(4.06184770924882,31.4218533139321,54.1314676822671));
#106458=CARTESIAN_POINT('Ctrl Pts',(4.0649364367016,31.4463071040002,54.1726828364681));
#106459=CARTESIAN_POINT('Ctrl Pts',(4.06662563888547,31.4592811039789,54.195788149299));
#106460=CARTESIAN_POINT('Ctrl Pts',(4.0720956847489,31.4998607068951,54.2722744549125));
#106461=CARTESIAN_POINT('Ctrl Pts',(4.07580726781239,31.5251314898594,54.3268422649182));
#106462=CARTESIAN_POINT('Ctrl Pts',(4.08363158950441,31.5724428485431,54.4454308566849));
#106463=CARTESIAN_POINT('Ctrl Pts',(4.08772902335711,31.5936425456686,54.5096668983709));
#106464=CARTESIAN_POINT('Ctrl Pts',(4.0953320080324,31.6250899440977,54.6288655270577));
#106465=CARTESIAN_POINT('Ctrl Pts',(4.09881093912048,31.6365870327772,54.6833932552034));
#106466=CARTESIAN_POINT('Ctrl Pts',(4.10355714718408,31.6481170479877,54.7559080333767));
#106467=CARTESIAN_POINT('Ctrl Pts',(4.10471580038967,31.6506225513418,54.7734700383525));
#106468=CARTESIAN_POINT('Ctrl Pts',(4.10640913186407,31.6538332404562,54.7988695636052));
#106469=CARTESIAN_POINT('Ctrl Pts',(4.1069320946566,31.6547641626954,54.8066779904675));
#106470=CARTESIAN_POINT('Ctrl Pts',(4.10786147985884,31.656311152587,54.8204847541879));
#106471=CARTESIAN_POINT('Ctrl Pts',(4.10826663774894,31.656949988806,54.8264802876139));
#106472=CARTESIAN_POINT('Ctrl Pts',(4.10905780292853,31.6581284720227,54.8381409510528));
#106473=CARTESIAN_POINT('Ctrl Pts',(4.10944355608575,31.6586716421921,54.8438053700639));
#106474=CARTESIAN_POINT('Ctrl Pts',(4.11031154180718,31.6598239276151,54.856506396263));
#106475=CARTESIAN_POINT('Ctrl Pts',(4.11079459211428,31.6604173316357,54.8635442729869));
#106476=CARTESIAN_POINT('Ctrl Pts',(4.11238837719785,31.6622193504549,54.8866722313403));
#106477=CARTESIAN_POINT('Ctrl Pts',(4.11350821152835,31.6632389234635,54.9027755704834));
#106478=CARTESIAN_POINT('Ctrl Pts',(4.11650950326211,31.6653267889015,54.9456097238552));
#106479=CARTESIAN_POINT('Ctrl Pts',(4.11840677441157,31.665985348925,54.9723548619076));
#106480=CARTESIAN_POINT('Ctrl Pts',(4.12032061737785,31.6659997582528,54.999102502649));
#106481=CARTESIAN_POINT('Ctrl Pts',(4.12032044382387,31.6659997569444,54.9991000770787));
#106482=CARTESIAN_POINT('Ctrl Pts',(4.1277658568908,31.6660559650028,55.1031563350326));
#106483=CARTESIAN_POINT('Ctrl Pts',(4.13542588510684,31.6563635124353,55.2069926789193));
#106484=CARTESIAN_POINT('Ctrl Pts',(4.14684877837074,31.6269365538621,55.3627664368907));
#106485=CARTESIAN_POINT('Ctrl Pts',(4.15072582248182,31.6142084265747,55.4157573269186));
#106486=CARTESIAN_POINT('Ctrl Pts',(4.15626917939867,31.5919075112809,55.4919421309294));
#106487=CARTESIAN_POINT('Ctrl Pts',(4.15799304522444,31.5843733837398,55.5156914561716));
#106488=CARTESIAN_POINT('Ctrl Pts',(4.16057877508544,31.5721582975419,55.5513970694736));
#106489=CARTESIAN_POINT('Ctrl Pts',(4.16145289012264,31.5678675441439,55.5634818607482));
#106490=CARTESIAN_POINT('Ctrl Pts',(4.16232242021249,31.5634376783906,55.5755159648424));
#106491=CARTESIAN_POINT('Ctrl Pts',(3.96712534830139,31.5634376767977,55.5755159691697));
#106492=CARTESIAN_POINT('Ctrl Pts',(3.96351693599737,31.5807588243258,55.5284616108175));
#106493=CARTESIAN_POINT('Ctrl Pts',(3.95994981330664,31.5959492132535,55.4806429514429));
#106494=CARTESIAN_POINT('Ctrl Pts',(3.95382910339297,31.6186666688434,55.3960731365343));
#106495=CARTESIAN_POINT('Ctrl Pts',(3.95124982411429,31.6271533038374,55.3596223372666));
#106496=CARTESIAN_POINT('Ctrl Pts',(3.94768576870063,31.6373274053918,55.3081268621989));
#106497=CARTESIAN_POINT('Ctrl Pts',(3.94666872224283,31.6400482132038,55.2933003238372));
#106498=CARTESIAN_POINT('Ctrl Pts',(3.94492685658813,31.6443901052209,55.2676865830567));
#106499=CARTESIAN_POINT('Ctrl Pts',(3.94419904482276,31.6461071253268,55.2569168476138));
#106500=CARTESIAN_POINT('Ctrl Pts',(3.94271778550572,31.6494012813139,55.2348641787326));
#106501=CARTESIAN_POINT('Ctrl Pts',(3.94196468106963,31.6509686863954,55.2235803584588));
#106502=CARTESIAN_POINT('Ctrl Pts',(3.94005976102336,31.6546578326869,55.1948636245157));
#106503=CARTESIAN_POINT('Ctrl Pts',(3.93891299250075,31.6566199416375,55.1774113374755));
#106504=CARTESIAN_POINT('Ctrl Pts',(3.93428740746794,31.663468325158,55.1064011320388));
#106505=CARTESIAN_POINT('Ctrl Pts',(3.93088051265922,31.6660363066166,55.0526495522779));
#106506=CARTESIAN_POINT('Ctrl Pts',(3.92156614302989,31.6659344230191,54.9033095725002));
#106507=CARTESIAN_POINT('Ctrl Pts',(3.9157973412044,31.6576488346749,54.8079391668846));
#106508=CARTESIAN_POINT('Ctrl Pts',(3.90524392672487,31.6281028549061,54.6385037627577));
#106509=CARTESIAN_POINT('Ctrl Pts',(3.90050166830427,31.6098072576345,54.564206456795));
#106510=CARTESIAN_POINT('Ctrl Pts',(3.89470757655666,31.5827296226805,54.4797366760682));
#106511=CARTESIAN_POINT('Ctrl Pts',(3.89389864654783,31.5788495192567,54.4680778642752));
#106512=CARTESIAN_POINT('Ctrl Pts',(3.89262085209436,31.5725731570898,54.4498927534408));
#106513=CARTESIAN_POINT('Ctrl Pts',(3.89215687439136,31.5702643108389,54.4433364509457));
#106514=CARTESIAN_POINT('Ctrl Pts',(3.8912843758664,31.5658687305618,54.4310995327023));
#106515=CARTESIAN_POINT('Ctrl Pts',(3.89087643158248,31.5637919861012,54.4254155914231));
#106516=CARTESIAN_POINT('Ctrl Pts',(3.88991079769832,31.5588251046717,54.4120478881272));
#106517=CARTESIAN_POINT('Ctrl Pts',(3.88935162749118,31.5559090901205,54.4043740359645));
#106518=CARTESIAN_POINT('Ctrl Pts',(3.88746983846932,31.5459593591221,54.3787617851433));
#106519=CARTESIAN_POINT('Ctrl Pts',(3.88613372408595,31.5386714650072,54.360924649634));
#106520=CARTESIAN_POINT('Ctrl Pts',(3.8828088246177,31.5199551331978,54.3172934742659));
#106521=CARTESIAN_POINT('Ctrl Pts',(3.88080553128511,31.5081778997748,54.2916561213737));
#106522=CARTESIAN_POINT('Ctrl Pts',(3.87164500323877,31.451873921206,54.176867164766));
#106523=CARTESIAN_POINT('Ctrl Pts',(3.86431661374217,31.4000540829402,54.0915207684663));
#106524=CARTESIAN_POINT('Ctrl Pts',(3.85113159956565,31.2915605416186,53.9443747845352));
#106525=CARTESIAN_POINT('Ctrl Pts',(3.84524751388157,31.2372542570995,53.8812154346461));
#106526=CARTESIAN_POINT('Ctrl Pts',(3.83821138036139,31.1645797457592,53.808490463106));
#106527=CARTESIAN_POINT('Ctrl Pts',(3.8368793069299,31.1504662557193,53.794857513695));
#106528=CARTESIAN_POINT('Ctrl Pts',(3.8347615511707,31.1274641692756,53.7734110588611));
#106529=CARTESIAN_POINT('Ctrl Pts',(3.83396907713306,31.1187278207651,53.7654377459773));
#106530=CARTESIAN_POINT('Ctrl Pts',(3.83246475185865,31.1019005912223,53.7504055263115));
#106531=CARTESIAN_POINT('Ctrl Pts',(3.83175224647607,31.093824971513,53.7433305118262));
#106532=CARTESIAN_POINT('Ctrl Pts',(3.83012024026566,31.0750878167344,53.7272324461413));
#106533=CARTESIAN_POINT('Ctrl Pts',(3.82920302194552,31.0643799857062,53.7182643308571));
#106534=CARTESIAN_POINT('Ctrl Pts',(3.82629690733746,31.0299015933912,53.6901177634513));
#106535=CARTESIAN_POINT('Ctrl Pts',(3.82432857957748,31.0057151105571,53.6714571631206));
#106536=CARTESIAN_POINT('Ctrl Pts',(3.81968080490962,30.9467625665421,53.6285066590519));
#106537=CARTESIAN_POINT('Ctrl Pts',(3.81702378475737,30.9115551663822,53.6048581083218));
#106538=CARTESIAN_POINT('Ctrl Pts',(3.80982203774112,30.8127342678802,53.5438206336987));
#106539=CARTESIAN_POINT('Ctrl Pts',(3.8053453193444,30.7474808736292,53.5092726434648));
#106540=CARTESIAN_POINT('Ctrl Pts',(3.80002286597666,30.6680575399765,53.4737527458333));
#106541=CARTESIAN_POINT('Ctrl Pts',(3.79921124124492,30.6558981942765,53.4684879656685));
#106542=CARTESIAN_POINT('Ctrl Pts',(3.79383689466949,30.5751743500369,53.4346736595079));
#106543=CARTESIAN_POINT('Ctrl Pts',(3.78922202893699,30.5048374316564,53.4105949396591));
#106544=CARTESIAN_POINT('Ctrl Pts',(3.7835697924003,30.4212828203044,53.3880981564157));
#106545=CARTESIAN_POINT('Ctrl Pts',(3.78276143036741,30.4093917966758,53.3850371202145));
#106546=CARTESIAN_POINT('Ctrl Pts',(3.78148434032301,30.3907200450586,53.3804500205093));
#106547=CARTESIAN_POINT('Ctrl Pts',(3.7810204903474,30.3839614771555,53.3788344102571));
#106548=CARTESIAN_POINT('Ctrl Pts',(3.78014808858631,30.371298176158,53.3758909233979));
#106549=CARTESIAN_POINT('Ctrl Pts',(3.77974011170337,30.3653960601807,53.3745528790974));
#106550=CARTESIAN_POINT('Ctrl Pts',(3.77877420558863,30.3514675648094,53.3714749001763));
#106551=CARTESIAN_POINT('Ctrl Pts',(3.77821479321375,30.3434354659475,53.369762126703));
#106552=CARTESIAN_POINT('Ctrl Pts',(3.77633131746291,30.31649722076,53.3642256964015));
#106553=CARTESIAN_POINT('Ctrl Pts',(3.77499372681293,30.2975381686213,53.3606711671988));
#106554=CARTESIAN_POINT('Ctrl Pts',(3.77166433063021,30.2506683260128,53.3527235914143));
#106555=CARTESIAN_POINT('Ctrl Pts',(3.7696579698927,30.2226998111734,53.3487099618955));
#106556=CARTESIAN_POINT('Ctrl Pts',(3.76047032018012,30.0953510883449,53.333728778789));
#106557=CARTESIAN_POINT('Ctrl Pts',(3.75311713354603,29.9952086114025,53.3310095594829));
#106558=CARTESIAN_POINT('Ctrl Pts',(3.73993782178608,29.8128003182597,53.3424819126742));
#106559=CARTESIAN_POINT('Ctrl Pts',(3.73408172994153,29.7306674360097,53.3538306208928));
#106560=CARTESIAN_POINT('Ctrl Pts',(3.7270725839085,29.630536633256,53.3753654722435));
#106561=CARTESIAN_POINT('Ctrl Pts',(3.72574127616074,29.611439214048,53.3798268300046));
#106562=CARTESIAN_POINT('Ctrl Pts',(3.72362443853387,29.5809587112737,53.387517371741));
#106563=CARTESIAN_POINT('Ctrl Pts',(3.72283212739023,29.569524016104,53.3905323029453));
#106564=CARTESIAN_POINT('Ctrl Pts',(3.72132792841555,29.547770076989,53.3965164886697));
#106565=CARTESIAN_POINT('Ctrl Pts',(3.72061538835289,29.537445593168,53.3994642446043));
#106566=CARTESIAN_POINT('Ctrl Pts',(3.7189830451154,29.5137535946439,53.4064769773177));
#106567=CARTESIAN_POINT('Ctrl Pts',(3.71806552775814,29.5004071562692,53.4106107459998));
#106568=CARTESIAN_POINT('Ctrl Pts',(3.71515738656525,29.4580304898693,53.4243225406966));
#106569=CARTESIAN_POINT('Ctrl Pts',(3.71318737309003,29.4292101969342,53.4345321484676));
#106570=CARTESIAN_POINT('Ctrl Pts',(3.70853476198478,29.3610808902053,53.4607988891379));
#106571=CARTESIAN_POINT('Ctrl Pts',(3.70587465761056,29.32207233312,53.4775768834822));
#106572=CARTESIAN_POINT('Ctrl Pts',(3.69867102988447,29.217171069946,53.527528635154));
#106573=CARTESIAN_POINT('Ctrl Pts',(3.69419532516638,29.1527736619489,53.5636153180848));
#106574=CARTESIAN_POINT('Ctrl Pts',(3.68885255439594,29.0795847512065,53.6112679801964));
#106575=CARTESIAN_POINT('Ctrl Pts',(3.6880196739884,29.0682822220925,53.6188255613811));
#106576=CARTESIAN_POINT('Ctrl Pts',(3.68264898927925,28.9961896184221,53.6683188567357));
#106577=CARTESIAN_POINT('Ctrl Pts',(3.67805884893528,28.938159744,53.71411413687));
#106578=CARTESIAN_POINT('Ctrl Pts',(3.67243408395006,28.8742548214744,53.7718287890703));
#106579=CARTESIAN_POINT('Ctrl Pts',(3.67162582078034,28.8652350049933,53.7801577500834));
#106580=CARTESIAN_POINT('Ctrl Pts',(3.67034885334892,28.8512556898266,53.7933555640755));
#106581=CARTESIAN_POINT('Ctrl Pts',(3.66988502560803,28.8462329980052,53.7981572541971));
#106582=CARTESIAN_POINT('Ctrl Pts',(3.66901264067446,28.8368921328437,53.8071996317067));
#106583=CARTESIAN_POINT('Ctrl Pts',(3.6686046580995,28.8325668401442,53.8114326094681));
#106584=CARTESIAN_POINT('Ctrl Pts',(3.66763870451816,28.8224261124351,53.8214656563581));
#106585=CARTESIAN_POINT('Ctrl Pts',(3.66707924992637,28.8166304003645,53.8272852676762));
#106586=CARTESIAN_POINT('Ctrl Pts',(3.6651954800106,28.7973657520686,53.846917579279));
#106587=CARTESIAN_POINT('Ctrl Pts',(3.66385763187953,28.7840943125196,53.8609207739745));
#106588=CARTESIAN_POINT('Ctrl Pts',(3.66052745121167,28.7519896194922,53.8959960689645));
#106589=CARTESIAN_POINT('Ctrl Pts',(3.65852055527039,28.7334440102807,53.9173226084009));
#106590=CARTESIAN_POINT('Ctrl Pts',(3.64932816259986,28.6517489897376,54.0162406772163));
#106591=CARTESIAN_POINT('Ctrl Pts',(3.64197063835687,28.5951240229557,54.0989522087406));
#106592=CARTESIAN_POINT('Ctrl Pts',(3.62879231646135,28.5058551570325,54.2584272815812));
#106593=CARTESIAN_POINT('Ctrl Pts',(3.622941111821,28.4708770270296,54.333527526658));
#106594=CARTESIAN_POINT('Ctrl Pts',(3.61593668169071,28.4346869464832,54.4292675800241));
#106595=CARTESIAN_POINT('Ctrl Pts',(3.61460551102319,28.4280781306889,54.4477300076102));
#106596=CARTESIAN_POINT('Ctrl Pts',(3.61248883777089,28.4180086221042,54.4775068436473));
#106597=CARTESIAN_POINT('Ctrl Pts',(3.61169655579118,28.4143399910984,54.4887484309854));
#106598=CARTESIAN_POINT('Ctrl Pts',(3.6101923794108,28.4075691574767,54.5102701883214));
#106599=CARTESIAN_POINT('Ctrl Pts',(3.60947983312135,28.4044460615004,54.5205431039082));
#106600=CARTESIAN_POINT('Ctrl Pts',(3.60784742945471,28.3974878709704,54.5442521637048));
#106601=CARTESIAN_POINT('Ctrl Pts',(3.60692985848848,28.3937220208725,54.5577079161389));
#106602=CARTESIAN_POINT('Ctrl Pts',(3.60402135387329,28.3822570389804,54.6007526931826));
#106603=CARTESIAN_POINT('Ctrl Pts',(3.60205103809121,28.3752026247366,54.6305079471121));
#106604=CARTESIAN_POINT('Ctrl Pts',(3.59739755945635,28.3603176302196,54.7020063840521));
#106605=CARTESIAN_POINT('Ctrl Pts',(3.5947369018002,28.3532560667696,54.74388817644));
#106606=CARTESIAN_POINT('Ctrl Pts',(3.5875329551255,28.338330628906,54.8591188383726));
#106607=CARTESIAN_POINT('Ctrl Pts',(3.58305744987355,28.3337239340639,54.9327910685991));
#106608=CARTESIAN_POINT('Ctrl Pts',(3.57771156749899,28.3340662538672,55.0201759678629));
#106609=CARTESIAN_POINT('Ctrl Pts',(3.57687538987544,28.3342874727752,55.0338243592471));
#106610=CARTESIAN_POINT('Ctrl Pts',(3.57150536251012,28.3367786751581,55.1212227054904));
#106611=CARTESIAN_POINT('Ctrl Pts',(3.56691914791976,28.3437780972681,55.194746932433));
#106612=CARTESIAN_POINT('Ctrl Pts',(3.56129874328014,28.3575962943456,55.2796726514467));
#106613=CARTESIAN_POINT('Ctrl Pts',(3.56049049588562,28.3597017575764,55.2917676789191));
#106614=CARTESIAN_POINT('Ctrl Pts',(3.55921354801901,28.3632078893186,55.3106700348482));
#106615=CARTESIAN_POINT('Ctrl Pts',(3.55874972382617,28.3645178623578,55.317494027066));
#106616=CARTESIAN_POINT('Ctrl Pts',(3.55787734157736,28.3670486025996,55.3302459130961));
#106617=CARTESIAN_POINT('Ctrl Pts',(3.55746935809367,28.3682590321286,55.3361756066161));
#106618=CARTESIAN_POINT('Ctrl Pts',(3.55650339693592,28.3711882914034,55.3501369437018));
#106619=CARTESIAN_POINT('Ctrl Pts',(3.55594393560588,28.3729342376776,55.3581626158835));
#106620=CARTESIAN_POINT('Ctrl Pts',(3.55406011873552,28.3789799050259,55.3849962043276));
#106621=CARTESIAN_POINT('Ctrl Pts',(3.55272222950467,28.3835468020544,55.4037415079455));
#106622=CARTESIAN_POINT('Ctrl Pts',(3.54939192360981,28.3956031643451,55.4497393126902));
#106623=CARTESIAN_POINT('Ctrl Pts',(3.54738494223224,28.4034624406231,55.4768881387664));
#106624=CARTESIAN_POINT('Ctrl Pts',(3.53819179213125,28.4422629619782,55.599183078923));
#106625=CARTESIAN_POINT('Ctrl Pts',(3.53083357515847,28.4810458725131,55.691624061468));
#106626=CARTESIAN_POINT('Ctrl Pts',(3.51765541113551,28.5666142170721,55.8531133259261));
#106627=CARTESIAN_POINT('Ctrl Pts',(3.51180498673131,28.6107333819444,55.923222144402));
#106628=CARTESIAN_POINT('Ctrl Pts',(3.50480130961133,28.6715341526858,56.0055440969087));
#106629=CARTESIAN_POINT('Ctrl Pts',(3.50347016092373,28.6834606778057,56.0211095477042));
#106630=CARTESIAN_POINT('Ctrl Pts',(3.50135351402786,28.7030159288008,56.0457189563342));
#106631=CARTESIAN_POINT('Ctrl Pts',(3.50056123672444,28.7104707040302,56.0548981106696));
#106632=CARTESIAN_POINT('Ctrl Pts',(3.49905706396646,28.7248797876153,56.0722591669003));
#106633=CARTESIAN_POINT('Ctrl Pts',(3.49834451667812,28.7318166707834,56.0804546865723));
#106634=CARTESIAN_POINT('Ctrl Pts',(3.49671210331965,28.7479619189958,56.0991596160014));
#106635=CARTESIAN_POINT('Ctrl Pts',(3.49579452375558,28.7572243157534,56.1096214832458));
#106636=CARTESIAN_POINT('Ctrl Pts',(3.49288596085128,28.7871705448035,56.1426003062044));
#106637=CARTESIAN_POINT('Ctrl Pts',(3.49091559658207,28.8083437336193,56.1646657365186));
#106638=CARTESIAN_POINT('Ctrl Pts',(3.48626197879834,28.8603413031889,56.2159509237159));
#106639=CARTESIAN_POINT('Ctrl Pts',(3.48360123239604,28.8916992694844,56.2445997202942));
#106640=CARTESIAN_POINT('Ctrl Pts',(3.47639723507272,28.9804156426917,56.3196364139072));
#106641=CARTESIAN_POINT('Ctrl Pts',(3.47192176230318,29.0398121681107,56.3634633188437));
#106642=CARTESIAN_POINT('Ctrl Pts',(3.46657539492045,29.113420514866,56.4105741249164));
#106643=CARTESIAN_POINT('Ctrl Pts',(3.46573870203686,29.1250143099819,56.4177949717942));
#106644=CARTESIAN_POINT('Ctrl Pts',(3.46036878010049,29.1997917024351,56.4631012467367));
#106645=CARTESIAN_POINT('Ctrl Pts',(3.45578318171749,29.265349860318,56.4970921781871));
#106646=CARTESIAN_POINT('Ctrl Pts',(3.45016346146697,29.3441845464325,56.5315393609799));
#106647=CARTESIAN_POINT('Ctrl Pts',(3.44935521655202,29.3554879984601,56.5363303620918));
#106648=CARTESIAN_POINT('Ctrl Pts',(3.44807827176066,29.3732702477765,56.5436366482108));
#106649=CARTESIAN_POINT('Ctrl Pts',(3.44761444812548,29.379713855339,56.5462371675752));
#106650=CARTESIAN_POINT('Ctrl Pts',(3.44674206629878,29.3917998468096,56.5510271445306));
#106651=CARTESIAN_POINT('Ctrl Pts',(3.44633408267239,29.397438135996,56.5532262632292));
#106652=CARTESIAN_POINT('Ctrl Pts',(3.44536812032378,29.4107564046268,56.5583373983087));
#106653=CARTESIAN_POINT('Ctrl Pts',(3.44480865793477,29.4184460743518,56.5612233940571));
#106654=CARTESIAN_POINT('Ctrl Pts',(3.4429248336845,29.4442691941899,56.5706977750823));
#106655=CARTESIAN_POINT('Ctrl Pts',(3.44158693799392,29.4624949483031,56.5770277325728));
#106656=CARTESIAN_POINT('Ctrl Pts',(3.43825661241683,29.5076789101521,56.5918462898501));
#106657=CARTESIAN_POINT('Ctrl Pts',(3.43624961761092,29.5347505899071,56.5999679597363));
#106658=CARTESIAN_POINT('Ctrl Pts',(3.42705634845486,29.6585415037072,56.6336986955327));
#106659=CARTESIAN_POINT('Ctrl Pts',(3.41969802259601,29.7572411300288,56.6512522235544));
#106660=CARTESIAN_POINT('Ctrl Pts',(3.40651988337975,29.9393243258093,56.6669479103152));
#106661=CARTESIAN_POINT('Ctrl Pts',(3.40066958160671,30.0221527718848,56.6679058252841));
#106662=CARTESIAN_POINT('Ctrl Pts',(3.39366602284187,30.1242894650576,56.661473010684));
#106663=CARTESIAN_POINT('Ctrl Pts',(3.39233487761129,30.1438351473273,56.6598951604656));
#106664=CARTESIAN_POINT('Ctrl Pts',(3.39021823486088,30.1751165889508,56.6568132051034));
#106665=CARTESIAN_POINT('Ctrl Pts',(3.38942595829297,30.1868715880752,56.6555285676722));
#106666=CARTESIAN_POINT('Ctrl Pts',(3.38792178610482,30.209272329075,56.652838881856));
#106667=CARTESIAN_POINT('Ctrl Pts',(3.3872092386594,30.219920061012,56.6514558586476));
#106668=CARTESIAN_POINT('Ctrl Pts',(3.38557682377657,30.2443915131544,56.648036409374));
#106669=CARTESIAN_POINT('Ctrl Pts',(3.38465924286035,30.2582045956096,56.6459288030873));
#106670=CARTESIAN_POINT('Ctrl Pts',(3.38175067078847,30.3021534403055,56.6386561729252));
#106671=CARTESIAN_POINT('Ctrl Pts',(3.37978029889314,30.3321752646589,56.6328351221111));
#106672=CARTESIAN_POINT('Ctrl Pts',(3.37512665922375,30.4034641383369,56.6169648428055));
#106673=CARTESIAN_POINT('Ctrl Pts',(3.37246589886321,30.4445408937129,56.6061576468486));
#106674=CARTESIAN_POINT('Ctrl Pts',(3.36526189358678,30.5556991842574,56.5723202382245));
#106675=CARTESIAN_POINT('Ctrl Pts',(3.36078642593863,30.6247345265697,56.5461887510835));
#106676=CARTESIAN_POINT('Ctrl Pts',(3.35132894064446,30.7653706120716,56.4819926279907));
#106677=CARTESIAN_POINT('Ctrl Pts',(3.34635158199632,30.8363787465844,56.443108378759));
#106678=CARTESIAN_POINT('Ctrl Pts',(3.34004640934146,30.9181186591092,56.3902826448104));
#106679=CARTESIAN_POINT('Ctrl Pts',(3.33896795752298,30.9318285094974,56.3811311608567));
#106680=CARTESIAN_POINT('Ctrl Pts',(3.33736587219883,30.9517556144202,56.3673978338083));
#106681=CARTESIAN_POINT('Ctrl Pts',(3.33685212205673,30.9580808678511,56.3629734517851));
#106682=CARTESIAN_POINT('Ctrl Pts',(3.3359333169489,30.9692729037333,56.3550284560361));
#106683=CARTESIAN_POINT('Ctrl Pts',(3.33552942920174,30.9741517222669,56.351525248855));
#106684=CARTESIAN_POINT('Ctrl Pts',(3.33463148557265,30.9849073268589,56.3437137537299));
#106685=CARTESIAN_POINT('Ctrl Pts',(3.33413663572504,30.9907747699822,56.3393933121366));
#106686=CARTESIAN_POINT('Ctrl Pts',(3.33266690514873,31.008030792598,56.3265115594664));
#106687=CARTESIAN_POINT('Ctrl Pts',(3.33168516312223,31.0193377699553,56.3178427346103));
#106688=CARTESIAN_POINT('Ctrl Pts',(3.32938713765778,31.0453300263599,56.2973803790608));
#106689=CARTESIAN_POINT('Ctrl Pts',(3.32806507818891,31.0599290851682,56.2854808369965));
#106690=CARTESIAN_POINT('Ctrl Pts',(3.32335736215911,31.1107736650876,56.2425829360346));
#106691=CARTESIAN_POINT('Ctrl Pts',(3.31991667456228,31.1458851744092,56.2102797571266));
#106692=CARTESIAN_POINT('Ctrl Pts',(3.30829275845901,31.2589670846898,56.096905358102));
#106693=CARTESIAN_POINT('Ctrl Pts',(3.30006621409789,31.3301201011451,56.0094481072516));
#106694=CARTESIAN_POINT('Ctrl Pts',(3.28892506433188,31.4169972062571,55.8773580650816));
#106695=CARTESIAN_POINT('Ctrl Pts',(3.28575959374229,31.4404972149207,55.8382163896087));
#106696=CARTESIAN_POINT('Ctrl Pts',(3.28151599394438,31.4703489322232,55.7835227668013));
#106697=CARTESIAN_POINT('Ctrl Pts',(3.28038842618937,31.4781157212353,55.7687703547314));
#106698=CARTESIAN_POINT('Ctrl Pts',(3.27859099704444,31.4902254515667,55.7449066303861));
#106699=CARTESIAN_POINT('Ctrl Pts',(3.27791624043787,31.4947091471847,55.7358684376632));
#106700=CARTESIAN_POINT('Ctrl Pts',(3.27652061557265,31.5038513541364,55.7170112976197));
#106701=CARTESIAN_POINT('Ctrl Pts',(3.2758002386179,31.5084964591263,55.7071863534999));
#106702=CARTESIAN_POINT('Ctrl Pts',(3.27410330459937,31.51926038285,55.6838306692777));
#106703=CARTESIAN_POINT('Ctrl Pts',(3.27312966385485,31.5252951562397,55.6702620420479));
#106704=CARTESIAN_POINT('Ctrl Pts',(3.27026542530456,31.5426175643117,55.6298682013147));
#106705=CARTESIAN_POINT('Ctrl Pts',(3.26839227694276,31.5533845038351,55.6028262616837));
#106706=CARTESIAN_POINT('Ctrl Pts',(3.26653908718979,31.5634376777881,55.5755159664792));
#106707=CARTESIAN_POINT('Origin',(5.,30.,55.));
#106708=CARTESIAN_POINT('',(2.56903902087732,31.5634376730794,55.5755159792709));
#106709=CARTESIAN_POINT('',(2.75980447732861,31.5634376782628,55.5755159651897));
#106710=CARTESIAN_POINT('',(5.,31.5634376782623,55.5755159651912));
#106711=CARTESIAN_POINT('Ctrl Pts',(2.75980447732862,31.5634376782628,55.5755159651897));
#106712=CARTESIAN_POINT('Ctrl Pts',(2.762192831449,31.5501199861041,55.6116945996113));
#106713=CARTESIAN_POINT('Ctrl Pts',(2.76460760539681,31.5355513221819,55.6473978851748));
#106714=CARTESIAN_POINT('Ctrl Pts',(2.76861985484581,31.5098628697695,55.7045945635996));
#106715=CARTESIAN_POINT('Ctrl Pts',(2.77018535434155,31.4994898538802,55.7264085747185));
#106716=CARTESIAN_POINT('Ctrl Pts',(2.77236755591098,31.4846263241562,55.7559899968398));
#106717=CARTESIAN_POINT('Ctrl Pts',(2.77296145010307,31.4805412912738,55.7639592093834));
#106718=CARTESIAN_POINT('Ctrl Pts',(2.77397123613029,31.4735332071027,55.7773634720219));
#106719=CARTESIAN_POINT('Ctrl Pts',(2.77438506543448,31.4706437663534,55.7828160647602));
#106720=CARTESIAN_POINT('Ctrl Pts',(2.77524682266853,31.4645925727568,55.7940833721435));
#106721=CARTESIAN_POINT('Ctrl Pts',(2.77569500274132,31.4614263844038,55.7998954464275));
#106722=CARTESIAN_POINT('Ctrl Pts',(2.77689891593948,31.4528682672194,55.8153848924919));
#106723=CARTESIAN_POINT('Ctrl Pts',(2.77765835717101,31.4474144115905,55.8250274112784));
#106724=CARTESIAN_POINT('Ctrl Pts',(2.7812277508218,31.4215069847876,55.8697846158843));
#106725=CARTESIAN_POINT('Ctrl Pts',(2.78410026247713,31.3998707259214,55.9041950820981));
#106726=CARTESIAN_POINT('Ctrl Pts',(2.79352160172908,31.325822373065,56.0129252103728));
#106727=CARTESIAN_POINT('Ctrl Pts',(2.8001962293002,31.2685795415418,56.083756522839));
#106728=CARTESIAN_POINT('Ctrl Pts',(2.81124499199724,31.1632224067688,56.1942717860872));
#106729=CARTESIAN_POINT('Ctrl Pts',(2.81566486019702,31.1181438060857,56.2365788324746));
#106730=CARTESIAN_POINT('Ctrl Pts',(2.8218800493281,31.050170696569,56.2936088005877));
#106731=CARTESIAN_POINT('Ctrl Pts',(2.82374966321167,31.029107863017,56.3104271700733));
#106732=CARTESIAN_POINT('Ctrl Pts',(2.82709019006151,30.9903547873915,56.3398599940553));
#106733=CARTESIAN_POINT('Ctrl Pts',(2.82856765666853,30.9728086357885,56.3526532607957));
#106734=CARTESIAN_POINT('Ctrl Pts',(2.83085950494593,30.9449618921524,56.372134687948));
#106735=CARTESIAN_POINT('Ctrl Pts',(2.83168277375302,30.934829477541,56.3790578092931));
#106736=CARTESIAN_POINT('Ctrl Pts',(2.83321372702154,30.9157484639601,56.3917882455475));
#106737=CARTESIAN_POINT('Ctrl Pts',(2.83392240747059,30.9068188547276,56.3976227471841));
#106738=CARTESIAN_POINT('Ctrl Pts',(2.83550396357362,30.8866767929159,56.4105090175721));
#106739=CARTESIAN_POINT('Ctrl Pts',(2.83637506625521,30.8754349580437,56.4175136947662));
#106740=CARTESIAN_POINT('Ctrl Pts',(2.83859722948818,30.8463880922487,56.4351351413961));
#106741=CARTESIAN_POINT('Ctrl Pts',(2.83994118263824,30.8284659718062,56.4455552120685));
#106742=CARTESIAN_POINT('Ctrl Pts',(2.85099728879109,30.6782536221692,56.5291783711156));
#106743=CARTESIAN_POINT('Ctrl Pts',(2.86000964392068,30.5367660063161,56.5843920509653));
#106744=CARTESIAN_POINT('Ctrl Pts',(2.87303656083141,30.3313639210802,56.6338183443995));
#106745=CARTESIAN_POINT('Ctrl Pts',(2.87679073185298,30.272249373356,56.6447015492948));
#106746=CARTESIAN_POINT('Ctrl Pts',(2.88167460469858,30.1976711930005,56.6543008174358));
#106747=CARTESIAN_POINT('Ctrl Pts',(2.88266681174194,30.1826341565861,56.6560283272249));
#106748=CARTESIAN_POINT('Ctrl Pts',(2.88416436774143,30.1601500610783,56.6583014415473));
#106749=CARTESIAN_POINT('Ctrl Pts',(2.88466158482524,30.1527190117687,56.6590022939116));
#106750=CARTESIAN_POINT('Ctrl Pts',(2.88556369250385,30.1393040470891,56.6601766208769));
#106751=CARTESIAN_POINT('Ctrl Pts',(2.8859676064051,30.1333219425452,56.6606677231264));
#106752=CARTESIAN_POINT('Ctrl Pts',(2.88688210129736,30.1198330423465,56.6617017440049));
#106753=CARTESIAN_POINT('Ctrl Pts',(2.8873936575018,30.1123252029223,56.6622261240094));
#106754=CARTESIAN_POINT('Ctrl Pts',(2.88896372817565,30.0893888561556,56.6636719991686));
#106755=CARTESIAN_POINT('Ctrl Pts',(2.89003051600365,30.073951350422,56.6644296451507));
#106756=CARTESIAN_POINT('Ctrl Pts',(2.89841483180061,29.953590291132,56.6686590687371));
#106757=CARTESIAN_POINT('Ctrl Pts',(2.90611038012386,29.8485695373917,56.6624206311296));
#106758=CARTESIAN_POINT('Ctrl Pts',(2.92159852329018,29.6380276938933,56.6297900808525));
#106759=CARTESIAN_POINT('Ctrl Pts',(2.92934586780103,29.5330599040482,56.6028768622299));
#106760=CARTESIAN_POINT('Ctrl Pts',(2.93825155730654,29.411100299962,56.558595750202));
#106761=CARTESIAN_POINT('Ctrl Pts',(2.93972285830505,29.3909200051703,56.5508208166785));
#106762=CARTESIAN_POINT('Ctrl Pts',(2.94200735171948,29.3595505069973,56.5380281442608));
#106763=CARTESIAN_POINT('Ctrl Pts',(2.94282933771966,29.3482562028332,56.5332762837722));
#106764=CARTESIAN_POINT('Ctrl Pts',(2.94435911114239,29.3272281004076,56.5241547753734));
#106765=CARTESIAN_POINT('Ctrl Pts',(2.9450678807507,29.3174819320897,56.5198154178061));
#106766=CARTESIAN_POINT('Ctrl Pts',(2.94665117543704,29.2957073454677,56.5098688544217));
#106767=CARTESIAN_POINT('Ctrl Pts',(2.94752390959784,29.2837028001406,56.5042109025053));
#106768=CARTESIAN_POINT('Ctrl Pts',(2.95013865196282,29.2477457558812,56.4867356372854));
#106769=CARTESIAN_POINT('Ctrl Pts',(2.95186564912727,29.2240078698965,56.4744848744385));
#106770=CARTESIAN_POINT('Ctrl Pts',(2.96293133879509,29.0723255020617,56.3915256328562));
#106771=CARTESIAN_POINT('Ctrl Pts',(2.97164640739505,28.9538721806745,56.3048145778868));
#106772=CARTESIAN_POINT('Ctrl Pts',(2.98431526781305,28.8054976525151,56.1628505146025));
#106773=CARTESIAN_POINT('Ctrl Pts',(2.98801594309327,28.7649582031302,56.1196997227499));
#106774=CARTESIAN_POINT('Ctrl Pts',(2.99283557954543,28.717109766335,56.0630026220432));
#106775=CARTESIAN_POINT('Ctrl Pts',(2.99382105457645,28.7075719127845,56.0513855272244));
#106776=CARTESIAN_POINT('Ctrl Pts',(2.99531041724624,28.6935479008493,56.0338250913653));
#106777=CARTESIAN_POINT('Ctrl Pts',(2.9958063029131,28.6889419930898,56.027977774141));
#106778=CARTESIAN_POINT('Ctrl Pts',(2.99670710456393,28.680692824441,56.0173596263555));
#106779=CARTESIAN_POINT('Ctrl Pts',(2.99711105929862,28.6770359548356,56.0125997061588));
#106780=CARTESIAN_POINT('Ctrl Pts',(2.99802706545986,28.6688390849313,56.0018101535062));
#106781=CARTESIAN_POINT('Ctrl Pts',(2.9985401081394,28.6643143205601,55.9957694138972));
#106782=CARTESIAN_POINT('Ctrl Pts',(3.00011933530606,28.650583307638,55.9771759901348));
#106783=CARTESIAN_POINT('Ctrl Pts',(3.00119392854953,28.6415121174535,55.964525248448));
#106784=CARTESIAN_POINT('Ctrl Pts',(3.00944127222337,28.5738467964191,55.867310405856));
#106785=CARTESIAN_POINT('Ctrl Pts',(3.01697666831238,28.5230264519377,55.7776156329591));
#106786=CARTESIAN_POINT('Ctrl Pts',(3.03262326792838,28.434707796143,55.5814032477442));
#106787=CARTESIAN_POINT('Ctrl Pts',(3.04067575700009,28.3990762155491,55.4745746203949));
#106788=CARTESIAN_POINT('Ctrl Pts',(3.04976801332803,28.3700047520245,55.3450885213731));
#106789=CARTESIAN_POINT('Ctrl Pts',(3.05115157336887,28.3659087435678,55.3251406240996));
#106790=CARTESIAN_POINT('Ctrl Pts',(3.05333118837893,28.3599839285205,55.2933376427417));
#106791=CARTESIAN_POINT('Ctrl Pts',(3.05413475010823,28.3579157569915,55.2815298194306));
#106792=CARTESIAN_POINT('Ctrl Pts',(3.055648314555,28.3542421066987,55.2591361868749));
#106793=CARTESIAN_POINT('Ctrl Pts',(3.05635909650707,28.3526108872717,55.2485552797859));
#106794=CARTESIAN_POINT('Ctrl Pts',(3.0579709878513,28.3491275371512,55.2244176950384));
#106795=CARTESIAN_POINT('Ctrl Pts',(3.0588700172328,28.3473401740332,55.2108523384027));
#106796=CARTESIAN_POINT('Ctrl Pts',(3.06121659479051,28.3430876175583,55.1751902723923));
#106797=CARTESIAN_POINT('Ctrl Pts',(3.06265558152968,28.3408972216891,55.1530631240404));
#106798=CARTESIAN_POINT('Ctrl Pts',(3.07364340595797,28.32744332101,54.9823582686439));
#106799=CARTESIAN_POINT('Ctrl Pts',(3.0825251144406,28.3357148773882,54.8329272952165));
#106800=CARTESIAN_POINT('Ctrl Pts',(3.0953890685054,28.3749502571241,54.6280911057452));
#106801=CARTESIAN_POINT('Ctrl Pts',(3.09911265225977,28.3892814806941,54.5702474521909));
#106802=CARTESIAN_POINT('Ctrl Pts',(3.10395979775142,28.4110804312326,54.4988833585535));
#106803=CARTESIAN_POINT('Ctrl Pts',(3.10494816403895,28.4156799775532,54.4845261288192));
#106804=CARTESIAN_POINT('Ctrl Pts',(3.10644104603881,28.4228432903786,54.4631683208464));
#106805=CARTESIAN_POINT('Ctrl Pts',(3.1069375041088,28.4252603851029,54.456118874751));
#106806=CARTESIAN_POINT('Ctrl Pts',(3.10783886624866,28.429709585898,54.4434211225431));
#106807=CARTESIAN_POINT('Ctrl Pts',(3.1082428024251,28.4317250317328,54.4377672614678));
#106808=CARTESIAN_POINT('Ctrl Pts',(3.10915815445181,28.4363405364721,54.4250374720399));
#106809=CARTESIAN_POINT('Ctrl Pts',(3.10967055462556,28.4389580734989,54.417968278697));
#106810=CARTESIAN_POINT('Ctrl Pts',(3.11124582010558,28.4471107606551,54.3964009233395));
#106811=CARTESIAN_POINT('Ctrl Pts',(3.11231703545546,28.4528004126447,54.3819625991251));
#106812=CARTESIAN_POINT('Ctrl Pts',(3.12061211693978,28.4980248061075,54.2717388502146));
#106813=CARTESIAN_POINT('Ctrl Pts',(3.12820411794129,28.5462140142126,54.1797581401613));
#106814=CARTESIAN_POINT('Ctrl Pts',(3.14383534850046,28.6632727544579,53.9994397683538));
#106815=CARTESIAN_POINT('Ctrl Pts',(3.15181898770457,28.7331417194772,53.9123240341774));
#106816=CARTESIAN_POINT('Ctrl Pts',(3.16085896318759,28.8255619578962,53.8181913236632));
#106817=CARTESIAN_POINT('Ctrl Pts',(3.16225249928016,28.840197038981,53.8038254228799));
#106818=CARTESIAN_POINT('Ctrl Pts',(3.1644440570885,28.8638242082639,53.7814742567735));
#106819=CARTESIAN_POINT('Ctrl Pts',(3.16524972770047,28.8726435140325,53.7733102334799));
#106820=CARTESIAN_POINT('Ctrl Pts',(3.16676506993478,28.8894808849447,53.7580588643268));
#106821=CARTESIAN_POINT('Ctrl Pts',(3.16747554454272,28.8974803529654,53.7509519919538));
#106822=CARTESIAN_POINT('Ctrl Pts',(3.16908378019546,28.9158241625205,53.7349685661392));
#106823=CARTESIAN_POINT('Ctrl Pts',(3.16997949767706,28.926210167351,53.7261408284813));
#106824=CARTESIAN_POINT('Ctrl Pts',(3.17231120001677,28.9536802011014,53.7033669870436));
#106825=CARTESIAN_POINT('Ctrl Pts',(3.17373880401777,28.970935165951,53.6896306124683));
#106826=CARTESIAN_POINT('Ctrl Pts',(3.18230574952777,29.0769891874961,53.6085901835577));
#106827=CARTESIAN_POINT('Ctrl Pts',(3.18910123354758,29.1720852095538,53.5499893559828));
#106828=CARTESIAN_POINT('Ctrl Pts',(3.20022244779849,29.3359103095552,53.470445641023));
#106829=CARTESIAN_POINT('Ctrl Pts',(3.2045378348824,29.4013876629973,53.4436537849391));
#106830=CARTESIAN_POINT('Ctrl Pts',(3.21049743224233,29.490866766143,53.4135249184435));
#106831=CARTESIAN_POINT('Ctrl Pts',(3.21201219932955,29.5135287978645,53.4064299550166));
#106832=CARTESIAN_POINT('Ctrl Pts',(3.21464760816669,29.5526355101684,53.3950984199941));
#106833=CARTESIAN_POINT('Ctrl Pts',(3.21575731031687,29.5690079807562,53.3906243778192));
#106834=CARTESIAN_POINT('Ctrl Pts',(3.21739724754887,29.5930100407439,53.3844579306685));
#106835=CARTESIAN_POINT('Ctrl Pts',(3.21791692644899,29.6005883092084,53.3825676830527));
#106836=CARTESIAN_POINT('Ctrl Pts',(3.2188038607759,29.6134689097773,53.3794509160738));
#106837=CARTESIAN_POINT('Ctrl Pts',(3.21916955387508,29.618764420622,53.3781969759039));
#106838=CARTESIAN_POINT('Ctrl Pts',(3.220007119421,29.6308567066252,53.3753961051972));
#106839=CARTESIAN_POINT('Ctrl Pts',(3.22047989784708,29.6376569484175,53.373865905105));
#106840=CARTESIAN_POINT('Ctrl Pts',(3.22179789165491,29.6565495628262,53.3697390498291));
#106841=CARTESIAN_POINT('Ctrl Pts',(3.2226479409213,29.6686612668371,53.3672343739002));
#106842=CARTESIAN_POINT('Ctrl Pts',(3.22917445446895,29.7611800149765,53.349173449974));
#106843=CARTESIAN_POINT('Ctrl Pts',(3.23510297296059,29.842599846584,53.3394321656467));
#106844=CARTESIAN_POINT('Ctrl Pts',(3.2453972073933,29.9839539088188,53.3330107847476));
#106845=CARTESIAN_POINT('Ctrl Pts',(3.2497437502269,30.04361661882,53.3335041080862));
#106846=CARTESIAN_POINT('Ctrl Pts',(3.25792115360078,30.1569285241922,53.3405316204381));
#106847=CARTESIAN_POINT('Ctrl Pts',(3.26175709224196,30.2105415118794,53.346477979323));
#106848=CARTESIAN_POINT('Ctrl Pts',(3.26804866122616,30.2995237469021,53.3607464292378));
#106849=CARTESIAN_POINT('Ctrl Pts',(3.27054251608933,30.3350771148501,53.3676426796411));
#106850=CARTESIAN_POINT('Ctrl Pts',(3.27401105181878,30.3849012283676,53.3790037401622));
#106851=CARTESIAN_POINT('Ctrl Pts',(3.27501571520984,30.3993777957766,53.3825095885063));
#106852=CARTESIAN_POINT('Ctrl Pts',(3.27674331498653,30.4243423652611,53.3889109660382));
#106853=CARTESIAN_POINT('Ctrl Pts',(3.27746911128389,30.4348524062334,53.3917159104296));
#106854=CARTESIAN_POINT('Ctrl Pts',(3.27895236015647,30.4563716396816,53.3976853865388));
#106855=CARTESIAN_POINT('Ctrl Pts',(3.27970941238696,30.4673771962034,53.4008609311399));
#106856=CARTESIAN_POINT('Ctrl Pts',(3.28163677980139,30.4954448162457,53.4092740817893));
#106857=CARTESIAN_POINT('Ctrl Pts',(3.2828018047602,30.5124573361096,53.4146728944527));
#106858=CARTESIAN_POINT('Ctrl Pts',(3.28761811353891,30.5829226736348,53.4382875114647));
#106859=CARTESIAN_POINT('Ctrl Pts',(3.29118940451463,30.6355215500645,53.4589425391526));
#106860=CARTESIAN_POINT('Ctrl Pts',(3.30250392432469,30.8011028190942,53.5338881184471));
#106861=CARTESIAN_POINT('Ctrl Pts',(3.30996626207958,30.909032617586,53.5982487361089));
#106862=CARTESIAN_POINT('Ctrl Pts',(3.32066125008828,31.0452831200364,53.701905535497));
#106863=CARTESIAN_POINT('Ctrl Pts',(3.32357878701688,31.0806717960673,53.7312156670767));
#106864=CARTESIAN_POINT('Ctrl Pts',(3.32731472610871,31.1230393696455,53.7693654162959));
#106865=CARTESIAN_POINT('Ctrl Pts',(3.32804645879156,31.1312033393007,53.7768655457425));
#106866=CARTESIAN_POINT('Ctrl Pts',(3.3292246124801,31.1441219706879,53.7889736808378));
#106867=CARTESIAN_POINT('Ctrl Pts',(3.32966722735544,31.1489252291285,53.7935296756392));
#106868=CARTESIAN_POINT('Ctrl Pts',(3.33052191820137,31.1581012955926,53.8023378643225));
#106869=CARTESIAN_POINT('Ctrl Pts',(3.33093366719485,31.1624780971939,53.8065856248699));
#106870=CARTESIAN_POINT('Ctrl Pts',(3.33195040009536,31.1731806683872,53.8170873877078));
#106871=CARTESIAN_POINT('Ctrl Pts',(3.33255740227154,31.1794798064217,53.8233681517258));
#106872=CARTESIAN_POINT('Ctrl Pts',(3.33468528086541,31.2012587371824,53.8454341749122));
#106873=CARTESIAN_POINT('Ctrl Pts',(3.33622399157413,31.2164736499495,53.8614761565749));
#106874=CARTESIAN_POINT('Ctrl Pts',(3.34518700790741,31.3023029519025,53.9556559223591));
#106875=CARTESIAN_POINT('Ctrl Pts',(3.35292833181909,31.3656971655209,54.040043359502));
#106876=CARTESIAN_POINT('Ctrl Pts',(3.3676544003265,31.4717278134838,54.2131591836692));
#106877=CARTESIAN_POINT('Ctrl Pts',(3.37462543029682,31.5153361751184,54.3008124080588));
#106878=CARTESIAN_POINT('Ctrl Pts',(3.38281218895757,31.5588838560674,54.41186580207));
#106879=CARTESIAN_POINT('Ctrl Pts',(3.38427888458028,31.5663637237997,54.4320867391528));
#106880=CARTESIAN_POINT('Ctrl Pts',(3.38655788291962,31.5774717521726,54.464006849123));
#106881=CARTESIAN_POINT('Ctrl Pts',(3.3873789096106,31.5813667661031,54.4756099241933));
#106882=CARTESIAN_POINT('Ctrl Pts',(3.38890780464844,31.5884174094386,54.4974067532732));
#106883=CARTESIAN_POINT('Ctrl Pts',(3.389616644836,31.5916036295338,54.5075898723917));
#106884=CARTESIAN_POINT('Ctrl Pts',(3.39120125897616,31.5985383373874,54.5305239109813));
#106885=CARTESIAN_POINT('Ctrl Pts',(3.39207522842764,31.6022325485948,54.5432905830679));
#106886=CARTESIAN_POINT('Ctrl Pts',(3.39431006211169,31.6113374570936,54.5762269109505));
#106887=CARTESIAN_POINT('Ctrl Pts',(3.39566367665842,31.6165225243874,54.5964569144616));
#106888=CARTESIAN_POINT('Ctrl Pts',(3.40533445059828,31.6511211387637,54.7428365560153));
#106889=CARTESIAN_POINT('Ctrl Pts',(3.41316151932202,31.6661145849942,54.8719377554898));
#106890=CARTESIAN_POINT('Ctrl Pts',(3.42170261966234,31.6659904235466,55.0115057965245));
#106891=CARTESIAN_POINT('Ctrl Pts',(3.42231671609912,31.6658910431593,55.0215291638363));
#106892=CARTESIAN_POINT('Ctrl Pts',(3.42758549390243,31.6642652244521,55.1073626089405));
#106893=CARTESIAN_POINT('Ctrl Pts',(3.43229186060158,31.6576553938596,55.1829784297439));
#106894=CARTESIAN_POINT('Ctrl Pts',(3.4380460691107,31.6440199935811,55.2700096958341));
#106895=CARTESIAN_POINT('Ctrl Pts',(3.43885497469513,31.6419839622348,55.2821269591806));
#106896=CARTESIAN_POINT('Ctrl Pts',(3.44013282772137,31.6385863721852,55.3010631749777));
#106897=CARTESIAN_POINT('Ctrl Pts',(3.44059688965219,31.6373157829344,55.3078982900468));
#106898=CARTESIAN_POINT('Ctrl Pts',(3.44146962565931,31.6348588246095,55.3206700389454));
#106899=CARTESIAN_POINT('Ctrl Pts',(3.4418777237089,31.633682829636,55.3266084165438));
#106900=CARTESIAN_POINT('Ctrl Pts',(3.44284384765443,31.6308349267368,55.340589070502));
#106901=CARTESIAN_POINT('Ctrl Pts',(3.44340335671327,31.6291358758658,55.3486255356502));
#106902=CARTESIAN_POINT('Ctrl Pts',(3.44528687674318,31.623248403358,55.3754898845752));
#106903=CARTESIAN_POINT('Ctrl Pts',(3.44662441249491,31.6187926235885,55.3942567628162));
#106904=CARTESIAN_POINT('Ctrl Pts',(3.44995347821207,31.6070106220397,55.4403076373684));
#106905=CARTESIAN_POINT('Ctrl Pts',(3.45195955689978,31.5993144282699,55.4674902505505));
#106906=CARTESIAN_POINT('Ctrl Pts',(3.45602872890287,31.5824589863616,55.5217225823812));
#106907=CARTESIAN_POINT('Ctrl Pts',(3.45809077358494,31.573290843425,55.5487490034217));
#106908=CARTESIAN_POINT('Ctrl Pts',(3.46016014030872,31.5634377287949,55.5755158279149));
#106909=CARTESIAN_POINT('',(3.22999287141707,31.6660003168857,54.9993964881822));
#106910=CARTESIAN_POINT('Ctrl Pts',(3.26653908718979,31.5634376777881,55.5755159664792));
#106911=CARTESIAN_POINT('Ctrl Pts',(3.26610426703045,31.5657964878847,55.569108059845));
#106912=CARTESIAN_POINT('Ctrl Pts',(3.2656705388314,31.5681160028208,55.5626853798124));
#106913=CARTESIAN_POINT('Ctrl Pts',(3.26185959025895,31.5881978274955,55.5059905195));
#106914=CARTESIAN_POINT('Ctrl Pts',(3.25854924041725,31.6035775375029,55.4549048857212));
#106915=CARTESIAN_POINT('Ctrl Pts',(3.25151260756041,31.631268582732,55.3438786386606));
#106916=CARTESIAN_POINT('Ctrl Pts',(3.24780193291552,31.6427825896574,55.2838223117538));
#106917=CARTESIAN_POINT('Ctrl Pts',(3.23947063478459,31.6610074929674,55.1490576405224));
#106918=CARTESIAN_POINT('Ctrl Pts',(3.23484348653673,31.6660269351427,55.0742640495692));
#106919=CARTESIAN_POINT('Ctrl Pts',(3.22999372004333,31.6659998913039,54.9993981898735));
#106920=CARTESIAN_POINT('Ctrl Pts',(3.22999360673357,31.6659998906711,54.9993964407109));
#106921=CARTESIAN_POINT('Ctrl Pts',(3.22944625435921,31.6659968295913,54.9909469664633));
#106922=CARTESIAN_POINT('Ctrl Pts',(3.22889611782431,31.665929488637,54.9824977945502));
#106923=CARTESIAN_POINT('Ctrl Pts',(3.22781975627913,31.6656734189151,54.9660602298663));
#106924=CARTESIAN_POINT('Ctrl Pts',(3.22729387167398,31.6654914836522,54.9580719856899));
#106925=CARTESIAN_POINT('Ctrl Pts',(3.22635465675499,31.6650663378729,54.9438882199871));
#106926=CARTESIAN_POINT('Ctrl Pts',(3.22594251123523,31.6648459880331,54.9376920993005));
#106927=CARTESIAN_POINT('Ctrl Pts',(3.22514987919618,31.6643579486853,54.9258328877708));
#106928=CARTESIAN_POINT('Ctrl Pts',(3.22476970234351,31.6640959248837,54.9201695956893));
#106929=CARTESIAN_POINT('Ctrl Pts',(3.22394833587324,31.6634701117978,54.9079903461829));
#106930=CARTESIAN_POINT('Ctrl Pts',(3.22350664129181,31.6630969373089,54.9014750657985));
#106931=CARTESIAN_POINT('Ctrl Pts',(3.22233805425277,31.6620133732046,54.8843228801411));
#106932=CARTESIAN_POINT('Ctrl Pts',(3.22160780912958,31.6612391601384,54.8736905120352));
#106933=CARTESIAN_POINT('Ctrl Pts',(3.21836849965964,31.6573778981183,54.8268714064288));
#106934=CARTESIAN_POINT('Ctrl Pts',(3.2158095147202,31.6532102762678,54.7907863561573));
#106935=CARTESIAN_POINT('Ctrl Pts',(3.20797664671837,31.6370635512358,54.6822414682852));
#106936=CARTESIAN_POINT('Ctrl Pts',(3.20261267191694,31.621470453918,54.6104100660507));
#106937=CARTESIAN_POINT('Ctrl Pts',(3.18901679655734,31.5698386859,54.4307483437689));
#106938=CARTESIAN_POINT('Ctrl Pts',(3.18087215203561,31.5274134839663,54.3251238290562));
#106939=CARTESIAN_POINT('Ctrl Pts',(3.17168389567752,31.4650118142507,54.206452432826));
#106940=CARTESIAN_POINT('Ctrl Pts',(3.17028884243349,31.4551229572515,54.1884615832385));
#106941=CARTESIAN_POINT('Ctrl Pts',(3.16809563275909,31.438920359593,54.16023296824));
#106942=CARTESIAN_POINT('Ctrl Pts',(3.16728980407335,31.4328242176489,54.1498733957147));
#106943=CARTESIAN_POINT('Ctrl Pts',(3.16577459790435,31.4210926113148,54.1304218365937));
#106944=CARTESIAN_POINT('Ctrl Pts',(3.16506441320801,31.4154806941634,54.1213164359299));
#106945=CARTESIAN_POINT('Ctrl Pts',(3.16345742492406,31.4025264738042,54.1007442727398));
#106946=CARTESIAN_POINT('Ctrl Pts',(3.16256265628449,31.3951304473644,54.0893121139253));
#106947=CARTESIAN_POINT('Ctrl Pts',(3.16023468771261,31.3754145265064,54.0596408888545));
#106948=CARTESIAN_POINT('Ctrl Pts',(3.15880982704021,31.3628716677318,54.0415526790033));
#106949=CARTESIAN_POINT('Ctrl Pts',(3.15015445315678,31.283853656419,53.9322889758917));
#106950=CARTESIAN_POINT('Ctrl Pts',(3.14327792943381,31.2086154424092,53.8478110738396));
#106951=CARTESIAN_POINT('Ctrl Pts',(3.13044718459681,31.0537023702456,53.7058885608238));
#106952=CARTESIAN_POINT('Ctrl Pts',(3.12451208724406,30.9763924990241,53.6466095846522));
#106953=CARTESIAN_POINT('Ctrl Pts',(3.11725516956851,30.882278959991,53.5867253749865));
#106954=CARTESIAN_POINT('Ctrl Pts',(3.11631468519567,30.870091269779,53.5791894998109));
#106955=CARTESIAN_POINT('Ctrl Pts',(3.11488026934627,30.8515478539379,53.5680518213126));
#106956=CARTESIAN_POINT('Ctrl Pts',(3.11439349757838,30.845262795309,53.5643328603626));
#106957=CARTESIAN_POINT('Ctrl Pts',(3.11350154655221,30.8337650922628,53.5576311712793));
#106958=CARTESIAN_POINT('Ctrl Pts',(3.11309722308082,30.8285605044065,53.5546351484413));
#106959=CARTESIAN_POINT('Ctrl Pts',(3.11217037658896,30.8166463855088,53.5478622787772));
#106960=CARTESIAN_POINT('Ctrl Pts',(3.11164674768942,30.8099268230292,53.544103775739));
#106961=CARTESIAN_POINT('Ctrl Pts',(3.11000083133167,30.7888334572667,53.5324966835846));
#106962=CARTESIAN_POINT('Ctrl Pts',(3.1088691140153,30.7743703147326,53.5248136481837));
#106963=CARTESIAN_POINT('Ctrl Pts',(3.10208074778319,30.687724397871,53.4804113270766));
#106964=CARTESIAN_POINT('Ctrl Pts',(3.09620202750226,30.6130613270886,53.4487850172177));
#106965=CARTESIAN_POINT('Ctrl Pts',(3.08494313061414,30.4666078721951,53.3989791149915));
#106966=CARTESIAN_POINT('Ctrl Pts',(3.07957728196145,30.3953096316626,53.3799004998563));
#106967=CARTESIAN_POINT('Ctrl Pts',(3.07128440049202,30.2813036242831,53.3573713465668));
#106968=CARTESIAN_POINT('Ctrl Pts',(3.06828938676094,30.2393263287214,53.3507322740104));
#106969=CARTESIAN_POINT('Ctrl Pts',(3.06321778836286,30.1667666607243,53.3420855259456));
#106970=CARTESIAN_POINT('Ctrl Pts',(3.06111973650694,30.1362997298789,53.3393031224058));
#106971=CARTESIAN_POINT('Ctrl Pts',(3.05810102127006,30.091825577335,53.3364738224719));
#106972=CARTESIAN_POINT('Ctrl Pts',(3.05715992828005,30.0778685421131,53.3357620991018));
#106973=CARTESIAN_POINT('Ctrl Pts',(3.05550546941852,30.0531747294682,53.3348142051769));
#106974=CARTESIAN_POINT('Ctrl Pts',(3.05478989953064,30.0424416922831,53.3345060807169));
#106975=CARTESIAN_POINT('Ctrl Pts',(3.05329315273818,30.0198850563073,53.3340767200262));
#106976=CARTESIAN_POINT('Ctrl Pts',(3.05251270364678,30.0080615973514,53.3339775472694));
#106977=CARTESIAN_POINT('Ctrl Pts',(3.05044858315771,29.9766359979648,53.3340485130381));
#106978=CARTESIAN_POINT('Ctrl Pts',(3.04917179384185,29.9570358455797,53.3344387229689));
#106979=CARTESIAN_POINT('Ctrl Pts',(3.04257019029153,29.8549561663917,53.3382742283473));
#106980=CARTESIAN_POINT('Ctrl Pts',(3.0374286121493,29.7728050168556,53.3475003235681));
#106981=CARTESIAN_POINT('Ctrl Pts',(3.02620358572786,29.5932013787038,53.3813244962504));
#106982=CARTESIAN_POINT('Ctrl Pts',(3.02017876609559,29.4966152516834,53.4087121705521));
#106983=CARTESIAN_POINT('Ctrl Pts',(3.01212508639738,29.3766796929032,53.4547403165617));
#106984=CARTESIAN_POINT('Ctrl Pts',(3.01033233590518,29.3505420139992,53.4655424937043));
#106985=CARTESIAN_POINT('Ctrl Pts',(3.00726507334515,29.3070480101583,53.4848280240195));
#106986=CARTESIAN_POINT('Ctrl Pts',(3.00600688656322,29.2895408219206,53.4929577791572));
#106987=CARTESIAN_POINT('Ctrl Pts',(3.00418874694282,29.2647901408738,53.5049782779568));
#106988=CARTESIAN_POINT('Ctrl Pts',(3.00364284317889,29.257427364817,53.5086216573862));
#106989=CARTESIAN_POINT('Ctrl Pts',(3.00268894182674,29.2446875114186,53.5150435443472));
#106990=CARTESIAN_POINT('Ctrl Pts',(3.00228247342119,29.2392981416458,53.517797142107));
#106991=CARTESIAN_POINT('Ctrl Pts',(3.00140532337214,29.2277540232609,53.5237749414149));
#106992=CARTESIAN_POINT('Ctrl Pts',(3.00093411632965,29.2216044962385,53.5270082459475));
#106993=CARTESIAN_POINT('Ctrl Pts',(2.9996242585279,29.2046483340678,53.5360593053381));
#106994=CARTESIAN_POINT('Ctrl Pts',(2.99878086378888,29.1938857409914,53.5419580220997));
#106995=CARTESIAN_POINT('Ctrl Pts',(2.99289408307777,29.1197662669068,53.5836525831057));
#106996=CARTESIAN_POINT('Ctrl Pts',(2.98765082980358,29.0587552784197,53.6234436232251));
#106997=CARTESIAN_POINT('Ctrl Pts',(2.98135709746304,28.9894379669817,53.6754196156919));
#106998=CARTESIAN_POINT('Ctrl Pts',(2.98034696811561,28.9784329928107,53.6838884305932));
#106999=CARTESIAN_POINT('Ctrl Pts',(2.97386431526517,28.9085277927202,53.7390886700488));
#107000=CARTESIAN_POINT('Ctrl Pts',(2.96839083863729,28.8527384250328,53.7896276440894));
#107001=CARTESIAN_POINT('Ctrl Pts',(2.9600254768904,28.7713493275451,53.8740586261583));
#107002=CARTESIAN_POINT('Ctrl Pts',(2.95706002226077,28.7433035656484,53.9054494014103));
#107003=CARTESIAN_POINT('Ctrl Pts',(2.95203237405372,28.697109961684,53.9612718610856));
#107004=CARTESIAN_POINT('Ctrl Pts',(2.94994921517149,28.678387924918,53.9851993642137));
#107005=CARTESIAN_POINT('Ctrl Pts',(2.94694762549407,28.6520443636831,54.0208341053681));
#107006=CARTESIAN_POINT('Ctrl Pts',(2.94600909136777,28.6438999581359,54.0321451846255));
#107007=CARTESIAN_POINT('Ctrl Pts',(2.9443575149301,28.6297368585232,54.0523449436327));
#107008=CARTESIAN_POINT('Ctrl Pts',(2.9436422946478,28.6236604205636,54.0611919503485));
#107009=CARTESIAN_POINT('Ctrl Pts',(2.94214469650621,28.611060010307,54.0799228636113));
#107010=CARTESIAN_POINT('Ctrl Pts',(2.94136306172215,28.6045550567397,54.0898188892371));
#107011=CARTESIAN_POINT('Ctrl Pts',(2.93929208467216,28.5875167798997,54.1163514063674));
#107012=CARTESIAN_POINT('Ctrl Pts',(2.93800970825652,28.5771717322979,54.1331070089019));
#107013=CARTESIAN_POINT('Ctrl Pts',(2.93117728150452,28.5232266526374,54.2240486481736));
#107014=CARTESIAN_POINT('Ctrl Pts',(2.92582806964664,28.4851239674327,54.3013489112153));
#107015=CARTESIAN_POINT('Ctrl Pts',(2.91458588276082,28.4170642128829,54.4714959253409));
#107016=CARTESIAN_POINT('Ctrl Pts',(2.90873407783388,28.3889358859035,54.5647156968043));
#107017=CARTESIAN_POINT('Ctrl Pts',(2.90088882838858,28.3633995412924,54.6871535286934));
#107018=CARTESIAN_POINT('Ctrl Pts',(2.89911969706786,28.3583916357568,54.7145954093701));
#107019=CARTESIAN_POINT('Ctrl Pts',(2.89608879704332,28.351117483773,54.7610279685365));
#107020=CARTESIAN_POINT('Ctrl Pts',(2.8948428542756,28.3484850138574,54.7799560068179));
#107021=CARTESIAN_POINT('Ctrl Pts',(2.89303935152854,28.3451912035126,54.8070471412584));
#107022=CARTESIAN_POINT('Ctrl Pts',(2.89249553452392,28.3442634723556,54.8151771044148));
#107023=CARTESIAN_POINT('Ctrl Pts',(2.89154398184076,28.3427542405423,54.8293275797033));
#107024=CARTESIAN_POINT('Ctrl Pts',(2.89113775191381,28.3421455742041,54.8353449552002));
#107025=CARTESIAN_POINT('Ctrl Pts',(2.89025956765069,28.3409063533848,54.8483002949875));
#107026=CARTESIAN_POINT('Ctrl Pts',(2.88978707286325,28.340286552025,54.8552388349163));
#107027=CARTESIAN_POINT('Ctrl Pts',(2.88847022316319,28.3386881860321,54.8744941526137));
#107028=CARTESIAN_POINT('Ctrl Pts',(2.88762104546219,28.3378031218823,54.8868179483406));
#107029=CARTESIAN_POINT('Ctrl Pts',(2.88112077333767,28.3321196560862,54.9805342419203));
#107030=CARTESIAN_POINT('Ctrl Pts',(2.87521974773726,28.3331656720694,55.0621623683281));
#107031=CARTESIAN_POINT('Ctrl Pts',(2.86495103515304,28.3453134726731,55.2027938404641));
#107032=CARTESIAN_POINT('Ctrl Pts',(2.86060273911687,28.3536330663101,55.2618954082176));
#107033=CARTESIAN_POINT('Ctrl Pts',(2.85240635342677,28.375515817583,55.3735472215677));
#107034=CARTESIAN_POINT('Ctrl Pts',(2.84855362817948,28.3885110195655,55.4261344838264));
#107035=CARTESIAN_POINT('Ctrl Pts',(2.84223842724568,28.4144620106634,55.5127801267044));
#107036=CARTESIAN_POINT('Ctrl Pts',(2.83973733851493,28.4260137041177,55.5472126344215));
#107037=CARTESIAN_POINT('Ctrl Pts',(2.83626087343051,28.4438829990229,55.5952126432583));
#107038=CARTESIAN_POINT('Ctrl Pts',(2.83525532147062,28.4492711499528,55.6091126908437));
#107039=CARTESIAN_POINT('Ctrl Pts',(2.8335268665955,28.458912294769,55.6330268485495));
#107040=CARTESIAN_POINT('Ctrl Pts',(2.83280109276724,28.4630780702189,55.6430748771489));
#107041=CARTESIAN_POINT('Ctrl Pts',(2.83140944006814,28.4712915149809,55.6623502656591));
#107042=CARTESIAN_POINT('Ctrl Pts',(2.83074312094827,28.4753250595583,55.6715830850484));
#107043=CARTESIAN_POINT('Ctrl Pts',(2.82898675566258,28.4862232765387,55.6959248624893));
#107044=CARTESIAN_POINT('Ctrl Pts',(2.82790161495484,28.4932304757536,55.7109690682439));
#107045=CARTESIAN_POINT('Ctrl Pts',(2.82389877873612,28.5200840665376,55.7664417663029));
#107046=CARTESIAN_POINT('Ctrl Pts',(2.82102973601192,28.5413433076273,55.8061670747001));
#107047=CARTESIAN_POINT('Ctrl Pts',(2.81110653575018,28.6214991568649,55.9423691996979));
#107048=CARTESIAN_POINT('Ctrl Pts',(2.80431620736474,28.688567738787,56.0336683329275));
#107049=CARTESIAN_POINT('Ctrl Pts',(2.79442207206462,28.7964541714676,56.1529624923979));
#107050=CARTESIAN_POINT('Ctrl Pts',(2.79145131585022,28.8300574893814,56.1870463186561));
#107051=CARTESIAN_POINT('Ctrl Pts',(2.78720342425234,28.8788932887346,56.2324901074083));
#107052=CARTESIAN_POINT('Ctrl Pts',(2.78599026920631,28.8929252320497,56.2451094401012));
#107053=CARTESIAN_POINT('Ctrl Pts',(2.783834156443,28.9179382289738,56.2668472426611));
#107054=CARTESIAN_POINT('Ctrl Pts',(2.78289752377072,28.9288279736686,56.2760682071113));
#107055=CARTESIAN_POINT('Ctrl Pts',(2.78146781171153,28.9454585764189,56.28978740258));
#107056=CARTESIAN_POINT('Ctrl Pts',(2.78098182185311,28.9511130561891,56.2943899458835));
#107057=CARTESIAN_POINT('Ctrl Pts',(2.780090597682,28.9614804595104,56.3027161009907));
#107058=CARTESIAN_POINT('Ctrl Pts',(2.77968620990052,28.966183547632,56.3064515356395));
#107059=CARTESIAN_POINT('Ctrl Pts',(2.77875829834379,28.976973031557,56.314926357589));
#107060=CARTESIAN_POINT('Ctrl Pts',(2.77823365791272,28.9830721907153,56.3196489415116));
#107061=CARTESIAN_POINT('Ctrl Pts',(2.77658132671932,29.0022841383563,56.3343124925949));
#107062=CARTESIAN_POINT('Ctrl Pts',(2.77544410510628,29.0155110958333,56.3441013039572));
#107063=CARTESIAN_POINT('Ctrl Pts',(2.76848716838464,29.0965746376666,56.4022551531613));
#107064=CARTESIAN_POINT('Ctrl Pts',(2.76243293500468,29.1678102502294,56.4456675084561));
#107065=CARTESIAN_POINT('Ctrl Pts',(2.74992033862268,29.3208844366412,56.5238793235253));
#107066=CARTESIAN_POINT('Ctrl Pts',(2.74348287288277,29.4028809997553,56.5578375837998));
#107067=CARTESIAN_POINT('Ctrl Pts',(2.73373856018003,29.5341394610491,56.6003013130221));
#107068=CARTESIAN_POINT('Ctrl Pts',(2.73031112311749,29.5817381565389,56.6133964875471));
#107069=CARTESIAN_POINT('Ctrl Pts',(2.72581910047962,29.64605340353,56.6280521815794));
#107070=CARTESIAN_POINT('Ctrl Pts',(2.72469529579295,29.6623091435252,56.6315014616292));
#107071=CARTESIAN_POINT('Ctrl Pts',(2.72282713652296,29.6896017220355,56.6368672209045));
#107072=CARTESIAN_POINT('Ctrl Pts',(2.72207860831648,29.7006108758323,56.6389165789433));
#107073=CARTESIAN_POINT('Ctrl Pts',(2.72060770965235,29.7223859096299,56.6427432713776));
#107074=CARTESIAN_POINT('Ctrl Pts',(2.71988519772299,29.7331502299482,56.6445261471513));
#107075=CARTESIAN_POINT('Ctrl Pts',(2.71829434589841,29.7569973567743,56.6482355906932));
#107076=CARTESIAN_POINT('Ctrl Pts',(2.71742760742161,29.7700872368508,56.6501124158597));
#107077=CARTESIAN_POINT('Ctrl Pts',(2.71487975612785,29.8088381245535,56.655198434563));
#107078=CARTESIAN_POINT('Ctrl Pts',(2.71321229972178,29.8345537499226,56.6579663365107));
#107079=CARTESIAN_POINT('Ctrl Pts',(2.70239519965883,30.0033581612133,56.672168699889));
#107080=CARTESIAN_POINT('Ctrl Pts',(2.69383560305068,30.1473400697987,56.6656683525366));
#107081=CARTESIAN_POINT('Ctrl Pts',(2.68230533942275,30.3313663860346,56.633287556543));
#107082=CARTESIAN_POINT('Ctrl Pts',(2.67960485524833,30.373711324652,56.6241216907912));
#107083=CARTESIAN_POINT('Ctrl Pts',(2.67518111768609,30.4408283217483,56.6068299612183));
#107084=CARTESIAN_POINT('Ctrl Pts',(2.67349910458422,30.4658516583023,56.5997544148883));
#107085=CARTESIAN_POINT('Ctrl Pts',(2.67118053179044,30.4994914333947,56.5893863556519));
#107086=CARTESIAN_POINT('Ctrl Pts',(2.67057064858865,30.5082625215215,56.5866032519627));
#107087=CARTESIAN_POINT('Ctrl Pts',(2.66954182784076,30.5229191861294,56.5818186262539));
#107088=CARTESIAN_POINT('Ctrl Pts',(2.66912514071762,30.5288175982171,56.5798565085947));
#107089=CARTESIAN_POINT('Ctrl Pts',(2.6683206113678,30.5401305370615,56.5760227859248));
#107090=CARTESIAN_POINT('Ctrl Pts',(2.66793309463653,30.5455466087627,56.5741561911006));
#107091=CARTESIAN_POINT('Ctrl Pts',(2.66687209972316,30.5602886939326,56.5689902613267));
#107092=CARTESIAN_POINT('Ctrl Pts',(2.66619552454134,30.569594939344,56.5656357985697));
#107093=CARTESIAN_POINT('Ctrl Pts',(2.6635033370614,30.6062756534328,56.5520438135286));
#107094=CARTESIAN_POINT('Ctrl Pts',(2.6614557153734,30.6334069519871,56.5411701896093));
#107095=CARTESIAN_POINT('Ctrl Pts',(2.6515659254076,30.7614462791947,56.4859029450022));
#107096=CARTESIAN_POINT('Ctrl Pts',(2.64344117357296,30.8580676792771,56.4322804830139));
#107097=CARTESIAN_POINT('Ctrl Pts',(2.63127095580434,30.996582925341,56.3363284610601));
#107098=CARTESIAN_POINT('Ctrl Pts',(2.62711151325164,31.0427120272375,56.300655238638));
#107099=CARTESIAN_POINT('Ctrl Pts',(2.62036560635973,31.1158043504782,56.2377370993233));
#107100=CARTESIAN_POINT('Ctrl Pts',(2.61773318828583,31.1438658827417,56.2118513631203));
#107101=CARTESIAN_POINT('Ctrl Pts',(2.61410981907972,31.1818154865199,56.1743503280618));
#107102=CARTESIAN_POINT('Ctrl Pts',(2.6130851363498,31.1924693439305,56.1635305872637));
#107103=CARTESIAN_POINT('Ctrl Pts',(2.61133433434729,31.2105319151769,56.1446780458907));
#107104=CARTESIAN_POINT('Ctrl Pts',(2.61060514115145,31.218012096855,56.1367153945103));
#107105=CARTESIAN_POINT('Ctrl Pts',(2.60921397460609,31.2321976134097,56.1213141018225));
#107106=CARTESIAN_POINT('Ctrl Pts',(2.60855149694907,31.238915234735,56.113887481748));
#107107=CARTESIAN_POINT('Ctrl Pts',(2.606821103123,31.2563589197377,56.0942496994622));
#107108=CARTESIAN_POINT('Ctrl Pts',(2.60575781323695,31.2669741422331,56.08194116913));
#107109=CARTESIAN_POINT('Ctrl Pts',(2.60193832302589,31.3047017734345,56.0368785012215));
#107110=CARTESIAN_POINT('Ctrl Pts',(2.59922496084412,31.3307392569159,56.003243361325));
#107111=CARTESIAN_POINT('Ctrl Pts',(2.58929244575557,31.4225128198616,55.8748211975686));
#107112=CARTESIAN_POINT('Ctrl Pts',(2.58236290164678,31.4796386600055,55.7742899947083));
#107113=CARTESIAN_POINT('Ctrl Pts',(2.57321247415541,31.5393658010715,55.6379893698703));
#107114=CARTESIAN_POINT('Ctrl Pts',(2.5711402764649,31.5518752793647,55.6069261964945));
#107115=CARTESIAN_POINT('Ctrl Pts',(2.56903902087732,31.5634376730794,55.5755159792709));
#107116=CARTESIAN_POINT('Origin',(5.,30.,55.));
#107117=CARTESIAN_POINT('',(1.86810672180998,31.5634374966623,55.5755164585225));
#107118=CARTESIAN_POINT('',(2.06220431895159,31.5634376782779,55.5755159651488));
#107119=CARTESIAN_POINT('',(5.,31.5634376782623,55.5755159651912));
#107120=CARTESIAN_POINT('',(2.72303746985885,31.6659995411549,54.9999657602353));
#107121=CARTESIAN_POINT('Ctrl Pts',(2.06220431895159,31.5634376782779,55.5755159651488));
#107122=CARTESIAN_POINT('Ctrl Pts',(2.06232540429763,31.5627902658092,55.5772747157451));
#107123=CARTESIAN_POINT('Ctrl Pts',(2.06244639919516,31.5621398792575,55.5790323912606));
#107124=CARTESIAN_POINT('Ctrl Pts',(2.0692563660251,31.5253396178637,55.6779721330753));
#107125=CARTESIAN_POINT('Ctrl Pts',(2.07563303263128,31.4801978116672,55.7715732829012));
#107126=CARTESIAN_POINT('Ctrl Pts',(2.08880065368226,31.368895752159,55.956129126645));
#107127=CARTESIAN_POINT('Ctrl Pts',(2.09555586961352,31.3016663470947,56.0458088321837));
#107128=CARTESIAN_POINT('Ctrl Pts',(2.10378745721772,31.2158931193864,56.1390266486023));
#107129=CARTESIAN_POINT('Ctrl Pts',(2.10476405948136,31.2056632308649,56.1498495206366));
#107130=CARTESIAN_POINT('Ctrl Pts',(2.10624261757951,31.1901238226439,56.1658543175442));
#107131=CARTESIAN_POINT('Ctrl Pts',(2.10673674116683,31.1849222201491,56.1711406106491));
#107132=CARTESIAN_POINT('Ctrl Pts',(2.10763582711352,31.175446637847,56.180642723389));
#107133=CARTESIAN_POINT('Ctrl Pts',(2.10803984872027,31.1711849345059,56.1848704084022));
#107134=CARTESIAN_POINT('Ctrl Pts',(2.1089579113828,31.1614929324864,56.1943816683135));
#107135=CARTESIAN_POINT('Ctrl Pts',(2.10947296534857,31.1560494206872,56.1996512547932));
#107136=CARTESIAN_POINT('Ctrl Pts',(2.11106463315109,31.1392031375439,56.2157381499317));
#107137=CARTESIAN_POINT('Ctrl Pts',(2.11214984141663,31.1276834487795,56.2264310141797));
#107138=CARTESIAN_POINT('Ctrl Pts',(2.11778809318652,31.0675774153764,56.2806601597612));
#107139=CARTESIAN_POINT('Ctrl Pts',(2.12248677020479,31.0166194999587,56.3214745987046));
#107140=CARTESIAN_POINT('Ctrl Pts',(2.13556736520961,30.8696443067331,56.4256517293417));
#107141=CARTESIAN_POINT('Ctrl Pts',(2.14397173822651,30.7692440274854,56.4822394713103));
#107142=CARTESIAN_POINT('Ctrl Pts',(2.15507110839096,30.624442798128,56.5451438230635));
#107143=CARTESIAN_POINT('Ctrl Pts',(2.1580434821902,30.5844267309309,56.5607191329328));
#107144=CARTESIAN_POINT('Ctrl Pts',(2.16207539005294,30.5284319188495,56.5800575279464));
#107145=CARTESIAN_POINT('Ctrl Pts',(2.16317814180095,30.512935607371,56.5851558850938));
#107146=CARTESIAN_POINT('Ctrl Pts',(2.16494665405738,30.4877970899146,56.5930193128866));
#107147=CARTESIAN_POINT('Ctrl Pts',(2.16561701565783,30.4782007523768,56.5959262452181));
#107148=CARTESIAN_POINT('Ctrl Pts',(2.16701157104049,30.4580993054746,56.6018178032274));
#107149=CARTESIAN_POINT('Ctrl Pts',(2.16773520592432,30.4475898883431,56.6047861383744));
#107150=CARTESIAN_POINT('Ctrl Pts',(2.1694543836726,30.4224394307187,56.6116234765641));
#107151=CARTESIAN_POINT('Ctrl Pts',(2.17044679570398,30.4077731709646,56.6153966598869));
#107152=CARTESIAN_POINT('Ctrl Pts',(2.17389927620722,30.3562599329835,56.6279031612635));
#107153=CARTESIAN_POINT('Ctrl Pts',(2.17632582431559,30.3191669303792,56.6355802197411));
#107154=CARTESIAN_POINT('Ctrl Pts',(2.182362810349,30.225083285305,56.6517293966722));
#107155=CARTESIAN_POINT('Ctrl Pts',(2.18592659607798,30.1678545427402,56.6585228573174));
#107156=CARTESIAN_POINT('Ctrl Pts',(2.19615443991781,30.0015118365955,56.6695686655818));
#107157=CARTESIAN_POINT('Ctrl Pts',(2.20270356128101,29.8922012011302,56.6660843688747));
#107158=CARTESIAN_POINT('Ctrl Pts',(2.21158303835314,29.7532908855624,56.6479233778603));
#107159=CARTESIAN_POINT('Ctrl Pts',(2.21357661494237,29.7226753163071,56.6430482587471));
#107160=CARTESIAN_POINT('Ctrl Pts',(2.21627674049872,29.6822823236471,56.6354551784842));
#107161=CARTESIAN_POINT('Ctrl Pts',(2.21694522979157,29.6723662571569,56.6334975606553));
#107162=CARTESIAN_POINT('Ctrl Pts',(2.21800325380079,29.6568166465546,56.6302804978471));
#107163=CARTESIAN_POINT('Ctrl Pts',(2.21838944968555,29.6511705922984,56.6290817528651));
#107164=CARTESIAN_POINT('Ctrl Pts',(2.21919302385363,29.6394872564652,56.6265376787553));
#107165=CARTESIAN_POINT('Ctrl Pts',(2.21961066290857,29.6334511193051,56.6251880419655));
#107166=CARTESIAN_POINT('Ctrl Pts',(2.22064278062039,29.6186190682315,56.6217848720257));
#107167=CARTESIAN_POINT('Ctrl Pts',(2.22125934184864,29.6098321469426,56.6196933732738));
#107168=CARTESIAN_POINT('Ctrl Pts',(2.22357638913647,29.5770675073683,56.6116125185774));
#107169=CARTESIAN_POINT('Ctrl Pts',(2.22529981193475,29.553208261852,56.6051616082514));
#107170=CARTESIAN_POINT('Ctrl Pts',(2.22987510543446,29.4909791340074,56.5868416629499));
#107171=CARTESIAN_POINT('Ctrl Pts',(2.23275733939101,29.4528803159673,56.5741119254505));
#107172=CARTESIAN_POINT('Ctrl Pts',(2.24419459540176,29.3048255743947,56.5186187630342));
#107173=CARTESIAN_POINT('Ctrl Pts',(2.25285973217857,29.1990648359915,56.4655984032174));
#107174=CARTESIAN_POINT('Ctrl Pts',(2.26476836567766,29.0574037426249,56.3746292807991));
#107175=CARTESIAN_POINT('Ctrl Pts',(2.26827238203317,29.0162710885428,56.345500540494));
#107176=CARTESIAN_POINT('Ctrl Pts',(2.2728789672711,28.9629495293853,56.3039854385422));
#107177=CARTESIAN_POINT('Ctrl Pts',(2.2740429137102,28.9495450536394,56.2932115630105));
#107178=CARTESIAN_POINT('Ctrl Pts',(2.2759592062457,28.9275981007034,56.2750052057164));
#107179=CARTESIAN_POINT('Ctrl Pts',(2.27671619512917,28.9189605493326,56.2676899562755));
#107180=CARTESIAN_POINT('Ctrl Pts',(2.27819882052242,28.9021103634607,56.2531218504513));
#107181=CARTESIAN_POINT('Ctrl Pts',(2.27892464645223,28.8938934120145,56.2458748941433));
#107182=CARTESIAN_POINT('Ctrl Pts',(2.28065894651848,28.8743421507444,56.2282857190393));
#107183=CARTESIAN_POINT('Ctrl Pts',(2.28166414082456,28.8630779233587,56.2178668312642));
#107184=CARTESIAN_POINT('Ctrl Pts',(2.28521842693762,28.8235149853102,56.1802455923551));
#107185=CARTESIAN_POINT('Ctrl Pts',(2.28773119898034,28.7960342589038,56.1521994274092));
#107186=CARTESIAN_POINT('Ctrl Pts',(2.29404930433798,28.7285906386371,56.0783174165078));
#107187=CARTESIAN_POINT('Ctrl Pts',(2.29780172839346,28.6900982352185,56.0312169440984));
#107188=CARTESIAN_POINT('Ctrl Pts',(2.30694124963367,28.6021546988718,55.9107130399362));
#107189=CARTESIAN_POINT('Ctrl Pts',(2.31227860491102,28.5558135544345,55.8352805588255));
#107190=CARTESIAN_POINT('Ctrl Pts',(2.32057073070602,28.4955949243702,55.7171312077826));
#107191=CARTESIAN_POINT('Ctrl Pts',(2.32338154721156,28.4770912611605,55.6769490630186));
#107192=CARTESIAN_POINT('Ctrl Pts',(2.32701979222787,28.4558797041877,55.6256014025907));
#107193=CARTESIAN_POINT('Ctrl Pts',(2.32776792652735,28.4516572204354,55.6150765988106));
#107194=CARTESIAN_POINT('Ctrl Pts',(2.32896628765358,28.4451203323608,55.5982890483825));
#107195=CARTESIAN_POINT('Ctrl Pts',(2.32941247766674,28.4427354787605,55.592053860074));
#107196=CARTESIAN_POINT('Ctrl Pts',(2.33027364152953,28.4382280083915,55.5800534364318));
#107197=CARTESIAN_POINT('Ctrl Pts',(2.33068828068522,28.436099716354,55.574290554183));
#107198=CARTESIAN_POINT('Ctrl Pts',(2.33170146322498,28.4309999000106,55.5602429418544));
#107199=CARTESIAN_POINT('Ctrl Pts',(2.33230191906718,28.4280620889743,55.5519462500468));
#107200=CARTESIAN_POINT('Ctrl Pts',(2.33448864828343,28.4176626624701,55.5218205916539));
#107201=CARTESIAN_POINT('Ctrl Pts',(2.33609476245566,28.4105892768647,55.4998615833911));
#107202=CARTESIAN_POINT('Ctrl Pts',(2.34689949531901,28.3665701099992,55.3528105654454));
#107203=CARTESIAN_POINT('Ctrl Pts',(2.3565633048541,28.3439692621466,55.2238999392736));
#107204=CARTESIAN_POINT('Ctrl Pts',(2.37140380373618,28.3323620291091,55.0177874383956));
#107205=CARTESIAN_POINT('Ctrl Pts',(2.37676301517307,28.3332859493035,54.9416904755232));
#107206=CARTESIAN_POINT('Ctrl Pts',(2.38328526312079,28.3409599723459,54.846652124405));
#107207=CARTESIAN_POINT('Ctrl Pts',(2.3845966977376,28.3428502146688,54.8274195032873));
#107208=CARTESIAN_POINT('Ctrl Pts',(2.38668986434178,28.3464291687937,54.7965351221572));
#107209=CARTESIAN_POINT('Ctrl Pts',(2.38747810704083,28.3479074508192,54.7848612736721));
#107210=CARTESIAN_POINT('Ctrl Pts',(2.38897950539198,28.3509736779068,54.7625470581729));
#107211=CARTESIAN_POINT('Ctrl Pts',(2.38969326231711,28.3525412411101,54.7519045394426));
#107212=CARTESIAN_POINT('Ctrl Pts',(2.39133541711911,28.3564020907914,54.7273448410855));
#107213=CARTESIAN_POINT('Ctrl Pts',(2.39226143663871,28.358769272765,54.713439983484));
#107214=CARTESIAN_POINT('Ctrl Pts',(2.39522661232573,28.3669611969427,54.6687578782081));
#107215=CARTESIAN_POINT('Ctrl Pts',(2.3972439680344,28.3734775612873,54.6381132316702));
#107216=CARTESIAN_POINT('Ctrl Pts',(2.40866426114851,28.4157197191725,54.4637803802679));
#107217=CARTESIAN_POINT('Ctrl Pts',(2.41745314600417,28.4696054994871,54.3251910621148));
#107218=CARTESIAN_POINT('Ctrl Pts',(2.43006580999499,28.5678372695841,54.147044230671));
#107219=CARTESIAN_POINT('Ctrl Pts',(2.43355478808953,28.5969805827967,54.0999117734772));
#107220=CARTESIAN_POINT('Ctrl Pts',(2.43796010627278,28.6352253575784,54.0444424581536));
#107221=CARTESIAN_POINT('Ctrl Pts',(2.43875089438252,28.6421442394223,54.0346359477472));
#107222=CARTESIAN_POINT('Ctrl Pts',(2.44000179015747,28.6531593556398,54.0193763319056));
#107223=CARTESIAN_POINT('Ctrl Pts',(2.44045723538463,28.6571843152702,54.0138719492775));
#107224=CARTESIAN_POINT('Ctrl Pts',(2.44132385619027,28.6648672601333,54.0034992989771));
#107225=CARTESIAN_POINT('Ctrl Pts',(2.4417345686675,28.6685182948526,53.9986261716564));
#107226=CARTESIAN_POINT('Ctrl Pts',(2.44272092878818,28.6773113839332,53.9870229219868));
#107227=CARTESIAN_POINT('Ctrl Pts',(2.44329824605438,28.6824781531593,53.9803118559885));
#107228=CARTESIAN_POINT('Ctrl Pts',(2.4453090611323,28.7005511090837,53.9572037530578));
#107229=CARTESIAN_POINT('Ctrl Pts',(2.44675858528434,28.7137134583588,53.9410107333393));
#107230=CARTESIAN_POINT('Ctrl Pts',(2.45043444918533,28.7475038916599,53.9009994854796));
#107231=CARTESIAN_POINT('Ctrl Pts',(2.45267918224455,28.7685096749546,53.8775117026402));
#107232=CARTESIAN_POINT('Ctrl Pts',(2.46441336530542,28.880742763951,53.7589614976529));
#107233=CARTESIAN_POINT('Ctrl Pts',(2.47414013539612,28.9823624478311,53.674355286441));
#107234=CARTESIAN_POINT('Ctrl Pts',(2.48702869590481,29.135186787656,53.5751501738372));
#107235=CARTESIAN_POINT('Ctrl Pts',(2.49053665606153,29.1787119961823,53.5496256177514));
#107236=CARTESIAN_POINT('Ctrl Pts',(2.49514743340021,29.2385505214296,53.5180935960251));
#107237=CARTESIAN_POINT('Ctrl Pts',(2.49631177454217,29.2538923896594,53.510310310537));
#107238=CARTESIAN_POINT('Ctrl Pts',(2.49822853941949,29.2795255501322,53.4978013773415));
#107239=CARTESIAN_POINT('Ctrl Pts',(2.49898561064752,29.2897490759343,53.4929406877568));
#107240=CARTESIAN_POINT('Ctrl Pts',(2.50046826964479,29.309962594973,53.4835817236322));
#107241=CARTESIAN_POINT('Ctrl Pts',(2.50119404805641,29.3199489719083,53.4790770505477));
#107242=CARTESIAN_POINT('Ctrl Pts',(2.50292802448296,29.3440226492828,53.4685023717036));
#107243=CARTESIAN_POINT('Ctrl Pts',(2.50393294586499,29.3581509286866,53.462527702485));
#107244=CARTESIAN_POINT('Ctrl Pts',(2.50748502761936,29.4086913844414,53.4419729106831));
#107245=CARTESIAN_POINT('Ctrl Pts',(2.50999593016234,29.4455350909037,53.4284837475064));
#107246=CARTESIAN_POINT('Ctrl Pts',(2.5163078623732,29.540533303779,53.397460763133));
#107247=CARTESIAN_POINT('Ctrl Pts',(2.52005612543067,29.5992335025666,53.3817822557363));
#107248=CARTESIAN_POINT('Ctrl Pts',(2.52918028931319,29.7450012008427,53.3512693465073));
#107249=CARTESIAN_POINT('Ctrl Pts',(2.53450661555806,29.8326348764367,53.3400829932201));
#107250=CARTESIAN_POINT('Ctrl Pts',(2.54280178006679,29.9651737470456,53.3337700469263));
#107251=CARTESIAN_POINT('Ctrl Pts',(2.54562869825601,30.0096735549496,53.3334344312139));
#107252=CARTESIAN_POINT('Ctrl Pts',(2.54928513062462,30.0654805395876,53.3352485791749));
#107253=CARTESIAN_POINT('Ctrl Pts',(2.55003437755436,30.0768276500641,53.3357336484546));
#107254=CARTESIAN_POINT('Ctrl Pts',(2.55123410948158,30.094838715699,53.3366881728324));
#107255=CARTESIAN_POINT('Ctrl Pts',(2.55168054181886,30.1015065726278,53.3370817734519));
#107256=CARTESIAN_POINT('Ctrl Pts',(2.55254183077088,30.1143006228662,53.3379142350946));
#107257=CARTESIAN_POINT('Ctrl Pts',(2.55295634921271,30.1204270113956,53.3383468917561));
#107258=CARTESIAN_POINT('Ctrl Pts',(2.55396874729597,30.1353172514732,53.3394812437472));
#107259=CARTESIAN_POINT('Ctrl Pts',(2.55456853233412,30.1440781362252,53.340218453983));
#107260=CARTESIAN_POINT('Ctrl Pts',(2.55674998041512,30.1757381218518,53.3431351197193));
#107261=CARTESIAN_POINT('Ctrl Pts',(2.55835136365921,30.198596189258,53.3457193275088));
#107262=CARTESIAN_POINT('Ctrl Pts',(2.57021060639035,30.3655949302287,53.3681100971558));
#107263=CARTESIAN_POINT('Ctrl Pts',(2.58103335778621,30.5066440734105,53.4062496758576));
#107264=CARTESIAN_POINT('Ctrl Pts',(2.59589384632307,30.698864366677,53.4863682291498));
#107265=CARTESIAN_POINT('Ctrl Pts',(2.60028874690668,30.7553727954231,53.5137610596324));
#107266=CARTESIAN_POINT('Ctrl Pts',(2.6058376094995,30.8263475215815,53.5532633359977));
#107267=CARTESIAN_POINT('Ctrl Pts',(2.60708996396829,30.8423377164095,53.5625145494312));
#107268=CARTESIAN_POINT('Ctrl Pts',(2.60911224063516,30.8681017366143,53.5779980295346));
#107269=CARTESIAN_POINT('Ctrl Pts',(2.60988789851,30.8779698390797,53.5840694923429));
#107270=CARTESIAN_POINT('Ctrl Pts',(2.61138052753846,30.8969282597795,53.5960082873435));
#107271=CARTESIAN_POINT('Ctrl Pts',(2.61209794429056,30.9060263082142,53.6018621775289));
#107272=CARTESIAN_POINT('Ctrl Pts',(2.6137710775707,30.927206093141,53.615783295755));
#107273=CARTESIAN_POINT('Ctrl Pts',(2.61472411340977,30.9392407372461,53.6239208296653));
#107274=CARTESIAN_POINT('Ctrl Pts',(2.61787987952028,30.9789702972248,53.6515490562528));
#107275=CARTESIAN_POINT('Ctrl Pts',(2.62005655018282,31.0061782815751,53.6717273221006));
#107276=CARTESIAN_POINT('Ctrl Pts',(2.62531616961249,31.0711782562362,53.7230775159884));
#107277=CARTESIAN_POINT('Ctrl Pts',(2.62836732340689,31.1082474357985,53.7551136465377));
#107278=CARTESIAN_POINT('Ctrl Pts',(2.6374473329851,31.21529249259,53.8562015181109));
#107279=CARTESIAN_POINT('Ctrl Pts',(2.64335522083053,31.2806198628961,53.9298493947642));
#107280=CARTESIAN_POINT('Ctrl Pts',(2.65273274339902,31.3704383735152,54.0511935192407));
#107281=CARTESIAN_POINT('Ctrl Pts',(2.65606072062755,31.3997700024202,54.0950260547638));
#107282=CARTESIAN_POINT('Ctrl Pts',(2.66028177518287,31.433074748508,54.1502985224751));
#107283=CARTESIAN_POINT('Ctrl Pts',(2.66106118743689,31.4390695697947,54.1604914596091));
#107284=CARTESIAN_POINT('Ctrl Pts',(2.6622980768278,31.4483304220239,54.1766282912769));
#107285=CARTESIAN_POINT('Ctrl Pts',(2.66275106203928,31.4516696616105,54.1825300179458));
#107286=CARTESIAN_POINT('Ctrl Pts',(2.66361610631598,31.4579450949911,54.1937808403398));
#107287=CARTESIAN_POINT('Ctrl Pts',(2.66402773558948,31.4608880549701,54.1991259030078));
#107288=CARTESIAN_POINT('Ctrl Pts',(2.66502064479975,31.4678847725331,54.212000368039));
#107289=CARTESIAN_POINT('Ctrl Pts',(2.66560365398541,31.4719100086226,54.2195449763146));
#107290=CARTESIAN_POINT('Ctrl Pts',(2.66765658815592,31.4858009951762,54.2460709397786));
#107291=CARTESIAN_POINT('Ctrl Pts',(2.66914341484772,31.4953586259579,54.2652101666436));
#107292=CARTESIAN_POINT('Ctrl Pts',(2.67293736702885,31.5185557684826,54.3139906685801));
#107293=CARTESIAN_POINT('Ctrl Pts',(2.67526429493369,31.5316976635665,54.343857912993));
#107294=CARTESIAN_POINT('Ctrl Pts',(2.68304221476275,31.5723114456568,54.4440412753233));
#107295=CARTESIAN_POINT('Ctrl Pts',(2.68856836627649,31.5958823139534,54.5158380075733));
#107296=CARTESIAN_POINT('Ctrl Pts',(2.70125404883385,31.6390406682402,54.6853677622887));
#107297=CARTESIAN_POINT('Ctrl Pts',(2.7083411534123,31.65490114175,54.7837682524219));
#107298=CARTESIAN_POINT('Ctrl Pts',(2.71648668243657,31.6632558801577,54.9024516376962));
#107299=CARTESIAN_POINT('Ctrl Pts',(2.7178104124869,31.6642832231064,54.921915333777));
#107300=CARTESIAN_POINT('Ctrl Pts',(2.71989468522261,31.6653714860199,54.9528320087661));
#107301=CARTESIAN_POINT('Ctrl Pts',(2.72066212585408,31.6656562449746,54.9642747883555));
#107302=CARTESIAN_POINT('Ctrl Pts',(2.72196519519543,31.6659408519501,54.9838012238661));
#107303=CARTESIAN_POINT('Ctrl Pts',(2.72250264605235,31.6659998341427,54.9918834489475));
#107304=CARTESIAN_POINT('Ctrl Pts',(2.72303827374538,31.6659999996507,54.9999658845042));
#107305=CARTESIAN_POINT('Ctrl Pts',(2.72303826203026,31.6659999996471,54.9999657077272));
#107306=CARTESIAN_POINT('Ctrl Pts',(2.72365866824712,31.6660001923448,55.0093274212484));
#107307=CARTESIAN_POINT('Ctrl Pts',(2.72427661150426,31.6659214760123,55.0186891663787));
#107308=CARTESIAN_POINT('Ctrl Pts',(2.72592145939162,31.6655002618234,55.0437032318179));
#107309=CARTESIAN_POINT('Ctrl Pts',(2.72694394157471,31.6650160391201,55.05935243227));
#107310=CARTESIAN_POINT('Ctrl Pts',(2.73099403122546,31.6622067581869,55.1216985516583));
#107311=CARTESIAN_POINT('Ctrl Pts',(2.73396789704877,31.6581370098067,55.1682976661332));
#107312=CARTESIAN_POINT('Ctrl Pts',(2.74466954164758,31.6361375639892,55.3376086933545));
#107313=CARTESIAN_POINT('Ctrl Pts',(2.75207414576663,31.6064916702442,55.4583768259009));
#107314=CARTESIAN_POINT('Ctrl Pts',(2.75977020846451,31.5636287079815,55.5749968174508));
#107315=CARTESIAN_POINT('Ctrl Pts',(2.7597873422125,31.5635332253174,55.5752564035542));
#107316=CARTESIAN_POINT('Ctrl Pts',(2.75980447732862,31.5634376782628,55.5755159651897));
#107317=CARTESIAN_POINT('Ctrl Pts',(2.56903902087732,31.5634376730794,55.5755159792709));
#107318=CARTESIAN_POINT('Ctrl Pts',(2.56703832709278,31.5744467142337,55.5456089909248));
#107319=CARTESIAN_POINT('Ctrl Pts',(2.56501125490043,31.584597150557,55.5153873830606));
#107320=CARTESIAN_POINT('Ctrl Pts',(2.56192251703097,31.5984538539087,55.4698390336222));
#107321=CARTESIAN_POINT('Ctrl Pts',(2.56089224524731,31.6028185591783,55.4547263606249));
#107322=CARTESIAN_POINT('Ctrl Pts',(2.55934852915817,31.6089676453066,55.4322459177972));
#107323=CARTESIAN_POINT('Ctrl Pts',(2.55884397055743,31.6109169204052,55.4249236249913));
#107324=CARTESIAN_POINT('Ctrl Pts',(2.55793465409424,31.6143203786623,55.4117787400294));
#107325=CARTESIAN_POINT('Ctrl Pts',(2.55753095870801,31.6157931457939,55.4059612334005));
#107326=CARTESIAN_POINT('Ctrl Pts',(2.55662466577699,31.6190142929406,55.3929422780383));
#107327=CARTESIAN_POINT('Ctrl Pts',(2.55612117936977,31.6207460562079,55.3857371263221));
#107328=CARTESIAN_POINT('Ctrl Pts',(2.55459979059657,31.6258080166508,55.3640403690167));
#107329=CARTESIAN_POINT('Ctrl Pts',(2.55357431454301,31.628992224923,55.3495159370959));
#107330=CARTESIAN_POINT('Ctrl Pts',(2.54475053051766,31.6545010834067,55.2252293240228));
#107331=CARTESIAN_POINT('Ctrl Pts',(2.53651828560861,31.6658963723887,55.1135246429918));
#107332=CARTESIAN_POINT('Ctrl Pts',(2.52138067042813,31.6660879584933,54.9050563313741));
#107333=CARTESIAN_POINT('Ctrl Pts',(2.51447540910696,31.6577966079625,54.8087432123935));
#107334=CARTESIAN_POINT('Ctrl Pts',(2.50627876799148,31.6373615881475,54.6916093219608));
#107335=CARTESIAN_POINT('Ctrl Pts',(2.50474819009306,31.6330669601417,54.6696211739158));
#107336=CARTESIAN_POINT('Ctrl Pts',(2.50230218166022,31.6254272867301,54.634308073459));
#107337=CARTESIAN_POINT('Ctrl Pts',(2.50137813197071,31.6223587769904,54.6209268304253));
#107338=CARTESIAN_POINT('Ctrl Pts',(2.49974276754146,31.6166030602353,54.5971784561518));
#107339=CARTESIAN_POINT('Ctrl Pts',(2.49902942185785,31.6139806664587,54.5867965778889));
#107340=CARTESIAN_POINT('Ctrl Pts',(2.49752647213994,31.6082191044489,54.5648790799132));
#107341=CARTESIAN_POINT('Ctrl Pts',(2.49673770137291,31.6050554856787,54.5533504691269));
#107342=CARTESIAN_POINT('Ctrl Pts',(2.49462544257866,31.5962079662301,54.522417632488));
#107343=CARTESIAN_POINT('Ctrl Pts',(2.49330943344632,31.5902943589723,54.5030807927141));
#107344=CARTESIAN_POINT('Ctrl Pts',(2.48464646038119,31.5487257399475,54.3755080608609));
#107345=CARTESIAN_POINT('Ctrl Pts',(2.47767428538728,31.5023976900992,54.2710644312253));
#107346=CARTESIAN_POINT('Ctrl Pts',(2.4645313593107,31.3954452534932,54.0842800468393));
#107347=CARTESIAN_POINT('Ctrl Pts',(2.45837550547428,31.3372257074833,54.0011844958416));
#107348=CARTESIAN_POINT('Ctrl Pts',(2.4507870835654,31.2616745700886,53.9118912286464));
#107349=CARTESIAN_POINT('Ctrl Pts',(2.44975685549702,31.2513454478176,53.90002820698));
#107350=CARTESIAN_POINT('Ctrl Pts',(2.44821319246676,31.2357942230931,53.8826701233351));
#107351=CARTESIAN_POINT('Ctrl Pts',(2.44770864232784,31.2306997473911,53.8770612032184));
#107352=CARTESIAN_POINT('Ctrl Pts',(2.44679933447179,31.2215021565176,53.8670725984019));
#107353=CARTESIAN_POINT('Ctrl Pts',(2.44639563913415,31.2174133919079,53.8626800598839));
#107354=CARTESIAN_POINT('Ctrl Pts',(2.44548933794259,31.208222550221,53.8529127384811));
#107355=CARTESIAN_POINT('Ctrl Pts',(2.44498584313436,31.2031083485751,53.8475499087982));
#107356=CARTESIAN_POINT('Ctrl Pts',(2.4434644035796,31.1876248635897,53.8315290765823));
#107357=CARTESIAN_POINT('Ctrl Pts',(2.44243888442806,31.1771488118049,53.8209759323005));
#107358=CARTESIAN_POINT('Ctrl Pts',(2.44001941682391,31.1523109414172,53.7966162976543));
#107359=CARTESIAN_POINT('Ctrl Pts',(2.4386188679723,31.1378401207268,53.7829245602019));
#107360=CARTESIAN_POINT('Ctrl Pts',(2.43350353001001,31.0845441051653,53.7342792419828));
#107361=CARTESIAN_POINT('Ctrl Pts',(2.42972451406117,31.0443274033177,53.7008985532057));
#107362=CARTESIAN_POINT('Ctrl Pts',(2.41654038897413,30.8994768408192,53.5917478557784));
#107363=CARTESIAN_POINT('Ctrl Pts',(2.4071292340123,30.7876355721483,53.5262721418095));
#107364=CARTESIAN_POINT('Ctrl Pts',(2.39613397636486,30.6423752199784,53.4625420018965));
#107365=CARTESIAN_POINT('Ctrl Pts',(2.39411604863357,30.615100729484,53.4514283024843));
#107366=CARTESIAN_POINT('Ctrl Pts',(2.39118965336059,30.5746564907069,53.4361855580708));
#107367=CARTESIAN_POINT('Ctrl Pts',(2.39026248305905,30.5617085149661,53.4314882037128));
#107368=CARTESIAN_POINT('Ctrl Pts',(2.38862364152204,30.5385885245693,53.4234235949403));
#107369=CARTESIAN_POINT('Ctrl Pts',(2.38790990771771,30.5284396251308,53.4199929330566));
#107370=CARTESIAN_POINT('Ctrl Pts',(2.38640819107006,30.5069209778355,53.412949457667));
#107371=CARTESIAN_POINT('Ctrl Pts',(2.3856210214882,30.4955440524567,53.4093603782715));
#107372=CARTESIAN_POINT('Ctrl Pts',(2.38351802995604,30.464896883769,53.4000528479526));
#107373=CARTESIAN_POINT('Ctrl Pts',(2.38220957042046,30.4455596983682,53.394560305201));
#107374=CARTESIAN_POINT('Ctrl Pts',(2.37933594228214,30.4025404061344,53.3831782717954));
#107375=CARTESIAN_POINT('Ctrl Pts',(2.3777760734263,30.3788185833725,53.3774563640163));
#107376=CARTESIAN_POINT('Ctrl Pts',(2.37288859520862,30.3034742800915,53.3610252513701));
#107377=CARTESIAN_POINT('Ctrl Pts',(2.36961407675322,30.251463441224,53.3522434593206));
#107378=CARTESIAN_POINT('Ctrl Pts',(2.36376389457143,30.1570463585992,53.3408772389344));
#107379=CARTESIAN_POINT('Ctrl Pts',(2.3611790268356,30.114793663017,53.3374193562994));
#107380=CARTESIAN_POINT('Ctrl Pts',(2.35276587877904,29.9771579868969,53.3314278794156));
#107381=CARTESIAN_POINT('Ctrl Pts',(2.34694670894351,29.8816930190841,53.3354720126228));
#107382=CARTESIAN_POINT('Ctrl Pts',(2.33972386028802,29.7712103413333,53.3497065808873));
#107383=CARTESIAN_POINT('Ctrl Pts',(2.33867417491907,29.7553392796416,53.3519847808123));
#107384=CARTESIAN_POINT('Ctrl Pts',(2.33710691593126,29.7319632171216,53.3556853780243));
#107385=CARTESIAN_POINT('Ctrl Pts',(2.33659862398766,29.7244306196399,53.3569309801671));
#107386=CARTESIAN_POINT('Ctrl Pts',(2.33568548985234,29.7109914235352,53.3592483193188));
#107387=CARTESIAN_POINT('Ctrl Pts',(2.33528175280421,29.7050816801383,53.3603002662017));
#107388=CARTESIAN_POINT('Ctrl Pts',(2.33437901140455,29.6919402558563,53.3627128110156));
#107389=CARTESIAN_POINT('Ctrl Pts',(2.33387915794543,29.6847119187796,53.3640893771848));
#107390=CARTESIAN_POINT('Ctrl Pts',(2.33237961804386,29.6631632595541,53.3683412275828));
#107391=CARTESIAN_POINT('Ctrl Pts',(2.33137266330465,29.6488718101618,53.3713569152939));
#107392=CARTESIAN_POINT('Ctrl Pts',(2.32347606220776,29.5380388992977,53.3962706947691));
#107393=CARTESIAN_POINT('Ctrl Pts',(2.31624123179921,29.4435914353407,53.4265446369797));
#107394=CARTESIAN_POINT('Ctrl Pts',(2.30099907038259,29.2505860335259,53.5079726290602));
#107395=CARTESIAN_POINT('Ctrl Pts',(2.29304595366654,29.1532831835809,53.5609567768923));
#107396=CARTESIAN_POINT('Ctrl Pts',(2.28390852586352,29.0436911163339,53.635625948877));
#107397=CARTESIAN_POINT('Ctrl Pts',(2.28240082919366,29.0256975327826,53.6484164785268));
#107398=CARTESIAN_POINT('Ctrl Pts',(2.27998386290921,28.9970094800734,53.6696797761203));
#107399=CARTESIAN_POINT('Ctrl Pts',(2.27906630214358,28.9861560739729,53.6779325304779));
#107400=CARTESIAN_POINT('Ctrl Pts',(2.2774381380777,28.966969774949,53.6928967187799));
#107401=CARTESIAN_POINT('Ctrl Pts',(2.27672556952316,28.9585980332496,53.6995568499692));
#107402=CARTESIAN_POINT('Ctrl Pts',(2.27521990454015,28.9409659160703,53.71386353309));
#107403=CARTESIAN_POINT('Ctrl Pts',(2.27442768406975,28.9317228609004,53.7215305364587));
#107404=CARTESIAN_POINT('Ctrl Pts',(2.27229544511293,28.9069467837972,53.7425383205256));
#107405=CARTESIAN_POINT('Ctrl Pts',(2.27096315925479,28.8915751630459,53.7560668630174));
#107406=CARTESIAN_POINT('Ctrl Pts',(2.26238190380118,28.793401970359,53.8457341321196));
#107407=CARTESIAN_POINT('Ctrl Pts',(2.25549600707798,28.718240184404,53.9298110173004));
#107408=CARTESIAN_POINT('Ctrl Pts',(2.24236958218581,28.5918981527878,54.1037279383149));
#107409=CARTESIAN_POINT('Ctrl Pts',(2.23614509653355,28.539461417703,54.1919926911794));
#107410=CARTESIAN_POINT('Ctrl Pts',(2.22848555235427,28.4887690525829,54.2985868698199));
#107411=CARTESIAN_POINT('Ctrl Pts',(2.22746362733322,28.4822678394983,54.3127675780948));
#107412=CARTESIAN_POINT('Ctrl Pts',(2.22593004321559,28.4729162592118,54.3339457317402));
#107413=CARTESIAN_POINT('Ctrl Pts',(2.22542710207359,28.469912611736,54.3408751116811));
#107414=CARTESIAN_POINT('Ctrl Pts',(2.22451942302356,28.4646071489452,54.3533464581515));
#107415=CARTESIAN_POINT('Ctrl Pts',(2.2241157290447,28.4622880178096,54.358880769807));
#107416=CARTESIAN_POINT('Ctrl Pts',(2.22320782431244,28.4571628260129,54.3712991837081));
#107417=CARTESIAN_POINT('Ctrl Pts',(2.22270270691986,28.4543729410728,54.3781895375374));
#107418=CARTESIAN_POINT('Ctrl Pts',(2.22117145138896,28.4460973068399,54.3990282284693));
#107419=CARTESIAN_POINT('Ctrl Pts',(2.22013759968003,28.4407537570065,54.4130317174724));
#107420=CARTESIAN_POINT('Ctrl Pts',(2.21087348919067,28.3949562074735,54.5380906778809));
#107421=CARTESIAN_POINT('Ctrl Pts',(2.20216477450047,28.3662411647657,54.6530784275947));
#107422=CARTESIAN_POINT('Ctrl Pts',(2.18703014679514,28.337439096311,54.8598252212338));
#107423=CARTESIAN_POINT('Ctrl Pts',(2.18056557021985,28.3322762760155,54.9504032813295));
#107424=CARTESIAN_POINT('Ctrl Pts',(2.17279666076356,28.3350483283738,55.0631074250266));
#107425=CARTESIAN_POINT('Ctrl Pts',(2.17128361314673,28.3360345210605,55.0852383860907));
#107426=CARTESIAN_POINT('Ctrl Pts',(2.16885985122805,28.3383416784113,55.1209715001071));
#107427=CARTESIAN_POINT('Ctrl Pts',(2.16794076955702,28.339389093405,55.1345879553264));
#107428=CARTESIAN_POINT('Ctrl Pts',(2.16631092169266,28.3415555733005,55.1588476210601));
#107429=CARTESIAN_POINT('Ctrl Pts',(2.16559817485443,28.3426099715321,55.1694956809977));
#107430=CARTESIAN_POINT('Ctrl Pts',(2.16409316554087,28.3450638891817,55.1920582223113));
#107431=CARTESIAN_POINT('Ctrl Pts',(2.16330176887972,28.3464896624196,55.2039692815413));
#107432=CARTESIAN_POINT('Ctrl Pts',(2.16117430280529,28.350688962815,55.2361055065412));
#107433=CARTESIAN_POINT('Ctrl Pts',(2.15984590508754,28.353705824445,55.256297199131));
#107434=CARTESIAN_POINT('Ctrl Pts',(2.15126733036294,28.3757580586625,55.3873607116074));
#107435=CARTESIAN_POINT('Ctrl Pts',(2.1443804974883,28.4056103303477,55.4961209340929));
#107436=CARTESIAN_POINT('Ctrl Pts',(2.1312461149849,28.4832109679758,55.6967284291529));
#107437=CARTESIAN_POINT('Ctrl Pts',(2.12501464617572,28.5289736279465,55.7887681582714));
#107438=CARTESIAN_POINT('Ctrl Pts',(2.11734771545702,28.5910959131991,55.8892627822139));
#107439=CARTESIAN_POINT('Ctrl Pts',(2.11632647603932,28.5994782285968,55.9024066415216));
#107440=CARTESIAN_POINT('Ctrl Pts',(2.1147937244984,28.6121921510527,55.9217387824128));
#107441=CARTESIAN_POINT('Ctrl Pts',(2.114290916621,28.6163836689581,55.9280187775906));
#107442=CARTESIAN_POINT('Ctrl Pts',(2.11338337210674,28.6239828058318,55.9392383569808));
#107443=CARTESIAN_POINT('Ctrl Pts',(2.11297967787029,28.627374625035,55.9441883218439));
#107444=CARTESIAN_POINT('Ctrl Pts',(2.11207163863731,28.6350293224486,55.9552310402254));
#107445=CARTESIAN_POINT('Ctrl Pts',(2.11156638552315,28.6393062478497,55.9613135795951));
#107446=CARTESIAN_POINT('Ctrl Pts',(2.11003430704773,28.6523324186776,55.9795779897269));
#107447=CARTESIAN_POINT('Ctrl Pts',(2.10899975639033,28.6612053183635,55.9916701614192));
#107448=CARTESIAN_POINT('Ctrl Pts',(2.10655505230234,28.6823772340039,56.0197216135052));
#107449=CARTESIAN_POINT('Ctrl Pts',(2.10513812012677,28.6948047644001,56.0355806308413));
#107450=CARTESIAN_POINT('Ctrl Pts',(2.09993527430348,28.7410978032091,56.0924988718621));
#107451=CARTESIAN_POINT('Ctrl Pts',(2.09608309853945,28.776636689922,56.1321528427651));
#107452=CARTESIAN_POINT('Ctrl Pts',(2.08254317607198,28.9074212941199,56.2647208324352));
#107453=CARTESIAN_POINT('Ctrl Pts',(2.07286121941079,29.0118549316054,56.3478979244634));
#107454=CARTESIAN_POINT('Ctrl Pts',(2.06189989286676,29.146972301534,56.4312795825947));
#107455=CARTESIAN_POINT('Ctrl Pts',(2.06014216595753,29.1691706150017,56.4442784214195));
#107456=CARTESIAN_POINT('Ctrl Pts',(2.05750725913073,29.2032428107282,56.4631846727804));
#107457=CARTESIAN_POINT('Ctrl Pts',(2.05661664438505,29.2148999834214,56.4694724859158));
#107458=CARTESIAN_POINT('Ctrl Pts',(2.05501788598772,29.2360757654427,56.4805706551836));
#107459=CARTESIAN_POINT('Ctrl Pts',(2.0543080493953,29.2455678220526,56.4854298364726));
#107460=CARTESIAN_POINT('Ctrl Pts',(2.05278862245614,29.2660762589244,56.4956812351074));
#107461=CARTESIAN_POINT('Ctrl Pts',(2.05198010356523,29.2771069031143,56.5010436365183));
#107462=CARTESIAN_POINT('Ctrl Pts',(2.04975301920599,29.3078080386062,56.5155516527618));
#107463=CARTESIAN_POINT('Ctrl Pts',(2.04834344038275,29.327599889755,56.5244358582175));
#107464=CARTESIAN_POINT('Ctrl Pts',(2.04521158281744,29.3723282421418,56.5434729467122));
#107465=CARTESIAN_POINT('Ctrl Pts',(2.04349626842317,29.3973488938929,56.5534131244396));
#107466=CARTESIAN_POINT('Ctrl Pts',(2.03790339842026,29.4804422881466,56.5841143230176));
#107467=CARTESIAN_POINT('Ctrl Pts',(2.03409883039588,29.5394289221737,56.6022588775444));
#107468=CARTESIAN_POINT('Ctrl Pts',(2.02477031179079,29.6872769446932,56.6388952322896));
#107469=CARTESIAN_POINT('Ctrl Pts',(2.019298032406,29.7768921739977,56.6534794371085));
#107470=CARTESIAN_POINT('Ctrl Pts',(2.01104110948433,29.9081421314178,56.6639716345134));
#107471=CARTESIAN_POINT('Ctrl Pts',(2.00842634409198,29.9491449704016,56.6657288578313));
#107472=CARTESIAN_POINT('Ctrl Pts',(2.00501052258785,30.001274131753,56.6660365392934));
#107473=CARTESIAN_POINT('Ctrl Pts',(2.00427742585355,30.012381316934,56.6659910144505));
#107474=CARTESIAN_POINT('Ctrl Pts',(2.0030976812207,30.0301098493991,56.665741057276));
#107475=CARTESIAN_POINT('Ctrl Pts',(2.00265485925248,30.0367320948796,56.6656081839085));
#107476=CARTESIAN_POINT('Ctrl Pts',(2.00179553940694,30.0495164249859,56.6652753929621));
#107477=CARTESIAN_POINT('Ctrl Pts',(2.00137932908808,30.0556784508741,56.6650807535451));
#107478=CARTESIAN_POINT('Ctrl Pts',(2.00035559313652,30.0707646597869,56.6645203930283));
#107479=CARTESIAN_POINT('Ctrl Pts',(1.99974605845575,30.0796871799554,56.6641170993239));
#107480=CARTESIAN_POINT('Ctrl Pts',(1.99748588980919,30.1125681851058,56.6623658531569));
#107481=CARTESIAN_POINT('Ctrl Pts',(1.99581369419722,30.1364987544499,56.6605721215487));
#107482=CARTESIAN_POINT('Ctrl Pts',(1.99141230716418,30.1986662884355,56.6545595200941));
#107483=CARTESIAN_POINT('Ctrl Pts',(1.98865527953901,30.2368099072141,56.6495321154896));
#107484=CARTESIAN_POINT('Ctrl Pts',(1.98078049732849,30.3442941709518,56.6315606482647));
#107485=CARTESIAN_POINT('Ctrl Pts',(1.97562095791853,30.413036767812,56.6155275690231));
#107486=CARTESIAN_POINT('Ctrl Pts',(1.96362254397682,30.5716560136923,56.5677428501653));
#107487=CARTESIAN_POINT('Ctrl Pts',(1.95685560119414,30.6602494140888,56.532541822499));
#107488=CARTESIAN_POINT('Ctrl Pts',(1.94898191140086,30.7631094854507,56.4810852682087));
#107489=CARTESIAN_POINT('Ctrl Pts',(1.94763453161505,30.7806944746662,56.4718919303925));
#107490=CARTESIAN_POINT('Ctrl Pts',(1.94549842501006,30.8085345767801,56.4566979205397));
#107491=CARTESIAN_POINT('Ctrl Pts',(1.94470269637493,30.8188965471971,56.450898153276));
#107492=CARTESIAN_POINT('Ctrl Pts',(1.94319581221635,30.8384977918962,56.4396501212028));
#107493=CARTESIAN_POINT('Ctrl Pts',(1.94248396456794,30.8477481428783,56.4342224771344));
#107494=CARTESIAN_POINT('Ctrl Pts',(1.94085851683372,30.8688444294752,56.421568807772));
#107495=CARTESIAN_POINT('Ctrl Pts',(1.93994713472802,30.8806538975934,56.4142832989968));
#107496=CARTESIAN_POINT('Ctrl Pts',(1.9370803637487,30.9177222215727,56.3907707099766));
#107497=CARTESIAN_POINT('Ctrl Pts',(1.93514474017117,30.9426350508713,56.3740074901538));
#107498=CARTESIAN_POINT('Ctrl Pts',(1.92370972981544,31.0886747386681,56.2698982545292));
#107499=CARTESIAN_POINT('Ctrl Pts',(1.91484519344245,31.1980536579125,56.1672706669635));
#107500=CARTESIAN_POINT('Ctrl Pts',(1.90212103745279,31.3276316898167,56.0080105142467));
#107501=CARTESIAN_POINT('Ctrl Pts',(1.89859554197249,31.3607534859795,55.96282899989));
#107502=CARTESIAN_POINT('Ctrl Pts',(1.89414911264204,31.3981491541458,55.9060240876121));
#107503=CARTESIAN_POINT('Ctrl Pts',(1.89335654397829,31.4046543808281,55.8959055499316));
#107504=CARTESIAN_POINT('Ctrl Pts',(1.8921035461101,31.4146769956061,55.8799383845685));
#107505=CARTESIAN_POINT('Ctrl Pts',(1.89164780712139,31.4182691340537,55.8741368438452));
#107506=CARTESIAN_POINT('Ctrl Pts',(1.89078118143745,31.4249970225,55.8631202205903));
#107507=CARTESIAN_POINT('Ctrl Pts',(1.89037076350753,31.4281399738144,55.8579098085268));
#107508=CARTESIAN_POINT('Ctrl Pts',(1.88938589843034,31.4355802337925,55.8454210981417));
#107509=CARTESIAN_POINT('Ctrl Pts',(1.88880979341608,31.4398507874121,55.8381271640748));
#107510=CARTESIAN_POINT('Ctrl Pts',(1.88680716602338,31.4544213841984,55.8128011348444));
#107511=CARTESIAN_POINT('Ctrl Pts',(1.88536478096997,31.4644391965092,55.7946099609426));
#107512=CARTESIAN_POINT('Ctrl Pts',(1.88171118202069,31.4886957518609,55.7485455421434));
#107513=CARTESIAN_POINT('Ctrl Pts',(1.87948183114997,31.5024936600626,55.7204498882326));
#107514=CARTESIAN_POINT('Ctrl Pts',(1.87421257502843,31.532948237739,55.6537523329074));
#107515=CARTESIAN_POINT('Ctrl Pts',(1.87116107209707,31.5489395752854,55.6149012468612));
#107516=CARTESIAN_POINT('Ctrl Pts',(1.86810672180998,31.5634374966623,55.5755164585225));
#107517=CARTESIAN_POINT('Origin',(5.,30.,55.));
#107518=CARTESIAN_POINT('',(1.16624544379888,31.5634376782622,55.5755159651913));
#107519=CARTESIAN_POINT('',(1.36116735710803,31.5634376788384,55.575515963626));
#107520=CARTESIAN_POINT('',(5.,31.5634376782623,55.5755159651912));
#107521=CARTESIAN_POINT('Ctrl Pts',(1.36116735710803,31.5634376788384,55.575515963626));
#107522=CARTESIAN_POINT('Ctrl Pts',(1.3613845116336,31.5624022301552,55.578328847348));
#107523=CARTESIAN_POINT('Ctrl Pts',(1.36160158161901,31.5613591468225,55.5811390545062));
#107524=CARTESIAN_POINT('Ctrl Pts',(1.36633196778185,31.538452467193,55.6423458298376));
#107525=CARTESIAN_POINT('Ctrl Pts',(1.37079547469062,31.5133333770567,55.699476656108));
#107526=CARTESIAN_POINT('Ctrl Pts',(1.37796171917311,31.4669765940998,55.790651004218));
#107527=CARTESIAN_POINT('Ctrl Pts',(1.38071830898915,31.447611335838,55.8255732699834));
#107528=CARTESIAN_POINT('Ctrl Pts',(1.38447982978756,31.4190422483487,55.8729910592628));
#107529=CARTESIAN_POINT('Ctrl Pts',(1.38552202255295,31.4108922490538,55.8861023538935));
#107530=CARTESIAN_POINT('Ctrl Pts',(1.38729356594832,31.396639243336,55.9083365150875));
#107531=CARTESIAN_POINT('Ctrl Pts',(1.38802617708115,31.3906263001302,55.9175156151169));
#107532=CARTESIAN_POINT('Ctrl Pts',(1.38941786703856,31.3789787627736,55.9349186768279));
#107533=CARTESIAN_POINT('Ctrl Pts',(1.39007750555529,31.3733602099005,55.9431527456587));
#107534=CARTESIAN_POINT('Ctrl Pts',(1.39161885991712,31.360003835093,55.9623542532146));
#107535=CARTESIAN_POINT('Ctrl Pts',(1.39249828427459,31.3522066363019,55.9732796978327));
#107536=CARTESIAN_POINT('Ctrl Pts',(1.39556426922443,31.3244124818949,56.0112460557422));
#107537=CARTESIAN_POINT('Ctrl Pts',(1.3977244576177,31.3037288181165,56.0377757082481));
#107538=CARTESIAN_POINT('Ctrl Pts',(1.40772469980558,31.2031196223636,56.1590610238801));
#107539=CARTESIAN_POINT('Ctrl Pts',(1.4151738033165,31.1135871821581,56.2453290536538));
#107540=CARTESIAN_POINT('Ctrl Pts',(1.42590888589875,30.9749844173835,56.3518684976956));
#107541=CARTESIAN_POINT('Ctrl Pts',(1.4290589355703,30.9332624940005,56.3810008860487));
#107542=CARTESIAN_POINT('Ctrl Pts',(1.43353903457282,30.8737101246704,56.4186510391869));
#107543=CARTESIAN_POINT('Ctrl Pts',(1.43479747631727,30.8569606918965,56.4288311501258));
#107544=CARTESIAN_POINT('Ctrl Pts',(1.43702636567507,30.8273519677758,56.4461191051649));
#107545=CARTESIAN_POINT('Ctrl Pts',(1.43798987789507,30.8145707229978,56.4533568887049));
#107546=CARTESIAN_POINT('Ctrl Pts',(1.43945248612774,30.795230077515,56.4639738831506));
#107547=CARTESIAN_POINT('Ctrl Pts',(1.43994399730035,30.7887408087137,56.4674802684311));
#107548=CARTESIAN_POINT('Ctrl Pts',(1.44084056948911,30.7769272363381,56.473762573178));
#107549=CARTESIAN_POINT('Ctrl Pts',(1.44124472029134,30.7716109256635,56.4765529549372));
#107550=CARTESIAN_POINT('Ctrl Pts',(1.44216596302616,30.7595129121344,56.4828196823788));
#107551=CARTESIAN_POINT('Ctrl Pts',(1.44268410095706,30.7527224067631,56.486278253488));
#107552=CARTESIAN_POINT('Ctrl Pts',(1.44429495887164,30.7316465041888,56.4968312519475));
#107553=CARTESIAN_POINT('Ctrl Pts',(1.44539656354536,30.717283249439,56.5037669691452));
#107554=CARTESIAN_POINT('Ctrl Pts',(1.45323504987242,30.6152832017317,56.5512269124238));
#107555=CARTESIAN_POINT('Ctrl Pts',(1.46028962061975,30.5243756124098,56.5842680973235));
#107556=CARTESIAN_POINT('Ctrl Pts',(1.47571355515163,30.3196248322529,56.639122111583));
#107557=CARTESIAN_POINT('Ctrl Pts',(1.48401553333094,30.205299966021,56.657329888676));
#107558=CARTESIAN_POINT('Ctrl Pts',(1.49344027156436,30.0682231815618,56.6647453082959));
#107559=CARTESIAN_POINT('Ctrl Pts',(1.49492403274362,30.0464307622696,56.6654956038666));
#107560=CARTESIAN_POINT('Ctrl Pts',(1.49722338728746,30.0123403598309,56.6659996273685));
#107561=CARTESIAN_POINT('Ctrl Pts',(1.49804796372593,30.0000498425013,56.6660453338416));
#107562=CARTESIAN_POINT('Ctrl Pts',(1.49958012541974,29.9770954033315,56.6658766796563));
#107563=CARTESIAN_POINT('Ctrl Pts',(1.50028872069814,29.9664319453511,56.6656959287701));
#107564=CARTESIAN_POINT('Ctrl Pts',(1.50186853324321,29.9425563120589,56.6650618508168));
#107565=CARTESIAN_POINT('Ctrl Pts',(1.50273799558165,29.9293462208004,56.6645536352387));
#107566=CARTESIAN_POINT('Ctrl Pts',(1.50495291904238,29.8955279958919,56.6628492621613));
#107567=CARTESIAN_POINT('Ctrl Pts',(1.50629135347019,29.8749331415438,56.6614272205867));
#107568=CARTESIAN_POINT('Ctrl Pts',(1.51736969143367,29.7033490444511,56.646370837997));
#107569=CARTESIAN_POINT('Ctrl Pts',(1.52640483462278,29.5548521132859,56.6125704629521));
#107570=CARTESIAN_POINT('Ctrl Pts',(1.53944594997554,29.356944332807,56.5380569741244));
#107571=CARTESIAN_POINT('Ctrl Pts',(1.54318793533599,29.3021019400113,56.5139605787668));
#107572=CARTESIAN_POINT('Ctrl Pts',(1.54805717667697,29.2351931073914,56.4801536376115));
#107573=CARTESIAN_POINT('Ctrl Pts',(1.54904785588184,29.2217989583892,56.4731556175565));
#107574=CARTESIAN_POINT('Ctrl Pts',(1.5505435522493,29.201938576557,56.4624327703978));
#107575=CARTESIAN_POINT('Ctrl Pts',(1.55104046708579,29.1953987485923,56.4588449075971));
#107576=CARTESIAN_POINT('Ctrl Pts',(1.5519422768732,29.183640314036,56.4522909121648));
#107577=CARTESIAN_POINT('Ctrl Pts',(1.55234619862556,29.1784133446259,56.4493403310046));
#107578=CARTESIAN_POINT('Ctrl Pts',(1.55326103080455,29.1666642339802,56.442624073368));
#107579=CARTESIAN_POINT('Ctrl Pts',(1.55377292004837,29.1601516635725,56.4388424105032));
#107580=CARTESIAN_POINT('Ctrl Pts',(1.55534504166852,29.1403306326248,56.4271524918029));
#107581=CARTESIAN_POINT('Ctrl Pts',(1.55641357765907,29.1271069975175,56.4191030334511));
#107582=CARTESIAN_POINT('Ctrl Pts',(1.56476075036911,29.0255711178278,56.3553402961769));
#107583=CARTESIAN_POINT('Ctrl Pts',(1.57241330265993,28.9425679890345,56.2916242129417));
#107584=CARTESIAN_POINT('Ctrl Pts',(1.58792565713245,28.7862453544414,56.1463987663533));
#107585=CARTESIAN_POINT('Ctrl Pts',(1.59573718666305,28.7138669473411,56.0645656690184));
#107586=CARTESIAN_POINT('Ctrl Pts',(1.60468710956191,28.6374377502348,55.9588738902445));
#107587=CARTESIAN_POINT('Ctrl Pts',(1.60614459488135,28.6252189309845,55.9412715380698));
#107588=CARTESIAN_POINT('Ctrl Pts',(1.60841259941169,28.6065741700207,55.9132740909396));
#107589=CARTESIAN_POINT('Ctrl Pts',(1.60923170409134,28.5999175919399,55.903036197077));
#107590=CARTESIAN_POINT('Ctrl Pts',(1.6107588485616,28.5876551787815,55.8837148904707));
#107591=CARTESIAN_POINT('Ctrl Pts',(1.61146783941328,28.5820229444001,55.8746490613466));
#107592=CARTESIAN_POINT('Ctrl Pts',(1.6130551443398,28.5695533716093,55.854140564694));
#107593=CARTESIAN_POINT('Ctrl Pts',(1.61393162628132,28.5627654065791,55.8426686190815));
#107594=CARTESIAN_POINT('Ctrl Pts',(1.61657005535108,28.5426376325992,55.8077009712989));
#107595=CARTESIAN_POINT('Ctrl Pts',(1.61831657374723,28.529730589903,55.7839604090271));
#107596=CARTESIAN_POINT('Ctrl Pts',(1.62848372593572,28.4572477316185,55.6425464302532));
#107597=CARTESIAN_POINT('Ctrl Pts',(1.63641476948454,28.4112391723817,55.5184516451336));
#107598=CARTESIAN_POINT('Ctrl Pts',(1.64775293039193,28.3679465253655,55.3387616204373));
#107599=CARTESIAN_POINT('Ctrl Pts',(1.65102565499799,28.3580084947632,55.2867422065955));
#107600=CARTESIAN_POINT('Ctrl Pts',(1.65566383450378,28.3477389281926,55.214459010337));
#107601=CARTESIAN_POINT('Ctrl Pts',(1.65695225245788,28.345273939358,55.1945273919168));
#107602=CARTESIAN_POINT('Ctrl Pts',(1.65922912249614,28.3416022271565,55.1596768735656));
#107603=CARTESIAN_POINT('Ctrl Pts',(1.66021021849415,28.3402351105793,55.144776899537));
#107604=CARTESIAN_POINT('Ctrl Pts',(1.66169424919326,28.3384897467637,55.1224536071972));
#107605=CARTESIAN_POINT('Ctrl Pts',(1.66218926588359,28.3379601559401,55.115042422648));
#107606=CARTESIAN_POINT('Ctrl Pts',(1.66308921941328,28.3370923625884,55.1016377135591));
#107607=CARTESIAN_POINT('Ctrl Pts',(1.66349320510095,28.3367369549213,55.0956455702197));
#107608=CARTESIAN_POINT('Ctrl Pts',(1.6644102166037,28.3360070230248,55.082100861987));
#107609=CARTESIAN_POINT('Ctrl Pts',(1.66492424428685,28.3356515321349,55.0745476417261));
#107610=CARTESIAN_POINT('Ctrl Pts',(1.66650955598791,28.3347185531049,55.0513646427978));
#107611=CARTESIAN_POINT('Ctrl Pts',(1.66758933931891,28.3343097566956,55.0357294455583));
#107612=CARTESIAN_POINT('Ctrl Pts',(1.6757861888573,28.3328902581874,54.9180324692068));
#107613=CARTESIAN_POINT('Ctrl Pts',(1.68325974279632,28.3410408456804,54.8160849339055));
#107614=CARTESIAN_POINT('Ctrl Pts',(1.69884571307632,28.3776353914028,54.6049135283959));
#107615=CARTESIAN_POINT('Ctrl Pts',(1.70689902126361,28.4079406611171,54.4964964104152));
#107616=CARTESIAN_POINT('Ctrl Pts',(1.71602137160445,28.4565090893896,54.3726062413552));
#107617=CARTESIAN_POINT('Ctrl Pts',(1.71743285902179,28.4644484000797,54.35341785432));
#107618=CARTESIAN_POINT('Ctrl Pts',(1.71964589679254,28.4775677706495,54.3233155548683));
#107619=CARTESIAN_POINT('Ctrl Pts',(1.72045535448743,28.4825111185041,54.3123014911524));
#107620=CARTESIAN_POINT('Ctrl Pts',(1.72197394412251,28.4920572586976,54.2916364026767));
#107621=CARTESIAN_POINT('Ctrl Pts',(1.72268392131808,28.4966340612578,54.2819741227576));
#107622=CARTESIAN_POINT('Ctrl Pts',(1.72428586243481,28.5072174880883,54.2601758927125));
#107623=CARTESIAN_POINT('Ctrl Pts',(1.72517584585647,28.5132797400498,54.2480676731046));
#107624=CARTESIAN_POINT('Ctrl Pts',(1.7279007153697,28.5323973828499,54.2110190430211));
#107625=CARTESIAN_POINT('Ctrl Pts',(1.72971859866416,28.5459381668397,54.1863337746199));
#107626=CARTESIAN_POINT('Ctrl Pts',(1.73986196903656,28.6257893369015,54.049128380564));
#107627=CARTESIAN_POINT('Ctrl Pts',(1.74771443297892,28.7045222853212,53.9443714226131));
#107628=CARTESIAN_POINT('Ctrl Pts',(1.75895510742115,28.8310035613843,53.8118203862827));
#107629=CARTESIAN_POINT('Ctrl Pts',(1.7622084757703,28.8691003975332,53.7755046818852));
#107630=CARTESIAN_POINT('Ctrl Pts',(1.76742481691253,28.9311394508808,53.7217342598243));
#107631=CARTESIAN_POINT('Ctrl Pts',(1.76932618509085,28.9539383697286,53.703010798017));
#107632=CARTESIAN_POINT('Ctrl Pts',(1.77190001742731,28.9848233937124,53.6789908311738));
#107633=CARTESIAN_POINT('Ctrl Pts',(1.77253770469505,28.9924771643754,53.6731441333751));
#107634=CARTESIAN_POINT('Ctrl Pts',(1.77360030297302,29.0052241327182,53.6635806333742));
#107635=CARTESIAN_POINT('Ctrl Pts',(1.77402263028919,29.0102886472361,53.6598256885007));
#107636=CARTESIAN_POINT('Ctrl Pts',(1.7748790321333,29.0205517785922,53.6523062744813));
#107637=CARTESIAN_POINT('Ctrl Pts',(1.77531316346494,29.025751054369,53.6485429401458));
#107638=CARTESIAN_POINT('Ctrl Pts',(1.77643968277249,29.0392372137466,53.6388996675455));
#107639=CARTESIAN_POINT('Ctrl Pts',(1.77713501381907,29.0475562336769,53.6330654348135));
#107640=CARTESIAN_POINT('Ctrl Pts',(1.78000127547812,29.081847900978,53.6094812622407));
#107641=CARTESIAN_POINT('Ctrl Pts',(1.78220944109247,29.1082657825847,53.5923937263753));
#107642=CARTESIAN_POINT('Ctrl Pts',(1.7921834047149,29.2282112954471,53.5195427930953));
#107643=CARTESIAN_POINT('Ctrl Pts',(1.80020665929339,29.3265877951364,53.4722804099938));
#107644=CARTESIAN_POINT('Ctrl Pts',(1.81220800968084,29.4827655406637,53.4152868022079));
#107645=CARTESIAN_POINT('Ctrl Pts',(1.81630075860788,29.5376438405063,53.3984147595423));
#107646=CARTESIAN_POINT('Ctrl Pts',(1.82295375790556,29.6299151533283,53.3751862352941));
#107647=CARTESIAN_POINT('Ctrl Pts',(1.82555830594628,29.6668475383269,53.3672133032159));
#107648=CARTESIAN_POINT('Ctrl Pts',(1.82915078435788,29.7189097200391,53.3578145262619));
#107649=CARTESIAN_POINT('Ctrl Pts',(1.83017167337182,29.7338340236791,53.3553296455147));
#107650=CARTESIAN_POINT('Ctrl Pts',(1.83191821038516,29.7595833396045,53.3514021036281));
#107651=CARTESIAN_POINT('Ctrl Pts',(1.83264689021625,29.77039227256,53.3498619767445));
#107652=CARTESIAN_POINT('Ctrl Pts',(1.8340385624863,29.7911585120793,53.3471110668164));
#107653=CARTESIAN_POINT('Ctrl Pts',(1.83470204593146,29.8011131045779,53.3458837396373));
#107654=CARTESIAN_POINT('Ctrl Pts',(1.83643840095637,29.8273020336422,53.3428946778498));
#107655=CARTESIAN_POINT('Ctrl Pts',(1.83750658547659,29.8435525035648,53.3412815645414));
#107656=CARTESIAN_POINT('Ctrl Pts',(1.84136466773641,29.9027149308821,53.3362859872617));
#107657=CARTESIAN_POINT('Ctrl Pts',(1.84411054842524,29.9457320033905,53.3343277124911));
#107658=CARTESIAN_POINT('Ctrl Pts',(1.85404050963707,30.1036047654424,53.3332644314698));
#107659=CARTESIAN_POINT('Ctrl Pts',(1.86094049954242,30.2181998099546,53.3443638947905));
#107660=CARTESIAN_POINT('Ctrl Pts',(1.87097559680838,30.378138044721,53.3767606775331));
#107661=CARTESIAN_POINT('Ctrl Pts',(1.87397676478242,30.4250877286833,53.388418771063));
#107662=CARTESIAN_POINT('Ctrl Pts',(1.87883442126873,30.4982724912221,53.4100119522052));
#107663=CARTESIAN_POINT('Ctrl Pts',(1.88063906103567,30.5248793281929,53.418595895637));
#107664=CARTESIAN_POINT('Ctrl Pts',(1.88310065145339,30.5601726003448,53.4309710188183));
#107665=CARTESIAN_POINT('Ctrl Pts',(1.88372653088112,30.5690624433048,53.4341733138086));
#107666=CARTESIAN_POINT('Ctrl Pts',(1.88477477000892,30.5838021380773,53.4396249365411));
#107667=CARTESIAN_POINT('Ctrl Pts',(1.88519468936442,30.5896675709933,53.4418320281007));
#107668=CARTESIAN_POINT('Ctrl Pts',(1.88599902327518,30.6008246053475,53.4461023037309));
#107669=CARTESIAN_POINT('Ctrl Pts',(1.88638305838771,30.6061183576474,53.4481595472037));
#107670=CARTESIAN_POINT('Ctrl Pts',(1.88742242905564,30.6203591087152,53.4537777307764));
#107671=CARTESIAN_POINT('Ctrl Pts',(1.88808065298119,30.6292857570461,53.4573891759503));
#107672=CARTESIAN_POINT('Ctrl Pts',(1.89061116502186,30.6632735111864,53.4714836600468));
#107673=CARTESIAN_POINT('Ctrl Pts',(1.8925109634703,30.6881067549831,53.4825011224374));
#107674=CARTESIAN_POINT('Ctrl Pts',(1.90232643874191,30.8134854672589,53.5418366013268));
#107675=CARTESIAN_POINT('Ctrl Pts',(1.91054940359927,30.9092625715218,53.5995572370022));
#107676=CARTESIAN_POINT('Ctrl Pts',(1.92287904315784,31.0458478202143,53.7018284200254));
#107677=CARTESIAN_POINT('Ctrl Pts',(1.92709918374005,31.0912304092289,53.7397363424899));
#107678=CARTESIAN_POINT('Ctrl Pts',(1.93306878782953,31.1537069462699,53.7978337343026));
#107679=CARTESIAN_POINT('Ctrl Pts',(1.93488616758742,31.1724841225784,53.8161399741545));
#107680=CARTESIAN_POINT('Ctrl Pts',(1.93814322064888,31.2056876787681,53.8500760723677));
#107681=CARTESIAN_POINT('Ctrl Pts',(1.93958896415238,31.2202615054464,53.8655531088244));
#107682=CARTESIAN_POINT('Ctrl Pts',(1.94184294799629,31.2427114999154,53.8903278080177));
#107683=CARTESIAN_POINT('Ctrl Pts',(1.9426595985208,31.2507882782727,53.8994397143947));
#107684=CARTESIAN_POINT('Ctrl Pts',(1.94418453071952,31.2657586511735,53.9167063984218));
#107685=CARTESIAN_POINT('Ctrl Pts',(1.94489373676881,31.2726751026927,53.924840438681));
#107686=CARTESIAN_POINT('Ctrl Pts',(1.94648458733679,31.2880823222194,53.9433169969082));
#107687=CARTESIAN_POINT('Ctrl Pts',(1.94736436352499,31.2965277084127,53.9536965275173));
#107688=CARTESIAN_POINT('Ctrl Pts',(1.94962492938421,31.3180231906617,53.9807748228198));
#107689=CARTESIAN_POINT('Ctrl Pts',(1.95099817639356,31.3308815990393,53.9976231611595));
#107690=CARTESIAN_POINT('Ctrl Pts',(1.96048457186252,31.4181813568334,54.1166543017011));
#107691=CARTESIAN_POINT('Ctrl Pts',(1.96813546344748,31.4811022622504,54.2267744266908));
#107692=CARTESIAN_POINT('Ctrl Pts',(1.98110323404326,31.5647173877109,54.421605940013));
#107693=CARTESIAN_POINT('Ctrl Pts',(1.98636871638347,31.5923547647007,54.5027247491917));
#107694=CARTESIAN_POINT('Ctrl Pts',(1.9928544280686,31.6171410703874,54.5992392132915));
#107695=CARTESIAN_POINT('Ctrl Pts',(1.99377937361443,31.6204718191115,54.6129270081891));
#107696=CARTESIAN_POINT('Ctrl Pts',(1.99519489801449,31.6252544143446,54.6337258784986));
#107697=CARTESIAN_POINT('Ctrl Pts',(1.9956785992869,31.6268341179498,54.6408073063535));
#107698=CARTESIAN_POINT('Ctrl Pts',(1.99656786505943,31.6296378505498,54.6537737636451));
#107699=CARTESIAN_POINT('Ctrl Pts',(1.99697261158695,31.6308763519442,54.6596553928348));
#107700=CARTESIAN_POINT('Ctrl Pts',(1.99790428819096,31.6336415143507,54.6731488542433));
#107701=CARTESIAN_POINT('Ctrl Pts',(1.99843237039652,31.6351468131204,54.6807647224817));
#107702=CARTESIAN_POINT('Ctrl Pts',(2.00006592327948,31.6396151401567,54.7042327551615));
#107703=CARTESIAN_POINT('Ctrl Pts',(2.00118039423116,31.6424011672701,54.7201171157184));
#107704=CARTESIAN_POINT('Ctrl Pts',(2.00843434240002,31.6588863359117,54.8228495023147));
#107705=CARTESIAN_POINT('Ctrl Pts',(2.0148359334606,31.6659214902038,54.9106190018576));
#107706=CARTESIAN_POINT('Ctrl Pts',(2.02993617082025,31.6661052143905,55.118056849621));
#107707=CARTESIAN_POINT('Ctrl Pts',(2.03856946052953,31.6533464665299,55.2372744191505));
#107708=CARTESIAN_POINT('Ctrl Pts',(2.04830036998259,31.6233134415598,55.3753416569323));
#107709=CARTESIAN_POINT('Ctrl Pts',(2.04978357248641,31.6182812322145,55.3964767578125));
#107710=CARTESIAN_POINT('Ctrl Pts',(2.05216955248848,31.6094449571812,55.430611338695));
#107711=CARTESIAN_POINT('Ctrl Pts',(2.05308027434977,31.6058933891001,55.4436728939457));
#107712=CARTESIAN_POINT('Ctrl Pts',(2.054701096337,31.5992524351727,55.466971021231));
#107713=CARTESIAN_POINT('Ctrl Pts',(2.05541309076138,31.5962229790226,55.47722373837));
#107714=CARTESIAN_POINT('Ctrl Pts',(2.05692248619468,31.5895619642043,55.4989935590384));
#107715=CARTESIAN_POINT('Ctrl Pts',(2.0577189617956,31.5859034382728,55.5105018191712));
#107716=CARTESIAN_POINT('Ctrl Pts',(2.05975211463279,31.576196994763,55.5399226136569));
#107717=CARTESIAN_POINT('Ctrl Pts',(2.06098283076197,31.5699686641503,55.5577739909768));
#107718=CARTESIAN_POINT('Ctrl Pts',(2.06220431895159,31.5634376782779,55.5755159651488));
#107719=CARTESIAN_POINT('',(1.82701796270648,31.6659995261751,54.9996754260968));
#107720=CARTESIAN_POINT('Ctrl Pts',(1.86810672180998,31.5634374966623,55.5755164585225));
#107721=CARTESIAN_POINT('Ctrl Pts',(1.86162124916867,31.5942217432641,55.4918885366255));
#107722=CARTESIAN_POINT('Ctrl Pts',(1.85513196704194,31.6182725433958,55.4058535797404));
#107723=CARTESIAN_POINT('Ctrl Pts',(1.84519623197039,31.6450887968234,55.2680535911724));
#107724=CARTESIAN_POINT('Ctrl Pts',(1.8416383236559,31.652540421337,55.217441910937));
#107725=CARTESIAN_POINT('Ctrl Pts',(1.83699844869998,31.6593446954984,55.1497249313236));
#107726=CARTESIAN_POINT('Ctrl Pts',(1.83585274662337,31.660779980928,55.132861827411));
#107727=CARTESIAN_POINT('Ctrl Pts',(1.8339491592536,31.6627512610417,55.1046137945673));
#107728=CARTESIAN_POINT('Ctrl Pts',(1.83318694045077,31.6634278047983,55.0932402889168));
#107729=CARTESIAN_POINT('Ctrl Pts',(1.83175227031401,31.6644865851243,55.0717183387098));
#107730=CARTESIAN_POINT('Ctrl Pts',(1.83107910221284,31.6648928048197,55.0615716525277));
#107731=CARTESIAN_POINT('Ctrl Pts',(1.82982340625863,31.6654799565435,55.0425577175188));
#107732=CARTESIAN_POINT('Ctrl Pts',(1.82924022080164,31.6656829016532,55.0336915593658));
#107733=CARTESIAN_POINT('Ctrl Pts',(1.82810991512576,31.6659399624236,55.0164415316275));
#107734=CARTESIAN_POINT('Ctrl Pts',(1.82756258501001,31.6660016065409,55.0080580840373));
#107735=CARTESIAN_POINT('Ctrl Pts',(1.82701713034439,31.6659999681879,54.9996744265695));
#107736=CARTESIAN_POINT('Ctrl Pts',(1.8270171986045,31.6659999683926,54.9996754757297));
#107737=CARTESIAN_POINT('Ctrl Pts',(1.82545459450402,31.6659952900083,54.9756582024739));
#107738=CARTESIAN_POINT('Ctrl Pts',(1.82390766287911,31.6654712595334,54.9516426944095));
#107739=CARTESIAN_POINT('Ctrl Pts',(1.81315015462543,31.6581516881125,54.7832643755715));
#107740=CARTESIAN_POINT('Ctrl Pts',(1.80453959996092,31.6331175236017,54.6403210644769));
#107741=CARTESIAN_POINT('Ctrl Pts',(1.79300163391142,31.5773144908242,54.4620173072672));
#107742=CARTESIAN_POINT('Ctrl Pts',(1.79036091279522,31.5631434602999,54.4221345953644));
#107743=CARTESIAN_POINT('Ctrl Pts',(1.78602424539879,31.5379874958443,54.3590586422362));
#107744=CARTESIAN_POINT('Ctrl Pts',(1.78436756545193,31.5279578624559,54.3355032268822));
#107745=CARTESIAN_POINT('Ctrl Pts',(1.78207860655124,31.5136128755519,54.3038564981124));
#107746=CARTESIAN_POINT('Ctrl Pts',(1.7814721376765,31.5097670407183,54.2955546965675));
#107747=CARTESIAN_POINT('Ctrl Pts',(1.78044741990471,31.5031982042695,54.2816757882732));
#107748=CARTESIAN_POINT('Ctrl Pts',(1.78003138120708,31.5005119884205,54.2760812991001));
#107749=CARTESIAN_POINT('Ctrl Pts',(1.77922665751888,31.4952808050423,54.2653407102399));
#107750=CARTESIAN_POINT('Ctrl Pts',(1.77883828585564,31.4927404000865,54.2601925565485));
#107751=CARTESIAN_POINT('Ctrl Pts',(1.77777213454489,31.4857222691937,54.2461535724902));
#107752=CARTESIAN_POINT('Ctrl Pts',(1.77709120786874,31.4811914696723,54.2372897565894));
#107753=CARTESIAN_POINT('Ctrl Pts',(1.7743593978341,31.4628120778357,54.2021147411864));
#107754=CARTESIAN_POINT('Ctrl Pts',(1.77227534997809,31.4483404714248,54.1761373406294));
#107755=CARTESIAN_POINT('Ctrl Pts',(1.76236674633126,31.3771367907041,54.0560014286126));
#107756=CARTESIAN_POINT('Ctrl Pts',(1.75426545387636,31.3118715025401,53.967221323938));
#107757=CARTESIAN_POINT('Ctrl Pts',(1.74213386481641,31.1994948296562,53.8423558831478));
#107758=CARTESIAN_POINT('Ctrl Pts',(1.73798944924613,31.1584177609886,53.8012518331443));
#107759=CARTESIAN_POINT('Ctrl Pts',(1.73211358199466,31.0960080514969,53.7450119661342));
#107760=CARTESIAN_POINT('Ctrl Pts',(1.73031656073776,31.0763381613991,53.7281018505269));
#107761=CARTESIAN_POINT('Ctrl Pts',(1.72749013393833,31.0444689505283,53.7019730726805));
#107762=CARTESIAN_POINT('Ctrl Pts',(1.7264489937337,31.0325244545265,53.6924516948419));
#107763=CARTESIAN_POINT('Ctrl Pts',(1.72446897629792,31.0094182648121,53.6745470387924));
#107764=CARTESIAN_POINT('Ctrl Pts',(1.72352910642904,30.9982789087764,53.6661371784974));
#107765=CARTESIAN_POINT('Ctrl Pts',(1.7218760262348,30.9783869572933,53.6515081770223));
#107766=CARTESIAN_POINT('Ctrl Pts',(1.72116062434236,30.9696775921364,53.6452318975485));
#107767=CARTESIAN_POINT('Ctrl Pts',(1.7196634746959,30.9512422684978,53.6322156066511));
#107768=CARTESIAN_POINT('Ctrl Pts',(1.71888246202362,30.9415039114763,53.6254941262773));
#107769=CARTESIAN_POINT('Ctrl Pts',(1.7168150815245,30.9154098789987,53.6078913024881));
#107770=CARTESIAN_POINT('Ctrl Pts',(1.71553563556124,30.8989316521528,53.597194307843));
#107771=CARTESIAN_POINT('Ctrl Pts',(1.70892845913668,30.8122012453888,53.5430484505212));
#107772=CARTESIAN_POINT('Ctrl Pts',(1.70378412295184,30.7389745377882,53.5045743745793));
#107773=CARTESIAN_POINT('Ctrl Pts',(1.69256306151661,30.5713699875706,53.4318449418227));
#107774=CARTESIAN_POINT('Ctrl Pts',(1.68654443308458,30.4761547902633,53.4003599704506));
#107775=CARTESIAN_POINT('Ctrl Pts',(1.67849819986473,30.3511711655311,53.3711864013255));
#107776=CARTESIAN_POINT('Ctrl Pts',(1.67670627845677,30.3234882523873,53.3654633386732));
#107777=CARTESIAN_POINT('Ctrl Pts',(1.67364029107188,30.2766855969896,53.3570230076238));
#107778=CARTESIAN_POINT('Ctrl Pts',(1.67238253268194,30.2576393175246,53.353928852905));
#107779=CARTESIAN_POINT('Ctrl Pts',(1.6705649045693,30.2304153576684,53.3499902330701));
#107780=CARTESIAN_POINT('Ctrl Pts',(1.67001907312608,30.2222777255236,53.3488743010434));
#107781=CARTESIAN_POINT('Ctrl Pts',(1.66906525194994,30.2081303849035,53.3470407228183));
#107782=CARTESIAN_POINT('Ctrl Pts',(1.66865879056953,30.2021244785667,53.3462955756964));
#107783=CARTESIAN_POINT('Ctrl Pts',(1.66778159904653,30.1892142541833,53.3447651985333));
#107784=CARTESIAN_POINT('Ctrl Pts',(1.66731034295626,30.1823091485964,53.343990443292));
#107785=CARTESIAN_POINT('Ctrl Pts',(1.66600022926708,30.1631916496731,53.341966469299));
#107786=CARTESIAN_POINT('Ctrl Pts',(1.6651566249039,30.150970271677,53.3408090349767));
#107787=CARTESIAN_POINT('Ctrl Pts',(1.6592168991312,30.0654620199834,53.3336634369441));
#107788=CARTESIAN_POINT('Ctrl Pts',(1.65391673065422,29.9918691341066,53.3323986358104));
#107789=CARTESIAN_POINT('Ctrl Pts',(1.64756627910136,29.9045673928382,53.3366775421322));
#107790=CARTESIAN_POINT('Ctrl Pts',(1.64655561902706,29.8907013871527,53.3375311157672));
#107791=CARTESIAN_POINT('Ctrl Pts',(1.64017844236694,29.8033223804976,53.3440079722916));
#107792=CARTESIAN_POINT('Ctrl Pts',(1.63481220114361,29.7302352218971,53.3543329734595));
#107793=CARTESIAN_POINT('Ctrl Pts',(1.62652038347741,29.6165109170415,53.3781815319759));
#107794=CARTESIAN_POINT('Ctrl Pts',(1.62352675071475,29.5752986202062,53.3884826222272));
#107795=CARTESIAN_POINT('Ctrl Pts',(1.61845720268266,29.505163266743,53.4088911016016));
#107796=CARTESIAN_POINT('Ctrl Pts',(1.61635984400561,29.4760437236068,53.4182411838164));
#107797=CARTESIAN_POINT('Ctrl Pts',(1.61334192209568,29.4340153478832,53.4330243757939));
#107798=CARTESIAN_POINT('Ctrl Pts',(1.61240094466489,29.4208928935409,53.43782644588));
#107799=CARTESIAN_POINT('Ctrl Pts',(1.61074661247312,29.3977963482315,53.4466095012775));
#107800=CARTESIAN_POINT('Ctrl Pts',(1.61003105491761,29.3877975768246,53.4505228359022));
#107801=CARTESIAN_POINT('Ctrl Pts',(1.60853425910978,29.3668683551399,53.4589483678406));
#107802=CARTESIAN_POINT('Ctrl Pts',(1.60775374939678,29.3559466698598,53.4634808387872));
#107803=CARTESIAN_POINT('Ctrl Pts',(1.60568929300342,29.3270462736511,53.4758367270113));
#107804=CARTESIAN_POINT('Ctrl Pts',(1.60441223239766,29.3091555001576,53.4838620345714));
#107805=CARTESIAN_POINT('Ctrl Pts',(1.59780139379085,29.2165740891088,53.5273706809531));
#107806=CARTESIAN_POINT('Ctrl Pts',(1.5926515337153,29.1444554901765,53.5680644717262));
#107807=CARTESIAN_POINT('Ctrl Pts',(1.58142593811846,28.9923901465746,53.6694761797207));
#107808=CARTESIAN_POINT('Ctrl Pts',(1.57540808406082,28.9143084514867,53.7323869777593));
#107809=CARTESIAN_POINT('Ctrl Pts',(1.56736278156584,28.8220230030647,53.8215582210736));
#107810=CARTESIAN_POINT('Ctrl Pts',(1.56557096281884,28.8022018018608,53.8417106889399));
#107811=CARTESIAN_POINT('Ctrl Pts',(1.56250513301176,28.7697283474813,53.876452072187));
#107812=CARTESIAN_POINT('Ctrl Pts',(1.56124742731583,28.7567993401324,53.8907748981509));
#107813=CARTESIAN_POINT('Ctrl Pts',(1.55942986174889,28.7387256357218,53.9115100166402));
#107814=CARTESIAN_POINT('Ctrl Pts',(1.55888403880474,28.7333746086386,53.9177414464075));
#107815=CARTESIAN_POINT('Ctrl Pts',(1.55793022935023,28.7241612274403,53.9286326237052));
#107816=CARTESIAN_POINT('Ctrl Pts',(1.55752377112301,28.7202778318203,53.9332742622951));
#107817=CARTESIAN_POINT('Ctrl Pts',(1.55664658713342,28.7119901085546,53.9432905789275));
#107818=CARTESIAN_POINT('Ctrl Pts',(1.55617533542854,28.7075941538739,53.9486715995747));
#107819=CARTESIAN_POINT('Ctrl Pts',(1.55486522167967,28.6955250552195,53.9636352845701));
#107820=CARTESIAN_POINT('Ctrl Pts',(1.55402161266648,28.6879241519822,53.9732752794011));
#107821=CARTESIAN_POINT('Ctrl Pts',(1.54807856574748,28.6355148457625,54.0412768276282));
#107822=CARTESIAN_POINT('Ctrl Pts',(1.54277481148151,28.5945138895433,54.1024610031834));
#107823=CARTESIAN_POINT('Ctrl Pts',(1.53642350898985,28.5507604716399,54.1781406808692));
#107824=CARTESIAN_POINT('Ctrl Pts',(1.53541554604558,28.5439759738917,54.190221028372));
#107825=CARTESIAN_POINT('Ctrl Pts',(1.52904081938915,28.5020437887612,54.2671157321701));
#107826=CARTESIAN_POINT('Ctrl Pts',(1.52367434873561,28.471078415021,54.3341229360585));
#107827=CARTESIAN_POINT('Ctrl Pts',(1.51538281450795,28.4294383682575,54.44260012493));
#107828=CARTESIAN_POINT('Ctrl Pts',(1.51238966252254,28.4157435181653,54.4828052975065));
#107829=CARTESIAN_POINT('Ctrl Pts',(1.50732083444693,28.3948543619303,54.5527884341238));
#107830=CARTESIAN_POINT('Ctrl Pts',(1.50522372261267,28.3869175343474,54.5823208456159));
#107831=CARTESIAN_POINT('Ctrl Pts',(1.50220609444681,28.3765440683641,54.6256444867381));
#107832=CARTESIAN_POINT('Ctrl Pts',(1.5012651688785,28.3734615738662,54.6392729823871));
#107833=CARTESIAN_POINT('Ctrl Pts',(1.49961090561002,28.3683141622381,54.6634400481494));
#107834=CARTESIAN_POINT('Ctrl Pts',(1.49889536551323,28.3661790367167,54.6739626653955));
#107835=CARTESIAN_POINT('Ctrl Pts',(1.49739858490073,28.361906545279,54.6961157336074));
#107836=CARTESIAN_POINT('Ctrl Pts',(1.4966180731144,28.3597909716438,54.707749817461));
#107837=CARTESIAN_POINT('Ctrl Pts',(1.49455356233962,28.3544971109928,54.738732560366));
#107838=CARTESIAN_POINT('Ctrl Pts',(1.49327645039224,28.3515361626938,54.7581168412506));
#107839=CARTESIAN_POINT('Ctrl Pts',(1.48666336828763,28.3378726599678,54.8595307272466));
#107840=CARTESIAN_POINT('Ctrl Pts',(1.48151148629976,28.3329476417354,54.9422259193693));
#107841=CARTESIAN_POINT('Ctrl Pts',(1.47028574270696,28.3356854107449,55.1249893805996));
#107842=CARTESIAN_POINT('Ctrl Pts',(1.4642695819662,28.3461916918903,55.2246800784204));
#107843=CARTESIAN_POINT('Ctrl Pts',(1.45622631486988,28.3710513278489,55.3505436374686));
#107844=CARTESIAN_POINT('Ctrl Pts',(1.45443472761848,28.3772314402018,55.378122519316));
#107845=CARTESIAN_POINT('Ctrl Pts',(1.45136925654467,28.3888056774827,55.4242417539828));
#107846=CARTESIAN_POINT('Ctrl Pts',(1.45011167355326,28.39382627003,55.4428702768221));
#107847=CARTESIAN_POINT('Ctrl Pts',(1.44829425887694,28.4014436626229,55.4692985144436));
#107848=CARTESIAN_POINT('Ctrl Pts',(1.44774846134071,28.4037766650638,55.4771734668222));
#107849=CARTESIAN_POINT('Ctrl Pts',(1.44679468340232,28.4079297042952,55.4908205384443));
#107850=CARTESIAN_POINT('Ctrl Pts',(1.44638823104354,28.4097231193882,55.496600512557));
#107851=CARTESIAN_POINT('Ctrl Pts',(1.44551104208058,28.4136433481497,55.5089959295817));
#107852=CARTESIAN_POINT('Ctrl Pts',(1.44503977937014,28.4157800345318,55.515607777103));
#107853=CARTESIAN_POINT('Ctrl Pts',(1.44372960885209,28.4218061357239,55.5338640724257));
#107854=CARTESIAN_POINT('Ctrl Pts',(1.44288595344469,28.4257829089762,55.5454789173592));
#107855=CARTESIAN_POINT('Ctrl Pts',(1.4369315645855,28.4545440905291,55.6265460139007));
#107856=CARTESIAN_POINT('Ctrl Pts',(1.43161561287307,28.4837851026776,55.694322583514));
#107857=CARTESIAN_POINT('Ctrl Pts',(1.42526155549592,28.5236756656456,55.7721469283415));
#107858=CARTESIAN_POINT('Ctrl Pts',(1.42426289883446,28.5300876309351,55.7842844146353));
#107859=CARTESIAN_POINT('Ctrl Pts',(1.41789682521329,28.5718958598099,55.861110930057));
#107860=CARTESIAN_POINT('Ctrl Pts',(1.41252976239839,28.6114064343231,55.9234731705136));
#107861=CARTESIAN_POINT('Ctrl Pts',(1.40423943834486,28.6799580098698,56.0172736240694));
#107862=CARTESIAN_POINT('Ctrl Pts',(1.40124798970957,28.706296106715,56.050565189975));
#107863=CARTESIAN_POINT('Ctrl Pts',(1.39618168343564,28.7537417114864,56.1060426049515));
#107864=CARTESIAN_POINT('Ctrl Pts',(1.39408541939701,28.7742410938291,56.1287184247126));
#107865=CARTESIAN_POINT('Ctrl Pts',(1.3910687584268,28.8050038513502,56.1609200493473));
#107866=CARTESIAN_POINT('Ctrl Pts',(1.39012797114075,28.8147806762966,56.1708997957246));
#107867=CARTESIAN_POINT('Ctrl Pts',(1.38847385639718,28.8322914476585,56.188329923855));
#107868=CARTESIAN_POINT('Ctrl Pts',(1.38775832804057,28.8399739474269,56.1958306058005));
#107869=CARTESIAN_POINT('Ctrl Pts',(1.38626147944064,28.8562694708485,56.2114356439742));
#107870=CARTESIAN_POINT('Ctrl Pts',(1.38548088882809,28.8648973858091,56.219523640689));
#107871=CARTESIAN_POINT('Ctrl Pts',(1.38341595200232,28.8880613567772,56.2407792296484));
#107872=CARTESIAN_POINT('Ctrl Pts',(1.38213849778741,28.9027453236686,56.2537834226763));
#107873=CARTESIAN_POINT('Ctrl Pts',(1.37551350721059,28.9806793800562,56.3203840874707));
#107874=CARTESIAN_POINT('Ctrl Pts',(1.37035093906019,29.0476387778234,56.3694667858024));
#107875=CARTESIAN_POINT('Ctrl Pts',(1.35912456372117,29.2027232024081,56.4662480885993));
#107876=CARTESIAN_POINT('Ctrl Pts',(1.35311749275381,29.2920432085326,56.5113995486379));
#107877=CARTESIAN_POINT('Ctrl Pts',(1.34508516528203,29.4111071176862,56.5587041622979));
#107878=CARTESIAN_POINT('Ctrl Pts',(1.34329479314591,29.437610964459,56.568461630211));
#107879=CARTESIAN_POINT('Ctrl Pts',(1.34023118724796,29.4826074929771,56.583740138446));
#107880=CARTESIAN_POINT('Ctrl Pts',(1.33897422775287,29.5009718970461,56.5896221900902));
#107881=CARTESIAN_POINT('Ctrl Pts',(1.33715755068577,29.5272960708878,56.5975526376363));
#107882=CARTESIAN_POINT('Ctrl Pts',(1.33661185106327,29.5351760729126,56.5998631642844));
#107883=CARTESIAN_POINT('Ctrl Pts',(1.33565816888094,29.5488926446665,56.6037751655902));
#107884=CARTESIAN_POINT('Ctrl Pts',(1.33525171306428,29.5547213811644,56.6054032446893));
#107885=CARTESIAN_POINT('Ctrl Pts',(1.33437441443045,29.5672630641948,56.6088328220225));
#107886=CARTESIAN_POINT('Ctrl Pts',(1.33390304450917,29.5739783496648,56.6106240572732));
#107887=CARTESIAN_POINT('Ctrl Pts',(1.3325923797577,29.5925916017846,56.6154644088117));
#107888=CARTESIAN_POINT('Ctrl Pts',(1.33174833256043,29.6045121023447,56.618423974039));
#107889=CARTESIAN_POINT('Ctrl Pts',(1.32569160292859,29.6896575730394,56.6385666687387));
#107890=CARTESIAN_POINT('Ctrl Pts',(1.3202655089478,29.7639321438001,56.6509035733368));
#107891=CARTESIAN_POINT('Ctrl Pts',(1.31070997068137,29.894793894958,56.6636271464996));
#107892=CARTESIAN_POINT('Ctrl Pts',(1.30660272508455,29.9510524710172,56.6662316696808));
#107893=CARTESIAN_POINT('Ctrl Pts',(1.29817811186969,30.0675683411384,56.665718640139));
#107894=CARTESIAN_POINT('Ctrl Pts',(1.29387263590671,30.1277471969581,56.662187100707));
#107895=CARTESIAN_POINT('Ctrl Pts',(1.28692410013935,30.2263751524321,56.6510095420821));
#107896=CARTESIAN_POINT('Ctrl Pts',(1.28423137128154,30.2649788139003,56.6452552633158));
#107897=CARTESIAN_POINT('Ctrl Pts',(1.28054086101679,30.318398556562,56.6353631569457));
#107898=CARTESIAN_POINT('Ctrl Pts',(1.27950765465472,30.3334107026459,56.6323687164494));
#107899=CARTESIAN_POINT('Ctrl Pts',(1.27774683097975,30.359084741412,56.6268786009717));
#107900=CARTESIAN_POINT('Ctrl Pts',(1.27701604876348,30.369766981032,56.6244839868125));
#107901=CARTESIAN_POINT('Ctrl Pts',(1.27562484554485,30.3901503610339,56.6197032074149));
#107902=CARTESIAN_POINT('Ctrl Pts',(1.27496389274934,30.3998551189811,56.6173347444214));
#107903=CARTESIAN_POINT('Ctrl Pts',(1.27341498931098,30.4226417428048,56.6115559884474));
#107904=CARTESIAN_POINT('Ctrl Pts',(1.27252939093446,30.4357046894401,56.6080734398498));
#107905=CARTESIAN_POINT('Ctrl Pts',(1.26941772926448,30.481703914959,56.5952084759964));
#107906=CARTESIAN_POINT('Ctrl Pts',(1.2672191170551,30.5143931039393,56.5849696322846));
#107907=CARTESIAN_POINT('Ctrl Pts',(1.25644277347106,30.6749036518491,56.529205044749));
#107908=CARTESIAN_POINT('Ctrl Pts',(1.24834585110935,30.797137664849,56.4691952569685));
#107909=CARTESIAN_POINT('Ctrl Pts',(1.2373489311958,30.9462572848193,56.3718425264055));
#107910=CARTESIAN_POINT('Ctrl Pts',(1.23470228392069,30.980870334512,56.3473112755981));
#107911=CARTESIAN_POINT('Ctrl Pts',(1.23035696506312,31.0348454794541,56.3058745178396));
#107912=CARTESIAN_POINT('Ctrl Pts',(1.22869775243213,31.0548191214636,56.2897945078219));
#107913=CARTESIAN_POINT('Ctrl Pts',(1.22640582586112,31.0814091491183,56.2673571174912));
#107914=CARTESIAN_POINT('Ctrl Pts',(1.22579900734392,31.0883568653186,56.2613957092289));
#107915=CARTESIAN_POINT('Ctrl Pts',(1.22477387015729,31.0999320792366,56.2512969065872));
#107916=CARTESIAN_POINT('Ctrl Pts',(1.22435776580286,31.1045863560583,56.2471902452294));
#107917=CARTESIAN_POINT('Ctrl Pts',(1.22349863386286,31.1141030028915,56.2386982568206));
#107918=CARTESIAN_POINT('Ctrl Pts',(1.22305541799609,31.1189626173108,56.2343101432923));
#107919=CARTESIAN_POINT('Ctrl Pts',(1.22187833058131,31.1317407156787,56.2226343547589));
#107920=CARTESIAN_POINT('Ctrl Pts',(1.22114102080575,31.1396145163202,56.2152985443536));
#107921=CARTESIAN_POINT('Ctrl Pts',(1.21782195287873,31.1745048246528,56.1821549588813));
#107922=CARTESIAN_POINT('Ctrl Pts',(1.21518732554207,31.2007177114103,56.1555208490829));
#107923=CARTESIAN_POINT('Ctrl Pts',(1.20585337135115,31.2891848315141,56.0593695155096));
#107924=CARTESIAN_POINT('Ctrl Pts',(1.19900156327357,31.3464777613659,55.9855244947298));
#107925=CARTESIAN_POINT('Ctrl Pts',(1.18770469930283,31.4314555064802,55.8546506428026));
#107926=CARTESIAN_POINT('Ctrl Pts',(1.1832123278711,31.4626265737974,55.8001358997034));
#107927=CARTESIAN_POINT('Ctrl Pts',(1.17690862871526,31.5027993434716,55.7196459222719));
#107928=CARTESIAN_POINT('Ctrl Pts',(1.17502061616985,31.5143508787191,55.6950091230303));
#107929=CARTESIAN_POINT('Ctrl Pts',(1.17165087375399,31.5340909334462,55.6500763802735));
#107930=CARTESIAN_POINT('Ctrl Pts',(1.17016241288042,31.5424926772205,55.629881506246));
#107931=CARTESIAN_POINT('Ctrl Pts',(1.16786919232177,31.5549326156587,55.598237158764));
#107932=CARTESIAN_POINT('Ctrl Pts',(1.16705525638087,31.5592472018856,55.5868997478374));
#107933=CARTESIAN_POINT('Ctrl Pts',(1.16624544379888,31.5634376782622,55.5755159651914));
#107934=CARTESIAN_POINT('Origin',(5.,30.,55.));
#107935=CARTESIAN_POINT('',(0.468131466136091,31.5634376737814,55.5755159773639));
#107936=CARTESIAN_POINT('',(0.659214778542432,31.5634376782623,55.5755159651912));
#107937=CARTESIAN_POINT('',(5.,31.5634376782623,55.5755159651912));
#107938=CARTESIAN_POINT('',(0.428519636557294,31.6659995598398,55.0012110382147));
#107939=CARTESIAN_POINT('Ctrl Pts',(0.468131466136093,31.5634376737814,
55.5755159773639));
#107940=CARTESIAN_POINT('Ctrl Pts',(0.464345120637409,31.5848558755545,
55.5173316264964));
#107941=CARTESIAN_POINT('Ctrl Pts',(0.460549326597193,31.60301167801,55.4579905871979));
#107942=CARTESIAN_POINT('Ctrl Pts',(0.454337482247741,31.6265637629815,
55.3621989390725));
#107943=CARTESIAN_POINT('Ctrl Pts',(0.451994271554866,31.6341331843492,
55.3263526177191));
#107944=CARTESIAN_POINT('Ctrl Pts',(0.448892310075098,31.6423730132732,
55.2797867743918));
#107945=CARTESIAN_POINT('Ctrl Pts',(0.448187753916178,31.6441304562902,
55.2692671198243));
#107946=CARTESIAN_POINT('Ctrl Pts',(0.447044451267056,31.6467972710023,
55.2523035667945));
#107947=CARTESIAN_POINT('Ctrl Pts',(0.44660917319137,31.6477701312234,55.2458697471883));
#107948=CARTESIAN_POINT('Ctrl Pts',(0.445791850431163,31.6495173148384,
55.2338387385693));
#107949=CARTESIAN_POINT('Ctrl Pts',(0.445410339313308,31.6503009011882,
55.2282429847506));
#107950=CARTESIAN_POINT('Ctrl Pts',(0.44460714387084,31.6518841620995,55.2165020060958));
#107951=CARTESIAN_POINT('Ctrl Pts',(0.444185149393181,31.6526780456202,
55.2103560746072));
#107952=CARTESIAN_POINT('Ctrl Pts',(0.443174754118641,31.65448920107,55.1956913104553));
#107953=CARTESIAN_POINT('Ctrl Pts',(0.442584768285556,31.655474981912,55.1871688601511));
#107954=CARTESIAN_POINT('Ctrl Pts',(0.440597126672424,31.6585582222188,
55.1585801863687));
#107955=CARTESIAN_POINT('Ctrl Pts',(0.439185907728137,31.6603569074475,
55.1384843286982));
#107956=CARTESIAN_POINT('Ctrl Pts',(0.435001096303271,31.6645687872148,
55.0793498872961));
#107957=CARTESIAN_POINT('Ctrl Pts',(0.432193622589638,31.6659726121579,
55.0402549587981));
#107958=CARTESIAN_POINT('Ctrl Pts',(0.429364752169372,31.6659996031586,
55.0011499023514));
#107959=CARTESIAN_POINT('',(0.,28.7309291201476,56.0793586530485));
#107960=CARTESIAN_POINT('Ctrl Pts',(0.428519636557294,31.6659995598398,
55.0012110382147));
#107961=CARTESIAN_POINT('Ctrl Pts',(0.424501125348764,31.6660430829186,
54.9413372627796));
#107962=CARTESIAN_POINT('Ctrl Pts',(0.420482614140233,31.6628547021932,
54.8813422492068));
#107963=CARTESIAN_POINT('Ctrl Pts',(0.416464102931704,31.6564216609204,
54.8216091896046));
#107964=CARTESIAN_POINT('Ctrl Pts',(0.412450057222996,31.6499957682515,
54.761942507313));
#107965=CARTESIAN_POINT('Ctrl Pts',(0.408436011514289,31.6403324089542,
54.7025377229252));
#107966=CARTESIAN_POINT('Ctrl Pts',(0.404421965805581,31.6274708361703,
54.6437772081757));
#107967=CARTESIAN_POINT('Ctrl Pts',(0.400410794811274,31.6146184743798,
54.5850587755822));
#107968=CARTESIAN_POINT('Ctrl Pts',(0.396399623816967,31.5985725481162,
54.5269842119095));
#107969=CARTESIAN_POINT('Ctrl Pts',(0.39238845282266,31.5794237286546,54.469927660255));
#107970=CARTESIAN_POINT('Ctrl Pts',(0.38837857024516,31.5602810599308,54.4128894355728));
#107971=CARTESIAN_POINT('Ctrl Pts',(0.384368687667659,31.5380376421222,
54.3568690735601));
#107972=CARTESIAN_POINT('Ctrl Pts',(0.380358805090159,31.5128338933948,
54.3022252433659));
#107973=CARTESIAN_POINT('Ctrl Pts',(0.376345830822693,31.4876107121341,
54.2475392818179));
#107974=CARTESIAN_POINT('Ctrl Pts',(0.372332856555225,31.4594228570205,
54.1942324538898));
#107975=CARTESIAN_POINT('Ctrl Pts',(0.368319882287759,31.4284581866362,
54.1426417265623));
#107976=CARTESIAN_POINT('Ctrl Pts',(0.364305504855201,31.3974826892339,
54.0910329601688));
#107977=CARTESIAN_POINT('Ctrl Pts',(0.360291127422645,31.3637287366319,
54.0411419279943));
#107978=CARTESIAN_POINT('Ctrl Pts',(0.356276749990087,31.3274275547484,
53.9932765588829));
#107979=CARTESIAN_POINT('Ctrl Pts',(0.352255018940661,31.2910598756338,
53.945323509031));
#107980=CARTESIAN_POINT('Ctrl Pts',(0.348233287891235,31.2521359874029,
53.8994039381293));
#107981=CARTESIAN_POINT('Ctrl Pts',(0.344211556841809,31.2109267358645,
53.8557917845215));
#107982=CARTESIAN_POINT('Ctrl Pts',(0.340609642066431,31.1740191927757,
53.8167321710029));
#107983=CARTESIAN_POINT('Ctrl Pts',(0.337007727291054,31.13527922971,53.779523063681));
#107984=CARTESIAN_POINT('Ctrl Pts',(0.333405812515677,31.094923595558,53.7443335156617));
#107985=CARTESIAN_POINT('Ctrl Pts',(0.329325373458233,31.0492066044432,
53.7044689394277));
#107986=CARTESIAN_POINT('Ctrl Pts',(0.325244934400788,31.0012172877576,
53.6670237995497));
#107987=CARTESIAN_POINT('Ctrl Pts',(0.321164495343345,30.9512418930247,
53.6322665241522));
#107988=CARTESIAN_POINT('Ctrl Pts',(0.317043913940585,30.900774852779,53.5971673153177));
#107989=CARTESIAN_POINT('Ctrl Pts',(0.312923332537826,30.8482827832112,
53.5648095557538));
#107990=CARTESIAN_POINT('Ctrl Pts',(0.308802751135066,30.7940968522758,
53.5354296912727));
#107991=CARTESIAN_POINT('Ctrl Pts',(0.304733332277322,30.7405837123521,
53.5064146172161));
#107992=CARTESIAN_POINT('Ctrl Pts',(0.30066391341958,30.6854189962044,53.4803041598103));
#107993=CARTESIAN_POINT('Ctrl Pts',(0.296594494561836,30.6289508082089,
53.4572826309225));
#107994=CARTESIAN_POINT('Ctrl Pts',(0.292527494313683,30.572516181394,53.4342747846004));
#107995=CARTESIAN_POINT('Ctrl Pts',(0.288460494065529,30.514780091052,53.4143524190334));
#107996=CARTESIAN_POINT('Ctrl Pts',(0.284393493817376,30.4561123350777,
53.3976524915644));
#107997=CARTESIAN_POINT('Ctrl Pts',(0.280327407330037,30.3974577603903,
53.3809563161824));
#107998=CARTESIAN_POINT('Ctrl Pts',(0.2762613208427,30.3378724268665,53.3674812812633));
#107999=CARTESIAN_POINT('Ctrl Pts',(0.272195234355361,30.2777410795449,
53.3573144266984));
#108000=CARTESIAN_POINT('Ctrl Pts',(0.268034843298841,30.2162151084686,
53.3469117727124));
#108001=CARTESIAN_POINT('Ctrl Pts',(0.26387445224232,30.1541180189296,53.3399728205527));
#108002=CARTESIAN_POINT('Ctrl Pts',(0.259714061185799,30.0918702755418,
53.3365349860992));
#108003=CARTESIAN_POINT('Ctrl Pts',(0.255642675296597,30.030954226877,53.333170698826));
#108004=CARTESIAN_POINT('Ctrl Pts',(0.251571289407394,29.9698944311992,
53.3331591269708));
#108005=CARTESIAN_POINT('Ctrl Pts',(0.247499903518191,29.9090849219344,
53.3364825072815));
#108006=CARTESIAN_POINT('Ctrl Pts',(0.243295009878012,29.8462813641954,
53.3399148669529));
#108007=CARTESIAN_POINT('Ctrl Pts',(0.239090116237834,29.7837453854805,
53.3469046841571));
#108008=CARTESIAN_POINT('Ctrl Pts',(0.234885222597655,29.7219023645269,
53.3573747520678));
#108009=CARTESIAN_POINT('Ctrl Pts',(0.230680328957476,29.6600593435732,
53.3678448199785));
#108010=CARTESIAN_POINT('Ctrl Pts',(0.226475435317296,29.5989098420213,
53.3817949370555));
#108011=CARTESIAN_POINT('Ctrl Pts',(0.222270541677116,29.5388618222693,
53.3990916387753));
#108012=CARTESIAN_POINT('Ctrl Pts',(0.218232113312067,29.4811910113088,
53.4157035906638));
#108013=CARTESIAN_POINT('Ctrl Pts',(0.214193684947017,29.4242870361325,
53.4354739837199));
#108014=CARTESIAN_POINT('Ctrl Pts',(0.210155256581968,29.3685250348176,
53.4583141148899));
#108015=CARTESIAN_POINT('Ctrl Pts',(0.206029423842659,29.3115561672686,
53.4816485788033));
#108016=CARTESIAN_POINT('Ctrl Pts',(0.20190359110335,29.2557798435259,53.5081871754044));
#108017=CARTESIAN_POINT('Ctrl Pts',(0.197777758364041,29.2015823541271,
53.5377807063375));
#108018=CARTESIAN_POINT('Ctrl Pts',(0.193750441684768,29.1486789848385,
53.566667607057));
#108019=CARTESIAN_POINT('Ctrl Pts',(0.189723125005496,29.097280373175,53.5984649015941));
#108020=CARTESIAN_POINT('Ctrl Pts',(0.185695808326223,29.0477253943993,
53.6329853418752));
#108021=CARTESIAN_POINT('Ctrl Pts',(0.181670839359022,28.9981993035486,
53.6674856585701));
#108022=CARTESIAN_POINT('Ctrl Pts',(0.177645870391821,28.9505151443782,
53.7047056779388));
#108023=CARTESIAN_POINT('Ctrl Pts',(0.17362090142462,28.9049840044379,53.7444140931568));
#108024=CARTESIAN_POINT('Ctrl Pts',(0.169596713967543,28.8594617050743,
53.7841147983704));
#108025=CARTESIAN_POINT('Ctrl Pts',(0.165572526510465,28.8160919892732,
53.8263025973608));
#108026=CARTESIAN_POINT('Ctrl Pts',(0.161548339053389,28.7751521989994,
53.8707064755415));
#108027=CARTESIAN_POINT('Ctrl Pts',(0.157347250035486,28.7324127130412,
53.9170623292305));
#108028=CARTESIAN_POINT('Ctrl Pts',(0.153146161017584,28.6923222014449,
53.9658331994606));
#108029=CARTESIAN_POINT('Ctrl Pts',(0.148945071999681,28.6551506234517,
54.0166708819537));
#108030=CARTESIAN_POINT('Ctrl Pts',(0.144914792838728,28.6194903849928,
54.0654415819959));
#108031=CARTESIAN_POINT('Ctrl Pts',(0.140884513677775,28.5865165179998,
54.1161137639525));
#108032=CARTESIAN_POINT('Ctrl Pts',(0.136854234516822,28.5564222938698,
54.1683513924956));
#108033=CARTESIAN_POINT('Ctrl Pts',(0.13282069613264,28.5263037330152,54.2206312647855));
#108034=CARTESIAN_POINT('Ctrl Pts',(0.128787157748456,28.4990696747672,
54.2744786325056));
#108035=CARTESIAN_POINT('Ctrl Pts',(0.124753619364273,28.4748660351428,
54.3295356913013));
#108036=CARTESIAN_POINT('Ctrl Pts',(0.120712602360063,28.450617519331,54.3846948318881));
#108037=CARTESIAN_POINT('Ctrl Pts',(0.116671585355855,28.4294107979235,
54.4410676451706));
#108038=CARTESIAN_POINT('Ctrl Pts',(0.112630568351645,28.411342132553,54.4982807755341));
#108039=CARTESIAN_POINT('Ctrl Pts',(0.112132135847282,28.4091134831507,
54.5053376337012));
#108040=CARTESIAN_POINT('Ctrl Pts',(0.11163370334292,28.4069325106936,54.5124072648878));
#108041=CARTESIAN_POINT('Ctrl Pts',(0.111135270838558,28.4047993415728,
54.5194889602171));
#108042=CARTESIAN_POINT('Ctrl Pts',(0.10694773358615,28.3868777070868,54.5789852064324));
#108043=CARTESIAN_POINT('Ctrl Pts',(0.102760196333741,28.3722582064485,
54.6395867581065));
#108044=CARTESIAN_POINT('Ctrl Pts',(0.0985726590813334,28.361068114678,
54.7009042372838));
#108045=CARTESIAN_POINT('Ctrl Pts',(0.094394065281421,28.3499019219317,
54.7620907588291));
#108046=CARTESIAN_POINT('Ctrl Pts',(0.0902154714815101,28.3421506564006,
54.823989699565));
#108047=CARTESIAN_POINT('Ctrl Pts',(0.0860368776815976,28.3378913362989,
54.8861984620064));
#108048=CARTESIAN_POINT('Ctrl Pts',(0.081863555698731,28.3336373898605,
54.9483287403381));
#108049=CARTESIAN_POINT('Ctrl Pts',(0.0776902337158637,28.3328666732709,
55.0107675896895));
#108050=CARTESIAN_POINT('Ctrl Pts',(0.0735169117329972,28.3356047239275,
55.0731051638905));
#108051=CARTESIAN_POINT('Ctrl Pts',(0.0693476153733081,28.3383401334363,
55.1353826067179));
#108052=CARTESIAN_POINT('Ctrl Pts',(0.0651783190136198,28.344577566342,
55.1975584921095));
#108053=CARTESIAN_POINT('Ctrl Pts',(0.0610090226539306,28.3542905195358,
55.2592225027079));
#108054=CARTESIAN_POINT('Ctrl Pts',(0.0568425112665161,28.363996984751,
55.3208453234878));
#108055=CARTESIAN_POINT('Ctrl Pts',(0.0526759998791017,28.3771742824678,
55.3819564771624));
#108056=CARTESIAN_POINT('Ctrl Pts',(0.0485094884916872,28.3937442181091,
55.4421519683798));
#108057=CARTESIAN_POINT('Ctrl Pts',(0.0443432162434608,28.4103132027099,
55.5023440046443));
#108058=CARTESIAN_POINT('Ctrl Pts',(0.0401769439952331,28.4302743247372,
55.5616200178857));
#108059=CARTESIAN_POINT('Ctrl Pts',(0.0360106717470066,28.4534988203197,
55.6195886548731));
#108060=CARTESIAN_POINT('Ctrl Pts',(0.0318448920729993,28.4767205700933,
55.6775504382863));
#108061=CARTESIAN_POINT('Ctrl Pts',(0.0276791123989913,28.5032047426116,
55.7342047105123));
#108062=CARTESIAN_POINT('Ctrl Pts',(0.0235133327249839,28.5327742282485,
55.789179659335));
#108063=CARTESIAN_POINT('Ctrl Pts',(0.0193442787315363,28.562366955619,
55.8441978186868));
#108064=CARTESIAN_POINT('Ctrl Pts',(0.0151752247380916,28.5950496116564,
55.8975335963454));
#108065=CARTESIAN_POINT('Ctrl Pts',(0.0110061707446443,28.6305993113128,
55.9488402151169));
#108066=CARTESIAN_POINT('Ctrl Pts',(0.0073374471630959,28.6618826723945,
55.9939894989765));
#108067=CARTESIAN_POINT('Ctrl Pts',(0.00366872358154585,28.6953854232188,
56.0375676592882));
#108068=CARTESIAN_POINT('Ctrl Pts',(-2.66453525910038E-15,28.7309291201476,
56.0793586530485));
#108069=CARTESIAN_POINT('',(0.,31.2524971005285,56.0985476836113));
#108070=CARTESIAN_POINT('Origin',(0.,30.,55.));
#108071=CARTESIAN_POINT('Ctrl Pts',(2.67147415300428E-15,31.2524971005285,
56.0985476836113));
#108072=CARTESIAN_POINT('Ctrl Pts',(1.83597981159629E-5,31.2523211353076,
56.0987483084291));
#108073=CARTESIAN_POINT('Ctrl Pts',(3.6656070824688E-5,31.2521457602486,
56.0989481631351));
#108074=CARTESIAN_POINT('Ctrl Pts',(0.000824856977073492,31.2445898311209,
56.1075546572744));
#108075=CARTESIAN_POINT('Ctrl Pts',(0.00160018034423123,31.2371243889807,
56.1158872690425));
#108076=CARTESIAN_POINT('Ctrl Pts',(0.0110976438791952,31.1452132458219,
56.2164186425925));
#108077=CARTESIAN_POINT('Ctrl Pts',(0.0203386739047423,31.0507368921928,
56.2988984721567));
#108078=CARTESIAN_POINT('Ctrl Pts',(0.0338113421918995,30.8975843292538,
56.4048652618427));
#108079=CARTESIAN_POINT('Ctrl Pts',(0.0381896109813574,30.8453534875539,
56.4369004143079));
#108080=CARTESIAN_POINT('Ctrl Pts',(0.0452509386994067,30.7566195219529,
56.4848069695065));
#108081=CARTESIAN_POINT('Ctrl Pts',(0.0479850563921831,30.7211038969048,
56.5023762710287));
#108082=CARTESIAN_POINT('Ctrl Pts',(0.0517303998707915,30.6708493560734,
56.5250435672022));
#108083=CARTESIAN_POINT('Ctrl Pts',(0.0527777899603529,30.656616890892,
56.5312253351431));
#108084=CARTESIAN_POINT('Ctrl Pts',(0.0545628029434932,30.632060782159,
56.5414857464113));
#108085=CARTESIAN_POINT('Ctrl Pts',(0.0553036355238125,30.6217791529212,
56.5456616168665));
#108086=CARTESIAN_POINT('Ctrl Pts',(0.056804276582878,30.6007730323576,
56.5539496981985));
#108087=CARTESIAN_POINT('Ctrl Pts',(0.0575638025458454,30.5900461949569,
56.5580543635409));
#108088=CARTESIAN_POINT('Ctrl Pts',(0.0594718706053218,30.5628657219638,
56.568134104341));
#108089=CARTESIAN_POINT('Ctrl Pts',(0.060615561867242,30.5463585282036,
56.5739614944509));
#108090=CARTESIAN_POINT('Ctrl Pts',(0.0651444211712528,30.4801836818865,
56.5961560523604));
#108091=CARTESIAN_POINT('Ctrl Pts',(0.0684634539763917,30.4298469161307,
56.6104418433936));
#108092=CARTESIAN_POINT('Ctrl Pts',(0.0791568788711061,30.2633513629574,
56.6493290014665));
#108093=CARTESIAN_POINT('Ctrl Pts',(0.0862781617391556,30.1452383291482,
56.663894336486));
#108094=CARTESIAN_POINT('Ctrl Pts',(0.0968562652397831,29.9756139385913,
56.6666012978211));
#108095=CARTESIAN_POINT('Ctrl Pts',(0.100084655815293,29.924638792038,56.66507483552));
#108096=CARTESIAN_POINT('Ctrl Pts',(0.104178676525356,29.8623061231741,
56.6603402406218));
#108097=CARTESIAN_POINT('Ctrl Pts',(0.104940381370858,29.8508027193609,
56.659346097684));
#108098=CARTESIAN_POINT('Ctrl Pts',(0.106161960988369,29.832522341434,56.6575746595812));
#108099=CARTESIAN_POINT('Ctrl Pts',(0.106617769261076,29.8257379675249,
56.6568751486365));
#108100=CARTESIAN_POINT('Ctrl Pts',(0.107490412906336,29.8128235478706,
56.6554633973033));
#108101=CARTESIAN_POINT('Ctrl Pts',(0.107906844171426,29.8066929315724,
56.6547587305746));
#108102=CARTESIAN_POINT('Ctrl Pts',(0.108834943345581,29.7930992167291,
56.6531196679365));
#108103=CARTESIAN_POINT('Ctrl Pts',(0.109347476754292,29.7856383144847,
56.6521687665214));
#108104=CARTESIAN_POINT('Ctrl Pts',(0.110874759711977,29.7635344966901,
56.6491993679362));
#108105=CARTESIAN_POINT('Ctrl Pts',(0.11189662808557,29.7489121464357,56.647036533615));
#108106=CARTESIAN_POINT('Ctrl Pts',(0.118448471979047,29.6560969241584,
56.6320433127101));
#108107=CARTESIAN_POINT('Ctrl Pts',(0.124191073859531,29.5788810749015,
56.6138436072384));
#108108=CARTESIAN_POINT('Ctrl Pts',(0.135432551178239,29.4313115670386,
56.5677472179664));
#108109=CARTESIAN_POINT('Ctrl Pts',(0.140916869769389,29.3609656178965,
56.5404136788341));
#108110=CARTESIAN_POINT('Ctrl Pts',(0.149296156777252,29.2545748905735,
56.4905272177693));
#108111=CARTESIAN_POINT('Ctrl Pts',(0.15226404725487,29.2171297806641,56.4712051811317));
#108112=CARTESIAN_POINT('Ctrl Pts',(0.157297029857244,29.1539762159922,
56.4355224445658));
#108113=CARTESIAN_POINT('Ctrl Pts',(0.159382911851385,29.127911008596,56.4198386989598));
#108114=CARTESIAN_POINT('Ctrl Pts',(0.1623911100197,29.0905019115551,56.3959100915562));
#108115=CARTESIAN_POINT('Ctrl Pts',(0.163333410471777,29.0788106865775,
56.3882226140059));
#108116=CARTESIAN_POINT('Ctrl Pts',(0.164992836773618,29.0582756200063,
56.3743462651356));
#108117=CARTESIAN_POINT('Ctrl Pts',(0.165712132913501,29.0493926091652,
56.3682171107777));
#108118=CARTESIAN_POINT('Ctrl Pts',(0.167219573811755,29.0308186496625,
56.3551331196595));
#108119=CARTESIAN_POINT('Ctrl Pts',(0.168006957659973,29.0211415386663,
56.348159629608));
#108120=CARTESIAN_POINT('Ctrl Pts',(0.170096504076276,28.9955348448932,
56.329285927887));
#108121=CARTESIAN_POINT('Ctrl Pts',(0.171391576806219,28.9797416927699,
56.3172032368028));
#108122=CARTESIAN_POINT('Ctrl Pts',(0.178581572859988,28.8925967655724,
56.2480242730929));
#108123=CARTESIAN_POINT('Ctrl Pts',(0.184248021750184,28.8258168839281,
56.1854128375601));
#108124=CARTESIAN_POINT('Ctrl Pts',(0.195563713904977,28.7019202403468,
56.0484501502279));
#108125=CARTESIAN_POINT('Ctrl Pts',(0.201192073634327,28.6452632852692,
55.9741381166266));
#108126=CARTESIAN_POINT('Ctrl Pts',(0.209602091530792,28.5732648357742,
55.8611835014227));
#108127=CARTESIAN_POINT('Ctrl Pts',(0.212197524231318,28.5526684593564,
55.8260999130033));
#108128=CARTESIAN_POINT('Ctrl Pts',(0.215568687310567,28.5282918390693,
55.7808623779926));
#108129=CARTESIAN_POINT('Ctrl Pts',(0.216277043595974,28.5232969751751,
55.7713748284425));
#108130=CARTESIAN_POINT('Ctrl Pts',(0.217427156332468,28.5153981723771,
55.7560134513898));
#108131=CARTESIAN_POINT('Ctrl Pts',(0.217865444868287,28.5124366097955,
55.7501693686632));
#108132=CARTESIAN_POINT('Ctrl Pts',(0.218717502412834,28.5067745952872,
55.7388310828383));
#108133=CARTESIAN_POINT('Ctrl Pts',(0.219131006050289,28.5040698497753,
55.7333392522463));
#108134=CARTESIAN_POINT('Ctrl Pts',(0.220163695622516,28.4974202177336,
55.7196476893046));
#108135=CARTESIAN_POINT('Ctrl Pts',(0.220785064485526,28.4935121674317,
55.7114303898661));
#108136=CARTESIAN_POINT('Ctrl Pts',(0.2230250187394,28.4797485635398,55.681868245285));
#108137=CARTESIAN_POINT('Ctrl Pts',(0.224664018238215,28.4702782582574,
55.6603483852834));
#108138=CARTESIAN_POINT('Ctrl Pts',(0.233658549623416,28.4213621754429,
55.5424898549807));
#108139=CARTESIAN_POINT('Ctrl Pts',(0.241313474749086,28.3905586237278,
55.4428196748542));
#108140=CARTESIAN_POINT('Ctrl Pts',(0.255856475213649,28.349538573163,55.2466130624324));
#108141=CARTESIAN_POINT('Ctrl Pts',(0.262732574084232,28.3380368449464,
55.1507480538985));
#108142=CARTESIAN_POINT('Ctrl Pts',(0.270853560327245,28.334174254411,55.0325458625757));
#108143=CARTESIAN_POINT('Ctrl Pts',(0.272342630146473,28.3338904751538,
55.0106667020239));
#108144=CARTESIAN_POINT('Ctrl Pts',(0.274645055299875,28.3341202396614,
54.9765285345599));
#108145=CARTESIAN_POINT('Ctrl Pts',(0.275467564185079,28.3343380541171,
54.9642707172966));
#108146=CARTESIAN_POINT('Ctrl Pts',(0.276992962365944,28.3349962955883,
54.9414260544925));
#108147=CARTESIAN_POINT('Ctrl Pts',(0.27769688979855,28.335402451747,54.9308389266132));
#108148=CARTESIAN_POINT('Ctrl Pts',(0.279262445145711,28.3365353768146,
54.9071970979099));
#108149=CARTESIAN_POINT('Ctrl Pts',(0.280122373210363,28.3373148886055,
54.8941455342565));
#108150=CARTESIAN_POINT('Ctrl Pts',(0.282304998167148,28.3396961325095,
54.8608639867664));
#108151=CARTESIAN_POINT('Ctrl Pts',(0.283620911834001,28.3415140027721,
54.8406512717586));
#108152=CARTESIAN_POINT('Ctrl Pts',(0.293631048118927,28.3582822096851,
54.6859467139495));
#108153=CARTESIAN_POINT('Ctrl Pts',(0.301776924415256,28.389197942145,54.5536961079399));
#108154=CARTESIAN_POINT('Ctrl Pts',(0.314901330963546,28.4630105634767,
54.3523249702993));
#108155=CARTESIAN_POINT('Ctrl Pts',(0.319787514929989,28.4955049501309,
54.2800618458996));
#108156=CARTESIAN_POINT('Ctrl Pts',(0.325858242338115,28.5397332197106,
54.1978912546828));
#108157=CARTESIAN_POINT('Ctrl Pts',(0.32678994045868,28.5466204008419,54.1854785352419));
#108158=CARTESIAN_POINT('Ctrl Pts',(0.328211698808857,28.5572613786767,
54.166865090334));
#108159=CARTESIAN_POINT('Ctrl Pts',(0.328694681296393,28.5608986143964,
54.1605980080032));
#108160=CARTESIAN_POINT('Ctrl Pts',(0.329581771722879,28.5676169682787,
54.1491940703694));
#108161=CARTESIAN_POINT('Ctrl Pts',(0.329985051861543,28.5706850616466,
54.1440498365433));
#108162=CARTESIAN_POINT('Ctrl Pts',(0.330911122899019,28.5777624440121,
54.1323274350608));
#108163=CARTESIAN_POINT('Ctrl Pts',(0.331435040839736,28.5817896769313,
54.1257604337139));
#108164=CARTESIAN_POINT('Ctrl Pts',(0.333082024375022,28.5945263519232,
54.1053110030829));
#108165=CARTESIAN_POINT('Ctrl Pts',(0.33421453204808,28.6033948858236,54.0915294822928));
#108166=CARTESIAN_POINT('Ctrl Pts',(0.340824267351567,28.6558644839782,
54.0125771277401));
#108167=CARTESIAN_POINT('Ctrl Pts',(0.346509541133681,28.7038163245726,
53.9504240108421));
#108168=CARTESIAN_POINT('Ctrl Pts',(0.357115853067144,28.8007587007387,
53.841590449507));
#108169=CARTESIAN_POINT('Ctrl Pts',(0.362022899779359,28.8485682275159,
53.7940571768463));
#108170=CARTESIAN_POINT('Ctrl Pts',(0.370272839559134,28.9349387281348,
53.7180182855952));
#108171=CARTESIAN_POINT('Ctrl Pts',(0.373651723276434,28.9720919153647,
53.6880402897391));
#108172=CARTESIAN_POINT('Ctrl Pts',(0.379288772256287,29.037247746346,53.6399371948873));
#108173=CARTESIAN_POINT('Ctrl Pts',(0.381575400116662,29.0645990448363,
53.620982936451));
#108174=CARTESIAN_POINT('Ctrl Pts',(0.384811013073159,29.1046165366089,
53.5949899801629));
#108175=CARTESIAN_POINT('Ctrl Pts',(0.385784713883485,29.1168338497882,
53.5872784151604));
#108176=CARTESIAN_POINT('Ctrl Pts',(0.387477641220054,29.1383769427103,
53.5740691304188));
#108177=CARTESIAN_POINT('Ctrl Pts',(0.388199389372679,29.1476587105933,
53.5685016683409));
#108178=CARTESIAN_POINT('Ctrl Pts',(0.389691410715679,29.167045108487,53.5571285798178));
#108179=CARTESIAN_POINT('Ctrl Pts',(0.390461121931159,29.1771577455723,
53.5513377127813));
#108180=CARTESIAN_POINT('Ctrl Pts',(0.392457484151237,29.2036704560835,
53.5365227650024));
#108181=CARTESIAN_POINT('Ctrl Pts',(0.393678099810462,29.2201636067752,
53.5276679703333));
#108182=CARTESIAN_POINT('Ctrl Pts',(0.399163327670633,29.2954986011431,
53.4888435015911));
#108183=CARTESIAN_POINT('Ctrl Pts',(0.403315864424741,29.3559444883501,
53.4621085362646));
#108184=CARTESIAN_POINT('Ctrl Pts',(0.41451443773383,29.5254452944506,53.3988918496805));
#108185=CARTESIAN_POINT('Ctrl Pts',(0.421385131033552,29.6369217232387,
53.3699935622469));
#108186=CARTESIAN_POINT('Ctrl Pts',(0.431351459641604,29.7944101138259,
53.3461368985851));
#108187=CARTESIAN_POINT('Ctrl Pts',(0.4341776012236,29.8385872564153,53.3412427745767));
#108188=CARTESIAN_POINT('Ctrl Pts',(0.437810857550247,29.8938795668999,
53.3373468359415));
#108189=CARTESIAN_POINT('Ctrl Pts',(0.43853732886452,29.9048634872641,53.3366821956495));
#108190=CARTESIAN_POINT('Ctrl Pts',(0.439709907753333,29.9224606919825,
53.3357922511445));
#108191=CARTESIAN_POINT('Ctrl Pts',(0.440152303627195,29.9290703515636,
53.3354974446387));
#108192=CARTESIAN_POINT('Ctrl Pts',(0.441008403262815,29.9417999500566,
53.3350056317995));
#108193=CARTESIAN_POINT('Ctrl Pts',(0.441421798811537,29.9479194765934,
53.3348029827983));
#108194=CARTESIAN_POINT('Ctrl Pts',(0.442349261851213,29.961590530056,53.3344256938195));
#108195=CARTESIAN_POINT('Ctrl Pts',(0.442864265507579,29.9691424003378,
53.3342686711598));
#108196=CARTESIAN_POINT('Ctrl Pts',(0.444663580905068,29.9953994953719,
53.3339013336793));
#108197=CARTESIAN_POINT('Ctrl Pts',(0.445960831834122,30.0141062315033,
53.3339547206964));
#108198=CARTESIAN_POINT('Ctrl Pts',(0.454857550442134,30.1411447509441,
53.3364568664201));
#108199=CARTESIAN_POINT('Ctrl Pts',(0.462822343415812,30.2490086222056,
53.3491548485529));
#108200=CARTESIAN_POINT('Ctrl Pts',(0.47689960307504,30.4385638680515,53.3904797244061));
#108201=CARTESIAN_POINT('Ctrl Pts',(0.483033883756178,30.5207366015291,
53.4151559036246));
#108202=CARTESIAN_POINT('Ctrl Pts',(0.491051664193381,30.6285696140749,
53.4568370730676));
#108203=CARTESIAN_POINT('Ctrl Pts',(0.493103366587028,30.6561887941298,
53.4683773163695));
#108204=CARTESIAN_POINT('Ctrl Pts',(0.496069210098696,30.6961281892577,
53.4863442323496));
#108205=CARTESIAN_POINT('Ctrl Pts',(0.497002754327989,30.7087015074602,
53.4921901869558));
#108206=CARTESIAN_POINT('Ctrl Pts',(0.498649231103817,30.7308740344684,
53.5028379186073));
#108207=CARTESIAN_POINT('Ctrl Pts',(0.499364285110635,30.7405024325399,
53.507576699164));
#108208=CARTESIAN_POINT('Ctrl Pts',(0.500865187011454,30.7607060936868,
53.5177639395345));
#108209=CARTESIAN_POINT('Ctrl Pts',(0.501650255515002,30.7712701779175,
53.5232333207597));
#108210=CARTESIAN_POINT('Ctrl Pts',(0.503739044624494,30.7993584242877,
53.5381591775348));
#108211=CARTESIAN_POINT('Ctrl Pts',(0.505035592197242,30.8167734899739,
53.547817641679));
#108212=CARTESIAN_POINT('Ctrl Pts',(0.512569449201807,30.9177357515773,
53.6062026952636));
#108213=CARTESIAN_POINT('Ctrl Pts',(0.518546636043419,30.9970894914989,
53.6618199679902));
#108214=CARTESIAN_POINT('Ctrl Pts',(0.529871425488197,31.1388681621492,
53.7808418367603));
#108215=CARTESIAN_POINT('Ctrl Pts',(0.535214815243482,31.2019256108957,
53.8429606082419));
#108216=CARTESIAN_POINT('Ctrl Pts',(0.543254265624867,31.2856508676295,
53.939705758929));
#108217=CARTESIAN_POINT('Ctrl Pts',(0.545781372741443,31.3104705599105,
53.9705397596888));
#108218=CARTESIAN_POINT('Ctrl Pts',(0.549073637453976,31.3405238789814,
54.0107253184978));
#108219=CARTESIAN_POINT('Ctrl Pts',(0.549774907106035,31.3467993099269,
54.0192858367955));
#108220=CARTESIAN_POINT('Ctrl Pts',(0.550915557698269,31.3567951809981,
54.0331984102282));
#108221=CARTESIAN_POINT('Ctrl Pts',(0.551351547160664,31.3605668750842,
54.0385135196339));
#108222=CARTESIAN_POINT('Ctrl Pts',(0.552203363780374,31.3678384781535,
54.0488891988903));
#108223=CARTESIAN_POINT('Ctrl Pts',(0.552618961901155,31.371341695453,54.0539472488365));
#108224=CARTESIAN_POINT('Ctrl Pts',(0.553660460574954,31.3800120201602,
54.0666150670986));
#108225=CARTESIAN_POINT('Ctrl Pts',(0.554288606335351,31.3851442229303,
54.0742483698756));
#108226=CARTESIAN_POINT('Ctrl Pts',(0.556571975011686,31.4034611217988,
54.1019850442026));
#108227=CARTESIAN_POINT('Ctrl Pts',(0.55824850234757,31.4162728292788,54.1223297263369));
#108228=CARTESIAN_POINT('Ctrl Pts',(0.567250499211459,31.4819470958181,
54.2318030018032));
#108229=CARTESIAN_POINT('Ctrl Pts',(0.574867304558297,31.526845771178,54.3254378698075));
#108230=CARTESIAN_POINT('Ctrl Pts',(0.588424246287592,31.5916261467172,
54.5007779820069));
#108231=CARTESIAN_POINT('Ctrl Pts',(0.594384838700808,31.6145987734815,
54.5809885521008));
#108232=CARTESIAN_POINT('Ctrl Pts',(0.602235581992067,31.637525566472,54.6918466129138));
#108233=CARTESIAN_POINT('Ctrl Pts',(0.604283661190095,31.6427882680995,
54.721261061071));
#108234=CARTESIAN_POINT('Ctrl Pts',(0.607244579136839,31.6493283518256,
54.7644926987932));
#108235=CARTESIAN_POINT('Ctrl Pts',(0.60817678024153,31.6512286668053,54.7782081807424));
#108236=CARTESIAN_POINT('Ctrl Pts',(0.609820963984576,31.6542961946478,
54.8025792443031));
#108237=CARTESIAN_POINT('Ctrl Pts',(0.610535064463687,31.6555319541182,
54.8132252358287));
#108238=CARTESIAN_POINT('Ctrl Pts',(0.612034014795316,31.6579208692689,
54.8356967950003));
#108239=CARTESIAN_POINT('Ctrl Pts',(0.612818085869981,31.6590504294753,
54.8475243078358));
#108240=CARTESIAN_POINT('Ctrl Pts',(0.614904274286197,31.6617322708977,
54.8791803077942));
#108241=CARTESIAN_POINT('Ctrl Pts',(0.6161992268751,31.6630562114821,54.8990265850614));
#108242=CARTESIAN_POINT('Ctrl Pts',(0.623783185459972,31.6687721426706,
55.016296285606));
#108243=CARTESIAN_POINT('Ctrl Pts',(0.62980687651647,31.6649590129717,55.1139341390001));
#108244=CARTESIAN_POINT('Ctrl Pts',(0.640245327946243,31.6433754112351,
55.2832344436734));
#108245=CARTESIAN_POINT('Ctrl Pts',(0.644678555324356,31.6293602331118,
55.3550900063826));
#108246=CARTESIAN_POINT('Ctrl Pts',(0.652476622941987,31.5972936523927,
55.4763911004249));
#108247=CARTESIAN_POINT('Ctrl Pts',(0.655783593749164,31.5815409558817,
55.5263293049961));
#108248=CARTESIAN_POINT('Ctrl Pts',(0.659211143171056,31.5634568606164,
55.5754638529456));
#108249=CARTESIAN_POINT('Ctrl Pts',(0.659212960815814,31.5634472697237,
55.575489909177));
#108250=CARTESIAN_POINT('Ctrl Pts',(0.659214778542432,31.5634376782623,
55.5755159651912));
#108251=CARTESIAN_POINT('Origin',(5.,-30.,55.));
#108252=CARTESIAN_POINT('',(9.56912142374065,-28.4365623107092,55.5755159352313));
#108253=CARTESIAN_POINT('',(9.76070771184276,-28.4365623102018,55.5755159338528));
#108254=CARTESIAN_POINT('',(5.,-28.4365623102018,55.5755159338528));
#108255=CARTESIAN_POINT('',(10.,-31.3346917155535,55.9970727277551));
#108256=CARTESIAN_POINT('Ctrl Pts',(9.76070771184276,-28.4365623102018,
55.5755159338528));
#108257=CARTESIAN_POINT('Ctrl Pts',(9.76500820034434,-28.4587264214961,
55.6357266159905));
#108258=CARTESIAN_POINT('Ctrl Pts',(9.76930868884592,-28.4843410012575,
55.6945691379123));
#108259=CARTESIAN_POINT('Ctrl Pts',(9.7736091773475,-28.5132039305782,55.7516604605484));
#108260=CARTESIAN_POINT('Ctrl Pts',(9.77498260433929,-28.5224217499437,
55.7698934504696));
#108261=CARTESIAN_POINT('Ctrl Pts',(9.77635603133109,-28.5319705443847,
55.7879480397777));
#108262=CARTESIAN_POINT('Ctrl Pts',(9.77772945832288,-28.5418428014225,
55.8058123753309));
#108263=CARTESIAN_POINT('Ctrl Pts',(9.78176793020917,-28.5708715250019,
55.8583412810026));
#108264=CARTESIAN_POINT('Ctrl Pts',(9.78580640209546,-28.6028089144853,
55.9094197125127));
#108265=CARTESIAN_POINT('Ctrl Pts',(9.78984487398175,-28.637485007624,55.95870167182));
#108266=CARTESIAN_POINT('Ctrl Pts',(9.7939707012809,-28.6729111727002,56.0090496397621));
#108267=CARTESIAN_POINT('Ctrl Pts',(9.79809652858006,-28.7111957462312,
56.0575219711458));
#108268=CARTESIAN_POINT('Ctrl Pts',(9.80222235587921,-28.7521073143149,
56.1037752692526));
#108269=CARTESIAN_POINT('Ctrl Pts',(9.80624971620123,-28.7920424870852,
56.1489246863395));
#108270=CARTESIAN_POINT('Ctrl Pts',(9.81027707652325,-28.834480283458,56.1919594013044));
#108271=CARTESIAN_POINT('Ctrl Pts',(9.81430443684527,-28.8791627372751,
56.2325906986861));
#108272=CARTESIAN_POINT('Ctrl Pts',(9.81832944941489,-28.9238191434258,
56.2731983100256));
#108273=CARTESIAN_POINT('Ctrl Pts',(9.82235446198451,-28.9707172287795,
56.311404928579));
#108274=CARTESIAN_POINT('Ctrl Pts',(9.82637947455413,-29.0195622566284,
56.3469587341015));
#108275=CARTESIAN_POINT('Ctrl Pts',(9.83040370552636,-29.0683977995017,
56.3825056356055));
#108276=CARTESIAN_POINT('Ctrl Pts',(9.8344279364986,-29.1191791123094,56.4154004386937));
#108277=CARTESIAN_POINT('Ctrl Pts',(9.83845216747083,-29.1715802553535,
56.445433058526));
#108278=CARTESIAN_POINT('Ctrl Pts',(9.84265321427838,-29.2262837890762,
56.4767852454506));
#108279=CARTESIAN_POINT('Ctrl Pts',(9.84685426108594,-29.2827522879325,
56.5050175498202));
#108280=CARTESIAN_POINT('Ctrl Pts',(9.85105530789349,-29.3405862250839,
56.5299442713546));
#108281=CARTESIAN_POINT('Ctrl Pts',(9.85508562993745,-29.3960698705818,
56.5538580052134));
#108282=CARTESIAN_POINT('Ctrl Pts',(9.85911595198142,-29.4528095736924,
56.5747295449078));
#108283=CARTESIAN_POINT('Ctrl Pts',(9.86314627402539,-29.5104347118588,
56.5924452356823));
#108284=CARTESIAN_POINT('Ctrl Pts',(9.8671798550718,-29.5681064469136,56.6101752517337));
#108285=CARTESIAN_POINT('Ctrl Pts',(9.87121343611822,-29.6266645330332,
56.6247442253542));
#108286=CARTESIAN_POINT('Ctrl Pts',(9.87524701716463,-29.6857276615195,
56.6360895138305));
#108287=CARTESIAN_POINT('Ctrl Pts',(9.87928807622649,-29.7449002894757,
56.6474558357857));
#108288=CARTESIAN_POINT('Ctrl Pts',(9.88332913528834,-29.8045793101271,
56.6555864968878));
#108289=CARTESIAN_POINT('Ctrl Pts',(9.88737019435019,-29.8643793020183,
56.6604707243065));
#108290=CARTESIAN_POINT('Ctrl Pts',(9.88786837262061,-29.8717513933626,
56.6610728476436));
#108291=CARTESIAN_POINT('Ctrl Pts',(9.88836655089103,-29.8791253265308,
56.6616256974425));
#108292=CARTESIAN_POINT('Ctrl Pts',(9.88886472916145,-29.8865003834034,
56.6621293081564));
#108293=CARTESIAN_POINT('Ctrl Pts',(9.89305223342453,-29.9484924130206,
56.6663624755514));
#108294=CARTESIAN_POINT('Ctrl Pts',(9.8972397376876,-30.0108272523294,56.6671303990113));
#108295=CARTESIAN_POINT('Ctrl Pts',(9.90142724195068,-30.0730969702636,
56.6643956359407));
#108296=CARTESIAN_POINT('Ctrl Pts',(9.90560580264708,-30.1352336940947,
56.6616667137084));
#108297=CARTESIAN_POINT('Ctrl Pts',(9.90978436334349,-30.1973050985972,
56.6554500042795));
#108298=CARTESIAN_POINT('Ctrl Pts',(9.91396292403989,-30.2589015472335,
56.6457600034149));
#108299=CARTESIAN_POINT('Ctrl Pts',(9.91813621293491,-30.3204202838853,
56.636082227755));
#108300=CARTESIAN_POINT('Ctrl Pts',(9.92230950182992,-30.3814647846837,
56.6229399359512));
#108301=CARTESIAN_POINT('Ctrl Pts',(9.92648279072493,-30.4416298012493,
56.6063994268701));
#108302=CARTESIAN_POINT('Ctrl Pts',(9.93065205411825,-30.5017367834006,
56.5898748725549));
#108303=CARTESIAN_POINT('Ctrl Pts',(9.93482131751156,-30.5609655066609,
56.5699587383165));
#108304=CARTESIAN_POINT('Ctrl Pts',(9.93899058090487,-30.6189218430517,
56.5467681636863));
#108305=CARTESIAN_POINT('Ctrl Pts',(9.94315705955352,-30.6768394691037,
56.5235930785618));
#108306=CARTESIAN_POINT('Ctrl Pts',(9.94732353820217,-30.733485953722,56.4971480767127));
#108307=CARTESIAN_POINT('Ctrl Pts',(9.95149001685081,-30.7884848346613,
56.4675992864229));
#108308=CARTESIAN_POINT('Ctrl Pts',(9.95565625704499,-30.8434805679236,
56.4380521872593));
#108309=CARTESIAN_POINT('Ctrl Pts',(9.95982249723917,-30.8968284567992,
56.4054018668211));
#108310=CARTESIAN_POINT('Ctrl Pts',(9.96398873743335,-30.948175616757,56.3698609417702));
#108311=CARTESIAN_POINT('Ctrl Pts',(9.96815448544298,-30.999516710747,56.3343242153956));
#108312=CARTESIAN_POINT('Ctrl Pts',(9.9723202334526,-31.0488571554576,56.2958978408706));
#108313=CARTESIAN_POINT('Ctrl Pts',(9.97648598146223,-31.0958738754253,
56.2548372201845));
#108314=CARTESIAN_POINT('Ctrl Pts',(9.98065500484387,-31.1429275628832,
56.2137443150665));
#108315=CARTESIAN_POINT('Ctrl Pts',(9.98482402822551,-31.1876535157859,
56.1700133431822));
#108316=CARTESIAN_POINT('Ctrl Pts',(9.98899305160715,-31.2297632520183,
56.1239387634499));
#108317=CARTESIAN_POINT('Ctrl Pts',(9.99266203440477,-31.2668222664938,
56.0833904563356));
#108318=CARTESIAN_POINT('Ctrl Pts',(9.99633101720238,-31.3018554059886,
56.0410277464068));
#108319=CARTESIAN_POINT('Ctrl Pts',(10.,-31.3346917155535,55.997072727755));
#108320=CARTESIAN_POINT('',(10.,-30.7922981853442,53.5344558739157));
#108321=CARTESIAN_POINT('Origin',(10.,-30.,55.));
#108322=CARTESIAN_POINT('Ctrl Pts',(10.,-30.7922981853442,53.5344558739157));
#108323=CARTESIAN_POINT('Ctrl Pts',(9.9999895507263,-30.7924317913625,53.5345281036111));
#108324=CARTESIAN_POINT('Ctrl Pts',(9.99997912415357,-30.7925650844869,
53.5346001877614));
#108325=CARTESIAN_POINT('Ctrl Pts',(9.99922746147901,-30.8021727116768,
53.5397976234626));
#108326=CARTESIAN_POINT('Ctrl Pts',(9.99848123226477,-30.8115971491062,
53.5450147446011));
#108327=CARTESIAN_POINT('Ctrl Pts',(9.9887478481477,-30.9331383582474,53.6138450241866));
#108328=CARTESIAN_POINT('Ctrl Pts',(9.97920752635469,-31.0375491743558,
53.6901670441422));
#108329=CARTESIAN_POINT('Ctrl Pts',(9.96562194606746,-31.1754837971264,
53.8179303698092));
#108330=CARTESIAN_POINT('Ctrl Pts',(9.96140028395281,-31.2166884014272,
53.8603854672475));
#108331=CARTESIAN_POINT('Ctrl Pts',(9.95455608602756,-31.2809875574851,
53.9341086583401));
#108332=CARTESIAN_POINT('Ctrl Pts',(9.95188652061651,-31.3054008952533,
53.9641513625317));
#108333=CARTESIAN_POINT('Ctrl Pts',(9.94821315572095,-31.3380263903812,
54.007287561637));
#108334=CARTESIAN_POINT('Ctrl Pts',(9.94717501445229,-31.3471351882834,
54.0196840211513));
#108335=CARTESIAN_POINT('Ctrl Pts',(9.94540101462986,-31.3625022167179,
54.0412162572487));
#108336=CARTESIAN_POINT('Ctrl Pts',(9.9446620441781,-31.3688433226312,54.0502913477976));
#108337=CARTESIAN_POINT('Ctrl Pts',(9.94316113007218,-31.3815964603314,
54.0689361512455));
#108338=CARTESIAN_POINT('Ctrl Pts',(9.94239950637326,-31.3880006531753,
54.0785105168658));
#108339=CARTESIAN_POINT('Ctrl Pts',(9.94047814363316,-31.4039804294269,
54.1029451306809));
#108340=CARTESIAN_POINT('Ctrl Pts',(9.93932340119048,-31.4134198898699,
54.1178930121746));
#108341=CARTESIAN_POINT('Ctrl Pts',(9.93467599619422,-31.4507053135286,
54.1790721362612));
#108342=CARTESIAN_POINT('Ctrl Pts',(9.93125419284011,-31.476536662721,54.2264957622331));
#108343=CARTESIAN_POINT('Ctrl Pts',(9.91846158366147,-31.565638033155,54.4108699618767));
#108344=CARTESIAN_POINT('Ctrl Pts',(9.90954918582949,-31.6125064658418,
54.5549057966934));
#108345=CARTESIAN_POINT('Ctrl Pts',(9.89842211506384,-31.6433755242008,
54.7254437253278));
#108346=CARTESIAN_POINT('Ctrl Pts',(9.89695743171525,-31.6469401338778,
54.7477058456394));
#108347=CARTESIAN_POINT('Ctrl Pts',(9.89488686068027,-31.6512723519226,
54.7787901175801));
#108348=CARTESIAN_POINT('Ctrl Pts',(9.89430004866978,-31.6524231747233,
54.7875574536069));
#108349=CARTESIAN_POINT('Ctrl Pts',(9.89329214313155,-31.6542680176757,
54.8025351371788));
#108350=CARTESIAN_POINT('Ctrl Pts',(9.89287292972902,-31.6549970072383,
54.8087411424422));
#108351=CARTESIAN_POINT('Ctrl Pts',(9.89199136166798,-31.6564496852979,
54.8217387086142));
#108352=CARTESIAN_POINT('Ctrl Pts',(9.89152865629633,-31.6571665474248,
54.8285308253323));
#108353=CARTESIAN_POINT('Ctrl Pts',(9.8902558830858,-31.6590147704626,54.8471377684626));
#108354=CARTESIAN_POINT('Ctrl Pts',(9.88944145643934,-31.6600616429765,
54.8589603176703));
#108355=CARTESIAN_POINT('Ctrl Pts',(9.88501590135887,-31.6650282123523,
54.9228063800054));
#108356=CARTESIAN_POINT('Ctrl Pts',(9.88130256055543,-31.6666284927841,
54.9749765033606));
#108357=CARTESIAN_POINT('Ctrl Pts',(9.87047810674105,-31.6641825107861,
55.1251595544139));
#108358=CARTESIAN_POINT('Ctrl Pts',(9.86328280742476,-31.653935251428,55.222863017276));
#108359=CARTESIAN_POINT('Ctrl Pts',(9.8527376184587,-31.6257789510615,55.367144749838));
#108360=CARTESIAN_POINT('Ctrl Pts',(9.84926831083307,-31.6142888003592,
55.4147587925479));
#108361=CARTESIAN_POINT('Ctrl Pts',(9.84350003437192,-31.5913292520589,
55.494342247431));
#108362=CARTESIAN_POINT('Ctrl Pts',(9.84117104050136,-31.5809506733445,
55.5265912076722));
#108363=CARTESIAN_POINT('Ctrl Pts',(9.8378852659409,-31.5647108406881,55.5722309758614));
#108364=CARTESIAN_POINT('Ctrl Pts',(9.83690290765468,-31.5596462140594,
55.5858942011597));
#108365=CARTESIAN_POINT('Ctrl Pts',(9.83519807901544,-31.550491546665,55.609631128162));
#108366=CARTESIAN_POINT('Ctrl Pts',(9.83447302624096,-31.5464810124777,
55.6197343272185));
#108367=CARTESIAN_POINT('Ctrl Pts',(9.83297703475667,-31.5379640059224,
55.640592436894));
#108368=CARTESIAN_POINT('Ctrl Pts',(9.83220663305353,-31.5334429147084,
55.6513407653839));
#108369=CARTESIAN_POINT('Ctrl Pts',(9.83021468689445,-31.5214041070829,
55.6791412205976));
#108370=CARTESIAN_POINT('Ctrl Pts',(9.82899907408536,-31.5137123418511,
55.696116546252));
#108371=CARTESIAN_POINT('Ctrl Pts',(9.82364997459325,-31.4783569714157,
55.7707854021922));
#108372=CARTESIAN_POINT('Ctrl Pts',(9.8196209352178,-31.44766674586,55.8269896200116));
#108373=CARTESIAN_POINT('Ctrl Pts',(9.80666555862741,-31.337086300955,56.0043883113706));
#108374=CARTESIAN_POINT('Ctrl Pts',(9.7981000873514,-31.2446210532701,56.1169171280181));
#108375=CARTESIAN_POINT('Ctrl Pts',(9.78733159535497,-31.1220372754486,
56.2317118161577));
#108376=CARTESIAN_POINT('Ctrl Pts',(9.78584323162145,-31.1049817906408,
56.2470351889401));
#108377=CARTESIAN_POINT('Ctrl Pts',(9.78375101357186,-31.0809555234475,
56.2677414884306));
#108378=CARTESIAN_POINT('Ctrl Pts',(9.78316749508805,-31.0742492733071,
56.2734291560583));
#108379=CARTESIAN_POINT('Ctrl Pts',(9.7821697175137,-31.0627802015948,56.2830011738737));
#108380=CARTESIAN_POINT('Ctrl Pts',(9.78175739471841,-31.0580402140477,
56.2869128459267));
#108381=CARTESIAN_POINT('Ctrl Pts',(9.78089484030599,-31.0481262362839,
56.2950025551221));
#108382=CARTESIAN_POINT('Ctrl Pts',(9.78044431334554,-31.0429487327193,
56.2991759549698));
#108383=CARTESIAN_POINT('Ctrl Pts',(9.77922112279171,-31.0288899855247,
56.3103700104131));
#108384=CARTESIAN_POINT('Ctrl Pts',(9.77844450833406,-31.0199621259124,
56.3173311696475));
#108385=CARTESIAN_POINT('Ctrl Pts',(9.77459103245255,-30.9756214528343,
56.3511831708394));
#108386=CARTESIAN_POINT('Ctrl Pts',(9.77143878767359,-30.9392156813891,
56.376737570432));
#108387=CARTESIAN_POINT('Ctrl Pts',(9.7619054639744,-30.8276186391752,56.4485836171115));
#108388=CARTESIAN_POINT('Ctrl Pts',(9.75542554905745,-30.7497230379969,
56.4903900467147));
#108389=CARTESIAN_POINT('Ctrl Pts',(9.74464520482683,-30.6132492585995,
56.5502164831805));
#108390=CARTESIAN_POINT('Ctrl Pts',(9.74030073825637,-30.5563197766408,
56.5715455366727));
#108391=CARTESIAN_POINT('Ctrl Pts',(9.73330221244073,-30.4609531853645,
56.6014411947685));
#108392=CARTESIAN_POINT('Ctrl Pts',(9.73059706325198,-30.4231545833061,
56.6118413017412));
#108393=CARTESIAN_POINT('Ctrl Pts',(9.72689685990628,-30.3701592184003,
56.6244295927669));
#108394=CARTESIAN_POINT('Ctrl Pts',(9.72586575739022,-30.3552487260126,
56.6277554234771));
#108395=CARTESIAN_POINT('Ctrl Pts',(9.72411086194284,-30.3296332350201,
56.633100282859));
#108396=CARTESIAN_POINT('Ctrl Pts',(9.72338387492583,-30.3189505470272,
56.6352202181431));
#108397=CARTESIAN_POINT('Ctrl Pts',(9.72191376625709,-30.2972073622525,
56.6393138782821));
#108398=CARTESIAN_POINT('Ctrl Pts',(9.72117089719986,-30.2861461435036,
56.6412807812171));
#108399=CARTESIAN_POINT('Ctrl Pts',(9.71931079089906,-30.2582697916766,
56.6459473626901));
#108400=CARTESIAN_POINT('Ctrl Pts',(9.71819821761413,-30.2414313330276,
56.6485014263601));
#108401=CARTESIAN_POINT('Ctrl Pts',(9.71389173401649,-30.1756571723526,
56.6574486152894));
#108402=CARTESIAN_POINT('Ctrl Pts',(9.71075787729547,-30.1264837773524,
56.6619247621374));
#108403=CARTESIAN_POINT('Ctrl Pts',(9.70018132944217,-29.9575452347866,
56.6697595411296));
#108404=CARTESIAN_POINT('Ctrl Pts',(9.69302581855393,-29.8376659477646,
56.6623917367566));
#108405=CARTESIAN_POINT('Ctrl Pts',(9.6831214731309,-29.6796904926494,56.6354198625513));
#108406=CARTESIAN_POINT('Ctrl Pts',(9.68059085175588,-29.640031892613,56.6271505255885));
#108407=CARTESIAN_POINT('Ctrl Pts',(9.67641614440543,-29.5766079541128,
56.6114936648456));
#108408=CARTESIAN_POINT('Ctrl Pts',(9.67480824130579,-29.5526367319564,
56.6050042381909));
#108409=CARTESIAN_POINT('Ctrl Pts',(9.67257868960013,-29.5201803359578,
56.5954341864869));
#108410=CARTESIAN_POINT('Ctrl Pts',(9.67198146693663,-29.5115606595721,
56.59281642225));
#108411=CARTESIAN_POINT('Ctrl Pts',(9.67096952054722,-29.4970892778027,
56.5882930067925));
#108412=CARTESIAN_POINT('Ctrl Pts',(9.67055692859207,-29.4912259825609,
56.5864245547614));
#108413=CARTESIAN_POINT('Ctrl Pts',(9.66975456632122,-29.4798979011573,
56.5827453830793));
#108414=CARTESIAN_POINT('Ctrl Pts',(9.669365077656,-29.4744319869831,56.5809387723855));
#108415=CARTESIAN_POINT('Ctrl Pts',(9.66829238069286,-29.4594655189485,
56.5759058173555));
#108416=CARTESIAN_POINT('Ctrl Pts',(9.66760596238923,-29.4499847634579,
56.5726219817434));
#108417=CARTESIAN_POINT('Ctrl Pts',(9.66482384437344,-29.411921143772,56.559051650655));
#108418=CARTESIAN_POINT('Ctrl Pts',(9.66269348856463,-29.383594161389,56.5480705276859));
#108419=CARTESIAN_POINT('Ctrl Pts',(9.65353982683574,-29.2647002145217,
56.4982001288676));
#108420=CARTESIAN_POINT('Ctrl Pts',(9.64629819090916,-29.1773805179267,
56.4520900750812));
#108421=CARTESIAN_POINT('Ctrl Pts',(9.63445285251202,-29.0401627209945,
56.3632613643615));
#108422=CARTESIAN_POINT('Ctrl Pts',(9.62979898090483,-28.9877781664185,
56.3248311546177));
#108423=CARTESIAN_POINT('Ctrl Pts',(9.62237133318643,-28.9061861294285,
56.2573017133974));
#108424=CARTESIAN_POINT('Ctrl Pts',(9.61953852456733,-28.8755799817851,
56.2300067102434));
#108425=CARTESIAN_POINT('Ctrl Pts',(9.61569165448205,-28.8347575791015,
56.1908020327079));
#108426=CARTESIAN_POINT('Ctrl Pts',(9.61463815165872,-28.8236575723699,
56.1798380830576));
#108427=CARTESIAN_POINT('Ctrl Pts',(9.61285237687562,-28.8049848186099,
56.1608686724202));
#108428=CARTESIAN_POINT('Ctrl Pts',(9.6121167360181,-28.7973346690859,56.1529412258251));
#108429=CARTESIAN_POINT('Ctrl Pts',(9.61072247753064,-28.7829188287173,
56.1377032211147));
#108430=CARTESIAN_POINT('Ctrl Pts',(9.61006327013571,-28.7761389990831,
56.1304067650837));
#108431=CARTESIAN_POINT('Ctrl Pts',(9.60836128941283,-28.7587319146771,
56.1113330564206));
#108432=CARTESIAN_POINT('Ctrl Pts',(9.60732281296323,-28.7482065419591,
56.0994638642334));
#108433=CARTESIAN_POINT('Ctrl Pts',(9.60370527085614,-28.7119034297809,
56.0573285225653));
#108434=CARTESIAN_POINT('Ctrl Pts',(9.60116297775279,-28.6870397505686,
56.0262904803422));
#108435=CARTESIAN_POINT('Ctrl Pts',(9.59053082494693,-28.5864620714503,
55.8910907793065));
#108436=CARTESIAN_POINT('Ctrl Pts',(9.58283499485131,-28.5218515488968,
55.7792362877486));
#108437=CARTESIAN_POINT('Ctrl Pts',(9.57297692957263,-28.4585765100932,
55.6328611417994));
#108438=CARTESIAN_POINT('Ctrl Pts',(9.57106299303262,-28.4471713507646,
55.6043362893767));
#108439=CARTESIAN_POINT('Ctrl Pts',(9.56912142374065,-28.4365623107092,
55.5755159352313));
#108440=CARTESIAN_POINT('Origin',(5.,-30.,55.));
#108441=CARTESIAN_POINT('',(8.86797186106678,-28.4365624698124,55.5755163674483));
#108442=CARTESIAN_POINT('',(9.06224859760916,-28.4365623100358,55.5755159334019));
#108443=CARTESIAN_POINT('',(5.,-28.4365623102018,55.5755159338528));
#108444=CARTESIAN_POINT('',(9.72158590647257,-28.3340000001852,55.0000017306777));
#108445=CARTESIAN_POINT('Ctrl Pts',(9.06224859760915,-28.4365623100358,
55.5755159334018));
#108446=CARTESIAN_POINT('Ctrl Pts',(9.06293925223953,-28.4402324751857,
55.5854862473248));
#108447=CARTESIAN_POINT('Ctrl Pts',(9.06362689414098,-28.4439980831935,
55.5954216415668));
#108448=CARTESIAN_POINT('Ctrl Pts',(9.07227367572701,-28.4927460191911,
55.7204193176186));
#108449=CARTESIAN_POINT('Ctrl Pts',(9.0797793055815,-28.550296491161,55.8301701699813));
#108450=CARTESIAN_POINT('Ctrl Pts',(9.09272385742568,-28.6688828142423,
56.0057230412234));
#108451=CARTESIAN_POINT('Ctrl Pts',(9.09813287492223,-28.7240382781921,
56.0748346903343));
#108452=CARTESIAN_POINT('Ctrl Pts',(9.10491892357804,-28.7956645587084,
56.1512616956104));
#108453=CARTESIAN_POINT('Ctrl Pts',(9.10599668128744,-28.8071059684168,
56.1631126885977));
#108454=CARTESIAN_POINT('Ctrl Pts',(9.10759804419394,-28.8241637427529,
56.1802646644835));
#108455=CARTESIAN_POINT('Ctrl Pts',(9.10811178289267,-28.8296446470031,
56.1856997612915));
#108456=CARTESIAN_POINT('Ctrl Pts',(9.10903056196332,-28.8394571506665,
56.195295934259));
#108457=CARTESIAN_POINT('Ctrl Pts',(9.10943443474575,-28.8437737686655,
56.199471956883));
#108458=CARTESIAN_POINT('Ctrl Pts',(9.11033226203008,-28.8533761183069,
56.2086615511469));
#108459=CARTESIAN_POINT('Ctrl Pts',(9.11082700958379,-28.8586721271647,
56.2136637726093));
#108460=CARTESIAN_POINT('Ctrl Pts',(9.11229690775663,-28.8744251359664,
56.228348618249));
#108461=CARTESIAN_POINT('Ctrl Pts',(9.11327893163169,-28.8849734602126,
56.2379316961005));
#108462=CARTESIAN_POINT('Ctrl Pts',(9.12157709962656,-28.9744078912339,
56.3171118266752));
#108463=CARTESIAN_POINT('Ctrl Pts',(9.12928507060617,-29.0595936277881,
56.3792225741385));
#108464=CARTESIAN_POINT('Ctrl Pts',(9.14455037579019,-29.240137526273,56.486315778396));
#108465=CARTESIAN_POINT('Ctrl Pts',(9.15207139677135,-29.3350692252378,
56.5311431599763));
#108466=CARTESIAN_POINT('Ctrl Pts',(9.16082162778065,-29.4544741908131,
56.5743095113059));
#108467=CARTESIAN_POINT('Ctrl Pts',(9.16233819953936,-29.47550153301,56.5814393084298));
#108468=CARTESIAN_POINT('Ctrl Pts',(9.16476621371594,-29.5096945368631,
56.592276152332));
#108469=CARTESIAN_POINT('Ctrl Pts',(9.16568608273025,-29.5227737084982,
56.5962449306129));
#108470=CARTESIAN_POINT('Ctrl Pts',(9.16731651785406,-29.5461738849994,
56.6030322134154));
#108471=CARTESIAN_POINT('Ctrl Pts',(9.16802907659645,-29.5564758457131,
56.6059130591792));
#108472=CARTESIAN_POINT('Ctrl Pts',(9.16953285683048,-29.578372654003,56.6118095090994));
#108473=CARTESIAN_POINT('Ctrl Pts',(9.17032322088,-29.5899737673449,56.6147996822084));
#108474=CARTESIAN_POINT('Ctrl Pts',(9.17244582798156,-29.621370520841,56.6225319814092));
#108475=CARTESIAN_POINT('Ctrl Pts',(9.1737704504239,-29.6412228620489,56.6270369808837));
#108476=CARTESIAN_POINT('Ctrl Pts',(9.18237025923551,-29.7716661776567,
56.6541341353175));
#108477=CARTESIAN_POINT('Ctrl Pts',(9.18927890005292,-29.8842296768193,
56.6658023665987));
#108478=CARTESIAN_POINT('Ctrl Pts',(9.20241624195797,-30.0993869791171,
56.6661742910775));
#108479=CARTESIAN_POINT('Ctrl Pts',(9.20862919714916,-30.2014393774716,
56.6569342414695));
#108480=CARTESIAN_POINT('Ctrl Pts',(9.21627684966869,-30.3173428481181,
56.6355712725491));
#108481=CARTESIAN_POINT('Ctrl Pts',(9.21729982790151,-30.3326592857006,
56.6325249239855));
#108482=CARTESIAN_POINT('Ctrl Pts',(9.21883460208811,-30.3553174785965,
56.6276862577836));
#108483=CARTESIAN_POINT('Ctrl Pts',(9.21933765095702,-30.3626940090964,
56.6260584597764));
#108484=CARTESIAN_POINT('Ctrl Pts',(9.22024544229879,-30.3759099800456,
56.6230476570874));
#108485=CARTESIAN_POINT('Ctrl Pts',(9.22064913911115,-30.3817533713685,
56.6216831906735));
#108486=CARTESIAN_POINT('Ctrl Pts',(9.22155693640405,-30.3948175656427,
56.6185581011228));
#108487=CARTESIAN_POINT('Ctrl Pts',(9.22206194297282,-30.4020339628245,
56.6167807285658));
#108488=CARTESIAN_POINT('Ctrl Pts',(9.22359194301112,-30.4237508079991,
56.6112775669169));
#108489=CARTESIAN_POINT('Ctrl Pts',(9.22462463028459,-30.4382127126801,
56.607404654866));
#108490=CARTESIAN_POINT('Ctrl Pts',(9.22706393457485,-30.4719613889587,
56.5978774534785));
#108491=CARTESIAN_POINT('Ctrl Pts',(9.22847729085736,-30.4912016862202,
56.5920680690244));
#108492=CARTESIAN_POINT('Ctrl Pts',(9.23365984005963,-30.560772506691,56.5696808522721));
#108493=CARTESIAN_POINT('Ctrl Pts',(9.23749483522645,-30.6104077332117,
56.5510530316408));
#108494=CARTESIAN_POINT('Ctrl Pts',(9.25094771624656,-30.780338231835,56.4778576835971));
#108495=CARTESIAN_POINT('Ctrl Pts',(9.26056312309516,-30.8949926774089,
56.4113792041917));
#108496=CARTESIAN_POINT('Ctrl Pts',(9.27155611086018,-31.0221614749094,
56.3158529296848));
#108497=CARTESIAN_POINT('Ctrl Pts',(9.27340012341623,-31.0433245390844,
56.2991370468007));
#108498=CARTESIAN_POINT('Ctrl Pts',(9.27612501687463,-31.0743249503579,
56.2734046484244));
#108499=CARTESIAN_POINT('Ctrl Pts',(9.27702108322519,-31.0844740865783,
56.2647724977327));
#108500=CARTESIAN_POINT('Ctrl Pts',(9.27862625966872,-31.1025682513995,
56.249004902254));
#108501=CARTESIAN_POINT('Ctrl Pts',(9.27933711215892,-31.1105501999869,
56.2419131440087));
#108502=CARTESIAN_POINT('Ctrl Pts',(9.28085512987648,-31.1275249598017,
56.2265369726383));
#108503=CARTESIAN_POINT('Ctrl Pts',(9.28166125861218,-31.1364959033203,
56.2182292704265));
#108504=CARTESIAN_POINT('Ctrl Pts',(9.28387231140808,-31.1609728163527,
56.1950562688631));
#108505=CARTESIAN_POINT('Ctrl Pts',(9.2852684822894,-31.1762843504367,56.1799883734328));
#108506=CARTESIAN_POINT('Ctrl Pts',(9.29385695711891,-31.2694401842072,
56.0846990464278));
#108507=CARTESIAN_POINT('Ctrl Pts',(9.30069509648075,-31.3393403806675,
55.9971066837057));
#108508=CARTESIAN_POINT('Ctrl Pts',(9.31368930568585,-31.4546887899291,
55.8183111790544));
#108509=CARTESIAN_POINT('Ctrl Pts',(9.31982939229436,-31.5015957314056,
55.7286682986457));
#108510=CARTESIAN_POINT('Ctrl Pts',(9.32740139997794,-31.5461082135954,
55.6207689138374));
#108511=CARTESIAN_POINT('Ctrl Pts',(9.32843414023273,-31.5519142476679,
55.606107891618));
#108512=CARTESIAN_POINT('Ctrl Pts',(9.32998126384525,-31.5602056810896,
55.5842703660201));
#108513=CARTESIAN_POINT('Ctrl Pts',(9.33048672862475,-31.5628517048656,
55.5771552398773));
#108514=CARTESIAN_POINT('Ctrl Pts',(9.33139800273318,-31.5675077089459,
55.5643684862156));
#108515=CARTESIAN_POINT('Ctrl Pts',(9.33180275126667,-31.5695357181002,
55.5587037072991));
#108516=CARTESIAN_POINT('Ctrl Pts',(9.33271206263157,-31.574002648334,55.5460100851986));
#108517=CARTESIAN_POINT('Ctrl Pts',(9.33321752467188,-31.5764251792079,
55.5389758799242));
#108518=CARTESIAN_POINT('Ctrl Pts',(9.33474551486824,-31.5835697411635,
55.5177702221211));
#108519=CARTESIAN_POINT('Ctrl Pts',(9.33577565581616,-31.5881482262139,
55.5035516866736));
#108520=CARTESIAN_POINT('Ctrl Pts',(9.33820703864514,-31.5984160511905,
55.4701310205612));
#108521=CARTESIAN_POINT('Ctrl Pts',(9.33961492299902,-31.6039514758649,
55.4508842837714));
#108522=CARTESIAN_POINT('Ctrl Pts',(9.34476690521399,-31.6227780381693,
55.380683824411));
#108523=CARTESIAN_POINT('Ctrl Pts',(9.34857567270648,-31.6339979886334,
55.3292091247706));
#108524=CARTESIAN_POINT('Ctrl Pts',(9.36193004229679,-31.6645861375307,
55.147996405325));
#108525=CARTESIAN_POINT('Ctrl Pts',(9.37147470611721,-31.6710738317391,
55.0165497831416));
#108526=CARTESIAN_POINT('Ctrl Pts',(9.38242621515086,-31.6602043746123,
54.8585091856916));
#108527=CARTESIAN_POINT('Ctrl Pts',(9.3842897278416,-31.6576685808561,54.8313784026227));
#108528=CARTESIAN_POINT('Ctrl Pts',(9.38703814307414,-31.6528960294267,
54.7910265075426));
#108529=CARTESIAN_POINT('Ctrl Pts',(9.38793856963188,-31.651163482567,54.7777515430919));
#108530=CARTESIAN_POINT('Ctrl Pts',(9.38954939596825,-31.6477590895474,
54.753909791038));
#108531=CARTESIAN_POINT('Ctrl Pts',(9.39026157129356,-31.646145137778,54.7433356225638));
#108532=CARTESIAN_POINT('Ctrl Pts',(9.39178016933653,-31.6424702423539,
54.7207211101581));
#108533=CARTESIAN_POINT('Ctrl Pts',(9.3925855762082,-31.6403784834013,54.7086863548727));
#108534=CARTESIAN_POINT('Ctrl Pts',(9.3947888594805,-31.6342636490974,54.6756621820449));
#108535=CARTESIAN_POINT('Ctrl Pts',(9.39617811114267,-31.6299686970547,
54.6547250241144));
#108536=CARTESIAN_POINT('Ctrl Pts',(9.39925653958761,-31.6194733673752,
54.6081349580547));
#108537=CARTESIAN_POINT('Ctrl Pts',(9.40093914108252,-31.613063903461,54.5825348471223));
#108538=CARTESIAN_POINT('Ctrl Pts',(9.40637463139229,-31.5901957480408,
54.4996107091246));
#108539=CARTESIAN_POINT('Ctrl Pts',(9.41005936867706,-31.5712669266334,
54.4430143776762));
#108540=CARTESIAN_POINT('Ctrl Pts',(9.4205939150763,-31.5080853540179,54.2831805288463));
#108541=CARTESIAN_POINT('Ctrl Pts',(9.42732977788127,-31.4563915375526,
54.183256368342));
#108542=CARTESIAN_POINT('Ctrl Pts',(9.4361514317286,-31.3807813342478,54.0674332831621));
#108543=CARTESIAN_POINT('Ctrl Pts',(9.43783905729265,-31.3659970051774,
54.0459089260239));
#108544=CARTESIAN_POINT('Ctrl Pts',(9.44018158972882,-31.3451600439263,
54.0170501169487));
#108545=CARTESIAN_POINT('Ctrl Pts',(9.44080996623051,-31.339540607661,54.0094057509363));
#108546=CARTESIAN_POINT('Ctrl Pts',(9.44181972215474,-31.3304696530224,
53.9972844606632));
#108547=CARTESIAN_POINT('Ctrl Pts',(9.4421982689784,-31.3270600077186,53.992776249313));
#108548=CARTESIAN_POINT('Ctrl Pts',(9.44299895906726,-31.3198309374382,
53.9833184455798));
#108549=CARTESIAN_POINT('Ctrl Pts',(9.44342147455041,-31.3160065241504,
53.9783729105213));
#108550=CARTESIAN_POINT('Ctrl Pts',(9.44449150750472,-31.3062946332791,
53.9659590089201));
#108551=CARTESIAN_POINT('Ctrl Pts',(9.44514149752914,-31.300370935075,53.9585193902067));
#108552=CARTESIAN_POINT('Ctrl Pts',(9.44777621567138,-31.276249854754,53.9287521407785));
#108553=CARTESIAN_POINT('Ctrl Pts',(9.44979277863327,-31.2575396136645,
53.906848799934));
#108554=CARTESIAN_POINT('Ctrl Pts',(9.45542926711212,-31.2043369205143,
53.8477406187477));
#108555=CARTESIAN_POINT('Ctrl Pts',(9.45909768839969,-31.1686991170854,
53.8116099816927));
#108556=CARTESIAN_POINT('Ctrl Pts',(9.47172458057161,-31.0412385142775,
53.6936726870126));
#108557=CARTESIAN_POINT('Ctrl Pts',(9.48070688070601,-30.942026348135,53.620411760282));
#108558=CARTESIAN_POINT('Ctrl Pts',(9.49175140214039,-30.8051607615466,
53.5410572863816));
#108559=CARTESIAN_POINT('Ctrl Pts',(9.49417917103131,-30.7741215032174,
53.5243530514464));
#108560=CARTESIAN_POINT('Ctrl Pts',(9.49759843923497,-30.7290488303423,
53.5019105256419));
#108561=CARTESIAN_POINT('Ctrl Pts',(9.49861798839922,-30.7154326791235,
53.4953603826383));
#108562=CARTESIAN_POINT('Ctrl Pts',(9.50035228431299,-30.6919739828229,
53.4844658732685));
#108563=CARTESIAN_POINT('Ctrl Pts',(9.50107016476252,-30.6821752256601,
53.4800300486228));
#108564=CARTESIAN_POINT('Ctrl Pts',(9.50253301346504,-30.6620301972741,
53.4711445978106));
#108565=CARTESIAN_POINT('Ctrl Pts',(9.50327762984543,-30.6516803741721,
53.4667043587695));
#108566=CARTESIAN_POINT('Ctrl Pts',(9.50514731649012,-30.6254573448493,
53.4557677506344));
#108567=CARTESIAN_POINT('Ctrl Pts',(9.50626763091572,-30.6095271323434,
53.4494108084193));
#108568=CARTESIAN_POINT('Ctrl Pts',(9.51094699021412,-30.5421213952134,
53.4237119587478));
#108569=CARTESIAN_POINT('Ctrl Pts',(9.51442941034639,-30.4898000691273,
53.4066775493768));
#108570=CARTESIAN_POINT('Ctrl Pts',(9.52473473766321,-30.33024411988,53.3633356490567));
#108571=CARTESIAN_POINT('Ctrl Pts',(9.53135041530668,-30.2211543199084,
53.3450614276894));
#108572=CARTESIAN_POINT('Ctrl Pts',(9.54197303705375,-30.0494914689011,
53.3335924351692));
#108573=CARTESIAN_POINT('Ctrl Pts',(9.54584118843888,-29.9877490583328,
53.3329032054045));
#108574=CARTESIAN_POINT('Ctrl Pts',(9.55065742154364,-29.9141340963614,
53.3361709955755));
#108575=CARTESIAN_POINT('Ctrl Pts',(9.55144757943654,-29.9021561964138,
53.336832396005));
#108576=CARTESIAN_POINT('Ctrl Pts',(9.55270090921045,-29.8833347764164,
53.3380756989943));
#108577=CARTESIAN_POINT('Ctrl Pts',(9.55315944036612,-29.8764856576638,
53.3385706877353));
#108578=CARTESIAN_POINT('Ctrl Pts',(9.5540278250404,-29.863588304781,53.3395829748461));
#108579=CARTESIAN_POINT('Ctrl Pts',(9.55443716751813,-29.8575395593624,
53.3400910067401));
#108580=CARTESIAN_POINT('Ctrl Pts',(9.55541228837665,-29.8432010029824,
53.3413742444181));
#108581=CARTESIAN_POINT('Ctrl Pts',(9.55597963507766,-29.8349140293788,
53.3421785568071));
#108582=CARTESIAN_POINT('Ctrl Pts',(9.55791262463374,-29.80685538861,53.3451143177642));
#108583=CARTESIAN_POINT('Ctrl Pts',(9.55929268811388,-29.7871168162554,
53.3475375568392));
#108584=CARTESIAN_POINT('Ctrl Pts',(9.56274982125294,-29.7382834551279,
53.3544220758374));
#108585=CARTESIAN_POINT('Ctrl Pts',(9.56484276194549,-29.7092550692085,
53.3593021483128));
#108586=CARTESIAN_POINT('Ctrl Pts',(9.57273146158079,-29.6013457664813,
53.3803967296731));
#108587=CARTESIAN_POINT('Ctrl Pts',(9.57863170854992,-29.523544332806,53.4015540115763));
#108588=CARTESIAN_POINT('Ctrl Pts',(9.59116414568343,-29.360567195844,53.4588354995367));
#108589=CARTESIAN_POINT('Ctrl Pts',(9.59775266420647,-29.2762338746358,
53.4965939755112));
#108590=CARTESIAN_POINT('Ctrl Pts',(9.60564497624947,-29.1759671815406,
53.5518905768821));
#108591=CARTESIAN_POINT('Ctrl Pts',(9.60716507294531,-29.1567015847465,
53.5630244078401));
#108592=CARTESIAN_POINT('Ctrl Pts',(9.60960076574813,-29.1259198022432,
53.5816459506195));
#108593=CARTESIAN_POINT('Ctrl Pts',(9.61052475964601,-29.1142636027221,
53.5888956610034));
#108594=CARTESIAN_POINT('Ctrl Pts',(9.61216377771439,-29.0936307767483,
53.6020848949512));
#108595=CARTESIAN_POINT('Ctrl Pts',(9.61288078876066,-29.0846197267271,
53.6079688313926));
#108596=CARTESIAN_POINT('Ctrl Pts',(9.61439537966407,-29.0656213488485,
53.6206384425984));
#108597=CARTESIAN_POINT('Ctrl Pts',(9.61519208187553,-29.0556494602472,
53.627446233963));
#108598=CARTESIAN_POINT('Ctrl Pts',(9.61733564201717,-29.0288873985013,
53.6461463852554));
#108599=CARTESIAN_POINT('Ctrl Pts',(9.61867474065101,-29.0122417381222,
53.6582425810944));
#108600=CARTESIAN_POINT('Ctrl Pts',(9.62162446182995,-28.9757834746243,
53.6857826327796));
#108601=CARTESIAN_POINT('Ctrl Pts',(9.62322938883063,-28.9560873070933,
53.7013725838815));
#108602=CARTESIAN_POINT('Ctrl Pts',(9.62831039557595,-28.8943328442518,
53.7525658937851));
#108603=CARTESIAN_POINT('Ctrl Pts',(9.63172889701348,-28.8536836290377,
53.7898135885128));
#108604=CARTESIAN_POINT('Ctrl Pts',(9.64164017127283,-28.7403816030223,
53.9044756750137));
#108605=CARTESIAN_POINT('Ctrl Pts',(9.64801663953327,-28.6731954207139,
53.9868867254564));
#108606=CARTESIAN_POINT('Ctrl Pts',(9.65698296904393,-28.5942444095642,
54.1051743135878));
#108607=CARTESIAN_POINT('Ctrl Pts',(9.65929641099807,-28.575168431265,54.1358724844858));
#108608=CARTESIAN_POINT('Ctrl Pts',(9.66236915911345,-28.5517514234138,
54.1764425714994));
#108609=CARTESIAN_POINT('Ctrl Pts',(9.66307682217678,-28.5464855587735,
54.1857724322418));
#108610=CARTESIAN_POINT('Ctrl Pts',(9.66422796605379,-28.5381313958928,
54.2009133458744));
#108611=CARTESIAN_POINT('Ctrl Pts',(9.6646680359289,-28.5349867978189,54.2066932428746));
#108612=CARTESIAN_POINT('Ctrl Pts',(9.66553988730539,-28.5288553286742,
54.2181239178098));
#108613=CARTESIAN_POINT('Ctrl Pts',(9.66597152911856,-28.525866582324,54.2237735411965));
#108614=CARTESIAN_POINT('Ctrl Pts',(9.66705364139782,-28.5184884739654,
54.2379166682481));
#108615=CARTESIAN_POINT('Ctrl Pts',(9.66770646402914,-28.5141396418008,
54.2464308978936));
#108616=CARTESIAN_POINT('Ctrl Pts',(9.67027370243341,-28.4974259497794,
54.2798605076404));
#108617=CARTESIAN_POINT('Ctrl Pts',(9.67221643695832,-28.4856132568221,
54.3050451472343));
#108618=CARTESIAN_POINT('Ctrl Pts',(9.67756592902582,-28.4551879071138,
54.3743753946855));
#108619=CARTESIAN_POINT('Ctrl Pts',(9.68101367702895,-28.437840339896,54.4190462898142));
#108620=CARTESIAN_POINT('Ctrl Pts',(9.69456347867808,-28.3776483703072,
54.5963357292153));
#108621=CARTESIAN_POINT('Ctrl Pts',(9.7046919813584,-28.3495734734474,54.7333991472846));
#108622=CARTESIAN_POINT('Ctrl Pts',(9.71584768315985,-28.3371437734708,
54.8951754240954));
#108623=CARTESIAN_POINT('Ctrl Pts',(9.71740609096478,-28.3358614383319,
54.9180124536265));
#108624=CARTESIAN_POINT('Ctrl Pts',(9.71973947582919,-28.3346347042239,
54.9525539573496));
#108625=CARTESIAN_POINT('Ctrl Pts',(9.72052498555687,-28.3343427385083,
54.96424256035));
#108626=CARTESIAN_POINT('Ctrl Pts',(9.72184116965428,-28.3340583620148,
54.9839264509187));
#108627=CARTESIAN_POINT('Ctrl Pts',(9.72237383948339,-28.3340004141805,
54.9919201945016));
#108628=CARTESIAN_POINT('Ctrl Pts',(9.72290474247879,-28.3340000022123,
54.999914142671));
#108629=CARTESIAN_POINT('Ctrl Pts',(9.72148036344419,-28.3340000000229,
55.0000087401189));
#108630=CARTESIAN_POINT('Ctrl Pts',(9.72575161781573,-28.3340003369473,
55.0642316688592));
#108631=CARTESIAN_POINT('Ctrl Pts',(9.73002287218727,-28.3377185882288,
55.1283809457949));
#108632=CARTESIAN_POINT('Ctrl Pts',(9.73429412655882,-28.345103558767,55.1920254378838));
#108633=CARTESIAN_POINT('Ctrl Pts',(9.73869639077281,-28.3527150444557,
55.2576220625679));
#108634=CARTESIAN_POINT('Ctrl Pts',(9.7430986549868,-28.3642217675405,55.3226819356344));
#108635=CARTESIAN_POINT('Ctrl Pts',(9.74750091920079,-28.3795114745026,
55.3867466079117));
#108636=CARTESIAN_POINT('Ctrl Pts',(9.75190318341478,-28.3948011814646,
55.4508112801889));
#108637=CARTESIAN_POINT('Ctrl Pts',(9.75630544762877,-28.4138736612379,
55.5138803007899));
#108638=CARTESIAN_POINT('Ctrl Pts',(9.76070771184276,-28.4365623102018,
55.5755159338528));
#108639=CARTESIAN_POINT('Ctrl Pts',(9.56912142374065,-28.4365623107092,
55.5755159352313));
#108640=CARTESIAN_POINT('Ctrl Pts',(9.56843982933344,-28.4328379716411,
55.5653984533158));
#108641=CARTESIAN_POINT('Ctrl Pts',(9.56775482209394,-28.4292117451295,
55.5552445547067));
#108642=CARTESIAN_POINT('Ctrl Pts',(9.56545070081313,-28.4174148268356,
55.5211708329592));
#108643=CARTESIAN_POINT('Ctrl Pts',(9.56381428263611,-28.4096906314247,
55.4971024197191));
#108644=CARTESIAN_POINT('Ctrl Pts',(9.56154800177924,-28.3999277035981,
55.4641205574211));
#108645=CARTESIAN_POINT('Ctrl Pts',(9.56094315248967,-28.3974100062228,
55.4553510162443));
#108646=CARTESIAN_POINT('Ctrl Pts',(9.55991948585289,-28.3932987692135,
55.4405743698173));
#108647=CARTESIAN_POINT('Ctrl Pts',(9.55950284485447,-28.391666536423,55.4345780581646));
#108648=CARTESIAN_POINT('Ctrl Pts',(9.55864108061242,-28.3883756569633,
55.4222158820929));
#108649=CARTESIAN_POINT('Ctrl Pts',(9.55819575267008,-28.3867211118918,
55.4158491307793));
#108650=CARTESIAN_POINT('Ctrl Pts',(9.55700855891035,-28.3824307669899,
55.3989286959595));
#108651=CARTESIAN_POINT('Ctrl Pts',(9.55626316310687,-28.3798606038035,
55.3883589180524));
#108652=CARTESIAN_POINT('Ctrl Pts',(9.55285032949156,-28.3686428085694,
55.340175377312));
#108653=CARTESIAN_POINT('Ctrl Pts',(9.55012650698277,-28.3612010007808,
55.3022960426285));
#108654=CARTESIAN_POINT('Ctrl Pts',(9.54076273385981,-28.340433079154,55.1729923015376));
#108655=CARTESIAN_POINT('Ctrl Pts',(9.53398086220428,-28.3333953684809,
55.0807302803421));
#108656=CARTESIAN_POINT('Ctrl Pts',(9.52053162090534,-28.3346934974039,
54.89491061205));
#108657=CARTESIAN_POINT('Ctrl Pts',(9.51389170401175,-28.3432082207743,
54.8016675754));
#108658=CARTESIAN_POINT('Ctrl Pts',(9.50615126326317,-28.3629221622149,
54.6902949781091));
#108659=CARTESIAN_POINT('Ctrl Pts',(9.504819026515,-28.366683601444,54.6710339731172));
#108660=CARTESIAN_POINT('Ctrl Pts',(9.50270080794925,-28.3732571062508,
54.6402729633543));
#108661=CARTESIAN_POINT('Ctrl Pts',(9.50190803913437,-28.3758528513925,
54.6287291616344));
#108662=CARTESIAN_POINT('Ctrl Pts',(9.5004030200086,-28.3810394896025,54.6067592945939));
#108663=CARTESIAN_POINT('Ctrl Pts',(9.49969011667312,-28.3836086688535,
54.5963287718655));
#108664=CARTESIAN_POINT('Ctrl Pts',(9.49807241286668,-28.3896945298868,
54.5726112054111));
#108665=CARTESIAN_POINT('Ctrl Pts',(9.49716971639863,-28.3932751389009,
54.5593412564179));
#108666=CARTESIAN_POINT('Ctrl Pts',(9.49430665080666,-28.4052188461538,
54.5171596376686));
#108667=CARTESIAN_POINT('Ctrl Pts',(9.49236626320087,-28.4142015647743,
54.4884286494787));
#108668=CARTESIAN_POINT('Ctrl Pts',(9.48140364221558,-28.4699402372424,
54.325763453626));
#108669=CARTESIAN_POINT('Ctrl Pts',(9.47294371389912,-28.5328687792529,
54.1979997753101));
#108670=CARTESIAN_POINT('Ctrl Pts',(9.46152684923223,-28.6350523915768,
54.0437913974955));
#108671=CARTESIAN_POINT('Ctrl Pts',(9.45883675440065,-28.6602665261369,
54.0087731918474));
#108672=CARTESIAN_POINT('Ctrl Pts',(9.45442796353356,-28.7027690980143,
53.9543324535729));
#108673=CARTESIAN_POINT('Ctrl Pts',(9.45275016278633,-28.7192032270749,
53.9342664120844));
#108674=CARTESIAN_POINT('Ctrl Pts',(9.45043648313065,-28.7420876220084,
53.9076186681539));
#108675=CARTESIAN_POINT('Ctrl Pts',(9.44982713344136,-28.7481348478599,
53.9006937841948));
#108676=CARTESIAN_POINT('Ctrl Pts',(9.44879896852383,-28.7583650458036,
53.8891727145041));
#108677=CARTESIAN_POINT('Ctrl Pts',(9.44838239755285,-28.7625170994122,
53.8845491105663));
#108678=CARTESIAN_POINT('Ctrl Pts',(9.44752390494259,-28.7710860209794,
53.8751137422702));
#108679=CARTESIAN_POINT('Ctrl Pts',(9.44708180805566,-28.7755054557552,
53.8703045684471));
#108680=CARTESIAN_POINT('Ctrl Pts',(9.44591019537158,-28.7872380805656,
53.8576870039915));
#108681=CARTESIAN_POINT('Ctrl Pts',(9.44517729170724,-28.7945982635757,
53.8499230056618));
#108682=CARTESIAN_POINT('Ctrl Pts',(9.44190864263936,-28.8275367866623,
53.8158408435692));
#108683=CARTESIAN_POINT('Ctrl Pts',(9.43932188267386,-28.8539040904638,
53.7903030928028));
#108684=CARTESIAN_POINT('Ctrl Pts',(9.42913576754911,-28.9595985416822,
53.6944928522457));
#108685=CARTESIAN_POINT('Ctrl Pts',(9.42133171400559,-29.0447157504235,
53.6309797445694));
#108686=CARTESIAN_POINT('Ctrl Pts',(9.40776038693575,-29.2056130035749,
53.5332777111057));
#108687=CARTESIAN_POINT('Ctrl Pts',(9.4019419353104,-29.2790118032807,53.4958375566414));
#108688=CARTESIAN_POINT('Ctrl Pts',(9.39496989100612,-29.3729447943659,
53.4563869188035));
#108689=CARTESIAN_POINT('Ctrl Pts',(9.39364026752912,-29.3911349317075,
53.449121874289));
#108690=CARTESIAN_POINT('Ctrl Pts',(9.391525854498,-29.4204964220282,53.4379913024474));
#108691=CARTESIAN_POINT('Ctrl Pts',(9.39073429734198,-29.4315876706034,
53.4339211372488));
#108692=CARTESIAN_POINT('Ctrl Pts',(9.38923139282455,-29.4528321573832,
53.4263804602427));
#108693=CARTESIAN_POINT('Ctrl Pts',(9.38851939509967,-29.4629774129986,
53.4228893969851));
#108694=CARTESIAN_POINT('Ctrl Pts',(9.38688812482984,-29.4864026205342,
53.4150808520019));
#108695=CARTESIAN_POINT('Ctrl Pts',(9.38597113856145,-29.4997046624214,
53.4108317997254));
#108696=CARTESIAN_POINT('Ctrl Pts',(9.38306414242658,-29.5422838554441,
53.3978184219363));
#108697=CARTESIAN_POINT('Ctrl Pts',(9.38109475180961,-29.5717503830855,
53.3896918520039));
#108698=CARTESIAN_POINT('Ctrl Pts',(9.37644359037693,-29.6426284050969,
53.3722278097989));
#108699=CARTESIAN_POINT('Ctrl Pts',(9.37378432443822,-29.6842061876161,
53.3636530297656));
#108700=CARTESIAN_POINT('Ctrl Pts',(9.3665790489543,-29.7988468226766,53.3445431817866));
#108701=CARTESIAN_POINT('Ctrl Pts',(9.36210110838623,-29.872352442782,53.3372593860087));
#108702=CARTESIAN_POINT('Ctrl Pts',(9.35677680363508,-29.9593516241079,
53.3344431782267));
#108703=CARTESIAN_POINT('Ctrl Pts',(9.35596467135432,-29.9726088394847,
53.3341724169929));
#108704=CARTESIAN_POINT('Ctrl Pts',(9.35059042223113,-30.060133318606,53.3334299438422));
#108705=CARTESIAN_POINT('Ctrl Pts',(9.34597602956322,-30.1343488081574,
53.3377667565187));
#108706=CARTESIAN_POINT('Ctrl Pts',(9.34032438422154,-30.2201947115743,
53.348570033923));
#108707=CARTESIAN_POINT('Ctrl Pts',(9.33951636813612,-30.2323546219843,
53.3502370013402));
#108708=CARTESIAN_POINT('Ctrl Pts',(9.33823994150718,-30.2513637382742,
53.3530572276845));
#108709=CARTESIAN_POINT('Ctrl Pts',(9.33777641073297,-30.2582263202643,
53.354119266971));
#108710=CARTESIAN_POINT('Ctrl Pts',(9.33690444727359,-30.2710552563362,
53.3561868549869));
#108711=CARTESIAN_POINT('Ctrl Pts',(9.3364965877071,-30.2770230327132,53.3571820422393));
#108712=CARTESIAN_POINT('Ctrl Pts',(9.33553098709224,-30.2910759625075,
53.3596042581156));
#108713=CARTESIAN_POINT('Ctrl Pts',(9.33497176309603,-30.2991561388637,
53.3610585722903));
#108714=CARTESIAN_POINT('Ctrl Pts',(9.3330897392773,-30.3261652793219,53.3661262066272));
#108715=CARTESIAN_POINT('Ctrl Pts',(9.33175344091018,-30.3450414642944,
53.370008076396));
#108716=CARTESIAN_POINT('Ctrl Pts',(9.32842802591731,-30.3913787009429,
53.3803781970309));
#108717=CARTESIAN_POINT('Ctrl Pts',(9.32642439701582,-30.4187498854221,
53.3872382611992));
#108718=CARTESIAN_POINT('Ctrl Pts',(9.31726137253638,-30.5419721526149,
53.4214697600547));
#108719=CARTESIAN_POINT('Ctrl Pts',(9.30993076456218,-30.6354233282733,
53.4567148252314));
#108720=CARTESIAN_POINT('Ctrl Pts',(9.29674502322023,-30.8000262380954,
53.536296368608));
#108721=CARTESIAN_POINT('Ctrl Pts',(9.2908622671464,-30.8720824507001,53.5780484288349));
#108722=CARTESIAN_POINT('Ctrl Pts',(9.28382709947328,-30.9569245390145,
53.6360951194296));
#108723=CARTESIAN_POINT('Ctrl Pts',(9.28249479011752,-30.9729240730013,
53.6474616819082));
#108724=CARTESIAN_POINT('Ctrl Pts',(9.28037659732261,-30.9982412846925,
53.6661295821638));
#108725=CARTESIAN_POINT('Ctrl Pts',(9.27958392229206,-31.0076880679296,
53.6732518233335));
#108726=CARTESIAN_POINT('Ctrl Pts',(9.27807917023678,-31.0255643299315,
53.6870304118883));
#108727=CARTESIAN_POINT('Ctrl Pts',(9.27736643937243,-31.0340068325236,
53.6936687963469));
#108728=CARTESIAN_POINT('Ctrl Pts',(9.27573384209259,-31.0532839107511,
53.7091304413902));
#108729=CARTESIAN_POINT('Ctrl Pts',(9.27481625973758,-31.0640729577196,
53.7180093704176));
#108730=CARTESIAN_POINT('Ctrl Pts',(9.27190858983632,-31.0980995111877,
53.746737321285));
#108731=CARTESIAN_POINT('Ctrl Pts',(9.26993908930246,-31.1209039444224,
53.7670910766533));
#108732=CARTESIAN_POINT('Ctrl Pts',(9.26528795718768,-31.1740022260542,
53.8171749782271));
#108733=CARTESIAN_POINT('Ctrl Pts',(9.26262878491381,-31.2037456791508,
53.847458036821));
#108734=CARTESIAN_POINT('Ctrl Pts',(9.25542783362706,-31.2819016189352,
53.9333620953678));
#108735=CARTESIAN_POINT('Ctrl Pts',(9.25095376802016,-31.3278298814751,
53.9911113274041));
#108736=CARTESIAN_POINT('Ctrl Pts',(9.24560870097535,-31.377558575413,54.0629434549367));
#108737=CARTESIAN_POINT('Ctrl Pts',(9.244771832375,-31.385195404497,54.0742698648418));
#108738=CARTESIAN_POINT('Ctrl Pts',(9.23940293652337,-31.4331660357246,
54.1473394244863));
#108739=CARTESIAN_POINT('Ctrl Pts',(9.23481861900438,-31.4694967952229,
54.2116020319002));
#108740=CARTESIAN_POINT('Ctrl Pts',(9.22920032731129,-31.5067684117664,
54.2891162361011));
#108741=CARTESIAN_POINT('Ctrl Pts',(9.22839194632402,-31.5119667141518,
54.3002404655774));
#108742=CARTESIAN_POINT('Ctrl Pts',(9.22711470826635,-31.5199143470558,
54.3177502696748));
#108743=CARTESIAN_POINT('Ctrl Pts',(9.22665072584179,-31.5227475939977,
54.3240975828462));
#108744=CARTESIAN_POINT('Ctrl Pts',(9.22577806818685,-31.5279739563276,
54.336005844064));
#108745=CARTESIAN_POINT('Ctrl Pts',(9.2253699678682,-31.5303765876197,54.3415623448388));
#108746=CARTESIAN_POINT('Ctrl Pts',(9.22440365707393,-31.5359688645001,
54.3546914190152));
#108747=CARTESIAN_POINT('Ctrl Pts',(9.22384396179741,-31.5391328278752,
54.362274629258));
#108748=CARTESIAN_POINT('Ctrl Pts',(9.22195875922678,-31.5495439119172,
54.3877561469904));
#108749=CARTESIAN_POINT('Ctrl Pts',(9.22061969485834,-31.5565356277408,
54.4057562531847));
#108750=CARTESIAN_POINT('Ctrl Pts',(9.21728586842703,-31.572996774463,54.4504204727444));
#108751=CARTESIAN_POINT('Ctrl Pts',(9.21527650740867,-31.582102599997,54.4772116187155));
#108752=CARTESIAN_POINT('Ctrl Pts',(9.20606240262917,-31.6203698432869,
54.5999774999973));
#108753=CARTESIAN_POINT('Ctrl Pts',(9.19868506509942,-31.6415097503523,
54.6982341342242));
#108754=CARTESIAN_POINT('Ctrl Pts',(9.1855125076129,-31.6636848490288,54.8795891810071));
#108755=CARTESIAN_POINT('Ctrl Pts',(9.17968480780526,-31.6676052581658,
54.9620207906268));
#108756=CARTESIAN_POINT('Ctrl Pts',(9.17270305762754,-31.6648853608091,
55.0640063135525));
#108757=CARTESIAN_POINT('Ctrl Pts',(9.171372554744,-31.6640172269966,55.0835870682194));
#108758=CARTESIAN_POINT('Ctrl Pts',(9.16925666316464,-31.6620717712169,
55.1149486982338));
#108759=CARTESIAN_POINT('Ctrl Pts',(9.16846450472534,-31.6612141794798,
55.1267408311022));
#108760=CARTESIAN_POINT('Ctrl Pts',(9.16696039087394,-31.6593383100204,
55.1492235560166));
#108761=CARTESIAN_POINT('Ctrl Pts',(9.16624778535209,-31.6583420611814,
55.1599153341477));
#108762=CARTESIAN_POINT('Ctrl Pts',(9.16461500352786,-31.6558112813696,
55.1845002744488));
#108763=CARTESIAN_POINT('Ctrl Pts',(9.16369711686896,-31.654205130409,55.1983853750473));
#108764=CARTESIAN_POINT('Ctrl Pts',(9.16078659953252,-31.6485260489236,
55.2425987930737));
#108765=CARTESIAN_POINT('Ctrl Pts',(9.15881462747923,-31.6437921258762,
55.2728368443439));
#108766=CARTESIAN_POINT('Ctrl Pts',(9.15415647739166,-31.6304991198075,
55.3447248955641));
#108767=CARTESIAN_POINT('Ctrl Pts',(9.15149286832201,-31.6211735082459,
55.3862116899348));
#108768=CARTESIAN_POINT('Ctrl Pts',(9.14428667704628,-31.5913613838325,
55.4985583713471));
#108769=CARTESIAN_POINT('Ctrl Pts',(9.13981172839539,-31.5677422328208,
55.5684858492453));
#108770=CARTESIAN_POINT('Ctrl Pts',(9.13445242539774,-31.5342663757148,
55.6494422527935));
#108771=CARTESIAN_POINT('Ctrl Pts',(9.13360234543159,-31.5288039470944,
55.6621986385028));
#108772=CARTESIAN_POINT('Ctrl Pts',(9.12823490300193,-31.4934056370254,
55.7420908914308));
#108773=CARTESIAN_POINT('Ctrl Pts',(9.12366504441963,-31.4592167996161,
55.8072440055121));
#108774=CARTESIAN_POINT('Ctrl Pts',(9.11806278095909,-31.4144339826314,
55.88038810281));
#108775=CARTESIAN_POINT('Ctrl Pts',(9.1172545888331,-31.4079085981119,55.8907862035323));
#108776=CARTESIAN_POINT('Ctrl Pts',(9.11597771776019,-31.397510899214,55.906955107001));
#108777=CARTESIAN_POINT('Ctrl Pts',(9.1155139144663,-31.39371621713,55.9127756467359));
#108778=CARTESIAN_POINT('Ctrl Pts',(9.11464158231399,-31.386548593571,55.9236209296218));
#108779=CARTESIAN_POINT('Ctrl Pts',(9.11423362809236,-31.3831845406598,
55.9286512508888));
#108780=CARTESIAN_POINT('Ctrl Pts',(9.1132677452322,-31.3751906057792,55.9404649100221));
#108781=CARTESIAN_POINT('Ctrl Pts',(9.11270833320018,-31.3705378886568,
55.9472324624377));
#108782=CARTESIAN_POINT('Ctrl Pts',(9.11082469136427,-31.3547891085982,
55.9697807094916));
#108783=CARTESIAN_POINT('Ctrl Pts',(9.10948692932894,-31.3434694753646,
55.9854023760814));
#108784=CARTESIAN_POINT('Ctrl Pts',(9.1061569667178,-31.3149066189579,56.0234134364546));
#108785=CARTESIAN_POINT('Ctrl Pts',(9.104150203266,-31.2973603905905,56.0455669826529));
#108786=CARTESIAN_POINT('Ctrl Pts',(9.09495877155585,-31.2151836626063,
56.14406706998));
#108787=CARTESIAN_POINT('Ctrl Pts',(9.08760208414111,-31.1443209697658,
56.214944752921));
#108788=CARTESIAN_POINT('Ctrl Pts',(9.07442319040452,-31.0040062123244,
56.3320560612969));
#108789=CARTESIAN_POINT('Ctrl Pts',(9.06857067604743,-30.9366157485235,
56.380274060758));
#108790=CARTESIAN_POINT('Ctrl Pts',(9.0615650718232,-30.8491604071941,56.4334807406714));
#108791=CARTESIAN_POINT('Ctrl Pts',(9.06023393573327,-30.8322307293258,
56.4433753847078));
#108792=CARTESIAN_POINT('Ctrl Pts',(9.05811735329604,-30.804817906601,56.4587542411534));
#108793=CARTESIAN_POINT('Ctrl Pts',(9.05732512688044,-30.7944446206193,
56.4644294302267));
#108794=CARTESIAN_POINT('Ctrl Pts',(9.05582108009009,-30.7745390133528,
56.4750459551692));
#108795=CARTESIAN_POINT('Ctrl Pts',(9.05510860762732,-30.7650176708136,
56.4800064951252));
#108796=CARTESIAN_POINT('Ctrl Pts',(9.05347640982454,-30.7429977266769,
56.4912094207845));
#108797=CARTESIAN_POINT('Ctrl Pts',(9.05255897021153,-30.7304671162053,
56.4973873815154));
#108798=CARTESIAN_POINT('Ctrl Pts',(9.04965105585291,-30.690277175909,56.5165776245903));
#108799=CARTESIAN_POINT('Ctrl Pts',(9.04768119069732,-30.6623358984938,
56.528987121049));
#108800=CARTESIAN_POINT('Ctrl Pts',(9.04302895869763,-30.5948187974355,
56.5567748692359));
#108801=CARTESIAN_POINT('Ctrl Pts',(9.0403690836724,-30.5549653424431,56.5714233174479));
#108802=CARTESIAN_POINT('Ctrl Pts',(9.03316538696934,-30.4444578123017,
56.607311761038));
#108803=CARTESIAN_POINT('Ctrl Pts',(9.02868941849306,-30.3728854674023,
56.6254078383399));
#108804=CARTESIAN_POINT('Ctrl Pts',(9.02334926032758,-30.2870221723148,
56.6411452884556));
#108805=CARTESIAN_POINT('Ctrl Pts',(9.0225192580234,-30.2736656094489,56.6434252991884));
#108806=CARTESIAN_POINT('Ctrl Pts',(9.01714806449828,-30.187281603874,56.657089047366));
#108807=CARTESIAN_POINT('Ctrl Pts',(9.01255454864607,-30.113601784719,56.6637639169931));
#108808=CARTESIAN_POINT('Ctrl Pts',(9.00692604406243,-30.0274594297945,
56.6658189278203));
#108809=CARTESIAN_POINT('Ctrl Pts',(9.00611780898928,-30.0151836717667,
56.6659760367197));
#108810=CARTESIAN_POINT('Ctrl Pts',(9.00484090339151,-29.9959595232366,
56.6660095895564));
#108811=CARTESIAN_POINT('Ctrl Pts',(9.00437710977084,-29.9890114499722,
56.6659782487605));
#108812=CARTESIAN_POINT('Ctrl Pts',(9.0035047711123,-29.9760122462962,56.665838291924));
#108813=CARTESIAN_POINT('Ctrl Pts',(9.00309680049941,-29.9699612497489,
56.6657401646032));
#108814=CARTESIAN_POINT('Ctrl Pts',(9.00213088035454,-29.9556998549556,
56.6654311609913));
#108815=CARTESIAN_POINT('Ctrl Pts',(9.00157144727216,-29.9474903332707,
56.6651925362206));
#108816=CARTESIAN_POINT('Ctrl Pts',(8.99968785824294,-29.9200056619961,
56.6641901997295));
#108817=CARTESIAN_POINT('Ctrl Pts',(8.99835017321592,-29.9007428652824,
56.6631524454962));
#108818=CARTESIAN_POINT('Ctrl Pts',(8.99502049859785,-29.8533204619571,
56.6597708982724));
#108819=CARTESIAN_POINT('Ctrl Pts',(8.99301395119953,-29.8251946587656,
56.6570447290768));
#108820=CARTESIAN_POINT('Ctrl Pts',(8.98382472161351,-29.6979001206998,
56.6414295980765));
#108821=CARTESIAN_POINT('Ctrl Pts',(8.97647010130321,-29.5999452568105,
56.6203432050362));
#108822=CARTESIAN_POINT('Ctrl Pts',(8.9632863275333,-29.4253875891599,56.5659622782712));
#108823=CARTESIAN_POINT('Ctrl Pts',(8.95742726686729,-29.348241621807,56.5354582465984));
#108824=CARTESIAN_POINT('Ctrl Pts',(8.95041778574361,-29.2560579783346,
56.4908016167568));
#108825=CARTESIAN_POINT('Ctrl Pts',(8.94908884592761,-29.2385921309491,
56.4819572550457));
#108826=CARTESIAN_POINT('Ctrl Pts',(8.94697482534883,-29.2108380198982,
56.4672828744456));
#108827=CARTESIAN_POINT('Ctrl Pts',(8.94618299607484,-29.2004493333971,
56.4616478401007));
#108828=CARTESIAN_POINT('Ctrl Pts',(8.94467913016412,-29.1807365661083,
56.4506821675457));
#108829=CARTESIAN_POINT('Ctrl Pts',(8.943966447355,-29.1714023942565,56.4453710050757));
#108830=CARTESIAN_POINT('Ctrl Pts',(8.94233295505179,-29.1500310266431,
56.4329355776126));
#108831=CARTESIAN_POINT('Ctrl Pts',(8.94141444204003,-29.1380307809724,
56.4257491751591));
#108832=CARTESIAN_POINT('Ctrl Pts',(8.93849967941638,-29.1000225099225,
56.4023324395238));
#108833=CARTESIAN_POINT('Ctrl Pts',(8.93652417520848,-29.074370457933,56.3855345155379));
#108834=CARTESIAN_POINT('Ctrl Pts',(8.93185580310137,-29.014203377522,56.3437175673087));
#108835=CARTESIAN_POINT('Ctrl Pts',(8.92918564404222,-28.9801558974309,
56.3180630752109));
#108836=CARTESIAN_POINT('Ctrl Pts',(8.92197730625953,-28.8900402613201,
56.2445768479305));
#108837=CARTESIAN_POINT('Ctrl Pts',(8.91750625586159,-28.8361018933773,
56.1942879506145));
#108838=CARTESIAN_POINT('Ctrl Pts',(8.91212697057785,-28.7759045854073,
56.1301990163297));
#108839=CARTESIAN_POINT('Ctrl Pts',(8.91125318109112,-28.7662744476001,
56.1196788179742));
#108840=CARTESIAN_POINT('Ctrl Pts',(8.90589475245924,-28.7082152470863,
56.0545949992605));
#108841=CARTESIAN_POINT('Ctrl Pts',(8.90135742994437,-28.6632842109067,
55.997028924508));
#108842=CARTESIAN_POINT('Ctrl Pts',(8.8957912991061,-28.6153741340944,55.9265623920747));
#108843=CARTESIAN_POINT('Ctrl Pts',(8.89498323257773,-28.6085855900273,
55.9163364954661));
#108844=CARTESIAN_POINT('Ctrl Pts',(8.89370649200509,-28.5981321318931,
55.9002059538589));
#108845=CARTESIAN_POINT('Ctrl Pts',(8.8932426909668,-28.5943899667841,55.894351557915));
#108846=CARTESIAN_POINT('Ctrl Pts',(8.89237030599036,-28.5874567813836,
55.8833540000798));
#108847=CARTESIAN_POINT('Ctrl Pts',(8.89196229610667,-28.5842570262775,
55.8782166370528));
#108848=CARTESIAN_POINT('Ctrl Pts',(8.89099619480252,-28.5767802659301,
55.8660652845525));
#108849=CARTESIAN_POINT('Ctrl Pts',(8.89043661869484,-28.5725270698195,
55.8590369695671));
#108850=CARTESIAN_POINT('Ctrl Pts',(8.8885520288937,-28.5584549325702,55.8353899754078));
#108851=CARTESIAN_POINT('Ctrl Pts',(8.88721346726057,-28.5488732706043,
55.8186328409601));
#108852=CARTESIAN_POINT('Ctrl Pts',(8.88388111898545,-28.5259767132005,
55.7769241164269));
#108853=CARTESIAN_POINT('Ctrl Pts',(8.88187274655414,-28.5130021496351,
55.7517931531932));
#108854=CARTESIAN_POINT('Ctrl Pts',(8.87592642271712,-28.476821238482,55.6771083647092));
#108855=CARTESIAN_POINT('Ctrl Pts',(8.87194753167041,-28.4554291605364,
55.6267692839885));
#108856=CARTESIAN_POINT('Ctrl Pts',(8.86797186106679,-28.4365624698124,
55.5755163674484));
#108857=CARTESIAN_POINT('Origin',(5.,-30.,55.));
#108858=CARTESIAN_POINT('',(8.16625309736762,-28.4365623102018,55.5755159338529));
#108859=CARTESIAN_POINT('',(8.36103879467172,-28.436562302838,55.5755159138484));
#108860=CARTESIAN_POINT('',(5.,-28.4365623102018,55.5755159338528));
#108861=CARTESIAN_POINT('Ctrl Pts',(8.36103879467171,-28.436562302838,55.5755159138484));
#108862=CARTESIAN_POINT('Ctrl Pts',(8.36205644453806,-28.4414052882876,
55.588672293779));
#108863=CARTESIAN_POINT('Ctrl Pts',(8.36307260053714,-28.4464149009599,
55.6017690642261));
#108864=CARTESIAN_POINT('Ctrl Pts',(8.36843620734845,-28.4737909734731,
55.6707169719365));
#108865=CARTESIAN_POINT('Ctrl Pts',(8.37273626111417,-28.499005882396,55.7253917146297));
#108866=CARTESIAN_POINT('Ctrl Pts',(8.37880434975973,-28.5395168239628,
55.8020273527629));
#108867=CARTESIAN_POINT('Ctrl Pts',(8.38064282139152,-28.5524661183118,
55.825169544951));
#108868=CARTESIAN_POINT('Ctrl Pts',(8.38393361830657,-28.5768762279705,
55.8664493240042));
#108869=CARTESIAN_POINT('Ctrl Pts',(8.38539220672554,-28.5881451872141,
55.8846930335348));
#108870=CARTESIAN_POINT('Ctrl Pts',(8.38766153209908,-28.6063819676379,
55.9129808164793));
#108871=CARTESIAN_POINT('Ctrl Pts',(8.38848087095959,-28.6131131288968,
55.923173879566));
#108872=CARTESIAN_POINT('Ctrl Pts',(8.39000823397003,-28.6259344944288,
55.9421326244342));
#108873=CARTESIAN_POINT('Ctrl Pts',(8.39071721165674,-28.6319979717759,
55.9509155353961));
#108874=CARTESIAN_POINT('Ctrl Pts',(8.39230420627689,-28.6458205638035,
55.9705316032104));
#108875=CARTESIAN_POINT('Ctrl Pts',(8.39318039436532,-28.6536261471042,
55.9813312405345));
#108876=CARTESIAN_POINT('Ctrl Pts',(8.39542503868652,-28.6740650956907,
56.0089071387764));
#108877=CARTESIAN_POINT('Ctrl Pts',(8.3967861342715,-28.6868878282321,56.0255405757992));
#108878=CARTESIAN_POINT('Ctrl Pts',(8.40638936492191,-28.7803165422586,
56.1421084132425));
#108879=CARTESIAN_POINT('Ctrl Pts',(8.41415177060872,-28.8719214473129,
56.2326726449401));
#108880=CARTESIAN_POINT('Ctrl Pts',(8.42714696822361,-29.0391627200592,
56.3635990773941));
#108881=CARTESIAN_POINT('Ctrl Pts',(8.43232025710095,-29.1091116456632,
56.4102925275115));
#108882=CARTESIAN_POINT('Ctrl Pts',(8.43870212862059,-29.1945373812508,
56.4584183817035));
#108883=CARTESIAN_POINT('Ctrl Pts',(8.43962651935254,-29.206889992403,56.4651725802872));
#108884=CARTESIAN_POINT('Ctrl Pts',(8.44104136647557,-29.2257343601534,
56.4751682402998));
#108885=CARTESIAN_POINT('Ctrl Pts',(8.44152495526307,-29.23216449391,56.4785253629525));
#108886=CARTESIAN_POINT('Ctrl Pts',(8.44241411649535,-29.2439627235751,
56.4845874068499));
#108887=CARTESIAN_POINT('Ctrl Pts',(8.44281887228989,-29.2493238017906,
56.4873054069796));
#108888=CARTESIAN_POINT('Ctrl Pts',(8.44375070472134,-29.2616445175238,
56.4934682733055));
#108889=CARTESIAN_POINT('Ctrl Pts',(8.44427893507324,-29.2686135932243,
56.4968935232104));
#108890=CARTESIAN_POINT('Ctrl Pts',(8.44591339711864,-29.2901385345245,
56.5072866764585));
#108891=CARTESIAN_POINT('Ctrl Pts',(8.44702864302743,-29.3047714142887,
56.5140916719036));
#108892=CARTESIAN_POINT('Ctrl Pts',(8.45379899117702,-29.393409462981,56.553756868862));
#108893=CARTESIAN_POINT('Ctrl Pts',(8.45967657610195,-29.4696248630934,
56.5813956586708));
#108894=CARTESIAN_POINT('Ctrl Pts',(8.47093278662194,-29.6184664632564,
56.6233975123883));
#108895=CARTESIAN_POINT('Ctrl Pts',(8.47629706234238,-29.6906484190402,
56.6386855198168));
#108896=CARTESIAN_POINT('Ctrl Pts',(8.48459243043702,-29.8057117566777,
56.6551788834509));
#108897=CARTESIAN_POINT('Ctrl Pts',(8.48759127115807,-29.8480327784988,
56.6595998085246));
#108898=CARTESIAN_POINT('Ctrl Pts',(8.4926686735133,-29.921028765655,56.664408856142));
#108899=CARTESIAN_POINT('Ctrl Pts',(8.49476876468717,-29.9516291189015,
56.6655791088764));
#108900=CARTESIAN_POINT('Ctrl Pts',(8.49778999847616,-29.9962272512632,
56.6660543986621));
#108901=CARTESIAN_POINT('Ctrl Pts',(8.49873161364051,-30.0102100143427,
56.6660273915031));
#108902=CARTESIAN_POINT('Ctrl Pts',(8.50038684624884,-30.0349308025088,
56.6656683953599));
#108903=CARTESIAN_POINT('Ctrl Pts',(8.5011026713807,-30.0456688965927,56.6654085761269));
#108904=CARTESIAN_POINT('Ctrl Pts',(8.50259981806097,-30.0682226359772,
56.6646445607507));
#108905=CARTESIAN_POINT('Ctrl Pts',(8.50338041258762,-30.0800369755225,
56.6641183660979));
#108906=CARTESIAN_POINT('Ctrl Pts',(8.50544462227414,-30.1114161797634,
56.6623858260673));
#108907=CARTESIAN_POINT('Ctrl Pts',(8.5067213576112,-30.1309674272096,56.6609598988043));
#108908=CARTESIAN_POINT('Ctrl Pts',(8.51331367343572,-30.2325582257957,
56.6517455407422));
#108909=CARTESIAN_POINT('Ctrl Pts',(8.51844672269567,-30.3139667150035,
56.6382228295446));
#108910=CARTESIAN_POINT('Ctrl Pts',(8.5296706241596,-30.4915155920471,56.5950019394245));
#108911=CARTESIAN_POINT('Ctrl Pts',(8.53570210564608,-30.5866339665642,
56.562522641987));
#108912=CARTESIAN_POINT('Ctrl Pts',(8.54376387583394,-30.7040915238797,
56.51016944154));
#108913=CARTESIAN_POINT('Ctrl Pts',(8.54555761589486,-30.7296366316034,
56.4979942661551));
#108914=CARTESIAN_POINT('Ctrl Pts',(8.54862647067718,-30.7720732595398,
56.4764253499417));
#108915=CARTESIAN_POINT('Ctrl Pts',(8.54988524072237,-30.7891343436007,
56.4673771981978));
#108916=CARTESIAN_POINT('Ctrl Pts',(8.55170417616894,-30.81322558651,56.4540590364872));
#108917=CARTESIAN_POINT('Ctrl Pts',(8.55225027883618,-30.8203880714563,
56.4500299794666));
#108918=CARTESIAN_POINT('Ctrl Pts',(8.55320451184597,-30.8327748791546,
56.4429409741923));
#108919=CARTESIAN_POINT('Ctrl Pts',(8.55361111171659,-30.8380128057251,
56.4399052713465));
#108920=CARTESIAN_POINT('Ctrl Pts',(8.55448854161612,-30.8492282442665,
56.4333233032224));
#108921=CARTESIAN_POINT('Ctrl Pts',(8.5549598973233,-30.855200057358,56.4297682189466));
#108922=CARTESIAN_POINT('Ctrl Pts',(8.55627017576744,-30.8716590714876,
56.419829986096));
#108923=CARTESIAN_POINT('Ctrl Pts',(8.55711384547436,-30.8820979793374,
56.4133682673177));
#108924=CARTESIAN_POINT('Ctrl Pts',(8.56302668609428,-30.9542258111416,
56.3676106129489));
#108925=CARTESIAN_POINT('Ctrl Pts',(8.56829775310585,-31.0133336436953,
56.3244086390886));
#108926=CARTESIAN_POINT('Ctrl Pts',(8.57463982260552,-31.0802725996905,
56.2683721730138));
#108927=CARTESIAN_POINT('Ctrl Pts',(8.575670883623,-31.0910233073556,56.2591366081106));
#108928=CARTESIAN_POINT('Ctrl Pts',(8.58206616323697,-31.1569380531708,
56.2010334493029));
#108929=CARTESIAN_POINT('Ctrl Pts',(8.5874303076493,-31.2089304011858,56.1486842910115));
#108930=CARTESIAN_POINT('Ctrl Pts',(8.59572617725535,-31.2851989808541,
56.0609568018601));
#108931=CARTESIAN_POINT('Ctrl Pts',(8.59872561969606,-31.3118721025196,
56.0277927056786));
#108932=CARTESIAN_POINT('Ctrl Pts',(8.60380392478917,-31.3555105251157,
55.9690638693902));
#108933=CARTESIAN_POINT('Ctrl Pts',(8.60590432699071,-31.3730927610895,
55.9439862551947));
#108934=CARTESIAN_POINT('Ctrl Pts',(8.60892592555243,-31.3976832438337,
55.9067706805712));
#108935=CARTESIAN_POINT('Ctrl Pts',(8.60986760105582,-31.4052447101054,
55.8950077332954));
#108936=CARTESIAN_POINT('Ctrl Pts',(8.61152290904499,-31.4183512174646,
55.8740430154364));
#108937=CARTESIAN_POINT('Ctrl Pts',(8.61223874974407,-31.4239569440843,
55.8648803383123));
#108938=CARTESIAN_POINT('Ctrl Pts',(8.6137358992321,-31.4355472781651,55.8455175036047));
#108939=CARTESIAN_POINT('Ctrl Pts',(8.61451648127609,-31.4415127028641,
55.8353065164166));
#108940=CARTESIAN_POINT('Ctrl Pts',(8.61658058904433,-31.4570751102941,
55.8080051162473));
#108941=CARTESIAN_POINT('Ctrl Pts',(8.61785723642462,-31.4664802657605,
55.7908070735944));
#108942=CARTESIAN_POINT('Ctrl Pts',(8.62444637975549,-31.5138148183353,
55.7005022801057));
#108943=CARTESIAN_POINT('Ctrl Pts',(8.62957658200243,-31.5465906782297,
55.6248187713869));
#108944=CARTESIAN_POINT('Ctrl Pts',(8.64080018953408,-31.6065866081312,
55.45222361441));
#108945=CARTESIAN_POINT('Ctrl Pts',(8.64683397242618,-31.6309023755291,
55.3546573288335));
#108946=CARTESIAN_POINT('Ctrl Pts',(8.65489850440016,-31.6506312553793,
55.2275376077274));
#108947=CARTESIAN_POINT('Ctrl Pts',(8.65669255702701,-31.654257954759,55.1994676481461));
#108948=CARTESIAN_POINT('Ctrl Pts',(8.65976189679851,-31.6591539726957,
55.1521089341842));
#108949=CARTESIAN_POINT('Ctrl Pts',(8.66102083330871,-31.6608057681174,
55.1328651780026));
#108950=CARTESIAN_POINT('Ctrl Pts',(8.66283997513964,-31.6626829756213,
55.1053986143683));
#108951=CARTESIAN_POINT('Ctrl Pts',(8.66338611408049,-31.6631826740899,
55.0971953236136));
#108952=CARTESIAN_POINT('Ctrl Pts',(8.66434040252225,-31.6639450484021,
55.0829429548707));
#108953=CARTESIAN_POINT('Ctrl Pts',(8.66474702134359,-31.6642354771929,
55.0768955978695));
#108954=CARTESIAN_POINT('Ctrl Pts',(8.66562449518401,-31.6647885075575,
55.0639025257418));
#108955=CARTESIAN_POINT('Ctrl Pts',(8.66609587591762,-31.6650406074545,
55.0569568153376));
#108956=CARTESIAN_POINT('Ctrl Pts',(8.66740620304431,-31.6656177770549,
55.0377379924225));
#108957=CARTESIAN_POINT('Ctrl Pts',(8.66824989617126,-31.6658506406607,
55.0254628398163));
#108958=CARTESIAN_POINT('Ctrl Pts',(8.67416384317432,-31.6665268657327,
54.9400315946026));
#108959=CARTESIAN_POINT('Ctrl Pts',(8.67943605895062,-31.6622866253168,
54.8669255549198));
#108960=CARTESIAN_POINT('Ctrl Pts',(8.68577817864848,-31.6515101591123,
54.7802941976796));
#108961=CARTESIAN_POINT('Ctrl Pts',(8.68680816770537,-31.6495834545274,
54.7662675291058));
#108962=CARTESIAN_POINT('Ctrl Pts',(8.69320209769039,-31.6365202242126,
54.6793941441958));
#108963=CARTESIAN_POINT('Ctrl Pts',(8.69856595038103,-31.6207385068172,
54.607323846346));
#108964=CARTESIAN_POINT('Ctrl Pts',(8.70686087509572,-31.5884031908434,
54.4956783554412));
#108965=CARTESIAN_POINT('Ctrl Pts',(8.70985967282089,-31.5750100999582,
54.455290255304));
#108966=CARTESIAN_POINT('Ctrl Pts',(8.7149370230895,-31.5493429339376,54.3867873445081));
#108967=CARTESIAN_POINT('Ctrl Pts',(8.71703710263003,-31.5378123294387,
54.3584185624472));
#108968=CARTESIAN_POINT('Ctrl Pts',(8.72005835386869,-31.5198858063695,
54.3175788398036));
#108969=CARTESIAN_POINT('Ctrl Pts',(8.72099999632613,-31.5141047841358,
54.3048466157444));
#108970=CARTESIAN_POINT('Ctrl Pts',(8.72265529221371,-31.5036004776881,
54.2824646494459));
#108971=CARTESIAN_POINT('Ctrl Pts',(8.72337115320179,-31.4989429357188,
54.2727851345396));
#108972=CARTESIAN_POINT('Ctrl Pts',(8.72486839116716,-31.4889613980052,
54.2525444382857));
#108973=CARTESIAN_POINT('Ctrl Pts',(8.72564904091723,-31.483617885189,54.241993506377));
#108974=CARTESIAN_POINT('Ctrl Pts',(8.72771343806372,-31.469119782213,54.2141072944889));
#108975=CARTESIAN_POINT('Ctrl Pts',(8.72899030426879,-31.459770638328,54.196874844649));
#108976=CARTESIAN_POINT('Ctrl Pts',(8.73558559721569,-31.4095283935687,
54.1080450425794));
#108977=CARTESIAN_POINT('Ctrl Pts',(8.74072128450398,-31.3636637003218,
54.0393867941631));
#108978=CARTESIAN_POINT('Ctrl Pts',(8.75194544474392,-31.2511675681152,
53.8953774628601));
#108979=CARTESIAN_POINT('Ctrl Pts',(8.75797478313652,-31.1824329905659,
53.8220946088521));
#108980=CARTESIAN_POINT('Ctrl Pts',(8.76603397739983,-31.0863981786469,
53.7366333243088));
#108981=CARTESIAN_POINT('Ctrl Pts',(8.76782744259251,-31.0647896451103,
53.7183685432193));
#108982=CARTESIAN_POINT('Ctrl Pts',(8.77089587993537,-31.0276682897423,
53.6885783532414));
#108983=CARTESIAN_POINT('Ctrl Pts',(8.77215451400889,-31.0124005085154,
53.6767562651925));
#108984=CARTESIAN_POINT('Ctrl Pts',(8.77397329505741,-30.9903474299995,
53.6602852914252));
#108985=CARTESIAN_POINT('Ctrl Pts',(8.77451938328889,-30.9837272029174,
53.655416675801));
#108986=CARTESIAN_POINT('Ctrl Pts',(8.7754735945591,-30.9721677266366,53.6470467249977));
#108987=CARTESIAN_POINT('Ctrl Pts',(8.77588018723681,-30.9672449712374,
53.6435230126054));
#108988=CARTESIAN_POINT('Ctrl Pts',(8.77675758223686,-30.956629953191,53.6360119394475));
#108989=CARTESIAN_POINT('Ctrl Pts',(8.77722891007052,-30.9509320019738,
53.6320333995711));
#108990=CARTESIAN_POINT('Ctrl Pts',(8.77853914920168,-30.9350997440919,
53.6211253897916));
#108991=CARTESIAN_POINT('Ctrl Pts',(8.77938280795775,-30.9249137140377,
53.6142722772674));
#108992=CARTESIAN_POINT('Ctrl Pts',(8.78530369925469,-30.8534232347532,
53.5673131882141));
#108993=CARTESIAN_POINT('Ctrl Pts',(8.79058348920429,-30.7896135565884,
53.5311804838857));
#108994=CARTESIAN_POINT('Ctrl Pts',(8.79692812260266,-30.7109515274574,
53.4932477243841));
#108995=CARTESIAN_POINT('Ctrl Pts',(8.79795311102322,-30.6981841198993,
53.4872893781569));
#108996=CARTESIAN_POINT('Ctrl Pts',(8.80434319745441,-30.6181612345226,
53.4511728970002));
#108997=CARTESIAN_POINT('Ctrl Pts',(8.80970816508356,-30.5490373573055,
53.4253419421403));
#108998=CARTESIAN_POINT('Ctrl Pts',(8.81800317227188,-30.4376978687496,
53.391962534131));
#108999=CARTESIAN_POINT('Ctrl Pts',(8.82100103842605,-30.3965141228512,
53.3813150494601));
#109000=CARTESIAN_POINT('Ctrl Pts',(8.82607696360062,-30.3250599639222,
53.3657329272283));
#109001=CARTESIAN_POINT('Ctrl Pts',(8.82817653807854,-30.2949792333003,
53.3600364909898));
#109002=CARTESIAN_POINT('Ctrl Pts',(8.83119712952773,-30.2509545656604,
53.3529501391233));
#109003=CARTESIAN_POINT('Ctrl Pts',(8.83213860989103,-30.2371245329765,
53.3509022421972));
#109004=CARTESIAN_POINT('Ctrl Pts',(8.83379364001393,-30.2126270881354,
53.3475893173124));
#109005=CARTESIAN_POINT('Ctrl Pts',(8.83450939671646,-30.2019703127115,
53.3462529380408));
#109006=CARTESIAN_POINT('Ctrl Pts',(8.8360064320162,-30.1795545076767,53.3436618685142));
#109007=CARTESIAN_POINT('Ctrl Pts',(8.83678698335938,-30.1677935041096,
53.3424291329911));
#109008=CARTESIAN_POINT('Ctrl Pts',(8.83885114807321,-30.1365052080355,
53.3394860647382));
#109009=CARTESIAN_POINT('Ctrl Pts',(8.84012788069282,-30.1169587959746,
53.3379949176761));
#109010=CARTESIAN_POINT('Ctrl Pts',(8.84672214900402,-30.0150948249356,
53.3320300202904));
#109011=CARTESIAN_POINT('Ctrl Pts',(8.85185698973024,-29.9325502691058,
53.3333252505191));
#109012=CARTESIAN_POINT('Ctrl Pts',(8.86308110306673,-29.7505476214336,
53.3497310871379));
#109013=CARTESIAN_POINT('Ctrl Pts',(8.86911115851816,-29.6516868776118,
53.3677348265827));
#109014=CARTESIAN_POINT('Ctrl Pts',(8.87717122241691,-29.5277875874255,
53.4020726358655));
#109015=CARTESIAN_POINT('Ctrl Pts',(8.8789647494459,-29.5007219164786,53.4103215298553));
#109016=CARTESIAN_POINT('Ctrl Pts',(8.88203326287157,-29.4555596232797,
53.425352886429));
#109017=CARTESIAN_POINT('Ctrl Pts',(8.8832919070243,-29.4373466267782,53.431768524837));
#109018=CARTESIAN_POINT('Ctrl Pts',(8.88511066943044,-29.4115483061215,
53.4413633750677));
#109019=CARTESIAN_POINT('Ctrl Pts',(8.885656726495,-29.4038678960609,53.4442847200538));
#109020=CARTESIAN_POINT('Ctrl Pts',(8.88661088852498,-29.390567287998,53.4494567341726));
#109021=CARTESIAN_POINT('Ctrl Pts',(8.88701746323427,-29.3849372369696,
53.4516814133233));
#109022=CARTESIAN_POINT('Ctrl Pts',(8.88789485391384,-29.3728698153983,
53.4565259863154));
#109023=CARTESIAN_POINT('Ctrl Pts',(8.8883661956736,-29.3664367724308,53.4591554485851));
#109024=CARTESIAN_POINT('Ctrl Pts',(8.88967642476368,-29.348685923088,53.4665409408362));
#109025=CARTESIAN_POINT('Ctrl Pts',(8.89052005883307,-29.3374042122592,
53.4713818289472));
#109026=CARTESIAN_POINT('Ctrl Pts',(8.89642016612353,-29.2594531926701,
53.5058549975597));
#109027=CARTESIAN_POINT('Ctrl Pts',(8.90167754063202,-29.1947464344649,
53.539711261887));
#109028=CARTESIAN_POINT('Ctrl Pts',(8.90801553430914,-29.1202638437203,
53.5851414010311));
#109029=CARTESIAN_POINT('Ctrl Pts',(8.90905604928723,-29.1081499619329,
53.5927459130084));
#109030=CARTESIAN_POINT('Ctrl Pts',(8.91545981092512,-29.0342408953424,
53.6404801292691));
#109031=CARTESIAN_POINT('Ctrl Pts',(8.92082310075635,-28.9750624191942,
53.6845194073648));
#109032=CARTESIAN_POINT('Ctrl Pts',(8.92912210705646,-28.8865821753877,
53.7599714079682));
#109033=CARTESIAN_POINT('Ctrl Pts',(8.93212534648026,-28.8552427302041,
53.788842925313));
#109034=CARTESIAN_POINT('Ctrl Pts',(8.93720933003145,-28.8033146684374,
53.8405003335306));
#109035=CARTESIAN_POINT('Ctrl Pts',(8.93931167812699,-28.7821865816071,
53.8627111396972));
#109036=CARTESIAN_POINT('Ctrl Pts',(8.94233553529857,-28.7523245677706,
53.8958905507051));
#109037=CARTESIAN_POINT('Ctrl Pts',(8.94327756581707,-28.7430981623012,
53.9064052618435));
#109038=CARTESIAN_POINT('Ctrl Pts',(8.94493329592076,-28.7270223427386,
53.925198030514));
#109039=CARTESIAN_POINT('Ctrl Pts',(8.94564920707794,-28.7201186316598,
53.9334283513217));
#109040=CARTESIAN_POINT('Ctrl Pts',(8.94714630731439,-28.7057844444699,
53.9508565934256));
#109041=CARTESIAN_POINT('Ctrl Pts',(8.94792677151531,-28.6983712865154,
53.960068032947));
#109042=CARTESIAN_POINT('Ctrl Pts',(8.94999010985199,-28.6789379725493,
53.9847488652794));
#109043=CARTESIAN_POINT('Ctrl Pts',(8.95126611577876,-28.6670913012273,
54.0003529622062));
#109044=CARTESIAN_POINT('Ctrl Pts',(8.95783367769749,-28.607079341856,54.0823632362805));
#109045=CARTESIAN_POINT('Ctrl Pts',(8.96294453783008,-28.563588779137,54.1520551625051));
#109046=CARTESIAN_POINT('Ctrl Pts',(8.97416634056554,-28.4785763442164,
54.313740794546));
#109047=CARTESIAN_POINT('Ctrl Pts',(8.98021592572293,-28.4399154439783,
54.406859661282));
#109048=CARTESIAN_POINT('Ctrl Pts',(8.98829942708434,-28.4014388681968,
54.5299349225709));
#109049=CARTESIAN_POINT('Ctrl Pts',(8.99009560655676,-28.3936759344107,
54.5571888841898));
#109050=CARTESIAN_POINT('Ctrl Pts',(8.99316823603421,-28.3817922938904,
54.6033470874716));
#109051=CARTESIAN_POINT('Ctrl Pts',(8.99442829321239,-28.3772989097884,
54.6221497562056));
#109052=CARTESIAN_POINT('Ctrl Pts',(8.99624880765714,-28.3713623134828,
54.6490542938006));
#109053=CARTESIAN_POINT('Ctrl Pts',(8.9967951727833,-28.3696502004651,54.6570960385376));
#109054=CARTESIAN_POINT('Ctrl Pts',(8.99774979133304,-28.3667804987433,
54.6710824759717));
#109055=CARTESIAN_POINT('Ctrl Pts',(8.99815651255716,-28.365595686052,54.6770213411244));
#109056=CARTESIAN_POINT('Ctrl Pts',(8.99903420273079,-28.363120286176,54.6897917886652));
#109057=CARTESIAN_POINT('Ctrl Pts',(8.99950569737639,-28.361840089689,54.6966249256274));
#109058=CARTESIAN_POINT('Ctrl Pts',(9.00081615719047,-28.3584173748759,
54.7155474909531));
#109059=CARTESIAN_POINT('Ctrl Pts',(9.00165986625656,-28.3563657264857,
54.7276526155108));
#109060=CARTESIAN_POINT('Ctrl Pts',(9.0075490219938,-28.3430770800997,54.8116855909185));
#109061=CARTESIAN_POINT('Ctrl Pts',(9.01279435896811,-28.3364327181828,
54.8842527204255));
#109062=CARTESIAN_POINT('Ctrl Pts',(9.01908759015743,-28.3341972495725,
54.9708607673746));
#109063=CARTESIAN_POINT('Ctrl Pts',(9.02009525019884,-28.334012546769,54.9847127412555));
#109064=CARTESIAN_POINT('Ctrl Pts',(9.0304494357485,-28.3338900269998,55.1269885971));
#109065=CARTESIAN_POINT('Ctrl Pts',(9.03975369241362,-28.348629138094,55.2550190002214));
#109066=CARTESIAN_POINT('Ctrl Pts',(9.05003535051255,-28.3827275479487,
55.4005324143705));
#109067=CARTESIAN_POINT('Ctrl Pts',(9.05146702747879,-28.3879012721811,
55.4208730929955));
#109068=CARTESIAN_POINT('Ctrl Pts',(9.05378747600319,-28.3969855076301,
55.4539581682557));
#109069=CARTESIAN_POINT('Ctrl Pts',(9.05468348272912,-28.4006669186226,
55.4667624599023));
#109070=CARTESIAN_POINT('Ctrl Pts',(9.05628845107866,-28.4075741374467,
55.4897446524266));
#109071=CARTESIAN_POINT('Ctrl Pts',(9.05699915607152,-28.4107449022115,
55.4999381917423));
#109072=CARTESIAN_POINT('Ctrl Pts',(9.05851675083272,-28.4177557499196,
55.5217360615256));
#109073=CARTESIAN_POINT('Ctrl Pts',(9.0593226053885,-28.4216260198357,55.5333300825033));
#109074=CARTESIAN_POINT('Ctrl Pts',(9.06083567546823,-28.4291700832666,
55.5551278718492));
#109075=CARTESIAN_POINT('Ctrl Pts',(9.06154370570593,-28.4328164874729,
55.5653400897199));
#109076=CARTESIAN_POINT('Ctrl Pts',(9.06224859760915,-28.4365623100358,
55.5755159334018));
#109077=CARTESIAN_POINT('',(8.82705499792788,-28.3340000601472,54.9995523275645));
#109078=CARTESIAN_POINT('Ctrl Pts',(8.86797186106679,-28.4365624698124,
55.5755163674484));
#109079=CARTESIAN_POINT('Ctrl Pts',(8.86184838023776,-28.4075032668568,
55.4965746534193));
#109080=CARTESIAN_POINT('Ctrl Pts',(8.85573819692927,-28.3844353272406,
55.4154645023934));
#109081=CARTESIAN_POINT('Ctrl Pts',(8.84631922382268,-28.3578004428699,
55.284849712552));
#109082=CARTESIAN_POINT('Ctrl Pts',(8.84291224277331,-28.3501300158674,
55.2364077463103));
#109083=CARTESIAN_POINT('Ctrl Pts',(8.83841124708172,-28.3426889489288,
55.1707800401415));
#109084=CARTESIAN_POINT('Ctrl Pts',(8.83725936146111,-28.3410305162976,
55.1538376794101));
#109085=CARTESIAN_POINT('Ctrl Pts',(8.83535766250728,-28.3387052404224,
55.1256302681827));
#109086=CARTESIAN_POINT('Ctrl Pts',(8.83460334789464,-28.3378926845071,
55.1143788663979));
#109087=CARTESIAN_POINT('Ctrl Pts',(8.83318000510604,-28.3365689127441,
55.0930330699288));
#109088=CARTESIAN_POINT('Ctrl Pts',(8.8325103041271,-28.3360351588518,55.0829406367506));
#109089=CARTESIAN_POINT('Ctrl Pts',(8.83105715513884,-28.3350722484711,
55.0609391077272));
#109090=CARTESIAN_POINT('Ctrl Pts',(8.8302748545869,-28.3346789595391,55.0490289411635));
#109091=CARTESIAN_POINT('Ctrl Pts',(8.82867837466067,-28.3341345156952,
55.024596487052));
#109092=CARTESIAN_POINT('Ctrl Pts',(8.82786465131135,-28.3339966952485,
55.0120747003937));
#109093=CARTESIAN_POINT('Ctrl Pts',(8.82705499792788,-28.3340000601472,
54.9995523275645));
#109094=CARTESIAN_POINT('Ctrl Pts',(8.82705508282654,-28.3340000597949,
54.9995536406356));
#109095=CARTESIAN_POINT('Ctrl Pts',(8.82553617924465,-28.3340063538018,
54.9760617728887));
#109096=CARTESIAN_POINT('Ctrl Pts',(8.82403188229458,-28.3345095256223,
54.9525716062054));
#109097=CARTESIAN_POINT('Ctrl Pts',(8.81396006572755,-28.3412605954388,
54.7940821744825));
#109098=CARTESIAN_POINT('Ctrl Pts',(8.80588749310837,-28.3634168684129,
54.6602725688371));
#109099=CARTESIAN_POINT('Ctrl Pts',(8.79388659909176,-28.4182312943844,
54.4736034974832));
#109100=CARTESIAN_POINT('Ctrl Pts',(8.79017169561399,-28.4380053519377,
54.4175424887028));
#109101=CARTESIAN_POINT('Ctrl Pts',(8.78533509524416,-28.46648813663,54.3487519108468));
#109102=CARTESIAN_POINT('Ctrl Pts',(8.7843479530302,-28.4724362915505,54.3349197142162));
#109103=CARTESIAN_POINT('Ctrl Pts',(8.78285665722318,-28.4816052876738,
54.3143696632688));
#109104=CARTESIAN_POINT('Ctrl Pts',(8.78236053876815,-28.4846852308977,
54.3075892791853));
#109105=CARTESIAN_POINT('Ctrl Pts',(8.7814596510359,-28.4903287297755,54.2953833218251));
#109106=CARTESIAN_POINT('Ctrl Pts',(8.78105584701978,-28.4928762783555,
54.2899506412407));
#109107=CARTESIAN_POINT('Ctrl Pts',(8.78014063116624,-28.4986904656686,
54.2777240781553));
#109108=CARTESIAN_POINT('Ctrl Pts',(8.77962823377947,-28.5019738749475,
54.2709385840204));
#109109=CARTESIAN_POINT('Ctrl Pts',(8.77805246895655,-28.512160580754,54.2502460916597));
#109110=CARTESIAN_POINT('Ctrl Pts',(8.77698074146401,-28.5192121106592,
54.2364135646621));
#109111=CARTESIAN_POINT('Ctrl Pts',(8.76869615160337,-28.5747294637855,
54.1311705239456));
#109112=CARTESIAN_POINT('Ctrl Pts',(8.76111630225965,-28.6314189173206,
54.0443624123599));
#109113=CARTESIAN_POINT('Ctrl Pts',(8.74555672798814,-28.7645693483943,
53.8768405178082));
#109114=CARTESIAN_POINT('Ctrl Pts',(8.73763045269787,-28.8418059592626,
53.7973484058349));
#109115=CARTESIAN_POINT('Ctrl Pts',(8.72900071158429,-28.9380252977885,
53.7162561166272));
#109116=CARTESIAN_POINT('Ctrl Pts',(8.72796110462585,-28.9498226287945,
53.7065874045834));
#109117=CARTESIAN_POINT('Ctrl Pts',(8.72598367510743,-28.9726543404673,
53.6883936362838));
#109118=CARTESIAN_POINT('Ctrl Pts',(8.72504486619891,-28.9836661623395,
53.6798424683227));
#109119=CARTESIAN_POINT('Ctrl Pts',(8.72339298715939,-29.0033432477191,
53.6649544916141));
#109120=CARTESIAN_POINT('Ctrl Pts',(8.72267773617592,-29.011964718241,53.6585614130366));
#109121=CARTESIAN_POINT('Ctrl Pts',(8.72118025132079,-29.0302255532999,
53.6452920235054));
#109122=CARTESIAN_POINT('Ctrl Pts',(8.72039875880233,-29.0398776852558,
53.6384342351684));
#109123=CARTESIAN_POINT('Ctrl Pts',(8.7183285774858,-29.0657655664845,53.6204532232389));
#109124=CARTESIAN_POINT('Ctrl Pts',(8.71704684500549,-29.0821269919892,
53.6095135813616));
#109125=CARTESIAN_POINT('Ctrl Pts',(8.71044167823371,-29.1680949753429,
53.5542121251439));
#109126=CARTESIAN_POINT('Ctrl Pts',(8.70530125383583,-29.2407377204961,
53.5147754977768));
#109127=CARTESIAN_POINT('Ctrl Pts',(8.69408430280294,-29.4072735079882,
53.439792230691));
#109128=CARTESIAN_POINT('Ctrl Pts',(8.6880659644171,-29.5020453078056,53.407011688188));
#109129=CARTESIAN_POINT('Ctrl Pts',(8.68002007710013,-29.626613460373,53.3761350480645));
#109130=CARTESIAN_POINT('Ctrl Pts',(8.67822819671343,-29.6542149849184,
53.3700345300044));
#109131=CARTESIAN_POINT('Ctrl Pts',(8.67516227436431,-29.7008969899472,
53.3609558601034));
#109132=CARTESIAN_POINT('Ctrl Pts',(8.67390453944673,-29.719898870554,53.3576018805989));
#109133=CARTESIAN_POINT('Ctrl Pts',(8.67208694303045,-29.7470660136405,
53.3532918095146));
#109134=CARTESIAN_POINT('Ctrl Pts',(8.67154111947347,-29.7551875249804,
53.3520648340582));
#109135=CARTESIAN_POINT('Ctrl Pts',(8.67058731054735,-29.7693083164924,
53.3500381896775));
#109136=CARTESIAN_POINT('Ctrl Pts',(8.67018085349109,-29.7753034193322,
53.3492110753782));
#109137=CARTESIAN_POINT('Ctrl Pts',(8.66930366891522,-29.7881914309504,
53.3475044897134));
#109138=CARTESIAN_POINT('Ctrl Pts',(8.66883241543114,-29.7950852703291,
53.346635481631));
#109139=CARTESIAN_POINT('Ctrl Pts',(8.66752230948051,-29.8141732233366,
53.3443505471619));
#109140=CARTESIAN_POINT('Ctrl Pts',(8.66667871027514,-29.8263775745153,
53.3430262727278));
#109141=CARTESIAN_POINT('Ctrl Pts',(8.66074013012445,-29.9117637561331,
53.3347148112614));
#109142=CARTESIAN_POINT('Ctrl Pts',(8.65544119128776,-29.9853159410088,
53.3324441906106));
#109143=CARTESIAN_POINT('Ctrl Pts',(8.64909097603331,-30.0726650564518,
53.3355273673913));
#109144=CARTESIAN_POINT('Ctrl Pts',(8.64807933770529,-30.0865548732217,
53.3361918363297));
#109145=CARTESIAN_POINT('Ctrl Pts',(8.6417012039095,-30.174027301581,53.341474712998));
#109146=CARTESIAN_POINT('Ctrl Pts',(8.63633497716954,-30.2472483890798,
53.3507998365353));
#109147=CARTESIAN_POINT('Ctrl Pts',(8.62804294649771,-30.3612905792742,
53.3730923844101));
#109148=CARTESIAN_POINT('Ctrl Pts',(8.62504909572653,-30.4026426831145,
53.382830051275));
#109149=CARTESIAN_POINT('Ctrl Pts',(8.61997922178802,-30.4730547026799,
53.4022796663642));
#109150=CARTESIAN_POINT('Ctrl Pts',(8.61788175145896,-30.5023007734022,
53.411231557993));
#109151=CARTESIAN_POINT('Ctrl Pts',(8.61486370094582,-30.5445289221495,
53.4254399045841));
#109152=CARTESIAN_POINT('Ctrl Pts',(8.61392270409118,-30.5577160072512,
53.4300623843458));
#109153=CARTESIAN_POINT('Ctrl Pts',(8.61226834979894,-30.5809306607443,
53.4385292676582));
#109154=CARTESIAN_POINT('Ctrl Pts',(8.61155278937163,-30.5909819853868,
53.4423056837817));
#109155=CARTESIAN_POINT('Ctrl Pts',(8.61005599931498,-30.6120242441422,
53.4504445366153));
#109156=CARTESIAN_POINT('Ctrl Pts',(8.60927549811119,-30.6230066922844,
53.4548273614169));
#109157=CARTESIAN_POINT('Ctrl Pts',(8.60721109163747,-30.652072438047,53.4667870627722));
#109158=CARTESIAN_POINT('Ctrl Pts',(8.60593407181327,-30.6700705716299,
53.4745669935996));
#109159=CARTESIAN_POINT('Ctrl Pts',(8.59932458490185,-30.7632185103023,
53.5167982592224));
#109160=CARTESIAN_POINT('Ctrl Pts',(8.59417593504113,-30.8358690107976,
53.5564919847867));
#109161=CARTESIAN_POINT('Ctrl Pts',(8.58295050239305,-30.9893056217987,
53.655809202575));
#109162=CARTESIAN_POINT('Ctrl Pts',(8.57693170498292,-31.0682536377392,
53.7176559206365));
#109163=CARTESIAN_POINT('Ctrl Pts',(8.56888527237285,-31.1617625285975,
53.8055701051896));
#109164=CARTESIAN_POINT('Ctrl Pts',(8.56709332884275,-31.18185871352,53.8254512578571));
#109165=CARTESIAN_POINT('Ctrl Pts',(8.56402730661505,-31.214805938451,53.8597478978994));
#109166=CARTESIAN_POINT('Ctrl Pts',(8.5627695357879,-31.227930119295,53.8738934913865));
#109167=CARTESIAN_POINT('Ctrl Pts',(8.56095189065356,-31.2462862250038,
53.8943806647541));
#109168=CARTESIAN_POINT('Ctrl Pts',(8.56040605480154,-31.2517220138551,
53.9005385581389));
#109169=CARTESIAN_POINT('Ctrl Pts',(8.55945222787983,-31.2610834968888,
53.911303052612));
#109170=CARTESIAN_POINT('Ctrl Pts',(8.55904576520032,-31.2650299848567,
53.9158912575542));
#109171=CARTESIAN_POINT('Ctrl Pts',(8.55816857569379,-31.2734538244118,
53.925793484299));
#109172=CARTESIAN_POINT('Ctrl Pts',(8.55769732296065,-31.2779228908654,
53.9311139621629));
#109173=CARTESIAN_POINT('Ctrl Pts',(8.55638721937728,-31.2901951930068,
53.9459112632415));
#109174=CARTESIAN_POINT('Ctrl Pts',(8.55554362180173,-31.2979269808047,
53.9554463961042));
#109175=CARTESIAN_POINT('Ctrl Pts',(8.54960520472496,-31.3512188815377,
54.0226732451926));
#109176=CARTESIAN_POINT('Ctrl Pts',(8.54430643992107,-31.3930175213769,
54.0832340313737));
#109177=CARTESIAN_POINT('Ctrl Pts',(8.53795631379941,-31.4378021014612,
54.1582907248116));
#109178=CARTESIAN_POINT('Ctrl Pts',(8.53694459249697,-31.4447778272773,
54.1703215001261));
#109179=CARTESIAN_POINT('Ctrl Pts',(8.53056640387706,-31.4877820559782,
54.2466766125069));
#109180=CARTESIAN_POINT('Ctrl Pts',(8.52520020317049,-31.5196602441179,
54.3132499505791));
#109181=CARTESIAN_POINT('Ctrl Pts',(8.51690814852958,-31.5627843248727,
54.4211524549926));
#109182=CARTESIAN_POINT('Ctrl Pts',(8.51391425079502,-31.5770315741539,
54.4611760569905));
#109183=CARTESIAN_POINT('Ctrl Pts',(8.50884431074162,-31.5988806006418,
54.5308818288539));
#109184=CARTESIAN_POINT('Ctrl Pts',(8.50674682029753,-31.6072219285935,
54.5603081546132));
#109185=CARTESIAN_POINT('Ctrl Pts',(8.50372875040669,-31.6181881227919,
54.6034921939073));
#109186=CARTESIAN_POINT('Ctrl Pts',(8.50278775369559,-31.6214568223152,
54.6170782912113));
#109187=CARTESIAN_POINT('Ctrl Pts',(8.50113340343795,-31.6269342863765,
54.6411739876842));
#109188=CARTESIAN_POINT('Ctrl Pts',(8.50041784685424,-31.629213055609,54.6516666711136));
#109189=CARTESIAN_POINT('Ctrl Pts',(8.4989210686974,-31.6337878561679,54.6737592182554));
#109190=CARTESIAN_POINT('Ctrl Pts',(8.49814057550794,-31.6360621575444,
54.68536301009));
#109191=CARTESIAN_POINT('Ctrl Pts',(8.49607619983112,-31.641778536238,54.7162684374084));
#109192=CARTESIAN_POINT('Ctrl Pts',(8.49479920254292,-31.645003838611,54.7356086513292));
#109193=CARTESIAN_POINT('Ctrl Pts',(8.48819042771245,-31.6600424222173,
54.8367600307408));
#109194=CARTESIAN_POINT('Ctrl Pts',(8.48304241671865,-31.666097380804,54.9193145426247));
#109195=CARTESIAN_POINT('Ctrl Pts',(8.47181692945927,-31.6658794680774,
55.1020898418589));
#109196=CARTESIAN_POINT('Ctrl Pts',(8.46579750244033,-31.6567382489378,
55.2019722042967));
#109197=CARTESIAN_POINT('Ctrl Pts',(8.4577503063853,-31.6335917670788,55.3282270027051));
#109198=CARTESIAN_POINT('Ctrl Pts',(8.45595827716415,-31.6277879651729,
55.3558949102023));
#109199=CARTESIAN_POINT('Ctrl Pts',(8.45289212413416,-31.6168428185066,
55.4021786306713));
#109200=CARTESIAN_POINT('Ctrl Pts',(8.45163431029328,-31.612076412706,55.4208775504655));
#109201=CARTESIAN_POINT('Ctrl Pts',(8.4498166167352,-31.6048197357512,55.4474115397722));
#109202=CARTESIAN_POINT('Ctrl Pts',(8.44927077675313,-31.6025943780206,
55.4553182653044));
#109203=CARTESIAN_POINT('Ctrl Pts',(8.44831694777217,-31.5986279751689,
55.4690215624216));
#109204=CARTESIAN_POINT('Ctrl Pts',(8.44791048724636,-31.5969136645005,
55.4748256267276));
#109205=CARTESIAN_POINT('Ctrl Pts',(8.44703330777454,-31.5931631989013,
55.4872733333099));
#109206=CARTESIAN_POINT('Ctrl Pts',(8.44656206298062,-31.591117127449,55.493913516746));
#109207=CARTESIAN_POINT('Ctrl Pts',(8.44525199896465,-31.5853414970811,
55.5122489896442));
#109208=CARTESIAN_POINT('Ctrl Pts',(8.44440843343443,-31.5815242072024,
55.5239158803544));
#109209=CARTESIAN_POINT('Ctrl Pts',(8.43847834147419,-31.5539863145305,
55.6050363588819));
#109210=CARTESIAN_POINT('Ctrl Pts',(8.43318852934751,-31.5258300482248,
55.6728913269193));
#109211=CARTESIAN_POINT('Ctrl Pts',(8.42684056546539,-31.4870903879816,
55.7512084489353));
#109212=CARTESIAN_POINT('Ctrl Pts',(8.4258221531402,-31.4807259853443,55.7636769660354));
#109213=CARTESIAN_POINT('Ctrl Pts',(8.4194377937421,-31.4398650350181,55.8412961414796));
#109214=CARTESIAN_POINT('Ctrl Pts',(8.41407206250087,-31.4012307904917,
55.9041814545707));
#109215=CARTESIAN_POINT('Ctrl Pts',(8.40577891656175,-31.3339646014261,
55.9989491898386));
#109216=CARTESIAN_POINT('Ctrl Pts',(8.40278354136814,-31.3080554206888,
56.0326434814578));
#109217=CARTESIAN_POINT('Ctrl Pts',(8.39771140638847,-31.261324527223,56.0888306192055));
#109218=CARTESIAN_POINT('Ctrl Pts',(8.39561317319922,-31.2411196382306,
56.1118066096013));
#109219=CARTESIAN_POINT('Ctrl Pts',(8.39259425012894,-31.2107783230305,
56.144450586437));
#109220=CARTESIAN_POINT('Ctrl Pts',(8.39165312661661,-31.2011356725252,
56.154566762543));
#109221=CARTESIAN_POINT('Ctrl Pts',(8.38999863394394,-31.1838612475959,
56.1722388112475));
#109222=CARTESIAN_POINT('Ctrl Pts',(8.38928306044775,-31.1762816832033,
56.1798443521048));
#109223=CARTESIAN_POINT('Ctrl Pts',(8.38778632549781,-31.1602025490578,
56.1956696156224));
#109224=CARTESIAN_POINT('Ctrl Pts',(8.38700589167017,-31.1516879105022,
56.2038732298281));
#109225=CARTESIAN_POINT('Ctrl Pts',(8.38494185700755,-31.1288272498575,
56.2254343028839));
#109226=CARTESIAN_POINT('Ctrl Pts',(8.38366513722902,-31.1143313357955,
56.2386306622115));
#109227=CARTESIAN_POINT('Ctrl Pts',(8.37706589660129,-31.0376183063484,
56.3060293343457));
#109228=CARTESIAN_POINT('Ctrl Pts',(8.37192643767452,-30.9716670751973,
56.3558133911492));
#109229=CARTESIAN_POINT('Ctrl Pts',(8.36070155094149,-30.8180344104257,
56.4547925755347));
#109230=CARTESIAN_POINT('Ctrl Pts',(8.35467494395419,-30.7290572541563,
56.5013576889035));
#109231=CARTESIAN_POINT('Ctrl Pts',(8.34661911461226,-30.6103037973624,
56.5504467713805));
#109232=CARTESIAN_POINT('Ctrl Pts',(8.34482612517006,-30.583896668051,56.5605833578003));
#109233=CARTESIAN_POINT('Ctrl Pts',(8.3417584951817,-30.5390535898384,56.5764992480857));
#109234=CARTESIAN_POINT('Ctrl Pts',(8.34050018504127,-30.5207513650662,
56.5826391217805));
#109235=CARTESIAN_POINT('Ctrl Pts',(8.3386818982657,-30.4945146110847,56.5909364509638));
#109236=CARTESIAN_POINT('Ctrl Pts',(8.33813597382793,-30.4866636385935,
56.5933555747084));
#109237=CARTESIAN_POINT('Ctrl Pts',(8.3371820492612,-30.47299827125,56.5974558730859));
#109238=CARTESIAN_POINT('Ctrl Pts',(8.33677557854923,-30.4671920862621,
56.5991635889597));
#109239=CARTESIAN_POINT('Ctrl Pts',(8.33589843860159,-30.4547006474348,
56.6027637352125));
#109240=CARTESIAN_POINT('Ctrl Pts',(8.33542724411356,-30.4480129241238,
56.6046459687753));
#109241=CARTESIAN_POINT('Ctrl Pts',(8.33411745535199,-30.4294798514906,
56.6097371422419));
#109242=CARTESIAN_POINT('Ctrl Pts',(8.33327411788015,-30.4176107948431,
56.6128570339284));
#109243=CARTESIAN_POINT('Ctrl Pts',(8.32739887247102,-30.3352905007319,
56.6335261323278));
#109244=CARTESIAN_POINT('Ctrl Pts',(8.32216800137943,-30.2637991907535,
56.6465828242112));
#109245=CARTESIAN_POINT('Ctrl Pts',(8.31584324417443,-30.1773078760519,
56.656601230076));
#109246=CARTESIAN_POINT('Ctrl Pts',(8.31478973529396,-30.1629013581077,
56.6580798719303));
#109247=CARTESIAN_POINT('Ctrl Pts',(8.30828496922489,-30.0738836088459,
56.666045019249));
#109248=CARTESIAN_POINT('Ctrl Pts',(8.30283360293201,-29.9989197191716,
56.6676825293435));
#109249=CARTESIAN_POINT('Ctrl Pts',(8.29449525406011,-29.8821389467974,
56.6623564165119));
#109250=CARTESIAN_POINT('Ctrl Pts',(8.2915353389042,-29.8402662970178,56.6588567490511));
#109251=CARTESIAN_POINT('Ctrl Pts',(8.2865159350786,-29.7684557613351,56.650110131308));
#109252=CARTESIAN_POINT('Ctrl Pts',(8.28443557452401,-29.7384480479612,
56.6456205408177));
#109253=CARTESIAN_POINT('Ctrl Pts',(8.2814372037558,-29.6948624013613,56.6378770095487));
#109254=CARTESIAN_POINT('Ctrl Pts',(8.28049915127017,-29.6811776570974,
56.6352682919464));
#109255=CARTESIAN_POINT('Ctrl Pts',(8.27884811610634,-29.6570112764264,
56.6303465581826));
#109256=CARTESIAN_POINT('Ctrl Pts',(8.2781329603651,-29.6465164119705,56.6281033525343));
#109257=CARTESIAN_POINT('Ctrl Pts',(8.27663519685349,-29.6244843353795,
56.6231710637236));
#109258=CARTESIAN_POINT('Ctrl Pts',(8.27585333506021,-29.6129526152548,
56.6204600120473));
#109259=CARTESIAN_POINT('Ctrl Pts',(8.27378104800953,-29.5823162646349,
56.6129118519075));
#109260=CARTESIAN_POINT('Ctrl Pts',(8.27249760463375,-29.5632665222696,
56.6078582859401));
#109261=CARTESIAN_POINT('Ctrl Pts',(8.26560998383705,-29.4607368949674,
56.5787021918441));
#109262=CARTESIAN_POINT('Ctrl Pts',(8.26021101340171,-29.3791454853494,
56.5484339677419));
#109263=CARTESIAN_POINT('Ctrl Pts',(8.24896385204374,-29.2127209986545,
56.4714130038672));
#109264=CARTESIAN_POINT('Ctrl Pts',(8.24315303708851,-29.1288541209504,
56.4233647014439));
#109265=CARTESIAN_POINT('Ctrl Pts',(8.23451324305029,-29.015739650852,56.344800855531));
#109266=CARTESIAN_POINT('Ctrl Pts',(8.23188275192659,-28.9827464906395,
56.3200198681405));
#109267=CARTESIAN_POINT('Ctrl Pts',(8.22847293050118,-28.9423632052686,
56.2872745959769));
#109268=CARTESIAN_POINT('Ctrl Pts',(8.22776317684413,-28.9340823991569,
56.2804261510396));
#109269=CARTESIAN_POINT('Ctrl Pts',(8.22661218532108,-28.9208658939211,
56.2692786983777));
#109270=CARTESIAN_POINT('Ctrl Pts',(8.22617445375682,-28.915888112556,56.2650297407005));
#109271=CARTESIAN_POINT('Ctrl Pts',(8.22532203759895,-28.9062916430472,
56.2567401039398));
#109272=CARTESIAN_POINT('Ctrl Pts',(8.22490760932303,-28.9016700400614,
56.2527030587226));
#109273=CARTESIAN_POINT('Ctrl Pts',(8.22397306517343,-28.8913444267807,
56.2435824056227));
#109274=CARTESIAN_POINT('Ctrl Pts',(8.22345195593882,-28.8856528795086,
56.2384849086761));
#109275=CARTESIAN_POINT('Ctrl Pts',(8.22160690026736,-28.865725949537,56.2203892727729));
#109276=CARTESIAN_POINT('Ctrl Pts',(8.22026914383081,-28.8516819005572,
56.2071839390308));
#109277=CARTESIAN_POINT('Ctrl Pts',(8.21136055728577,-28.7605972343528,
56.1185111434971));
#109278=CARTESIAN_POINT('Ctrl Pts',(8.20343270390961,-28.6908154886555,
56.0359632342641));
#109279=CARTESIAN_POINT('Ctrl Pts',(8.18941145534872,-28.5809488814632,
55.8770076844964));
#109280=CARTESIAN_POINT('Ctrl Pts',(8.18329627340985,-28.5378615511692,
55.8031209869155));
#109281=CARTESIAN_POINT('Ctrl Pts',(8.17529351248492,-28.4875624006019,
55.6992757608946));
#109282=CARTESIAN_POINT('Ctrl Pts',(8.17323888610889,-28.4752280989282,
55.6719560493771));
#109283=CARTESIAN_POINT('Ctrl Pts',(8.17027014972838,-28.4582743093055,
55.6315300108923));
#109284=CARTESIAN_POINT('Ctrl Pts',(8.16933655472817,-28.4530714954049,
55.6186763951053));
#109285=CARTESIAN_POINT('Ctrl Pts',(8.16769052677727,-28.4441305326062,
55.5957694140264));
#109286=CARTESIAN_POINT('Ctrl Pts',(8.16697596606473,-28.4403279098729,
55.5857422426098));
#109287=CARTESIAN_POINT('Ctrl Pts',(8.16626077429774,-28.4366022942655,
55.5756245452141));
#109288=CARTESIAN_POINT('Ctrl Pts',(8.16625693578549,-28.4365823008186,
55.5755702400533));
#109289=CARTESIAN_POINT('Ctrl Pts',(8.16625309736762,-28.4365623102018,
55.5755159338529));
#109290=CARTESIAN_POINT('Origin',(5.,-30.,55.));
#109291=CARTESIAN_POINT('',(7.4682788092303,-28.4365623654365,55.5755160839024));
#109292=CARTESIAN_POINT('',(7.65925610934961,-28.4365623095611,55.5755159321123));
#109293=CARTESIAN_POINT('',(5.,-28.4365623102018,55.5755159338528));
#109294=CARTESIAN_POINT('',(8.32030899669651,-28.3340003265563,55.0010431133336));
#109295=CARTESIAN_POINT('Ctrl Pts',(7.65925610934961,-28.4365623095611,
55.5755159321123));
#109296=CARTESIAN_POINT('Ctrl Pts',(7.6596315560846,-28.4385623445714,55.5809491963241));
#109297=CARTESIAN_POINT('Ctrl Pts',(7.66000835454394,-28.4405908269087,
55.5863723737114));
#109298=CARTESIAN_POINT('Ctrl Pts',(7.66118867024847,-28.4470093428382,
55.6032634517357));
#109299=CARTESIAN_POINT('Ctrl Pts',(7.66199704716634,-28.4514976072287,
55.6146926803279));
#109300=CARTESIAN_POINT('Ctrl Pts',(7.66327424463479,-28.4587235614784,
55.632511856785));
#109301=CARTESIAN_POINT('Ctrl Pts',(7.66373818777893,-28.4613757176395,
55.6389363209823));
#109302=CARTESIAN_POINT('Ctrl Pts',(7.6646108341278,-28.4664131588991,55.6509255380234));
#109303=CARTESIAN_POINT('Ctrl Pts',(7.6650189628302,-28.4687886778772,55.6564941260748));
#109304=CARTESIAN_POINT('Ctrl Pts',(7.66598534126336,-28.4744599805603,
55.6695903043105));
#109305=CARTESIAN_POINT('Ctrl Pts',(7.66654507652535,-28.4777811654128,
55.6771065935943));
#109306=CARTESIAN_POINT('Ctrl Pts',(7.66843017181659,-28.489091667823,55.7021999681124));
#109307=CARTESIAN_POINT('Ctrl Pts',(7.66976908625898,-28.4973305851432,
55.7196619579204));
#109308=CARTESIAN_POINT('Ctrl Pts',(7.67310235261717,-28.5183838684203,
55.7623449412159));
#109309=CARTESIAN_POINT('Ctrl Pts',(7.67511129716783,-28.5315405108667,
55.7873898138015));
#109310=CARTESIAN_POINT('Ctrl Pts',(7.68432086803433,-28.5941909948013,
55.8996142816884));
#109311=CARTESIAN_POINT('Ctrl Pts',(7.69169396224523,-28.6508540825793,
55.9825530883988));
#109312=CARTESIAN_POINT('Ctrl Pts',(7.70486796129938,-28.7670982509054,
56.123526146945));
#109313=CARTESIAN_POINT('Ctrl Pts',(7.71070089544379,-28.8242252665084,
56.1831801157415));
#109314=CARTESIAN_POINT('Ctrl Pts',(7.71768794115089,-28.9001166530769,
56.2514778947734));
#109315=CARTESIAN_POINT('Ctrl Pts',(7.7190188398837,-28.9149190952913,56.2643337317098));
#109316=CARTESIAN_POINT('Ctrl Pts',(7.72113535107662,-28.939009811252,56.284521574664));
#109317=CARTESIAN_POINT('Ctrl Pts',(7.72192773760227,-28.9481548771276,
56.2920207840315));
#109318=CARTESIAN_POINT('Ctrl Pts',(7.72343228537405,-28.9657566586118,
56.3061439717789));
#109319=CARTESIAN_POINT('Ctrl Pts',(7.72414509708789,-28.9741990595568,
56.3127847515955));
#109320=CARTESIAN_POINT('Ctrl Pts',(7.72577836149336,-28.9937771938607,
56.3278806929596));
#109321=CARTESIAN_POINT('Ctrl Pts',(7.72669652299578,-29.0049564194279,
56.3362783253617));
#109322=CARTESIAN_POINT('Ctrl Pts',(7.72960801873068,-29.0409441086675,
56.3626095491915));
#109323=CARTESIAN_POINT('Ctrl Pts',(7.73158067886816,-29.0661424916406,
56.3800012061073));
#109324=CARTESIAN_POINT('Ctrl Pts',(7.73624067789816,-29.1274567344713,
56.4198705942748));
#109325=CARTESIAN_POINT('Ctrl Pts',(7.73890542608523,-29.1639824111575,
56.44167930767));
#109326=CARTESIAN_POINT('Ctrl Pts',(7.74611134338234,-29.2659870836606,
56.4974022123086));
#109327=CARTESIAN_POINT('Ctrl Pts',(7.75058500742547,-29.332944493393,56.5284062490572));
#109328=CARTESIAN_POINT('Ctrl Pts',(7.75594783319387,-29.4147581248127,
56.5598854628989));
#109329=CARTESIAN_POINT('Ctrl Pts',(7.7568026874433,-29.4278435645864,56.5647324746603));
#109330=CARTESIAN_POINT('Ctrl Pts',(7.76216751804569,-29.5101164097297,
56.5940373447245));
#109331=CARTESIAN_POINT('Ctrl Pts',(7.76673002031649,-29.5807875270263,
56.6140629379912));
#109332=CARTESIAN_POINT('Ctrl Pts',(7.77232424267155,-29.6645460512457,
56.6319244453593));
#109333=CARTESIAN_POINT('Ctrl Pts',(7.77313255053717,-29.6765814720595,
56.6343522206432));
#109334=CARTESIAN_POINT('Ctrl Pts',(7.77440966238008,-29.6954699527762,
56.6379455900366));
#109335=CARTESIAN_POINT('Ctrl Pts',(7.77487359000941,-29.702305624994,56.6392017448432));
#109336=CARTESIAN_POINT('Ctrl Pts',(7.77574622456606,-29.7151102335457,
56.6414720457116));
#109337=CARTESIAN_POINT('Ctrl Pts',(7.77615435718938,-29.7210770958674,
56.6424964732844));
#109338=CARTESIAN_POINT('Ctrl Pts',(7.77712076862338,-29.7351561467272,
56.6448347232629));
#109339=CARTESIAN_POINT('Ctrl Pts',(7.77768053327363,-29.7432726184884,
56.6461210702653));
#109340=CARTESIAN_POINT('Ctrl Pts',(7.77956583391251,-29.7704919999724,
56.6502287597163));
#109341=CARTESIAN_POINT('Ctrl Pts',(7.78090492818634,-29.7896335978844,
56.6527778976221));
#109342=CARTESIAN_POINT('Ctrl Pts',(7.784238742733,-29.8369196142278,56.6582404071742));
#109343=CARTESIAN_POINT('Ctrl Pts',(7.78624806138309,-29.8651017184155,
56.6607705239147));
#109344=CARTESIAN_POINT('Ctrl Pts',(7.79546095777827,-29.9934115102855,
56.6690025611873));
#109345=CARTESIAN_POINT('Ctrl Pts',(7.8028370944624,-30.0938647460717,56.6663741579223));
#109346=CARTESIAN_POINT('Ctrl Pts',(7.81601040849399,-30.2753412307959,
56.645155692686));
#109347=CARTESIAN_POINT('Ctrl Pts',(7.82183992568639,-30.3563961126456,
56.629520032418));
#109348=CARTESIAN_POINT('Ctrl Pts',(7.82882366971938,-30.4548903340898,
56.6028147197367));
#109349=CARTESIAN_POINT('Ctrl Pts',(7.83015446910984,-30.4737180015393,
56.5973514183847));
#109350=CARTESIAN_POINT('Ctrl Pts',(7.83227086104797,-30.503742946058,56.5880613632532));
#109351=CARTESIAN_POINT('Ctrl Pts',(7.83306322630967,-30.5150030150613,
56.5844455674211));
#109352=CARTESIAN_POINT('Ctrl Pts',(7.83456775740151,-30.536414862361,56.5773174890502));
#109353=CARTESIAN_POINT('Ctrl Pts',(7.8352805734515,-30.5465729900774,56.5738263378019));
#109354=CARTESIAN_POINT('Ctrl Pts',(7.83691388118452,-30.5698748483488,
56.5655651198284));
#109355=CARTESIAN_POINT('Ctrl Pts',(7.83783208124924,-30.5829938300014,
56.5607272987701));
#109356=CARTESIAN_POINT('Ctrl Pts',(7.84074383938508,-30.6246380314961,
56.5447719989589));
#109357=CARTESIAN_POINT('Ctrl Pts',(7.84271671792307,-30.6529193600798,
56.5330328427604));
#109358=CARTESIAN_POINT('Ctrl Pts',(7.84737734417492,-30.7196789794392,
56.503139044398));
#109359=CARTESIAN_POINT('Ctrl Pts',(7.85004249251946,-30.757817324341,56.4842769632459));
#109360=CARTESIAN_POINT('Ctrl Pts',(7.85724860998728,-30.8599585141434,
56.4287964516835));
#109361=CARTESIAN_POINT('Ctrl Pts',(7.86172210057593,-30.922318605461,56.3893583772187));
#109362=CARTESIAN_POINT('Ctrl Pts',(7.86708635212909,-30.9931562915815,
56.3376815812076));
#109363=CARTESIAN_POINT('Ctrl Pts',(7.86794279505195,-31.0043459190581,
56.3293008316584));
#109364=CARTESIAN_POINT('Ctrl Pts',(7.87330715120606,-31.0735776699446,
56.2760747934682));
#109365=CARTESIAN_POINT('Ctrl Pts',(7.87786760414623,-31.1287038233733,
56.2275833377726));
#109366=CARTESIAN_POINT('Ctrl Pts',(7.88345955154642,-31.1891130484753,
56.1669262623574));
#109367=CARTESIAN_POINT('Ctrl Pts',(7.88426785085735,-31.1976802127793,
56.1581316116883));
#109368=CARTESIAN_POINT('Ctrl Pts',(7.88554495202271,-31.2109434769139,
56.1442116066855));
#109369=CARTESIAN_POINT('Ctrl Pts',(7.88600887765798,-31.2157062284432,
56.1391499755974));
#109370=CARTESIAN_POINT('Ctrl Pts',(7.88688151058901,-31.2245583480746,
56.1296236134685));
#109371=CARTESIAN_POINT('Ctrl Pts',(7.88728964360507,-31.2286552289323,
56.1251662009145));
#109372=CARTESIAN_POINT('Ctrl Pts',(7.88825605881983,-31.2382557009753,
56.1146059183747));
#109373=CARTESIAN_POINT('Ctrl Pts',(7.8888158268952,-31.2437385314501,56.1084845477414));
#109374=CARTESIAN_POINT('Ctrl Pts',(7.89070115173866,-31.2619526209694,
56.0878439573151));
#109375=CARTESIAN_POINT('Ctrl Pts',(7.89204026725288,-31.2744761648335,
56.0731445936323));
#109376=CARTESIAN_POINT('Ctrl Pts',(7.89537414655539,-31.3047122392942,
56.0363794995134));
#109377=CARTESIAN_POINT('Ctrl Pts',(7.89738350940413,-31.3221232040059,
56.0140742315358));
#109378=CARTESIAN_POINT('Ctrl Pts',(7.90659679740837,-31.3986329290325,
55.9107358812078));
#109379=CARTESIAN_POINT('Ctrl Pts',(7.91397329232241,-31.4509088925012,
55.8249107642318));
#109380=CARTESIAN_POINT('Ctrl Pts',(7.9271465324345,-31.5315066775885,55.6609360433827));
#109381=CARTESIAN_POINT('Ctrl Pts',(7.93297565374477,-31.5623292826959,
55.5843629414212));
#109382=CARTESIAN_POINT('Ctrl Pts',(7.93995901538397,-31.5933109535508,
55.4871349307183));
#109383=CARTESIAN_POINT('Ctrl Pts',(7.94128980341016,-31.598932388612,55.4683540423891));
#109384=CARTESIAN_POINT('Ctrl Pts',(7.94340618173923,-31.6074117931698,
55.4380903736915));
#109385=CARTESIAN_POINT('Ctrl Pts',(7.94419854460112,-31.6104810488991,
55.4266692535922));
#109386=CARTESIAN_POINT('Ctrl Pts',(7.9457030738659,-31.616105442028,55.4048142367437));
#109387=CARTESIAN_POINT('Ctrl Pts',(7.94641589046009,-31.61868177556,55.3943864661833));
#109388=CARTESIAN_POINT('Ctrl Pts',(7.94804920328722,-31.6243792662271,
55.3703288925008));
#109389=CARTESIAN_POINT('Ctrl Pts',(7.94896740785243,-31.6274300755234,
55.3566831341589));
#109390=CARTESIAN_POINT('Ctrl Pts',(7.95187919642386,-31.6366117267863,
55.3130419773073));
#109391=CARTESIAN_POINT('Ctrl Pts',(7.95385210027032,-31.6420879724912,
55.282914303293));
#109392=CARTESIAN_POINT('Ctrl Pts',(7.95851279929422,-31.6531809977565,
55.2106121423244));
#109393=CARTESIAN_POINT('Ctrl Pts',(7.96117799410164,-31.6580190158564,
55.1683395656584));
#109394=CARTESIAN_POINT('Ctrl Pts',(7.96838413370204,-31.6668048613645,
55.0524352083223));
#109395=CARTESIAN_POINT('Ctrl Pts',(7.97285760312556,-31.6674929153515,
54.9786543191881));
#109396=CARTESIAN_POINT('Ctrl Pts',(7.97822200922568,-31.6624964839714,
54.8911103660414));
#109397=CARTESIAN_POINT('Ctrl Pts',(7.97907862662128,-31.661524041769,54.8771612268574));
#109398=CARTESIAN_POINT('Ctrl Pts',(7.98444292609883,-31.6543548082804,
54.7901298280449));
#109399=CARTESIAN_POINT('Ctrl Pts',(7.98900314939803,-31.6435137818949,
54.7175198237225));
#109400=CARTESIAN_POINT('Ctrl Pts',(7.99459484191308,-31.6253177426105,
54.6338730014353));
#109401=CARTESIAN_POINT('Ctrl Pts',(7.99540314040856,-31.6225754969494,
54.6219054635903));
#109402=CARTESIAN_POINT('Ctrl Pts',(7.99668024064619,-31.6180742135462,
54.6032127212348));
#109403=CARTESIAN_POINT('Ctrl Pts',(7.99714416618442,-31.6164048617091,
54.5964660809779));
#109404=CARTESIAN_POINT('Ctrl Pts',(7.99801679953228,-31.6132024186657,
54.5838622674543));
#109405=CARTESIAN_POINT('Ctrl Pts',(7.99842493306825,-31.6116795505877,
54.5780027516996));
#109406=CARTESIAN_POINT('Ctrl Pts',(7.99939135017537,-31.6080143394654,
54.5642094325487));
#109407=CARTESIAN_POINT('Ctrl Pts',(7.99995111963336,-31.6058451931492,
54.5562830370985));
#109408=CARTESIAN_POINT('Ctrl Pts',(8.00183645150218,-31.5983827698241,
54.5297857750607));
#109409=CARTESIAN_POINT('Ctrl Pts',(8.00317557275699,-31.5928254863949,
54.5112917162276));
#109410=CARTESIAN_POINT('Ctrl Pts',(8.00650946905542,-31.5783364026377,
54.4659487819985));
#109411=CARTESIAN_POINT('Ctrl Pts',(8.00851884330254,-31.5690397929779,
54.4392233504771));
#109412=CARTESIAN_POINT('Ctrl Pts',(8.01773223419145,-31.5237162941274,
54.31889587768));
#109413=CARTESIAN_POINT('Ctrl Pts',(8.02510882288873,-31.4799627653021,
54.2284270276355));
#109414=CARTESIAN_POINT('Ctrl Pts',(8.03828201941204,-31.3859135837764,
54.0717799769512));
#109415=CARTESIAN_POINT('Ctrl Pts',(8.04411101395925,-31.3382991674952,
54.0043555409284));
#109416=CARTESIAN_POINT('Ctrl Pts',(8.05109425364852,-31.2734181694795,
53.9255948626369));
#109417=CARTESIAN_POINT('Ctrl Pts',(8.05242503832777,-31.2606884265202,
53.9106860040677));
#109418=CARTESIAN_POINT('Ctrl Pts',(8.05454141312019,-31.2398615655984,
53.8871481920678));
#109419=CARTESIAN_POINT('Ctrl Pts',(8.05533377573571,-31.2319308439942,
53.8783751712968));
#109420=CARTESIAN_POINT('Ctrl Pts',(8.05683830565413,-31.2166199590876,
53.8617964850396));
#109421=CARTESIAN_POINT('Ctrl Pts',(8.05755112313711,-31.2092564384435,
53.8539763346173));
#109422=CARTESIAN_POINT('Ctrl Pts',(8.05918443961101,-31.1921347033163,
53.8361416153578));
#109423=CARTESIAN_POINT('Ctrl Pts',(8.06010264691097,-31.1823249294284,
53.8261774958079));
#109424=CARTESIAN_POINT('Ctrl Pts',(8.06301445107528,-31.1506397252153,
53.7947940181171));
#109425=CARTESIAN_POINT('Ctrl Pts',(8.06498736748796,-31.1282981279739,
53.7738528803521));
#109426=CARTESIAN_POINT('Ctrl Pts',(8.0696481017676,-31.0735699597277,53.7253186834731));
#109427=CARTESIAN_POINT('Ctrl Pts',(8.07231331880534,-31.040678596113,53.6983267087313));
#109428=CARTESIAN_POINT('Ctrl Pts',(8.07951947072292,-30.948067180262,53.6280829110851));
#109429=CARTESIAN_POINT('Ctrl Pts',(8.08399293166016,-30.8864539014938,
53.5874888596716));
#109430=CARTESIAN_POINT('Ctrl Pts',(8.08935743038982,-30.8101931956547,
53.5442051850884));
#109431=CARTESIAN_POINT('Ctrl Pts',(8.09021414840303,-30.7979450499567,
53.5374558985732));
#109432=CARTESIAN_POINT('Ctrl Pts',(8.09557842413529,-30.7209381047754,
53.4962768664403));
#109433=CARTESIAN_POINT('Ctrl Pts',(8.10013852385392,-30.6540573596111,
53.4660048030172));
#109434=CARTESIAN_POINT('Ctrl Pts',(8.10573007927809,-30.5739151158481,
53.4359257743946));
#109435=CARTESIAN_POINT('Ctrl Pts',(8.10653837745834,-30.5623733761013,
53.4317388905237));
#109436=CARTESIAN_POINT('Ctrl Pts',(8.10781547739135,-30.5442274605415,
53.4253823396363));
#109437=CARTESIAN_POINT('Ctrl Pts',(8.10827940294775,-30.5376539180235,
53.4231256977185));
#109438=CARTESIAN_POINT('Ctrl Pts',(8.10915203571862,-30.5253280243721,
53.4189803534619));
#109439=CARTESIAN_POINT('Ctrl Pts',(8.10956016865383,-30.5195792499108,
53.4170817916549));
#109440=CARTESIAN_POINT('Ctrl Pts',(8.11052658399545,-30.5060030287681,
53.4126800986567));
#109441=CARTESIAN_POINT('Ctrl Pts',(8.11108635228107,-30.4981672687478,
53.4102035037174));
#109442=CARTESIAN_POINT('Ctrl Pts',(8.11297168031135,-30.471858470391,53.4021018559924));
#109443=CARTESIAN_POINT('Ctrl Pts',(8.11431079888123,-30.4533067742275,
53.3967402631907));
#109444=CARTESIAN_POINT('Ctrl Pts',(8.11764468799606,-30.4073539461049,
53.3843208046556));
#109445=CARTESIAN_POINT('Ctrl Pts',(8.1196540577223,-30.3798586655754,53.3776363807328));
#109446=CARTESIAN_POINT('Ctrl Pts',(8.12886741042828,-30.2541850188842,
53.3504533801769));
#109447=CARTESIAN_POINT('Ctrl Pts',(8.13624396510959,-30.1544483420492,
53.3381455381687));
#109448=CARTESIAN_POINT('Ctrl Pts',(8.1494171904731,-29.9718331268217,53.3322003625689));
#109449=CARTESIAN_POINT('Ctrl Pts',(8.15524624346938,-29.8893617754007,
53.3356346962159));
#109450=CARTESIAN_POINT('Ctrl Pts',(8.16222953788076,-29.7880015852572,
53.3474271859046));
#109451=CARTESIAN_POINT('Ctrl Pts',(8.16356032289799,-29.7685718438436,
53.3500359703248));
#109452=CARTESIAN_POINT('Ctrl Pts',(8.16567669699883,-29.737500971642,53.3547674608046));
#109453=CARTESIAN_POINT('Ctrl Pts',(8.16646905861369,-29.7258290509246,
53.3566722326081));
#109454=CARTESIAN_POINT('Ctrl Pts',(8.16797358582743,-29.703596540222,53.3605438844531));
#109455=CARTESIAN_POINT('Ctrl Pts',(8.16868640161362,-29.6930328071546,
53.3624889259901));
#109456=CARTESIAN_POINT('Ctrl Pts',(8.170319713004,-29.6687629437538,53.3672007161043));
#109457=CARTESIAN_POINT('Ctrl Pts',(8.17123791693804,-29.6550712339391,
53.3700381430823));
#109458=CARTESIAN_POINT('Ctrl Pts',(8.17414970500974,-29.6115199307771,
53.3796369357906));
#109459=CARTESIAN_POINT('Ctrl Pts',(8.17612260895051,-29.5818092768106,
53.3870493089765));
#109460=CARTESIAN_POINT('Ctrl Pts',(8.18078330878355,-29.5113515103222,
53.406705444463));
#109461=CARTESIAN_POINT('Ctrl Pts',(8.18344850424901,-29.4708356084273,
53.4196992962317));
#109462=CARTESIAN_POINT('Ctrl Pts',(8.19065464629215,-29.3615917532791,
53.4594082911376));
#109463=CARTESIAN_POINT('Ctrl Pts',(8.19512811731426,-29.294069905572,53.4891555445464));
#109464=CARTESIAN_POINT('Ctrl Pts',(8.20459017312364,-29.1569752385731,
53.5607570765928));
#109465=CARTESIAN_POINT('Ctrl Pts',(8.20957423370653,-29.0880468383341,
53.6034151552594));
#109466=CARTESIAN_POINT('Ctrl Pts',(8.21586584900291,-29.0094249711747,
53.6603814546508));
#109467=CARTESIAN_POINT('Ctrl Pts',(8.21692238130636,-28.9964882490675,
53.6700447926968));
#109468=CARTESIAN_POINT('Ctrl Pts',(8.21850511857984,-28.977539903036,53.68463249162));
#109469=CARTESIAN_POINT('Ctrl Pts',(8.219021997144,-28.9714185582601,53.6894136641493));
#109470=CARTESIAN_POINT('Ctrl Pts',(8.21994422016446,-28.9606197152262,
53.6979705238945));
#109471=CARTESIAN_POINT('Ctrl Pts',(8.22034836307997,-28.9559288917451,
53.7017289760014));
#109472=CARTESIAN_POINT('Ctrl Pts',(8.22122419628099,-28.9458534075547,
53.7098917291308));
#109473=CARTESIAN_POINT('Ctrl Pts',(8.22169644366011,-28.9404760071868,
53.7143043543697));
#109474=CARTESIAN_POINT('Ctrl Pts',(8.22301296868687,-28.9256332769151,
53.7266404597789));
#109475=CARTESIAN_POINT('Ctrl Pts',(8.22386202866696,-28.9162283592018,
53.7346354744026));
#109476=CARTESIAN_POINT('Ctrl Pts',(8.22585938682102,-28.8944727698386,
53.7535501195441));
#109477=CARTESIAN_POINT('Ctrl Pts',(8.2270123840631,-28.8821937710913,53.7645498995407));
#109478=CARTESIAN_POINT('Ctrl Pts',(8.23090034323011,-28.841655072139,53.8019643995563));
#109479=CARTESIAN_POINT('Ctrl Pts',(8.23367343440232,-28.8141536174004,
53.8291796650484));
#109480=CARTESIAN_POINT('Ctrl Pts',(8.24157336144965,-28.7391808075946,
53.9087255738542));
#109481=CARTESIAN_POINT('Ctrl Pts',(8.2467414030818,-28.6940535625495,53.963154351128));
#109482=CARTESIAN_POINT('Ctrl Pts',(8.25869913563055,-28.5969514253275,
54.0967067060545));
#109483=CARTESIAN_POINT('Ctrl Pts',(8.26541855150029,-28.5479806500927,
54.1777292059504));
#109484=CARTESIAN_POINT('Ctrl Pts',(8.27325579944305,-28.4973093277464,
54.2803649727449));
#109485=CARTESIAN_POINT('Ctrl Pts',(8.27461045852226,-28.4888011840107,
54.2984075061279));
#109486=CARTESIAN_POINT('Ctrl Pts',(8.27675545298924,-28.4757378446312,
54.3274507733873));
#109487=CARTESIAN_POINT('Ctrl Pts',(8.2775528893772,-28.4709732073057,54.3383545810277));
#109488=CARTESIAN_POINT('Ctrl Pts',(8.27906142254259,-28.4621374276909,
54.3591804461267));
#109489=CARTESIAN_POINT('Ctrl Pts',(8.27977322862785,-28.4580444945273,
54.3690925422433));
#109490=CARTESIAN_POINT('Ctrl Pts',(8.28139639334399,-28.4488888500594,
54.3918867243803));
#109491=CARTESIAN_POINT('Ctrl Pts',(8.28230556022336,-28.4438903496652,
54.4047938754036));
#109492=CARTESIAN_POINT('Ctrl Pts',(8.28515651846395,-28.428635215,54.4456920313092));
#109493=CARTESIAN_POINT('Ctrl Pts',(8.28707886797538,-28.4189683074252,
54.4738977536022));
#109494=CARTESIAN_POINT('Ctrl Pts',(8.2985133530453,-28.3654098926784,54.6450107049187));
#109495=CARTESIAN_POINT('Ctrl Pts',(8.3073877056156,-28.340162129873,54.793022665805));
#109496=CARTESIAN_POINT('Ctrl Pts',(8.31786221559161,-28.3343198191641,
54.961952380141));
#109497=CARTESIAN_POINT('Ctrl Pts',(8.3190804844051,-28.3339880886474,54.9814974401968));
#109498=CARTESIAN_POINT('Ctrl Pts',(8.32030899669651,-28.3340003265563,
55.0010431133336));
#109499=CARTESIAN_POINT('Ctrl Pts',(8.32030914920813,-28.3340003280773,
55.0010455397981));
#109500=CARTESIAN_POINT('Ctrl Pts',(8.32194769227677,-28.3340166884934,
55.0271147988701));
#109501=CARTESIAN_POINT('Ctrl Pts',(8.32360406721264,-28.3346449372721,
55.0531790113172));
#109502=CARTESIAN_POINT('Ctrl Pts',(8.32632093082785,-28.3366466934674,
55.09523022013));
#109503=CARTESIAN_POINT('Ctrl Pts',(8.3273651812665,-28.3376400610496,55.1112313189089));
#109504=CARTESIAN_POINT('Ctrl Pts',(8.32888511474766,-28.3394022593687,
55.1342416033686));
#109505=CARTESIAN_POINT('Ctrl Pts',(8.32935147437191,-28.3399849547518,
55.1412646790038));
#109506=CARTESIAN_POINT('Ctrl Pts',(8.33019846042677,-28.3411183219608,
55.1539477710566));
#109507=CARTESIAN_POINT('Ctrl Pts',(8.33057825232876,-28.3416534540907,
55.1596091138152));
#109508=CARTESIAN_POINT('Ctrl Pts',(8.33136428957251,-28.3428159595042,
55.1712700941568));
#109509=CARTESIAN_POINT('Ctrl Pts',(8.33177075129179,-28.3434469360366,
55.1772690925057));
#109510=CARTESIAN_POINT('Ctrl Pts',(8.33271291659901,-28.3449781720149,
55.1911046033392));
#109511=CARTESIAN_POINT('Ctrl Pts',(8.333249858305,-28.3459015212706,55.198938274101));
#109512=CARTESIAN_POINT('Ctrl Pts',(8.33496701273572,-28.3490158297965,
55.2238376865618));
#109513=CARTESIAN_POINT('Ctrl Pts',(8.3361576887361,-28.3514154721163,55.2408755639152));
#109514=CARTESIAN_POINT('Ctrl Pts',(8.34123777236479,-28.3626743593439,
55.3127376448182));
#109515=CARTESIAN_POINT('Ctrl Pts',(8.34522556615071,-28.3740075307818,
55.367134152179));
#109516=CARTESIAN_POINT('Ctrl Pts',(8.35316767324996,-28.4016930087281,
55.4731747815175));
#109517=CARTESIAN_POINT('Ctrl Pts',(8.35711500669199,-28.4178890354192,
55.5247884022205));
#109518=CARTESIAN_POINT('Ctrl Pts',(8.36103879467171,-28.436562302838,55.5755159138484));
#109519=CARTESIAN_POINT('Ctrl Pts',(8.16625309736762,-28.4365623102018,
55.5755159338529));
#109520=CARTESIAN_POINT('Ctrl Pts',(8.16546900852282,-28.4324787476223,
55.5644225908714));
#109521=CARTESIAN_POINT('Ctrl Pts',(8.1646888611418,-28.4285132831813,55.5532858653556));
#109522=CARTESIAN_POINT('Ctrl Pts',(8.16260809123437,-28.4182030219882,
55.5233248429461));
#109523=CARTESIAN_POINT('Ctrl Pts',(8.16131463944129,-28.4120756698158,
55.5044273457766));
#109524=CARTESIAN_POINT('Ctrl Pts',(8.15400401417909,-28.3791017214555,
55.396169449892));
#109525=CARTESIAN_POINT('Ctrl Pts',(8.14822704388146,-28.3594599777026,
55.3047836788268));
#109526=CARTESIAN_POINT('Ctrl Pts',(8.13814302729113,-28.3384785387546,
55.1414169046907));
#109527=CARTESIAN_POINT('Ctrl Pts',(8.13381646698004,-28.3339455089076,
55.0701010364793));
#109528=CARTESIAN_POINT('Ctrl Pts',(8.12585889475046,-28.3340444862641,
54.9416043726171));
#109529=CARTESIAN_POINT('Ctrl Pts',(8.12226602372084,-28.3370252731339,
54.8845381314829));
#109530=CARTESIAN_POINT('Ctrl Pts',(8.1177519470481,-28.344165103434,54.8158541310242));
#109531=CARTESIAN_POINT('Ctrl Pts',(8.11696448188888,-28.3455290147279,
54.8039779490404));
#109532=CARTESIAN_POINT('Ctrl Pts',(8.11571331928025,-28.3478785654863,
54.7852954409316));
#109533=CARTESIAN_POINT('Ctrl Pts',(8.11525418418712,-28.348778782158,54.7784785166936));
#109534=CARTESIAN_POINT('Ctrl Pts',(8.11438523257934,-28.3505530710785,
54.7656547984055));
#109535=CARTESIAN_POINT('Ctrl Pts',(8.11397592984726,-28.3514178051278,
54.7596469539634));
#109536=CARTESIAN_POINT('Ctrl Pts',(8.11299942379024,-28.3535496628824,
54.7453886020238));
#109537=CARTESIAN_POINT('Ctrl Pts',(8.11243063921369,-28.3548459875767,
54.7371427296385));
#109538=CARTESIAN_POINT('Ctrl Pts',(8.11048097973005,-28.3594762245311,
54.7090668706257));
#109539=CARTESIAN_POINT('Ctrl Pts',(8.10908530369263,-28.3631070215134,
54.6892885073624));
#109540=CARTESIAN_POINT('Ctrl Pts',(8.10557743963958,-28.3730293277662,
54.6402531092369));
#109541=CARTESIAN_POINT('Ctrl Pts',(8.10344877244855,-28.3797527453266,
54.611091244009));
#109542=CARTESIAN_POINT('Ctrl Pts',(8.09308103662054,-28.4159849388838,
54.4712560593727));
#109543=CARTESIAN_POINT('Ctrl Pts',(8.08463856667436,-28.4560691427194,
54.3636401338143));
#109544=CARTESIAN_POINT('Ctrl Pts',(8.0716448370268,-28.536633554827,54.200866850913));
#109545=CARTESIAN_POINT('Ctrl Pts',(8.06693618316653,-28.5699937877662,
54.1425972712099));
#109546=CARTESIAN_POINT('Ctrl Pts',(8.06106916973828,-28.6170649074812,
54.0708077405523));
#109547=CARTESIAN_POINT('Ctrl Pts',(8.05979720519407,-28.6276128114538,
54.0552983646907));
#109548=CARTESIAN_POINT('Ctrl Pts',(8.05775156035253,-28.6451301183857,
54.0304541433732));
#109549=CARTESIAN_POINT('Ctrl Pts',(8.0569718895653,-28.6519392106594,54.0210088435764));
#109550=CARTESIAN_POINT('Ctrl Pts',(8.05547692155473,-28.6652490759773,
54.002948131386));
#109551=CARTESIAN_POINT('Ctrl Pts',(8.05476112505549,-28.6717356194537,
53.9943230127946));
#109552=CARTESIAN_POINT('Ctrl Pts',(8.05309978540135,-28.68705348084,53.9743617038643));
#109553=CARTESIAN_POINT('Ctrl Pts',(8.05215681150299,-28.6959486521331,
53.9630754221371));
#109554=CARTESIAN_POINT('Ctrl Pts',(8.04907207461392,-28.7256970358459,
53.9263187373103));
#109555=CARTESIAN_POINT('Ctrl Pts',(8.04695474220814,-28.74715985946,53.901350232345));
#109556=CARTESIAN_POINT('Ctrl Pts',(8.04187226865597,-28.8010614640508,
53.8422799211189));
#109557=CARTESIAN_POINT('Ctrl Pts',(8.0389360108893,-28.8342326158722,53.8088844385573));
#109558=CARTESIAN_POINT('Ctrl Pts',(8.03183109091855,-28.9186875411587,
53.7307711687195));
#109559=CARTESIAN_POINT('Ctrl Pts',(8.02770383609716,-28.9713794343182,
53.6877049174311));
#109560=CARTESIAN_POINT('Ctrl Pts',(8.02330844259633,-29.0296581024667,
53.6457447752059));
#109561=CARTESIAN_POINT('Ctrl Pts',(8.0230743735086,-29.0327679287627,53.6435219381598));
#109562=CARTESIAN_POINT('Ctrl Pts',(8.01786334683111,-29.102133579534,53.5943006808269));
#109563=CARTESIAN_POINT('Ctrl Pts',(8.01284061693164,-29.171722824896,53.5522057810508));
#109564=CARTESIAN_POINT('Ctrl Pts',(8.00673017319034,-29.2550980487812,
53.509755191596));
#109565=CARTESIAN_POINT('Ctrl Pts',(8.00591726795293,-29.2661646092712,
53.5042747233868));
#109566=CARTESIAN_POINT('Ctrl Pts',(8.0046345438046,-29.2835660683993,53.4958966355738));
#109567=CARTESIAN_POINT('Ctrl Pts',(8.00416967275482,-29.2898602135499,
53.4929147374727));
#109568=CARTESIAN_POINT('Ctrl Pts',(8.00329649269078,-29.3016551582643,
53.4874170868999));
#109569=CARTESIAN_POINT('Ctrl Pts',(8.00288877162436,-29.3071511989961,
53.4848917130128));
#109570=CARTESIAN_POINT('Ctrl Pts',(8.00192502043843,-29.3201169499807,
53.4790193832166));
#109571=CARTESIAN_POINT('Ctrl Pts',(8.00136752728035,-29.3275977051412,
53.4756974889465));
#109572=CARTESIAN_POINT('Ctrl Pts',(7.99949738824004,-29.3526376119806,
53.4647984903462));
#109573=CARTESIAN_POINT('Ctrl Pts',(7.9981714647494,-29.3703019991891,53.4574689348044));
#109574=CARTESIAN_POINT('Ctrl Pts',(7.99487755470649,-29.4140572537097,
53.4401901756449));
#109575=CARTESIAN_POINT('Ctrl Pts',(7.99289538147933,-29.4402791342934,
53.430589930077));
#109576=CARTESIAN_POINT('Ctrl Pts',(7.98391882243183,-29.5590100201079,
53.3904746396749));
#109577=CARTESIAN_POINT('Ctrl Pts',(7.97675833426756,-29.6538472536567,
53.3674490779349));
#109578=CARTESIAN_POINT('Ctrl Pts',(7.96353290311014,-29.8349647461463,
53.3399765506513));
#109579=CARTESIAN_POINT('Ctrl Pts',(7.9574569470784,-29.9206536848369,53.3336798741204));
#109580=CARTESIAN_POINT('Ctrl Pts',(7.95023689186184,-30.0261430299179,
53.3340888309023));
#109581=CARTESIAN_POINT('Ctrl Pts',(7.94890036541021,-30.0458252244153,
53.3345140085225));
#109582=CARTESIAN_POINT('Ctrl Pts',(7.94677727012515,-30.0773277297797,
53.3357534352295));
#109583=CARTESIAN_POINT('Ctrl Pts',(7.94598384871292,-30.0891544006187,
53.3363450743846));
#109584=CARTESIAN_POINT('Ctrl Pts',(7.94447878517693,-30.1116868932502,
53.3377132538303));
#109585=CARTESIAN_POINT('Ctrl Pts',(7.94376647780302,-30.1223934302214,
53.3384672600128));
#109586=CARTESIAN_POINT('Ctrl Pts',(7.9421364137043,-30.1469869957855,53.3404382717573));
#109587=CARTESIAN_POINT('Ctrl Pts',(7.94122092039929,-30.1608676543762,
53.341726221602));
#109588=CARTESIAN_POINT('Ctrl Pts',(7.93832647686448,-30.2049499915313,
53.346375238147));
#109589=CARTESIAN_POINT('Ctrl Pts',(7.93636785511698,-30.2350776469022,
53.3503885194899));
#109590=CARTESIAN_POINT('Ctrl Pts',(7.93174789312771,-30.3066445631736,
53.3619225973425));
#109591=CARTESIAN_POINT('Ctrl Pts',(7.92910859949375,-30.347941924589,53.3701947190784));
#109592=CARTESIAN_POINT('Ctrl Pts',(7.92182837098411,-30.4620845980504,
53.3975952578798));
#109593=CARTESIAN_POINT('Ctrl Pts',(7.91726071798911,-30.5340105435723,
53.4201087854077));
#109594=CARTESIAN_POINT('Ctrl Pts',(7.9118254931315,-30.6167923712374,53.4523221719086));
#109595=CARTESIAN_POINT('Ctrl Pts',(7.91099547021895,-30.6293555933179,
53.457388247056));
#109596=CARTESIAN_POINT('Ctrl Pts',(7.90567971731644,-30.7092000568921,
53.4907229951963));
#109597=CARTESIAN_POINT('Ctrl Pts',(7.90114106778398,-30.7746162459226,
53.523230287453));
#109598=CARTESIAN_POINT('Ctrl Pts',(7.89557346532666,-30.848291891667,53.5660866426888));
#109599=CARTESIAN_POINT('Ctrl Pts',(7.89476541350128,-30.8588325425529,
53.572374947034));
#109600=CARTESIAN_POINT('Ctrl Pts',(7.89348870806266,-30.8752295279517,
53.5824043072435));
#109601=CARTESIAN_POINT('Ctrl Pts',(7.89302492773093,-30.8811338146683,
53.5860666667068));
#109602=CARTESIAN_POINT('Ctrl Pts',(7.89215257845308,-30.8921380957446,
53.592988184354));
#109603=CARTESIAN_POINT('Ctrl Pts',(7.8917445835153,-30.8972434608367,53.5962383398328));
#109604=CARTESIAN_POINT('Ctrl Pts',(7.8907785278172,-30.9092364130671,53.6039653921374));
#109605=CARTESIAN_POINT('Ctrl Pts',(7.89021898252295,-30.9161087216678,
53.608465492986));
#109606=CARTESIAN_POINT('Ctrl Pts',(7.88833458111314,-30.9390152971421,
53.6237083245001));
#109607=CARTESIAN_POINT('Ctrl Pts',(7.88699618031173,-30.9548954524501,
53.6346783895893));
#109608=CARTESIAN_POINT('Ctrl Pts',(7.88366431575138,-30.9935617605602,
53.6623937403691));
#109609=CARTESIAN_POINT('Ctrl Pts',(7.88165627098331,-31.0161185989506,
53.6794477328594));
#109610=CARTESIAN_POINT('Ctrl Pts',(7.87245368756215,-31.1165619573282,
53.7594849891748));
#109611=CARTESIAN_POINT('Ctrl Pts',(7.86508684248383,-31.1891057293026,
53.8288398422448));
#109612=CARTESIAN_POINT('Ctrl Pts',(7.85191064094459,-31.309292669304,53.9664972289344));
#109613=CARTESIAN_POINT('Ctrl Pts',(7.84606992941473,-31.3589102415018,
54.0326624554777));
#109614=CARTESIAN_POINT('Ctrl Pts',(7.83907562884825,-31.4139849812364,
54.1187584011698));
#109615=CARTESIAN_POINT('Ctrl Pts',(7.83774475576899,-31.4242565806027,
54.135457616866));
#109616=CARTESIAN_POINT('Ctrl Pts',(7.83562843921193,-31.4402473031941,
54.1625135808108));
#109617=CARTESIAN_POINT('Ctrl Pts',(7.83483622039832,-31.4461547662397,
54.172756262495));
#109618=CARTESIAN_POINT('Ctrl Pts',(7.8333320926736,-31.4572177774492,54.1924186537517));
#109619=CARTESIAN_POINT('Ctrl Pts',(7.8326195326189,-31.4623922532045,54.2018269681982));
#109620=CARTESIAN_POINT('Ctrl Pts',(7.83098699700206,-31.4740909391633,
54.2235934259987));
#109621=CARTESIAN_POINT('Ctrl Pts',(7.83006930914324,-31.4805513999805,
54.235985054596));
#109622=CARTESIAN_POINT('Ctrl Pts',(7.82716001290008,-31.5006516964904,
54.2757515434737));
#109623=CARTESIAN_POINT('Ctrl Pts',(7.82518903873379,-31.5136944720293,
54.3034222409728));
#109624=CARTESIAN_POINT('Ctrl Pts',(7.82053367074762,-31.543014066843,54.3703431421876));
#109625=CARTESIAN_POINT('Ctrl Pts',(7.81787180813912,-31.5585660890979,
54.4098878968463));
#109626=CARTESIAN_POINT('Ctrl Pts',(7.81066718564559,-31.5969304771628,
54.519578706459));
#109627=CARTESIAN_POINT('Ctrl Pts',(7.80619213276827,-31.6166246125156,
54.5907118408678));
#109628=CARTESIAN_POINT('Ctrl Pts',(7.80083998974719,-31.6343260681113,
54.67638973737));
#109629=CARTESIAN_POINT('Ctrl Pts',(7.79999712957875,-31.6369428261872,
54.6898976345195));
#109630=CARTESIAN_POINT('Ctrl Pts',(7.79462853320518,-31.6525019294607,
54.7759077140508));
#109631=CARTESIAN_POINT('Ctrl Pts',(7.79005037438479,-31.6607903231339,
54.8491599059464));
#109632=CARTESIAN_POINT('Ctrl Pts',(7.78443891600197,-31.6647757171713,
54.9349729018631));
#109633=CARTESIAN_POINT('Ctrl Pts',(7.78363070096398,-31.6652096702806,
54.9472416430588));
#109634=CARTESIAN_POINT('Ctrl Pts',(7.78235379315276,-31.665676847285,54.9664601280206));
#109635=CARTESIAN_POINT('Ctrl Pts',(7.78188997616242,-31.6658022439129,
54.9734074748025));
#109636=CARTESIAN_POINT('Ctrl Pts',(7.78101759921209,-31.6659555402362,
54.9864070727862));
#109637=CARTESIAN_POINT('Ctrl Pts',(7.78060961373072,-31.6659939248547,
54.9924589532505));
#109638=CARTESIAN_POINT('Ctrl Pts',(7.77964363661456,-31.6660066763997,
55.0067245017045));
#109639=CARTESIAN_POINT('Ctrl Pts',(7.77908416117705,-31.6659532755312,
55.014937918535));
#109640=CARTESIAN_POINT('Ctrl Pts',(7.77720024656801,-31.6655710354316,
55.0424428808545));
#109641=CARTESIAN_POINT('Ctrl Pts',(7.77586227187023,-31.6649678121603,
55.0617282543878));
#109642=CARTESIAN_POINT('Ctrl Pts',(7.77253170571016,-31.6626557677863,
55.1092272434393));
#109643=CARTESIAN_POINT('Ctrl Pts',(7.77052454681614,-31.6605636233287,
55.1374156667221));
#109644=CARTESIAN_POINT('Ctrl Pts',(7.76132982361888,-31.6478131991142,
55.2651047806643));
#109645=CARTESIAN_POINT('Ctrl Pts',(7.75397016803103,-31.6289206569506,
55.3635750560071));
#109646=CARTESIAN_POINT('Ctrl Pts',(7.740792332311,-31.5784866574934,55.5392340574848));
#109647=CARTESIAN_POINT('Ctrl Pts',(7.73494352861573,-31.5497793390555,
55.6169126425103));
#109648=CARTESIAN_POINT('Ctrl Pts',(7.72794141551738,-31.5072707847691,
55.7099825307644));
#109649=CARTESIAN_POINT('Ctrl Pts',(7.72661031233688,-31.4988107101176,
55.7276722647103));
#109650=CARTESIAN_POINT('Ctrl Pts',(7.72449371985725,-31.484750962785,55.7557846200141));
#109651=CARTESIAN_POINT('Ctrl Pts',(7.72370145208496,-31.4793493633843,
55.7663036518721));
#109652=CARTESIAN_POINT('Ctrl Pts',(7.72219728644031,-31.4688301486798,
55.7862628518513));
#109653=CARTESIAN_POINT('Ctrl Pts',(7.72148473684885,-31.4637323889801,
55.7957127500098));
#109654=CARTESIAN_POINT('Ctrl Pts',(7.71985230273546,-31.4517912495304,
55.8173453330737));
#109655=CARTESIAN_POINT('Ctrl Pts',(7.71893470491997,-31.4448851897696,
55.8294926363736));
#109656=CARTESIAN_POINT('Ctrl Pts',(7.71602601921615,-31.4223823722624,
55.8679396485503));
#109657=CARTESIAN_POINT('Ctrl Pts',(7.71405555293017,-31.4062135939717,
55.893898407259));
#109658=CARTESIAN_POINT('Ctrl Pts',(7.70940164256252,-31.3659066215379,
55.9548078123419));
#109659=CARTESIAN_POINT('Ctrl Pts',(7.70674070961701,-31.341128450423,55.9893097167809));
#109660=CARTESIAN_POINT('Ctrl Pts',(7.69953660653275,-31.2697905595201,
56.0810292800917));
#109661=CARTESIAN_POINT('Ctrl Pts',(7.69506120270623,-31.2207087286931,
56.1361614923766));
#109662=CARTESIAN_POINT('Ctrl Pts',(7.68971382987555,-31.1583853663143,
56.1974499424351));
#109663=CARTESIAN_POINT('Ctrl Pts',(7.68887606729939,-31.1485170256714,
56.2069182481364));
#109664=CARTESIAN_POINT('Ctrl Pts',(7.68350636732053,-31.0846905780033,
56.2666655909917));
#109665=CARTESIAN_POINT('Ctrl Pts',(7.67892205130089,-31.0275669466909,
56.3134301586142));
#109666=CARTESIAN_POINT('Ctrl Pts',(7.67330375513987,-30.9575480283627,
56.3633812727313));
#109667=CARTESIAN_POINT('Ctrl Pts',(7.67249551524096,-30.9474755745075,
56.3704002099435));
#109668=CARTESIAN_POINT('Ctrl Pts',(7.67121857658665,-30.9315822833227,
56.3812163962233));
#109669=CARTESIAN_POINT('Ctrl Pts',(7.67075475399479,-30.9258134552311,
56.3850897897023));
#109670=CARTESIAN_POINT('Ctrl Pts',(7.66988237278712,-30.9149750155157,
56.3922691372242));
#109671=CARTESIAN_POINT('Ctrl Pts',(7.66947438872151,-30.9099114027328,
56.3955837001008));
#109672=CARTESIAN_POINT('Ctrl Pts',(7.66850842349245,-30.8979333566605,
56.4033314466776));
#109673=CARTESIAN_POINT('Ctrl Pts',(7.66794895863715,-30.891004075234,56.407741166936));
#109674=CARTESIAN_POINT('Ctrl Pts',(7.66606511783465,-30.8676895567504,
56.4223371858038));
#109675=CARTESIAN_POINT('Ctrl Pts',(7.66472720775049,-30.8511607041876,
56.4322896401871));
#109676=CARTESIAN_POINT('Ctrl Pts',(7.66139683848214,-30.810003199556,56.4561076559533));
#109677=CARTESIAN_POINT('Ctrl Pts',(7.65938981392534,-30.7851878409481,
56.4696375618476));
#109678=CARTESIAN_POINT('Ctrl Pts',(7.65019628198844,-30.6710101870318,
56.5281725370147));
#109679=CARTESIAN_POINT('Ctrl Pts',(7.64283771594158,-30.5780486528418,
56.5657030917546));
#109680=CARTESIAN_POINT('Ctrl Pts',(7.62965963226652,-30.4031158893757,
56.6186086127721));
#109681=CARTESIAN_POINT('Ctrl Pts',(7.6238096017832,-30.3222688212911,56.636625425118));
#109682=CARTESIAN_POINT('Ctrl Pts',(7.61680630458279,-30.2210046219497,
56.6513925606158));
#109683=CARTESIAN_POINT('Ctrl Pts',(7.61547516674784,-30.2015537731965,
56.6538792476108));
#109684=CARTESIAN_POINT('Ctrl Pts',(7.61335853269813,-30.1703092579291,
56.6573142648629));
#109685=CARTESIAN_POINT('Ctrl Pts',(7.61256625753809,-30.1585420226049,
56.658481309934));
#109686=CARTESIAN_POINT('Ctrl Pts',(7.61106208614438,-30.1360681069418,
56.6604688336651));
#109687=CARTESIAN_POINT('Ctrl Pts',(7.61034953810482,-30.1253640212102,
56.6613112738711));
#109688=CARTESIAN_POINT('Ctrl Pts',(7.60871711920563,-30.1007133393514,
56.6630117387076));
#109689=CARTESIAN_POINT('Ctrl Pts',(7.60779953490273,-30.0867624737311,
56.6637979182151));
#109690=CARTESIAN_POINT('Ctrl Pts',(7.60489094090366,-30.0422581709076,
56.6657445840105));
#109691=CARTESIAN_POINT('Ctrl Pts',(7.6029205509142,-30.0116809387551,56.6662396333481));
#109692=CARTESIAN_POINT('Ctrl Pts',(7.59826685952555,-29.9386507725836,
56.6654113403378));
#109693=CARTESIAN_POINT('Ctrl Pts',(7.59560606624645,-29.8962277386669,
56.6633070543167));
#109694=CARTESIAN_POINT('Ctrl Pts',(7.58840204249181,-29.7804804725137,
56.6531193737223));
#109695=CARTESIAN_POINT('Ctrl Pts',(7.58392658717963,-29.7075404125967,
56.6417856876531));
#109696=CARTESIAN_POINT('Ctrl Pts',(7.57445468397707,-29.5564589046027,
56.6079190951));
#109697=CARTESIAN_POINT('Ctrl Pts',(7.56946275296196,-29.4787368325959,
56.5844286264686));
#109698=CARTESIAN_POINT('Ctrl Pts',(7.56316352201244,-29.3879867527561,
56.5495986265538));
#109699=CARTESIAN_POINT('Ctrl Pts',(7.56210821029538,-29.3730148709698,
56.5436015416121));
#109700=CARTESIAN_POINT('Ctrl Pts',(7.5605270577653,-29.3509701531688,56.5343977675635));
#109701=CARTESIAN_POINT('Ctrl Pts',(7.56001051929912,-29.3438283773067,
56.5313572564199));
#109702=CARTESIAN_POINT('Ctrl Pts',(7.55908877903474,-29.3311961112442,
56.5258746560235));
#109703=CARTESIAN_POINT('Ctrl Pts',(7.55868477604811,-29.3256972062326,
56.523452607614));
#109704=CARTESIAN_POINT('Ctrl Pts',(7.55778911525175,-29.3135907342639,
56.5180418007835));
#109705=CARTESIAN_POINT('Ctrl Pts',(7.55729669037934,-29.3069896099765,
56.5150396639586));
#109706=CARTESIAN_POINT('Ctrl Pts',(7.55584129356492,-29.2876340401669,
56.5060839487491));
#109707=CARTESIAN_POINT('Ctrl Pts',(7.55487165208585,-29.2749355656764,
56.5000118848959));
#109708=CARTESIAN_POINT('Ctrl Pts',(7.54806860581032,-29.1871007072822,
56.456635774672));
#109709=CARTESIAN_POINT('Ctrl Pts',(7.54198189040395,-29.1148057167452,
56.4138674778945));
#109710=CARTESIAN_POINT('Ctrl Pts',(7.52652509404827,-28.9406920829547,
56.292260316728));
#109711=CARTESIAN_POINT('Ctrl Pts',(7.51721417737031,-28.8441848903718,
56.2067200671039));
#109712=CARTESIAN_POINT('Ctrl Pts',(7.50692684856819,-28.744471106177,56.095282386431));
#109713=CARTESIAN_POINT('Ctrl Pts',(7.50549531179536,-28.7307750450062,
56.0793814860348));
#109714=CARTESIAN_POINT('Ctrl Pts',(7.50317533137304,-28.7088834736268,
56.0529726812225));
#109715=CARTESIAN_POINT('Ctrl Pts',(7.5022796488648,-28.7005074940628,56.0426181453256));
#109716=CARTESIAN_POINT('Ctrl Pts',(7.50067542772868,-28.6856467537763,
56.0237897050599));
#109717=CARTESIAN_POINT('Ctrl Pts',(7.49996514494438,-28.6791176127512,
56.0153519311982));
#109718=CARTESIAN_POINT('Ctrl Pts',(7.49844864434826,-28.6652894490124,
55.9971222991381));
#109719=CARTESIAN_POINT('Ctrl Pts',(7.4976434587183,-28.6580160994207,55.9873116824316));
#109720=CARTESIAN_POINT('Ctrl Pts',(7.49543584894414,-28.638271690347,55.9600581991023));
#109721=CARTESIAN_POINT('Ctrl Pts',(7.49404214718164,-28.6260282016741,
55.9424528107725));
#109722=CARTESIAN_POINT('Ctrl Pts',(7.48818262791022,-28.575570571396,55.8668236908045));
#109723=CARTESIAN_POINT('Ctrl Pts',(7.483837667993,-28.540663753194,55.8066733054715));
#109724=CARTESIAN_POINT('Ctrl Pts',(7.47576624225721,-28.4821501698588,
55.6895391101249));
#109725=CARTESIAN_POINT('Ctrl Pts',(7.47203392693749,-28.4577667277519,
55.6331195097459));
#109726=CARTESIAN_POINT('Ctrl Pts',(7.4682788092303,-28.4365623654365,55.5755160839024));
#109727=CARTESIAN_POINT('Origin',(5.,-30.,55.));
#109728=CARTESIAN_POINT('',(6.76892552105682,-28.4365623357949,55.5755160033788));
#109729=CARTESIAN_POINT('',(6.96168426276526,-28.4365622954254,55.5755158937115));
#109730=CARTESIAN_POINT('',(5.,-28.4365623102018,55.5755159338528));
#109731=CARTESIAN_POINT('Ctrl Pts',(6.96168426276526,-28.4365622954254,
55.5755158937115));
#109732=CARTESIAN_POINT('Ctrl Pts',(6.96621518142781,-28.4616675932655,
55.6437165631571));
#109733=CARTESIAN_POINT('Ctrl Pts',(6.97064208339495,-28.4912153733055,
55.7102200871842));
#109734=CARTESIAN_POINT('Ctrl Pts',(6.98045131201361,-28.5658855718998,
55.8524056583878));
#109735=CARTESIAN_POINT('Ctrl Pts',(6.98582286381548,-28.6128348680477,
55.9268489312456));
#109736=CARTESIAN_POINT('Ctrl Pts',(6.99273224835812,-28.6769889517844,
56.0127046830646));
#109737=CARTESIAN_POINT('Ctrl Pts',(6.9939911449183,-28.6888171338552,56.0279729676906));
#109738=CARTESIAN_POINT('Ctrl Pts',(6.99581023495253,-28.7060527208452,
56.0494398416683));
#109739=CARTESIAN_POINT('Ctrl Pts',(6.99635636275573,-28.7112452400216,
56.0558099753933));
#109740=CARTESIAN_POINT('Ctrl Pts',(6.99731062774461,-28.7203444544684,
56.0668056713412));
#109741=CARTESIAN_POINT('Ctrl Pts',(6.99771723422941,-28.7242295780451,
56.0714487784013));
#109742=CARTESIAN_POINT('Ctrl Pts',(6.99859466467693,-28.7326289929784,
56.0813764524015));
#109743=CARTESIAN_POINT('Ctrl Pts',(6.99906601418982,-28.7371509997338,
56.0866539004525));
#109744=CARTESIAN_POINT('Ctrl Pts',(7.00037624838465,-28.749751868468,56.1011749736396));
#109745=CARTESIAN_POINT('Ctrl Pts',(7.00121987943293,-28.7578998983068,
56.1103576127689));
#109746=CARTESIAN_POINT('Ctrl Pts',(7.00712258834165,-28.8151970859454,
56.173510313324));
#109747=CARTESIAN_POINT('Ctrl Pts',(7.01238275956817,-28.8677406511134,
56.2242837933754));
#109748=CARTESIAN_POINT('Ctrl Pts',(7.01866998297382,-28.9337897989067,
56.2802092961043));
#109749=CARTESIAN_POINT('Ctrl Pts',(7.01965683970123,-28.9442495711575,
56.2888487355971));
#109750=CARTESIAN_POINT('Ctrl Pts',(7.02605497037705,-29.0127083006775,
56.3440008618084));
#109751=CARTESIAN_POINT('Ctrl Pts',(7.03146755548613,-29.0736637822695,
56.3867176214096));
#109752=CARTESIAN_POINT('Ctrl Pts',(7.03981425682617,-29.1737129336764,
56.4472802831541));
#109753=CARTESIAN_POINT('Ctrl Pts',(7.04281780370092,-29.2109888247271,
56.4679347412167));
#109754=CARTESIAN_POINT('Ctrl Pts',(7.04790219938002,-29.2763767610055,
56.5009546190904));
#109755=CARTESIAN_POINT('Ctrl Pts',(7.05000465795058,-29.304112765303,56.5140133855634));
#109756=CARTESIAN_POINT('Ctrl Pts',(7.05302861890522,-29.3450098454189,
56.5319071632787));
#109757=CARTESIAN_POINT('Ctrl Pts',(7.05397064568387,-29.3578951848249,
56.5373526227106));
#109758=CARTESIAN_POINT('Ctrl Pts',(7.05562634932108,-29.3807941633213,
56.5466917968988));
#109759=CARTESIAN_POINT('Ctrl Pts',(7.05634223797634,-29.3907795927555,
56.5506520845949));
#109760=CARTESIAN_POINT('Ctrl Pts',(7.05783927153277,-29.4118344015886,
56.5587677843286));
#109761=CARTESIAN_POINT('Ctrl Pts',(7.05861969177156,-29.4229111546025,
56.5629025091999));
#109762=CARTESIAN_POINT('Ctrl Pts',(7.06068286589565,-29.452453973323,56.5735733301861));
#109763=CARTESIAN_POINT('Ctrl Pts',(7.06195875277496,-29.470993236278,56.5799023935795));
#109764=CARTESIAN_POINT('Ctrl Pts',(7.06855152141681,-29.5681014126966,
56.6111527766408));
#109765=CARTESIAN_POINT('Ctrl Pts',(7.07368575319151,-29.6483329508286,
56.6305466646248));
#109766=CARTESIAN_POINT('Ctrl Pts',(7.08491115739104,-29.828668763627,56.660200438404));
#109767=CARTESIAN_POINT('Ctrl Pts',(7.09094296923891,-29.9289195531927,
56.6675026571761));
#109768=CARTESIAN_POINT('Ctrl Pts',(7.09900513516252,-30.0575029425793,
56.6652477505995));
#109769=CARTESIAN_POINT('Ctrl Pts',(7.10079892255601,-30.0857757204209,
56.6640309505864));
#109770=CARTESIAN_POINT('Ctrl Pts',(7.10386785218044,-30.1332687369025,
56.6607734318758));
#109771=CARTESIAN_POINT('Ctrl Pts',(7.10512664904486,-30.1525099028869,
56.6591171145437));
#109772=CARTESIAN_POINT('Ctrl Pts',(7.1069456199482,-30.1798913003411,56.6562797644973));
#109773=CARTESIAN_POINT('Ctrl Pts',(7.10749173082356,-30.1880591027401,
56.6553722557459));
#109774=CARTESIAN_POINT('Ctrl Pts',(7.10844597672613,-30.2022318599154,
56.6536913043409));
#109775=CARTESIAN_POINT('Ctrl Pts',(7.1088525812426,-30.2082398547515,56.6529454972162));
#109776=CARTESIAN_POINT('Ctrl Pts',(7.1097300199277,-30.2211361800173,56.6512731733999));
#109777=CARTESIAN_POINT('Ctrl Pts',(7.11020137976753,-30.2280227138228,
56.6503363114462));
#109778=CARTESIAN_POINT('Ctrl Pts',(7.11151166998711,-30.2470575564767,
56.6476253497013));
#109779=CARTESIAN_POINT('Ctrl Pts',(7.11235534736275,-30.2591921405052,
56.6457600497577));
#109780=CARTESIAN_POINT('Ctrl Pts',(7.11827021345181,-30.3434985463762,
56.631845184428));
#109781=CARTESIAN_POINT('Ctrl Pts',(7.12354345524137,-30.414821449314,56.6151875278324));
#109782=CARTESIAN_POINT('Ctrl Pts',(7.12988609766378,-30.4983484276038,
56.5897814599893));
#109783=CARTESIAN_POINT('Ctrl Pts',(7.13091558348857,-30.5118337578577,
56.5854912318652));
#109784=CARTESIAN_POINT('Ctrl Pts',(7.13730938858278,-30.5952008931364,
56.5577943155168));
#109785=CARTESIAN_POINT('Ctrl Pts',(7.14267361662341,-30.6635246454671,
56.5299423479419));
#109786=CARTESIAN_POINT('Ctrl Pts',(7.15096898362861,-30.7680184096244,
56.4790242830641));
#109787=CARTESIAN_POINT('Ctrl Pts',(7.15396786626985,-30.8055290254171,
56.4589340628651));
#109788=CARTESIAN_POINT('Ctrl Pts',(7.15904533529387,-30.8686474719768,
56.421951084817));
#109789=CARTESIAN_POINT('Ctrl Pts',(7.1611454515922,-30.8946324639411,56.4057475898815));
#109790=CARTESIAN_POINT('Ctrl Pts',(7.16416672082881,-30.93181357247,56.3811136678013));
#109791=CARTESIAN_POINT('Ctrl Pts',(7.16510834657614,-30.943372104113,56.373244548908));
#109792=CARTESIAN_POINT('Ctrl Pts',(7.16676359793443,-30.9636323138791,
56.359074733226));
#109793=CARTESIAN_POINT('Ctrl Pts',(7.16747943125642,-30.9723745493317,
56.352833734036));
#109794=CARTESIAN_POINT('Ctrl Pts',(7.16897659545759,-30.9906137865963,
56.3395447625111));
#109795=CARTESIAN_POINT('Ctrl Pts',(7.16975719930146,-31.0000973623873,
56.3324793142298));
#109796=CARTESIAN_POINT('Ctrl Pts',(7.17182143522502,-31.025098045213,56.3134360309749));
#109797=CARTESIAN_POINT('Ctrl Pts',(7.17309818736336,-31.0404806551089,
56.3012840845532));
#109798=CARTESIAN_POINT('Ctrl Pts',(7.17969080504897,-31.119400282756,56.2366448120204));
#109799=CARTESIAN_POINT('Ctrl Pts',(7.18482411989755,-31.1791966486213,
56.1797648604262));
#109800=CARTESIAN_POINT('Ctrl Pts',(7.19604801789148,-31.301898830322,56.0443549800158));
#109801=CARTESIAN_POINT('Ctrl Pts',(7.20207925632942,-31.3623991066989,
55.9640976176675));
#109802=CARTESIAN_POINT('Ctrl Pts',(7.21014073276843,-31.4302373332694,
55.854855402271));
#109803=CARTESIAN_POINT('Ctrl Pts',(7.21193444353455,-31.4445484845188,
55.8304433054732));
#109804=CARTESIAN_POINT('Ctrl Pts',(7.2150032552912,-31.4675692333252,55.7887771989649));
#109805=CARTESIAN_POINT('Ctrl Pts',(7.21626201254865,-31.4766130971013,
55.7717140711922));
#109806=CARTESIAN_POINT('Ctrl Pts',(7.21808093612233,-31.4890796617931,
55.7471715314109));
#109807=CARTESIAN_POINT('Ctrl Pts',(7.21862704027083,-31.4927470977546,
55.7398172961326));
#109808=CARTESIAN_POINT('Ctrl Pts',(7.21958127858724,-31.4990215967239,
55.7269985609439));
#109809=CARTESIAN_POINT('Ctrl Pts',(7.21998788231997,-31.5016535251124,
55.7215464948521));
#109810=CARTESIAN_POINT('Ctrl Pts',(7.22086532427292,-31.507243053211,55.7098046792364));
#109811=CARTESIAN_POINT('Ctrl Pts',(7.22133668821244,-31.5101909861983,
55.7035108278614));
#109812=CARTESIAN_POINT('Ctrl Pts',(7.22264700068007,-31.518237332114,55.6860482045806));
#109813=CARTESIAN_POINT('Ctrl Pts',(7.22349069645405,-31.5232516753402,
55.6748414977552));
#109814=CARTESIAN_POINT('Ctrl Pts',(7.22941044138503,-31.5573139459685,
55.5964004568086));
#109815=CARTESIAN_POINT('Ctrl Pts',(7.2346889293594,-31.5820214166076,55.5273766125611));
#109816=CARTESIAN_POINT('Ctrl Pts',(7.24103312200397,-31.6059735451085,
55.44340027442));
#109817=CARTESIAN_POINT('Ctrl Pts',(7.24205896876814,-31.6096688516448,
55.4297918277798));
#109818=CARTESIAN_POINT('Ctrl Pts',(7.24844958324113,-31.6316006943965,
55.3447713906876));
#109819=CARTESIAN_POINT('Ctrl Pts',(7.25381422201391,-31.6452554597833,
55.2722570870789));
#109820=CARTESIAN_POINT('Ctrl Pts',(7.26210883717743,-31.6591440513098,
55.1568593254738));
#109821=CARTESIAN_POINT('Ctrl Pts',(7.26510662173684,-31.6626071101923,
55.1144636658827));
#109822=CARTESIAN_POINT('Ctrl Pts',(7.27018245977213,-31.6657667624,55.04139964646));
#109823=CARTESIAN_POINT('Ctrl Pts',(7.27228202438619,-31.6662462802018,
55.0107881790076));
#109824=CARTESIAN_POINT('Ctrl Pts',(7.27530265957547,-31.6657157551822,
54.96619937969));
#109825=CARTESIAN_POINT('Ctrl Pts',(7.27624419081851,-31.6653734541985,
54.9522219952471));
#109826=CARTESIAN_POINT('Ctrl Pts',(7.27789933561335,-31.6644571358084,
54.9275168560619));
#109827=CARTESIAN_POINT('Ctrl Pts',(7.27861515591332,-31.6639552387455,
54.9167874057729));
#109828=CARTESIAN_POINT('Ctrl Pts',(7.2801123509929,-31.6626827836571,54.8942558652585));
#109829=CARTESIAN_POINT('Ctrl Pts',(7.28089299817733,-31.66189024367,54.8824555776007));
#109830=CARTESIAN_POINT('Ctrl Pts',(7.28295748474491,-31.6594501587259,
54.8511191539172));
#109831=CARTESIAN_POINT('Ctrl Pts',(7.28423444113182,-31.6575832903937,
54.8316015924579));
#109832=CARTESIAN_POINT('Ctrl Pts',(7.2908340214254,-31.6460668721509,54.7301323310598));
#109833=CARTESIAN_POINT('Ctrl Pts',(7.29597358115768,-31.630682765215,54.6489431522947));
#109834=CARTESIAN_POINT('Ctrl Pts',(7.30719789076433,-31.5834295010451,
54.4724106234053));
#109835=CARTESIAN_POINT('Ctrl Pts',(7.31322386323513,-31.5488355934436,
54.3781435087354));
#109836=CARTESIAN_POINT('Ctrl Pts',(7.32127900734691,-31.4938894219803,
54.2619957108953));
#109837=CARTESIAN_POINT('Ctrl Pts',(7.32307201393636,-31.4811461754492,
54.236742663029));
#109838=CARTESIAN_POINT('Ctrl Pts',(7.32613974251045,-31.4586338393338,
54.1948192588194));
#109839=CARTESIAN_POINT('Ctrl Pts',(7.32739813576945,-31.4492060642606,
54.1779717714153));
#109840=CARTESIAN_POINT('Ctrl Pts',(7.3292166243775,-31.4353514814661,54.1541929029019));
#109841=CARTESIAN_POINT('Ctrl Pts',(7.32976266671018,-31.4311624149671,
54.1471238918628));
#109842=CARTESIAN_POINT('Ctrl Pts',(7.33071683533746,-31.4237964218145,
54.1349009288898));
#109843=CARTESIAN_POINT('Ctrl Pts',(7.33112343189134,-31.4206434164772,
54.1297328367203));
#109844=CARTESIAN_POINT('Ctrl Pts',(7.33200090396927,-31.413809917374,54.1186681503736));
#109845=CARTESIAN_POINT('Ctrl Pts',(7.3324723056546,-31.410120727729,54.1127774571996));
#109846=CARTESIAN_POINT('Ctrl Pts',(7.3337828228654,-31.3998120274257,54.096543812465));
#109847=CARTESIAN_POINT('Ctrl Pts',(7.33462668793699,-31.3931150106181,
54.086250942553));
#109848=CARTESIAN_POINT('Ctrl Pts',(7.34059242515841,-31.3453186346939,
54.0145380033295));
#109849=CARTESIAN_POINT('Ctrl Pts',(7.34592038894971,-31.3002901097811,
53.9558444632713));
#109850=CARTESIAN_POINT('Ctrl Pts',(7.35218794612908,-31.2433539942865,
53.8910455671176));
#109851=CARTESIAN_POINT('Ctrl Pts',(7.35308802366798,-31.2350838655923,
53.8818421704967));
#109852=CARTESIAN_POINT('Ctrl Pts',(7.36062545788623,-31.1650070666426,
53.8055834316504));
#109853=CARTESIAN_POINT('Ctrl Pts',(7.36725972676522,-31.097886844223,53.7436083656047));
#109854=CARTESIAN_POINT('Ctrl Pts',(7.37724821209399,-30.9865425254855,
53.6565710456839));
#109855=CARTESIAN_POINT('Ctrl Pts',(7.38073115976119,-30.9456835841416,
53.6275019235884));
#109856=CARTESIAN_POINT('Ctrl Pts',(7.38528285569322,-30.8895369049362,
53.5912561711071));
#109857=CARTESIAN_POINT('Ctrl Pts',(7.38641285185037,-30.875365759119,53.5824070034882));
#109858=CARTESIAN_POINT('Ctrl Pts',(7.38828856707251,-30.8514596660405,
53.5679740616524));
#109859=CARTESIAN_POINT('Ctrl Pts',(7.38903852978729,-30.8417973694629,
53.5622729569252));
#109860=CARTESIAN_POINT('Ctrl Pts',(7.3905102575756,-30.8226341482198,53.5512253846552));
#109861=CARTESIAN_POINT('Ctrl Pts',(7.39123218298962,-30.8131368882363,
53.5458737199049));
#109862=CARTESIAN_POINT('Ctrl Pts',(7.39281935311893,-30.7920466236917,
53.5342606902959));
#109863=CARTESIAN_POINT('Ctrl Pts',(7.39368302601269,-30.7804304172427,
53.5280428136756));
#109864=CARTESIAN_POINT('Ctrl Pts',(7.39663601617687,-30.7402478366114,
53.5071434600193));
#109865=CARTESIAN_POINT('Ctrl Pts',(7.39870152466308,-30.7113303486268,
53.4931500212548));
#109866=CARTESIAN_POINT('Ctrl Pts',(7.40872301150565,-30.5674845587046,
53.4286063155227));
#109867=CARTESIAN_POINT('Ctrl Pts',(7.41626853170064,-30.447504509216,53.390323535924));
#109868=CARTESIAN_POINT('Ctrl Pts',(7.42712522636434,-30.2740500514831,
53.3558944230957));
#109869=CARTESIAN_POINT('Ctrl Pts',(7.43030053923293,-30.2233114199783,
53.3482379541306));
#109870=CARTESIAN_POINT('Ctrl Pts',(7.43481324112559,-30.1527098241845,
53.3408966854821));
#109871=CARTESIAN_POINT('Ctrl Pts',(7.43607791719862,-30.133081537075,53.3392070170325));
#109872=CARTESIAN_POINT('Ctrl Pts',(7.43831679471423,-30.0987175930176,
53.336861922427));
#109873=CARTESIAN_POINT('Ctrl Pts',(7.43928397423673,-30.0839942976495,
53.3360533813809));
#109874=CARTESIAN_POINT('Ctrl Pts',(7.44075105084913,-30.0618818367307,
53.3351332750675));
#109875=CARTESIAN_POINT('Ctrl Pts',(7.4412432940879,-30.0544990499121,53.3348752533596));
#109876=CARTESIAN_POINT('Ctrl Pts',(7.44214056586419,-30.0411133774042,
53.3344965511557));
#109877=CARTESIAN_POINT('Ctrl Pts',(7.44254467559746,-30.0351112299551,
53.3343592085464));
#109878=CARTESIAN_POINT('Ctrl Pts',(7.44346500644764,-30.0215015784999,
53.3341213837841));
#109879=CARTESIAN_POINT('Ctrl Pts',(7.44398226414735,-30.0138940923868,
53.334040567615));
#109880=CARTESIAN_POINT('Ctrl Pts',(7.44558763121654,-29.9904031635162,
53.3339519259724));
#109881=CARTESIAN_POINT('Ctrl Pts',(7.44668454175472,-29.97452048513,53.3341191421271));
#109882=CARTESIAN_POINT('Ctrl Pts',(7.45476353841384,-29.8585905154747,
53.3369978642721));
#109883=CARTESIAN_POINT('Ctrl Pts',(7.46208676688197,-29.7589736460459,
53.3484928754846));
#109884=CARTESIAN_POINT('Ctrl Pts',(7.47213594336692,-29.6237086119743,
53.3766049502253));
#109885=CARTESIAN_POINT('Ctrl Pts',(7.47489892943558,-29.5866931442184,
53.3856319166404));
#109886=CARTESIAN_POINT('Ctrl Pts',(7.48142576930492,-29.499368230722,53.4101285660257));
#109887=CARTESIAN_POINT('Ctrl Pts',(7.48516551511177,-29.4494155830256,
53.4267291953293));
#109888=CARTESIAN_POINT('Ctrl Pts',(7.49132041496104,-29.3671139153554,
53.4584817222655));
#109889=CARTESIAN_POINT('Ctrl Pts',(7.49377163356675,-29.3343168795382,
53.4723581201619));
#109890=CARTESIAN_POINT('Ctrl Pts',(7.49719222671062,-29.2885480472576,
53.4934771184817));
#109891=CARTESIAN_POINT('Ctrl Pts',(7.49819047278937,-29.2751915258093,
53.4998574154764));
#109892=CARTESIAN_POINT('Ctrl Pts',(7.49991061207578,-29.2521835396078,
53.5112271749809));
#109893=CARTESIAN_POINT('Ctrl Pts',(7.50063529771064,-29.2424927577267,
53.5161345173923));
#109894=CARTESIAN_POINT('Ctrl Pts',(7.50202778199032,-29.2238804487528,
53.5257895147222));
#109895=CARTESIAN_POINT('Ctrl Pts',(7.50269599466004,-29.214952793889,53.530524241602));
#109896=CARTESIAN_POINT('Ctrl Pts',(7.50446412777975,-29.1913451926609,
53.5433209423904));
#109897=CARTESIAN_POINT('Ctrl Pts',(7.50555901767156,-29.1767425448151,
53.5515236729096));
#109898=CARTESIAN_POINT('Ctrl Pts',(7.50964843614083,-29.1223032317046,
53.5831930872221));
#109899=CARTESIAN_POINT('Ctrl Pts',(7.51259140897434,-29.083323481546,53.6080954798478));
#109900=CARTESIAN_POINT('Ctrl Pts',(7.52375930369471,-28.9374086499711,
53.7101060285925));
#109901=CARTESIAN_POINT('Ctrl Pts',(7.53160242487166,-28.8387395689174,
53.7981684816556));
#109902=CARTESIAN_POINT('Ctrl Pts',(7.54195581803577,-28.7285328946065,
53.9229073378102));
#109903=CARTESIAN_POINT('Ctrl Pts',(7.54413613941967,-28.706402904693,53.9495889090035));
#109904=CARTESIAN_POINT('Ctrl Pts',(7.54779198220074,-28.671413597476,53.9945585353159));
#109905=CARTESIAN_POINT('Ctrl Pts',(7.54924189184222,-28.6580610589869,
54.0124504419106));
#109906=CARTESIAN_POINT('Ctrl Pts',(7.55128792260117,-28.6400150024705,
54.0376734632412));
#109907=CARTESIAN_POINT('Ctrl Pts',(7.55186477472032,-28.6350127266119,
54.0447820708678));
#109908=CARTESIAN_POINT('Ctrl Pts',(7.5528544247746,-28.6265810741588,54.0569655543058));
#109909=CARTESIAN_POINT('Ctrl Pts',(7.5532653558838,-28.623123558812,54.0620209084459));
#109910=CARTESIAN_POINT('Ctrl Pts',(7.55413120447432,-28.6159311662204,
54.072662618983));
#109911=CARTESIAN_POINT('Ctrl Pts',(7.55458646436,-28.6122021372565,54.0782526143093));
#109912=CARTESIAN_POINT('Ctrl Pts',(7.55582953476184,-28.6021599485698,
54.0935054236412));
#109913=CARTESIAN_POINT('Ctrl Pts',(7.55662146536172,-28.5959133642476,
54.1032113253135));
#109914=CARTESIAN_POINT('Ctrl Pts',(7.5606717483727,-28.5647023001121,54.1528323937191));
#109915=CARTESIAN_POINT('Ctrl Pts',(7.56401414950227,-28.5413390646799,
54.1937247004124));
#109916=CARTESIAN_POINT('Ctrl Pts',(7.57465819325055,-28.4734298242484,
54.3252216886936));
#109917=CARTESIAN_POINT('Ctrl Pts',(7.58207943763155,-28.4353629164446,
54.4189197609928));
#109918=CARTESIAN_POINT('Ctrl Pts',(7.59484869291408,-28.3837010598797,
54.5888822390953));
#109919=CARTESIAN_POINT('Ctrl Pts',(7.60025561399403,-28.3664855423021,
54.6637357930428));
#109920=CARTESIAN_POINT('Ctrl Pts',(7.6067905302043,-28.351538376,54.7581602691291));
#109921=CARTESIAN_POINT('Ctrl Pts',(7.60807070902892,-28.3489044641932,
54.7768503557741));
#109922=CARTESIAN_POINT('Ctrl Pts',(7.61012637510473,-28.3451566054189,
54.8071644565715));
#109923=CARTESIAN_POINT('Ctrl Pts',(7.61090795850382,-28.3438463174616,
54.8187620370786));
#109924=CARTESIAN_POINT('Ctrl Pts',(7.61240455514058,-28.3415596979604,
54.8411034310793));
#109925=CARTESIAN_POINT('Ctrl Pts',(7.61312008857083,-28.3405656386302,
54.8518447953176));
#109926=CARTESIAN_POINT('Ctrl Pts',(7.61476159942384,-28.3385153641405,
54.8766191984961));
#109927=CARTESIAN_POINT('Ctrl Pts',(7.61568524304847,-28.3375324730583,
54.8906576050593));
#109928=CARTESIAN_POINT('Ctrl Pts',(7.61869404810372,-28.3348951746517,
54.9366898681428));
#109929=CARTESIAN_POINT('Ctrl Pts',(7.6207561365832,-28.333985579211,54.9687203240773));
#109930=CARTESIAN_POINT('Ctrl Pts',(7.62567548929244,-28.3340208019506,
55.0460479823162));
#109931=CARTESIAN_POINT('Ctrl Pts',(7.62850641392198,-28.3358881379129,
55.0913195357843));
#109932=CARTESIAN_POINT('Ctrl Pts',(7.63562978463511,-28.3453222475496,
55.2061096476721));
#109933=CARTESIAN_POINT('Ctrl Pts',(7.6398721484824,-28.3554230730368,55.2753300496743));
#109934=CARTESIAN_POINT('Ctrl Pts',(7.64492142645656,-28.372447151158,55.3560720407562));
#109935=CARTESIAN_POINT('Ctrl Pts',(7.64569544833211,-28.3751937864551,
55.3684024129919));
#109936=CARTESIAN_POINT('Ctrl Pts',(7.65064042938412,-28.3935912442189,
55.4467821799943));
#109937=CARTESIAN_POINT('Ctrl Pts',(7.65485612376256,-28.4131232317943,
55.5118416955448));
#109938=CARTESIAN_POINT('Ctrl Pts',(7.65925610934961,-28.4365623095611,
55.5755159321123));
#109939=CARTESIAN_POINT('',(7.4292447960249,-28.334000270279,55.0012652250353));
#109940=CARTESIAN_POINT('Ctrl Pts',(7.4682788092303,-28.4365623654365,55.5755160839024));
#109941=CARTESIAN_POINT('Ctrl Pts',(7.46565398779176,-28.4217405491484,
55.5352513788047));
#109942=CARTESIAN_POINT('Ctrl Pts',(7.46301745838831,-28.4084720557853,
55.4944082845082));
#109943=CARTESIAN_POINT('Ctrl Pts',(7.45745230202699,-28.3842278948838,
55.4086204717661));
#109944=CARTESIAN_POINT('Ctrl Pts',(7.45452079180897,-28.3735200811348,
55.3636652702551));
#109945=CARTESIAN_POINT('Ctrl Pts',(7.45074651845308,-28.3625045631199,
55.3070766733074));
#109946=CARTESIAN_POINT('Ctrl Pts',(7.44999050083058,-28.3604306357742,
55.2958034330771));
#109947=CARTESIAN_POINT('Ctrl Pts',(7.44878251692798,-28.357328900644,55.2779074726101));
#109948=CARTESIAN_POINT('Ctrl Pts',(7.44833470111328,-28.3562244056175,
55.2712981668777));
#109949=CARTESIAN_POINT('Ctrl Pts',(7.44747288453206,-28.3541860165994,
55.2586308246002));
#109950=CARTESIAN_POINT('Ctrl Pts',(7.44705924353949,-28.3532456414348,
55.2525740462948));
#109951=CARTESIAN_POINT('Ctrl Pts',(7.44622485822675,-28.3514243133995,
55.2404004926074));
#109952=CARTESIAN_POINT('Ctrl Pts',(7.44580409338623,-28.3505439254131,
55.2342836876218));
#109953=CARTESIAN_POINT('Ctrl Pts',(7.44479674920522,-28.3485261035645,
55.2196887392727));
#109954=CARTESIAN_POINT('Ctrl Pts',(7.44420859215493,-28.347419908211,55.2112065471316));
#109955=CARTESIAN_POINT('Ctrl Pts',(7.44212394764507,-28.34374975745,55.1812679874869));
#109956=CARTESIAN_POINT('Ctrl Pts',(7.44061142409316,-28.341538091476,55.1597715450636));
#109957=CARTESIAN_POINT('Ctrl Pts',(7.43585344695961,-28.3359513990773,
55.0926753750645));
#109958=CARTESIAN_POINT('Ctrl Pts',(7.4325603205512,-28.334035143807,55.0469779164252));
#109959=CARTESIAN_POINT('Ctrl Pts',(7.42924502128251,-28.3340004789752,
55.001263307162));
#109960=CARTESIAN_POINT('Ctrl Pts',(7.42924515845182,-28.3340004804105,
55.0012651985876));
#109961=CARTESIAN_POINT('Ctrl Pts',(7.41936138148925,-28.3338969807047,
54.8649779297204));
#109962=CARTESIAN_POINT('Ctrl Pts',(7.40938172257902,-28.3505181555921,
54.7291574322246));
#109963=CARTESIAN_POINT('Ctrl Pts',(7.39771731316611,-28.3911434361544,
54.5662587165018));
#109964=CARTESIAN_POINT('Ctrl Pts',(7.39555203419563,-28.3996441494935,
54.5358746621357));
#109965=CARTESIAN_POINT('Ctrl Pts',(7.39245620643845,-28.4131976353831,
54.4922459575998));
#109966=CARTESIAN_POINT('Ctrl Pts',(7.39150372512375,-28.4175640806743,
54.4787970696937));
#109967=CARTESIAN_POINT('Ctrl Pts',(7.38983637728091,-28.4255536596276,
54.455215205413));
#109968=CARTESIAN_POINT('Ctrl Pts',(7.3891191905053,-28.4291046840929,54.4450588617478));
#109969=CARTESIAN_POINT('Ctrl Pts',(7.38762591951027,-28.4367372116957,
54.4238894383361));
#109970=CARTESIAN_POINT('Ctrl Pts',(7.38685049739493,-28.4408372981033,
54.4128836525272));
#109971=CARTESIAN_POINT('Ctrl Pts',(7.38481545440832,-28.4519566996848,
54.3839742601459));
#109972=CARTESIAN_POINT('Ctrl Pts',(7.38356236486527,-28.4591703266196,
54.3661469103846));
#109973=CARTESIAN_POINT('Ctrl Pts',(7.37750134567894,-28.495828037269,54.2798796988732));
#109974=CARTESIAN_POINT('Ctrl Pts',(7.37283976866374,-28.529533271925,54.2133386246886));
#109975=CARTESIAN_POINT('Ctrl Pts',(7.36163441330213,-28.6223908901131,
54.056989494922));
#109976=CARTESIAN_POINT('Ctrl Pts',(7.35519978860848,-28.68598340088,53.9702264620119));
#109977=CARTESIAN_POINT('Ctrl Pts',(7.34664978927114,-28.7769532270693,
53.8683783022279));
#109978=CARTESIAN_POINT('Ctrl Pts',(7.34479829125985,-28.7970024065456,
53.8470873104637));
#109979=CARTESIAN_POINT('Ctrl Pts',(7.34166019357542,-28.8313208588417,
53.8125134149638));
#109980=CARTESIAN_POINT('Ctrl Pts',(7.34039162646372,-28.8452821164815,
53.7989330349147));
#109981=CARTESIAN_POINT('Ctrl Pts',(7.33858418817246,-28.8652345270069,
53.7801944012327));
#109982=CARTESIAN_POINT('Ctrl Pts',(7.33805984107423,-28.871029812833,53.774828710835));
#109983=CARTESIAN_POINT('Ctrl Pts',(7.33752872251798,-28.8769039574688,
53.7694670738485));
#109984=CARTESIAN_POINT('Ctrl Pts',(7.33752500883319,-28.8769450308333,
53.7694295878243));
#109985=CARTESIAN_POINT('Ctrl Pts',(7.33751750847075,-28.8770279852585,
53.7693538862362));
#109986=CARTESIAN_POINT('Ctrl Pts',(7.33751372179506,-28.8770698663054,
53.7693156708339));
#109987=CARTESIAN_POINT('Ctrl Pts',(7.33750607161743,-28.8771544785145,
53.7692384722354));
#109988=CARTESIAN_POINT('Ctrl Pts',(7.3375022081073,-28.8771972097754,53.769199489109));
#109989=CARTESIAN_POINT('Ctrl Pts',(7.33749440017999,-28.87728356757,53.7691207143516));
#109990=CARTESIAN_POINT('Ctrl Pts',(7.33749045577606,-28.8773271939658,
53.7690809230181));
#109991=CARTESIAN_POINT('Ctrl Pts',(7.33748248175057,-28.8774153897306,
53.7690004888609));
#109992=CARTESIAN_POINT('Ctrl Pts',(7.33747845210965,-28.8774599593233,
53.7689598460181));
#109993=CARTESIAN_POINT('Ctrl Pts',(7.33747030301537,-28.8775500923283,
53.768877663037));
#109994=CARTESIAN_POINT('Ctrl Pts',(7.33746618354772,-28.8775956559089,
53.7688361229442));
#109995=CARTESIAN_POINT('Ctrl Pts',(7.33745784989176,-28.8776878312054,
53.7687520965486));
#109996=CARTESIAN_POINT('Ctrl Pts',(7.3374536356941,-28.8777344430355,53.7687096103563));
#109997=CARTESIAN_POINT('Ctrl Pts',(7.33744510734816,-28.8778287727079,
53.7686236396594));
#109998=CARTESIAN_POINT('Ctrl Pts',(7.33744079318678,-28.8778764907065,
53.7685801552441));
#109999=CARTESIAN_POINT('Ctrl Pts',(7.33743205931893,-28.877973094627,53.7684921323871));
#110000=CARTESIAN_POINT('Ctrl Pts',(7.33742763961158,-28.8780219805711,
53.7684475941756));
#110001=CARTESIAN_POINT('Ctrl Pts',(7.33741868867015,-28.8781209865791,
53.7683574041785));
#110002=CARTESIAN_POINT('Ctrl Pts',(7.33741415743625,-28.8781711066546,
53.7683117526535));
#110003=CARTESIAN_POINT('Ctrl Pts',(7.33740497705346,-28.8782726516231,
53.7682192724593));
#110004=CARTESIAN_POINT('Ctrl Pts',(7.33740032788345,-28.8783240767642,
53.7681724438581));
#110005=CARTESIAN_POINT('Ctrl Pts',(7.33739090476232,-28.8784283078511,
53.7680775412106));
#110006=CARTESIAN_POINT('Ctrl Pts',(7.33738613079863,-28.8784811139514,
53.7680294673427));
#110007=CARTESIAN_POINT('Ctrl Pts',(7.33737645071386,-28.8785881885908,
53.7679320008146));
#110008=CARTESIAN_POINT('Ctrl Pts',(7.33737154457397,-28.8786424573547,
53.7678826082969));
#110009=CARTESIAN_POINT('Ctrl Pts',(7.33736159219885,-28.8787525451723,
53.7677824255685));
#110010=CARTESIAN_POINT('Ctrl Pts',(7.33735654594842,-28.8788083644123,
53.7677316355665));
#110011=CARTESIAN_POINT('Ctrl Pts',(7.337346304797,-28.8789216478662,53.7676285728679));
#110012=CARTESIAN_POINT('Ctrl Pts',(7.33734110988152,-28.87897911226,53.7675763004205));
#110013=CARTESIAN_POINT('Ctrl Pts',(7.33733056216958,-28.8790957881795,
53.7674701811605));
#110014=CARTESIAN_POINT('Ctrl Pts',(7.33732520935568,-28.8791549999193,
53.7674163346046));
#110015=CARTESIAN_POINT('Ctrl Pts',(7.33731433586652,-28.8792752809908,
53.7673069680517));
#110016=CARTESIAN_POINT('Ctrl Pts',(7.33730881517404,-28.8793363505361,
53.7672514483553));
#110017=CARTESIAN_POINT('Ctrl Pts',(7.3372975951219,-28.8794604668154,53.7671386283006));
#110018=CARTESIAN_POINT('Ctrl Pts',(7.33729189573896,-28.8795235138322,
53.7670813282284));
#110019=CARTESIAN_POINT('Ctrl Pts',(7.33728030657738,-28.879651714866,53.7669648310991));
#110020=CARTESIAN_POINT('Ctrl Pts',(7.33727441677917,-28.8797168691269,
53.7669056344178));
#110021=CARTESIAN_POINT('Ctrl Pts',(7.33726243404441,-28.8798494256865,
53.7667852177515));
#110022=CARTESIAN_POINT('Ctrl Pts',(7.33725634107848,-28.8799168283404,
53.7667239981026));
#110023=CARTESIAN_POINT('Ctrl Pts',(7.33724393813633,-28.880054035225,53.7665993980568));
#110024=CARTESIAN_POINT('Ctrl Pts',(7.3372376281186,-28.8801238399478,53.7665360179411));
#110025=CARTESIAN_POINT('Ctrl Pts',(7.33722477591552,-28.8802660187392,
53.7664069468568));
#110026=CARTESIAN_POINT('Ctrl Pts',(7.33721823370589,-28.8803383931125,
53.7663412564184));
#110027=CARTESIAN_POINT('Ctrl Pts',(7.33720490055903,-28.8804858945012,
53.7662074007842));
#110028=CARTESIAN_POINT('Ctrl Pts',(7.33719810957887,-28.8805610220313,
53.7661392360177));
#110029=CARTESIAN_POINT('Ctrl Pts',(7.33718426073402,-28.8807142307094,
53.7660002521169));
#110030=CARTESIAN_POINT('Ctrl Pts',(7.33717720283863,-28.8807923122409,
53.7659294336332));
#110031=CARTESIAN_POINT('Ctrl Pts',(7.3371628002295,-28.8809516495688,53.7657849452276));
#110032=CARTESIAN_POINT('Ctrl Pts',(7.33715545546863,-28.881032905935,53.7657112759044));
#110033=CARTESIAN_POINT('Ctrl Pts',(7.33714045718768,-28.8811988357995,
53.7655608690414));
#110034=CARTESIAN_POINT('Ctrl Pts',(7.33713280360971,-28.8812835099917,
53.7654841321223));
#110035=CARTESIAN_POINT('Ctrl Pts',(7.33711716346841,-28.8814565436755,
53.7653273508625));
#110036=CARTESIAN_POINT('Ctrl Pts',(7.33710917684828,-28.8815449038548,
53.7652473073035));
#110037=CARTESIAN_POINT('Ctrl Pts',(7.33709284381398,-28.8817256062719,
53.7650836482374));
#110038=CARTESIAN_POINT('Ctrl Pts',(7.33708449734189,-28.8818179492163,
53.7650000336746));
#110039=CARTESIAN_POINT('Ctrl Pts',(7.33706741487229,-28.882006946281,53.7648289394457));
#110040=CARTESIAN_POINT('Ctrl Pts',(7.33705867879913,-28.8821036013116,
53.7647414607483));
#110041=CARTESIAN_POINT('Ctrl Pts',(7.33704078404828,-28.8823015887304,
53.7645623123294));
#110042=CARTESIAN_POINT('Ctrl Pts',(7.33703162528436,-28.8824029221547,
53.7644706437065));
#110043=CARTESIAN_POINT('Ctrl Pts',(7.33661966045941,-28.886960980076,53.760348335792));
#110044=CARTESIAN_POINT('Ctrl Pts',(7.33621503627641,-28.8914392347911,
53.7563420347391));
#110045=CARTESIAN_POINT('Ctrl Pts',(7.33528351882049,-28.9017524608487,
53.7472156598144));
#110046=CARTESIAN_POINT('Ctrl Pts',(7.33475547267559,-28.9076015956614,
53.742112095438));
#110047=CARTESIAN_POINT('Ctrl Pts',(7.33312165043831,-28.9257146258615,
53.7265294865155));
#110048=CARTESIAN_POINT('Ctrl Pts',(7.33200686745723,-28.9380948134998,
53.7161878872425));
#110049=CARTESIAN_POINT('Ctrl Pts',(7.32522949568416,-29.0135973813667,
53.6549572758446));
#110050=CARTESIAN_POINT('Ctrl Pts',(7.31934378950463,-29.0802105747121,
53.6085565082187));
#110051=CARTESIAN_POINT('Ctrl Pts',(7.30807746792457,-29.2133365480952,
53.5295740986431));
#110052=CARTESIAN_POINT('Ctrl Pts',(7.30271120111838,-29.2791754050481,
53.4962031596171));
#110053=CARTESIAN_POINT('Ctrl Pts',(7.29441927823271,-29.3860771915527,
53.4506588836747));
#110054=CARTESIAN_POINT('Ctrl Pts',(7.29142556736562,-29.4257671184623,
53.4355140754363));
#110055=CARTESIAN_POINT('Ctrl Pts',(7.28635590441309,-29.4949589952015,
53.412100590152));
#110056=CARTESIAN_POINT('Ctrl Pts',(7.28425850738909,-29.5241885382703,
53.4030984318918));
#110057=CARTESIAN_POINT('Ctrl Pts',(7.28124054464323,-29.5671128843571,
53.3911619162331));
#110058=CARTESIAN_POINT('Ctrl Pts',(7.28029956371222,-29.5806216193866,
53.3875878227953));
#110059=CARTESIAN_POINT('Ctrl Pts',(7.27864523099934,-29.6045874622423,
53.3815685977633));
#110060=CARTESIAN_POINT('Ctrl Pts',(7.27792967634378,-29.6150260817573,
53.3790538656968));
#110061=CARTESIAN_POINT('Ctrl Pts',(7.2764328922464,-29.6370099740115,53.373982149372));
#110062=CARTESIAN_POINT('Ctrl Pts',(7.27565239128449,-29.64855966445,53.3714468039974));
#110063=CARTESIAN_POINT('Ctrl Pts',(7.27358797160599,-29.6793290370596,
53.3650350104078));
#110064=CARTESIAN_POINT('Ctrl Pts',(7.27231093861435,-29.6985921782093,
53.3613744292037));
#110065=CARTESIAN_POINT('Ctrl Pts',(7.26570090209875,-29.7993981666942,
53.3440561045228));
#110066=CARTESIAN_POINT('Ctrl Pts',(7.26055175831115,-29.8818143795768,
53.3361412514622));
#110067=CARTESIAN_POINT('Ctrl Pts',(7.24932622292816,-30.0645502504756,
53.3322450467618));
#110068=CARTESIAN_POINT('Ctrl Pts',(7.24330777673946,-30.1645960286204,
53.3391330199052));
#110069=CARTESIAN_POINT('Ctrl Pts',(7.23526176216511,-30.2913214536345,
53.3594248829007));
#110070=CARTESIAN_POINT('Ctrl Pts',(7.23346986520759,-30.3191110235992,
53.3646031433493));
#110071=CARTESIAN_POINT('Ctrl Pts',(7.2304039155781,-30.3656265500736,53.3745014502709));
#110072=CARTESIAN_POINT('Ctrl Pts',(7.22914617000949,-30.3844271259328,
53.3788448512516));
#110073=CARTESIAN_POINT('Ctrl Pts',(7.22732855753112,-30.4111167666871,
53.3855011701696));
#110074=CARTESIAN_POINT('Ctrl Pts',(7.22678272860742,-30.4190714886125,
53.3875476602974));
#110075=CARTESIAN_POINT('Ctrl Pts',(7.22582891152124,-30.4328605496481,
53.3912040609785));
#110076=CARTESIAN_POINT('Ctrl Pts',(7.22542245169999,-30.4387017762115,
53.3927870772486));
#110077=CARTESIAN_POINT('Ctrl Pts',(7.22454526481024,-30.451230976305,53.3962559782332));
#110078=CARTESIAN_POINT('Ctrl Pts',(7.22407401180635,-30.4579157150116,
53.3981518564881));
#110079=CARTESIAN_POINT('Ctrl Pts',(7.22276390505091,-30.4763773340345,
53.4035128131894));
#110080=CARTESIAN_POINT('Ctrl Pts',(7.22192030452483,-30.4881277979946,
53.4070662497296));
#110081=CARTESIAN_POINT('Ctrl Pts',(7.21598093992014,-30.56997618762,53.4328084987455));
#110082=CARTESIAN_POINT('Ctrl Pts',(7.21068115500295,-30.6385701759523,
53.4594845699778));
#110083=CARTESIAN_POINT('Ctrl Pts',(7.20433076996824,-30.7177599366058,
53.4964808702952));
#110084=CARTESIAN_POINT('Ctrl Pts',(7.20331979855189,-30.7302756521869,
53.5025199272583));
#110085=CARTESIAN_POINT('Ctrl Pts',(7.19694229428744,-30.8087096757976,
53.5415829254223));
#110086=CARTESIAN_POINT('Ctrl Pts',(7.19157603405899,-30.8724546306259,
53.5787977144274));
#110087=CARTESIAN_POINT('Ctrl Pts',(7.18328409547715,-30.9686982658194,
53.6439089987239));
#110088=CARTESIAN_POINT('Ctrl Pts',(7.18029036352442,-31.0029487190825,
53.6690403831172));
#110089=CARTESIAN_POINT('Ctrl Pts',(7.17522066924653,-31.0601469590131,
53.7144731092484));
#110090=CARTESIAN_POINT('Ctrl Pts',(7.17312326162279,-31.0835632395142,
53.734147765123));
#110091=CARTESIAN_POINT('Ctrl Pts',(7.17010528669471,-31.1168723862871,
53.7637365539046));
#110092=CARTESIAN_POINT('Ctrl Pts',(7.16916430394805,-31.127201811013,53.7731473872925));
#110093=CARTESIAN_POINT('Ctrl Pts',(7.1675099691897,-31.1452570596212,53.790017543011));
#110094=CARTESIAN_POINT('Ctrl Pts',(7.16679441428582,-31.1530313308955,
53.7974235832662));
#110095=CARTESIAN_POINT('Ctrl Pts',(7.16529763078826,-31.1692155684582,
53.8131424838291));
#110096=CARTESIAN_POINT('Ctrl Pts',(7.16451713066375,-31.1776097512204,
53.8214707915453));
#110097=CARTESIAN_POINT('Ctrl Pts',(7.16245271582189,-31.1996847304443,
53.8438438994774));
#110098=CARTESIAN_POINT('Ctrl Pts',(7.16117568677052,-31.213207739598,53.8580422886749));
#110099=CARTESIAN_POINT('Ctrl Pts',(7.15456578763205,-31.2824297370214,
53.9333393664157));
#110100=CARTESIAN_POINT('Ctrl Pts',(7.14941676711014,-31.3337777872687,
53.9982863447298));
#110101=CARTESIAN_POINT('Ctrl Pts',(7.13819124008231,-31.4361609777227,
54.1496969210285));
#110102=CARTESIAN_POINT('Ctrl Pts',(7.13217269008688,-31.4846364094691,
54.23748700274));
#110103=CARTESIAN_POINT('Ctrl Pts',(7.12412655065735,-31.5363205511849,
54.3549619537736));
#110104=CARTESIAN_POINT('Ctrl Pts',(7.12233463978635,-31.5470422331034,
54.3811178900663));
#110105=CARTESIAN_POINT('Ctrl Pts',(7.11926866875335,-31.5639547193652,
54.4255664099045));
#110106=CARTESIAN_POINT('Ctrl Pts',(7.1180109159911,-31.5705024379246,54.4437174024808));
#110107=CARTESIAN_POINT('Ctrl Pts',(7.1161932949173,-31.5793857218873,54.4697508046372));
#110108=CARTESIAN_POINT('Ctrl Pts',(7.11564746477252,-31.5819807383557,
54.477543873458));
#110109=CARTESIAN_POINT('Ctrl Pts',(7.11469364631046,-31.5863875356006,
54.4911117845995));
#110110=CARTESIAN_POINT('Ctrl Pts',(7.11428718634815,-31.5882256471835,
54.496877826798));
#110111=CARTESIAN_POINT('Ctrl Pts',(7.1134100000558,-31.5921066586156,54.5092855527162));
#110112=CARTESIAN_POINT('Ctrl Pts',(7.11293874779902,-31.594139408157,54.5159299388113));
#110113=CARTESIAN_POINT('Ctrl Pts',(7.11162864509591,-31.5996483385049,
54.5343478830958));
#110114=CARTESIAN_POINT('Ctrl Pts',(7.11078504792078,-31.603035959432,54.546147169756));
#110115=CARTESIAN_POINT('Ctrl Pts',(7.10484659272836,-31.6257969310291,
54.6288605765015));
#110116=CARTESIAN_POINT('Ctrl Pts',(7.09954778605901,-31.6405863392822,
54.7009444858452));
#110117=CARTESIAN_POINT('Ctrl Pts',(7.09319763078049,-31.6524554706508,
54.7875375335864));
#110118=CARTESIAN_POINT('Ctrl Pts',(7.09218592180018,-31.6541713232472,
54.8013379454803));
#110119=CARTESIAN_POINT('Ctrl Pts',(7.08580773362252,-31.6638941094912,
54.8884294529822));
#110120=CARTESIAN_POINT('Ctrl Pts',(7.08044152169657,-31.66720173276,54.9621675725987));
#110121=CARTESIAN_POINT('Ctrl Pts',(7.07214946850077,-31.6646987504846,
55.0783414519699));
#110122=CARTESIAN_POINT('Ctrl Pts',(7.06915558233061,-31.6621610745342,
55.120749228861));
#110123=CARTESIAN_POINT('Ctrl Pts',(7.06408565893557,-31.6550132327113,
55.1934482581732));
#110124=CARTESIAN_POINT('Ctrl Pts',(7.06198817377946,-31.6511837676141,
55.2237932252094));
#110125=CARTESIAN_POINT('Ctrl Pts',(7.05897010973319,-31.6443904664943,
55.2678268740775));
#110126=CARTESIAN_POINT('Ctrl Pts',(7.05802911369633,-31.6420863034479,
55.2816093632342));
#110127=CARTESIAN_POINT('Ctrl Pts',(7.05637476395455,-31.6377054454607,
55.305928346623));
#110128=CARTESIAN_POINT('Ctrl Pts',(7.05565920722219,-31.6356997955474,
55.3164766460311));
#110129=CARTESIAN_POINT('Ctrl Pts',(7.05416242808172,-31.6312714381596,
55.3385990283326));
#110130=CARTESIAN_POINT('Ctrl Pts',(7.05338193406396,-31.6288271946948,
55.350168229426));
#110131=CARTESIAN_POINT('Ctrl Pts',(7.05131755453722,-31.6220033896862,
55.3808482208801));
#110132=CARTESIAN_POINT('Ctrl Pts',(7.05004055426368,-31.6174092267133,
55.3999097516673));
#110133=CARTESIAN_POINT('Ctrl Pts',(7.04343165782151,-31.5916964694584,
55.4988895514643));
#110134=CARTESIAN_POINT('Ctrl Pts',(7.03828353698695,-31.5649871134795,
55.577240213801));
#110135=CARTESIAN_POINT('Ctrl Pts',(7.02705807103857,-31.4933150681704,
55.7453766986767));
#110136=CARTESIAN_POINT('Ctrl Pts',(7.02103876349687,-31.4458453571029,
55.8337296792155));
#110137=CARTESIAN_POINT('Ctrl Pts',(7.01299171293547,-31.3751735386733,
55.9408787114126));
#110138=CARTESIAN_POINT('Ctrl Pts',(7.01119970053903,-31.3590129854394,
55.9640739268158));
#110139=CARTESIAN_POINT('Ctrl Pts',(7.00813357332449,-31.3308411804608,
56.0023921876658));
#110140=CARTESIAN_POINT('Ctrl Pts',(7.00687576806807,-31.3191425089811,
56.0177383301558));
#110141=CARTESIAN_POINT('Ctrl Pts',(7.00505808426361,-31.3020881047485,
56.039321912314));
#110142=CARTESIAN_POINT('Ctrl Pts',(7.00451224520122,-31.2969481690766,
56.0457288891856));
#110143=CARTESIAN_POINT('Ctrl Pts',(7.0035584166858,-31.2879391709183,56.0567901026722));
#110144=CARTESIAN_POINT('Ctrl Pts',(7.00315195568784,-31.2840917841132,
56.0614616892386));
#110145=CARTESIAN_POINT('Ctrl Pts',(7.00227477374129,-31.2757724766153,
56.0714517572007));
#110146=CARTESIAN_POINT('Ctrl Pts',(7.0018035269298,-31.2712927812697,56.0767631772989));
#110147=CARTESIAN_POINT('Ctrl Pts',(7.00049345376872,-31.2588071940219,
56.0913803830859));
#110148=CARTESIAN_POINT('Ctrl Pts',(6.99964988102214,-31.2507316598614,
56.1006257244048));
#110149=CARTESIAN_POINT('Ctrl Pts',(6.99371803261137,-31.1936488650788,
56.1645379154008));
#110150=CARTESIAN_POINT('Ctrl Pts',(6.98842633237386,-31.1411817993022,
56.2159966617393));
#110151=CARTESIAN_POINT('Ctrl Pts',(6.9820778981905,-31.0748950826226,56.2729304692034));
#110152=CARTESIAN_POINT('Ctrl Pts',(6.98106088278504,-31.0641763347269,
56.2819048884559));
#110153=CARTESIAN_POINT('Ctrl Pts',(6.97467780430104,-30.9962303623445,
56.337354036096));
#110154=CARTESIAN_POINT('Ctrl Pts',(6.96931196817566,-30.9360803177665,
56.3801252501119));
#110155=CARTESIAN_POINT('Ctrl Pts',(6.96101906000775,-30.837114462397,56.4410413047622));
#110156=CARTESIAN_POINT('Ctrl Pts',(6.95802400918304,-30.8000963776383,
56.4619189283905));
#110157=CARTESIAN_POINT('Ctrl Pts',(6.95295235555819,-30.7351211980397,
56.4953555974874));
#110158=CARTESIAN_POINT('Ctrl Pts',(6.9508542849393,-30.7075427826604,56.5086003323156));
#110159=CARTESIAN_POINT('Ctrl Pts',(6.94783554795873,-30.6668549486714,
56.526779538368));
#110160=CARTESIAN_POINT('Ctrl Pts',(6.94689445157823,-30.6540246834458,
56.5323194887012));
#110161=CARTESIAN_POINT('Ctrl Pts',(6.94523998870642,-30.6312157588782,
56.5418294163343));
#110162=CARTESIAN_POINT('Ctrl Pts',(6.94452441816591,-30.6212657269899,
56.5458655145503));
#110163=CARTESIAN_POINT('Ctrl Pts',(6.94302767190505,-30.6002785059707,
56.5541433347846));
#110164=CARTESIAN_POINT('Ctrl Pts',(6.94224722398002,-30.5892337447838,
56.5583643335002));
#110165=CARTESIAN_POINT('Ctrl Pts',(6.94018311099836,-30.5597611035498,
56.5692698100086));
#110166=CARTESIAN_POINT('Ctrl Pts',(6.93890632792845,-30.5412582511765,
56.5757473743571));
#110167=CARTESIAN_POINT('Ctrl Pts',(6.93230494682998,-30.4442666385814,
56.6077925404246));
#110168=CARTESIAN_POINT('Ctrl Pts',(6.92716356843504,-30.3640674084027,
56.6278289554652));
#110169=CARTESIAN_POINT('Ctrl Pts',(6.91593855588035,-30.1839574699845,
56.6588416857747));
#110170=CARTESIAN_POINT('Ctrl Pts',(6.90991356842101,-30.0838844468811,
56.6669004604288));
#110171=CARTESIAN_POINT('Ctrl Pts',(6.90185968682402,-29.9554228063539,
56.6656435960921));
#110172=CARTESIAN_POINT('Ctrl Pts',(6.90006691377061,-29.9271581116038,
56.6646469879206));
#110173=CARTESIAN_POINT('Ctrl Pts',(6.89699961643601,-29.8796672484711,
56.6617606966871));
#110174=CARTESIAN_POINT('Ctrl Pts',(6.89574141791898,-29.8604231664034,
56.6602550447939));
#110175=CARTESIAN_POINT('Ctrl Pts',(6.893923264176,-29.8330329714778,56.6576324979482));
#110176=CARTESIAN_POINT('Ctrl Pts',(6.89337735831805,-29.8248614467759,
56.6567890532728));
#110177=CARTESIAN_POINT('Ctrl Pts',(6.89242345449698,-29.8106811254468,
56.6552193191231));
#110178=CARTESIAN_POINT('Ctrl Pts',(6.89201698573904,-29.8046695069703,
56.6545206640629));
#110179=CARTESIAN_POINT('Ctrl Pts',(6.89113983633043,-29.7917647688217,
56.6529495940533));
#110180=CARTESIAN_POINT('Ctrl Pts',(6.89066863029436,-29.7848733638788,
56.6520668261346));
#110181=CARTESIAN_POINT('Ctrl Pts',(6.88935877833707,-29.7658242328667,
56.6495054829733));
#110182=CARTESIAN_POINT('Ctrl Pts',(6.8885153885033,-29.7536795098386,56.6477356651802));
#110183=CARTESIAN_POINT('Ctrl Pts',(6.88262968131166,-29.6696823628383,
56.6345456383852));
#110184=CARTESIAN_POINT('Ctrl Pts',(6.87738758094027,-29.5986329456008,
56.6185645888189));
#110185=CARTESIAN_POINT('Ctrl Pts',(6.87109323771207,-29.5155217465157,
56.5940609490431));
#110186=CARTESIAN_POINT('Ctrl Pts',(6.87008135385466,-29.5022294248012,
56.5899603573803));
#110187=CARTESIAN_POINT('Ctrl Pts',(6.86359737181203,-29.417433719875,56.5626338673675));
#110188=CARTESIAN_POINT('Ctrl Pts',(6.8581243384229,-29.3475156755454,56.5347552509911));
#110189=CARTESIAN_POINT('Ctrl Pts',(6.84975951773613,-29.2417769087201,
56.4840566258741));
#110190=CARTESIAN_POINT('Ctrl Pts',(6.84679417373141,-29.2045376312284,
56.4644338269463));
#110191=CARTESIAN_POINT('Ctrl Pts',(6.84176669003119,-29.1417630897022,
56.4282534635349));
#110192=CARTESIAN_POINT('Ctrl Pts',(6.83968358690166,-29.1158658286087,
56.4123687642179));
#110193=CARTESIAN_POINT('Ctrl Pts',(6.83668206118834,-29.0787392707339,
56.3881746689807));
#110194=CARTESIAN_POINT('Ctrl Pts',(6.83574353649287,-29.067158334824,56.3804190273599));
#110195=CARTESIAN_POINT('Ctrl Pts',(6.83409197048213,-29.0468340601644,
56.3664354626472));
#110196=CARTESIAN_POINT('Ctrl Pts',(6.83337675129373,-29.0380511629309,
56.3602667483142));
#110197=CARTESIAN_POINT('Ctrl Pts',(6.8318791493878,-29.0197038989824,56.3471138734307));
#110198=CARTESIAN_POINT('Ctrl Pts',(6.83109750980437,-29.0101531239621,
56.3401117146883));
#110199=CARTESIAN_POINT('Ctrl Pts',(6.82902650575648,-28.9849231178045,
56.3211974193374));
#110200=CARTESIAN_POINT('Ctrl Pts',(6.82774410746935,-28.9693787338623,
56.3091079240124));
#110201=CARTESIAN_POINT('Ctrl Pts',(6.82091060019877,-28.8870638654833,
56.2427131643128));
#110202=CARTESIAN_POINT('Ctrl Pts',(6.81556041461678,-28.8243591234056,
56.1835683743095));
#110203=CARTESIAN_POINT('Ctrl Pts',(6.80431813359718,-28.701179341995,56.0478857039811));
#110204=CARTESIAN_POINT('Ctrl Pts',(6.7984671325709,-28.6422840575745,55.9703631854246));
#110205=CARTESIAN_POINT('Ctrl Pts',(6.79062285321755,-28.5756154868537,
55.8645592129393));
#110206=CARTESIAN_POINT('Ctrl Pts',(6.78885383372478,-28.5613426363736,
55.8405942480984));
#110207=CARTESIAN_POINT('Ctrl Pts',(6.78582310593807,-28.5383161095083,
55.7996257584288));
#110208=CARTESIAN_POINT('Ctrl Pts',(6.78457722123195,-28.529241178391,55.7828087647592));
#110209=CARTESIAN_POINT('Ctrl Pts',(6.78277378782216,-28.5166964885727,
55.7585734302852));
#110210=CARTESIAN_POINT('Ctrl Pts',(6.78222998064803,-28.5129886970933,
55.7512791320508));
#110211=CARTESIAN_POINT('Ctrl Pts',(6.78127843890094,-28.5066339902723,
55.7385462362477));
#110212=CARTESIAN_POINT('Ctrl Pts',(6.78087220996819,-28.5039627157606,
55.7331200617019));
#110213=CARTESIAN_POINT('Ctrl Pts',(6.77999402036308,-28.4982781918607,
55.721412601067));
#110214=CARTESIAN_POINT('Ctrl Pts',(6.77952151916618,-28.4952748191201,
55.7151270206129));
#110215=CARTESIAN_POINT('Ctrl Pts',(6.77820463502334,-28.4870539875925,
55.6976410499048));
#110216=CARTESIAN_POINT('Ctrl Pts',(6.77735542890128,-28.4819217021689,
55.6864014351012));
#110217=CARTESIAN_POINT('Ctrl Pts',(6.77401860377976,-28.4623913119626,
55.6423395637711));
#110218=CARTESIAN_POINT('Ctrl Pts',(6.77148681170204,-28.4489342213664,
55.6091252718719));
#110219=CARTESIAN_POINT('Ctrl Pts',(6.76892552105682,-28.4365623357949,
55.5755160033788));
#110220=CARTESIAN_POINT('Origin',(5.,-30.,55.));
#110221=CARTESIAN_POINT('',(6.06643884243078,-28.4365623175998,55.5755159539501));
#110222=CARTESIAN_POINT('',(6.26189393505974,-28.4365622331338,55.5755157244911));
#110223=CARTESIAN_POINT('',(5.,-28.4365623102018,55.5755159338528));
#110224=CARTESIAN_POINT('',(6.92208048413035,-28.3340006487619,54.9985297366875));
#110225=CARTESIAN_POINT('Ctrl Pts',(6.26189393505974,-28.4365622331338,
55.5755157244911));
#110226=CARTESIAN_POINT('Ctrl Pts',(6.26454443424848,-28.4494994604332,
55.6106608107115));
#110227=CARTESIAN_POINT('Ctrl Pts',(6.26716430935981,-28.4636250038082,
55.6453785126745));
#110228=CARTESIAN_POINT('Ctrl Pts',(6.27128111558779,-28.4879917747115,
55.6999155997547));
#110229=CARTESIAN_POINT('Ctrl Pts',(6.27280063026977,-28.4974711607094,
55.7200402001679));
#110230=CARTESIAN_POINT('Ctrl Pts',(6.27523275603405,-28.5134292830489,
55.7522305318072));
#110231=CARTESIAN_POINT('Ctrl Pts',(6.27615382522183,-28.5196584349094,
55.764416208322));
#110232=CARTESIAN_POINT('Ctrl Pts',(6.27778607461691,-28.5310271577228,
55.7859958028606));
#110233=CARTESIAN_POINT('Ctrl Pts',(6.27849925380626,-28.5361084051871,
55.7954193996187));
#110234=CARTESIAN_POINT('Ctrl Pts',(6.28000404443252,-28.5470699735413,
55.8152876705199));
#110235=CARTESIAN_POINT('Ctrl Pts',(6.28079480055977,-28.5529729035312,
55.8257192272144));
#110236=CARTESIAN_POINT('Ctrl Pts',(6.28291777598941,-28.5692026238206,
55.8536914811434));
#110237=CARTESIAN_POINT('Ctrl Pts',(6.28424238439093,-28.579739333538,55.8711084746527));
#110238=CARTESIAN_POINT('Ctrl Pts',(6.2930977839093,-28.6528863625755,55.9871623009155));
#110239=CARTESIAN_POINT('Ctrl Pts',(6.30023264072672,-28.7254041138658,
56.0791729420103));
#110240=CARTESIAN_POINT('Ctrl Pts',(6.31334404471934,-28.8752744103748,
56.2329344202666));
#110241=CARTESIAN_POINT('Ctrl Pts',(6.31930588883164,-28.9496223452665,
56.2968564631899));
#110242=CARTESIAN_POINT('Ctrl Pts',(6.32668321439504,-29.042062018077,56.3631448104139));
#110243=CARTESIAN_POINT('Ctrl Pts',(6.32772463441115,-29.055118261451,56.372227170059));
#110244=CARTESIAN_POINT('Ctrl Pts',(6.32928196947959,-29.0746123058996,
56.3853777672779));
#110245=CARTESIAN_POINT('Ctrl Pts',(6.32978877346842,-29.0809516278452,
56.3895913163429));
#110246=CARTESIAN_POINT('Ctrl Pts',(6.33070050964634,-29.092342411459,56.397050375253));
#110247=CARTESIAN_POINT('Ctrl Pts',(6.33110435486264,-29.0973828549652,
56.4003122280136));
#110248=CARTESIAN_POINT('Ctrl Pts',(6.33200895785928,-29.1086614883493,
56.407524840982));
#110249=CARTESIAN_POINT('Ctrl Pts',(6.33251058288281,-29.1149083016265,
56.411461370558));
#110250=CARTESIAN_POINT('Ctrl Pts',(6.33402027839573,-29.133692528476,56.4231248213934));
#110251=CARTESIAN_POINT('Ctrl Pts',(6.33503575608031,-29.1463060664516,
56.4307269212504));
#110252=CARTESIAN_POINT('Ctrl Pts',(6.33742713232091,-29.175996661458,56.4480888577481));
#110253=CARTESIAN_POINT('Ctrl Pts',(6.33880943404792,-29.1931488681659,
56.4577153429514));
#110254=CARTESIAN_POINT('Ctrl Pts',(6.34382787724757,-29.2555105829052,
56.4912773495486));
#110255=CARTESIAN_POINT('Ctrl Pts',(6.34752600754672,-29.3016444755732,
56.5134303915248));
#110256=CARTESIAN_POINT('Ctrl Pts',(6.36032778263557,-29.4637873504093,
56.5822959968397));
#110257=CARTESIAN_POINT('Ctrl Pts',(6.36944877284455,-29.5840091139911,
56.6180684694178));
#110258=CARTESIAN_POINT('Ctrl Pts',(6.38042265245481,-29.7392029462727,
56.6457835440303));
#110259=CARTESIAN_POINT('Ctrl Pts',(6.38266399484551,-29.7714555164209,
56.6505714927712));
#110260=CARTESIAN_POINT('Ctrl Pts',(6.38577523926507,-29.8169918410653,
56.6559709198486));
#110261=CARTESIAN_POINT('Ctrl Pts',(6.38666958545936,-29.8301723037498,
56.657374503499));
#110262=CARTESIAN_POINT('Ctrl Pts',(6.38829181642349,-29.8542409324696,
56.6596474201703));
#110263=CARTESIAN_POINT('Ctrl Pts',(6.38902124328637,-29.8651234633131,
56.6605672508789));
#110264=CARTESIAN_POINT('Ctrl Pts',(6.39049148943486,-29.8871763988337,
56.6622130180382));
#110265=CARTESIAN_POINT('Ctrl Pts',(6.39123210213837,-29.8983466530495,
56.6629335193349));
#110266=CARTESIAN_POINT('Ctrl Pts',(6.39306114458357,-29.9260788493085,
56.6644418139332));
#110267=CARTESIAN_POINT('Ctrl Pts',(6.39414533702312,-29.9426471277199,
56.6650950630284));
#110268=CARTESIAN_POINT('Ctrl Pts',(6.39840404599992,-30.0081958039325,
56.6666999165734));
#110269=CARTESIAN_POINT('Ctrl Pts',(6.40151935112882,-30.0572007786793,
56.6657384385704));
#110270=CARTESIAN_POINT('Ctrl Pts',(6.41006506225163,-30.1933658791567,
56.6570493918086));
#110271=CARTESIAN_POINT('Ctrl Pts',(6.41537370517354,-30.2800630003335,
56.6446181206207));
#110272=CARTESIAN_POINT('Ctrl Pts',(6.42592433737092,-30.4484520774009,
56.6067654527329));
#110273=CARTESIAN_POINT('Ctrl Pts',(6.43115151797511,-30.5299538928468,
56.5817552902691));
#110274=CARTESIAN_POINT('Ctrl Pts',(6.43771142480958,-30.6241671028476,
56.5447429617688));
#110275=CARTESIAN_POINT('Ctrl Pts',(6.43876529236094,-30.6390705533312,
56.5386371148954));
#110276=CARTESIAN_POINT('Ctrl Pts',(6.44034477585217,-30.6610189829191,
56.5292711035896));
#110277=CARTESIAN_POINT('Ctrl Pts',(6.44086112012565,-30.668133961902,56.5261760078868));
#110278=CARTESIAN_POINT('Ctrl Pts',(6.44178277919925,-30.68072167513,56.5205953203357));
#110279=CARTESIAN_POINT('Ctrl Pts',(6.44218689851657,-30.6862029559263,
56.5181296480535));
#110280=CARTESIAN_POINT('Ctrl Pts',(6.44308316261483,-30.6982746496565,
56.5126206416278));
#110281=CARTESIAN_POINT('Ctrl Pts',(6.44357607857959,-30.7048584846996,
56.509563911664));
#110282=CARTESIAN_POINT('Ctrl Pts',(6.44503391268635,-30.7241750915241,
56.5004417184846));
#110283=CARTESIAN_POINT('Ctrl Pts',(6.44600553060751,-30.7368506952597,
56.4942576530855));
#110284=CARTESIAN_POINT('Ctrl Pts',(6.4482755778935,-30.7660429090638,56.4795538565577));
#110285=CARTESIAN_POINT('Ctrl Pts',(6.44957959990121,-30.7824983244714,
56.470917286353));
#110286=CARTESIAN_POINT('Ctrl Pts',(6.45419582406069,-30.8397655975806,
56.4396278555028));
#110287=CARTESIAN_POINT('Ctrl Pts',(6.45756105367133,-30.8797650680921,
56.4155378848624));
#110288=CARTESIAN_POINT('Ctrl Pts',(6.46884719803039,-31.0095146381318,
56.3297698259801));
#110289=CARTESIAN_POINT('Ctrl Pts',(6.47681653686281,-31.0942392898449,
56.2609728641792));
#110290=CARTESIAN_POINT('Ctrl Pts',(6.48802982171822,-31.2069943132559,
56.149431417208));
#110291=CARTESIAN_POINT('Ctrl Pts',(6.49148702134616,-31.240759703818,56.1128989578508));
#110292=CARTESIAN_POINT('Ctrl Pts',(6.49604384421507,-31.2838947961095,
56.0618208604164));
#110293=CARTESIAN_POINT('Ctrl Pts',(6.49720311866262,-31.2947440448116,
56.0485643917151));
#110294=CARTESIAN_POINT('Ctrl Pts',(6.49911382138648,-31.3124112152241,
56.026284851335));
#110295=CARTESIAN_POINT('Ctrl Pts',(6.49986983686129,-31.3193449545432,
56.0173557370598));
#110296=CARTESIAN_POINT('Ctrl Pts',(6.50135207430642,-31.3328239830127,
55.9996281603467));
#110297=CARTESIAN_POINT('Ctrl Pts',(6.50207847116319,-31.3393743439319,
55.990834297567));
#110298=CARTESIAN_POINT('Ctrl Pts',(6.50381664423439,-31.3549110227476,
55.9695406601622));
#110299=CARTESIAN_POINT('Ctrl Pts',(6.50482510233097,-31.3638119482423,
55.956979606478));
#110300=CARTESIAN_POINT('Ctrl Pts',(6.5084058534178,-31.3949900649015,55.9116621283627));
#110301=CARTESIAN_POINT('Ctrl Pts',(6.51094107849887,-31.4162725664222,
55.8782354598566));
#110302=CARTESIAN_POINT('Ctrl Pts',(6.51733360379184,-31.4675700854227,
55.7909440369044));
#110303=CARTESIAN_POINT('Ctrl Pts',(6.52113625623734,-31.495824671124,55.736113986869));
#110304=CARTESIAN_POINT('Ctrl Pts',(6.53045827924483,-31.5579374823455,
55.5971519243775));
#110305=CARTESIAN_POINT('Ctrl Pts',(6.53592604086477,-31.58809067844,55.5115913280997));
#110306=CARTESIAN_POINT('Ctrl Pts',(6.54418381491401,-31.6216081323308,
55.384232870677));
#110307=CARTESIAN_POINT('Ctrl Pts',(6.546804833239,-31.6305989143249,55.3440848786691));
#110308=CARTESIAN_POINT('Ctrl Pts',(6.55022790961468,-31.6401206751567,
55.2927179031992));
#110309=CARTESIAN_POINT('Ctrl Pts',(6.55096166475799,-31.642037448462,55.2817669272673));
#110310=CARTESIAN_POINT('Ctrl Pts',(6.55214231022928,-31.6449216312794,
55.264258863758));
#110311=CARTESIAN_POINT('Ctrl Pts',(6.55258536627677,-31.6459597945717,
55.2577135443564));
#110312=CARTESIAN_POINT('Ctrl Pts',(6.55344501240524,-31.6478885285661,
55.2450661648734));
#110313=CARTESIAN_POINT('Ctrl Pts',(6.55386131345546,-31.648784311075,55.2389650984162));
#110314=CARTESIAN_POINT('Ctrl Pts',(6.55488510715645,-31.6508945156848,
55.2240157711139));
#110315=CARTESIAN_POINT('Ctrl Pts',(6.55549460765298,-31.6520716836945,
55.2151625213445));
#110316=CARTESIAN_POINT('Ctrl Pts',(6.55775367196738,-31.6561471291876,
55.1825041635758));
#110317=CARTESIAN_POINT('Ctrl Pts',(6.55942476648695,-31.6586023523677,
55.158647959365));
#110318=CARTESIAN_POINT('Ctrl Pts',(6.56382220246398,-31.6636495727199,
55.0964497839689));
#110319=CARTESIAN_POINT('Ctrl Pts',(6.56657631845046,-31.6654313142897,
55.0580571472878));
#110320=CARTESIAN_POINT('Ctrl Pts',(6.57445120362573,-31.6667160417164,
54.9490843839346));
#110321=CARTESIAN_POINT('Ctrl Pts',(6.57961396198102,-31.6630646877723,
54.8785476238241));
#110322=CARTESIAN_POINT('Ctrl Pts',(6.59159738118093,-31.6440420474533,
54.7141919616201));
#110323=CARTESIAN_POINT('Ctrl Pts',(6.59834696353943,-31.6250971284716,
54.6210207830579));
#110324=CARTESIAN_POINT('Ctrl Pts',(6.60621484709289,-31.5926783515014,
54.5107853364076));
#110325=CARTESIAN_POINT('Ctrl Pts',(6.6075720973104,-31.5866957127602,54.4917165221717));
#110326=CARTESIAN_POINT('Ctrl Pts',(6.60972019712478,-31.5766030886609,
54.4614645137954));
#110327=CARTESIAN_POINT('Ctrl Pts',(6.61051818373063,-31.5727139121417,
54.4502102834942));
#110328=CARTESIAN_POINT('Ctrl Pts',(6.6120271607111,-31.565093953576,54.4289029232398));
#110329=CARTESIAN_POINT('Ctrl Pts',(6.6127388667327,-31.5613861373545,54.4188422814309));
#110330=CARTESIAN_POINT('Ctrl Pts',(6.61436097808779,-31.552675349376,54.3958920569952));
#110331=CARTESIAN_POINT('Ctrl Pts',(6.61526920207865,-31.5476084876256,
54.3830274434801));
#110332=CARTESIAN_POINT('Ctrl Pts',(6.61811386707399,-31.5311448823686,
54.3427062959116));
#110333=CARTESIAN_POINT('Ctrl Pts',(6.62003099203653,-31.5191727540191,
54.3154899699754));
#110334=CARTESIAN_POINT('Ctrl Pts',(6.62754596938904,-31.4688594641646,
54.2089442347415));
#110335=CARTESIAN_POINT('Ctrl Pts',(6.6329590627278,-31.4249797997386,54.1323871235107));
#110336=CARTESIAN_POINT('Ctrl Pts',(6.64524540973922,-31.3114866432478,
53.9664045617817));
#110337=CARTESIAN_POINT('Ctrl Pts',(6.65206559460718,-31.2384165709876,
53.8798956084));
#110338=CARTESIAN_POINT('Ctrl Pts',(6.66036552659228,-31.1465515002008,
53.7912015860564));
#110339=CARTESIAN_POINT('Ctrl Pts',(6.66133383591659,-31.1357953540181,
53.7810894925221));
#110340=CARTESIAN_POINT('Ctrl Pts',(6.66280228957537,-31.1194550410455,
53.7661316779733));
#110341=CARTESIAN_POINT('Ctrl Pts',(6.66329475876906,-31.1139703526395,
53.7611777071479));
#110342=CARTESIAN_POINT('Ctrl Pts',(6.66419224763573,-31.1039708595749,
53.7522658985747));
#110343=CARTESIAN_POINT('Ctrl Pts',(6.66459634586287,-31.099467381068,53.7482957532474));
#110344=CARTESIAN_POINT('Ctrl Pts',(6.66551640010813,-31.0892113127656,
53.7393523333189));
#110345=CARTESIAN_POINT('Ctrl Pts',(6.66603338983346,-31.0834461069383,
53.7343940775085));
#110346=CARTESIAN_POINT('Ctrl Pts',(6.66763708710476,-31.0655497049758,
53.7192145114203));
#110347=CARTESIAN_POINT('Ctrl Pts',(6.66873257049119,-31.0533067096527,
53.709127205663));
#110348=CARTESIAN_POINT('Ctrl Pts',(6.67447627725844,-30.9889329192329,
53.6576135496223));
#110349=CARTESIAN_POINT('Ctrl Pts',(6.67927577834879,-30.9345011445328,
53.6191685166873));
#110350=CARTESIAN_POINT('Ctrl Pts',(6.69273899257741,-30.7769696367807,
53.5214928191034));
#110351=CARTESIAN_POINT('Ctrl Pts',(6.70141841924839,-30.669597349037,53.4698653735107));
#110352=CARTESIAN_POINT('Ctrl Pts',(6.71246226014045,-30.5210218901359,
53.417090640398));
#110353=CARTESIAN_POINT('Ctrl Pts',(6.71514591414966,-30.4839602232894,
53.4053687628767));
#110354=CARTESIAN_POINT('Ctrl Pts',(6.71885660419074,-30.4313759477885,
53.390739960444));
#110355=CARTESIAN_POINT('Ctrl Pts',(6.71991831292793,-30.4161728647477,
53.386741415857));
#110356=CARTESIAN_POINT('Ctrl Pts',(6.7217054999011,-30.3903206469363,53.3803318449864));
#110357=CARTESIAN_POINT('Ctrl Pts',(6.72243451998192,-30.3797005215353,
53.3778093011255));
#110358=CARTESIAN_POINT('Ctrl Pts',(6.72390481430653,-30.3581343286676,
53.3729101916273));
#110359=CARTESIAN_POINT('Ctrl Pts',(6.72464587395247,-30.347187546578,53.3705392733303));
#110360=CARTESIAN_POINT('Ctrl Pts',(6.72647765479427,-30.3199441082982,
53.364925740841));
#110361=CARTESIAN_POINT('Ctrl Pts',(6.72756411025945,-30.3036210497676,
53.3618161409262));
#110362=CARTESIAN_POINT('Ctrl Pts',(6.73184527654185,-30.2386899828942,
53.3504504281761));
#110363=CARTESIAN_POINT('Ctrl Pts',(6.7349799413163,-30.1897698543038,53.3441090603889));
#110364=CARTESIAN_POINT('Ctrl Pts',(6.74360761037585,-30.0524770583381,
53.3324778720197));
#110365=CARTESIAN_POINT('Ctrl Pts',(6.74897558756391,-29.9638616631134,
53.3320435002566));
#110366=CARTESIAN_POINT('Ctrl Pts',(6.7594938352577,-29.7923215208844,53.3448853630534));
#110367=CARTESIAN_POINT('Ctrl Pts',(6.76462755606351,-29.7096121550668,
53.3573782164383));
#110368=CARTESIAN_POINT('Ctrl Pts',(6.77110298398023,-29.6121919639257,
53.3796819447237));
#110369=CARTESIAN_POINT('Ctrl Pts',(6.7721774885088,-29.5962401927215,53.3835830854678));
#110370=CARTESIAN_POINT('Ctrl Pts',(6.77377489571398,-29.5728888557533,
53.3896610600392));
#110371=CARTESIAN_POINT('Ctrl Pts',(6.77428799971171,-29.5654420285151,
53.391654640737));
#110372=CARTESIAN_POINT('Ctrl Pts',(6.77520625420989,-29.552216891469,53.3952936772094));
#110373=CARTESIAN_POINT('Ctrl Pts',(6.77561024597358,-29.546433260931,53.3969188088018));
#110374=CARTESIAN_POINT('Ctrl Pts',(6.7765091908108,-29.5336417413808,53.4005878394914));
#110375=CARTESIAN_POINT('Ctrl Pts',(6.77700494655082,-29.5266385206989,
53.4026465045521));
#110376=CARTESIAN_POINT('Ctrl Pts',(6.77847958508031,-29.5059512434473,
53.4088757202914));
#110377=CARTESIAN_POINT('Ctrl Pts',(6.7794653931904,-29.4923075223388,53.4131764555359));
#110378=CARTESIAN_POINT('Ctrl Pts',(6.78632560307716,-29.3985226082869,
53.4440723573382));
#110379=CARTESIAN_POINT('Ctrl Pts',(6.79245505366984,-29.3204563505974,
53.4765488418306));
#110380=CARTESIAN_POINT('Ctrl Pts',(6.80788164753911,-29.1315073154385,
53.5725757407264));
#110381=CARTESIAN_POINT('Ctrl Pts',(6.81711789559479,-29.0248065886135,
53.6432284561324));
#110382=CARTESIAN_POINT('Ctrl Pts',(6.82734013490775,-28.9111276206617,
53.7389074687808));
#110383=CARTESIAN_POINT('Ctrl Pts',(6.82877353692025,-28.89530988061,53.7527401069981));
#110384=CARTESIAN_POINT('Ctrl Pts',(6.83109604993436,-28.869892769504,53.7758303762298));
#110385=CARTESIAN_POINT('Ctrl Pts',(6.83199242314646,-28.8601357967463,
53.7849101941681));
#110386=CARTESIAN_POINT('Ctrl Pts',(6.83359759708086,-28.8427636436285,
53.8014701025973));
#110387=CARTESIAN_POINT('Ctrl Pts',(6.83430814708804,-28.8351094944398,
53.8089080561819));
#110388=CARTESIAN_POINT('Ctrl Pts',(6.83507857929352,-28.8268512987124,
53.8170887481323));
#110389=CARTESIAN_POINT('Ctrl Pts',(6.83514161006157,-28.8261759781728,
53.8177588778444));
#110390=CARTESIAN_POINT('Ctrl Pts',(6.83526452264084,-28.8248596649576,
53.8190673129861));
#110391=CARTESIAN_POINT('Ctrl Pts',(6.83532440685726,-28.8242186175232,
53.8197055626126));
#110392=CARTESIAN_POINT('Ctrl Pts',(6.83544187066243,-28.8229617318725,
53.820959002801));
#110393=CARTESIAN_POINT('Ctrl Pts',(6.83549945192553,-28.8223458554046,
53.8215741544607));
#110394=CARTESIAN_POINT('Ctrl Pts',(6.83560305029199,-28.8212382498314,
53.8226821919843));
#110395=CARTESIAN_POINT('Ctrl Pts',(6.83564907499752,-28.8207463474032,
53.823174903577));
#110396=CARTESIAN_POINT('Ctrl Pts',(6.83573287662861,-28.8198509918158,
53.8240728570715));
#110397=CARTESIAN_POINT('Ctrl Pts',(6.83577065794308,-28.8194474383768,
53.8244779984022));
#110398=CARTESIAN_POINT('Ctrl Pts',(6.83584010609792,-28.818705846083,53.8252232757313));
#110399=CARTESIAN_POINT('Ctrl Pts',(6.83587177563708,-28.8183677454655,
53.8255633499389));
#110400=CARTESIAN_POINT('Ctrl Pts',(6.83593044164009,-28.8177415784931,
53.8261937161408));
#110401=CARTESIAN_POINT('Ctrl Pts',(6.83595743984718,-28.8174534721845,
53.8264839682376));
#110402=CARTESIAN_POINT('Ctrl Pts',(6.8360077757481,-28.8169164284342,53.8270254104384));
#110403=CARTESIAN_POINT('Ctrl Pts',(6.83603111461288,-28.8166674641071,
53.8272765737124));
#110404=CARTESIAN_POINT('Ctrl Pts',(6.83607486602183,-28.8162008317435,
53.8277476274427));
#110405=CARTESIAN_POINT('Ctrl Pts',(6.83609527937983,-28.8159831449993,
53.8279674992538));
#110406=CARTESIAN_POINT('Ctrl Pts',(6.83613372631143,-28.815573211118,53.8283817786788));
#110407=CARTESIAN_POINT('Ctrl Pts',(6.83615176046674,-28.8153809505954,
53.8285761729668));
#110408=CARTESIAN_POINT('Ctrl Pts',(6.8361858649719,-28.8150174139846,53.8289439252416));
#110409=CARTESIAN_POINT('Ctrl Pts',(6.83620193575106,-28.8148461280511,
53.8291172735098));
#110410=CARTESIAN_POINT('Ctrl Pts',(6.83623243619874,-28.814521086211,53.8294463733511));
#110411=CARTESIAN_POINT('Ctrl Pts',(6.83624686618403,-28.8143673229833,
53.8296021176157));
#110412=CARTESIAN_POINT('Ctrl Pts',(6.83627433952821,-28.8140746035144,
53.8298987252713));
#110413=CARTESIAN_POINT('Ctrl Pts',(6.836287383132,-28.8139356416561,53.8300395831406));
#110414=CARTESIAN_POINT('Ctrl Pts',(6.83631228732558,-28.8136703470738,
53.830308593273));
#110415=CARTESIAN_POINT('Ctrl Pts',(6.83632414810166,-28.8135440100357,
53.8304367412317));
#110416=CARTESIAN_POINT('Ctrl Pts',(6.83634685163478,-28.813302200916,53.8306820959549));
#110417=CARTESIAN_POINT('Ctrl Pts',(6.83635769454145,-28.8131867254108,
53.8307992993801));
#110418=CARTESIAN_POINT('Ctrl Pts',(6.83637849756472,-28.8129651939076,
53.8310242124088));
#110419=CARTESIAN_POINT('Ctrl Pts',(6.83638845779823,-28.8128591352087,
53.8311319193375));
#110420=CARTESIAN_POINT('Ctrl Pts',(6.83640760744377,-28.8126552408453,
53.8313390387445));
#110421=CARTESIAN_POINT('Ctrl Pts',(6.83641679694208,-28.8125574030905,
53.8314384489897));
#110422=CARTESIAN_POINT('Ctrl Pts',(6.83646057669842,-28.8120913255394,
53.8319121365132));
#110423=CARTESIAN_POINT('Ctrl Pts',(6.83649515985212,-28.8117232498803,
53.8322865759057));
#110424=CARTESIAN_POINT('Ctrl Pts',(6.83656431451738,-28.8109874134505,
53.8330358425514));
#110425=CARTESIAN_POINT('Ctrl Pts',(6.83659888602374,-28.8106196527552,
53.8334106698021));
#110426=CARTESIAN_POINT('Ctrl Pts',(6.83771103258841,-28.7987920731994,
53.8454769237986));
#110427=CARTESIAN_POINT('Ctrl Pts',(6.83878112541177,-28.7875047105982,
53.8573367857502));
#110428=CARTESIAN_POINT('Ctrl Pts',(6.84310129633435,-28.7423488813134,
53.90620559449));
#110429=CARTESIAN_POINT('Ctrl Pts',(6.84628873624599,-28.7099834588903,
53.9445708939718));
#110430=CARTESIAN_POINT('Ctrl Pts',(6.85516692072802,-28.6234808572727,
54.0570453664965));
#110431=CARTESIAN_POINT('Ctrl Pts',(6.8607218294409,-28.5736642265657,54.1342427942307));
#110432=CARTESIAN_POINT('Ctrl Pts',(6.86680934089025,-28.5268050245209,
54.2219816610238));
#110433=CARTESIAN_POINT('Ctrl Pts',(6.86728370050633,-28.5232044675888,
54.2288379378827));
#110434=CARTESIAN_POINT('Ctrl Pts',(6.8725302379048,-28.4839611774338,54.3048489007251));
#110435=CARTESIAN_POINT('Ctrl Pts',(6.8773524817932,-28.4531611918282,54.37638528604));
#110436=CARTESIAN_POINT('Ctrl Pts',(6.88323618885321,-28.4234128320027,
54.4614091006557));
#110437=CARTESIAN_POINT('Ctrl Pts',(6.8840458277414,-28.4194800173811,54.4730618462956));
#110438=CARTESIAN_POINT('Ctrl Pts',(6.88532459030823,-28.4135257891944,
54.4913705195861));
#110439=CARTESIAN_POINT('Ctrl Pts',(6.8857888172279,-28.411416350646,54.4979976548669));
#110440=CARTESIAN_POINT('Ctrl Pts',(6.88666167855222,-28.407548622983,54.5104172640336));
#110441=CARTESIAN_POINT('Ctrl Pts',(6.88706973481944,-28.4057803301274,
54.5162063631653));
#110442=CARTESIAN_POINT('Ctrl Pts',(6.88803550844753,-28.4016881818446,
54.5298694525105));
#110443=CARTESIAN_POINT('Ctrl Pts',(6.88859470570326,-28.3993909380068,
54.5377511240206));
#110444=CARTESIAN_POINT('Ctrl Pts',(6.89047605389359,-28.3918991639899,
54.5641804279561));
#110445=CARTESIAN_POINT('Ctrl Pts',(6.8918116887932,-28.3869682669896,54.5828003504918));
#110446=CARTESIAN_POINT('Ctrl Pts',(6.90253166792987,-28.3503542747171,
54.7314284138191));
#110447=CARTESIAN_POINT('Ctrl Pts',(6.91245387919625,-28.3341187293571,
54.8647290811869));
#110448=CARTESIAN_POINT('Ctrl Pts',(6.92208048413035,-28.3340006487619,
54.9985297366875));
#110449=CARTESIAN_POINT('Ctrl Pts',(6.92208059163593,-28.3340006474439,
54.9985312309128));
#110450=CARTESIAN_POINT('Ctrl Pts',(6.92754558400022,-28.3339336815855,
55.0744894450113));
#110451=CARTESIAN_POINT('Ctrl Pts',(6.9329088628046,-28.3390614478877,55.1503739691616));
#110452=CARTESIAN_POINT('Ctrl Pts',(6.93913001267378,-28.3513608312705,
55.240342760058));
#110453=CARTESIAN_POINT('Ctrl Pts',(6.94013956192787,-28.3535646995461,
55.2550030920907));
#110454=CARTESIAN_POINT('Ctrl Pts',(6.94187955803527,-28.3577252098531,
55.2803710625575));
#110455=CARTESIAN_POINT('Ctrl Pts',(6.94261278500586,-28.3595916142998,
55.2910923512533));
#110456=CARTESIAN_POINT('Ctrl Pts',(6.94407769604804,-28.3635481035932,
55.3125720400525));
#110457=CARTESIAN_POINT('Ctrl Pts',(6.94480929686973,-28.3656395611335,
55.3233296386573));
#110458=CARTESIAN_POINT('Ctrl Pts',(6.94620091272753,-28.3698387894156,
55.3438460153887));
#110459=CARTESIAN_POINT('Ctrl Pts',(6.9468614704027,-28.3719284220095,55.3536079737256));
#110460=CARTESIAN_POINT('Ctrl Pts',(6.94857774680902,-28.3776091700568,
55.3790277533253));
#110461=CARTESIAN_POINT('Ctrl Pts',(6.94962899207316,-28.3813392795987,
55.3946537021924));
#110462=CARTESIAN_POINT('Ctrl Pts',(6.95335095277997,-28.3954360792833,
55.4501409233542));
#110463=CARTESIAN_POINT('Ctrl Pts',(6.95598175595763,-28.4070544959849,
55.4896705798554));
#110464=CARTESIAN_POINT('Ctrl Pts',(6.95961845963333,-28.4253742592874,
55.5444108263045));
#110465=CARTESIAN_POINT('Ctrl Pts',(6.96065394412911,-28.4308534186706,
55.5600072461366));
#110466=CARTESIAN_POINT('Ctrl Pts',(6.96168426276526,-28.4365622954254,
55.5755158937115));
#110467=CARTESIAN_POINT('Ctrl Pts',(6.76892552105682,-28.4365623357949,
55.5755160033788));
#110468=CARTESIAN_POINT('Ctrl Pts',(6.76565913960721,-28.4207846271609,
55.5326545298688));
#110469=CARTESIAN_POINT('Ctrl Pts',(6.76234508913007,-28.4067718546495,
55.4891506581147));
#110470=CARTESIAN_POINT('Ctrl Pts',(6.75469118016146,-28.3786619363516,
55.3877638001349));
#110471=CARTESIAN_POINT('Ctrl Pts',(6.75035205900689,-28.3658452849425,
55.3296007955738));
#110472=CARTESIAN_POINT('Ctrl Pts',(6.74215952333329,-28.3473559318162,
55.2173964913116));
#110473=CARTESIAN_POINT('Ctrl Pts',(6.7383018338593,-28.3411578477954,55.1635154863884));
#110474=CARTESIAN_POINT('Ctrl Pts',(6.73197961047013,-28.3352107256762,
55.0731647396338));
#110475=CARTESIAN_POINT('Ctrl Pts',(6.72947634806754,-28.3340108244741,
55.0368351827447));
#110476=CARTESIAN_POINT('Ctrl Pts',(6.7260983248784,-28.3339961009531,54.9870677129444));
#110477=CARTESIAN_POINT('Ctrl Pts',(6.72519214130387,-28.3341544057567,
54.9736426547827));
#110478=CARTESIAN_POINT('Ctrl Pts',(6.72362205828857,-28.3347129509713,
54.9502568887751));
#110479=CARTESIAN_POINT('Ctrl Pts',(6.72295592249942,-28.3350403340662,
54.9402953013315));
#110480=CARTESIAN_POINT('Ctrl Pts',(6.72156263854722,-28.3359156860119,
54.9193794326819));
#110481=CARTESIAN_POINT('Ctrl Pts',(6.7208361119486,-28.3364824730713,54.90842638312));
#110482=CARTESIAN_POINT('Ctrl Pts',(6.71909604212404,-28.3381063644793,
54.8820874958341));
#110483=CARTESIAN_POINT('Ctrl Pts',(6.71808583914157,-28.3392690314072,
54.8667090002036));
#110484=CARTESIAN_POINT('Ctrl Pts',(6.71448948270676,-28.3441987761385,
54.8116796715743));
#110485=CARTESIAN_POINT('Ctrl Pts',(6.71194085023437,-28.349173988967,54.7721489212533));
#110486=CARTESIAN_POINT('Ctrl Pts',(6.7055033239652,-28.3655282164239,54.6714875184788));
#110487=CARTESIAN_POINT('Ctrl Pts',(6.70167015474496,-28.3789199735198,
54.6107457844851));
#110488=CARTESIAN_POINT('Ctrl Pts',(6.69223982706329,-28.4204369267072,
54.4624371944141));
#110489=CARTESIAN_POINT('Ctrl Pts',(6.68669528109406,-28.4524696586101,
54.3761883382278));
#110490=CARTESIAN_POINT('Ctrl Pts',(6.67845245895701,-28.5081580881101,
54.2573593702817));
#110491=CARTESIAN_POINT('Ctrl Pts',(6.67593863597083,-28.526130591661,54.2223009466579));
#110492=CARTESIAN_POINT('Ctrl Pts',(6.67264000283335,-28.5506590798549,
54.1783634791932));
#110493=CARTESIAN_POINT('Ctrl Pts',(6.67191773854498,-28.5560853256686,
54.1688645882659));
#110494=CARTESIAN_POINT('Ctrl Pts',(6.67075133868079,-28.564928023312,54.1537330145712));
#110495=CARTESIAN_POINT('Ctrl Pts',(6.67031087935598,-28.5682851323065,
54.148065775569));
#110496=CARTESIAN_POINT('Ctrl Pts',(6.66945256782083,-28.5748592929456,
54.1371163371139));
#110497=CARTESIAN_POINT('Ctrl Pts',(6.66903496784038,-28.5780722847564,
54.1318319182112));
#110498=CARTESIAN_POINT('Ctrl Pts',(6.66800259614495,-28.586052227117,54.1188704077936));
#110499=CARTESIAN_POINT('Ctrl Pts',(6.66738573788347,-28.5908523218151,
54.1112140446122));
#110500=CARTESIAN_POINT('Ctrl Pts',(6.66506535781466,-28.6090356622443,
54.0827284038169));
#110501=CARTESIAN_POINT('Ctrl Pts',(6.66333881220431,-28.6228197022216,
54.0621603339405));
#110502=CARTESIAN_POINT('Ctrl Pts',(6.65875255541449,-28.6602128406918,
54.0089663019004));
#110503=CARTESIAN_POINT('Ctrl Pts',(6.65586231210795,-28.6845550395998,
53.9768765597092));
#110504=CARTESIAN_POINT('Ctrl Pts',(6.64436107731688,-28.7851674674738,
53.8537741387872));
#110505=CARTESIAN_POINT('Ctrl Pts',(6.63563985538018,-28.8699229760116,
53.7701287418851));
#110506=CARTESIAN_POINT('Ctrl Pts',(6.62373755226918,-29.0016827291212,
53.6653164449545));
#110507=CARTESIAN_POINT('Ctrl Pts',(6.62028777090021,-29.0418737345012,
53.6361772485195));
#110508=CARTESIAN_POINT('Ctrl Pts',(6.61573906128677,-29.0976002886783,
53.599455937511));
#110509=CARTESIAN_POINT('Ctrl Pts',(6.61458074932236,-29.112035869094,53.5902593677723));
#110510=CARTESIAN_POINT('Ctrl Pts',(6.61267136477174,-29.1362331540602,
53.5753630257135));
#110511=CARTESIAN_POINT('Ctrl Pts',(6.61191571483802,-29.145915438421,53.5695374016819));
#110512=CARTESIAN_POINT('Ctrl Pts',(6.61043400696999,-29.1651067156508,
53.5582547455127));
#110513=CARTESIAN_POINT('Ctrl Pts',(6.60970777601657,-29.1746117728639,
53.5527921851536));
#110514=CARTESIAN_POINT('Ctrl Pts',(6.6079697011109,-29.1975930211952,53.5398849207254));
#110515=CARTESIAN_POINT('Ctrl Pts',(6.60696117765908,-29.2111199950772,
53.5325323280187));
#110516=CARTESIAN_POINT('Ctrl Pts',(6.60337852832171,-29.2598344180083,
53.5069218781544));
#110517=CARTESIAN_POINT('Ctrl Pts',(6.60084153221793,-29.2955706091488,
53.4897328088498));
#110518=CARTESIAN_POINT('Ctrl Pts',(6.59444280456623,-29.3884130256801,
53.4490890690541));
#110519=CARTESIAN_POINT('Ctrl Pts',(6.59063587572078,-29.446271590263,53.427502300134));
#110520=CARTESIAN_POINT('Ctrl Pts',(6.58129890638515,-29.5918521135978,
53.3822216512348));
#110521=CARTESIAN_POINT('Ctrl Pts',(6.57582061778002,-29.6805585883479,
53.3623960455244));
#110522=CARTESIAN_POINT('Ctrl Pts',(6.56756518769043,-29.8109303378142,
53.344258310898));
#110523=CARTESIAN_POINT('Ctrl Pts',(6.56495912441035,-29.8516190317749,
53.3401173639789));
#110524=CARTESIAN_POINT('Ctrl Pts',(6.56155321139184,-29.9034879401764,
53.3367608269718));
#110525=CARTESIAN_POINT('Ctrl Pts',(6.56082083952193,-29.9145674369421,
53.3361549395543));
#110526=CARTESIAN_POINT('Ctrl Pts',(6.55964198787364,-29.9322664048435,
53.3353643039506));
#110527=CARTESIAN_POINT('Ctrl Pts',(6.55919932393568,-29.9388825807096,
53.3351082624658));
#110528=CARTESIAN_POINT('Ctrl Pts',(6.55834007545749,-29.9516631893432,
53.3346899451462));
#110529=CARTESIAN_POINT('Ctrl Pts',(6.55792377613938,-29.9578272555728,
53.3345224466653));
#110530=CARTESIAN_POINT('Ctrl Pts',(6.55689948046678,-29.9729284031371,
53.3341959819868));
#110531=CARTESIAN_POINT('Ctrl Pts',(6.55628947003476,-29.9818660319469,
53.3340747171622));
#110532=CARTESIAN_POINT('Ctrl Pts',(6.55402543249386,-30.014848840184,53.3338926546128));
#110533=CARTESIAN_POINT('Ctrl Pts',(6.55234975124015,-30.0388923062775,
53.3342805107416));
#110534=CARTESIAN_POINT('Ctrl Pts',(6.54793660452432,-30.1014684288166,
53.3366454183497));
#110535=CARTESIAN_POINT('Ctrl Pts',(6.54517113475498,-30.1399549445576,
53.3394408923582));
#110536=CARTESIAN_POINT('Ctrl Pts',(6.53729713520417,-30.2482866903495,
53.3511023076848));
#110537=CARTESIAN_POINT('Ctrl Pts',(6.53214743478204,-30.3177182737567,
53.3630622936105));
#110538=CARTESIAN_POINT('Ctrl Pts',(6.52018033767066,-30.4784482649231,
53.4013633801534));
#110539=CARTESIAN_POINT('Ctrl Pts',(6.51343421824998,-30.5686776635636,
53.4311906017877));
#110540=CARTESIAN_POINT('Ctrl Pts',(6.50557015903207,-30.6742518370309,
53.4764057508554));
#110541=CARTESIAN_POINT('Ctrl Pts',(6.50421350324754,-30.6924708840814,
53.4845993563753));
#110542=CARTESIAN_POINT('Ctrl Pts',(6.50206627961172,-30.72130450789,53.498195260846));
#110543=CARTESIAN_POINT('Ctrl Pts',(6.50126858138943,-30.7320156596414,
53.5033869055708));
#110544=CARTESIAN_POINT('Ctrl Pts',(6.49976011864925,-30.7522648828816,
53.5134710135772));
#110545=CARTESIAN_POINT('Ctrl Pts',(6.49904863924309,-30.7618131200177,
53.5183415842971));
#110546=CARTESIAN_POINT('Ctrl Pts',(6.49742701024426,-30.7835650422488,
53.5297031375696));
#110547=CARTESIAN_POINT('Ctrl Pts',(6.49651904096685,-30.7957363897359,
53.5362545794267));
#110548=CARTESIAN_POINT('Ctrl Pts',(6.49367509061945,-30.8338168646511,
53.5573674509288));
#110549=CARTESIAN_POINT('Ctrl Pts',(6.49175841672865,-30.8594195421304,
53.5724715556519));
#110550=CARTESIAN_POINT('Ctrl Pts',(6.48423921188111,-30.9593206248306,
53.6350699472592));
#110551=CARTESIAN_POINT('Ctrl Pts',(6.47882182428877,-31.0302044313446,
53.6877457840761));
#110552=CARTESIAN_POINT('Ctrl Pts',(6.46653547230616,-31.181579873004,53.820097571756));
#110553=CARTESIAN_POINT('Ctrl Pts',(6.45971928616396,-31.2587834073888,
53.9028410379685));
#110554=CARTESIAN_POINT('Ctrl Pts',(6.45142363028504,-31.3359485144926,
54.004502277826));
#110555=CARTESIAN_POINT('Ctrl Pts',(6.45045488656884,-31.3447211317998,
54.01638463353));
#110556=CARTESIAN_POINT('Ctrl Pts',(6.44898599694043,-31.3576445911966,
54.0343852797418));
#110557=CARTESIAN_POINT('Ctrl Pts',(6.44849353533333,-31.3619148388974,
54.0404174916245));
#110558=CARTESIAN_POINT('Ctrl Pts',(6.44759619415702,-31.3695798107692,
54.0513993654085));
#110559=CARTESIAN_POINT('Ctrl Pts',(6.44719223723379,-31.3729881136117,
54.0563392248127));
#110560=CARTESIAN_POINT('Ctrl Pts',(6.4462726942587,-31.3806511842817,54.0675751779392));
#110561=CARTESIAN_POINT('Ctrl Pts',(6.4457560773142,-31.3848895887407,54.0738819930576));
#110562=CARTESIAN_POINT('Ctrl Pts',(6.44415419193571,-31.3978310598427,
54.0934266100667));
#110563=CARTESIAN_POINT('Ctrl Pts',(6.44306017257623,-31.4063882728738,
54.1067592913909));
#110564=CARTESIAN_POINT('Ctrl Pts',(6.43733025671541,-31.4498246622094,
54.1766076473768));
#110565=CARTESIAN_POINT('Ctrl Pts',(6.43254380757642,-31.4814888094224,
54.2350452908363));
#110566=CARTESIAN_POINT('Ctrl Pts',(6.41913087593009,-31.5596129183819,
54.4023780319856));
#110567=CARTESIAN_POINT('Ctrl Pts',(6.41048772483013,-31.5981003872293,
54.5145859991129));
#110568=CARTESIAN_POINT('Ctrl Pts',(6.39943625471713,-31.6331301734757,
54.6683465839482));
#110569=CARTESIAN_POINT('Ctrl Pts',(6.39671430126995,-31.6405167081928,
54.7070605367482));
#110570=CARTESIAN_POINT('Ctrl Pts',(6.3929613210461,-31.6489317475928,54.7616106358652));
#110571=CARTESIAN_POINT('Ctrl Pts',(6.39189452965546,-31.6511174567935,
54.7772522259164));
#110572=CARTESIAN_POINT('Ctrl Pts',(6.39010151789645,-31.654438577159,54.8037644873379));
#110573=CARTESIAN_POINT('Ctrl Pts',(6.38937169798392,-31.6556900011961,
54.8146192788589));
#110574=CARTESIAN_POINT('Ctrl Pts',(6.38790199257379,-31.6580055197637,
54.836602772055));
#110575=CARTESIAN_POINT('Ctrl Pts',(6.38716230119331,-31.6590645725183,
54.8477314471046));
#110576=CARTESIAN_POINT('Ctrl Pts',(6.38533804317809,-31.6614109970575,
54.875330799598));
#110577=CARTESIAN_POINT('Ctrl Pts',(6.38425766760158,-31.6625655640006,
54.8918117930393));
#110578=CARTESIAN_POINT('Ctrl Pts',(6.38003469447249,-31.6661436116671,
54.9567244872429));
#110579=CARTESIAN_POINT('Ctrl Pts',(6.37695000439576,-31.6666974965136,
55.0052376413418));
#110580=CARTESIAN_POINT('Ctrl Pts',(6.36853173401014,-31.6623660967111,
55.1395219713638));
#110581=CARTESIAN_POINT('Ctrl Pts',(6.3633149707635,-31.6529689842531,55.2249932908889));
#110582=CARTESIAN_POINT('Ctrl Pts',(6.35273130926609,-31.6208093352436,
55.3951693111171));
#110583=CARTESIAN_POINT('Ctrl Pts',(6.34737753893032,-31.5978743123499,
55.4795576963606));
#110584=CARTESIAN_POINT('Ctrl Pts',(6.34067490008158,-31.5629997112202,
55.5769297476035));
#110585=CARTESIAN_POINT('Ctrl Pts',(6.33961976133011,-31.5573425782077,
55.5920304706183));
#110586=CARTESIAN_POINT('Ctrl Pts',(6.33803882002499,-31.5486392841874,
55.6142740514982));
#110587=CARTESIAN_POINT('Ctrl Pts',(6.33752231626647,-31.5457607467596,
55.6214820598275));
#110588=CARTESIAN_POINT('Ctrl Pts',(6.3366006126894,-31.5405645387525,55.6342341910222));
#110589=CARTESIAN_POINT('Ctrl Pts',(6.33619661128963,-31.5382670870313,
55.6397862720448));
#110590=CARTESIAN_POINT('Ctrl Pts',(6.33530092274614,-31.5331304351076,
55.6520120122583));
#110591=CARTESIAN_POINT('Ctrl Pts',(6.3348084682096,-31.5302777091874,55.6586795298017));
#110592=CARTESIAN_POINT('Ctrl Pts',(6.33335289649635,-31.5217596048237,
55.6782343884176));
#110593=CARTESIAN_POINT('Ctrl Pts',(6.33238310745829,-31.5159744657094,
55.6910684243616));
#110594=CARTESIAN_POINT('Ctrl Pts',(6.32555324472647,-31.4744261789098,
55.780208305354));
#110595=CARTESIAN_POINT('Ctrl Pts',(6.31943758145037,-31.4330842354636,
55.8537705976458));
#110596=CARTESIAN_POINT('Ctrl Pts',(6.30398734668806,-31.3153632882223,
56.0304205842287));
#110597=CARTESIAN_POINT('Ctrl Pts',(6.29471262151449,-31.2323071698481,
56.1284405037142));
#110598=CARTESIAN_POINT('Ctrl Pts',(6.28445419227063,-31.1234770690454,
56.2303648311442));
#110599=CARTESIAN_POINT('Ctrl Pts',(6.28301927600217,-31.1078547368788,
56.2444501976226));
#110600=CARTESIAN_POINT('Ctrl Pts',(6.2806949817233,-31.0819006765262,56.2669746074155));
#110601=CARTESIAN_POINT('Ctrl Pts',(6.27979831944513,-31.0717273510327,
56.2755917186481));
#110602=CARTESIAN_POINT('Ctrl Pts',(6.2781930383006,-31.0532277523854,56.2908838604507));
#110603=CARTESIAN_POINT('Ctrl Pts',(6.27748266537849,-31.0449388083166,
56.2976026878558));
#110604=CARTESIAN_POINT('Ctrl Pts',(6.275966711171,-31.0270331436314,56.3118337604913));
#110605=CARTESIAN_POINT('Ctrl Pts',(6.27516215461958,-31.0173972371559,
56.3193209497322));
#110606=CARTESIAN_POINT('Ctrl Pts',(6.27295821498649,-30.9906425858215,
56.3396421102787));
#110607=CARTESIAN_POINT('Ctrl Pts',(6.27156750488079,-30.9733571736003,
56.3522535253417));
#110608=CARTESIAN_POINT('Ctrl Pts',(6.26848416334874,-30.9341758651185,
56.3796994699422));
#110609=CARTESIAN_POINT('Ctrl Pts',(6.26679816403113,-30.9121598520017,
56.394352785779));
#110610=CARTESIAN_POINT('Ctrl Pts',(6.2613425696314,-30.8391584250602,56.4404713568075));
#110611=CARTESIAN_POINT('Ctrl Pts',(6.25764181277045,-30.7868220310939,
56.4697130563502));
#110612=CARTESIAN_POINT('Ctrl Pts',(6.24705519159442,-30.631701448412,56.5457164832189));
#110613=CARTESIAN_POINT('Ctrl Pts',(6.24028335159298,-30.525611856789,56.5849331272356));
#110614=CARTESIAN_POINT('Ctrl Pts',(6.23147096204794,-30.391991959689,56.6194236928982));
#110615=CARTESIAN_POINT('Ctrl Pts',(6.22984092402359,-30.3674582929019,
56.6251661559635));
#110616=CARTESIAN_POINT('Ctrl Pts',(6.22756639512607,-30.333649021922,56.6322750618287));
#110617=CARTESIAN_POINT('Ctrl Pts',(6.22694650420925,-30.3244767785757,
56.6341231157266));
#110618=CARTESIAN_POINT('Ctrl Pts',(6.22594692689197,-30.3097638685522,
56.6369587701112));
#110619=CARTESIAN_POINT('Ctrl Pts',(6.22556997045007,-30.3042327582114,
56.63799575572));
#110620=CARTESIAN_POINT('Ctrl Pts',(6.2247659752807,-30.2924754111959,56.6401384461436));
#110621=CARTESIAN_POINT('Ctrl Pts',(6.22433851405639,-30.2862479628438,
56.6412367558021));
#110622=CARTESIAN_POINT('Ctrl Pts',(6.22324859214083,-30.2704253361429,
56.643934537624));
#110623=CARTESIAN_POINT('Ctrl Pts',(6.22258352627971,-30.2608222607942,
56.6454854491177));
#110624=CARTESIAN_POINT('Ctrl Pts',(6.21982557876068,-30.2211898667766,
56.6515305021562));
#110625=CARTESIAN_POINT('Ctrl Pts',(6.21769755102649,-30.1910559042534,
56.6552870815289));
#110626=CARTESIAN_POINT('Ctrl Pts',(6.21163307096178,-30.1059932103466,
56.6635377201471));
#110627=CARTESIAN_POINT('Ctrl Pts',(6.20764067030133,-30.0509208727521,
56.6661328452094));
#110628=CARTESIAN_POINT('Ctrl Pts',(6.19369668431815,-29.859214975582,56.6656524085174));
#110629=CARTESIAN_POINT('Ctrl Pts',(6.18377226498223,-29.7231363052639,
56.6485081443138));
#110630=CARTESIAN_POINT('Ctrl Pts',(6.17287212023248,-29.5693351443392,
56.6095241200098));
#110631=CARTESIAN_POINT('Ctrl Pts',(6.17137385763873,-29.5481154474207,
56.6036959008019));
#110632=CARTESIAN_POINT('Ctrl Pts',(6.16904845124402,-29.5150708146775,
56.593911821669));
#110633=CARTESIAN_POINT('Ctrl Pts',(6.16821220287055,-29.50316488592,56.5902408918359));
#110634=CARTESIAN_POINT('Ctrl Pts',(6.16667604723887,-29.4812574091198,
56.5832161473564));
#110635=CARTESIAN_POINT('Ctrl Pts',(6.16597494257161,-29.4712444664426,
56.579900262463));
#110636=CARTESIAN_POINT('Ctrl Pts',(6.16441998665112,-29.4490098870519,
56.5723020005301));
#110637=CARTESIAN_POINT('Ctrl Pts',(6.163567761031,-29.4368052453364,56.5679717374854));
#110638=CARTESIAN_POINT('Ctrl Pts',(6.16107954471644,-29.4011313341281,
56.5548441912792));
#110639=CARTESIAN_POINT('Ctrl Pts',(6.1594564367364,-29.3778080046413,56.5456588775443));
#110640=CARTESIAN_POINT('Ctrl Pts',(6.1557642500518,-29.324734250198,56.523360953281));
#110641=CARTESIAN_POINT('Ctrl Pts',(6.15370666320824,-29.2951423092575,
56.5098967703338));
#110642=CARTESIAN_POINT('Ctrl Pts',(6.14631411352556,-29.1892381060753,
56.4579182726777));
#110643=CARTESIAN_POINT('Ctrl Pts',(6.14111992281912,-29.1155245406598,
56.4144132103598));
#110644=CARTESIAN_POINT('Ctrl Pts',(6.13052716357668,-28.9734485739807,
56.3150933427554));
#110645=CARTESIAN_POINT('Ctrl Pts',(6.1251414737833,-28.9055305507484,56.2591310944306));
#110646=CARTESIAN_POINT('Ctrl Pts',(6.11840332696257,-28.8307574367917,
56.1868815102113));
#110647=CARTESIAN_POINT('Ctrl Pts',(6.11734846581929,-28.8193278486441,
56.1755122777082));
#110648=CARTESIAN_POINT('Ctrl Pts',(6.11576786352582,-28.8026433639619,
56.1584270869045));
#110649=CARTESIAN_POINT('Ctrl Pts',(6.11525141547136,-28.7972601671323,
56.1528369867466));
#110650=CARTESIAN_POINT('Ctrl Pts',(6.11432977076201,-28.7877786421232,
56.142852346549));
#110651=CARTESIAN_POINT('Ctrl Pts',(6.11392577189538,-28.7836647459912,
56.1384729483725));
#110652=CARTESIAN_POINT('Ctrl Pts',(6.11303003876439,-28.7746373588998,
56.1287581684698));
#110653=CARTESIAN_POINT('Ctrl Pts',(6.11253753657757,-28.7697350401914,
56.1234129822956));
#110654=CARTESIAN_POINT('Ctrl Pts',(6.1111662516064,-28.7562498899095,56.1085154827675));
#110655=CARTESIAN_POINT('Ctrl Pts',(6.11028232248432,-28.7477425734866,
56.0988959116583));
#110656=CARTESIAN_POINT('Ctrl Pts',(6.10386852958636,-28.6872780949533,
56.0289123142471));
#110657=CARTESIAN_POINT('Ctrl Pts',(6.09810499110205,-28.6396026750669,
55.9649952137625));
#110658=CARTESIAN_POINT('Ctrl Pts',(6.08576410893854,-28.5481673300027,
55.8220958458226));
#110659=CARTESIAN_POINT('Ctrl Pts',(6.07920231560819,-28.5058704460738,
55.7424548369521));
#110660=CARTESIAN_POINT('Ctrl Pts',(6.07066779044151,-28.458232716068,55.6320007499705));
#110661=CARTESIAN_POINT('Ctrl Pts',(6.06854154822013,-28.4470114662275,
55.6039019484675));
#110662=CARTESIAN_POINT('Ctrl Pts',(6.06643884243078,-28.4365623175998,
55.5755159539501));
#110663=CARTESIAN_POINT('Origin',(5.,-30.,55.));
#110664=CARTESIAN_POINT('',(5.36787289131612,-28.4365623102018,55.5755159338528));
#110665=CARTESIAN_POINT('',(5.55935721585159,-28.4365623067732,55.5755159245387));
#110666=CARTESIAN_POINT('',(5.,-28.4365623102018,55.5755159338528));
#110667=CARTESIAN_POINT('Ctrl Pts',(5.55935721585159,-28.4365623067732,
55.5755159245387));
#110668=CARTESIAN_POINT('Ctrl Pts',(5.56381476847205,-28.4585691496616,
55.6352993748544));
#110669=CARTESIAN_POINT('Ctrl Pts',(5.56841204010037,-28.4839877256715,
55.6937734764538));
#110670=CARTESIAN_POINT('Ctrl Pts',(5.57397509760752,-28.5184874138571,
55.7621298013789));
#110671=CARTESIAN_POINT('Ctrl Pts',(5.57491059573364,-28.5244144050035,
55.7735428404087));
#110672=CARTESIAN_POINT('Ctrl Pts',(5.58247805316143,-28.5734009825808,
55.8652594684437));
#110673=CARTESIAN_POINT('Ctrl Pts',(5.58910661587447,-28.6228547543361,
55.9419834019496));
#110674=CARTESIAN_POINT('Ctrl Pts',(5.59908095274396,-28.7087755324195,
56.0539424144225));
#110675=CARTESIAN_POINT('Ctrl Pts',(5.60255546273909,-28.7409836611449,
56.0922151764099));
#110676=CARTESIAN_POINT('Ctrl Pts',(5.60707502115421,-28.7859483278344,
56.1410091598792));
#110677=CARTESIAN_POINT('Ctrl Pts',(5.60818129790271,-28.7972057452019,
56.1528700617814));
#110678=CARTESIAN_POINT('Ctrl Pts',(5.60931537774297,-28.8090033880795,
56.1649392027702));
#110679=CARTESIAN_POINT('Ctrl Pts',(5.60935065576839,-28.8093706381696,
56.1653145491692));
#110680=CARTESIAN_POINT('Ctrl Pts',(5.60942120053917,-28.8101055381518,
56.1660649405104));
#110681=CARTESIAN_POINT('Ctrl Pts',(5.60945646727773,-28.8104731880354,
56.1664399853584));
#110682=CARTESIAN_POINT('Ctrl Pts',(5.60950124849403,-28.8109403532348,
56.1669160966205));
#110683=CARTESIAN_POINT('Ctrl Pts',(5.60951077018214,-28.8110397039575,
56.1670173240154));
#110684=CARTESIAN_POINT('Ctrl Pts',(5.60953061972351,-28.8112468563811,
56.1672283355068));
#110685=CARTESIAN_POINT('Ctrl Pts',(5.60954094747514,-28.8113546603562,
56.1673381173494));
#110686=CARTESIAN_POINT('Ctrl Pts',(5.60956252718555,-28.8115799618273,
56.1675674888317));
#110687=CARTESIAN_POINT('Ctrl Pts',(5.60957377901646,-28.811697462146,56.1676870756487));
#110688=CARTESIAN_POINT('Ctrl Pts',(5.60959734966741,-28.8119436603209,
56.1679375700131));
#110689=CARTESIAN_POINT('Ctrl Pts',(5.60960966833416,-28.8120723618202,
56.1680684740838));
#110690=CARTESIAN_POINT('Ctrl Pts',(5.60963554717833,-28.8123428021082,
56.1683434517053));
#110691=CARTESIAN_POINT('Ctrl Pts',(5.6096491071513,-28.8124845454619,56.1684875207208));
#110692=CARTESIAN_POINT('Ctrl Pts',(5.60967768438927,-28.8127833460569,
56.1687911133795));
#110693=CARTESIAN_POINT('Ctrl Pts',(5.60969270139474,-28.812940409274,56.1689506311989));
#110694=CARTESIAN_POINT('Ctrl Pts',(5.60972446299037,-28.8132727039299,
56.1692879829594));
#110695=CARTESIAN_POINT('Ctrl Pts',(5.60974120723446,-28.8134479432009,
56.1694658091782));
#110696=CARTESIAN_POINT('Ctrl Pts',(5.609776766907,-28.8138202221092,56.1698434139914));
#110697=CARTESIAN_POINT('Ctrl Pts',(5.60979558187417,-28.8140172722958,
56.1700431822474));
#110698=CARTESIAN_POINT('Ctrl Pts',(5.60983572721639,-28.8144378741486,
56.1704693703758));
#110699=CARTESIAN_POINT('Ctrl Pts',(5.60985705695728,-28.8146614402658,
56.1706957760446));
#110700=CARTESIAN_POINT('Ctrl Pts',(5.60990281747921,-28.8151412793974,
56.1711814313325));
#110701=CARTESIAN_POINT('Ctrl Pts',(5.60992724736499,-28.8153975726833,
56.1714406609307));
#110702=CARTESIAN_POINT('Ctrl Pts',(5.60997999805565,-28.8159512476809,
56.1720003117833));
#110703=CARTESIAN_POINT('Ctrl Pts',(5.61000831756943,-28.8162486587638,
56.1723007040903));
#110704=CARTESIAN_POINT('Ctrl Pts',(5.61006994216472,-28.8168962036133,
56.1729542421939));
#110705=CARTESIAN_POINT('Ctrl Pts',(5.61010324530987,-28.817246381325,56.1733073445681));
#110706=CARTESIAN_POINT('Ctrl Pts',(5.61085603759109,-28.8251671191855,
56.1812870866818));
#110707=CARTESIAN_POINT('Ctrl Pts',(5.61157226006442,-28.8328112839442,
56.1888406072384));
#110708=CARTESIAN_POINT('Ctrl Pts',(5.61306852499768,-28.849005497753,56.2045360216964));
#110709=CARTESIAN_POINT('Ctrl Pts',(5.6138478569042,-28.8575701104603,56.2126620845613));
#110710=CARTESIAN_POINT('Ctrl Pts',(5.61590473699746,-28.8805136005019,
56.2339719310193));
#110711=CARTESIAN_POINT('Ctrl Pts',(5.61717549465498,-28.8950391533021,
56.246995631246));
#110712=CARTESIAN_POINT('Ctrl Pts',(5.62377386703542,-28.9722329712203,
56.3137998748662));
#110713=CARTESIAN_POINT('Ctrl Pts',(5.62891788108628,-29.0386105406685,
56.3631243445983));
#110714=CARTESIAN_POINT('Ctrl Pts',(5.64015274367635,-29.1931222854185,
56.4610161214553));
#110715=CARTESIAN_POINT('Ctrl Pts',(5.64618451687078,-29.282534900663,56.5069377021184));
#110716=CARTESIAN_POINT('Ctrl Pts',(5.65424663631671,-29.4017612085817,
56.5551421166367));
#110717=CARTESIAN_POINT('Ctrl Pts',(5.65604041854473,-29.4282585662594,
56.5650776999504));
#110718=CARTESIAN_POINT('Ctrl Pts',(5.65910934022343,-29.4732437429048,
56.5806507496122));
#110719=CARTESIAN_POINT('Ctrl Pts',(5.6603681344177,-29.4916005110858,56.5866501909058));
#110720=CARTESIAN_POINT('Ctrl Pts',(5.66218710212996,-29.5179111785148,
56.5947457183845));
#110721=CARTESIAN_POINT('Ctrl Pts',(5.66273321255146,-29.5257834974828,
56.5971043296673));
#110722=CARTESIAN_POINT('Ctrl Pts',(5.66368745794205,-29.5394850809295,
56.6010992050839));
#110723=CARTESIAN_POINT('Ctrl Pts',(5.6640940624055,-29.5453063370879,56.6027620930042));
#110724=CARTESIAN_POINT('Ctrl Pts',(5.66497150131107,-29.5578297581885,
56.6062657876622));
#110725=CARTESIAN_POINT('Ctrl Pts',(5.66544286142756,-29.5645343148914,
56.6080963702605));
#110726=CARTESIAN_POINT('Ctrl Pts',(5.66675315314743,-29.5831136469388,
56.6130444811773));
#110727=CARTESIAN_POINT('Ctrl Pts',(5.66759683176353,-29.5950114524396,
56.6160727037659));
#110728=CARTESIAN_POINT('Ctrl Pts',(5.67351202571793,-29.6780509161312,
56.6362333069588));
#110729=CARTESIAN_POINT('Ctrl Pts',(5.67878562004379,-29.7502132858333,
56.6487919432388));
#110730=CARTESIAN_POINT('Ctrl Pts',(5.68512836949179,-29.8370256572337,
56.6580698161686));
#110731=CARTESIAN_POINT('Ctrl Pts',(5.68615761361952,-29.8511115592374,
56.6593939797661));
#110732=CARTESIAN_POINT('Ctrl Pts',(5.69255120868608,-29.9386682830437,
56.6665010402185));
#110733=CARTESIAN_POINT('Ctrl Pts',(5.69791546578073,-30.0124433489972,
56.6675832123819));
#110734=CARTESIAN_POINT('Ctrl Pts',(5.70621078107003,-30.1285269737078,
56.6615793197355));
#110735=CARTESIAN_POINT('Ctrl Pts',(5.70920958744079,-30.1709057512181,
56.6577565400483));
#110736=CARTESIAN_POINT('Ctrl Pts',(5.714286943184,-30.2434584523678,56.6483996077296));
#110737=CARTESIAN_POINT('Ctrl Pts',(5.7163870211675,-30.2737099797993,56.6436472692005));
#110738=CARTESIAN_POINT('Ctrl Pts',(5.71940824637081,-30.3175626297166,
56.6355138246984));
#110739=CARTESIAN_POINT('Ctrl Pts',(5.72034986555627,-30.3312778175844,
56.6327910224048));
#110740=CARTESIAN_POINT('Ctrl Pts',(5.72200510951612,-30.3554655900278,
56.6276718283769));
#110741=CARTESIAN_POINT('Ctrl Pts',(5.7227209419347,-30.3659521586349,56.6253462380257));
#110742=CARTESIAN_POINT('Ctrl Pts',(5.72421810828184,-30.3879355752872,
56.6202474611963));
#110743=CARTESIAN_POINT('Ctrl Pts',(5.72499871513617,-30.3994268996737,
56.6174529390502));
#110744=CARTESIAN_POINT('Ctrl Pts',(5.72706296846563,-30.4298837392738,
56.6097018945165));
#110745=CARTESIAN_POINT('Ctrl Pts',(5.72833973478736,-30.4487935475131,
56.6045325246997));
#110746=CARTESIAN_POINT('Ctrl Pts',(5.73493283338865,-30.5467125119296,
56.5758978421885));
#110747=CARTESIAN_POINT('Ctrl Pts',(5.74006657953628,-30.6239961763504,
56.5469259290523));
#110748=CARTESIAN_POINT('Ctrl Pts',(5.75129050574025,-30.7898777544275,
56.4702754004316));
#110749=CARTESIAN_POINT('Ctrl Pts',(5.75732138034986,-30.8769380467955,
56.4200682856675));
#110750=CARTESIAN_POINT('Ctrl Pts',(5.76538241930614,-30.9820859161215,
56.346054901022));
#110751=CARTESIAN_POINT('Ctrl Pts',(5.76717608144822,-31.00480279622,56.3291830962633));
#110752=CARTESIAN_POINT('Ctrl Pts',(5.77024481841223,-31.0422823480289,
56.2998370728428));
#110753=CARTESIAN_POINT('Ctrl Pts',(5.7715035505377,-31.0572780142117,56.2876692244578));
#110754=CARTESIAN_POINT('Ctrl Pts',(5.77332244408069,-31.0783484961954,
56.2699559268684));
#110755=CARTESIAN_POINT('Ctrl Pts',(5.77386854396232,-31.0845996045342,
56.2646213766478));
#110756=CARTESIAN_POINT('Ctrl Pts',(5.77482277746939,-31.0953869776575,
56.2552768715058));
#110757=CARTESIAN_POINT('Ctrl Pts',(5.77522938070761,-31.099941265392,56.2512880828584));
#110758=CARTESIAN_POINT('Ctrl Pts',(5.77610682474372,-31.1096771757829,
56.2426668379674));
#110759=CARTESIAN_POINT('Ctrl Pts',(5.77657819129145,-31.1148515049855,
56.2380268260678));
#110760=CARTESIAN_POINT('Ctrl Pts',(5.77788851790048,-31.1290857562103,
56.2251008508895));
#110761=CARTESIAN_POINT('Ctrl Pts',(5.77873222536627,-31.1380831339001,
56.2167470969534));
#110762=CARTESIAN_POINT('Ctrl Pts',(5.7846550842979,-31.200138735104,56.1578401489165));
#110763=CARTESIAN_POINT('Ctrl Pts',(5.78993692096085,-31.2498976765032,
56.1039385001513));
#110764=CARTESIAN_POINT('Ctrl Pts',(5.79628205926844,-31.3047821960186,
56.0360006440789));
#110765=CARTESIAN_POINT('Ctrl Pts',(5.79730553951035,-31.3134838791567,
56.0249458566415));
#110766=CARTESIAN_POINT('Ctrl Pts',(5.80369405025996,-31.3668958921132,
55.9552927763773));
#110767=CARTESIAN_POINT('Ctrl Pts',(5.80905892901138,-31.4078192001801,
55.8938876217719));
#110768=CARTESIAN_POINT('Ctrl Pts',(5.81735308261318,-31.4657204185634,
55.7931120445557));
#110769=CARTESIAN_POINT('Ctrl Pts',(5.82035020426002,-31.4854807608247,
55.7554538187264));
#110770=CARTESIAN_POINT('Ctrl Pts',(5.8254250576153,-31.5169523577242,55.6894549235681));
#110771=CARTESIAN_POINT('Ctrl Pts',(5.82752428912979,-31.5293615715799,
55.6614725573775));
#110772=CARTESIAN_POINT('Ctrl Pts',(5.83054454148244,-31.5463066077674,
55.6202316588876));
#110773=CARTESIAN_POINT('Ctrl Pts',(5.83148601565894,-31.5514568050176,
55.6072340889345));
#110774=CARTESIAN_POINT('Ctrl Pts',(5.8331410961117,-31.5602735301203,55.5841385726384));
#110775=CARTESIAN_POINT('Ctrl Pts',(5.83385690855483,-31.5640070815287,
55.5740672600437));
#110776=CARTESIAN_POINT('Ctrl Pts',(5.83535412230743,-31.5716465267158,
55.5528318604387));
#110777=CARTESIAN_POINT('Ctrl Pts',(5.83613479568354,-31.5755314737361,
55.5416608332368));
#110778=CARTESIAN_POINT('Ctrl Pts',(5.83819943370811,-31.5855398434333,
55.5118630838176));
#110779=CARTESIAN_POINT('Ctrl Pts',(5.83947651351413,-31.5914540856422,
55.4931676769893));
#110780=CARTESIAN_POINT('Ctrl Pts',(5.8460803395214,-31.6205504057329,55.3952109121176));
#110781=CARTESIAN_POINT('Ctrl Pts',(5.85122370793894,-31.6381472094588,
55.3144065706583));
#110782=CARTESIAN_POINT('Ctrl Pts',(5.86244827180834,-31.6636651722821,
55.1334411910619));
#110783=CARTESIAN_POINT('Ctrl Pts',(5.86847103463282,-31.6686770886506,
55.0332082588864));
#110784=CARTESIAN_POINT('Ctrl Pts',(5.87652231881853,-31.6635230087185,
54.9048856614526));
#110785=CARTESIAN_POINT('Ctrl Pts',(5.87831489579065,-31.6616691669251,
54.8766673709718));
#110786=CARTESIAN_POINT('Ctrl Pts',(5.88138196348994,-31.6573432045811,
54.8292895122289));
#110787=CARTESIAN_POINT('Ctrl Pts',(5.88264013464415,-31.6552542495464,
54.810100395298));
#110788=CARTESIAN_POINT('Ctrl Pts',(5.88445835783913,-31.6518015172962,
54.7828013380675));
#110789=CARTESIAN_POINT('Ctrl Pts',(5.88500436244594,-31.6507102573269,
54.7746577033895));
#110790=CARTESIAN_POINT('Ctrl Pts',(5.88595848854139,-31.6487103898355,
54.760528283153));
#110791=CARTESIAN_POINT('Ctrl Pts',(5.88636508071307,-31.6478293204928,
54.7545388383054));
#110792=CARTESIAN_POINT('Ctrl Pts',(5.88724257116995,-31.6458664996866,
54.741682789144));
#110793=CARTESIAN_POINT('Ctrl Pts',(5.8877139958863,-31.6447744323901,54.7348182163806));
#110794=CARTESIAN_POINT('Ctrl Pts',(5.88902463806697,-31.6416340616574,
54.7158443406801));
#110795=CARTESIAN_POINT('Ctrl Pts',(5.88986860648203,-31.639494811816,54.7037508295164));
#110796=CARTESIAN_POINT('Ctrl Pts',(5.89586299519639,-31.623469138227,54.6186515736115));
#110797=CARTESIAN_POINT('Ctrl Pts',(5.90122179749431,-31.604846489722,54.5466304369187));
#110798=CARTESIAN_POINT('Ctrl Pts',(5.90758332847298,-31.5773165755554,
54.4635264158598));
#110799=CARTESIAN_POINT('Ctrl Pts',(5.90854712647041,-31.5730010040137,
54.4510015260347));
#110800=CARTESIAN_POINT('Ctrl Pts',(5.91487932650507,-31.5436805226036,
54.369091174738));
#110801=CARTESIAN_POINT('Ctrl Pts',(5.920247202629,-31.5142393507344,54.3013756282619));
#110802=CARTESIAN_POINT('Ctrl Pts',(5.92853306006111,-31.4609744777292,
54.198186917614));
#110803=CARTESIAN_POINT('Ctrl Pts',(5.93151947819228,-31.440113129539,54.1612954539647));
#110804=CARTESIAN_POINT('Ctrl Pts',(5.93657842741133,-31.4018380147697,
54.0992569491608));
#110805=CARTESIAN_POINT('Ctrl Pts',(5.93867227575047,-31.3850977001122,
54.0737211886202));
#110806=CARTESIAN_POINT('Ctrl Pts',(5.94168634001977,-31.3596887748554,
54.0371929070712));
#110807=CARTESIAN_POINT('Ctrl Pts',(5.94262689100957,-31.3515693821288,
54.0258278958099));
#110808=CARTESIAN_POINT('Ctrl Pts',(5.94428093089611,-31.3369557741545,
54.0059071560768));
#110809=CARTESIAN_POINT('Ctrl Pts',(5.94499661655691,-31.330520038534,53.9973097383904));
#110810=CARTESIAN_POINT('Ctrl Pts',(5.94649413411054,-31.3168188840876,
53.9793707550318));
#110811=CARTESIAN_POINT('Ctrl Pts',(5.94727523258584,-31.3095361349709,
53.9700431307374));
#110812=CARTESIAN_POINT('Ctrl Pts',(5.94934232894496,-31.2899048585016,
53.945444594442));
#110813=CARTESIAN_POINT('Ctrl Pts',(5.95062141199184,-31.2773844271271,
53.9303127907655));
#110814=CARTESIAN_POINT('Ctrl Pts',(5.95729865268596,-31.2101163073132,
53.8518805455481));
#110815=CARTESIAN_POINT('Ctrl Pts',(5.96250795019032,-31.1509212589895,
53.7925470707537));
#110816=CARTESIAN_POINT('Ctrl Pts',(5.97373728748757,-31.0123609009764,
53.6731533349377));
#110817=CARTESIAN_POINT('Ctrl Pts',(5.97970471808478,-30.9315827223317,
53.6152444322808));
#110818=CARTESIAN_POINT('Ctrl Pts',(5.9876894205928,-30.8218868791671,53.550568867974));
#110819=CARTESIAN_POINT('Ctrl Pts',(5.98947454141996,-30.7972771096186,
53.5368876732036));
#110820=CARTESIAN_POINT('Ctrl Pts',(5.99253013626929,-30.755285132068,53.5149173087543));
#110821=CARTESIAN_POINT('Ctrl Pts',(5.99378444915729,-30.7380839028855,
53.5062937686262));
#110822=CARTESIAN_POINT('Ctrl Pts',(5.99559806116517,-30.7133393859499,
53.4944202892037));
#110823=CARTESIAN_POINT('Ctrl Pts',(5.99614340965538,-30.7059147286573,
53.4909248746346));
#110824=CARTESIAN_POINT('Ctrl Pts',(5.99709679651142,-30.6929694988752,
53.4849468949833));
#110825=CARTESIAN_POINT('Ctrl Pts',(5.99750331293053,-30.6874607307519,
53.4824393324454));
#110826=CARTESIAN_POINT('Ctrl Pts',(5.99838112511672,-30.6755910058959,
53.4771141904084));
#110827=CARTESIAN_POINT('Ctrl Pts',(5.9988529520233,-30.6692261260914,53.4743064580192));
#110828=CARTESIAN_POINT('Ctrl Pts',(6.00016577682306,-30.6515529495901,
53.4666421755225));
#110829=CARTESIAN_POINT('Ctrl Pts',(6.00101155022345,-30.6402084028865,
53.4618710578713));
#110830=CARTESIAN_POINT('Ctrl Pts',(6.00731587880736,-30.5558766721878,
53.4274986535648));
#110831=CARTESIAN_POINT('Ctrl Pts',(6.01300815964939,-30.4809323685515,
53.4029838221265));
#110832=CARTESIAN_POINT('Ctrl Pts',(6.01922058563892,-30.3980606676793,
53.3822397000027));
#110833=CARTESIAN_POINT('Ctrl Pts',(6.01970692183623,-30.3915664723031,
53.3806555706626));
#110834=CARTESIAN_POINT('Ctrl Pts',(6.02415494514287,-30.3321005371325,
53.3665286802304));
#110835=CARTESIAN_POINT('Ctrl Pts',(6.02812082550603,-30.278551673164,53.356549778747));
#110836=CARTESIAN_POINT('Ctrl Pts',(6.03600709162865,-30.1701402319231,
53.3417991408803));
#110837=CARTESIAN_POINT('Ctrl Pts',(6.03992186653345,-30.1153338575021,
53.3370878335869));
#110838=CARTESIAN_POINT('Ctrl Pts',(6.04551237462032,-30.0353478865128,
53.3341865434709));
#110839=CARTESIAN_POINT('Ctrl Pts',(6.04724676363678,-30.0102871466204,
53.3338432744814));
#110840=CARTESIAN_POINT('Ctrl Pts',(6.05037056930551,-29.9647050938863,
53.3342474817267));
#110841=CARTESIAN_POINT('Ctrl Pts',(6.05176532567895,-29.9441875297688,
53.33480865484));
#110842=CARTESIAN_POINT('Ctrl Pts',(6.05395834424886,-29.9116763066197,
53.3362994767213));
#110843=CARTESIAN_POINT('Ctrl Pts',(6.05476427279886,-29.8996739093941,
53.3369800979448));
#110844=CARTESIAN_POINT('Ctrl Pts',(6.05627983430849,-29.8770046672131,
53.3385119248834));
#110845=CARTESIAN_POINT('Ctrl Pts',(6.05699027314522,-29.8663366719089,
53.3393360967718));
#110846=CARTESIAN_POINT('Ctrl Pts',(6.05859807031123,-29.8421046495762,
53.3414431985336));
#110847=CARTESIAN_POINT('Ctrl Pts',(6.05949338946172,-29.8285468235387,
53.3427898648737));
#110848=CARTESIAN_POINT('Ctrl Pts',(6.06182330440288,-29.7931125650952,
53.3467489825772));
#110849=CARTESIAN_POINT('Ctrl Pts',(6.06324954091493,-29.7712683391104,
53.3496293637383));
#110850=CARTESIAN_POINT('Ctrl Pts',(6.07186433091572,-29.6385802226222,
53.3698108794264));
#110851=CARTESIAN_POINT('Ctrl Pts',(6.07870358396223,-29.5296578724719,
53.3978381298946));
#110852=CARTESIAN_POINT('Ctrl Pts',(6.09153487111977,-29.3324868948639,
53.4704349467432));
#110853=CARTESIAN_POINT('Ctrl Pts',(6.09750814091866,-29.2437774161109,
53.5122953460405));
#110854=CARTESIAN_POINT('Ctrl Pts',(6.10480659976119,-29.1469282496465,
53.5689063882489));
#110855=CARTESIAN_POINT('Ctrl Pts',(6.10574485994584,-29.13468111709,53.5762782806325));
#110856=CARTESIAN_POINT('Ctrl Pts',(6.10717665247066,-29.1163276266195,
53.5876500471782));
#110857=CARTESIAN_POINT('Ctrl Pts',(6.10766306661534,-29.110149854637,53.5915341798626));
#110858=CARTESIAN_POINT('Ctrl Pts',(6.10855483075937,-29.0989327856324,
53.5986899087401));
#110859=CARTESIAN_POINT('Ctrl Pts',(6.10895933054403,-29.0938854069513,
53.6019483423882));
#110860=CARTESIAN_POINT('Ctrl Pts',(6.10988720756494,-29.0823994873474,
53.6094516294687));
#110861=CARTESIAN_POINT('Ctrl Pts',(6.11041169872084,-29.0759727463843,
53.6137139183153));
#110862=CARTESIAN_POINT('Ctrl Pts',(6.11206255344805,-29.0559421252614,
53.6271996261016));
#110863=CARTESIAN_POINT('Ctrl Pts',(6.11319842191964,-29.0424454687913,
53.6365795195112));
#110864=CARTESIAN_POINT('Ctrl Pts',(6.12047377225749,-28.9576596554269,
53.6973837360031));
#110865=CARTESIAN_POINT('Ctrl Pts',(6.12687424672248,-28.8904015227084,
53.7541786006832));
#110866=CARTESIAN_POINT('Ctrl Pts',(6.13683052997786,-28.7931992036148,
53.8504009581148));
#110867=CARTESIAN_POINT('Ctrl Pts',(6.1403855256211,-28.7599845347559,53.886308807245));
#110868=CARTESIAN_POINT('Ctrl Pts',(6.1477139866559,-28.6942052960615,53.9640189361251));
#110869=CARTESIAN_POINT('Ctrl Pts',(6.15147701261901,-28.6619558355591,
54.0060204825314));
#110870=CARTESIAN_POINT('Ctrl Pts',(6.15766505398325,-28.6113629031833,
54.078848059903));
#110871=CARTESIAN_POINT('Ctrl Pts',(6.16012665094559,-28.5919166921978,
54.1088571276642));
#110872=CARTESIAN_POINT('Ctrl Pts',(6.16355892471389,-28.5657929311301,
54.1521640309832));
#110873=CARTESIAN_POINT('Ctrl Pts',(6.16455874167893,-28.5583055994359,
54.164959266376));
#110874=CARTESIAN_POINT('Ctrl Pts',(6.16628070563613,-28.5456277408097,
54.1873036261058));
#110875=CARTESIAN_POINT('Ctrl Pts',(6.16700566154838,-28.5403581294968,
54.1968065712734));
#110876=CARTESIAN_POINT('Ctrl Pts',(6.16839805906141,-28.5303706252655,
54.2152404824255));
#110877=CARTESIAN_POINT('Ctrl Pts',(6.16906592017479,-28.5256402519568,
54.2241641021098));
#110878=CARTESIAN_POINT('Ctrl Pts',(6.17083171466432,-28.5132964637648,
54.2479707179044));
#110879=CARTESIAN_POINT('Ctrl Pts',(6.17192464300019,-28.505825278829,54.2629264747883));
#110880=CARTESIAN_POINT('Ctrl Pts',(6.17599584452797,-28.4786538508444,
54.3194296620581));
#110881=CARTESIAN_POINT('Ctrl Pts',(6.17892318451078,-28.4604502161505,
54.3616763106675));
#110882=CARTESIAN_POINT('Ctrl Pts',(6.18884420582201,-28.4039406497918,
54.5093613396289));
#110883=CARTESIAN_POINT('Ctrl Pts',(6.19558337341051,-28.3745425837921,
54.6178738685986));
#110884=CARTESIAN_POINT('Ctrl Pts',(6.20541139166293,-28.3485115738653,
54.775483142563));
#110885=CARTESIAN_POINT('Ctrl Pts',(6.20836765990743,-28.3427717103106,
54.8227554954057));
#110886=CARTESIAN_POINT('Ctrl Pts',(6.21316097342454,-28.3369079177467,
54.8977922593837));
#110887=CARTESIAN_POINT('Ctrl Pts',(6.21494782603538,-28.3354398956936,
54.9254269200532));
#110888=CARTESIAN_POINT('Ctrl Pts',(6.21738873238108,-28.3343956212004,
54.9624941711237));
#110889=CARTESIAN_POINT('Ctrl Pts',(6.21801237348241,-28.3342102786804,
54.9719067991632));
#110890=CARTESIAN_POINT('Ctrl Pts',(6.21905789948024,-28.3340345366733,
54.9875797750158));
#110891=CARTESIAN_POINT('Ctrl Pts',(6.21947737096312,-28.3339996295805,
54.9938395881387));
#110892=CARTESIAN_POINT('Ctrl Pts',(6.22033482441398,-28.3340003891752,
55.0065742263296));
#110893=CARTESIAN_POINT('Ctrl Pts',(6.22077292106741,-28.3340385218274,
55.013048883104));
#110894=CARTESIAN_POINT('Ctrl Pts',(6.22192129714633,-28.3342365019233,
55.0299423925286));
#110895=CARTESIAN_POINT('Ctrl Pts',(6.22263472928739,-28.3344563561875,
55.0403600674017));
#110896=CARTESIAN_POINT('Ctrl Pts',(6.225923420595,-28.3359107794599,55.0880599199513));
#110897=CARTESIAN_POINT('Ctrl Pts',(6.22855209853136,-28.3382994949583,
55.1252934070511));
#110898=CARTESIAN_POINT('Ctrl Pts',(6.23683765239157,-28.3496118538595,
55.2407813463081));
#110899=CARTESIAN_POINT('Ctrl Pts',(6.24259886493134,-28.3628346246,55.3185050089652));
#110900=CARTESIAN_POINT('Ctrl Pts',(6.25289732980732,-28.3964364415772,
55.4561873285643));
#110901=CARTESIAN_POINT('Ctrl Pts',(6.25743981058664,-28.4148214150369,
55.5164549297136));
#110902=CARTESIAN_POINT('Ctrl Pts',(6.26189393505974,-28.4365622331338,
55.5755157244911));
#110903=CARTESIAN_POINT('',(6.02851963656333,-28.3340006962934,54.9984768292002));
#110904=CARTESIAN_POINT('Ctrl Pts',(6.06643884243078,-28.4365623175998,
55.5755159539501));
#110905=CARTESIAN_POINT('Ctrl Pts',(6.06476015297658,-28.4282202681816,
55.5528540723474));
#110906=CARTESIAN_POINT('Ctrl Pts',(6.06309642773074,-28.4203703265032,
55.5300091476633));
#110907=CARTESIAN_POINT('Ctrl Pts',(6.06024616305704,-28.4076552517071,
55.4902089456295));
#110908=CARTESIAN_POINT('Ctrl Pts',(6.05905255999884,-28.4025584563348,
55.4733362058938));
#110909=CARTESIAN_POINT('Ctrl Pts',(6.05710091519478,-28.394605925368,55.4454165873849));
#110910=CARTESIAN_POINT('Ctrl Pts',(6.05633787123136,-28.3915943141442,
55.4344159666343));
#110911=CARTESIAN_POINT('Ctrl Pts',(6.05485285341196,-28.3859263311193,
55.4128449529414));
#110912=CARTESIAN_POINT('Ctrl Pts',(6.05413059942039,-28.3832602559977,
55.402277731802));
#110913=CARTESIAN_POINT('Ctrl Pts',(6.05270061135005,-28.3781640856808,
55.3812091665214));
#110914=CARTESIAN_POINT('Ctrl Pts',(6.05199283979134,-28.3757318316159,
55.3707088990512));
#110915=CARTESIAN_POINT('Ctrl Pts',(6.0503374763543,-28.3702574687587,55.3459866700841));
#110916=CARTESIAN_POINT('Ctrl Pts',(6.0493925421128,-28.3672993157626,55.3317468778488));
#110917=CARTESIAN_POINT('Ctrl Pts',(6.04631836623588,-28.3582307013777,
55.2850291581921));
#110918=CARTESIAN_POINT('Ctrl Pts',(6.0442127279856,-28.3528998070025,55.2524068598318));
#110919=CARTESIAN_POINT('Ctrl Pts',(6.03746967039496,-28.3387916277564,
55.1463313002844));
#110920=CARTESIAN_POINT('Ctrl Pts',(6.03293646769578,-28.3339333426273,
55.0724469474433));
#110921=CARTESIAN_POINT('Ctrl Pts',(6.02841828083449,-28.3340006906443,
54.9984830206473));
#110922=CARTESIAN_POINT('Ctrl Pts',(6.02851963656333,-28.3340006962934,
54.9984768292002));
#110923=CARTESIAN_POINT('Ctrl Pts',(6.02319560874774,-28.3340734949223,
54.9188518357346));
#110924=CARTESIAN_POINT('Ctrl Pts',(6.01787158093214,-28.3398584615716,
54.8394810237176));
#110925=CARTESIAN_POINT('Ctrl Pts',(6.01254755311655,-28.3512247100071,
54.7610522167735));
#110926=CARTESIAN_POINT('Ctrl Pts',(6.0087999105051,-28.3592255391622,54.7058453040658));
#110927=CARTESIAN_POINT('Ctrl Pts',(6.00505226789365,-28.3699908306221,
54.6511044996732));
#110928=CARTESIAN_POINT('Ctrl Pts',(6.0013046252822,-28.3834612365896,54.597062751298));
#110929=CARTESIAN_POINT('Ctrl Pts',(5.99722727558209,-28.3981167311034,
54.5382665614325));
#110930=CARTESIAN_POINT('Ctrl Pts',(5.99314992588198,-28.4160144422306,
54.4801495795245));
#110931=CARTESIAN_POINT('Ctrl Pts',(5.98907257618187,-28.4370742327443,
54.423095288589));
#110932=CARTESIAN_POINT('Ctrl Pts',(5.98495160860944,-28.4583593125565,
54.3654306534446));
#110933=CARTESIAN_POINT('Ctrl Pts',(5.98083064103702,-28.4828744868665,
54.3088521143314));
#110934=CARTESIAN_POINT('Ctrl Pts',(5.97670967346459,-28.5104841015491,
54.2537437516094));
#110935=CARTESIAN_POINT('Ctrl Pts',(5.97264355643919,-28.5377262291206,
54.1993688874621));
#110936=CARTESIAN_POINT('Ctrl Pts',(5.96857743941378,-28.5679806888336,
54.1464257733204));
#110937=CARTESIAN_POINT('Ctrl Pts',(5.96451132238838,-28.6010683663903,
54.0952645223679));
#110938=CARTESIAN_POINT('Ctrl Pts',(5.96044769316901,-28.6341357996394,
54.044134573827));
#110939=CARTESIAN_POINT('Ctrl Pts',(5.95638406394963,-28.6700327363164,
53.994784755908));
#110940=CARTESIAN_POINT('Ctrl Pts',(5.95232043473026,-28.7085351232835,
53.9475388500246));
#110941=CARTESIAN_POINT('Ctrl Pts',(5.94825778211358,-28.7470282570601,
53.9003042986414));
#110942=CARTESIAN_POINT('Ctrl Pts',(5.94419512949691,-28.7881252748301,
53.8551730522363));
#110943=CARTESIAN_POINT('Ctrl Pts',(5.94013247688023,-28.8315612467165,
53.8124365786093));
#110944=CARTESIAN_POINT('Ctrl Pts',(5.93596888334385,-28.8760764314631,
53.7686382718994));
#110945=CARTESIAN_POINT('Ctrl Pts',(5.93180528980747,-28.9230479927169,
53.7273557654103));
#110946=CARTESIAN_POINT('Ctrl Pts',(5.92764169627109,-28.9721516994875,
53.6888616125162));
#110947=CARTESIAN_POINT('Ctrl Pts',(5.92357385644511,-29.0201261264481,
53.6512527424761));
#110948=CARTESIAN_POINT('Ctrl Pts',(5.91950601661914,-29.0701351964334,
53.6163055754419));
#110949=CARTESIAN_POINT('Ctrl Pts',(5.91543817679316,-29.1218462435001,
53.5842309581202));
#110950=CARTESIAN_POINT('Ctrl Pts',(5.91122670640158,-29.1753831458749,
53.551023824371));
#110951=CARTESIAN_POINT('Ctrl Pts',(5.90701523600999,-29.230743959214,53.520896213991));
#110952=CARTESIAN_POINT('Ctrl Pts',(5.90280376561841,-29.2875334118817,
53.4940294289678));
#110953=CARTESIAN_POINT('Ctrl Pts',(5.89859229522682,-29.3443228645495,
53.4671626439445));
#110954=CARTESIAN_POINT('Ctrl Pts',(5.89438082483524,-29.4025403724669,
53.4435568429065));
#110955=CARTESIAN_POINT('Ctrl Pts',(5.89016935444365,-29.4617725659754,
53.4233366785318));
#110956=CARTESIAN_POINT('Ctrl Pts',(5.88609200474354,-29.5191184200318,
53.4037604561002));
#110957=CARTESIAN_POINT('Ctrl Pts',(5.88201465504343,-29.5776521037462,
53.3872765390742));
#110958=CARTESIAN_POINT('Ctrl Pts',(5.87793730534331,-29.6370079727799,
53.3740255880935));
#110959=CARTESIAN_POINT('Ctrl Pts',(5.87381633777089,-29.6969988073934,
53.3606328836871));
#110960=CARTESIAN_POINT('Ctrl Pts',(5.86969537019846,-29.7578290526706,
53.3505429818469));
#110961=CARTESIAN_POINT('Ctrl Pts',(5.86557440262604,-29.8191024520456,
53.3438502250267));
#110962=CARTESIAN_POINT('Ctrl Pts',(5.86150828560063,-29.879560295507,53.3372465495609));
#110963=CARTESIAN_POINT('Ctrl Pts',(5.85744216857522,-29.9404490441909,
53.3339501953221));
#110964=CARTESIAN_POINT('Ctrl Pts',(5.85337605154982,-30.0013774075988,
53.3340005694034));
#110965=CARTESIAN_POINT('Ctrl Pts',(5.84931242233044,-30.062268492702,53.3340509126639));
#110966=CARTESIAN_POINT('Ctrl Pts',(5.84524879311107,-30.1231986335689,
53.3374439239197));
#110967=CARTESIAN_POINT('Ctrl Pts',(5.84118516389169,-30.1837742889552,
53.3441669737806));
#110968=CARTESIAN_POINT('Ctrl Pts',(5.83712251127501,-30.2443353863331,
53.3508884079063));
#110969=CARTESIAN_POINT('Ctrl Pts',(5.83305985865833,-30.3045416587428,
53.3609382354768));
#110970=CARTESIAN_POINT('Ctrl Pts',(5.82899720604165,-30.3640045429392,
53.3742519590294));
#110971=CARTESIAN_POINT('Ctrl Pts',(5.82483361250527,-30.4249448456562,
53.3878964761859));
#110972=CARTESIAN_POINT('Ctrl Pts',(5.82067001896889,-30.4851037654212,
53.4049691819279));
#110973=CARTESIAN_POINT('Ctrl Pts',(5.81650642543251,-30.5440764670278,
53.425345498839));
#110974=CARTESIAN_POINT('Ctrl Pts',(5.81243858560653,-30.6016929231359,
53.4452532042175));
#110975=CARTESIAN_POINT('Ctrl Pts',(5.80837074578055,-30.6581766839123,
53.4683139139434));
#110976=CARTESIAN_POINT('Ctrl Pts',(5.80430290595458,-30.7131701817946,
53.4943624965487));
#110977=CARTESIAN_POINT('Ctrl Pts',(5.800091435563,-30.7701054344026,53.5213308234932));
#110978=CARTESIAN_POINT('Ctrl Pts',(5.79587996517141,-30.8254426690907,
53.5515017203613));
#110979=CARTESIAN_POINT('Ctrl Pts',(5.79166849477983,-30.8788151850231,
53.5846414339211));
#110980=CARTESIAN_POINT('Ctrl Pts',(5.78745702438825,-30.9321877009555,
53.6177811474809));
#110981=CARTESIAN_POINT('Ctrl Pts',(5.78324555399667,-30.9835950480778,
53.6538892730566));
#110982=CARTESIAN_POINT('Ctrl Pts',(5.77903408360509,-31.0327083033889,
53.6926861279281));
#110983=CARTESIAN_POINT('Ctrl Pts',(5.77495673390497,-31.0802574722526,
53.7302474378429));
#110984=CARTESIAN_POINT('Ctrl Pts',(5.77087938420486,-31.1258528967952,
53.7704838505866));
#110985=CARTESIAN_POINT('Ctrl Pts',(5.76680203450474,-31.1691780895288,
53.8131644617026));
#110986=CARTESIAN_POINT('Ctrl Pts',(5.76268106693232,-31.2129667580159,
53.8563016530932));
#110987=CARTESIAN_POINT('Ctrl Pts',(5.75856009935989,-31.2544358643991,
53.901935391439));
#110988=CARTESIAN_POINT('Ctrl Pts',(5.75443913178747,-31.2932912321435,
53.9497839322974));
#110989=CARTESIAN_POINT('Ctrl Pts',(5.75037301476206,-31.3316294305246,
53.9969956036356));
#110990=CARTESIAN_POINT('Ctrl Pts',(5.74630689773665,-31.367422711798,54.0463630694734));
#110991=CARTESIAN_POINT('Ctrl Pts',(5.74224078071125,-31.4004257464349,
54.0975789626109));
#110992=CARTESIAN_POINT('Ctrl Pts',(5.73817715149187,-31.4334085885519,
54.1487635199047));
#110993=CARTESIAN_POINT('Ctrl Pts',(5.73411352227249,-31.4636042921283,
54.2017938327171));
#110994=CARTESIAN_POINT('Ctrl Pts',(5.73004989305312,-31.4908100250276,
54.2563324201788));
#110995=CARTESIAN_POINT('Ctrl Pts',(5.72598724043644,-31.5180092196355,
54.3108579005068));
#110996=CARTESIAN_POINT('Ctrl Pts',(5.72192458781976,-31.5422196416114,
54.3668904779901));
#110997=CARTESIAN_POINT('Ctrl Pts',(5.71786193520308,-31.563284735334,54.4240687226138));
#110998=CARTESIAN_POINT('Ctrl Pts',(5.7136983416667,-31.5848732136859,54.4826676214612));
#110999=CARTESIAN_POINT('Ctrl Pts',(5.70953474813032,-31.6031577274303,
54.5424693728216));
#111000=CARTESIAN_POINT('Ctrl Pts',(5.70537115459394,-31.6180233714046,
54.6030662906877));
#111001=CARTESIAN_POINT('Ctrl Pts',(5.70130331476796,-31.6325471374902,
54.6622696095692));
#111002=CARTESIAN_POINT('Ctrl Pts',(5.69723547494198,-31.6438075940157,
54.7222313780834));
#111003=CARTESIAN_POINT('Ctrl Pts',(5.69316763511601,-31.6517495433165,
54.7825616267683));
#111004=CARTESIAN_POINT('Ctrl Pts',(5.68895616472443,-31.6599719133613,
54.8450220644754));
#111005=CARTESIAN_POINT('Ctrl Pts',(5.68474469433285,-31.6646369573865,
54.9078768966285));
#111006=CARTESIAN_POINT('Ctrl Pts',(5.68053322394127,-31.6657421763009,
54.9706912625246));
#111007=CARTESIAN_POINT('Ctrl Pts',(5.67632175354969,-31.6668473952153,
55.0335056284207));
#111008=CARTESIAN_POINT('Ctrl Pts',(5.67211028315811,-31.6643928849112,
55.0962789304679));
#111009=CARTESIAN_POINT('Ctrl Pts',(5.66789881276653,-31.6584352230018,
55.1585831362628));
#111010=CARTESIAN_POINT('Ctrl Pts',(5.66382146306642,-31.6526672919133,
55.2189031696937));
#111011=CARTESIAN_POINT('Ctrl Pts',(5.6597441133663,-31.6435922496631,55.2790326571175));
#111012=CARTESIAN_POINT('Ctrl Pts',(5.65566676366619,-31.6312324376959,
55.3385804693257));
#111013=CARTESIAN_POINT('Ctrl Pts',(5.65154579609376,-31.6187404053552,
55.3987653004457));
#111014=CARTESIAN_POINT('Ctrl Pts',(5.64742482852134,-31.6028928679926,
55.4583554038117));
#111015=CARTESIAN_POINT('Ctrl Pts',(5.64330386094891,-31.5837669805994,
55.516950820836));
#111016=CARTESIAN_POINT('Ctrl Pts',(5.63923774392351,-31.5648956609425,
55.5747663261962));
#111017=CARTESIAN_POINT('Ctrl Pts',(5.6351716268981,-31.5428328927836,55.6316129613537));
#111018=CARTESIAN_POINT('Ctrl Pts',(5.6311055098727,-31.5177038507705,55.6871179093549));
#111019=CARTESIAN_POINT('Ctrl Pts',(5.62704188065332,-31.4925901836672,
55.7425888973045));
#111020=CARTESIAN_POINT('Ctrl Pts',(5.62297825143395,-31.4644141731088,
55.7967193602663));
#111021=CARTESIAN_POINT('Ctrl Pts',(5.61891462221457,-31.4333493426076,
55.8491558526245));
#111022=CARTESIAN_POINT('Ctrl Pts',(5.61485196959789,-31.4022919778458,
55.9015797430408));
#111023=CARTESIAN_POINT('Ctrl Pts',(5.61078931698121,-31.3683474321821,
55.9523100307528));
#111024=CARTESIAN_POINT('Ctrl Pts',(5.60672666436453,-31.3317344485686,
56.0010191599044));
#111025=CARTESIAN_POINT('Ctrl Pts',(5.60256307082815,-31.2942117764861,
56.0509385191097));
#111026=CARTESIAN_POINT('Ctrl Pts',(5.59839947729177,-31.2538865838703,
56.0987344577357));
#111027=CARTESIAN_POINT('Ctrl Pts',(5.59423588375539,-31.2110390650608,
56.1440893247019));
#111028=CARTESIAN_POINT('Ctrl Pts',(5.59016804392942,-31.1691769471728,
56.1884011271232));
#111029=CARTESIAN_POINT('Ctrl Pts',(5.58610020410344,-31.1249077208064,
56.2303826368797));
#111030=CARTESIAN_POINT('Ctrl Pts',(5.58203236427746,-31.0785290790624,
56.2697759745785));
#111031=CARTESIAN_POINT('Ctrl Pts',(5.57782089388588,-31.0305128628733,
56.3105602439798));
#111032=CARTESIAN_POINT('Ctrl Pts',(5.5736094234943,-30.9802359328576,56.3485697542235));
#111033=CARTESIAN_POINT('Ctrl Pts',(5.56939795310271,-30.9280622790166,
56.3835665528866));
#111034=CARTESIAN_POINT('Ctrl Pts',(5.56518648271113,-30.8758886251756,
56.4185633515496));
#111035=CARTESIAN_POINT('Ctrl Pts',(5.56097501231955,-30.8218188015808,
56.4505471950831));
#111036=CARTESIAN_POINT('Ctrl Pts',(5.55676354192797,-30.7662431025641,
56.4793334674011));
#111037=CARTESIAN_POINT('Ctrl Pts',(5.55268619222785,-30.712437296361,56.5072029970166));
#111038=CARTESIAN_POINT('Ctrl Pts',(5.54860884252774,-30.6569979178377,
56.5321907331816));
#111039=CARTESIAN_POINT('Ctrl Pts',(5.54453149282763,-30.6002656888766,
56.5541033114814));
#111040=CARTESIAN_POINT('Ctrl Pts',(5.5404105252552,-30.5429265609982,56.5762503018657));
#111041=CARTESIAN_POINT('Ctrl Pts',(5.53628955768277,-30.4842671843989,
56.595255627346));
#111042=CARTESIAN_POINT('Ctrl Pts',(5.53216859011035,-30.4246654278063,
56.6109671860178));
#111043=CARTESIAN_POINT('Ctrl Pts',(5.52810247308494,-30.3658569773717,
56.626469622057));
#111044=CARTESIAN_POINT('Ctrl Pts',(5.52403635605954,-30.3061315899491,
56.6387653027936));
#111045=CARTESIAN_POINT('Ctrl Pts',(5.51997023903413,-30.2458703755336,
56.6477571903757));
#111046=CARTESIAN_POINT('Ctrl Pts',(5.51590660981475,-30.1856460312356,
56.6567435763768));
#111047=CARTESIAN_POINT('Ctrl Pts',(5.51184298059538,-30.1248870152639,
56.6624301016414));
#111048=CARTESIAN_POINT('Ctrl Pts',(5.507779351376,-30.0639843855966,56.6647708546223));
#111049=CARTESIAN_POINT('Ctrl Pts',(5.50371669875932,-30.0030963925187,
56.6671110450554));
#111050=CARTESIAN_POINT('Ctrl Pts',(5.49965404614264,-29.9420653656139,
56.6661070397698));
#111051=CARTESIAN_POINT('Ctrl Pts',(5.49559139352596,-29.8812851371461,
56.6617649597153));
#111052=CARTESIAN_POINT('Ctrl Pts',(5.49142779998958,-29.81899475934,56.6573149960696));
#111053=CARTESIAN_POINT('Ctrl Pts',(5.4872642064532,-29.7569683731696,56.64935884579));
#111054=CARTESIAN_POINT('Ctrl Pts',(5.48310061291682,-29.6956248184907,
56.6379596298081));
#111055=CARTESIAN_POINT('Ctrl Pts',(5.47903277309084,-29.6356920338397,
56.626822571315));
#111056=CARTESIAN_POINT('Ctrl Pts',(5.47496493326487,-29.5764115003721,
56.6123993290894));
#111057=CARTESIAN_POINT('Ctrl Pts',(5.47089709343889,-29.5181613318447,
56.594800143551));
#111058=CARTESIAN_POINT('Ctrl Pts',(5.46668562304731,-29.4578544194411,
56.5765795517918));
#111059=CARTESIAN_POINT('Ctrl Pts',(5.46247415265573,-29.3986525730831,
56.554954706161));
#111060=CARTESIAN_POINT('Ctrl Pts',(5.45826268226415,-29.3409531220702,
56.5301023536649));
#111061=CARTESIAN_POINT('Ctrl Pts',(5.45405121187257,-29.2832536710573,
56.5052500011689));
#111062=CARTESIAN_POINT('Ctrl Pts',(5.44983974148099,-29.2270571205141,
56.4771704752151));
#111063=CARTESIAN_POINT('Ctrl Pts',(5.44562827108941,-29.1727302560843,
56.4460915499379));
#111064=CARTESIAN_POINT('Ctrl Pts',(5.44155183030149,-29.1201452381571,
56.4160090877892));
#111065=CARTESIAN_POINT('Ctrl Pts',(5.43747538951358,-29.0690946643213,
56.3829925194298));
#111066=CARTESIAN_POINT('Ctrl Pts',(5.43339894872566,-29.0199255540374,
56.3472230997021));
#111067=CARTESIAN_POINT('Ctrl Pts',(5.42932840892935,-28.9708276201846,
56.3115054592242));
#111068=CARTESIAN_POINT('Ctrl Pts',(5.42525786913304,-28.9236061612427,
56.2730431653487));
#111069=CARTESIAN_POINT('Ctrl Pts',(5.42118732933672,-28.8785820255251,
56.232062387432));
#111070=CARTESIAN_POINT('Ctrl Pts',(5.41712116909577,-28.8336063319563,
56.1911257013542));
#111071=CARTESIAN_POINT('Ctrl Pts',(5.41305500885481,-28.7908236495021,
56.1476762483564));
#111072=CARTESIAN_POINT('Ctrl Pts',(5.40898884861385,-28.7505226456888,
56.1019810983241));
#111073=CARTESIAN_POINT('Ctrl Pts',(5.4049250037414,-28.7102445902272,56.0563119681988));
#111074=CARTESIAN_POINT('Ctrl Pts',(5.40086115886896,-28.6724457517756,
56.0084000576405));
#111075=CARTESIAN_POINT('Ctrl Pts',(5.39679731399651,-28.6373773379912,
55.9585486325586));
#111076=CARTESIAN_POINT('Ctrl Pts',(5.39273479857771,-28.6023203965518,
55.9087135159632));
#111077=CARTESIAN_POINT('Ctrl Pts',(5.38867228315891,-28.5699923972564,
55.8569405655949));
#111078=CARTESIAN_POINT('Ctrl Pts',(5.38460976774011,-28.5406023334362,
55.8035635947628));
#111079=CARTESIAN_POINT('Ctrl Pts',(5.38054576406545,-28.5112015029036,
55.7501670698905));
#111080=CARTESIAN_POINT('Ctrl Pts',(5.37648176039079,-28.4847410005683,
55.6951658017754));
#111081=CARTESIAN_POINT('Ctrl Pts',(5.37241775671613,-28.461383953044,55.6389183516299));
#111082=CARTESIAN_POINT('Ctrl Pts',(5.37090280158279,-28.4526770517025,
55.6179507615004));
#111083=CARTESIAN_POINT('Ctrl Pts',(5.36938784644946,-28.4444009307782,
55.5968102093442));
#111084=CARTESIAN_POINT('Ctrl Pts',(5.36787289131612,-28.4365623102018,
55.5755159338528));
#111085=CARTESIAN_POINT('Origin',(5.,-30.,55.));
#111086=CARTESIAN_POINT('',(4.66781602203697,-28.4339760950611,55.5764682902535));
#111087=CARTESIAN_POINT('',(4.86076601588518,-28.4365623050844,55.575515919951));
#111088=CARTESIAN_POINT('',(5.,-28.4365623102018,55.5755159338528));
#111089=CARTESIAN_POINT('',(5.52206892288488,-28.3340005844715,55.0013955137945));
#111090=CARTESIAN_POINT('Ctrl Pts',(4.86076601588518,-28.4365623050844,
55.575515919951));
#111091=CARTESIAN_POINT('Ctrl Pts',(4.8623567140795,-28.4455582692477,55.5999542178111));
#111092=CARTESIAN_POINT('Ctrl Pts',(4.86394559269076,-28.4551274085992,
55.624182070837));
#111093=CARTESIAN_POINT('Ctrl Pts',(4.86634136946606,-28.4703643130818,
55.6602595159302));
#111094=CARTESIAN_POINT('Ctrl Pts',(4.86714462675909,-28.4756086977021,
55.672279046011));
#111095=CARTESIAN_POINT('Ctrl Pts',(4.87251974102098,-28.5115608474941,
55.7520929863859));
#111096=CARTESIAN_POINT('Ctrl Pts',(4.8771436608712,-28.546636291689,55.817817877537));
#111097=CARTESIAN_POINT('Ctrl Pts',(4.88280610841908,-28.5924758159412,
55.8913935790166));
#111098=CARTESIAN_POINT('Ctrl Pts',(4.8836146635785,-28.5990851600588,55.901745213947));
#111099=CARTESIAN_POINT('Ctrl Pts',(4.88489208210546,-28.6096133512663,
55.917839465566));
#111100=CARTESIAN_POINT('Ctrl Pts',(4.88535606533497,-28.6134548806998,
55.9236324730624));
#111101=CARTESIAN_POINT('Ctrl Pts',(4.88622874196377,-28.6207098919458,
55.9344257334858));
#111102=CARTESIAN_POINT('Ctrl Pts',(4.88663686034659,-28.6241145227322,
55.9394316379284));
#111103=CARTESIAN_POINT('Ctrl Pts',(4.88760315300092,-28.6322039812901,
55.9511874472255));
#111104=CARTESIAN_POINT('Ctrl Pts',(4.88816281200508,-28.6369115422406,
55.9579213734989));
#111105=CARTESIAN_POINT('Ctrl Pts',(4.89004737605434,-28.6528439655818,
55.9803566437827));
#111106=CARTESIAN_POINT('Ctrl Pts',(4.8913858255163,-28.6642913787573,55.9958970478198));
#111107=CARTESIAN_POINT('Ctrl Pts',(4.89471767494053,-28.6931674271695,
56.0337040434749));
#111108=CARTESIAN_POINT('Ctrl Pts',(4.89672565271892,-28.7108976090683,
56.0557321005616));
#111109=CARTESIAN_POINT('Ctrl Pts',(4.90592663770011,-28.7939321407047,
56.1536828542115));
#111110=CARTESIAN_POINT('Ctrl Pts',(4.91329187793459,-28.8654401602113,
56.224074438732));
#111111=CARTESIAN_POINT('Ctrl Pts',(4.92646765745908,-29.0066718683498,
56.3400286640871));
#111112=CARTESIAN_POINT('Ctrl Pts',(4.93230942541209,-29.07432292447,56.3876250390495));
#111113=CARTESIAN_POINT('Ctrl Pts',(4.93930500320949,-29.1620656893365,
56.4400717108394));
#111114=CARTESIAN_POINT('Ctrl Pts',(4.94063615588275,-29.1790723891478,
56.4498339063757));
#111115=CARTESIAN_POINT('Ctrl Pts',(4.94275297152449,-29.2066075804795,
56.4649997759076));
#111116=CARTESIAN_POINT('Ctrl Pts',(4.94354541202223,-29.2170277370284,
56.4705952273363));
#111117=CARTESIAN_POINT('Ctrl Pts',(4.94505000146004,-29.237023002231,56.4810595736852));
#111118=CARTESIAN_POINT('Ctrl Pts',(4.94576280150384,-29.2465872950526,
56.4859477329866));
#111119=CARTESIAN_POINT('Ctrl Pts',(4.94739595346363,-29.2687073054138,
56.496984442664));
#111120=CARTESIAN_POINT('Ctrl Pts',(4.94831401529336,-29.281294590246,56.5030681888911));
#111121=CARTESIAN_POINT('Ctrl Pts',(4.951224835303,-29.3216746427434,56.5219616119271));
#111122=CARTESIAN_POINT('Ctrl Pts',(4.95319693336021,-29.3497453274675,
56.5341647524631));
#111123=CARTESIAN_POINT('Ctrl Pts',(4.95785531877274,-29.4175720132559,
56.5614545913724));
#111124=CARTESIAN_POINT('Ctrl Pts',(4.96051903767616,-29.4576008687515,
56.5758065753862));
#111125=CARTESIAN_POINT('Ctrl Pts',(4.96772442826368,-29.5684244243163,
56.6108171440893));
#111126=CARTESIAN_POINT('Ctrl Pts',(4.9721985270971,-29.6401094669447,56.6283330490329));
#111127=CARTESIAN_POINT('Ctrl Pts',(4.97755739051451,-29.7263937469962,
56.643437965899));
#111128=CARTESIAN_POINT('Ctrl Pts',(4.97840787460967,-29.7400977788795,
56.6456608274519));
#111129=CARTESIAN_POINT('Ctrl Pts',(4.9837739274647,-29.8264979564302,56.6585692198715));
#111130=CARTESIAN_POINT('Ctrl Pts',(4.9883419844306,-29.8997978747434,56.6646055443897));
#111131=CARTESIAN_POINT('Ctrl Pts',(4.99394237339087,-29.9855231278391,
56.6659823456259));
#111132=CARTESIAN_POINT('Ctrl Pts',(4.99475070398619,-29.9978011708774,
56.6660437866857));
#111133=CARTESIAN_POINT('Ctrl Pts',(4.99602784400119,-30.0170284972259,
56.6659274704977));
#111134=CARTESIAN_POINT('Ctrl Pts',(4.99649177672391,-30.0239781819155,
56.6658419340061));
#111135=CARTESIAN_POINT('Ctrl Pts',(4.99736441514848,-30.0369803196991,
56.6656005258252));
#111136=CARTESIAN_POINT('Ctrl Pts',(4.99777254648116,-30.0430327202934,
56.6654551437902));
#111137=CARTESIAN_POINT('Ctrl Pts',(4.99873894704928,-30.0572982672592,
56.6650346662323));
#111138=CARTESIAN_POINT('Ctrl Pts',(4.99929870202256,-30.0655103184548,
56.6647317868905));
#111139=CARTESIAN_POINT('Ctrl Pts',(5.00118393497902,-30.0930099642885,
56.6635137497785));
#111140=CARTESIAN_POINT('Ctrl Pts',(5.00252296997056,-30.1122830336431,
56.6623240628892));
#111141=CARTESIAN_POINT('Ctrl Pts',(5.00585660377775,-30.159732425323,56.6585662232968));
#111142=CARTESIAN_POINT('Ctrl Pts',(5.00786579907666,-30.1878718297024,
56.6556147980918));
#111143=CARTESIAN_POINT('Ctrl Pts',(5.01707759850643,-30.3153460533314,
56.6389530614541));
#111144=CARTESIAN_POINT('Ctrl Pts',(5.02445273154417,-30.4133944052274,
56.6170082877466));
#111145=CARTESIAN_POINT('Ctrl Pts',(5.03762627195972,-30.587376957223,56.5611985428563));
#111146=CARTESIAN_POINT('Ctrl Pts',(5.04345691668225,-30.6639103968867,
56.5302219595604));
#111147=CARTESIAN_POINT('Ctrl Pts',(5.05044175034944,-30.7554208238062,
56.4850183969864));
#111148=CARTESIAN_POINT('Ctrl Pts',(5.05177258263981,-30.7728420864773,
56.4760269058343));
#111149=CARTESIAN_POINT('Ctrl Pts',(5.05388901410431,-30.8005126550865,
56.4611212614339));
#111150=CARTESIAN_POINT('Ctrl Pts',(5.05468138643945,-30.8108642600047,
56.4554020117813));
#111151=CARTESIAN_POINT('Ctrl Pts',(5.05618592313508,-30.8304998278226,
56.4442788516404));
#111152=CARTESIAN_POINT('Ctrl Pts',(5.05689873779717,-30.8397940969839,
56.4388944538067));
#111153=CARTESIAN_POINT('Ctrl Pts',(5.05853203132116,-30.8610654443726,
56.4262951244961));
#111154=CARTESIAN_POINT('Ctrl Pts',(5.05945021870636,-30.8730051755176,
56.4190184864598));
#111155=CARTESIAN_POINT('Ctrl Pts',(5.06236189036535,-30.9107900450925,
56.395333158323));
#111156=CARTESIAN_POINT('Ctrl Pts',(5.06433469690093,-30.936276023862,56.3783615362693));
#111157=CARTESIAN_POINT('Ctrl Pts',(5.06899511634689,-30.9960157188682,
56.3361576708979));
#111158=CARTESIAN_POINT('Ctrl Pts',(5.07166013274733,-31.0297995190664,
56.3102968994351));
#111159=CARTESIAN_POINT('Ctrl Pts',(5.07886618433584,-31.1193250042724,
56.2361632632531));
#111160=CARTESIAN_POINT('Ctrl Pts',(5.08333973224457,-31.1729108903475,
56.1854402076683));
#111161=CARTESIAN_POINT('Ctrl Pts',(5.08870351962095,-31.2324495439091,
56.1210795325227));
#111162=CARTESIAN_POINT('Ctrl Pts',(5.08955944453588,-31.2418075998604,
56.1107047651971));
#111163=CARTESIAN_POINT('Ctrl Pts',(5.09492395682153,-31.2994797634546,
56.0451267393175));
#111164=CARTESIAN_POINT('Ctrl Pts',(5.09948507939289,-31.3442282907643,
55.9869068538925));
#111165=CARTESIAN_POINT('Ctrl Pts',(5.10507777015086,-31.3918136507074,
55.9157300402534));
#111166=CARTESIAN_POINT('Ctrl Pts',(5.10588607230528,-31.3985241877153,
55.9054484079914));
#111167=CARTESIAN_POINT('Ctrl Pts',(5.10716317704671,-31.4088543762412,
55.8892320573665));
#111168=CARTESIAN_POINT('Ctrl Pts',(5.10762710337254,-31.4125517169767,
55.8833470143684));
#111169=CARTESIAN_POINT('Ctrl Pts',(5.1084997369603,-31.4194007466447,55.8722924832673));
#111170=CARTESIAN_POINT('Ctrl Pts',(5.10890786993506,-31.4225612186711,
55.8671287276937));
#111171=CARTESIAN_POINT('Ctrl Pts',(5.10987428417919,-31.4299451732476,
55.8549153967264));
#111172=CARTESIAN_POINT('Ctrl Pts',(5.11043405131392,-31.4341447174143,
55.8478516712772));
#111173=CARTESIAN_POINT('Ctrl Pts',(5.11231936904938,-31.4480368093912,
55.8240863354401));
#111174=CARTESIAN_POINT('Ctrl Pts',(5.11365847825465,-31.457490805846,55.8072480170422));
#111175=CARTESIAN_POINT('Ctrl Pts',(5.11699233824742,-31.4800699126507,
55.7653427584155));
#111176=CARTESIAN_POINT('Ctrl Pts',(5.11900168788523,-31.4928529323951,
55.7400989296676));
#111177=CARTESIAN_POINT('Ctrl Pts',(5.1282148593998,-31.5479994607116,55.6239481555645));
#111178=CARTESIAN_POINT('Ctrl Pts',(5.13559124771605,-31.5827444042041,
55.5296548402536));
#111179=CARTESIAN_POINT('Ctrl Pts',(5.14876450488049,-31.6302109985374,
55.3532159558411));
#111180=CARTESIAN_POINT('Ctrl Pts',(5.15459373927756,-31.6456900239156,
55.2721349564532));
#111181=CARTESIAN_POINT('Ctrl Pts',(5.16157721018784,-31.6573420426315,
55.170755939862));
#111182=CARTESIAN_POINT('Ctrl Pts',(5.16290800146684,-31.6592364802638,
55.1512435016055));
#111183=CARTESIAN_POINT('Ctrl Pts',(5.16502438375361,-31.6617210350949,
55.1199126770692));
#111184=CARTESIAN_POINT('Ctrl Pts',(5.16581674736336,-31.6625303644978,
55.1081140518327));
#111185=CARTESIAN_POINT('Ctrl Pts',(5.16732127730966,-31.6638349180154,
55.0855846457683));
#111186=CARTESIAN_POINT('Ctrl Pts',(5.16803409384519,-31.6643521220211,
55.0748557889417));
#111187=CARTESIAN_POINT('Ctrl Pts',(5.16966740550135,-31.6653036829076,
55.0501510955302));
#111188=CARTESIAN_POINT('Ctrl Pts',(5.17058560896727,-31.6656659359927,
55.0361731682925));
#111189=CARTESIAN_POINT('Ctrl Pts',(5.17349738971624,-31.6662599834833,
54.9915806851101));
#111190=CARTESIAN_POINT('Ctrl Pts',(5.17547028700397,-31.6658239656103,
54.9609625613734));
#111191=CARTESIAN_POINT('Ctrl Pts',(5.18013096702135,-31.6627668681661,
54.8878785891644));
#111192=CARTESIAN_POINT('Ctrl Pts',(5.18279614964513,-31.6593627377994,
54.8454666589146));
#111193=CARTESIAN_POINT('Ctrl Pts',(5.19000228389805,-31.6456340391557,
54.7300434846203));
#111194=CARTESIAN_POINT('Ctrl Pts',(5.19447575929849,-31.6320820950291,
54.6575145112323));
#111195=CARTESIAN_POINT('Ctrl Pts',(5.19984012921103,-31.6102985922564,
54.5725775668585));
#111196=CARTESIAN_POINT('Ctrl Pts',(5.20069670478339,-31.606654791506,54.5590783885206));
#111197=CARTESIAN_POINT('Ctrl Pts',(5.20606101995594,-31.5828379788928,
54.4750624841905));
#111198=CARTESIAN_POINT('Ctrl Pts',(5.21062130040077,-31.5581988168998,
54.4059047295577));
#111199=CARTESIAN_POINT('Ctrl Pts',(5.21621305634732,-31.5242143376925,
54.3273355990037));
#111200=CARTESIAN_POINT('Ctrl Pts',(5.21702135503304,-31.5192158653859,
54.3161214463109));
#111201=CARTESIAN_POINT('Ctrl Pts',(5.21829845547237,-31.5111945523011,
54.2986474993057));
#111202=CARTESIAN_POINT('Ctrl Pts',(5.21876238101803,-31.5082555808525,
54.292349377456));
#111203=CARTESIAN_POINT('Ctrl Pts',(5.21963501401595,-31.5026828588532,
54.2805996374192));
#111204=CARTESIAN_POINT('Ctrl Pts',(5.22004314719105,-31.5000586879212,
54.2751437493661));
#111205=CARTESIAN_POINT('Ctrl Pts',(5.22100956310321,-31.4938025170977,
54.2623160742457));
#111206=CARTESIAN_POINT('Ctrl Pts',(5.22156933172131,-31.4901456455509,
54.2549567244982));
#111207=CARTESIAN_POINT('Ctrl Pts',(5.22345465979769,-31.4777138538021,
54.2303957765015));
#111208=CARTESIAN_POINT('Ctrl Pts',(5.22479377805522,-31.4686946939059,
54.2133204520457));
#111209=CARTESIAN_POINT('Ctrl Pts',(5.22812766563737,-31.4457341579815,
54.1716225237206));
#111210=CARTESIAN_POINT('Ctrl Pts',(5.23013703410107,-31.4314586250855,
54.1471913915251));
#111211=CARTESIAN_POINT('Ctrl Pts',(5.23935037299783,-31.3637834991395,
54.0378624793571));
#111212=CARTESIAN_POINT('Ctrl Pts',(5.24672691444889,-31.3034065405392,
53.957528945681));
#111213=CARTESIAN_POINT('Ctrl Pts',(5.25990013707229,-31.1809163200732,
53.8219568472659));
#111214=CARTESIAN_POINT('Ctrl Pts',(5.26572919943675,-31.1211934776836,
53.7649785879782));
#111215=CARTESIAN_POINT('Ctrl Pts',(5.27271250410914,-31.042342038768,53.7002064361364));
#111216=CARTESIAN_POINT('Ctrl Pts',(5.27404329037955,-31.0269763187291,
53.688032038441));
#111217=CARTESIAN_POINT('Ctrl Pts',(5.27615966666045,-31.0020015288965,
53.6689519977381));
#111218=CARTESIAN_POINT('Ctrl Pts',(5.27695202920453,-30.9925279526575,
53.6618729044251));
#111219=CARTESIAN_POINT('Ctrl Pts',(5.27845655832646,-30.9743075682746,
53.6485577598412));
#111220=CARTESIAN_POINT('Ctrl Pts',(5.27916937509087,-30.9655742974295,
53.6423042861369));
#111221=CARTESIAN_POINT('Ctrl Pts',(5.28080268896172,-30.9453348711106,
53.6281058819975));
#111222=CARTESIAN_POINT('Ctrl Pts',(5.28172089439166,-30.9337878522869,
53.6202203957837));
#111223=CARTESIAN_POINT('Ctrl Pts',(5.28463268846466,-30.8966457784893,
53.5955358402068));
#111224=CARTESIAN_POINT('Ctrl Pts',(5.28660559683672,-30.870685523867,53.5792959015499));
#111225=CARTESIAN_POINT('Ctrl Pts',(5.29126630868025,-30.8076259751611,
53.542225949752));
#111226=CARTESIAN_POINT('Ctrl Pts',(5.29393151160667,-30.7701472740657,
53.5220830692988));
#111227=CARTESIAN_POINT('Ctrl Pts',(5.30113765592516,-30.6657290517363,
53.4710157881275));
#111228=CARTESIAN_POINT('Ctrl Pts',(5.30561112243963,-30.5974443170091,
53.4430643743414));
#111229=CARTESIAN_POINT('Ctrl Pts',(5.31097556277097,-30.5142693939606,
53.4152986026176));
#111230=CARTESIAN_POINT('Ctrl Pts',(5.31183221711195,-30.5009506498419,
53.4110380845298));
#111231=CARTESIAN_POINT('Ctrl Pts',(5.31719650821312,-30.4174481947714,
53.3854808103858));
#111232=CARTESIAN_POINT('Ctrl Pts',(5.32175668650177,-30.3459840202621,
53.3686730716207));
#111233=CARTESIAN_POINT('Ctrl Pts',(5.3273483290499,-30.2615444237552,53.3546121254132));
#111234=CARTESIAN_POINT('Ctrl Pts',(5.32815662731468,-30.2494119401777,
53.3527294072398));
#111235=CARTESIAN_POINT('Ctrl Pts',(5.32943372723195,-30.2303808519183,
53.3499912217858));
#111236=CARTESIAN_POINT('Ctrl Pts',(5.3298976526829,-30.2234955342965,53.3490445048733));
#111237=CARTESIAN_POINT('Ctrl Pts',(5.33077028560924,-30.2106016227377,
53.3473537545872));
#111238=CARTESIAN_POINT('Ctrl Pts',(5.33117841880865,-30.2045946371384,
53.3465993571583));
#111239=CARTESIAN_POINT('Ctrl Pts',(5.33214483492325,-30.1904244232498,
53.3448981682458));
#111240=CARTESIAN_POINT('Ctrl Pts',(5.33270460372141,-30.1822581545972,
53.343979018113));
#111241=CARTESIAN_POINT('Ctrl Pts',(5.334589933053,-30.1548808569597,53.3411025302052));
#111242=CARTESIAN_POINT('Ctrl Pts',(5.33592905240931,-30.1356434492066,
53.3394188757055));
#111243=CARTESIAN_POINT('Ctrl Pts',(5.33926294334032,-30.0881581864813,
53.3360935619194));
#111244=CARTESIAN_POINT('Ctrl Pts',(5.34127231408916,-30.0598899604796,
53.3348364907847));
#111245=CARTESIAN_POINT('Ctrl Pts',(5.35048567330346,-29.931333141851,53.3323972434933));
#111246=CARTESIAN_POINT('Ctrl Pts',(5.35786223334268,-29.8310949003424,
53.3395525825514));
#111247=CARTESIAN_POINT('Ctrl Pts',(5.37103726636608,-29.650735789786,53.3689366540128));
#111248=CARTESIAN_POINT('Ctrl Pts',(5.37686804534955,-29.570450487176,53.3882171285635));
#111249=CARTESIAN_POINT('Ctrl Pts',(5.3838520077568,-29.4732566832071,53.419341531383));
#111250=CARTESIAN_POINT('Ctrl Pts',(5.385181875842,-29.454707361839,53.4256443502839));
#111251=CARTESIAN_POINT('Ctrl Pts',(5.38729715109357,-29.425147278229,53.4362736396523));
#111252=CARTESIAN_POINT('Ctrl Pts',(5.38808931828124,-29.414064408873,53.4403925887271));
#111253=CARTESIAN_POINT('Ctrl Pts',(5.38959369642006,-29.3929977779737,
53.4484782682744));
#111254=CARTESIAN_POINT('Ctrl Pts',(5.39030655525759,-29.3830067470044,
53.4524242452993));
#111255=CARTESIAN_POINT('Ctrl Pts',(5.39194027574191,-29.3600951827815,
53.4617303642711));
#111256=CARTESIAN_POINT('Ctrl Pts',(5.39285884171903,-29.3472024782364,
53.4671571957145));
#111257=CARTESIAN_POINT('Ctrl Pts',(5.39577308252747,-29.3062849968276,
53.4849901954147));
#111258=CARTESIAN_POINT('Ctrl Pts',(5.39774802643174,-29.2785325887568,
53.4980079303492));
#111259=CARTESIAN_POINT('Ctrl Pts',(5.40241458416427,-29.2131057978863,
53.5309296521478));
#111260=CARTESIAN_POINT('Ctrl Pts',(5.40508351668301,-29.1758043966805,
53.5515276455805));
#111261=CARTESIAN_POINT('Ctrl Pts',(5.41233927071798,-29.0755889277856,
53.6119933702054));
#111262=CARTESIAN_POINT('Ctrl Pts',(5.41685663662433,-29.0144956493842,
53.6546822808664));
#111263=CARTESIAN_POINT('Ctrl Pts',(5.42222831087502,-28.9460619721675,
53.7096711251169));
#111264=CARTESIAN_POINT('Ctrl Pts',(5.42304575443613,-28.9357634833076,
53.7181518798815));
#111265=CARTESIAN_POINT('Ctrl Pts',(5.42835811847697,-28.8696756840611,
53.7739203002458));
#111266=CARTESIAN_POINT('Ctrl Pts',(5.43290592097097,-28.8169564015635,
53.8247087026248));
#111267=CARTESIAN_POINT('Ctrl Pts',(5.43848382745701,-28.7594879719249,
53.8878684286313));
#111268=CARTESIAN_POINT('Ctrl Pts',(5.43929207432471,-28.7513265425459,
53.8970397565057));
#111269=CARTESIAN_POINT('Ctrl Pts',(5.44056911049709,-28.7387049523823,
53.9115427865617));
#111270=CARTESIAN_POINT('Ctrl Pts',(5.44103302438772,-28.7341753467639,
53.9168138454005));
#111271=CARTESIAN_POINT('Ctrl Pts',(5.44190564857413,-28.7257617770451,
53.9267294806907));
#111272=CARTESIAN_POINT('Ctrl Pts',(5.44231378474214,-28.7218699799735,
53.9313670865621));
#111273=CARTESIAN_POINT('Ctrl Pts',(5.44328022557728,-28.7127551047572,
53.9423497178646));
#111274=CARTESIAN_POINT('Ctrl Pts',(5.44384001635758,-28.7075536035884,
53.9487122920186));
#111275=CARTESIAN_POINT('Ctrl Pts',(5.44572549893681,-28.6902871233375,
53.9701547936817));
#111276=CARTESIAN_POINT('Ctrl Pts',(5.4470647524444,-28.6784378188698,53.9854053567121));
#111277=CARTESIAN_POINT('Ctrl Pts',(5.45451784039417,-28.6146177603126,
54.0705596537538));
#111278=CARTESIAN_POINT('Ctrl Pts',(5.4608689980552,-28.5679296881899,54.1442456443403));
#111279=CARTESIAN_POINT('Ctrl Pts',(5.47371931183086,-28.4854029606339,
54.3003183657453));
#111280=CARTESIAN_POINT('Ctrl Pts',(5.48019531352583,-28.4500196967943,
54.3826483738021));
#111281=CARTESIAN_POINT('Ctrl Pts',(5.48939996520383,-28.4081176237134,
54.5068496067561));
#111282=CARTESIAN_POINT('Ctrl Pts',(5.49227856761209,-28.3962987109907,
54.5467566769934));
#111283=CARTESIAN_POINT('Ctrl Pts',(5.4962066027086,-28.3819888623059,54.6026890868305));
#111284=CARTESIAN_POINT('Ctrl Pts',(5.49729638143236,-28.3782191218697,
54.6183682160584));
#111285=CARTESIAN_POINT('Ctrl Pts',(5.49904973031991,-28.3724826607999,
54.6438494998385));
#111286=CARTESIAN_POINT('Ctrl Pts',(5.49971775081693,-28.3703755571437,
54.6536186336977));
#111287=CARTESIAN_POINT('Ctrl Pts',(5.50111176509432,-28.3661443964154,
54.674129257054));
#111288=CARTESIAN_POINT('Ctrl Pts',(5.50183716372146,-28.3640380641614,
54.6848739479423));
#111289=CARTESIAN_POINT('Ctrl Pts',(5.50327578275009,-28.360052837199,54.70632100565));
#111290=CARTESIAN_POINT('Ctrl Pts',(5.50398901833256,-28.3581724176039,
54.717022531921));
#111291=CARTESIAN_POINT('Ctrl Pts',(5.50566476235029,-28.3539818242413,
54.742320852755));
#111292=CARTESIAN_POINT('Ctrl Pts',(5.50662447759174,-28.3517608863835,
54.756931646552));
#111293=CARTESIAN_POINT('Ctrl Pts',(5.5125416898833,-28.3391939747328,54.8477199817409));
#111294=CARTESIAN_POINT('Ctrl Pts',(5.51733929466059,-28.3339361822987,
54.9245105823954));
#111295=CARTESIAN_POINT('Ctrl Pts',(5.52206892288488,-28.3340005844715,
55.0013955137945));
#111296=CARTESIAN_POINT('Ctrl Pts',(5.52206883519007,-28.334000583278,55.001394088226));
#111297=CARTESIAN_POINT('Ctrl Pts',(5.53024916938802,-28.3341118590488,
55.1343737416745));
#111298=CARTESIAN_POINT('Ctrl Pts',(5.53815870841351,-28.3501438770418,
55.2668475249079));
#111299=CARTESIAN_POINT('Ctrl Pts',(5.54797471152312,-28.3863352685772,
55.41474686797));
#111300=CARTESIAN_POINT('Ctrl Pts',(5.54923331350285,-28.3912502527335,
55.4334201225411));
#111301=CARTESIAN_POINT('Ctrl Pts',(5.55105205152663,-28.3987179130186,
55.459912173948));
#111302=CARTESIAN_POINT('Ctrl Pts',(5.55159812930721,-28.4010058783937,
55.4678047903748));
#111303=CARTESIAN_POINT('Ctrl Pts',(5.55255233789641,-28.4050807134963,
55.4814822156406));
#111304=CARTESIAN_POINT('Ctrl Pts',(5.55295893856606,-28.4068408784732,
55.4872747342021));
#111305=CARTESIAN_POINT('Ctrl Pts',(5.55383639336371,-28.4106896072668,
55.4996966908758));
#111306=CARTESIAN_POINT('Ctrl Pts',(5.55430777339972,-28.4127880620997,
55.5063225919339));
#111307=CARTESIAN_POINT('Ctrl Pts',(5.55561817318169,-28.4187082138394,
55.524617048843));
#111308=CARTESIAN_POINT('Ctrl Pts',(5.55646194115444,-28.4226174544054,
55.5362565091912));
#111309=CARTESIAN_POINT('Ctrl Pts',(5.55798998048575,-28.4298763917018,
55.5571030685315));
#111310=CARTESIAN_POINT('Ctrl Pts',(5.55867192322872,-28.4331790316067,
55.5663249713499));
#111311=CARTESIAN_POINT('Ctrl Pts',(5.55935721585159,-28.4365623067732,
55.5755159245387));
#111312=CARTESIAN_POINT('',(5.32851907597573,-28.3320375446013,55.0005309978053));
#111313=CARTESIAN_POINT('Ctrl Pts',(5.36787289131612,-28.4365623102018,
55.5755159338528));
#111314=CARTESIAN_POINT('Ctrl Pts',(5.36380422092234,-28.415510357728,55.5183265251754));
#111315=CARTESIAN_POINT('Ctrl Pts',(5.35973555052857,-28.3976176847615,
55.4600275468893));
#111316=CARTESIAN_POINT('Ctrl Pts',(5.3556668801348,-28.3829797838545,55.4010007737856));
#111317=CARTESIAN_POINT('Ctrl Pts',(5.35159065291195,-28.3683146956591,
55.3418643689861));
#111318=CARTESIAN_POINT('Ctrl Pts',(5.3475144256891,-28.3569165492793,55.2819979734425));
#111319=CARTESIAN_POINT('Ctrl Pts',(5.34343819846625,-28.3488294980143,
55.2217926359741));
#111320=CARTESIAN_POINT('Ctrl Pts',(5.34045646572778,-28.3429138745232,
55.1777528374188));
#111321=CARTESIAN_POINT('Ctrl Pts',(5.33747473298932,-28.3387688709573,
55.1335318564456));
#111322=CARTESIAN_POINT('Ctrl Pts',(5.33449300025085,-28.3363941013021,
55.0892827744734));
#111323=CARTESIAN_POINT('Ctrl Pts',(5.33250187903717,-28.3348082937692,
55.0597344233874));
#111324=CARTESIAN_POINT('Ctrl Pts',(5.33051075782348,-28.3340096599776,
55.0301434489476));
#111325=CARTESIAN_POINT('Ctrl Pts',(5.32851963660979,-28.3340000870979,
55.0005387116473));
#111326=CARTESIAN_POINT('Ctrl Pts',(5.32851891015794,-28.3314570866962,
55.0005287162952));
#111327=CARTESIAN_POINT('Ctrl Pts',(5.29346518324273,-28.3336687245373,
54.4785403892527));
#111328=CARTESIAN_POINT('Ctrl Pts',(5.221366366048,-28.8783648903703,53.4009406554565));
#111329=CARTESIAN_POINT('Ctrl Pts',(5.11222245857373,-30.7133240716271,
53.1646043309368));
#111330=CARTESIAN_POINT('Ctrl Pts',(5.00108718773517,-31.9288772063249,
54.6038419304127));
#111331=CARTESIAN_POINT('Ctrl Pts',(4.88995191689662,-31.3789833722224,
56.4056718508646));
#111332=CARTESIAN_POINT('Ctrl Pts',(4.77886152833055,-29.5676767012044,
56.9207218368853));
#111333=CARTESIAN_POINT('Ctrl Pts',(4.704816230044,-28.6243048912095,56.0933234227868));
#111334=CARTESIAN_POINT('Ctrl Pts',(4.66781602203697,-28.4339760950611,
55.5764682902535));
#111335=CARTESIAN_POINT('Origin',(5.,-30.,55.));
#111336=CARTESIAN_POINT('',(3.96712537028317,-28.4365623116664,55.5755159378315));
#111337=CARTESIAN_POINT('',(4.16232238521864,-28.4365623101738,55.5755159337767));
#111338=CARTESIAN_POINT('',(5.,-28.4365623102018,55.5755159338528));
#111339=CARTESIAN_POINT('Ctrl Pts',(4.16232238521864,-28.4365623101738,
55.5755159337767));
#111340=CARTESIAN_POINT('Ctrl Pts',(4.16243211065126,-28.4371213119974,
55.57703450949));
#111341=CARTESIAN_POINT('Ctrl Pts',(4.16254176393469,-28.4376825329798,
55.5785522888462));
#111342=CARTESIAN_POINT('Ctrl Pts',(4.16358804680715,-28.4430622566701,
55.5930364300062));
#111343=CARTESIAN_POINT('Ctrl Pts',(4.16451935117471,-28.4480399748959,
55.605943433365));
#111344=CARTESIAN_POINT('Ctrl Pts',(4.16616300711542,-28.4571605741507,
55.6287427762166));
#111345=CARTESIAN_POINT('Ctrl Pts',(4.1668774614397,-28.4612392419544,55.638659777453));
#111346=CARTESIAN_POINT('Ctrl Pts',(4.16837821887263,-28.4700469726591,
55.659500881152));
#111347=CARTESIAN_POINT('Ctrl Pts',(4.1691637322308,-28.4747979571576,55.6704151094574));
#111348=CARTESIAN_POINT('Ctrl Pts',(4.17125636230181,-28.4878298909142,
55.6994970775095));
#111349=CARTESIAN_POINT('Ctrl Pts',(4.17255624952594,-28.4963212858166,
55.717568798265));
#111350=CARTESIAN_POINT('Ctrl Pts',(4.17995993473596,-28.5469250244852,
55.8204203914948));
#111351=CARTESIAN_POINT('Ctrl Pts',(4.1858159223418,-28.5958792134244,55.9016454920731));
#111352=CARTESIAN_POINT('Ctrl Pts',(4.19592518127326,-28.6928722832729,
56.0353470365276));
#111353=CARTESIAN_POINT('Ctrl Pts',(4.20019943960676,-28.7378497637999,
56.0897259021831));
#111354=CARTESIAN_POINT('Ctrl Pts',(4.20696058789092,-28.8125992073484,
56.1692426038715));
#111355=CARTESIAN_POINT('Ctrl Pts',(4.20938085575127,-28.8400332859465,
56.1964638503042));
#111356=CARTESIAN_POINT('Ctrl Pts',(4.21290755393678,-28.8804767132497,
56.2338942312861));
#111357=CARTESIAN_POINT('Ctrl Pts',(4.2139711068955,-28.8927314107955,56.2449030447944));
#111358=CARTESIAN_POINT('Ctrl Pts',(4.21585137077576,-28.9144487382782,
56.2638381065356));
#111359=CARTESIAN_POINT('Ctrl Pts',(4.21666303688062,-28.9238401492346,
56.2718444303598));
#111360=CARTESIAN_POINT('Ctrl Pts',(4.21794280289821,-28.9386549214848,
56.2841926925827));
#111361=CARTESIAN_POINT('Ctrl Pts',(4.21840598100122,-28.9440181888169,
56.2886064789089));
#111362=CARTESIAN_POINT('Ctrl Pts',(4.21927452204453,-28.954074011514,56.2967771435341));
#111363=CARTESIAN_POINT('Ctrl Pts',(4.21967928766356,-28.9587594817694,
56.3005423148981));
#111364=CARTESIAN_POINT('Ctrl Pts',(4.22061123773838,-28.9695458685734,
56.3091144370171));
#111365=CARTESIAN_POINT('Ctrl Pts',(4.22113957705317,-28.9756600786149,
56.3139041234454));
#111366=CARTESIAN_POINT('Ctrl Pts',(4.22277467941608,-28.9945865701455,
56.3285181623988));
#111367=CARTESIAN_POINT('Ctrl Pts',(4.22389046619346,-29.007507924915,56.3381988289139));
#111368=CARTESIAN_POINT('Ctrl Pts',(4.23066062726888,-29.0860593549262,
56.3952860326472));
#111369=CARTESIAN_POINT('Ctrl Pts',(4.23653737146867,-29.1549277087525,
56.4380406696468));
#111370=CARTESIAN_POINT('Ctrl Pts',(4.24779272152279,-29.2918984796872,
56.509827652349));
#111371=CARTESIAN_POINT('Ctrl Pts',(4.25315698148687,-29.3593762754129,
56.5396719965527));
#111372=CARTESIAN_POINT('Ctrl Pts',(4.26145229165483,-29.468564696303,56.5795383907822));
#111373=CARTESIAN_POINT('Ctrl Pts',(4.26445109047989,-29.5090638997846,
56.5925913658569));
#111374=CARTESIAN_POINT('Ctrl Pts',(4.2695284350158,-29.5794984757368,56.612349760313));
#111375=CARTESIAN_POINT('Ctrl Pts',(4.27162850920852,-29.6091995610068,
56.6198050846228));
#111376=CARTESIAN_POINT('Ctrl Pts',(4.27464973005518,-29.6527409209396,
56.6294669761365));
#111377=CARTESIAN_POINT('Ctrl Pts',(4.27559134859135,-29.6664287623135,
56.6323240316784));
#111378=CARTESIAN_POINT('Ctrl Pts',(4.27724659181909,-29.690692397222,56.6370706073421));
#111379=CARTESIAN_POINT('Ctrl Pts',(4.27796242414816,-29.7012533758513,
56.6390307594453));
#111380=CARTESIAN_POINT('Ctrl Pts',(4.27945959070728,-29.7234802013295,
56.6429341578835));
#111381=CARTESIAN_POINT('Ctrl Pts',(4.28024019785937,-29.7351493072579,
56.6448556073072));
#111382=CARTESIAN_POINT('Ctrl Pts',(4.28230445291056,-29.7662120225624,
56.6496312924324));
#111383=CARTESIAN_POINT('Ctrl Pts',(4.28358122063522,-29.7856375905309,
56.6522678443218));
#111384=CARTESIAN_POINT('Ctrl Pts',(4.29017436683072,-29.8869577869544,
56.664202558619));
#111385=CARTESIAN_POINT('Ctrl Pts',(4.29530815566265,-29.9694175722315,
56.6677577436673));
#111386=CARTESIAN_POINT('Ctrl Pts',(4.30653208466127,-30.1520640630736,
56.6620749126426));
#111387=CARTESIAN_POINT('Ctrl Pts',(4.31256292326601,-30.2518243018729,
56.6499086851521));
#111388=CARTESIAN_POINT('Ctrl Pts',(4.32062391892838,-30.3775408688769,
56.6229046278441));
#111389=CARTESIAN_POINT('Ctrl Pts',(4.32241757625831,-30.4050462954552,
56.6162592170699));
#111390=CARTESIAN_POINT('Ctrl Pts',(4.3254863058203,-30.4510167220484,56.6039054909413));
#111391=CARTESIAN_POINT('Ctrl Pts',(4.32674503545846,-30.4695763640406,
56.5985702573787));
#111392=CARTESIAN_POINT('Ctrl Pts',(4.32856392602924,-30.4958955665614,
56.5905065615686));
#111393=CARTESIAN_POINT('Ctrl Pts',(4.32911002548848,-30.5037349143724,
56.5880411406401));
#111394=CARTESIAN_POINT('Ctrl Pts',(4.33006425851927,-30.517317354206,56.5836588679341));
#111395=CARTESIAN_POINT('Ctrl Pts',(4.33047086170832,-30.5230687574497,
56.5817685445683));
#111396=CARTESIAN_POINT('Ctrl Pts',(4.33134830595028,-30.5354006471635,
56.5776407866514));
#111397=CARTESIAN_POINT('Ctrl Pts',(4.33181967275585,-30.5419773753784,
56.5753935460262));
#111398=CARTESIAN_POINT('Ctrl Pts',(4.33313000076289,-30.5601327361099,
56.5690627960888));
#111399=CARTESIAN_POINT('Ctrl Pts',(4.33397370938485,-30.5716803123751,
56.5648924367061));
#111400=CARTESIAN_POINT('Ctrl Pts',(4.33989687688816,-30.6518335068084,
56.5349399088824));
#111401=CARTESIAN_POINT('Ctrl Pts',(4.34517904538841,-30.7187116703811,
56.5047852334948));
#111402=CARTESIAN_POINT('Ctrl Pts',(4.35152427570334,-30.7957926739051,
56.4637171319259));
#111403=CARTESIAN_POINT('Ctrl Pts',(4.35254751974055,-30.8081213881181,
56.456946684157));
#111404=CARTESIAN_POINT('Ctrl Pts',(4.35893581942883,-30.8845144947408,
56.4137265746421));
#111405=CARTESIAN_POINT('Ctrl Pts',(4.36430072111089,-30.9461908951115,
56.3732125915553));
#111406=CARTESIAN_POINT('Ctrl Pts',(4.37259482970425,-31.0388876293453,
56.3031022521645));
#111407=CARTESIAN_POINT('Ctrl Pts',(4.37559188714158,-31.07179940411,56.2761698655432));
#111408=CARTESIAN_POINT('Ctrl Pts',(4.38066664511901,-31.1265717084339,
56.2277331570357));
#111409=CARTESIAN_POINT('Ctrl Pts',(4.38276584436773,-31.1489344902655,
56.2068315001478));
#111410=CARTESIAN_POINT('Ctrl Pts',(4.38578605963622,-31.180656394891,56.175500706456));
#111411=CARTESIAN_POINT('Ctrl Pts',(4.3867275282844,-31.1904789142066,56.1655519761865));
#111412=CARTESIAN_POINT('Ctrl Pts',(4.38838260250387,-31.2076246259359,
56.1477430563729));
#111413=CARTESIAN_POINT('Ctrl Pts',(4.38909841418583,-31.2149990894154,
56.1399335869368));
#111414=CARTESIAN_POINT('Ctrl Pts',(4.39059562974747,-31.2303339792498,
56.1233762376435));
#111415=CARTESIAN_POINT('Ctrl Pts',(4.39137630566097,-31.2382778397364,
56.1146137786509));
#111416=CARTESIAN_POINT('Ctrl Pts',(4.39344095835931,-31.2591413065225,
56.0911020068116));
#111417=CARTESIAN_POINT('Ctrl Pts',(4.39471805012289,-31.2718952412442,
56.0762076783809));
#111418=CARTESIAN_POINT('Ctrl Pts',(4.40132228906001,-31.3369830112365,
55.9974230493677));
#111419=CARTESIAN_POINT('Ctrl Pts',(4.40646602792858,-31.3847789123154,
55.9299280429754));
#111420=CARTESIAN_POINT('Ctrl Pts',(4.41769061665509,-31.4790267099188,
55.7733480857006));
#111421=CARTESIAN_POINT('Ctrl Pts',(4.42371306737134,-31.5228307391293,
55.6830603693174));
#111422=CARTESIAN_POINT('Ctrl Pts',(4.43176397620187,-31.5682627428966,
55.5629453512309));
#111423=CARTESIAN_POINT('Ctrl Pts',(4.43355651138082,-31.5775904701257,
55.5362495944699));
#111424=CARTESIAN_POINT('Ctrl Pts',(4.43662351478916,-31.5921348118628,
55.4909534561919));
#111425=CARTESIAN_POINT('Ctrl Pts',(4.4378816643358,-31.5977156160317,55.47247570063));
#111426=CARTESIAN_POINT('Ctrl Pts',(4.43969986170973,-31.605212462451,55.4460005165346));
#111427=CARTESIAN_POINT('Ctrl Pts',(4.44024586264612,-31.6073924884716,
55.4380786360471));
#111428=CARTESIAN_POINT('Ctrl Pts',(4.44119998460395,-31.6110768784822,
55.4242922863489));
#111429=CARTESIAN_POINT('Ctrl Pts',(4.44160657634965,-31.6126080181545,
55.4184352172965));
#111430=CARTESIAN_POINT('Ctrl Pts',(4.44248406859626,-31.6158286004892,
55.4058352504433));
#111431=CARTESIAN_POINT('Ctrl Pts',(4.44295549555467,-31.6175077538273,
55.3990901885068));
#111432=CARTESIAN_POINT('Ctrl Pts',(4.44426614989972,-31.6220368388786,
55.3803989063622));
#111433=CARTESIAN_POINT('Ctrl Pts',(4.44511012837367,-31.6247968877908,
55.3684316570703));
#111434=CARTESIAN_POINT('Ctrl Pts',(4.45110730840338,-31.6433322501858,
55.2838023084108));
#111435=CARTESIAN_POINT('Ctrl Pts',(4.45646911568256,-31.6543581590369,
55.2101933988584));
#111436=CARTESIAN_POINT('Ctrl Pts',(4.46272943876652,-31.6613963162143,
55.1243295597897));
#111437=CARTESIAN_POINT('Ctrl Pts',(4.46358882770382,-31.6622361542528,
55.11254565401));
#111438=CARTESIAN_POINT('Ctrl Pts',(4.47401157832634,-31.6708972052907,
54.9695943126691));
#111439=CARTESIAN_POINT('Ctrl Pts',(4.48353089996228,-31.6633002424257,
54.8379284727486));
#111440=CARTESIAN_POINT('Ctrl Pts',(4.49406129198292,-31.6364677088518,
54.6869353601699));
#111441=CARTESIAN_POINT('Ctrl Pts',(4.49555251643617,-31.6322089684988,
54.6654405982236));
#111442=CARTESIAN_POINT('Ctrl Pts',(4.49786076861307,-31.6248965807297,
54.6320072085027));
#111443=CARTESIAN_POINT('Ctrl Pts',(4.4986868937088,-31.6221325673299,54.6200084990784));
#111444=CARTESIAN_POINT('Ctrl Pts',(4.5002204952924,-31.6167271428059,54.5976779439363));
#111445=CARTESIAN_POINT('Ctrl Pts',(4.50092899837004,-31.6141190791023,
54.5873387604858));
#111446=CARTESIAN_POINT('Ctrl Pts',(4.50250678748599,-31.6080633235219,
54.5642680843485));
#111447=CARTESIAN_POINT('Ctrl Pts',(4.50337433962746,-31.6045633168758,
54.5515509688137));
#111448=CARTESIAN_POINT('Ctrl Pts',(4.50558083920576,-31.5952274235107,
54.5191389417782));
#111449=CARTESIAN_POINT('Ctrl Pts',(4.50691285335141,-31.5891775592401,
54.4995076079731));
#111450=CARTESIAN_POINT('Ctrl Pts',(4.51676586711935,-31.541369031248,54.3539910411241));
#111451=CARTESIAN_POINT('Ctrl Pts',(4.52476790493922,-31.4850755979531,
54.233383937309));
#111452=CARTESIAN_POINT('Ctrl Pts',(4.53782898807933,-31.3724990106375,
54.052208504936));
#111453=CARTESIAN_POINT('Ctrl Pts',(4.54280835877174,-31.3250133922257,
53.9868867493938));
#111454=CARTESIAN_POINT('Ctrl Pts',(4.54897253594656,-31.2639220446676,
53.9145255623659));
#111455=CARTESIAN_POINT('Ctrl Pts',(4.54989574808572,-31.2547165702832,
53.9038978213636));
#111456=CARTESIAN_POINT('Ctrl Pts',(4.55130915368142,-31.2405623084587,
53.8879686502041));
#111457=CARTESIAN_POINT('Ctrl Pts',(4.55179250060612,-31.235711334333,53.8825806260069));
#111458=CARTESIAN_POINT('Ctrl Pts',(4.55268144352086,-31.2267742365302,
53.8727834687516));
#111459=CARTESIAN_POINT('Ctrl Pts',(4.55308622576839,-31.2226992165382,
53.8683645649483));
#111460=CARTESIAN_POINT('Ctrl Pts',(4.55401841394519,-31.2133019299071,
53.858284272262));
#111461=CARTESIAN_POINT('Ctrl Pts',(4.55454697711084,-31.2079639234371,
53.8526380127801));
#111462=CARTESIAN_POINT('Ctrl Pts',(4.55618342963906,-31.1914019573732,
53.8353633297176));
#111463=CARTESIAN_POINT('Ctrl Pts',(4.55730036319552,-31.1800485052258,
53.8238611157512));
#111464=CARTESIAN_POINT('Ctrl Pts',(4.56381289901495,-31.1134709966227,
53.758345703902));
#111465=CARTESIAN_POINT('Ctrl Pts',(4.56941075916856,-31.0547154314812,
53.7080649654478));
#111466=CARTESIAN_POINT('Ctrl Pts',(4.58180749125572,-30.9178907675277,
53.6065483117389));
#111467=CARTESIAN_POINT('Ctrl Pts',(4.58858959507342,-30.8385608835689,
53.5574155516046));
#111468=CARTESIAN_POINT('Ctrl Pts',(4.59875990850559,-30.7103669359251,
53.4921859887675));
#111469=CARTESIAN_POINT('Ctrl Pts',(4.60228315990653,-30.6641709818896,
53.4712743497823));
#111470=CARTESIAN_POINT('Ctrl Pts',(4.60687793181026,-30.6015142074444,
53.4462890221044));
#111471=CARTESIAN_POINT('Ctrl Pts',(4.6080121966321,-30.5858461287501,53.4403136553393));
#111472=CARTESIAN_POINT('Ctrl Pts',(4.60989300757114,-30.5595371860798,
53.4307325694619));
#111473=CARTESIAN_POINT('Ctrl Pts',(4.6106438469159,-30.5489455653351,53.4269962148431));
#111474=CARTESIAN_POINT('Ctrl Pts',(4.61211585078803,-30.5280096188241,
53.4198479617214));
#111475=CARTESIAN_POINT('Ctrl Pts',(4.6128371893371,-30.5176680300435,53.4164298430815));
#111476=CARTESIAN_POINT('Ctrl Pts',(4.61458303893485,-30.4924439150111,
53.4083662374511));
#111477=CARTESIAN_POINT('Ctrl Pts',(4.61560401789845,-30.4775280800389,
53.4038277024767));
#111478=CARTESIAN_POINT('Ctrl Pts',(4.61909824108944,-30.4259409882255,
53.3889188542871));
#111479=CARTESIAN_POINT('Ctrl Pts',(4.62153791870066,-30.3889774894569,
53.3795972591304));
#111480=CARTESIAN_POINT('Ctrl Pts',(4.63223687516057,-30.2234609931224,
53.3438477812189));
#111481=CARTESIAN_POINT('Ctrl Pts',(4.64007255399123,-30.0923796976781,
53.3313955347718));
#111482=CARTESIAN_POINT('Ctrl Pts',(4.6507661062621,-29.919328642491,53.3354274294738));
#111483=CARTESIAN_POINT('Ctrl Pts',(4.65338074260183,-29.877517033542,53.3379809966893));
#111484=CARTESIAN_POINT('Ctrl Pts',(4.65767940755035,-29.8105484071424,
53.3446116799654));
#111485=CARTESIAN_POINT('Ctrl Pts',(4.6593250213079,-29.7853100774154,53.3476954076343));
#111486=CARTESIAN_POINT('Ctrl Pts',(4.66160114849966,-29.7511209947354,
53.3526692620038));
#111487=CARTESIAN_POINT('Ctrl Pts',(4.66220622765236,-29.7420993333675,
53.3540575476851));
#111488=CARTESIAN_POINT('Ctrl Pts',(4.6632293753309,-29.7269666092213,53.3565136907798));
#111489=CARTESIAN_POINT('Ctrl Pts',(4.66364525086665,-29.7208491048592,
53.3575417030293));
#111490=CARTESIAN_POINT('Ctrl Pts',(4.66450501511909,-29.7082741981267,
53.359727128527));
#111491=CARTESIAN_POINT('Ctrl Pts',(4.66494910162733,-29.7018177008032,
53.3608885489187));
#111492=CARTESIAN_POINT('Ctrl Pts',(4.6661304539194,-29.6847398392727,53.3640648226665));
#111493=CARTESIAN_POINT('Ctrl Pts',(4.66687119817837,-29.6741311460916,
53.3661449427848));
#111494=CARTESIAN_POINT('Ctrl Pts',(4.6702301552907,-29.6264385410179,53.375979317183));
#111495=CARTESIAN_POINT('Ctrl Pts',(4.67290273966302,-29.5896081277386,
53.3848933902908));
#111496=CARTESIAN_POINT('Ctrl Pts',(4.6822505533842,-29.4636029282342,53.4199784320118));
#111497=CARTESIAN_POINT('Ctrl Pts',(4.68907383001019,-29.3763330994635,
53.4523471968534));
#111498=CARTESIAN_POINT('Ctrl Pts',(4.70033038323411,-29.2355654021857,
53.5184089186888));
#111499=CARTESIAN_POINT('Ctrl Pts',(4.70481073208242,-29.1804512695654,
53.5481688733211));
#111500=CARTESIAN_POINT('Ctrl Pts',(4.71200005293278,-29.0930579090775,
53.6019252793024));
#111501=CARTESIAN_POINT('Ctrl Pts',(4.71476333365495,-29.0597419654664,
53.6241104047534));
#111502=CARTESIAN_POINT('Ctrl Pts',(4.71853225852293,-29.014711894783,53.6564963537114));
#111503=CARTESIAN_POINT('Ctrl Pts',(4.71957535979378,-29.0022948355298,
53.6656915159536));
#111504=CARTESIAN_POINT('Ctrl Pts',(4.7213479694372,-28.9812788190681,53.6817118646445));
#111505=CARTESIAN_POINT('Ctrl Pts',(4.72208074819327,-28.9726163114684,
53.6884515949557));
#111506=CARTESIAN_POINT('Ctrl Pts',(4.72356045199374,-28.9551793651692,
53.7022969144946));
#111507=CARTESIAN_POINT('Ctrl Pts',(4.72430714197504,-28.9464092848474,
53.7094070848405));
#111508=CARTESIAN_POINT('Ctrl Pts',(4.72617304018116,-28.9245729713239,
53.7274813897998));
#111509=CARTESIAN_POINT('Ctrl Pts',(4.72728762436781,-28.9116013749652,
53.738558215573));
#111510=CARTESIAN_POINT('Ctrl Pts',(4.73157548840588,-28.862019959771,53.7822315414736));
#111511=CARTESIAN_POINT('Ctrl Pts',(4.73469009249451,-28.8266836419565,
53.8162398882538));
#111512=CARTESIAN_POINT('Ctrl Pts',(4.74610163635663,-28.7010252701647,
53.9483400712824));
#111513=CARTESIAN_POINT('Ctrl Pts',(4.75402214546896,-28.6210841601526,
54.0555890221869));
#111514=CARTESIAN_POINT('Ctrl Pts',(4.76431592560086,-28.5390445108868,
54.1986477869557));
#111515=CARTESIAN_POINT('Ctrl Pts',(4.76631260546256,-28.5240960123518,
54.2265250543874));
#111516=CARTESIAN_POINT('Ctrl Pts',(4.76969146729471,-28.5005914614878,
54.2735236631076));
#111517=CARTESIAN_POINT('Ctrl Pts',(4.77105269458402,-28.4915860059077,
54.2924118724151));
#111518=CARTESIAN_POINT('Ctrl Pts',(4.77299367876181,-28.4794350156575,
54.3191843004202));
#111519=CARTESIAN_POINT('Ctrl Pts',(4.77355668200135,-28.4759899599184,
54.3269314459267));
#111520=CARTESIAN_POINT('Ctrl Pts',(4.7745302154362,-28.4701720729221,54.3402882379023));
#111521=CARTESIAN_POINT('Ctrl Pts',(4.77493902497483,-28.4677706132277,
54.3458851777506));
#111522=CARTESIAN_POINT('Ctrl Pts',(4.77580932818307,-28.4627471193443,
54.3577726087513));
#111523=CARTESIAN_POINT('Ctrl Pts',(4.7762712350242,-28.4601330103361,54.3640659695152));
#111524=CARTESIAN_POINT('Ctrl Pts',(4.77755131660434,-28.4530294367921,
54.3814681589952));
#111525=CARTESIAN_POINT('Ctrl Pts',(4.77837401688177,-28.4486211932762,
54.3926094015151));
#111526=CARTESIAN_POINT('Ctrl Pts',(4.78299492143553,-28.4247101719522,
54.455000163146));
#111527=CARTESIAN_POINT('Ctrl Pts',(4.78690695310832,-28.4076285668422,
54.5071360843809));
#111528=CARTESIAN_POINT('Ctrl Pts',(4.80157603031304,-28.3539822088949,
54.7030548127338));
#111529=CARTESIAN_POINT('Ctrl Pts',(4.81249357102556,-28.334082356827,54.8507205956567));
#111530=CARTESIAN_POINT('Ctrl Pts',(4.82499125992332,-28.3339828077517,
55.0306050154698));
#111531=CARTESIAN_POINT('Ctrl Pts',(4.82715543606239,-28.3348602720593,
55.0621278638137));
#111532=CARTESIAN_POINT('Ctrl Pts',(4.83023987647433,-28.3374178031887,
55.1075735681334));
#111533=CARTESIAN_POINT('Ctrl Pts',(4.83118216722175,-28.3383795471822,
55.1215282897699));
#111534=CARTESIAN_POINT('Ctrl Pts',(4.83284056506335,-28.3403930376387,
55.1462081162762));
#111535=CARTESIAN_POINT('Ctrl Pts',(4.8335588633432,-28.3413732985971,55.1569380691767));
#111536=CARTESIAN_POINT('Ctrl Pts',(4.83505100254139,-28.3436359536721,
55.1793076978632));
#111537=CARTESIAN_POINT('Ctrl Pts',(4.8358242137481,-28.3449371141311,55.190944913774));
#111538=CARTESIAN_POINT('Ctrl Pts',(4.83784567712815,-28.3486775751411,
55.2214797554228));
#111539=CARTESIAN_POINT('Ctrl Pts',(4.83908756279389,-28.3513186039049,
55.2403512753014));
#111540=CARTESIAN_POINT('Ctrl Pts',(4.8454959978053,-28.3667318226923,55.3382229731083));
#111541=CARTESIAN_POINT('Ctrl Pts',(4.85049042030508,-28.3848606625276,
55.4162775354516));
#111542=CARTESIAN_POINT('Ctrl Pts',(4.85720459938426,-28.4171516170431,
55.5205730040301));
#111543=CARTESIAN_POINT('Ctrl Pts',(4.85898645989029,-28.4264982828747,
55.548176152032));
#111544=CARTESIAN_POINT('Ctrl Pts',(4.86076601588518,-28.4365623050844,
55.575515919951));
#111545=CARTESIAN_POINT('',(4.62852046319487,-28.3357683158861,55.0011944502022));
#111546=CARTESIAN_POINT('Ctrl Pts',(4.66781602203697,-28.4339760950611,
55.5764682902535));
#111547=CARTESIAN_POINT('Ctrl Pts',(4.66777113976448,-28.4337452209835,
55.5758413307269));
#111548=CARTESIAN_POINT('Ctrl Pts',(4.65467262015045,-28.3664872324192,
55.3928239783714));
#111549=CARTESIAN_POINT('Ctrl Pts',(4.64157410053641,-28.3344870714878,
55.1968759499582));
#111550=CARTESIAN_POINT('Ctrl Pts',(4.62852046319487,-28.3357683158861,
55.0011944502022));
#111551=CARTESIAN_POINT('Ctrl Pts',(4.6275029120089,-28.3340004729511,55.0012553377942));
#111552=CARTESIAN_POINT('Ctrl Pts',(4.62392610857778,-28.3339624265383,
54.9507627085131));
#111553=CARTESIAN_POINT('Ctrl Pts',(4.62040759124933,-28.3362198407892,
54.900289559962));
#111554=CARTESIAN_POINT('Ctrl Pts',(4.61603293442498,-28.3419878498603,
54.8364901137));
#111555=CARTESIAN_POINT('Ctrl Pts',(4.61511227194061,-28.3433732486938,
54.8230039587256));
#111556=CARTESIAN_POINT('Ctrl Pts',(4.61349180923425,-28.3461165050552,
54.7991658746005));
#111557=CARTESIAN_POINT('Ctrl Pts',(4.61278995550999,-28.3474073273124,
54.7888071318349));
#111558=CARTESIAN_POINT('Ctrl Pts',(4.61140048097976,-28.3501674411464,
54.7682350769568));
#111559=CARTESIAN_POINT('Ctrl Pts',(4.61071282033464,-28.3516344235026,
54.7580219302104));
#111560=CARTESIAN_POINT('Ctrl Pts',(4.60924926147721,-28.3549728395331,
54.736220920203));
#111561=CARTESIAN_POINT('Ctrl Pts',(4.60847427981564,-28.3568720538779,
54.7246378272849));
#111562=CARTESIAN_POINT('Ctrl Pts',(4.60644178568113,-28.3621997042574,
54.6941655536125));
#111563=CARTESIAN_POINT('Ctrl Pts',(4.60519077413458,-28.3658325448802,
54.6753135428048));
#111564=CARTESIAN_POINT('Ctrl Pts',(4.59879715589171,-28.3862164080763,
54.5785663407397));
#111565=CARTESIAN_POINT('Ctrl Pts',(4.59382468899969,-28.4082145364832,
54.5018783630823));
#111566=CARTESIAN_POINT('Ctrl Pts',(4.58411984082222,-28.462485560859,54.3536966381393));
#111567=CARTESIAN_POINT('Ctrl Pts',(4.57939577425797,-28.4944769933123,
54.2823240242972));
#111568=CARTESIAN_POINT('Ctrl Pts',(4.57086876488907,-28.5597682281909,
54.1604108765062));
#111569=CARTESIAN_POINT('Ctrl Pts',(4.56710814704191,-28.5910298677669,
54.1089449571422));
#111570=CARTESIAN_POINT('Ctrl Pts',(4.56221665598818,-28.6335551471678,
54.0467875999827));
#111571=CARTESIAN_POINT('Ctrl Pts',(4.56122377112638,-28.6422773535168,
54.0344045406386));
#111572=CARTESIAN_POINT('Ctrl Pts',(4.55972548438599,-28.6555482313965,
54.0160990067003));
#111573=CARTESIAN_POINT('Ctrl Pts',(4.55922822850234,-28.6599701338663,
54.0100850161533));
#111574=CARTESIAN_POINT('Ctrl Pts',(4.55832621899242,-28.6680191659258,
53.9992907197034));
#111575=CARTESIAN_POINT('Ctrl Pts',(4.55792244375978,-28.6716319077777,
53.9945000176292));
#111576=CARTESIAN_POINT('Ctrl Pts',(4.55700849506298,-28.6798308344944,
53.9837490815523));
#111577=CARTESIAN_POINT('Ctrl Pts',(4.55649734960544,-28.6844315057099,
53.9778003687513));
#111578=CARTESIAN_POINT('Ctrl Pts',(4.55492930737978,-28.6985959399777,
53.9597396288654));
#111579=CARTESIAN_POINT('Ctrl Pts',(4.5538641646634,-28.7082875573673,53.9477295545404));
#111580=CARTESIAN_POINT('Ctrl Pts',(4.54544931006988,-28.7854979288526,
53.854722779957));
#111581=CARTESIAN_POINT('Ctrl Pts',(4.53771813303804,-28.8603967164886,
53.7801737291206));
#111582=CARTESIAN_POINT('Ctrl Pts',(4.522227603577,-29.0249939948267,53.6448201398954));
#111583=CARTESIAN_POINT('Ctrl Pts',(4.51451177172979,-29.1146045093627,
53.5846443771792));
#111584=CARTESIAN_POINT('Ctrl Pts',(4.5056353911302,-29.2284394062949,53.5232747213344));
#111585=CARTESIAN_POINT('Ctrl Pts',(4.50416452543651,-29.2476660519554,
53.513387405793));
#111586=CARTESIAN_POINT('Ctrl Pts',(4.501880716072,-29.2780803446503,53.4984880803524));
#111587=CARTESIAN_POINT('Ctrl Pts',(4.50105898371458,-29.2891395320179,
53.4932208381553));
#111588=CARTESIAN_POINT('Ctrl Pts',(4.49952969482263,-29.309934375398,53.4835966343295));
#111589=CARTESIAN_POINT('Ctrl Pts',(4.49882115655741,-29.3196556590131,
53.4792102971145));
#111590=CARTESIAN_POINT('Ctrl Pts',(4.49723840278723,-29.3415620830002,
53.4695780044849));
#111591=CARTESIAN_POINT('Ctrl Pts',(4.49636597671586,-29.3537692006748,
53.4643835941725));
#111592=CARTESIAN_POINT('Ctrl Pts',(4.4941374604437,-29.3852789953532,53.4514177398141));
#111593=CARTESIAN_POINT('Ctrl Pts',(4.49278855206704,-29.4046679148364,
53.4438609638078));
#111594=CARTESIAN_POINT('Ctrl Pts',(4.483078113687,-29.5463746798032,53.3916675330745));
#111595=CARTESIAN_POINT('Ctrl Pts',(4.47521287643015,-29.6734091076345,
53.3611432843665));
#111596=CARTESIAN_POINT('Ctrl Pts',(4.4622135647754,-29.8843073632692,53.3359916571011));
#111597=CARTESIAN_POINT('Ctrl Pts',(4.45714744851914,-29.9665012394781,
53.3323120954081));
#111598=CARTESIAN_POINT('Ctrl Pts',(4.45087209574492,-30.0629173671654,
53.3351270271916));
#111599=CARTESIAN_POINT('Ctrl Pts',(4.44993322119866,-30.0772089392624,
53.3357285807938));
#111600=CARTESIAN_POINT('Ctrl Pts',(4.448500771071,-30.0987773611785,53.3369148267931));
#111601=CARTESIAN_POINT('Ctrl Pts',(4.44801432582664,-30.1060614384736,
53.3373634712672));
#111602=CARTESIAN_POINT('Ctrl Pts',(4.44712267861577,-30.119334133906,53.3382685430023));
#111603=CARTESIAN_POINT('Ctrl Pts',(4.44671832857179,-30.1253235398353,
53.3387095144197));
#111604=CARTESIAN_POINT('Ctrl Pts',(4.44579103866265,-30.1389918948557,
53.3397901859565));
#111605=CARTESIAN_POINT('Ctrl Pts',(4.44526698842956,-30.1466688473069,
53.340450779032));
#111606=CARTESIAN_POINT('Ctrl Pts',(4.44361840258863,-30.1706796672498,
53.3426847848211));
#111607=CARTESIAN_POINT('Ctrl Pts',(4.44248439516168,-30.1869944829755,
53.3444462303274));
#111608=CARTESIAN_POINT('Ctrl Pts',(4.43561061410905,-30.2848382865128,
53.3564746852698));
#111609=CARTESIAN_POINT('Ctrl Pts',(4.42964240513635,-30.3655356789864,
53.3725205216777));
#111610=CARTESIAN_POINT('Ctrl Pts',(4.41714937591296,-30.5309443749194,
53.4183361143562));
#111611=CARTESIAN_POINT('Ctrl Pts',(4.41064528395722,-30.6151209513739,
53.4491319388265));
#111612=CARTESIAN_POINT('Ctrl Pts',(4.4008181228388,-30.7414845882965,53.5072786049749));
#111613=CARTESIAN_POINT('Ctrl Pts',(4.3973717343108,-30.7856017552619,53.5300179202062));
#111614=CARTESIAN_POINT('Ctrl Pts',(4.39285939822965,-30.8430831877679,
53.5629739655451));
#111615=CARTESIAN_POINT('Ctrl Pts',(4.3917335413244,-30.857399528334,53.5714695771727));
#111616=CARTESIAN_POINT('Ctrl Pts',(4.38986293367065,-30.8811347994737,
53.5860399620916));
#111617=CARTESIAN_POINT('Ctrl Pts',(4.38911398560713,-30.8906238257837,
53.5919976082481));
#111618=CARTESIAN_POINT('Ctrl Pts',(4.38764296689,-30.9092295081736,53.603942466339));
#111619=CARTESIAN_POINT('Ctrl Pts',(4.38692074810337,-30.9183488878025,
53.6099243669145));
#111620=CARTESIAN_POINT('Ctrl Pts',(4.385168041037,-30.940436928269,53.6247253656872));
#111621=CARTESIAN_POINT('Ctrl Pts',(4.38414115693104,-30.9533412349638,
53.633638974095));
#111622=CARTESIAN_POINT('Ctrl Pts',(4.38060684533501,-30.9975984047242,
53.6651417489173));
#111623=CARTESIAN_POINT('Ctrl Pts',(4.37813403593957,-31.0282912511862,
53.6886394125771));
#111624=CARTESIAN_POINT('Ctrl Pts',(4.36817806968181,-31.1500651240415,
53.7887733989361));
#111625=CARTESIAN_POINT('Ctrl Pts',(4.36102682012918,-31.2336237046339,
53.8739923280919));
#111626=CARTESIAN_POINT('Ctrl Pts',(4.34961635713186,-31.3487101084422,
54.0197035987373));
#111627=CARTESIAN_POINT('Ctrl Pts',(4.34547200827575,-31.3868473824026,
54.0744448297454));
#111628=CARTESIAN_POINT('Ctrl Pts',(4.34011993749505,-31.4298737934105,
54.1448574557848));
#111629=CARTESIAN_POINT('Ctrl Pts',(4.33908076338134,-31.43795409721,54.1585157129639));
#111630=CARTESIAN_POINT('Ctrl Pts',(4.3375262473493,-31.4496155212339,54.1788857206626));
#111631=CARTESIAN_POINT('Ctrl Pts',(4.33701997170316,-31.4533480218838,
54.1855103801808));
#111632=CARTESIAN_POINT('Ctrl Pts',(4.33610890578113,-31.4599452860549,
54.1974093290067));
#111633=CARTESIAN_POINT('Ctrl Pts',(4.33570519762758,-31.4628270807533,
54.2026738730948));
#111634=CARTESIAN_POINT('Ctrl Pts',(4.3348005663061,-31.4691919254312,54.2144520118825));
#111635=CARTESIAN_POINT('Ctrl Pts',(4.33429877277393,-31.472660102355,54.2209731884658));
#111636=CARTESIAN_POINT('Ctrl Pts',(4.33278758738486,-31.4829222481296,
54.2405824194703));
#111637=CARTESIAN_POINT('Ctrl Pts',(4.33177076520623,-31.489585718095,54.2537374411038));
#111638=CARTESIAN_POINT('Ctrl Pts',(4.32288193049175,-31.5458341430318,
54.3685386905486));
#111639=CARTESIAN_POINT('Ctrl Pts',(4.31456663493016,-31.5851202866657,
54.4748935993468));
#111640=CARTESIAN_POINT('Ctrl Pts',(4.29902897515919,-31.6385095041705,
54.6821459150766));
#111641=CARTESIAN_POINT('Ctrl Pts',(4.29181562246724,-31.6547580337849,
54.7819936210726));
#111642=CARTESIAN_POINT('Ctrl Pts',(4.28339373083651,-31.6633951059486,
54.9043743263053));
#111643=CARTESIAN_POINT('Ctrl Pts',(4.2819160403144,-31.6645002647794,54.9260642591598));
#111644=CARTESIAN_POINT('Ctrl Pts',(4.27962408977165,-31.6655657412128,
54.9600337944312));
#111645=CARTESIAN_POINT('Ctrl Pts',(4.2788009375129,-31.6658149139237,54.9723012203511));
#111646=CARTESIAN_POINT('Ctrl Pts',(4.27727034224551,-31.6660272999848,
54.9952327216606));
#111647=CARTESIAN_POINT('Ctrl Pts',(4.27656190223701,-31.6660236913173,
55.0058957819017));
#111648=CARTESIAN_POINT('Ctrl Pts',(4.27498107070525,-31.6657861469652,
55.0297949516669));
#111649=CARTESIAN_POINT('Ctrl Pts',(4.27411044877809,-31.665496824531,55.0430298835917));
#111650=CARTESIAN_POINT('Ctrl Pts',(4.27188990265222,-31.6643503819525,
55.0769593938813));
#111651=CARTESIAN_POINT('Ctrl Pts',(4.27054707101667,-31.6632650371319,
55.0976443502016));
#111652=CARTESIAN_POINT('Ctrl Pts',(4.2594866804815,-31.651052387174,55.2691925189657));
#111653=CARTESIAN_POINT('Ctrl Pts',(4.25046988720103,-31.6198129178493,
55.4179068699138));
#111654=CARTESIAN_POINT('Ctrl Pts',(4.23743998382687,-31.5487380940279,
55.616903896742));
#111655=CARTESIAN_POINT('Ctrl Pts',(4.23368794479393,-31.5255061695279,
55.6723016491408));
#111656=CARTESIAN_POINT('Ctrl Pts',(4.22880675416902,-31.4927428213331,
55.7399349819324));
#111657=CARTESIAN_POINT('Ctrl Pts',(4.22781494287351,-31.4859618934619,
55.7534600984559));
#111658=CARTESIAN_POINT('Ctrl Pts',(4.22631796239106,-31.4755633446396,
55.7735143760035));
#111659=CARTESIAN_POINT('Ctrl Pts',(4.22582091840187,-31.4720843017999,
55.7801150408666));
#111660=CARTESIAN_POINT('Ctrl Pts',(4.22491911749055,-31.4657276486024,
55.7919813548612));
#111661=CARTESIAN_POINT('Ctrl Pts',(4.2245153365082,-31.4628657704036,55.7972551292189));
#111662=CARTESIAN_POINT('Ctrl Pts',(4.22360115058551,-31.4563512872595,
55.8091066267131));
#111663=CARTESIAN_POINT('Ctrl Pts',(4.22308977112509,-31.4526826068413,
55.8156750845549));
#111664=CARTESIAN_POINT('Ctrl Pts',(4.22152029045961,-31.4413446078695,
55.83565568618));
#111665=CARTESIAN_POINT('Ctrl Pts',(4.22045392214018,-31.4335333431051,
55.848985757357));
#111666=CARTESIAN_POINT('Ctrl Pts',(4.21206353661835,-31.3711586920197,
55.9521137626122));
#111667=CARTESIAN_POINT('Ctrl Pts',(4.2043607910329,-31.3083999367107,56.0366691711607));
#111668=CARTESIAN_POINT('Ctrl Pts',(4.18875597665751,-31.1647656503903,
56.1961981873379));
#111669=CARTESIAN_POINT('Ctrl Pts',(4.18090317924967,-31.0835570647785,
56.2702288097924));
#111670=CARTESIAN_POINT('Ctrl Pts',(4.17196571236912,-30.9790234395173,
56.3481465552009));
#111671=CARTESIAN_POINT('Ctrl Pts',(4.17055605016112,-30.9621663993536,
56.3602286266402));
#111672=CARTESIAN_POINT('Ctrl Pts',(4.16834536007593,-30.9351525385659,
56.3788369258308));
#111673=CARTESIAN_POINT('Ctrl Pts',(4.16753644962788,-30.9251433248385,
56.3855725820712));
#111674=CARTESIAN_POINT('Ctrl Pts',(4.16601860007384,-30.9061300254342,
56.3980696023578));
#111675=CARTESIAN_POINT('Ctrl Pts',(4.16530881937272,-30.8971419947323,
56.4038541542522));
#111676=CARTESIAN_POINT('Ctrl Pts',(4.16370694898828,-30.8766410822502,
56.4167709075377));
#111677=CARTESIAN_POINT('Ctrl Pts',(4.16281684299518,-30.8650955627986,
56.4238500892831));
#111678=CARTESIAN_POINT('Ctrl Pts',(4.16050974938813,-30.8347804155901,
56.4419330692133));
#111679=CARTESIAN_POINT('Ctrl Pts',(4.15910085133093,-30.815878943252,56.4527115811984));
#111680=CARTESIAN_POINT('Ctrl Pts',(4.14831711560297,-30.6683914941956,
56.5330289548121));
#111681=CARTESIAN_POINT('Ctrl Pts',(4.1395835121069,-30.5313752272314,56.5857386897001));
#111682=CARTESIAN_POINT('Ctrl Pts',(4.1277278313492,-30.3441572616773,56.6307240559534));
#111683=CARTESIAN_POINT('Ctrl Pts',(4.12484548830372,-30.2986516729565,
56.6396681855563));
#111684=CARTESIAN_POINT('Ctrl Pts',(4.12015853858643,-30.2259539257416,
56.6508302438842));
#111685=CARTESIAN_POINT('Ctrl Pts',(4.11840145701979,-30.1989768295528,
56.6542985494061));
#111686=CARTESIAN_POINT('Ctrl Pts',(4.11599532056623,-30.1626246429899,
56.6580701810744));
#111687=CARTESIAN_POINT('Ctrl Pts',(4.11537559377679,-30.1533127533312,
56.6589571089811));
#111688=CARTESIAN_POINT('Ctrl Pts',(4.11433490021571,-30.1377711863339,
56.6603054288524));
#111689=CARTESIAN_POINT('Ctrl Pts',(4.1139163008067,-30.131545313265,56.6608102978583));
#111690=CARTESIAN_POINT('Ctrl Pts',(4.11305876459616,-30.1188465916916,
56.6617682117781));
#111691=CARTESIAN_POINT('Ctrl Pts',(4.11261969730611,-30.1123737091335,
56.6622184717697));
#111692=CARTESIAN_POINT('Ctrl Pts',(4.11146557317384,-30.0954304551078,
56.6632976440805));
#111693=CARTESIAN_POINT('Ctrl Pts',(4.11074730601297,-30.08495667814,56.6638654913282));
#111694=CARTESIAN_POINT('Ctrl Pts',(4.10764834969443,-30.0400404992496,
56.6658754799896));
#111695=CARTESIAN_POINT('Ctrl Pts',(4.10522278003539,-30.0055655661888,
56.6663472017879));
#111696=CARTESIAN_POINT('Ctrl Pts',(4.09512949626596,-29.8639607440026,
56.6638907429518));
#111697=CARTESIAN_POINT('Ctrl Pts',(4.08723575310939,-29.7572488287963,
56.6516994522656));
#111698=CARTESIAN_POINT('Ctrl Pts',(4.07545478092333,-29.5975221193336,
56.6176283697018));
#111699=CARTESIAN_POINT('Ctrl Pts',(4.0714518503984,-29.543220820414,56.6031418548263));
#111700=CARTESIAN_POINT('Ctrl Pts',(4.06492484580193,-29.4543116654028,
56.5745368063034));
#111701=CARTESIAN_POINT('Ctrl Pts',(4.06235864332962,-29.4192627504,56.5619495957426));
#111702=CARTESIAN_POINT('Ctrl Pts',(4.05880921038728,-29.3706808727808,
56.5426405296941));
#111703=CARTESIAN_POINT('Ctrl Pts',(4.05779406452489,-29.3567747521713,
56.5368941648966));
#111704=CARTESIAN_POINT('Ctrl Pts',(4.05605441962116,-29.3329310158615,
56.5266609943642));
#111705=CARTESIAN_POINT('Ctrl Pts',(4.05532694819434,-29.3229562883377,
56.5222636576955));
#111706=CARTESIAN_POINT('Ctrl Pts',(4.05393561719765,-29.3038755060226,
56.5136272847745));
#111707=CARTESIAN_POINT('Ctrl Pts',(4.05327128487744,-29.294763252735,56.5094031953438));
#111708=CARTESIAN_POINT('Ctrl Pts',(4.05152828726064,-29.2708566692665,
56.4980572668541));
#111709=CARTESIAN_POINT('Ctrl Pts',(4.05045438316149,-29.2561282163702,
56.4907985687313));
#111710=CARTESIAN_POINT('Ctrl Pts',(4.04654743223306,-29.2025869646305,
56.4634204772381));
#111711=CARTESIAN_POINT('Ctrl Pts',(4.04375994240473,-29.1644610870358,
56.4419924659824));
#111712=CARTESIAN_POINT('Ctrl Pts',(4.03383248155881,-29.0299387395775,
56.3592573039316));
#111713=CARTESIAN_POINT('Ctrl Pts',(4.02696968234985,-28.939069625645,56.2895838950884));
#111714=CARTESIAN_POINT('Ctrl Pts',(4.01698224638606,-28.8210110952625,
56.1780759261994));
#111715=CARTESIAN_POINT('Ctrl Pts',(4.01399126515501,-28.7874358938281,
56.1434882484943));
#111716=CARTESIAN_POINT('Ctrl Pts',(4.00914829142771,-28.7368695567408,
56.0866624481503));
#111717=CARTESIAN_POINT('Ctrl Pts',(4.00734777507053,-28.7188573426948,
56.0653671051593));
#111718=CARTESIAN_POINT('Ctrl Pts',(4.00489109669797,-28.6954762554006,
56.0362735644389));
#111719=CARTESIAN_POINT('Ctrl Pts',(4.00426585454349,-28.6896260048181,
56.0288659207905));
#111720=CARTESIAN_POINT('Ctrl Pts',(4.00321848191607,-28.6799990377026,
56.0164608660014));
#111721=CARTESIAN_POINT('Ctrl Pts',(4.00279878496326,-28.6761868804898,
56.0114910059185));
#111722=CARTESIAN_POINT('Ctrl Pts',(4.00194178692412,-28.6684971252078,
56.0013480365853));
#111723=CARTESIAN_POINT('Ctrl Pts',(4.00150437897295,-28.6646214671163,
55.996173662705));
#111724=CARTESIAN_POINT('Ctrl Pts',(4.00035939204268,-28.6546012462752,
55.9826321582129));
#111725=CARTESIAN_POINT('Ctrl Pts',(3.99964869153961,-28.6485047112594,
55.9742300732526));
#111726=CARTESIAN_POINT('Ctrl Pts',(3.99662843692014,-28.6230961752453,
55.9385152084614));
#111727=CARTESIAN_POINT('Ctrl Pts',(3.99427666864257,-28.6045318480446,
55.9106828325461));
#111728=CARTESIAN_POINT('Ctrl Pts',(3.98422447510363,-28.5297646077199,
55.7909298343998));
#111729=CARTESIAN_POINT('Ctrl Pts',(3.97628765621781,-28.4817092264681,
55.694229975399));
#111730=CARTESIAN_POINT('Ctrl Pts',(3.96805085260525,-28.4410366537565,
55.5875632574752));
#111731=CARTESIAN_POINT('Ctrl Pts',(3.96758778209095,-28.4387819867155,
55.5815458727116));
#111732=CARTESIAN_POINT('Ctrl Pts',(3.96712537028317,-28.4365623116664,
55.5755159378315));
#111733=CARTESIAN_POINT('Origin',(5.,-30.,55.));
#111734=CARTESIAN_POINT('',(3.26653910946692,-28.436562310676,55.575515935141));
#111735=CARTESIAN_POINT('',(3.46016010521239,-28.436562259669,55.5755157965761));
#111736=CARTESIAN_POINT('',(5.,-28.4365623102018,55.5755159338528));
#111737=CARTESIAN_POINT('',(4.12032058488633,-28.3340002417459,54.9991025049737));
#111738=CARTESIAN_POINT('Ctrl Pts',(3.46016010521239,-28.436562259669,55.5755157965761));
#111739=CARTESIAN_POINT('Ctrl Pts',(3.46533507067826,-28.4612024188361,
55.6424528902211));
#111740=CARTESIAN_POINT('Ctrl Pts',(3.47055209814345,-28.4901263132498,
55.7077667856819));
#111741=CARTESIAN_POINT('Ctrl Pts',(3.4816728450369,-28.561500676386,55.8444740038002));
#111742=CARTESIAN_POINT('Ctrl Pts',(3.48753193624495,-28.6052619862572,
55.9149460362316));
#111743=CARTESIAN_POINT('Ctrl Pts',(3.4945442331466,-28.6656515254426,55.9977248446239));
#111744=CARTESIAN_POINT('Ctrl Pts',(3.49587587405831,-28.6774907555878,
56.0133657151434));
#111745=CARTESIAN_POINT('Ctrl Pts',(3.49799327515109,-28.6969081840013,
56.0380980826434));
#111746=CARTESIAN_POINT('Ctrl Pts',(3.49878581952017,-28.7043115090283,
56.0473238548627));
#111747=CARTESIAN_POINT('Ctrl Pts',(3.50029048938778,-28.7186233711836,
56.0647747587509));
#111748=CARTESIAN_POINT('Ctrl Pts',(3.50100326721198,-28.7255143901523,
56.0730134161581));
#111749=CARTESIAN_POINT('Ctrl Pts',(3.50263620373059,-28.741555089818,56.0918185523204));
#111750=CARTESIAN_POINT('Ctrl Pts',(3.50355407445497,-28.7507591137388,
56.1023377753521));
#111751=CARTESIAN_POINT('Ctrl Pts',(3.50646359854809,-28.7805221397302,
56.1355021517643));
#111752=CARTESIAN_POINT('Ctrl Pts',(3.50843461858365,-28.8015734698569,
56.1576983321546));
#111753=CARTESIAN_POINT('Ctrl Pts',(3.51308990961696,-28.8532907294034,
56.2093047022373));
#111754=CARTESIAN_POINT('Ctrl Pts',(3.51575165480754,-28.8844940383775,
56.2381465353354));
#111755=CARTESIAN_POINT('Ctrl Pts',(3.52295598512166,-28.9727797848721,
56.3137007959192));
#111756=CARTESIAN_POINT('Ctrl Pts',(3.52743086962242,-29.0319135147452,
56.3578660005447));
#111757=CARTESIAN_POINT('Ctrl Pts',(3.53278088196181,-29.1052964903932,
56.4054358932715));
#111758=CARTESIAN_POINT('Ctrl Pts',(3.53362178043204,-29.1169064909165,
56.4127598057533));
#111759=CARTESIAN_POINT('Ctrl Pts',(3.53899018210172,-29.1914013093267,
56.458476102786));
#111760=CARTESIAN_POINT('Ctrl Pts',(3.54357009068761,-29.2566766513578,
56.4928000648305));
#111761=CARTESIAN_POINT('Ctrl Pts',(3.54918363924978,-29.3352220551691,
56.5276704678041));
#111762=CARTESIAN_POINT('Ctrl Pts',(3.5499920180097,-29.3464991429991,56.5325284278827));
#111763=CARTESIAN_POINT('Ctrl Pts',(3.55126921776027,-29.3642418616072,
56.5399402256163));
#111764=CARTESIAN_POINT('Ctrl Pts',(3.55173316131602,-29.3706717949457,
56.5425791114077));
#111765=CARTESIAN_POINT('Ctrl Pts',(3.55260580793278,-29.3827331852131,
56.5474412216904));
#111766=CARTESIAN_POINT('Ctrl Pts',(3.55301393648577,-29.3883604910852,
56.5496740824049));
#111767=CARTESIAN_POINT('Ctrl Pts',(3.55398031389767,-29.4016542852369,
56.5548652455937));
#111768=CARTESIAN_POINT('Ctrl Pts',(3.55454004827901,-29.4093306284353,
56.5577975519136));
#111769=CARTESIAN_POINT('Ctrl Pts',(3.55642513769437,-29.4351150229484,
56.5674290233935));
#111770=CARTESIAN_POINT('Ctrl Pts',(3.55776404703404,-29.4533170357476,
56.5738698922835));
#111771=CARTESIAN_POINT('Ctrl Pts',(3.56109729789562,-29.4984526808686,
56.5889639546728));
#111772=CARTESIAN_POINT('Ctrl Pts',(3.56310623189366,-29.5255021717906,
56.5972500721407));
#111773=CARTESIAN_POINT('Ctrl Pts',(3.57231570895063,-29.6493106982567,
56.6317541477482));
#111774=CARTESIAN_POINT('Ctrl Pts',(3.57968871738581,-29.7481045565724,
56.6498950674548));
#111775=CARTESIAN_POINT('Ctrl Pts',(3.59286273765847,-29.9300606427894,
56.666573260525));
#111776=CARTESIAN_POINT('Ctrl Pts',(3.59869576996069,-30.0126457335807,
56.6679933202466));
#111777=CARTESIAN_POINT('Ctrl Pts',(3.60568291042129,-30.1145793844572,
56.6621708288185));
#111778=CARTESIAN_POINT('Ctrl Pts',(3.60701381194024,-30.1341304728216,
56.660707491624));
#111779=CARTESIAN_POINT('Ctrl Pts',(3.6091303264183,-30.1654276195149,56.6578086618428));
#111780=CARTESIAN_POINT('Ctrl Pts',(3.60992271348219,-30.1771916203264,
56.6565925868325));
#111781=CARTESIAN_POINT('Ctrl Pts',(3.6114272615719,-30.1996134157015,56.6540332065644));
#111782=CARTESIAN_POINT('Ctrl Pts',(3.61214007307276,-30.2102730664417,
56.6527118959124));
#111783=CARTESIAN_POINT('Ctrl Pts',(3.61377333599463,-30.2347769944241,
56.6494336096584));
#111784=CARTESIAN_POINT('Ctrl Pts',(3.61469149623948,-30.2486110288411,
56.6474052463979));
#111785=CARTESIAN_POINT('Ctrl Pts',(3.61760298378825,-30.2926462580163,
56.6403814030073));
#111786=CARTESIAN_POINT('Ctrl Pts',(3.61957563716275,-30.3227370362852,
56.634727492153));
#111787=CARTESIAN_POINT('Ctrl Pts',(3.62423561685806,-30.3942162897078,
56.6192460450048));
#111788=CARTESIAN_POINT('Ctrl Pts',(3.62690035273671,-30.435418097124,56.6086564886076));
#111789=CARTESIAN_POINT('Ctrl Pts',(3.6341062637875,-30.5468017408791,56.5754352462528));
#111790=CARTESIAN_POINT('Ctrl Pts',(3.63857993307601,-30.6159574009169,
56.5497048762593));
#111791=CARTESIAN_POINT('Ctrl Pts',(3.64394271292471,-30.6959079561773,
56.5137578416862));
#111792=CARTESIAN_POINT('Ctrl Pts',(3.64479751632439,-30.7085613637542,
56.5078764785417));
#111793=CARTESIAN_POINT('Ctrl Pts',(3.6501623613977,-30.7872918596637,56.4700723375306));
#111794=CARTESIAN_POINT('Ctrl Pts',(3.65472492856013,-30.8512653739252,
56.4339754843858));
#111795=CARTESIAN_POINT('Ctrl Pts',(3.66031922293849,-30.9229147782607,
56.3870598614524));
#111796=CARTESIAN_POINT('Ctrl Pts',(3.66112753103553,-30.933111520811,56.3802208573828));
#111797=CARTESIAN_POINT('Ctrl Pts',(3.66240464314722,-30.9489603845603,
56.3693350554648));
#111798=CARTESIAN_POINT('Ctrl Pts',(3.66286857080968,-30.9546645855542,
56.3653643580756));
#111799=CARTESIAN_POINT('Ctrl Pts',(3.66374120540813,-30.9652909567697,
56.3578681911965));
#111800=CARTESIAN_POINT('Ctrl Pts',(3.66414933803981,-30.9702189693318,
56.3543514325137));
#111801=CARTESIAN_POINT('Ctrl Pts',(3.66511574942603,-30.9817907538313,
56.3459979380169));
#111802=CARTESIAN_POINT('Ctrl Pts',(3.6656755140195,-30.9884180268185,56.3411388185554));
#111803=CARTESIAN_POINT('Ctrl Pts',(3.66756081403966,-31.0104967772053,
56.3246981333178));
#111804=CARTESIAN_POINT('Ctrl Pts',(3.66889990773721,-31.0257821586928,
56.3128974691884));
#111805=CARTESIAN_POINT('Ctrl Pts',(3.67223372046557,-31.0629492180813,
56.2831583764351));
#111806=CARTESIAN_POINT('Ctrl Pts',(3.67424303785215,-31.0845852220542,
56.2649233868526));
#111807=CARTESIAN_POINT('Ctrl Pts',(3.68345592262898,-31.1807565686212,
56.1795875781764));
#111808=CARTESIAN_POINT('Ctrl Pts',(3.6908320486152,-31.2496045598371,56.1063913594428));
#111809=CARTESIAN_POINT('Ctrl Pts',(3.70400536495773,-31.3622862393517,
55.9625623488482));
#111810=CARTESIAN_POINT('Ctrl Pts',(3.70983489406662,-31.4082404947078,
55.8939868349359));
#111811=CARTESIAN_POINT('Ctrl Pts',(3.71681864975773,-31.4586091730715,
55.8052325889746));
#111812=CARTESIAN_POINT('Ctrl Pts',(3.7181494496141,-31.4679828039877,55.7880144581521));
#111813=CARTESIAN_POINT('Ctrl Pts',(3.72026584218626,-31.4825209316052,
55.7601496803738));
#111814=CARTESIAN_POINT('Ctrl Pts',(3.72105820762084,-31.4878794624363,
55.7496069416447));
#111815=CARTESIAN_POINT('Ctrl Pts',(3.72256273897859,-31.4978898526126,
55.7293814881765));
#111816=CARTESIAN_POINT('Ctrl Pts',(3.7232755551223,-31.5025611900257,55.7197091393741));
#111817=CARTESIAN_POINT('Ctrl Pts',(3.72490886298606,-31.5130972652106,
55.6973436407032));
#111818=CARTESIAN_POINT('Ctrl Pts',(3.72582706308861,-31.5188964588693,
55.6846203723183));
#111819=CARTESIAN_POINT('Ctrl Pts',(3.72873882102058,-31.5368801186652,
55.6438110745932));
#111820=CARTESIAN_POINT('Ctrl Pts',(3.73071169932679,-31.5484513546906,
55.6154606320993));
#111821=CARTESIAN_POINT('Ctrl Pts',(3.7353723248432,-31.5742155165618,55.5470012129056));
#111822=CARTESIAN_POINT('Ctrl Pts',(3.73803747269969,-31.5876666826755,
55.5066356725296));
#111823=CARTESIAN_POINT('Ctrl Pts',(3.74524358970001,-31.6201652502446,
55.3950348188002));
#111824=CARTESIAN_POINT('Ctrl Pts',(3.74971708030216,-31.6360535934458,
55.3229813453965));
#111825=CARTESIAN_POINT('Ctrl Pts',(3.75508132925589,-31.6492173559422,
55.2362912268376));
#111826=CARTESIAN_POINT('Ctrl Pts',(3.7559377695857,-31.651142025191,55.2224442348912));
#111827=CARTESIAN_POINT('Ctrl Pts',(3.76130212598135,-31.6620749542148,
55.1358040696191));
#111828=CARTESIAN_POINT('Ctrl Pts',(3.76586258171806,-31.6664408270576,
55.0625151886453));
#111829=CARTESIAN_POINT('Ctrl Pts',(3.77145453224788,-31.6658852283461,
54.9769099621336));
#111830=CARTESIAN_POINT('Ctrl Pts',(3.77226283165594,-31.6656698286316,
54.9646341393723));
#111831=CARTESIAN_POINT('Ctrl Pts',(3.77353993299118,-31.6651200478486,
54.9454149157525));
#111832=CARTESIAN_POINT('Ctrl Pts',(3.77400385869929,-31.6648778456966,
54.938469034597));
#111833=CARTESIAN_POINT('Ctrl Pts',(3.77487649182004,-31.6643433506988,
54.9254757291173));
#111834=CARTESIAN_POINT('Ctrl Pts',(3.77528462495342,-31.6640615444062,
54.9194281208315));
#111835=CARTESIAN_POINT('Ctrl Pts',(3.77625104051829,-31.6633195249161,
54.9051754653926));
#111836=CARTESIAN_POINT('Ctrl Pts',(3.77681080882754,-31.6628315570884,
54.8969721396775));
#111837=CARTESIAN_POINT('Ctrl Pts',(3.77869613475052,-31.6609937109529,
54.8695056104935));
#111838=CARTESIAN_POINT('Ctrl Pts',(3.78003525112307,-31.6593696638124,
54.8502631212124));
#111839=CARTESIAN_POINT('Ctrl Pts',(3.78336913296018,-31.6545424981376,
54.8029070838807));
#111840=CARTESIAN_POINT('Ctrl Pts',(3.7853784975037,-31.6509569595678,54.7748390961061));
#111841=CARTESIAN_POINT('Ctrl Pts',(3.79459180154555,-31.6314213865786,
54.6477526221542));
#111842=CARTESIAN_POINT('Ctrl Pts',(3.80196831110846,-31.6072648526433,
54.5502065840207));
#111843=CARTESIAN_POINT('Ctrl Pts',(3.81514154092422,-31.5475406464638,
54.377531484538));
#111844=CARTESIAN_POINT('Ctrl Pts',(3.82097063911164,-31.5148531962473,
54.301736026339));
#111845=CARTESIAN_POINT('Ctrl Pts',(3.82795397840051,-31.4676077985264,
54.2112873877401));
#111846=CARTESIAN_POINT('Ctrl Pts',(3.82928476571399,-31.4582260962093,
54.1940738592707));
#111847=CARTESIAN_POINT('Ctrl Pts',(3.83140114324562,-31.4427007411339,
54.1667470853075));
#111848=CARTESIAN_POINT('Ctrl Pts',(3.83219350601165,-31.4367496184512,
54.1565271820183));
#111849=CARTESIAN_POINT('Ctrl Pts',(3.8336980353053,-31.4251866204119,54.1371474847553));
#111850=CARTESIAN_POINT('Ctrl Pts',(3.83441085202203,-31.4195940172651,
54.1279769490283));
#111851=CARTESIAN_POINT('Ctrl Pts',(3.83604416543163,-31.4065181254434,
54.1069948196298));
#111852=CARTESIAN_POINT('Ctrl Pts',(3.83696237045255,-31.398973982648,54.0952219581659));
#111853=CARTESIAN_POINT('Ctrl Pts',(3.83987416175062,-31.3744417056323,
54.0579791808063));
#111854=CARTESIAN_POINT('Ctrl Pts',(3.84184706781425,-31.3568988139562,
54.0328810707788));
#111855=CARTESIAN_POINT('Ctrl Pts',(3.84650777302961,-31.3133557949168,
53.9741045631673));
#111856=CARTESIAN_POINT('Ctrl Pts',(3.84917297172773,-31.2867377822684,
53.9409102249999));
#111857=CARTESIAN_POINT('Ctrl Pts',(3.85637911395052,-31.2106025379552,
53.8530782982882));
#111858=CARTESIAN_POINT('Ctrl Pts',(3.86085258231618,-31.1586846644668,
53.8006509653216));
#111859=CARTESIAN_POINT('Ctrl Pts',(3.86621700799498,-31.0929898031349,
53.7425721447289));
#111860=CARTESIAN_POINT('Ctrl Pts',(3.86707364594395,-31.0823977313833,
53.7334429874551));
#111861=CARTESIAN_POINT('Ctrl Pts',(3.87243794205832,-31.015537602767,53.6772684931629));
#111862=CARTESIAN_POINT('Ctrl Pts',(3.87699814160988,-30.956335654659,53.6338540861278));
#111863=CARTESIAN_POINT('Ctrl Pts',(3.88258980776084,-30.8841173114052,
53.587894011364));
#111864=CARTESIAN_POINT('Ctrl Pts',(3.8833981061131,-30.8736870466041,53.581417021706));
#111865=CARTESIAN_POINT('Ctrl Pts',(3.88467520613897,-30.8572419752615,
53.5714551106219));
#111866=CARTESIAN_POINT('Ctrl Pts',(3.88513913160962,-30.8512750792828,
53.5678914007186));
#111867=CARTESIAN_POINT('Ctrl Pts',(3.88601176455082,-30.8400689488414,
53.5612933526364));
#111868=CARTESIAN_POINT('Ctrl Pts',(3.88641989774516,-30.8348352473261,
53.5582501045202));
#111869=CARTESIAN_POINT('Ctrl Pts',(3.88738631381759,-30.822458519497,53.5511433755737));
#111870=CARTESIAN_POINT('Ctrl Pts',(3.88794608257821,-30.8153018862798,
53.5471041463385));
#111871=CARTESIAN_POINT('Ctrl Pts',(3.88983141164857,-30.7912292369109,
53.5337513206564));
#111872=CARTESIAN_POINT('Ctrl Pts',(3.89117053077613,-30.7741819237347,
53.5246793011302));
#111873=CARTESIAN_POINT('Ctrl Pts',(3.89450442100987,-30.7317778661351,
53.5030505503537));
#111874=CARTESIAN_POINT('Ctrl Pts',(3.89651379128293,-30.7062519868691,
53.4908398194811));
#111875=CARTESIAN_POINT('Ctrl Pts',(3.90572714626701,-30.5888850592815,
53.4383251082537));
#111876=CARTESIAN_POINT('Ctrl Pts',(3.91310370243606,-30.4938301291272,
53.4057144697383));
#111877=CARTESIAN_POINT('Ctrl Pts',(3.92627692173973,-30.3163660216553,
53.3622388672596));
#111878=CARTESIAN_POINT('Ctrl Pts',(3.93210596757001,-30.2349591536741,
53.3485924605103));
#111879=CARTESIAN_POINT('Ctrl Pts',(3.93908925626508,-30.1333458377287,
53.3392293590827));
#111880=CARTESIAN_POINT('Ctrl Pts',(3.94042004205404,-30.1137957260913,
53.3377753389391));
#111881=CARTESIAN_POINT('Ctrl Pts',(3.9425364177577,-30.0824169444836,53.335997807855));
#111882=CARTESIAN_POINT('Ctrl Pts',(3.94332878019931,-30.0706030880016,
53.3354546973279));
#111883=CARTESIAN_POINT('Ctrl Pts',(3.94483330924203,-30.048050008775,53.3346584246025));
#111884=CARTESIAN_POINT('Ctrl Pts',(3.9455461260284,-30.0373122139648,53.3343832451624));
#111885=CARTESIAN_POINT('Ctrl Pts',(3.94717944011199,-30.0125923084443,
53.3339889185848));
#111886=CARTESIAN_POINT('Ctrl Pts',(3.94809764573079,-29.9986097332567,
53.3339419048151));
#111887=CARTESIAN_POINT('Ctrl Pts',(3.95100944108458,-29.9540149647219,
53.3343533970871));
#111888=CARTESIAN_POINT('Ctrl Pts',(3.95298235052212,-29.923414261244,53.3354796359063));
#111889=CARTESIAN_POINT('Ctrl Pts',(3.95764306542494,-29.8504172318816,
53.340183776567));
#111890=CARTESIAN_POINT('Ctrl Pts',(3.96030827030289,-29.808092467181,53.3445433320651));
#111891=CARTESIAN_POINT('Ctrl Pts',(3.96751441558857,-29.6930079632713,
53.3608710307328));
#111892=CARTESIAN_POINT('Ctrl Pts',(3.97198788124859,-29.6208031332967,
53.3760548073667));
#111893=CARTESIAN_POINT('Ctrl Pts',(3.98145087481888,-29.471874998016,53.4178503811606));
#111894=CARTESIAN_POINT('Ctrl Pts',(3.98643588803758,-29.3956171781785,
53.4453837472909));
#111895=CARTESIAN_POINT('Ctrl Pts',(3.99272796473029,-29.3069340813158,
53.4849171505347));
#111896=CARTESIAN_POINT('Ctrl Pts',(3.99378385082902,-29.2922919792224,
53.4917010512792));
#111897=CARTESIAN_POINT('Ctrl Pts',(3.99536579942446,-29.27075368414,53.5020627143139));
#111898=CARTESIAN_POINT('Ctrl Pts',(3.99588254882001,-29.2637797692355,
53.5054779804612));
#111899=CARTESIAN_POINT('Ctrl Pts',(3.99680463588934,-29.2514503874433,
53.5116231628943));
#111900=CARTESIAN_POINT('Ctrl Pts',(3.99720877349272,-29.2460854477374,
53.5143334905181));
#111901=CARTESIAN_POINT('Ctrl Pts',(3.99810471271478,-29.2342783552774,
53.5203787706192));
#111902=CARTESIAN_POINT('Ctrl Pts',(3.99859728165862,-29.2278433465843,
53.5237267470937));
#111903=CARTESIAN_POINT('Ctrl Pts',(4.00005306909992,-29.2089834454017,
53.533696132518));
#111904=CARTESIAN_POINT('Ctrl Pts',(4.00102296014675,-29.1966207411293,
53.5404329562588));
#111905=CARTESIAN_POINT('Ctrl Pts',(4.00784050609912,-29.1110213806209,
53.5884956873026));
#111906=CARTESIAN_POINT('Ctrl Pts',(4.01394266999757,-29.0409270220139,
53.6351543874145));
#111907=CARTESIAN_POINT('Ctrl Pts',(4.0293952595558,-28.8735844489236,53.7658241952184));
#111908=CARTESIAN_POINT('Ctrl Pts',(4.03868615453698,-28.7819389527459,
53.85617264269));
#111909=CARTESIAN_POINT('Ctrl Pts',(4.04895765924964,-28.6883939578906,
53.9725336430833));
#111910=CARTESIAN_POINT('Ctrl Pts',(4.05039121667119,-28.6755389650117,
53.9891584887335));
#111911=CARTESIAN_POINT('Ctrl Pts',(4.05271392806205,-28.6550495416177,
54.0167188082507));
#111912=CARTESIAN_POINT('Ctrl Pts',(4.05361034633035,-28.64722612561,54.0275101541731));
#111913=CARTESIAN_POINT('Ctrl Pts',(4.05521556900639,-28.6333727921665,
54.0471096729604));
#111914=CARTESIAN_POINT('Ctrl Pts',(4.05592612315437,-28.6272965001879,
54.0558840054014));
#111915=CARTESIAN_POINT('Ctrl Pts',(4.05744287378617,-28.6144492577345,
54.0748220359052));
#111916=CARTESIAN_POINT('Ctrl Pts',(4.05824804070232,-28.6077048660541,
54.0850030612331));
#111917=CARTESIAN_POINT('Ctrl Pts',(4.06045475455164,-28.5894362048065,
54.113250355165));
#111918=CARTESIAN_POINT('Ctrl Pts',(4.06184759497065,-28.5781473441289,
54.1314666120708));
#111919=CARTESIAN_POINT('Ctrl Pts',(4.06493627537763,-28.5536938984248,
54.1726810988376));
#111920=CARTESIAN_POINT('Ctrl Pts',(4.06662544909748,-28.5407200937467,
54.1957859911961));
#111921=CARTESIAN_POINT('Ctrl Pts',(4.07209536195944,-28.500141370793,54.2722703133314));
#111922=CARTESIAN_POINT('Ctrl Pts',(4.07580684446593,-28.4748711253273,
54.3268364918782));
#111923=CARTESIAN_POINT('Ctrl Pts',(4.0836312306726,-28.4275588387586,54.4454257478977));
#111924=CARTESIAN_POINT('Ctrl Pts',(4.0877288233016,-28.4063581487556,54.5096642743236));
#111925=CARTESIAN_POINT('Ctrl Pts',(4.09533197393208,-28.3749100600871,
54.6288655045144));
#111926=CARTESIAN_POINT('Ctrl Pts',(4.09881090675606,-28.3634129653081,
54.6833932601575));
#111927=CARTESIAN_POINT('Ctrl Pts',(4.10355711618487,-28.3518829483987,
54.7559080583615));
#111928=CARTESIAN_POINT('Ctrl Pts',(4.10471576887663,-28.3493774464063,
54.7734700553919));
#111929=CARTESIAN_POINT('Ctrl Pts',(4.10640909984927,-28.346166758398,54.7988695730129));
#111930=CARTESIAN_POINT('Ctrl Pts',(4.10693206266747,-28.3452358361631,
54.8066780002246));
#111931=CARTESIAN_POINT('Ctrl Pts',(4.1078614480346,-28.3436888460894,54.8204847663319));
#111932=CARTESIAN_POINT('Ctrl Pts',(4.10826660606492,-28.3430500097013,
54.826480301797));
#111933=CARTESIAN_POINT('Ctrl Pts',(4.10905777157065,-28.3418715261223,
54.8381409699613));
#111934=CARTESIAN_POINT('Ctrl Pts',(4.10944352491412,-28.341328355765,54.8438053916598));
#111935=CARTESIAN_POINT('Ctrl Pts',(4.1103115111552,-28.3401760698506,54.856506425341));
#111936=CARTESIAN_POINT('Ctrl Pts',(4.11079456179747,-28.3395826655597,
54.8635443068639));
#111937=CARTESIAN_POINT('Ctrl Pts',(4.11238834707366,-28.3377806470898,
54.8866722676899));
#111938=CARTESIAN_POINT('Ctrl Pts',(4.1135081812535,-28.3367610745716,54.9027756044905));
#111939=CARTESIAN_POINT('Ctrl Pts',(4.11650947216456,-28.3346732105405,
54.9456097457554));
#111940=CARTESIAN_POINT('Ctrl Pts',(4.11840674262356,-28.3340146510312,
54.9723548740222));
#111941=CARTESIAN_POINT('Ctrl Pts',(4.12032058488633,-28.3340002417459,
54.9991025049737));
#111942=CARTESIAN_POINT('Ctrl Pts',(4.1203204113275,-28.3340002430544,54.9991000793355));
#111943=CARTESIAN_POINT('Ctrl Pts',(4.12609722619094,-28.3339566319437,
55.0798361960743));
#111944=CARTESIAN_POINT('Ctrl Pts',(4.13201002271519,-28.3397818578504,
55.1604689461328));
#111945=CARTESIAN_POINT('Ctrl Pts',(4.14421232624134,-28.3640341023962,
55.3268078040519));
#111946=CARTESIAN_POINT('Ctrl Pts',(4.15047178471177,-28.3834192393927,
55.4121386308245));
#111947=CARTESIAN_POINT('Ctrl Pts',(4.15848277482955,-28.4177846659238,
55.5224394374832));
#111948=CARTESIAN_POINT('Ctrl Pts',(4.16041355774539,-28.4268376910685,
55.5490981838307));
#111949=CARTESIAN_POINT('Ctrl Pts',(4.16232238521864,-28.4365623101738,
55.5755159337767));
#111950=CARTESIAN_POINT('Ctrl Pts',(3.96712537028317,-28.4365623116664,
55.5755159378315));
#111951=CARTESIAN_POINT('Ctrl Pts',(3.9635169617427,-28.419241183033,55.5284616278987));
#111952=CARTESIAN_POINT('Ctrl Pts',(3.95994984272749,-28.4040508085702,
55.4806430184928));
#111953=CARTESIAN_POINT('Ctrl Pts',(3.95382913432262,-28.3813333530033,
55.3960732284496));
#111954=CARTESIAN_POINT('Ctrl Pts',(3.95124985306976,-28.3728467099228,
55.3596224024264));
#111955=CARTESIAN_POINT('Ctrl Pts',(3.94768579525725,-28.3626726004268,
55.3081268934566));
#111956=CARTESIAN_POINT('Ctrl Pts',(3.94666874832452,-28.3599517911125,
55.2933003483287));
#111957=CARTESIAN_POINT('Ctrl Pts',(3.94492688194108,-28.3556098970241,
55.267686597003));
#111958=CARTESIAN_POINT('Ctrl Pts',(3.94419906991847,-28.3538928762381,
55.256916857802));
#111959=CARTESIAN_POINT('Ctrl Pts',(3.94271781014448,-28.350598719155,55.2348641821718));
#111960=CARTESIAN_POINT('Ctrl Pts',(3.94196470550827,-28.3490313136447,
55.2235803589091));
#111961=CARTESIAN_POINT('Ctrl Pts',(3.94005978507564,-28.3453421666476,
55.194863619123));
#111962=CARTESIAN_POINT('Ctrl Pts',(3.93891301636762,-28.3433800574488,
55.1774113292266));
#111963=CARTESIAN_POINT('Ctrl Pts',(3.93428743136639,-28.3365316744345,
55.1064011240595));
#111964=CARTESIAN_POINT('Ctrl Pts',(3.93088053675959,-28.3339636933345,
55.0526495474743));
#111965=CARTESIAN_POINT('Ctrl Pts',(3.92156616836595,-28.3340655770633,
54.903309587721));
#111966=CARTESIAN_POINT('Ctrl Pts',(3.91579736750292,-28.3423511625915,
54.8079391988554));
#111967=CARTESIAN_POINT('Ctrl Pts',(3.90524395331732,-28.3718971366683,
54.6385037980415));
#111968=CARTESIAN_POINT('Ctrl Pts',(3.90050169416086,-28.3901927356272,
54.5642064794781));
#111969=CARTESIAN_POINT('Ctrl Pts',(3.89470760145473,-28.417270374608,54.4797366842595));
#111970=CARTESIAN_POINT('Ctrl Pts',(3.89389867128788,-28.4211504787493,
54.4680778701374));
#111971=CARTESIAN_POINT('Ctrl Pts',(3.89262087655178,-28.4274268422726,
54.4498927552401));
#111972=CARTESIAN_POINT('Ctrl Pts',(3.8921568987256,-28.4297356891334,54.4433364510008));
#111973=CARTESIAN_POINT('Ctrl Pts',(3.89128439993776,-28.4341312707437,
54.4310995290871));
#111974=CARTESIAN_POINT('Ctrl Pts',(3.89087645551415,-28.4362080159269,
54.4254155858815));
#111975=CARTESIAN_POINT('Ctrl Pts',(3.88991082123848,-28.4411748994157,
54.412047877239));
#111976=CARTESIAN_POINT('Ctrl Pts',(3.88935165077797,-28.4440909153328,
54.4043740216686));
#111977=CARTESIAN_POINT('Ctrl Pts',(3.88746986060579,-28.4540406526268,
54.3787617555055));
#111978=CARTESIAN_POINT('Ctrl Pts',(3.88613374530733,-28.4613285520364,
54.3609246082099));
#111979=CARTESIAN_POINT('Ctrl Pts',(3.88280884321164,-28.4800448998022,
54.3172933998151));
#111980=CARTESIAN_POINT('Ctrl Pts',(3.88080554814264,-28.4918221445719,
54.2916560260077));
#111981=CARTESIAN_POINT('Ctrl Pts',(3.87164500573624,-28.5481262188826,
54.1768668966667));
#111982=CARTESIAN_POINT('Ctrl Pts',(3.86431660325594,-28.5999461676628,
54.0915203632211));
#111983=CARTESIAN_POINT('Ctrl Pts',(3.85113159288279,-28.7084397443199,
53.9443744512792));
#111984=CARTESIAN_POINT('Ctrl Pts',(3.84524752264212,-28.7627459035744,
53.8812152726242));
#111985=CARTESIAN_POINT('Ctrl Pts',(3.83821140374396,-28.8354202650434,
53.8084904525874));
#111986=CARTESIAN_POINT('Ctrl Pts',(3.83687933048297,-28.8495337534513,
53.79485750498));
#111987=CARTESIAN_POINT('Ctrl Pts',(3.83476157476816,-28.8725358396175,
53.7734110506687));
#111988=CARTESIAN_POINT('Ctrl Pts',(3.83396910060841,-28.8812721895702,
53.7654377365938));
#111989=CARTESIAN_POINT('Ctrl Pts',(3.83246477495646,-28.8980994235554,
53.7504055132469));
#111990=CARTESIAN_POINT('Ctrl Pts',(3.83175226931959,-28.9061750462882,
53.7433304962984));
#111991=CARTESIAN_POINT('Ctrl Pts',(3.83012026231281,-28.9249122106184,
53.7272324229452));
#111992=CARTESIAN_POINT('Ctrl Pts',(3.82920304345483,-28.9356200482597,
53.7182643025602));
#111993=CARTESIAN_POINT('Ctrl Pts',(3.82629692619005,-28.9700984734691,
53.6901177101134));
#111994=CARTESIAN_POINT('Ctrl Pts',(3.82432859635999,-28.9942849835688,
53.6714570911085));
#111995=CARTESIAN_POINT('Ctrl Pts',(3.81968081595669,-29.0532376064061,
53.6285065378173));
#111996=CARTESIAN_POINT('Ctrl Pts',(3.817023792213,-29.0884450596126,53.6048579588468));
#111997=CARTESIAN_POINT('Ctrl Pts',(3.80982204312389,-29.1872660040813,
53.5438204829187));
#111998=CARTESIAN_POINT('Ctrl Pts',(3.80534532601377,-29.2525193868902,
53.5092725138221));
#111999=CARTESIAN_POINT('Ctrl Pts',(3.80002284717559,-29.331943104722,53.4737524598691));
#112000=CARTESIAN_POINT('Ctrl Pts',(3.79921119577326,-29.3441028520772,
53.46848751379));
#112001=CARTESIAN_POINT('Ctrl Pts',(3.79383685374464,-29.4248266442524,
53.4346733190953));
#112002=CARTESIAN_POINT('Ctrl Pts',(3.78922201898326,-29.4951630752107,
53.4105948032067));
#112003=CARTESIAN_POINT('Ctrl Pts',(3.78356981673008,-29.5787171797105,
53.3880981564084));
#112004=CARTESIAN_POINT('Ctrl Pts',(3.7827614546676,-29.5906082037673,53.3850371200989));
#112005=CARTESIAN_POINT('Ctrl Pts',(3.7814843644999,-29.6092799571756,53.3804500199643));
#112006=CARTESIAN_POINT('Ctrl Pts',(3.78102051442992,-29.6160385264455,
53.3788344093982));
#112007=CARTESIAN_POINT('Ctrl Pts',(3.78014811242765,-29.6287018309195,
53.3758909217718));
#112008=CARTESIAN_POINT('Ctrl Pts',(3.77974013539755,-29.6346039490077,
53.3745528770239));
#112009=CARTESIAN_POINT('Ctrl Pts',(3.77877422882975,-29.6485324508578,
53.3714748967726));
#112010=CARTESIAN_POINT('Ctrl Pts',(3.77821481614667,-29.6565645540976,
53.3697621224577));
#112011=CARTESIAN_POINT('Ctrl Pts',(3.77633133886228,-29.6835028210192,
53.3642256881099));
#112012=CARTESIAN_POINT('Ctrl Pts',(3.77499374696187,-29.7024618906122,
53.3606711562403));
#112013=CARTESIAN_POINT('Ctrl Pts',(3.77166434712926,-29.7493317837924,
53.3527235741344));
#112014=CARTESIAN_POINT('Ctrl Pts',(3.76965798395742,-29.7773003318921,
53.3487099420319));
#112015=CARTESIAN_POINT('Ctrl Pts',(3.76047031364741,-29.9046493373813,
53.3337287394431));
#112016=CARTESIAN_POINT('Ctrl Pts',(3.75311710831985,-30.004792066411,53.3310095464614));
#112017=CARTESIAN_POINT('Ctrl Pts',(3.73993780162785,-30.1872003055034,
53.3424819979876));
#112018=CARTESIAN_POINT('Ctrl Pts',(3.73408173161187,-30.2693328883665,
53.3538306889441));
#112019=CARTESIAN_POINT('Ctrl Pts',(3.72707260638483,-30.3694633944301,
53.3753654786031));
#112020=CARTESIAN_POINT('Ctrl Pts',(3.72574129900404,-30.3885608084496,
53.3798268354637));
#112021=CARTESIAN_POINT('Ctrl Pts',(3.72362446165702,-30.4190413072739,
53.3875173765517));
#112022=CARTESIAN_POINT('Ctrl Pts',(3.72283215043316,-30.4304760036318,
53.3905323082146));
#112023=CARTESIAN_POINT('Ctrl Pts',(3.72132795111338,-30.4522299477943,
53.3965164956323));
#112024=CARTESIAN_POINT('Ctrl Pts',(3.7206154107873,-30.462554435464,53.3994642528518));
#112025=CARTESIAN_POINT('Ctrl Pts',(3.71898306666611,-30.4862464468943,
53.4064769899088));
#112026=CARTESIAN_POINT('Ctrl Pts',(3.71806554869362,-30.4995928942776,
53.4106107618042));
#112027=CARTESIAN_POINT('Ctrl Pts',(3.71515740431842,-30.5419696072504,
53.4243225733271));
#112028=CARTESIAN_POINT('Ctrl Pts',(3.71318738833584,-30.5707899371035,
53.4345321965595));
#112029=CARTESIAN_POINT('Ctrl Pts',(3.70853477023838,-30.6389193463788,
53.4607989853292));
#112030=CARTESIAN_POINT('Ctrl Pts',(3.70587466147067,-30.6779279677004,
53.4775770153992));
#112031=CARTESIAN_POINT('Ctrl Pts',(3.69867103140397,-30.7828292599355,
53.5275288119121));
#112032=CARTESIAN_POINT('Ctrl Pts',(3.6941953284477,-30.847226636022,53.5636154952525));
#112033=CARTESIAN_POINT('Ctrl Pts',(3.68885253381612,-30.9204158627209,
53.6112683830241));
#112034=CARTESIAN_POINT('Ctrl Pts',(3.68801962789674,-30.9317187329648,
53.6188262015581));
#112035=CARTESIAN_POINT('Ctrl Pts',(3.68264894870969,-31.0038112018581,
53.6683195040345));
#112036=CARTESIAN_POINT('Ctrl Pts',(3.67805883917794,-31.0618406433122,
53.7141144866898));
#112037=CARTESIAN_POINT('Ctrl Pts',(3.67243410827982,-31.1257451785403,
53.7718287890793));
#112038=CARTESIAN_POINT('Ctrl Pts',(3.67162584508035,-31.1347649953463,
53.7801577503949));
#112039=CARTESIAN_POINT('Ctrl Pts',(3.67034887752532,-31.1487443118484,
53.793355565662));
#112040=CARTESIAN_POINT('Ctrl Pts',(3.6698850496902,-31.1537670046734,53.7981572567605));
#112041=CARTESIAN_POINT('Ctrl Pts',(3.66901266451562,-31.1631078723631,
53.807199636773));
#112042=CARTESIAN_POINT('Ctrl Pts',(3.66860468179352,-31.167433166583,53.8114326160646));
#112043=CARTESIAN_POINT('Ctrl Pts',(3.66763872775876,-31.1775738989273,
53.8214656676801));
#112044=CARTESIAN_POINT('Ctrl Pts',(3.66707927285857,-31.1833696140813,
53.8272852822221));
#112045=CARTESIAN_POINT('Ctrl Pts',(3.66519550140865,-31.2026342775704,
53.8469176098963));
#112046=CARTESIAN_POINT('Ctrl Pts',(3.6638576520264,-31.2159057288332,53.8609208178176));
#112047=CARTESIAN_POINT('Ctrl Pts',(3.66052746770596,-31.2480104546234,
53.8959961518953));
#112048=CARTESIAN_POINT('Ctrl Pts',(3.65852056932849,-31.2665560840594,
53.9173227178944));
#112049=CARTESIAN_POINT('Ctrl Pts',(3.64932815603016,-31.3482512745239,
54.0162410139549));
#112050=CARTESIAN_POINT('Ctrl Pts',(3.6419706130645,-31.4048763560687,54.0989527719164));
#112051=CARTESIAN_POINT('Ctrl Pts',(3.6287922962335,-31.4941451099922,54.2584278528237));
#112052=CARTESIAN_POINT('Ctrl Pts',(3.62294111344197,-31.5291230919963,
54.3335278367503));
#112053=CARTESIAN_POINT('Ctrl Pts',(3.61593670414302,-31.5653130633097,
54.4292676070656));
#112054=CARTESIAN_POINT('Ctrl Pts',(3.61460553384762,-31.5719218770181,
54.4477300297358));
#112055=CARTESIAN_POINT('Ctrl Pts',(3.61248886088143,-31.5819913839723,
54.4775068620174));
#112056=CARTESIAN_POINT('Ctrl Pts',(3.61169657882252,-31.5856600152315,
54.4887484505886));
#112057=CARTESIAN_POINT('Ctrl Pts',(3.61019240209761,-31.5924308501639,
54.5102702130772));
#112058=CARTESIAN_POINT('Ctrl Pts',(3.60947985554459,-31.5955539471479,
54.5205431325975));
#112059=CARTESIAN_POINT('Ctrl Pts',(3.60784745099199,-31.6025121410359,
54.5442522056277));
#112060=CARTESIAN_POINT('Ctrl Pts',(3.60692987940837,-31.6062779933274,
54.5577079674059));
#112061=CARTESIAN_POINT('Ctrl Pts',(3.60402137159618,-31.617742986394,54.6007527929264));
#112062=CARTESIAN_POINT('Ctrl Pts',(3.60205105329454,-31.6247974077053,
54.6305080864498));
#112063=CARTESIAN_POINT('Ctrl Pts',(3.59739756763203,-31.6396824175065,
54.7020066362002));
#112064=CARTESIAN_POINT('Ctrl Pts',(3.59473690555963,-31.6467439858054,
54.7438885023124));
#112065=CARTESIAN_POINT('Ctrl Pts',(3.58753295657385,-31.661669401561,54.859119212564));
#112066=CARTESIAN_POINT('Ctrl Pts',(3.58305745313266,-31.666276078668,54.9327914153874));
#112067=CARTESIAN_POINT('Ctrl Pts',(3.57771154800517,-31.6659337407174,
55.0201766843736));
#112068=CARTESIAN_POINT('Ctrl Pts',(3.57687534593039,-31.665712507855,55.03382547379));
#112069=CARTESIAN_POINT('Ctrl Pts',(3.57150532411575,-31.6632212291599,
55.1212237108034));
#112070=CARTESIAN_POINT('Ctrl Pts',(3.56691913931639,-31.6562218217219,
55.1947474301107));
#112071=CARTESIAN_POINT('Ctrl Pts',(3.56129876762668,-31.6424037056981,
55.279672651212));
#112072=CARTESIAN_POINT('Ctrl Pts',(3.56049052019865,-31.640298242381,55.2917676791794));
#112073=CARTESIAN_POINT('Ctrl Pts',(3.55921357220381,-31.6367921102805,
55.310670036992));
#112074=CARTESIAN_POINT('Ctrl Pts',(3.55874974791583,-31.6354821369628,
55.3174940305964));
#112075=CARTESIAN_POINT('Ctrl Pts',(3.55787736542533,-31.6329513959881,
55.3302459201189));
#112076=CARTESIAN_POINT('Ctrl Pts',(3.55746938179472,-31.631740965999,55.3361756157435));
#112077=CARTESIAN_POINT('Ctrl Pts',(3.55650342018544,-31.6288117052746,
55.3501369592597));
#112078=CARTESIAN_POINT('Ctrl Pts',(3.55594395854869,-31.6270657579701,
55.3581626357571));
#112079=CARTESIAN_POINT('Ctrl Pts',(3.55406014015536,-31.621020085398,55.3849962455256));
#112080=CARTESIAN_POINT('Ctrl Pts',(3.55272224968321,-31.6164531836484,
55.4037415660234));
#112081=CARTESIAN_POINT('Ctrl Pts',(3.54939194016605,-31.6043968064112,
55.4497394190887));
#112082=CARTESIAN_POINT('Ctrl Pts',(3.54738495637288,-31.5965375188805,
55.4768882762972));
#112083=CARTESIAN_POINT('Ctrl Pts',(3.53819178582436,-31.5577368996198,
55.5991834801321));
#112084=CARTESIAN_POINT('Ctrl Pts',(3.53083355029357,-31.5189538622006,
55.6916246799748));
#112085=CARTESIAN_POINT('Ctrl Pts',(3.51765539129601,-31.433385450734,55.8531138554362));
#112086=CARTESIAN_POINT('Ctrl Pts',(3.51180498855318,-31.3892664238125,
55.9232224102179));
#112087=CARTESIAN_POINT('Ctrl Pts',(3.5048013320846,-31.3284658300934,56.0055441195572));
#112088=CARTESIAN_POINT('Ctrl Pts',(3.50347018376456,-31.316539307935,56.021109565988));
#112089=CARTESIAN_POINT('Ctrl Pts',(3.50135353714934,-31.2969840591638,
56.0457189712757));
#112090=CARTESIAN_POINT('Ctrl Pts',(3.50056125976577,-31.2895292830279,
56.0548981265043));
#112091=CARTESIAN_POINT('Ctrl Pts',(3.49905708666253,-31.2751201958198,
56.0722591866397));
#112092=CARTESIAN_POINT('Ctrl Pts',(3.49834453911081,-31.2681833098963,
56.0804547092898));
#112093=CARTESIAN_POINT('Ctrl Pts',(3.49671212486831,-31.2520380524084,
56.099159648696));
#112094=CARTESIAN_POINT('Ctrl Pts',(3.49579454468861,-31.2427756490096,
56.1096215228316));
#112095=CARTESIAN_POINT('Ctrl Pts',(3.49288597859922,-31.2128293854217,
56.1426003813374));
#112096=CARTESIAN_POINT('Ctrl Pts',(3.49091561182028,-31.191656167289,56.1646658389564));
#112097=CARTESIAN_POINT('Ctrl Pts',(3.48626198703707,-31.139658511577,56.215951099881));
#112098=CARTESIAN_POINT('Ctrl Pts',(3.48360123623655,-31.1083004862128,
56.2445999403378));
#112099=CARTESIAN_POINT('Ctrl Pts',(3.47639723661924,-31.0195840607264,
56.3196366414693));
#112100=CARTESIAN_POINT('Ctrl Pts',(3.47192176566036,-30.9601875487601,
56.3634635166959));
#112101=CARTESIAN_POINT('Ctrl Pts',(3.46657537581815,-30.8865788856192,
56.4105745055347));
#112102=CARTESIAN_POINT('Ctrl Pts',(3.46573865877656,-30.8749847526216,
56.4177955540933));
#112103=CARTESIAN_POINT('Ctrl Pts',(3.46036874236968,-30.8002074105462,
56.4631017066652));
#112104=CARTESIAN_POINT('Ctrl Pts',(3.45578317346601,-30.7346496825615,
56.4970923778875));
#112105=CARTESIAN_POINT('Ctrl Pts',(3.45016348581876,-30.6558154538616,
56.5315393608582));
#112106=CARTESIAN_POINT('Ctrl Pts',(3.44935524086905,-30.6445120013537,
56.5363303621741));
#112107=CARTESIAN_POINT('Ctrl Pts',(3.44807829594802,-30.6267297502404,
56.5436366490223));
#112108=CARTESIAN_POINT('Ctrl Pts',(3.4476144722174,-30.6202861413578,56.5462371689067));
#112109=CARTESIAN_POINT('Ctrl Pts',(3.44674209014855,-30.6082001465491,
56.5510271471433));
#112110=CARTESIAN_POINT('Ctrl Pts',(3.4463341063751,-30.6025618553427,56.5532262665976));
#112111=CARTESIAN_POINT('Ctrl Pts',(3.44536814357594,-30.5892435805364,
56.5583374039422));
#112112=CARTESIAN_POINT('Ctrl Pts',(3.44480868088069,-30.5815539066334,
56.5612234011634));
#112113=CARTESIAN_POINT('Ctrl Pts',(3.44292485511082,-30.5557307660925,
56.5706977893494));
#112114=CARTESIAN_POINT('Ctrl Pts',(3.44158695818191,-30.5375049952772,
56.5770277520163));
#112115=CARTESIAN_POINT('Ctrl Pts',(3.4382566289914,-30.492320984845,56.5918463229098));
#112116=CARTESIAN_POINT('Ctrl Pts',(3.43624963177599,-30.4652492729126,
56.5999680002081));
#112117=CARTESIAN_POINT('Ctrl Pts',(3.42705634222611,-30.3414580852053,
56.6336987965965));
#112118=CARTESIAN_POINT('Ctrl Pts',(3.41969799785833,-30.2427582081686,
56.6512523358386));
#112119=CARTESIAN_POINT('Ctrl Pts',(3.40651986365603,-30.0606750507911,
56.6669479183889));
#112120=CARTESIAN_POINT('Ctrl Pts',(3.40066958348873,-29.9778469003161,
56.6679058063101));
#112121=CARTESIAN_POINT('Ctrl Pts',(3.39366604532178,-29.8757105066716,
56.6614730085073));
#112122=CARTESIAN_POINT('Ctrl Pts',(3.39233490045728,-29.8561648296538,
56.659895158409));
#112123=CARTESIAN_POINT('Ctrl Pts',(3.39021825798574,-29.8248833920187,
56.656813203101));
#112124=CARTESIAN_POINT('Ctrl Pts',(3.38942598133736,-29.8131283916478,
56.6555285653924));
#112125=CARTESIAN_POINT('Ctrl Pts',(3.38792180880369,-29.7907276453987,
56.6528388786504));
#112126=CARTESIAN_POINT('Ctrl Pts',(3.38720926109497,-29.7800799094665,
56.6514558547426));
#112127=CARTESIAN_POINT('Ctrl Pts',(3.38557684532886,-29.7556084439227,
56.6480364030898));
#112128=CARTESIAN_POINT('Ctrl Pts',(3.38465926379753,-29.741795352084,56.6459287949629));
#112129=CARTESIAN_POINT('Ctrl Pts',(3.38175068854431,-29.6978464588485,
56.638656155075));
#112130=CARTESIAN_POINT('Ctrl Pts',(3.37978031414253,-29.6678245957053,
56.6328350944521));
#112131=CARTESIAN_POINT('Ctrl Pts',(3.37512666748297,-29.5965356135099,
56.6169647828039));
#112132=CARTESIAN_POINT('Ctrl Pts',(3.37246590273011,-29.5554587893254,
56.6061575610529));
#112133=CARTESIAN_POINT('Ctrl Pts',(3.36526189516412,-29.4443004641779,
56.5723201126431));
#112134=CARTESIAN_POINT('Ctrl Pts',(3.36078642932549,-29.3752651540996,
56.5461886207057));
#112135=CARTESIAN_POINT('Ctrl Pts',(3.35132895099948,-29.2346291878216,
56.4819925197743));
#112136=CARTESIAN_POINT('Ctrl Pts',(3.34635159749342,-29.1636211361858,
56.4431083058159));
#112137=CARTESIAN_POINT('Ctrl Pts',(3.34004643120265,-29.0818813094028,
56.3902826238861));
#112138=CARTESIAN_POINT('Ctrl Pts',(3.33896798008594,-29.0681714683268,
56.3811311457641));
#112139=CARTESIAN_POINT('Ctrl Pts',(3.33736589551659,-29.0482443730791,
56.367397825104));
#112140=CARTESIAN_POINT('Ctrl Pts',(3.33685214541117,-29.0419191201869,
56.3629734433732));
#112141=CARTESIAN_POINT('Ctrl Pts',(3.3359333402193,-29.0307270834271,56.3550284468596));
#112142=CARTESIAN_POINT('Ctrl Pts',(3.33552945234985,-29.0258482634933,
56.3515252385991));
#112143=CARTESIAN_POINT('Ctrl Pts',(3.33463150824678,-29.0150926534159,
56.3437137392996));
#112144=CARTESIAN_POINT('Ctrl Pts',(3.33413665804466,-29.0092252062333,
56.3393932945706));
#112145=CARTESIAN_POINT('Ctrl Pts',(3.33266692581943,-28.9919691647904,
56.3265115272862));
#112146=CARTESIAN_POINT('Ctrl Pts',(3.33168518247879,-28.9806621729188,
56.3178426906261));
#112147=CARTESIAN_POINT('Ctrl Pts',(3.32938715348942,-28.9546698786251,
56.2973803029542));
#112148=CARTESIAN_POINT('Ctrl Pts',(3.32806509178823,-28.9400707968081,
56.2854807401345));
#112149=CARTESIAN_POINT('Ctrl Pts',(3.32335736482795,-28.8892261061332,
56.2425827361353));
#112150=CARTESIAN_POINT('Ctrl Pts',(3.31991666830189,-28.8541145153204,
56.2102794680983));
#112151=CARTESIAN_POINT('Ctrl Pts',(3.30829271145983,-28.7410322505317,
56.0969046396222));
#112152=CARTESIAN_POINT('Ctrl Pts',(3.300066135971,-28.66987902042,56.0094469981921));
#112153=CARTESIAN_POINT('Ctrl Pts',(3.28892499432238,-28.5830020896006,
55.8773569025731));
#112154=CARTESIAN_POINT('Ctrl Pts',(3.28575955836855,-28.5595023575564,
55.8382156284401));
#112155=CARTESIAN_POINT('Ctrl Pts',(3.28151599604221,-28.5296509133886,
55.7835224758517));
#112156=CARTESIAN_POINT('Ctrl Pts',(3.28038843228126,-28.521884153901,55.7687701134053));
#112157=CARTESIAN_POINT('Ctrl Pts',(3.27859100767267,-28.5097744564672,
55.7449064462911));
#112158=CARTESIAN_POINT('Ctrl Pts',(3.27791625165747,-28.5052907656171,
55.7358682604314));
#112159=CARTESIAN_POINT('Ctrl Pts',(3.27652062666157,-28.496148559462,55.7170111165739));
#112160=CARTESIAN_POINT('Ctrl Pts',(3.27580024899632,-28.4915034508356,
55.7071861616145));
#112161=CARTESIAN_POINT('Ctrl Pts',(3.27410331088587,-28.4807395036109,
55.683830418164));
#112162=CARTESIAN_POINT('Ctrl Pts',(3.27312966679654,-28.4747047114319,
55.6702617420705));
#112163=CARTESIAN_POINT('Ctrl Pts',(3.27026543266706,-28.4573823375009,
55.6298679555056));
#112164=CARTESIAN_POINT('Ctrl Pts',(3.26839229184022,-28.4466154441205,
55.6028261219895));
#112165=CARTESIAN_POINT('Ctrl Pts',(3.26653910946692,-28.436562310676,55.575515935141));
#112166=CARTESIAN_POINT('Origin',(5.,-30.,55.));
#112167=CARTESIAN_POINT('',(2.56903904312142,-28.4365623153847,55.5755159479327));
#112168=CARTESIAN_POINT('',(2.75980443758381,-28.4365622822719,55.5755158579788));
#112169=CARTESIAN_POINT('',(5.,-28.4365623102018,55.5755159338528));
#112170=CARTESIAN_POINT('Ctrl Pts',(2.75980443758381,-28.4365622822719,
55.5755158579788));
#112171=CARTESIAN_POINT('Ctrl Pts',(2.76084862674717,-28.4423847804517,
55.5913331689));
#112172=CARTESIAN_POINT('Ctrl Pts',(2.76189838302494,-28.4484491493631,
55.6070671061794));
#112173=CARTESIAN_POINT('Ctrl Pts',(2.76472966975531,-28.4653300576938,
55.6489567060463));
#112174=CARTESIAN_POINT('Ctrl Pts',(2.76652343433635,-28.4765725895492,
55.6749262053549));
#112175=CARTESIAN_POINT('Ctrl Pts',(2.76959232887108,-28.4965912984897,
55.7181164371627));
#112176=CARTESIAN_POINT('Ctrl Pts',(2.77085111394464,-28.5050159636729,
55.7354941156935));
#112177=CARTESIAN_POINT('Ctrl Pts',(2.77267007075862,-28.5174533808426,
55.7600520112067));
#112178=CARTESIAN_POINT('Ctrl Pts',(2.77321617963206,-28.5212205412668,
55.7673557474457));
#112179=CARTESIAN_POINT('Ctrl Pts',(2.77417042327773,-28.5278565440596,
55.7799912180931));
#112180=CARTESIAN_POINT('Ctrl Pts',(2.77457702756173,-28.5307006638238,
55.7853356699778));
#112181=CARTESIAN_POINT('Ctrl Pts',(2.7754544672218,-28.5368723641967,55.7967821690365));
#112182=CARTESIAN_POINT('Ctrl Pts',(2.77592582828356,-28.5402089645767,
55.8028788401981));
#112183=CARTESIAN_POINT('Ctrl Pts',(2.77723612513202,-28.5495449665656,
55.8196870909652));
#112184=CARTESIAN_POINT('Ctrl Pts',(2.77807980798882,-28.5556246380549,
55.8303532518169));
#112185=CARTESIAN_POINT('Ctrl Pts',(2.78399612441273,-28.5987665067569,
55.9041336780491));
#112186=CARTESIAN_POINT('Ctrl Pts',(2.78927092568923,-28.6398312245519,
55.9648064774068));
#112187=CARTESIAN_POINT('Ctrl Pts',(2.79561403829376,-28.6934222218326,
56.0337361065216));
#112188=CARTESIAN_POINT('Ctrl Pts',(2.79664245169486,-28.7022404609474,
56.0447851469678));
#112189=CARTESIAN_POINT('Ctrl Pts',(2.80303532269296,-28.7579000780151,
56.1127332544735));
#112190=CARTESIAN_POINT('Ctrl Pts',(2.80839967758463,-28.8083365515119,
56.1665877798951));
#112191=CARTESIAN_POINT('Ctrl Pts',(2.8166948171388,-28.8932415220021,56.2459736713992));
#112192=CARTESIAN_POINT('Ctrl Pts',(2.81969336519339,-28.9254095838873,
56.2738212822276));
#112193=CARTESIAN_POINT('Ctrl Pts',(2.82477033726503,-28.9825059802322,
56.3195450319847));
#112194=CARTESIAN_POINT('Ctrl Pts',(2.82687028547511,-29.0069255550884,
56.3380196307692));
#112195=CARTESIAN_POINT('Ctrl Pts',(2.82989136153209,-29.0432202700187,
56.3639369611078));
#112196=CARTESIAN_POINT('Ctrl Pts',(2.83083295848849,-29.0547008075624,
56.3719187086164));
#112197=CARTESIAN_POINT('Ctrl Pts',(2.83248817738217,-29.0751761748341,
56.3857749666196));
#112198=CARTESIAN_POINT('Ctrl Pts',(2.8332040067372,-29.0841297540399,56.3917086863124));
#112199=CARTESIAN_POINT('Ctrl Pts',(2.83470118034477,-29.1030605825925,
56.4039927105872));
#112200=CARTESIAN_POINT('Ctrl Pts',(2.83548179739137,-29.1130493569947,
56.4103242247415));
#112201=CARTESIAN_POINT('Ctrl Pts',(2.83754610966426,-29.1397721154538,
56.4268665791687));
#112202=CARTESIAN_POINT('Ctrl Pts',(2.83882292401875,-29.156620646126,56.4368895455709));
#112203=CARTESIAN_POINT('Ctrl Pts',(2.84541462351944,-29.2451874203696,
56.4874820591694));
#112204=CARTESIAN_POINT('Ctrl Pts',(2.85054703465835,-29.3196698669227,
56.522989919062));
#112205=CARTESIAN_POINT('Ctrl Pts',(2.86177072510637,-29.4899883195561,
56.5891847440522));
#112206=CARTESIAN_POINT('Ctrl Pts',(2.86780258761651,-29.5865793393545,
56.6170037339531));
#112207=CARTESIAN_POINT('Ctrl Pts',(2.87586481445836,-29.7128649715601,
56.6413135413438));
#112208=CARTESIAN_POINT('Ctrl Pts',(2.87765860862119,-29.7407810978298,
56.6459532331609));
#112209=CARTESIAN_POINT('Ctrl Pts',(2.88072754865766,-29.7879252352958,
56.6525596039357));
#112210=CARTESIAN_POINT('Ctrl Pts',(2.88198634902052,-29.8070944534942,
56.6549067413306));
#112211=CARTESIAN_POINT('Ctrl Pts',(2.88380532410374,-29.8344724979168,
56.65777688017));
#112212=CARTESIAN_POINT('Ctrl Pts',(2.88435143557233,-29.8426518971075,
56.658573213905));
#112213=CARTESIAN_POINT('Ctrl Pts',(2.8853056821432,-29.8568666806896,56.6598510499845));
#112214=CARTESIAN_POINT('Ctrl Pts',(2.88571228672807,-29.8628993408856,
56.6603602209035));
#112215=CARTESIAN_POINT('Ctrl Pts',(2.88658972512328,-29.8758633342632,
56.6613832765049));
#112216=CARTESIAN_POINT('Ctrl Pts',(2.88706108460031,-29.8827950427904,
56.6618866678659));
#112217=CARTESIAN_POINT('Ctrl Pts',(2.88837137285151,-29.9019797746057,
56.6631592719984));
#112218=CARTESIAN_POINT('Ctrl Pts',(2.88921504859943,-29.9142381750231,
56.6638364150015));
#112219=CARTESIAN_POINT('Ctrl Pts',(2.89512948429612,-29.9995957990739,
56.6676057352042));
#112220=CARTESIAN_POINT('Ctrl Pts',(2.90040226330886,-30.072814599904,56.666014619831));
#112221=CARTESIAN_POINT('Ctrl Pts',(2.90674476459987,-30.1597836940589,
56.6583803967387));
#112222=CARTESIAN_POINT('Ctrl Pts',(2.90777456706569,-30.1738682384566,
56.6569629449716));
#112223=CARTESIAN_POINT('Ctrl Pts',(2.91416864688873,-30.2611588673225,
56.6470528813881));
#112224=CARTESIAN_POINT('Ctrl Pts',(2.91953283646889,-30.3337571152297,
56.6338894229793));
#112225=CARTESIAN_POINT('Ctrl Pts',(2.92782827166228,-30.4465059785372,
56.6056144106314));
#112226=CARTESIAN_POINT('Ctrl Pts',(2.93082725500764,-30.4873546511607,
56.593691052775));
#112227=CARTESIAN_POINT('Ctrl Pts',(2.93590487360403,-30.5567449880516,
56.5705185069125));
#112228=CARTESIAN_POINT('Ctrl Pts',(2.93800504049296,-30.5855135870241,
56.5600216073858));
#112229=CARTESIAN_POINT('Ctrl Pts',(2.94102636787263,-30.6269762568795,
56.5435842296558));
#112230=CARTESIAN_POINT('Ctrl Pts',(2.94196800228605,-30.6399092148182,
56.5382677654497));
#112231=CARTESIAN_POINT('Ctrl Pts',(2.94362326341745,-30.6626561433115,
56.5285804535323));
#112232=CARTESIAN_POINT('Ctrl Pts',(2.94433909793452,-30.6724974899078,
56.5242763865341));
#112233=CARTESIAN_POINT('Ctrl Pts',(2.945836259308,-30.6930850663282,56.5150343013674));
#112234=CARTESIAN_POINT('Ctrl Pts',(2.94661685918045,-30.7038217632145,
56.5100764156993));
#112235=CARTESIAN_POINT('Ctrl Pts',(2.94868107213386,-30.7322118146042,
56.4965981614257));
#112236=CARTESIAN_POINT('Ctrl Pts',(2.94995780555345,-30.7497694714839,
56.4878796962328));
#112237=CARTESIAN_POINT('Ctrl Pts',(2.95654978905709,-30.8403138118442,
56.4409089163907));
#112238=CARTESIAN_POINT('Ctrl Pts',(2.96168253516177,-30.9105467642476,
56.3975882351707));
#112239=CARTESIAN_POINT('Ctrl Pts',(2.97290639597626,-31.0585363428373,
56.2903954326488));
#112240=CARTESIAN_POINT('Ctrl Pts',(2.97893811419045,-31.1342936735202,
56.2243345446972));
#112241=CARTESIAN_POINT('Ctrl Pts',(2.98700016752665,-31.2232081506081,
56.1314232046287));
#112242=CARTESIAN_POINT('Ctrl Pts',(2.98879394240773,-31.2422466352296,
56.110486273842));
#112243=CARTESIAN_POINT('Ctrl Pts',(2.99186285278546,-31.2733658988316,
56.0744618336756));
#112244=CARTESIAN_POINT('Ctrl Pts',(2.9931216431824,-31.2857344224755,56.059630058646));
#112245=CARTESIAN_POINT('Ctrl Pts',(2.99494060635712,-31.3029945020249,
56.0381853715191));
#112246=CARTESIAN_POINT('Ctrl Pts',(2.99548671613375,-31.30809973222,56.0317454247556));
#112247=CARTESIAN_POINT('Ctrl Pts',(2.99644096079728,-31.3168828671844,
56.0204960408095));
#112248=CARTESIAN_POINT('Ctrl Pts',(2.99684756518578,-31.3205825397465,
56.0157038985675));
#112249=CARTESIAN_POINT('Ctrl Pts',(2.99772500440536,-31.3284732640311,
56.0053671419888));
#112250=CARTESIAN_POINT('Ctrl Pts',(2.9981963649154,-31.3326557032567,55.9998165209716));
#112251=CARTESIAN_POINT('Ctrl Pts',(2.99950665876987,-31.3441300297743,
55.9843887409465));
#112252=CARTESIAN_POINT('Ctrl Pts',(3.00035033915101,-31.3513474805704,
55.9744571282957));
#112253=CARTESIAN_POINT('Ctrl Pts',(3.00626600008934,-31.4008193853317,
55.904774380765));
#112254=CARTESIAN_POINT('Ctrl Pts',(3.01154009654297,-31.4392021283956,
55.8423814402288));
#112255=CARTESIAN_POINT('Ctrl Pts',(3.01788299767828,-31.4799571554667,
55.7651685012765));
#112256=CARTESIAN_POINT('Ctrl Pts',(3.01891189680001,-31.4863993190228,
55.7525776225502));
#112257=CARTESIAN_POINT('Ctrl Pts',(3.02530519155831,-31.5254111935584,
55.6738754167684));
#112258=CARTESIAN_POINT('Ctrl Pts',(3.03066948964701,-31.553726557103,55.6057412675533));
#112259=CARTESIAN_POINT('Ctrl Pts',(3.03896473157217,-31.5911203218191,
55.4956823727837));
#112260=CARTESIAN_POINT('Ctrl Pts',(3.04196342995015,-31.6032563661161,
55.4549004515107));
#112261=CARTESIAN_POINT('Ctrl Pts',(3.04704062529491,-31.6214210699778,
55.3840402991145));
#112262=CARTESIAN_POINT('Ctrl Pts',(3.04914064902566,-31.6282046634651,
55.354179368634));
#112263=CARTESIAN_POINT('Ctrl Pts',(3.05216181187759,-31.6368822271656,
55.310432062136));
#112264=CARTESIAN_POINT('Ctrl Pts',(3.05310342177044,-31.6394299215402,
55.2966834067954));
#112265=CARTESIAN_POINT('Ctrl Pts',(3.05475865525201,-31.6436282107965,
55.2723190608297));
#112266=CARTESIAN_POINT('Ctrl Pts',(3.05547448639007,-31.6453497509308,
55.2617165883497));
#112267=CARTESIAN_POINT('Ctrl Pts',(3.05697165577289,-31.6487510314567,
55.2394073598353));
#112268=CARTESIAN_POINT('Ctrl Pts',(3.05775226688843,-31.6504089053787,
55.2276978367452));
#112269=CARTESIAN_POINT('Ctrl Pts',(3.0598165448598,-31.6544830698815,55.1965349901438));
#112270=CARTESIAN_POINT('Ctrl Pts',(3.06109333126192,-31.6566810024698,
55.1770546230399));
#112271=CARTESIAN_POINT('Ctrl Pts',(3.06768711141143,-31.666329154324,55.0754812808575));
#112272=CARTESIAN_POINT('Ctrl Pts',(3.07282146880245,-31.6680237074741,
54.9929526851745));
#112273=CARTESIAN_POINT('Ctrl Pts',(3.08404543505332,-31.6582209977923,
54.8104796978346));
#112274=CARTESIAN_POINT('Ctrl Pts',(3.090075794086,-31.6438088121805,54.7110275696209));
#112275=CARTESIAN_POINT('Ctrl Pts',(3.09813621308581,-31.6139789957503,
54.5859610155698));
#112276=CARTESIAN_POINT('Ctrl Pts',(3.09992980631561,-31.6067153458938,
54.5586134391347));
#112277=CARTESIAN_POINT('Ctrl Pts',(3.10299843727901,-31.5933286944746,
54.5129347490476));
#112278=CARTESIAN_POINT('Ctrl Pts',(3.10425713378501,-31.5875765118503,
54.4945006148859));
#112279=CARTESIAN_POINT('Ctrl Pts',(3.10607598476422,-31.578921655433,54.4683704862345));
#112280=CARTESIAN_POINT('Ctrl Pts',(3.10662207859731,-31.5762801411878,
54.460588799343));
#112281=CARTESIAN_POINT('Ctrl Pts',(3.10757630528491,-31.5715927824681,
54.4471087078719));
#112282=CARTESIAN_POINT('Ctrl Pts',(3.10798290782014,-31.5695732711773,
54.4414013964579));
#112283=CARTESIAN_POINT('Ctrl Pts',(3.10886035480113,-31.5651685128829,
54.4291656705731));
#112284=CARTESIAN_POINT('Ctrl Pts',(3.10933172504006,-31.5627735463399,
54.4226412347365));
#112285=CARTESIAN_POINT('Ctrl Pts',(3.11064207167359,-31.5560349762906,
54.4046329719528));
#112286=CARTESIAN_POINT('Ctrl Pts',(3.11148579569767,-31.5516052410342,
54.3931821530273));
#112287=CARTESIAN_POINT('Ctrl Pts',(3.11741308369604,-31.519831068272,54.3136694242717));
#112288=CARTESIAN_POINT('Ctrl Pts',(3.12269968353565,-31.4881469966343,
54.2474362038162));
#112289=CARTESIAN_POINT('Ctrl Pts',(3.12897795831892,-31.4457954860863,
54.1721095617963));
#112290=CARTESIAN_POINT('Ctrl Pts',(3.12992968542177,-31.4392495773928,
54.1607814253002));
#112291=CARTESIAN_POINT('Ctrl Pts',(3.13636420917426,-31.394116640355,54.0847572765692));
#112292=CARTESIAN_POINT('Ctrl Pts',(3.14184842700386,-31.3513108831972,
54.0226613941766));
#112293=CARTESIAN_POINT('Ctrl Pts',(3.15022708427755,-31.2782492633003,
53.9306971672022));
#112294=CARTESIAN_POINT('Ctrl Pts',(3.15319539232901,-31.2508087987226,
53.898724572899));
#112295=CARTESIAN_POINT('Ctrl Pts',(3.15822740938044,-31.2015272498147,
53.8455251350235));
#112296=CARTESIAN_POINT('Ctrl Pts',(3.16031212852798,-31.1802630076731,
53.8237944958652));
#112297=CARTESIAN_POINT('Ctrl Pts',(3.16331569393269,-31.148393479347,53.7929611251073));
#112298=CARTESIAN_POINT('Ctrl Pts',(3.16425467538618,-31.1382505965271,
53.7833915876739));
#112299=CARTESIAN_POINT('Ctrl Pts',(3.16590694772803,-31.1200875666372,
53.7666812634142));
#112300=CARTESIAN_POINT('Ctrl Pts',(3.16662241940188,-31.1121164071001,
53.7594886662014));
#112301=CARTESIAN_POINT('Ctrl Pts',(3.16812046145024,-31.0952057819338,
53.7445237572471));
#112302=CARTESIAN_POINT('Ctrl Pts',(3.16890228902653,-31.0862518020579,
53.7367686927485));
#112303=CARTESIAN_POINT('Ctrl Pts',(3.17097360174201,-31.0621939122129,
53.716377055268));
#112304=CARTESIAN_POINT('Ctrl Pts',(3.172256120478,-31.0469470934892,53.7039114196437));
#112305=CARTESIAN_POINT('Ctrl Pts',(3.17908433607625,-30.963964087262,53.6384855088989));
#112306=CARTESIAN_POINT('Ctrl Pts',(3.18442954900959,-30.8924222062561,
53.590555502987));
#112307=CARTESIAN_POINT('Ctrl Pts',(3.19567077599505,-30.7327633334874,
53.5006436441105));
#112308=CARTESIAN_POINT('Ctrl Pts',(3.20152533741797,-30.6440259628007,
53.4604416593067));
#112309=CARTESIAN_POINT('Ctrl Pts',(3.20937399290479,-30.5259733183579,
53.4189603130667));
#112310=CARTESIAN_POINT('Ctrl Pts',(3.21114360969615,-30.4994240480951,
53.4103742990245));
#112311=CARTESIAN_POINT('Ctrl Pts',(3.21417532913787,-30.4543438232803,
53.3970361604525));
#112312=CARTESIAN_POINT('Ctrl Pts',(3.21542159763641,-30.4359233300001,
53.3919290577827));
#112313=CARTESIAN_POINT('Ctrl Pts',(3.21722559179305,-30.4094958711268,
53.3850894360244));
#112314=CARTESIAN_POINT('Ctrl Pts',(3.2177695676107,-30.4015569161318,53.3830970856943));
#112315=CARTESIAN_POINT('Ctrl Pts',(3.21872141050845,-30.3877248162805,
53.3797339500482));
#112316=CARTESIAN_POINT('Ctrl Pts',(3.21912777105963,-30.3818383667019,
53.3783366360069));
#112317=CARTESIAN_POINT('Ctrl Pts',(3.22000626805444,-30.3691550877092,
53.3753987913549));
#112318=CARTESIAN_POINT('Ctrl Pts',(3.22047894557644,-30.3623562672298,
53.3738688561274));
#112319=CARTESIAN_POINT('Ctrl Pts',(3.22179639049477,-30.3434714283287,
53.3697435213393));
#112320=CARTESIAN_POINT('Ctrl Pts',(3.22264598555996,-30.3313661035989,
53.3672399774821));
#112321=CARTESIAN_POINT('Ctrl Pts',(3.22915571341237,-30.2390844380402,
53.3492233565304));
#112322=CARTESIAN_POINT('Ctrl Pts',(3.23506652234412,-30.1579008249054,
53.3394912537596));
#112323=CARTESIAN_POINT('Ctrl Pts',(3.24534818864056,-30.0167183015033,
53.3330150359672));
#112324=CARTESIAN_POINT('Ctrl Pts',(3.24969974366852,-29.9569894683763,
53.3334860006485));
#112325=CARTESIAN_POINT('Ctrl Pts',(3.25789042500893,-29.8434997288736,
53.3404875977497));
#112326=CARTESIAN_POINT('Ctrl Pts',(3.26173451339523,-29.7897757528789,
53.3464340184039));
#112327=CARTESIAN_POINT('Ctrl Pts',(3.26803762893499,-29.7006328938803,
53.3607166948735));
#112328=CARTESIAN_POINT('Ctrl Pts',(3.27053506647565,-29.6650291418784,
53.3676197457849));
#112329=CARTESIAN_POINT('Ctrl Pts',(3.27400762581134,-29.6151476306214,
53.3789920683604));
#112330=CARTESIAN_POINT('Ctrl Pts',(3.27501282437738,-29.6006634406929,
53.3824993359752));
#112331=CARTESIAN_POINT('Ctrl Pts',(3.2767410473374,-29.5756899766321,53.3889024391067));
#112332=CARTESIAN_POINT('Ctrl Pts',(3.27746693728155,-29.565178621745,53.3917075125066));
#112333=CARTESIAN_POINT('Ctrl Pts',(3.27895011610086,-29.5436604818607,
53.3976762562637));
#112334=CARTESIAN_POINT('Ctrl Pts',(3.27970700707528,-29.5326573117655,
53.4008508642494));
#112335=CARTESIAN_POINT('Ctrl Pts',(3.28163342629008,-29.5046036094821,
53.4092591366056));
#112336=CARTESIAN_POINT('Ctrl Pts',(3.28279767479856,-29.4876025180866,
53.4146536849117));
#112337=CARTESIAN_POINT('Ctrl Pts',(3.28760670020865,-29.4172441155678,
53.4382289406238));
#112338=CARTESIAN_POINT('Ctrl Pts',(3.29117179504496,-29.3647372953229,
53.4588395436778));
#112339=CARTESIAN_POINT('Ctrl Pts',(3.3024876846289,-29.1991307741788,53.5337510418467));
#112340=CARTESIAN_POINT('Ctrl Pts',(3.30995634925944,-29.091096712291,53.5981549779476));
#112341=CARTESIAN_POINT('Ctrl Pts',(3.32065902743955,-28.9547435124863,
53.7018835770136));
#112342=CARTESIAN_POINT('Ctrl Pts',(3.32357745043948,-28.9193431756693,
53.7312023903951));
#112343=CARTESIAN_POINT('Ctrl Pts',(3.32731439418433,-28.8769639798445,
53.7693623509025));
#112344=CARTESIAN_POINT('Ctrl Pts',(3.32804618964863,-28.868799275869,53.7768631183228));
#112345=CARTESIAN_POINT('Ctrl Pts',(3.32922442078874,-28.855879760206,53.788972044402));
#112346=CARTESIAN_POINT('Ctrl Pts',(3.32966704946267,-28.8510763403816,
53.7935281798187));
#112347=CARTESIAN_POINT('Ctrl Pts',(3.33052174706599,-28.8419001819753,
53.8023364360759));
#112348=CARTESIAN_POINT('Ctrl Pts',(3.33093348881995,-28.8375234473256,
53.806584120905));
#112349=CARTESIAN_POINT('Ctrl Pts',(3.33195017462254,-28.8268213461241,
53.8170853941172));
#112350=CARTESIAN_POINT('Ctrl Pts',(3.33255713651355,-28.8205226053615,
53.8233657384761));
#112351=CARTESIAN_POINT('Ctrl Pts',(3.33468472875068,-28.7987465153784,
53.845428777766));
#112352=CARTESIAN_POINT('Ctrl Pts',(3.33622318731427,-28.7835339507551,
53.8614681042838));
#112353=CARTESIAN_POINT('Ctrl Pts',(3.3451861371016,-28.6977040653504,53.9556468510971));
#112354=CARTESIAN_POINT('Ctrl Pts',(3.35292769577762,-28.6343074301702,
54.0400364727233));
#112355=CARTESIAN_POINT('Ctrl Pts',(3.36765412257765,-28.528273717525,54.2131561119856));
#112356=CARTESIAN_POINT('Ctrl Pts',(3.3746252771296,-28.4846644689147,54.3008107779306));
#112357=CARTESIAN_POINT('Ctrl Pts',(3.38281215200732,-28.4411161655249,
54.4118657443026));
#112358=CARTESIAN_POINT('Ctrl Pts',(3.38427884864516,-28.4336362920606,
54.4320866948534));
#112359=CARTESIAN_POINT('Ctrl Pts',(3.38655784839013,-28.4225282563106,
54.4640068240206));
#112360=CARTESIAN_POINT('Ctrl Pts',(3.38737887548464,-28.4186332403263,
54.4756099046659));
#112361=CARTESIAN_POINT('Ctrl Pts',(3.38890777118908,-28.4115825937538,
54.4974067430999));
#112362=CARTESIAN_POINT('Ctrl Pts',(3.3896166116414,-28.4083963724233,54.5075898659803));
#112363=CARTESIAN_POINT('Ctrl Pts',(3.39120122627427,-28.4014616623823,
54.5305239116674));
#112364=CARTESIAN_POINT('Ctrl Pts',(3.39207519595345,-28.39776745023,54.5432905870902));
#112365=CARTESIAN_POINT('Ctrl Pts',(3.39431003004672,-28.3886625402012,
54.5762269210969));
#112366=CARTESIAN_POINT('Ctrl Pts',(3.39566364477448,-28.3834774723459,
54.5964569274004));
#112367=CARTESIAN_POINT('Ctrl Pts',(3.40533441856615,-28.3488788598153,
54.7428365674983));
#112368=CARTESIAN_POINT('Ctrl Pts',(3.41316148703126,-28.3338854148425,
54.8719377623552));
#112369=CARTESIAN_POINT('Ctrl Pts',(3.42170258281582,-28.3340095764059,
55.0115057284734));
#112370=CARTESIAN_POINT('Ctrl Pts',(3.42231667494751,-28.3341089554762,
55.0215290255626));
#112371=CARTESIAN_POINT('Ctrl Pts',(3.42758545230639,-28.3357347633383,
55.1073624654341));
#112372=CARTESIAN_POINT('Ctrl Pts',(3.43229182281094,-28.3423445945348,
55.1829783514376));
#112373=CARTESIAN_POINT('Ctrl Pts',(3.43804603572568,-28.3559800045717,
55.2700096847301));
#112374=CARTESIAN_POINT('Ctrl Pts',(3.43885494151344,-28.3580160363671,
55.2821269511806));
#112375=CARTESIAN_POINT('Ctrl Pts',(3.44013279489624,-28.3614136273147,
55.3010631723082));
#112376=CARTESIAN_POINT('Ctrl Pts',(3.44059685697841,-28.3626842169741,
55.3078982896115));
#112377=CARTESIAN_POINT('Ctrl Pts',(3.44146959330465,-28.365141176209,55.3206700431645));
#112378=CARTESIAN_POINT('Ctrl Pts',(3.44187769152197,-28.3663171716823,
55.3266084231833));
#112379=CARTESIAN_POINT('Ctrl Pts',(3.44284381593315,-28.3691650760195,
55.3405890838047));
#112380=CARTESIAN_POINT('Ctrl Pts',(3.44340332529196,-28.3708641278656,
55.3486255531894));
#112381=CARTESIAN_POINT('Ctrl Pts',(3.44528684667179,-28.3767516048983,
55.3754899210434));
#112382=CARTESIAN_POINT('Ctrl Pts',(3.44662438349436,-28.3812073886652,
55.3942568138681));
#112383=CARTESIAN_POINT('Ctrl Pts',(3.44995345228143,-28.3929894026953,
55.4403077294224));
#112384=CARTESIAN_POINT('Ctrl Pts',(3.45195953299621,-28.4006856057976,
55.4674903687714));
#112385=CARTESIAN_POINT('Ctrl Pts',(3.45602870270282,-28.4175410426145,
55.521722666911));
#112386=CARTESIAN_POINT('Ctrl Pts',(3.45809074295246,-28.4267091667749,
55.5487490294756));
#112387=CARTESIAN_POINT('Ctrl Pts',(3.46016010521239,-28.436562259669,55.5755157965761));
#112388=CARTESIAN_POINT('',(3.22999374427404,-28.3340001086967,54.9993981883037));
#112389=CARTESIAN_POINT('Ctrl Pts',(3.26653910946692,-28.436562310676,55.575515935141));
#112390=CARTESIAN_POINT('Ctrl Pts',(3.26610426142956,-28.4342033494585,
55.5691076175777));
#112391=CARTESIAN_POINT('Ctrl Pts',(3.26567050549283,-28.4318836884431,
55.5626845247273));
#112392=CARTESIAN_POINT('Ctrl Pts',(3.26185948662694,-28.4118015327416,
55.5059885842083));
#112393=CARTESIAN_POINT('Ctrl Pts',(3.25854909571553,-28.3964216962971,
55.4549022657807));
#112394=CARTESIAN_POINT('Ctrl Pts',(3.25151246114565,-28.3687308606398,
55.3438758887792));
#112395=CARTESIAN_POINT('Ctrl Pts',(3.24780182374277,-28.3572170598544,
55.2838201505538));
#112396=CARTESIAN_POINT('Ctrl Pts',(3.23947059422819,-28.3389924365888,
55.14905659201));
#112397=CARTESIAN_POINT('Ctrl Pts',(3.23484347681183,-28.3339730649767,
55.0742635237064));
#112398=CARTESIAN_POINT('Ctrl Pts',(3.22999374427404,-28.3340001086967,
54.9993981883037));
#112399=CARTESIAN_POINT('Ctrl Pts',(3.22999363096242,-28.3340001093295,
54.9993964391124));
#112400=CARTESIAN_POINT('Ctrl Pts',(3.22944627893864,-28.3340031704154,
54.9909469702904));
#112401=CARTESIAN_POINT('Ctrl Pts',(3.22889614275794,-28.3340705112933,
54.9824978038024));
#112402=CARTESIAN_POINT('Ctrl Pts',(3.22781978152219,-28.3343265807982,
54.9660602437476));
#112403=CARTESIAN_POINT('Ctrl Pts',(3.22729389686768,-28.3345085160145,
54.9580719987756));
#112404=CARTESIAN_POINT('Ctrl Pts',(3.22635468175902,-28.3349336617773,
54.9438882301297));
#112405=CARTESIAN_POINT('Ctrl Pts',(3.22594253609832,-28.3351540116596,
54.9376921072977));
#112406=CARTESIAN_POINT('Ctrl Pts',(3.22514990380104,-28.335642051126,54.9258328918709));
#112407=CARTESIAN_POINT('Ctrl Pts',(3.22476972683143,-28.3359040749976,
54.920169598038));
#112408=CARTESIAN_POINT('Ctrl Pts',(3.22394836010653,-28.3365298882734,
54.9079903447517));
#112409=CARTESIAN_POINT('Ctrl Pts',(3.2235066653871,-28.3369030628881,54.9014750623392));
#112410=CARTESIAN_POINT('Ctrl Pts',(3.22233807798199,-28.3379866273858,
54.8843228713518));
#112411=CARTESIAN_POINT('Ctrl Pts',(3.22160783262883,-28.3387608407594,
54.8736904999473));
#112412=CARTESIAN_POINT('Ctrl Pts',(3.21836852194565,-28.3426221046375,
54.8268713771079));
#112413=CARTESIAN_POINT('Ctrl Pts',(3.21580953598852,-28.3467897288866,
54.790786312995));
#112414=CARTESIAN_POINT('Ctrl Pts',(3.20731403660343,-28.3643024104152,
54.6730589349306));
#112415=CARTESIAN_POINT('Ctrl Pts',(3.20125683106105,-28.3825472288322,
54.5922711479893));
#112416=CARTESIAN_POINT('Ctrl Pts',(3.1877162694469,-28.4370344941116,54.4139447672884));
#112417=CARTESIAN_POINT('Ctrl Pts',(3.18030069668878,-28.4765622657465,
54.3177491133614));
#112418=CARTESIAN_POINT('Ctrl Pts',(3.17176083280522,-28.5344476544525,
54.2074445994328));
#112419=CARTESIAN_POINT('Ctrl Pts',(3.17034830519417,-28.5444466599546,
54.1892273545916));
#112420=CARTESIAN_POINT('Ctrl Pts',(3.16813418766622,-28.5607901277092,
54.1607284754705));
#112421=CARTESIAN_POINT('Ctrl Pts',(3.16732467365762,-28.5669097891404,
54.1503211140598));
#112422=CARTESIAN_POINT('Ctrl Pts',(3.16580630126171,-28.5786588857188,
54.1308281849853));
#112423=CARTESIAN_POINT('Ctrl Pts',(3.16509659458045,-28.5842636368123,
54.1217285350187));
#112424=CARTESIAN_POINT('Ctrl Pts',(3.16349570110759,-28.5971608547623,
54.1012334308335));
#112425=CARTESIAN_POINT('Ctrl Pts',(3.16260648819195,-28.6045054017531,
54.0898715159586));
#112426=CARTESIAN_POINT('Ctrl Pts',(3.16030338536082,-28.6239933445402,
54.0605145535657));
#112427=CARTESIAN_POINT('Ctrl Pts',(3.15889753767737,-28.636351718973,54.0426648157582));
#112428=CARTESIAN_POINT('Ctrl Pts',(3.14810055666687,-28.7347428904244,
53.9063270784758));
#112429=CARTESIAN_POINT('Ctrl Pts',(3.13935341336748,-28.8357038579149,
53.799411666546));
#112430=CARTESIAN_POINT('Ctrl Pts',(3.1264851680095,-28.9978850741701,53.6676210004575));
#112431=CARTESIAN_POINT('Ctrl Pts',(3.12258401545807,-29.0486037724197,
53.6309449749112));
#112432=CARTESIAN_POINT('Ctrl Pts',(3.11752381426487,-29.1142390716444,
53.588893602026));
#112433=CARTESIAN_POINT('Ctrl Pts',(3.11651358879216,-29.1273347335693,
53.580757603548));
#112434=CARTESIAN_POINT('Ctrl Pts',(3.11499421644602,-29.1469806019274,
53.568926830563));
#112435=CARTESIAN_POINT('Ctrl Pts',(3.11449355491824,-29.1534463871775,
53.565092516941));
#112436=CARTESIAN_POINT('Ctrl Pts',(3.11358816554865,-29.1651195387486,
53.5582765101685));
#112437=CARTESIAN_POINT('Ctrl Pts',(3.11318445542479,-29.1703173683475,
53.5552790118577));
#112438=CARTESIAN_POINT('Ctrl Pts',(3.11227419952155,-29.1820204819202,
53.548614016058));
#112439=CARTESIAN_POINT('Ctrl Pts',(3.11176672144735,-29.1885342371351,
53.5449621734525));
#112440=CARTESIAN_POINT('Ctrl Pts',(3.11022112087113,-29.2083465956974,
53.5340290734638));
#112441=CARTESIAN_POINT('Ctrl Pts',(3.10917507923877,-29.2217198319965,
53.5268856766034));
#112442=CARTESIAN_POINT('Ctrl Pts',(3.10057284982028,-29.3315512107026,
53.470131519646));
#112443=CARTESIAN_POINT('Ctrl Pts',(3.09261133568641,-29.43253896802,53.4298707541041));
#112444=CARTESIAN_POINT('Ctrl Pts',(3.07698197601865,-29.6391638771441,
53.3700524321576));
#112445=CARTESIAN_POINT('Ctrl Pts',(3.06935006233231,-29.7442415509271,
53.3502949241533));
#112446=CARTESIAN_POINT('Ctrl Pts',(3.06061437130328,-29.8711612708734,
53.3388597899902));
#112447=CARTESIAN_POINT('Ctrl Pts',(3.05920439733073,-29.8918529525876,
53.3373844404174));
#112448=CARTESIAN_POINT('Ctrl Pts',(3.0569933343112,-29.9246158785417,53.3356626557412));
#112449=CARTESIAN_POINT('Ctrl Pts',(3.05618435818009,-29.936670918022,53.3351603675124));
#112450=CARTESIAN_POINT('Ctrl Pts',(3.05466645180861,-29.9594135456323,
53.3344601558104));
#112451=CARTESIAN_POINT('Ctrl Pts',(3.05395667924349,-29.9700995852406,
53.3342340479073));
#112452=CARTESIAN_POINT('Ctrl Pts',(3.05235491557288,-29.9943270642431,
53.3339546320657));
#112453=CARTESIAN_POINT('Ctrl Pts',(3.051464907086,-30.0078685717886,53.3339635496848));
#112454=CARTESIAN_POINT('Ctrl Pts',(3.04915824930715,-30.0431576168594,
53.3344170662982));
#112455=CARTESIAN_POINT('Ctrl Pts',(3.04774968439721,-30.0648996237534,
53.3351224676973));
#112456=CARTESIAN_POINT('Ctrl Pts',(3.03870910392438,-30.2055001305203,
53.3424427865775));
#112457=CARTESIAN_POINT('Ctrl Pts',(3.03147792461151,-30.3233742061746,
53.3613545167691));
#112458=CARTESIAN_POINT('Ctrl Pts',(3.01863056307776,-30.5262288172144,
53.4166625110284));
#112459=CARTESIAN_POINT('Ctrl Pts',(3.01304287671953,-30.6120920187647,
53.4478359225096));
#112460=CARTESIAN_POINT('Ctrl Pts',(3.0061689366359,-30.7081609296605,53.4919300270745));
#112461=CARTESIAN_POINT('Ctrl Pts',(3.00521596248045,-30.7212805608765,
53.4981607066755));
#112462=CARTESIAN_POINT('Ctrl Pts',(3.0037663020653,-30.7409068238937,53.5077979416642));
#112463=CARTESIAN_POINT('Ctrl Pts',(3.00327700526436,-30.7474755216954,
53.5110774889336));
#112464=CARTESIAN_POINT('Ctrl Pts',(3.00238268345898,-30.7593756964178,
53.5171174709025));
#112465=CARTESIAN_POINT('Ctrl Pts',(3.00197854401409,-30.7647142128652,
53.5198634479797));
#112466=CARTESIAN_POINT('Ctrl Pts',(3.00105503280201,-30.7768248621168,
53.5261758204016));
#112467=CARTESIAN_POINT('Ctrl Pts',(3.00053458915641,-30.78358730203,53.5297600491469));
#112468=CARTESIAN_POINT('Ctrl Pts',(2.9989087684212,-30.8045266660954,53.5410438278637));
#112469=CARTESIAN_POINT('Ctrl Pts',(2.99779427442511,-30.8186161365642,
53.5489025388923));
#112470=CARTESIAN_POINT('Ctrl Pts',(2.99015730724839,-30.9135268269829,
53.6036631766884));
#112471=CARTESIAN_POINT('Ctrl Pts',(2.98333816764977,-30.9903854703331,
53.6570847502175));
#112472=CARTESIAN_POINT('Ctrl Pts',(2.96786974510205,-31.1541054690272,
53.7926128824164));
#112473=CARTESIAN_POINT('Ctrl Pts',(2.95929418444401,-31.2374634431106,
53.8781990854792));
#112474=CARTESIAN_POINT('Ctrl Pts',(2.94965601886661,-31.3241494977233,
53.988743843993));
#112475=CARTESIAN_POINT('Ctrl Pts',(2.9482052314118,-31.3369876837706,54.0057792437966));
#112476=CARTESIAN_POINT('Ctrl Pts',(2.94594538787192,-31.3566430109031,
54.0329300449955));
#112477=CARTESIAN_POINT('Ctrl Pts',(2.94512784481786,-31.3636818870867,
54.0428812605454));
#112478=CARTESIAN_POINT('Ctrl Pts',(2.94360236659168,-31.3766774430358,
54.0616881694945));
#112479=CARTESIAN_POINT('Ctrl Pts',(2.94289349500745,-31.3826594275714,
54.0705255302949));
#112480=CARTESIAN_POINT('Ctrl Pts',(2.94130485505719,-31.3959338397611,
54.0905479793892));
#112481=CARTESIAN_POINT('Ctrl Pts',(2.9404269364868,-31.4031776041989,54.1017645680989));
#112482=CARTESIAN_POINT('Ctrl Pts',(2.93817410278817,-31.4215191215799,
54.1309288822595));
#112483=CARTESIAN_POINT('Ctrl Pts',(2.93680664500663,-31.4324123541753,
54.1490028599927));
#112484=CARTESIAN_POINT('Ctrl Pts',(2.92584690603423,-31.5176417988483,
54.2966906670115));
#112485=CARTESIAN_POINT('Ctrl Pts',(2.9169332446144,-31.5745735196394,54.4355529411328));
#112486=CARTESIAN_POINT('Ctrl Pts',(2.90396652503318,-31.6275957747198,
54.6391590427815));
#112487=CARTESIAN_POINT('Ctrl Pts',(2.90015847426865,-31.639709805863,54.6989611730654));
#112488=CARTESIAN_POINT('Ctrl Pts',(2.89521003509339,-31.6507200674583,
54.7743642884269));
#112489=CARTESIAN_POINT('Ctrl Pts',(2.89421124586475,-31.6527147589818,
54.7894718528435));
#112490=CARTESIAN_POINT('Ctrl Pts',(2.89270577674961,-31.6553794641724,
54.8120350550889));
#112491=CARTESIAN_POINT('Ctrl Pts',(2.89220735767949,-31.6562069748809,
54.8194717698079));
#112492=CARTESIAN_POINT('Ctrl Pts',(2.89130419949058,-31.6576077442492,
54.8328815655753));
#112493=CARTESIAN_POINT('Ctrl Pts',(2.89090045222045,-31.6581988690253,
54.8388525125584));
#112494=CARTESIAN_POINT('Ctrl Pts',(2.88998778994189,-31.659456482078,54.8522960232315));
#112495=CARTESIAN_POINT('Ctrl Pts',(2.88947791669023,-31.660104754796,54.8597699094282));
#112496=CARTESIAN_POINT('Ctrl Pts',(2.88791768108065,-31.6619247164145,
54.8825372410852));
#112497=CARTESIAN_POINT('Ctrl Pts',(2.88685918718747,-31.6629356605656,
54.8978422300975));
#112498=CARTESIAN_POINT('Ctrl Pts',(2.87834111157345,-31.669314901281,55.0200573273979));
#112499=CARTESIAN_POINT('Ctrl Pts',(2.87048803290338,-31.6645786189451,
55.1272364564882));
#112500=CARTESIAN_POINT('Ctrl Pts',(2.85496826171191,-31.6346843038774,
55.3386910226096));
#112501=CARTESIAN_POINT('Ctrl Pts',(2.84733960055973,-31.60968734588,55.4425137060117));
#112502=CARTESIAN_POINT('Ctrl Pts',(2.83855559392522,-31.5679459582342,
55.5635258536358));
#112503=CARTESIAN_POINT('Ctrl Pts',(2.83709665743696,-31.5605618518459,
55.5836631705559));
#112504=CARTESIAN_POINT('Ctrl Pts',(2.83482708438295,-31.5483654761976,
55.6150361844531));
#112505=CARTESIAN_POINT('Ctrl Pts',(2.83400783891793,-31.5438151425258,
55.6263704778624));
#112506=CARTESIAN_POINT('Ctrl Pts',(2.83248082019742,-31.5350572091674,
55.6475099833509));
#112507=CARTESIAN_POINT('Ctrl Pts',(2.83177209206372,-31.5308792864683,
55.6573267325063));
#112508=CARTESIAN_POINT('Ctrl Pts',(2.83018588366596,-31.5212752165224,
55.6793048166104));
#112509=CARTESIAN_POINT('Ctrl Pts',(2.82931022832937,-31.5157969373391,
55.6914426803144));
#112510=CARTESIAN_POINT('Ctrl Pts',(2.82706742469511,-31.5013145261524,
55.7225308452343));
#112511=CARTESIAN_POINT('Ctrl Pts',(2.82570761951889,-31.4920967516918,
55.7413794408279));
#112512=CARTESIAN_POINT('Ctrl Pts',(2.816093852784,-31.4238710771484,55.8744579580612));
#112513=CARTESIAN_POINT('Ctrl Pts',(2.80832125224955,-31.3521716760421,
55.9816929400111));
#112514=CARTESIAN_POINT('Ctrl Pts',(2.79533865777135,-31.2146708268911,
56.143293390646));
#112515=CARTESIAN_POINT('Ctrl Pts',(2.79018909716237,-31.1557861385896,
56.2027883453288));
#112516=CARTESIAN_POINT('Ctrl Pts',(2.78382474576343,-31.0819521131929,
56.266940479258));
#112517=CARTESIAN_POINT('Ctrl Pts',(2.7828904986132,-31.0710900428015,56.2761366072337));
#112518=CARTESIAN_POINT('Ctrl Pts',(2.7814637003255,-31.0544933075837,56.2898266988611));
#112519=CARTESIAN_POINT('Ctrl Pts',(2.7809781954083,-31.0488444705833,56.2944243200642));
#112520=CARTESIAN_POINT('Ctrl Pts',(2.78008742011743,-31.038482297435,56.302745792299));
#112521=CARTESIAN_POINT('Ctrl Pts',(2.77968299052434,-31.0337787315782,
56.3064813859954));
#112522=CARTESIAN_POINT('Ctrl Pts',(2.77875441001977,-31.0229814783373,
56.3149618015025));
#112523=CARTESIAN_POINT('Ctrl Pts',(2.77822913570513,-31.016874951954,56.3196897251195));
#112524=CARTESIAN_POINT('Ctrl Pts',(2.77657277686449,-30.9976161550111,
56.3343876463584));
#112525=CARTESIAN_POINT('Ctrl Pts',(2.77543209781001,-30.9843489264619,
56.3442044202042));
#112526=CARTESIAN_POINT('Ctrl Pts',(2.7684956901135,-30.903523275283,56.4021712369296));
#112527=CARTESIAN_POINT('Ctrl Pts',(2.7624677182888,-30.8325967535362,56.4454129443026));
#112528=CARTESIAN_POINT('Ctrl Pts',(2.74996617596909,-30.6796953435356,
56.5236325105155));
#112529=CARTESIAN_POINT('Ctrl Pts',(2.74351347344466,-30.5975230270371,
56.5576941062641));
#112530=CARTESIAN_POINT('Ctrl Pts',(2.73375019136946,-30.4660212316411,
56.6002564040124));
#112531=CARTESIAN_POINT('Ctrl Pts',(2.73031840039953,-30.4183648002468,
56.6133716575618));
#112532=CARTESIAN_POINT('Ctrl Pts',(2.7258217092867,-30.353983897029,56.6280441415306));
#112533=CARTESIAN_POINT('Ctrl Pts',(2.72469743180069,-30.3377215460728,
56.631495178735));
#112534=CARTESIAN_POINT('Ctrl Pts',(2.72282870837987,-30.310420992386,56.6368629228397));
#112535=CARTESIAN_POINT('Ctrl Pts',(2.72208008336844,-30.299410512033,56.638912681182));
#112536=CARTESIAN_POINT('Ctrl Pts',(2.7206091570574,-30.2776352411253,56.6427396896492));
#112537=CARTESIAN_POINT('Ctrl Pts',(2.71988671274985,-30.2668720189564,
56.6445225295421));
#112538=CARTESIAN_POINT('Ctrl Pts',(2.71829620642966,-30.2430302827037,
56.6482314809183));
#112539=CARTESIAN_POINT('Ctrl Pts',(2.71742974330725,-30.22994470645,56.6501079302735));
#112540=CARTESIAN_POINT('Ctrl Pts',(2.71488330973983,-30.1912158848906,
56.6551919175608));
#112541=CARTESIAN_POINT('Ctrl Pts',(2.71321697365155,-30.1655181001968,
56.6579588870477));
#112542=CARTESIAN_POINT('Ctrl Pts',(2.7023991179353,-29.9967065247133,56.6721710427702));
#112543=CARTESIAN_POINT('Ctrl Pts',(2.6938380018832,-29.8526983311679,56.6656739724049));
#112544=CARTESIAN_POINT('Ctrl Pts',(2.68230599518897,-29.6686435396513,
56.6332896460315));
#112545=CARTESIAN_POINT('Ctrl Pts',(2.67960534020977,-29.626295757772,56.6241233966154));
#112546=CARTESIAN_POINT('Ctrl Pts',(2.67518135412202,-29.5591748399306,
56.6068308471363));
#112547=CARTESIAN_POINT('Ctrl Pts',(2.67349926900117,-29.5341503899648,
56.599755029947));
#112548=CARTESIAN_POINT('Ctrl Pts',(2.67118061195524,-29.5005093711111,
56.5893866093527));
#112549=CARTESIAN_POINT('Ctrl Pts',(2.67057071900159,-29.4917381382286,
56.586603464184));
#112550=CARTESIAN_POINT('Ctrl Pts',(2.66954188643043,-29.4770812997456,
56.5818187869957));
#112551=CARTESIAN_POINT('Ctrl Pts',(2.66912519735029,-29.4711828578901,
56.579856661386));
#112552=CARTESIAN_POINT('Ctrl Pts',(2.66832066823801,-29.4598699187782,
56.5760229420342));
#112553=CARTESIAN_POINT('Ctrl Pts',(2.66793315373526,-29.4544538763469,
56.5741563591074));
#112554=CARTESIAN_POINT('Ctrl Pts',(2.66687217266515,-29.4397119780404,
56.5689905002283));
#112555=CARTESIAN_POINT('Ctrl Pts',(2.66619560923379,-29.430405889308,56.5656360989789));
#112556=CARTESIAN_POINT('Ctrl Pts',(2.66350352891703,-29.3937266106652,
56.5520446721225));
#112557=CARTESIAN_POINT('Ctrl Pts',(2.66145600574359,-29.3665965656147,
56.541171609305));
#112558=CARTESIAN_POINT('Ctrl Pts',(2.65156626645615,-29.2385575443992,
56.4859049675584));
#112559=CARTESIAN_POINT('Ctrl Pts',(2.64344145086671,-29.1419352694405,
56.4322823150409));
#112560=CARTESIAN_POINT('Ctrl Pts',(2.63127112856187,-29.0034187262987,
56.3363297165009));
#112561=CARTESIAN_POINT('Ctrl Pts',(2.62711164560393,-28.957289154711,56.3006562105568));
#112562=CARTESIAN_POINT('Ctrl Pts',(2.62036568228315,-28.8841961997182,
56.2377376027337));
#112563=CARTESIAN_POINT('Ctrl Pts',(2.61773324718341,-28.8561344807863,
56.2118517138311));
#112564=CARTESIAN_POINT('Ctrl Pts',(2.61410985880653,-28.8181846730051,
56.1743504890903));
#112565=CARTESIAN_POINT('Ctrl Pts',(2.61308517346219,-28.807530787673,56.1635307226346));
#112566=CARTESIAN_POINT('Ctrl Pts',(2.61133436822402,-28.7894681821005,
56.1446781488531));
#112567=CARTESIAN_POINT('Ctrl Pts',(2.61060517438068,-28.7819879934138,
56.1367154913242));
#112568=CARTESIAN_POINT('Ctrl Pts',(2.60921400741425,-28.7678024719221,
56.1213141955596));
#112569=CARTESIAN_POINT('Ctrl Pts',(2.60855152997597,-28.761084852487,56.1138875787272));
#112570=CARTESIAN_POINT('Ctrl Pts',(2.60682113852235,-28.743641190483,56.0942498255165));
#112571=CARTESIAN_POINT('Ctrl Pts',(2.60575785076168,-28.7330259884047,
56.0819413216085));
#112572=CARTESIAN_POINT('Ctrl Pts',(2.60193837916156,-28.6952985371508,
56.0368788814984));
#112573=CARTESIAN_POINT('Ctrl Pts',(2.59922503288759,-28.6692611985757,
56.003243954617));
#112574=CARTESIAN_POINT('Ctrl Pts',(2.58929251678008,-28.5774875695183,
55.8748218620233));
#112575=CARTESIAN_POINT('Ctrl Pts',(2.58236295841184,-28.5203615719412,
55.7742904733263));
#112576=CARTESIAN_POINT('Ctrl Pts',(2.57321250994743,-28.4606342676709,
55.637989541466));
#112577=CARTESIAN_POINT('Ctrl Pts',(2.57114030558061,-28.448124746154,55.6069262677602));
#112578=CARTESIAN_POINT('Ctrl Pts',(2.56903904312142,-28.4365623153847,
55.5755159479327));
#112579=CARTESIAN_POINT('Origin',(5.,-30.,55.));
#112580=CARTESIAN_POINT('',(1.86810673741824,-28.4365624617973,55.5755163456747));
#112581=CARTESIAN_POINT('',(2.06220428404732,-28.4365623101862,55.5755159338105));
#112582=CARTESIAN_POINT('',(5.,-28.4365623102018,55.5755159338528));
#112583=CARTESIAN_POINT('',(2.72303743726837,-28.3340004588354,54.9999657623987));
#112584=CARTESIAN_POINT('Ctrl Pts',(2.06220428404731,-28.4365623101862,
55.5755159338105));
#112585=CARTESIAN_POINT('Ctrl Pts',(2.06232537164583,-28.4372097346566,
55.5772747171192));
#112586=CARTESIAN_POINT('Ctrl Pts',(2.06244636879248,-28.4378601333206,
55.5790324253072));
#112587=CARTESIAN_POINT('Ctrl Pts',(2.06925635199033,-28.474660488052,55.6779724051352));
#112588=CARTESIAN_POINT('Ctrl Pts',(2.07563303131421,-28.5198024133307,
55.7715737442157));
#112589=CARTESIAN_POINT('Ctrl Pts',(2.08880064720991,-28.631104512992,55.956129471173));
#112590=CARTESIAN_POINT('Ctrl Pts',(2.09555584618043,-28.6983337519922,
56.0458089234561));
#112591=CARTESIAN_POINT('Ctrl Pts',(2.1037874159976,-28.7841067908732,56.1390265532599));
#112592=CARTESIAN_POINT('Ctrl Pts',(2.10476402048816,-28.794336702512,56.1498494512293));
#112593=CARTESIAN_POINT('Ctrl Pts',(2.1062425814088,-28.8098761402488,56.1658542797185));
#112594=CARTESIAN_POINT('Ctrl Pts',(2.10673670555073,-28.8150777485499,
56.1711405790335));
#112595=CARTESIAN_POINT('Ctrl Pts',(2.10763579219869,-28.8245533382064,
56.180642699559));
#112596=CARTESIAN_POINT('Ctrl Pts',(2.1080398139472,-28.8288150430316,56.1848703862104));
#112597=CARTESIAN_POINT('Ctrl Pts',(2.10895787655775,-28.8385070444761,
56.1943816458927));
#112598=CARTESIAN_POINT('Ctrl Pts',(2.10947293032625,-28.843950554172,56.1996512305486));
#112599=CARTESIAN_POINT('Ctrl Pts',(2.11106459631092,-28.8607968180041,
56.2157381079754));
#112600=CARTESIAN_POINT('Ctrl Pts',(2.1121498029255,-28.872316489137,56.2264309567949));
#112601=CARTESIAN_POINT('Ctrl Pts',(2.1177880363432,-28.9324223258129,56.2806599319491));
#112602=CARTESIAN_POINT('Ctrl Pts',(2.12248669566025,-28.9833800445922,
56.3214742366377));
#112603=CARTESIAN_POINT('Ctrl Pts',(2.13556722442658,-29.1303544521544,
56.4256509187734));
#112604=CARTESIAN_POINT('Ctrl Pts',(2.1439715499686,-29.2307540869289,56.4822384412262));
#112605=CARTESIAN_POINT('Ctrl Pts',(2.15507093025407,-29.3755552514984,
56.545143054548));
#112606=CARTESIAN_POINT('Ctrl Pts',(2.15804335451875,-29.4155719639695,
56.5607186637322));
#112607=CARTESIAN_POINT('Ctrl Pts',(2.16207531836975,-29.4715675354315,
56.580057346495));
#112608=CARTESIAN_POINT('Ctrl Pts',(2.16317807720657,-29.4870639426854,
56.5851557405528));
#112609=CARTESIAN_POINT('Ctrl Pts',(2.16494659793527,-29.5122025762183,
56.5930192107853));
#112610=CARTESIAN_POINT('Ctrl Pts',(2.16561696100031,-29.5217989332165,
56.5959261511413));
#112611=CARTESIAN_POINT('Ctrl Pts',(2.16701151724068,-29.5419003896495,
56.6018177159694));
#112612=CARTESIAN_POINT('Ctrl Pts',(2.16773515153564,-29.552409796694,56.604786050461));
#112613=CARTESIAN_POINT('Ctrl Pts',(2.16945432388753,-29.577560171593,56.6116233716226));
#112614=CARTESIAN_POINT('Ctrl Pts',(2.17044673116837,-29.5922263582524,
56.6153965403498));
#112615=CARTESIAN_POINT('Ctrl Pts',(2.1738991728499,-29.643739004778,56.6279029164711));
#112616=CARTESIAN_POINT('Ctrl Pts',(2.17632568794083,-29.6808314817495,
56.6355798976115));
#112617=CARTESIAN_POINT('Ctrl Pts',(2.18236256735586,-29.7749133965924,
56.651728902515));
#112618=CARTESIAN_POINT('Ctrl Pts',(2.18592628177591,-29.8321409245678,
56.6585223567415));
#112619=CARTESIAN_POINT('Ctrl Pts',(2.19615394835175,-29.9984806117492,
56.6695685422116));
#112620=CARTESIAN_POINT('Ctrl Pts',(2.20270296308616,-30.1077894711117,
56.6660848557805));
#112621=CARTESIAN_POINT('Ctrl Pts',(2.21158248489456,-30.2467011034689,
56.6479246333367));
#112622=CARTESIAN_POINT('Ctrl Pts',(2.21357624777269,-30.2773196429087,
56.6430491658818));
#112623=CARTESIAN_POINT('Ctrl Pts',(2.21627658998945,-30.3177159250042,
56.6354555208864));
#112624=CARTESIAN_POINT('Ctrl Pts',(2.21694510200407,-30.3276323380065,
56.6334978445986));
#112625=CARTESIAN_POINT('Ctrl Pts',(2.21800315353894,-30.3431823633909,
56.6302807065075));
#112626=CARTESIAN_POINT('Ctrl Pts',(2.21838935393333,-30.3488284870189,
56.629081950256));
#112627=CARTESIAN_POINT('Ctrl Pts',(2.21919292922282,-30.3605118456347,
56.626537877586));
#112628=CARTESIAN_POINT('Ctrl Pts',(2.21961056482069,-30.3665479364537,
56.6251882547481));
#112629=CARTESIAN_POINT('Ctrl Pts',(2.22064266066459,-30.3813796825504,
56.6217851643071));
#112630=CARTESIAN_POINT('Ctrl Pts',(2.22125920328352,-30.3901663460958,
56.6196937347975));
#112631=CARTESIAN_POINT('Ctrl Pts',(2.22357609493654,-30.422928819136,56.6116134523345));
#112632=CARTESIAN_POINT('Ctrl Pts',(2.22529937686746,-30.4467861772772,
56.6051631257141));
#112633=CARTESIAN_POINT('Ctrl Pts',(2.22987418722147,-30.5090089635778,
56.586845361317));
#112634=CARTESIAN_POINT('Ctrl Pts',(2.23275607171611,-30.5471034083806,
56.5741174618133));
#112635=CARTESIAN_POINT('Ctrl Pts',(2.24419054467396,-30.6951232592355,
56.5186395969525));
#112636=CARTESIAN_POINT('Ctrl Pts',(2.25285324302594,-30.8008562305663,
56.4656388529966));
#112637=CARTESIAN_POINT('Ctrl Pts',(2.26476217240214,-30.9425238823466,
56.3746801249062));
#112638=CARTESIAN_POINT('Ctrl Pts',(2.26826856786382,-30.983684970585,56.3455339113695));
#112639=CARTESIAN_POINT('Ctrl Pts',(2.27287768223769,-31.0370360334894,
56.3039969655379));
#112640=CARTESIAN_POINT('Ctrl Pts',(2.27404186700073,-31.0504433003046,
56.2932210685962));
#112641=CARTESIAN_POINT('Ctrl Pts',(2.27595844493011,-31.072393577105,56.2750122117591));
#112642=CARTESIAN_POINT('Ctrl Pts',(2.27671548372277,-31.0810317185521,
56.2676965562624));
#112643=CARTESIAN_POINT('Ctrl Pts',(2.27819812991193,-31.0978821783893,
56.2531283806536));
#112644=CARTESIAN_POINT('Ctrl Pts',(2.27892392746534,-31.1060988290708,
56.2458817785384));
#112645=CARTESIAN_POINT('Ctrl Pts',(2.28065803308938,-31.125647952973,56.2282947562899));
#112646=CARTESIAN_POINT('Ctrl Pts',(2.2816630632547,-31.1369103858714,56.2178777125427));
#112647=CARTESIAN_POINT('Ctrl Pts',(2.28521602191174,-31.1764587641485,
56.1802711568812));
#112648=CARTESIAN_POINT('Ctrl Pts',(2.28772766795328,-31.2039275785866,
56.1522386865298));
#112649=CARTESIAN_POINT('Ctrl Pts',(2.2940420544524,-31.2713335873471,56.0784043599753));
#112650=CARTESIAN_POINT('Ctrl Pts',(2.29779197162577,-31.3098029094427,
56.0313400000281));
#112651=CARTESIAN_POINT('Ctrl Pts',(2.30692224562847,-31.3976704159359,
55.910970646456));
#112652=CARTESIAN_POINT('Ctrl Pts',(2.31225296111814,-31.4439697563155,
55.8356433702257));
#112653=CARTESIAN_POINT('Ctrl Pts',(2.3205469139733,-31.5042476474273,55.7174711414809));
#112654=CARTESIAN_POINT('Ctrl Pts',(2.32336742338587,-31.5228247228412,
55.6771483885607));
#112655=CARTESIAN_POINT('Ctrl Pts',(2.32701661797487,-31.5441024545265,
55.625645625704));
#112656=CARTESIAN_POINT('Ctrl Pts',(2.32776542395504,-31.5483290824238,
55.6151112696775));
#112657=CARTESIAN_POINT('Ctrl Pts',(2.32896461272201,-31.5548708405906,
55.5983120136017));
#112658=CARTESIAN_POINT('Ctrl Pts',(2.32941094913306,-31.5572565922799,
55.5920747405724));
#112659=CARTESIAN_POINT('Ctrl Pts',(2.3302721886907,-31.5617646490663,55.5800731948575));
#112660=CARTESIAN_POINT('Ctrl Pts',(2.33068675504299,-31.5638926652388,
55.5743112892845));
#112661=CARTESIAN_POINT('Ctrl Pts',(2.33169946406485,-31.5689903492804,
55.5602701574488));
#112662=CARTESIAN_POINT('Ctrl Pts',(2.33229951492806,-31.5719263800903,
55.5519789963861));
#112663=CARTESIAN_POINT('Ctrl Pts',(2.33448305351163,-31.582311545585,55.5218970223855));
#112664=CARTESIAN_POINT('Ctrl Pts',(2.33608630911952,-31.5893739469681,
55.4999766557985));
#112665=CARTESIAN_POINT('Ctrl Pts',(2.34688195458569,-31.6333724849818,
55.353046209968));
#112666=CARTESIAN_POINT('Ctrl Pts',(2.35653951194391,-31.6559809784502,
55.2242203392077));
#112667=CARTESIAN_POINT('Ctrl Pts',(2.3713837843607,-31.6676404691382,55.0180706027472));
#112668=CARTESIAN_POINT('Ctrl Pts',(2.37675188179722,-31.6667252280184,
54.9418515613006));
#112669=CARTESIAN_POINT('Ctrl Pts',(2.38328298878817,-31.6590431426242,
54.846684956322));
#112670=CARTESIAN_POINT('Ctrl Pts',(2.38459490360139,-31.6571525643435,
54.8274454149686));
#112671=CARTESIAN_POINT('Ctrl Pts',(2.38668864642201,-31.6535729990847,
54.7965526561828));
#112672=CARTESIAN_POINT('Ctrl Pts',(2.38747699158815,-31.6520946505789,
54.7848773307288));
#112673=CARTESIAN_POINT('Ctrl Pts',(2.38897846674383,-31.6490284765637,
54.7625620394904));
#112674=CARTESIAN_POINT('Ctrl Pts',(2.38969219923063,-31.6474610718561,
54.7519199170015));
#112675=CARTESIAN_POINT('Ctrl Pts',(2.39133412842055,-31.643601005332,54.7273636665469));
#112676=CARTESIAN_POINT('Ctrl Pts',(2.39225994897923,-31.6412345179996,
54.7134618485977));
#112677=CARTESIAN_POINT('Ctrl Pts',(2.39522375499666,-31.6330471136552,
54.6688005721892));
#112678=CARTESIAN_POINT('Ctrl Pts',(2.39723996913978,-31.626535501754,54.638173523921));
#112679=CARTESIAN_POINT('Ctrl Pts',(2.40865774937288,-31.584311833556,54.4638804725321));
#112680=CARTESIAN_POINT('Ctrl Pts',(2.41744539140517,-31.5304448980797,
54.3253108118202));
#112681=CARTESIAN_POINT('Ctrl Pts',(2.43005911113584,-31.4322182909615,
54.1471343942842));
#112682=CARTESIAN_POINT('Ctrl Pts',(2.43355100001086,-31.4030518897346,
54.0999594254477));
#112683=CARTESIAN_POINT('Ctrl Pts',(2.43795956684985,-31.3647790702097,
54.0444487600586));
#112684=CARTESIAN_POINT('Ctrl Pts',(2.43875046842822,-31.3578592136122,
54.0346407828298));
#112685=CARTESIAN_POINT('Ctrl Pts',(2.44000150399177,-31.3468428827081,
54.0193794035324));
#112686=CARTESIAN_POINT('Ctrl Pts',(2.44045697382574,-31.3428177103678,
54.0138747049737));
#112687=CARTESIAN_POINT('Ctrl Pts',(2.44132361103844,-31.3351346272211,
54.003501828411));
#112688=CARTESIAN_POINT('Ctrl Pts',(2.44173431498744,-31.3314836717503,
53.9986287872728));
#112689=CARTESIAN_POINT('Ctrl Pts',(2.44272061236917,-31.3226911512107,
53.9870262388145));
#112690=CARTESIAN_POINT('Ctrl Pts',(2.44329787484986,-31.3175248797891,
53.9803157813484));
#112691=CARTESIAN_POINT('Ctrl Pts',(2.44530828720449,-31.299455578073,53.9572121864804));
#112692=CARTESIAN_POINT('Ctrl Pts',(2.44675745515867,-31.2862965224039,
53.941022955255));
#112693=CARTESIAN_POINT('Ctrl Pts',(2.45043219755399,-31.252516669011,53.901023222342));
#112694=CARTESIAN_POINT('Ctrl Pts',(2.45267615215947,-31.23151847852,53.8775428884371));
#112695=CARTESIAN_POINT('Ctrl Pts',(2.4644000109941,-31.1193868060104,53.7590923163931));
#112696=CARTESIAN_POINT('Ctrl Pts',(2.47411700419691,-31.0178819210741,
53.6745559900337));
#112697=CARTESIAN_POINT('Ctrl Pts',(2.48700607651239,-30.8650922961737,
53.5753152824368));
#112698=CARTESIAN_POINT('Ctrl Pts',(2.49052275850408,-30.8214658255248,
53.5497220805052));
#112699=CARTESIAN_POINT('Ctrl Pts',(2.4951428077502,-30.7615098031002,53.5181244475952));
#112700=CARTESIAN_POINT('Ctrl Pts',(2.4963080232623,-30.746156961148,53.510334882938));
#112701=CARTESIAN_POINT('Ctrl Pts',(2.49822583472365,-30.7205104297312,
53.4978186146416));
#112702=CARTESIAN_POINT('Ctrl Pts',(2.49898308859381,-30.7102846613519,
53.4929565684259));
#112703=CARTESIAN_POINT('Ctrl Pts',(2.50046582294605,-30.690070508046,53.4835967996442));
#112704=CARTESIAN_POINT('Ctrl Pts',(2.50119149677422,-30.6800857761678,
53.4790926001512));
#112705=CARTESIAN_POINT('Ctrl Pts',(2.50292475912295,-30.6560225347886,
53.4685218203231));
#112706=CARTESIAN_POINT('Ctrl Pts',(2.50392907806751,-30.6419031343307,
53.462550367359));
#112707=CARTESIAN_POINT('Ctrl Pts',(2.50747629739231,-30.5914336491069,
53.4420220368113));
#112708=CARTESIAN_POINT('Ctrl Pts',(2.5099830763626,-30.5546536001011,53.4285519879416));
#112709=CARTESIAN_POINT('Ctrl Pts',(2.51628140465738,-30.4598709784488,
53.3975826063392));
#112710=CARTESIAN_POINT('Ctrl Pts',(2.5200205008995,-30.401325838068,53.3819267040085));
#112711=CARTESIAN_POINT('Ctrl Pts',(2.52911069557165,-30.2561234165271,
53.3514654878174));
#112712=CARTESIAN_POINT('Ctrl Pts',(2.53441259504023,-30.1689058108366,
53.3402607070238));
#112713=CARTESIAN_POINT('Ctrl Pts',(2.54271454378882,-30.0362002277193,
53.333783670764));
#112714=CARTESIAN_POINT('Ctrl Pts',(2.54557713043139,-29.99111731265,53.3334143789789));
#112715=CARTESIAN_POINT('Ctrl Pts',(2.54927382481636,-29.9346904436815,
53.3352416067863));
#112716=CARTESIAN_POINT('Ctrl Pts',(2.55002548734156,-29.923305888315,53.3357272334477));
#112717=CARTESIAN_POINT('Ctrl Pts',(2.55122819544278,-29.9052492522322,
53.3366831266628));
#112718=CARTESIAN_POINT('Ctrl Pts',(2.55167515386943,-29.8985732399226,
53.3370768707666));
#112719=CARTESIAN_POINT('Ctrl Pts',(2.55253671827702,-29.8857745982139,
53.3379090771366));
#112720=CARTESIAN_POINT('Ctrl Pts',(2.55295097855857,-29.8796517665738,
53.338341197505));
#112721=CARTESIAN_POINT('Ctrl Pts',(2.55396169143693,-29.8647856678546,
53.3394729693465));
#112722=CARTESIAN_POINT('Ctrl Pts',(2.55456003425262,-29.8560453433546,
53.34020784932));
#112723=CARTESIAN_POINT('Ctrl Pts',(2.55673016520325,-29.824547395081,53.3431068301361));
#112724=CARTESIAN_POINT('Ctrl Pts',(2.55832141637395,-29.8018302012381,
53.3456701668783));
#112725=CARTESIAN_POINT('Ctrl Pts',(2.57014304077642,-29.6353238787771,
53.3679367817011));
#112726=CARTESIAN_POINT('Ctrl Pts',(2.58093805936272,-29.494603708959,53.4058866255745));
#112727=CARTESIAN_POINT('Ctrl Pts',(2.5958109354758,-29.3022010270493,53.4858570500897));
#112728=CARTESIAN_POINT('Ctrl Pts',(2.60024015860938,-29.2452490993818,
53.5134250434331));
#112729=CARTESIAN_POINT('Ctrl Pts',(2.60582443997335,-29.1738202688117,
53.5531670132731));
#112730=CARTESIAN_POINT('Ctrl Pts',(2.60707949169387,-29.157795432562,53.5624360347152));
#112731=CARTESIAN_POINT('Ctrl Pts',(2.60910500518627,-29.1319899343932,
53.5779420032617));
#112732=CARTESIAN_POINT('Ctrl Pts',(2.60988123722554,-29.1221144376701,
53.5840171712596));
#112733=CARTESIAN_POINT('Ctrl Pts',(2.6113742371713,-29.1031511415047,53.5959575906852));
#112734=CARTESIAN_POINT('Ctrl Pts',(2.61209145801452,-29.0940554880607,
53.6018092001378));
#112735=CARTESIAN_POINT('Ctrl Pts',(2.61376303092771,-29.072895216172,53.6157156612731));
#112736=CARTESIAN_POINT('Ctrl Pts',(2.61471471752167,-29.0608774158467,
53.6238404145796));
#112737=CARTESIAN_POINT('Ctrl Pts',(2.6178607294643,-29.0212697443292,53.6513780940761));
#112738=CARTESIAN_POINT('Ctrl Pts',(2.62002922316321,-28.9941624439332,
53.6714726132932));
#112739=CARTESIAN_POINT('Ctrl Pts',(2.62526424652121,-28.9294581597486,
53.7225541529866));
#112740=CARTESIAN_POINT('Ctrl Pts',(2.62829939636591,-28.892573652032,53.7543936711335));
#112741=CARTESIAN_POINT('Ctrl Pts',(2.63539054523375,-28.8089273258662,
53.8332559756977));
#112742=CARTESIAN_POINT('Ctrl Pts',(2.63941263783197,-28.7634737634398,
53.8815418020753));
#112743=CARTESIAN_POINT('Ctrl Pts',(2.64822466703058,-28.671238693962,53.9920400139026));
#112744=CARTESIAN_POINT('Ctrl Pts',(2.6530166086471,-28.6256986445518,54.0550751933649));
#112745=CARTESIAN_POINT('Ctrl Pts',(2.65910972067198,-28.5760893625325,
54.1349551968652));
#112746=CARTESIAN_POINT('Ctrl Pts',(2.66018099248169,-28.5676580842231,
54.1489884829723));
#112747=CARTESIAN_POINT('Ctrl Pts',(2.66177448828764,-28.555567660035,54.16980092671));
#112748=CARTESIAN_POINT('Ctrl Pts',(2.66228698183378,-28.5517462608473,
54.1764853448608));
#112749=CARTESIAN_POINT('Ctrl Pts',(2.66320459873939,-28.5450261128556,
54.1884317176277));
#112750=CARTESIAN_POINT('Ctrl Pts',(2.66360857029623,-28.5421092927669,
54.1936832057829));
#112751=CARTESIAN_POINT('Ctrl Pts',(2.66450803698854,-28.5357072809428,
54.2053577960637));
#112752=CARTESIAN_POINT('Ctrl Pts',(2.6650043408485,-28.5322359574577,54.2117880299653));
#112753=CARTESIAN_POINT('Ctrl Pts',(2.66648223450761,-28.5220760152506,
54.2309080266732));
#112754=CARTESIAN_POINT('Ctrl Pts',(2.66747079372325,-28.5155090597173,
54.2436611990011));
#112755=CARTESIAN_POINT('Ctrl Pts',(2.669787532922,-28.5006283879976,54.2735003215386));
#112756=CARTESIAN_POINT('Ctrl Pts',(2.67112161085381,-28.4924407775574,
54.2906466755577));
#112757=CARTESIAN_POINT('Ctrl Pts',(2.67589012380187,-28.4644569974568,
54.351923666433));
#112758=CARTESIAN_POINT('Ctrl Pts',(2.67938092240163,-28.4462919916914,
54.396770281843));
#112759=CARTESIAN_POINT('Ctrl Pts',(2.69259541230682,-28.3853722202072,
54.5682685761565));
#112760=CARTESIAN_POINT('Ctrl Pts',(2.70235946782802,-28.3559458481188,
54.6991469049287));
#112761=CARTESIAN_POINT('Ctrl Pts',(2.71369123867573,-28.3394891846822,
54.8616547109419));
#112762=CARTESIAN_POINT('Ctrl Pts',(2.71572545086426,-28.3372894008935,
54.8912376681486));
#112763=CARTESIAN_POINT('Ctrl Pts',(2.71867277504418,-28.3352233232247,
54.9346851049013));
#112764=CARTESIAN_POINT('Ctrl Pts',(2.71960486850662,-28.3347383030971,
54.9485129148139));
#112765=CARTESIAN_POINT('Ctrl Pts',(2.72102151940647,-28.334260260276,54.9696582383626));
#112766=CARTESIAN_POINT('Ctrl Pts',(2.72150992748456,-28.3341430975167,
54.976972052061));
#112767=CARTESIAN_POINT('Ctrl Pts',(2.72234473947519,-28.3340248097476,
54.9895127770705));
#112768=CARTESIAN_POINT('Ctrl Pts',(2.72269187194403,-28.3340001073699,
54.9947392960198));
#112769=CARTESIAN_POINT('Ctrl Pts',(2.72303824113791,-28.3340000003493,
54.9999658866651));
#112770=CARTESIAN_POINT('Ctrl Pts',(2.72303822942304,-28.3340000003529,
54.9999657098917));
#112771=CARTESIAN_POINT('Ctrl Pts',(2.72328729578586,-28.3339999229979,
55.003724034477));
#112772=CARTESIAN_POINT('Ctrl Pts',(2.72353596649594,-28.3340125632317,
55.0074823807488));
#112773=CARTESIAN_POINT('Ctrl Pts',(2.72421539065123,-28.3340819571948,
55.0177671377999));
#112774=CARTESIAN_POINT('Ctrl Pts',(2.72464534569333,-28.3341643443612,
55.0242933522203));
#112775=CARTESIAN_POINT('Ctrl Pts',(2.7262307742564,-28.3346107689681,55.048421854334));
#112776=CARTESIAN_POINT('Ctrl Pts',(2.72737878432969,-28.3352154790134,
55.0660189655808));
#112777=CARTESIAN_POINT('Ctrl Pts',(2.73222385219982,-28.3389708721576,
55.1407596639566));
#112778=CARTESIAN_POINT('Ctrl Pts',(2.73583856341932,-28.344785934576,55.197733325189));
#112779=CARTESIAN_POINT('Ctrl Pts',(2.74629491638921,-28.3704529590116,
55.3639159669714));
#112780=CARTESIAN_POINT('Ctrl Pts',(2.75293891978614,-28.3982795014471,
55.4715174317822));
#112781=CARTESIAN_POINT('Ctrl Pts',(2.75980443758381,-28.4365622822719,
55.5755158579788));
#112782=CARTESIAN_POINT('Ctrl Pts',(2.56903904312142,-28.4365623153847,
55.5755159479327));
#112783=CARTESIAN_POINT('Ctrl Pts',(2.56703835108036,-28.4255532845451,
55.5456089857579));
#112784=CARTESIAN_POINT('Ctrl Pts',(2.56501128067198,-28.415402857017,55.5153874046099));
#112785=CARTESIAN_POINT('Ctrl Pts',(2.56192254398484,-28.4015461573019,
55.4698390721243));
#112786=CARTESIAN_POINT('Ctrl Pts',(2.56089227150846,-28.3971814487163,
55.4547263888258));
#112787=CARTESIAN_POINT('Ctrl Pts',(2.55934855448598,-28.3910323585701,
55.4322459322886));
#112788=CARTESIAN_POINT('Ctrl Pts',(2.55884399565741,-28.3890830825208,
55.4249236361458));
#112789=CARTESIAN_POINT('Ctrl Pts',(2.55793467883482,-28.3856796228417,
55.411778745954));
#112790=CARTESIAN_POINT('Ctrl Pts',(2.55753098331845,-28.3842068552135,
55.4059612374387));
#112791=CARTESIAN_POINT('Ctrl Pts',(2.55662469014299,-28.3809857071768,
55.3929422785539));
#112792=CARTESIAN_POINT('Ctrl Pts',(2.55612120362156,-28.3792539435179,
55.3857371252025));
#112793=CARTESIAN_POINT('Ctrl Pts',(2.55459981462748,-28.3741919823816,
55.3640403647579));
#112794=CARTESIAN_POINT('Ctrl Pts',(2.55357433846662,-28.3710077738259,
55.3495159313299));
#112795=CARTESIAN_POINT('Ctrl Pts',(2.5447505544529,-28.3454989159792,55.2252293185456));
#112796=CARTESIAN_POINT('Ctrl Pts',(2.53651830970599,-28.3341036274991,
55.1135246394297));
#112797=CARTESIAN_POINT('Ctrl Pts',(2.52138069507772,-28.3339120416039,
54.9050563349742));
#112798=CARTESIAN_POINT('Ctrl Pts',(2.51447543413713,-28.3422033913261,
54.8087432211969));
#112799=CARTESIAN_POINT('Ctrl Pts',(2.50627879320001,-28.3626384096543,
54.6916093334645));
#112800=CARTESIAN_POINT('Ctrl Pts',(2.50474821514035,-28.3669330379638,
54.6696211831237));
#112801=CARTESIAN_POINT('Ctrl Pts',(2.50230220635249,-28.3745727123223,
54.6343080775627));
#112802=CARTESIAN_POINT('Ctrl Pts',(2.50137815646881,-28.3776412226831,
54.6209268317182));
#112803=CARTESIAN_POINT('Ctrl Pts',(2.49974279163186,-28.3833969408986,
54.5971784515154));
#112804=CARTESIAN_POINT('Ctrl Pts',(2.49902944573445,-28.3860193355058,
54.5867965701316));
#112805=CARTESIAN_POINT('Ctrl Pts',(2.49752649549474,-28.3917808996816,
54.5648790645174));
#112806=CARTESIAN_POINT('Ctrl Pts',(2.49673772442098,-28.3949445198246,
54.5533504492246));
#112807=CARTESIAN_POINT('Ctrl Pts',(2.49462546461138,-28.4037920440569,
54.5224175976414));
#112808=CARTESIAN_POINT('Ctrl Pts',(2.49330945477949,-28.4097056550107,
54.5030807475177));
#112809=CARTESIAN_POINT('Ctrl Pts',(2.48464430264063,-28.4512847352377,
54.3754759257311));
#112810=CARTESIAN_POINT('Ctrl Pts',(2.47767019940445,-28.4976297409374,
54.2710026203267));
#112811=CARTESIAN_POINT('Ctrl Pts',(2.4645277693078,-28.6045895067659,54.0842316977445));
#112812=CARTESIAN_POINT('Ctrl Pts',(2.45837431571896,-28.6627868525958,
54.0011719123958));
#112813=CARTESIAN_POINT('Ctrl Pts',(2.45078834182361,-28.7383130714074,
53.9119054837793));
#112814=CARTESIAN_POINT('Ctrl Pts',(2.44975778235109,-28.7486454778635,
53.9000384561234));
#112815=CARTESIAN_POINT('Ctrl Pts',(2.44821371706354,-28.7642007284754,
53.8826757003381));
#112816=CARTESIAN_POINT('Ctrl Pts',(2.44770910276128,-28.7692958458465,
53.8770660262105));
#112817=CARTESIAN_POINT('Ctrl Pts',(2.44679972961303,-28.7784940892631,
53.8670766460264));
#112818=CARTESIAN_POINT('Ctrl Pts',(2.44639603388026,-28.7825828549661,
53.8626840772073));
#112819=CARTESIAN_POINT('Ctrl Pts',(2.4454897952363,-28.7917730550158,53.8529173733814));
#112820=CARTESIAN_POINT('Ctrl Pts',(2.44498636406658,-28.7968866048078,
53.84755518314));
#112821=CARTESIAN_POINT('Ctrl Pts',(2.44346530923389,-28.8123661527817,
53.8315382665714));
#112822=CARTESIAN_POINT('Ctrl Pts',(2.44244011659792,-28.8228388400482,
53.820988319422));
#112823=CARTESIAN_POINT('Ctrl Pts',(2.44002156029704,-28.8476672351425,
53.7966373306589));
#112824=CARTESIAN_POINT('Ctrl Pts',(2.43862160262966,-28.862131830105,53.782950917727));
#112825=CARTESIAN_POINT('Ctrl Pts',(2.43350940658966,-28.9153944255774,
53.7343333684519));
#112826=CARTESIAN_POINT('Ctrl Pts',(2.42973301407763,-28.9555819868563,
53.7009728140392));
#112827=CARTESIAN_POINT('Ctrl Pts',(2.41656146691648,-29.1002856582031,
53.5919120668428));
#112828=CARTESIAN_POINT('Ctrl Pts',(2.40715987144216,-29.2119941384566,
53.5264820533905));
#112829=CARTESIAN_POINT('Ctrl Pts',(2.3961897696172,-29.3568803729204,53.4628579853087));
#112830=CARTESIAN_POINT('Ctrl Pts',(2.3941883938128,-29.3839181213363,53.4518230939087));
#112831=CARTESIAN_POINT('Ctrl Pts',(2.3912773375423,-29.4241239345395,53.4366341965357));
#112832=CARTESIAN_POINT('Ctrl Pts',(2.39034937294933,-29.437074635501,53.4319244495153));
#112833=CARTESIAN_POINT('Ctrl Pts',(2.38870750341623,-29.4602227096479,
53.4238299993902));
#112834=CARTESIAN_POINT('Ctrl Pts',(2.38799154866458,-29.4703970496479,
53.4203822873007));
#112835=CARTESIAN_POINT('Ctrl Pts',(2.3864956940411,-29.491819396112,53.4133532859725));
#112836=CARTESIAN_POINT('Ctrl Pts',(2.38571650565754,-29.5030735847893,
53.4097926326291));
#112837=CARTESIAN_POINT('Ctrl Pts',(2.38365967646332,-29.5330261765167,
53.4006651291111));
#112838=CARTESIAN_POINT('Ctrl Pts',(2.38238882909739,-29.5517864870996,
53.395306484153));
#112839=CARTESIAN_POINT('Ctrl Pts',(2.37528923996673,-29.6579175994826,
53.3669980200577));
#112840=CARTESIAN_POINT('Ctrl Pts',(2.36968483959418,-29.7469520122311,
53.3508530768575));
#112841=CARTESIAN_POINT('Ctrl Pts',(2.36069739872477,-29.8929118451649,
53.3364917698487));
#112842=CARTESIAN_POINT('Ctrl Pts',(2.35727588964617,-29.9492003328648,
53.3338226953154));
#112843=CARTESIAN_POINT('Ctrl Pts',(2.3492002131386,-30.0807564356624,53.3342582193225));
#112844=CARTESIAN_POINT('Ctrl Pts',(2.3445281650401,-30.1558849720682,53.3396041865704));
#112845=CARTESIAN_POINT('Ctrl Pts',(2.33881232788712,-30.2425488653579,
53.3517048489213));
#112846=CARTESIAN_POINT('Ctrl Pts',(2.33800373221752,-30.254693659358,53.3535377394982));
#112847=CARTESIAN_POINT('Ctrl Pts',(2.33672635232354,-30.2736768174056,
53.3566177253608));
#112848=CARTESIAN_POINT('Ctrl Pts',(2.33626244971412,-30.280529811979,53.3577736693134));
#112849=CARTESIAN_POINT('Ctrl Pts',(2.33539000788557,-30.2933364589578,
53.3600163573909));
#112850=CARTESIAN_POINT('Ctrl Pts',(2.33498204424106,-30.2992916804859,
53.3610927080827));
#112851=CARTESIAN_POINT('Ctrl Pts',(2.3340162496017,-30.31331317584,53.3637059309768));
#112852=CARTESIAN_POINT('Ctrl Pts',(2.33345693650485,-30.3213740963753,
53.3652700193635));
#112853=CARTESIAN_POINT('Ctrl Pts',(2.33157415325444,-30.3483226184663,
53.370705954563));
#112854=CARTESIAN_POINT('Ctrl Pts',(2.33023716885546,-30.3671537350826,
53.3748459184671));
#112855=CARTESIAN_POINT('Ctrl Pts',(2.32690961976266,-30.4133745851862,
53.3858517246691));
#112856=CARTESIAN_POINT('Ctrl Pts',(2.32490451916805,-30.4406692358917,
53.3930887867935));
#112857=CARTESIAN_POINT('Ctrl Pts',(2.31572802510407,-30.563590940929,53.4290481676522));
#112858=CARTESIAN_POINT('Ctrl Pts',(2.3083850395483,-30.6567020471508,53.4656378357968));
#112859=CARTESIAN_POINT('Ctrl Pts',(2.29520339350666,-30.8201431983275,
53.5474845819436));
#112860=CARTESIAN_POINT('Ctrl Pts',(2.28933579930071,-30.8914405336698,
53.5901158117819));
#112861=CARTESIAN_POINT('Ctrl Pts',(2.28231555892406,-30.9753107606886,
53.6491818670247));
#112862=CARTESIAN_POINT('Ctrl Pts',(2.28098393227696,-30.9911469095463,
53.6607582111378));
#112863=CARTESIAN_POINT('Ctrl Pts',(2.2788667120394,-31.016197820083,53.6797584153974));
#112864=CARTESIAN_POINT('Ctrl Pts',(2.2780743328379,-31.0255439463336,53.6870051493337));
#112865=CARTESIAN_POINT('Ctrl Pts',(2.27657008073348,-31.0432264373216,
53.7010196808139));
#112866=CARTESIAN_POINT('Ctrl Pts',(2.27585755480261,-31.051576047011,53.707769720322));
#112867=CARTESIAN_POINT('Ctrl Pts',(2.27422535106344,-31.0706378458176,
53.7234868823847));
#112868=CARTESIAN_POINT('Ctrl Pts',(2.2733079576977,-31.0813037655132,53.732509044325));
#112869=CARTESIAN_POINT('Ctrl Pts',(2.27040065826232,-31.1149349528493,
53.7616907595333));
#112870=CARTESIAN_POINT('Ctrl Pts',(2.26843134516235,-31.1374604122517,
53.7823490967137));
#112871=CARTESIAN_POINT('Ctrl Pts',(2.26378074398716,-31.1898721913184,
53.8331409470337));
#112872=CARTESIAN_POINT('Ctrl Pts',(2.26112192150893,-31.2192008410207,
53.8638197464072));
#112873=CARTESIAN_POINT('Ctrl Pts',(2.25391905425235,-31.2962132114888,
53.9507977488816));
#112874=CARTESIAN_POINT('Ctrl Pts',(2.24944290793472,-31.3413799036468,
54.0091950863668));
#112875=CARTESIAN_POINT('Ctrl Pts',(2.24410794920097,-31.3900407675514,
54.0815644312773));
#112876=CARTESIAN_POINT('Ctrl Pts',(2.2432832906862,-31.3974167380233,54.0928265412012));
#112877=CARTESIAN_POINT('Ctrl Pts',(2.23791108319823,-31.4444538425068,
54.1665809545085));
#112878=CARTESIAN_POINT('Ctrl Pts',(2.23331127110286,-31.4800446055248,
54.2315604178246));
#112879=CARTESIAN_POINT('Ctrl Pts',(2.22767576188936,-31.516362482387,54.3098177290135));
#112880=CARTESIAN_POINT('Ctrl Pts',(2.22686745979227,-31.5214075005587,
54.3210110894427));
#112881=CARTESIAN_POINT('Ctrl Pts',(2.2255904439769,-31.529113305343,54.3386250789237));
#112882=CARTESIAN_POINT('Ctrl Pts',(2.22512660737437,-31.5318585268876,
54.3450085985029));
#112883=CARTESIAN_POINT('Ctrl Pts',(2.2242542155818,-31.5369198486099,54.3569836643989));
#112884=CARTESIAN_POINT('Ctrl Pts',(2.22384623512155,-31.5392455178413,
54.3625708980347));
#112885=CARTESIAN_POINT('Ctrl Pts',(2.22288029982929,-31.544655492089,54.375770181163));
#112886=CARTESIAN_POINT('Ctrl Pts',(2.22232086158404,-31.5477140058777,
54.3833925033628));
#112887=CARTESIAN_POINT('Ctrl Pts',(2.22043720596458,-31.5577673375764,
54.4089931720024));
#112888=CARTESIAN_POINT('Ctrl Pts',(2.21909945793434,-31.5645059374945,
54.4270696019089));
#112889=CARTESIAN_POINT('Ctrl Pts',(2.21576958235504,-31.5803375905998,
54.4719019708231));
#112890=CARTESIAN_POINT('Ctrl Pts',(2.21376289459154,-31.5890665002595,
54.4987795831598));
#112891=CARTESIAN_POINT('Ctrl Pts',(2.20457234774951,-31.6255705800626,
54.621742186336));
#112892=CARTESIAN_POINT('Ctrl Pts',(2.19721651169948,-31.6453425273582,
54.7199873379671));
#112893=CARTESIAN_POINT('Ctrl Pts',(2.18403780551838,-31.665153196257,54.9016738693175));
#112894=CARTESIAN_POINT('Ctrl Pts',(2.1781846997846,-31.6679827934126,54.9844979088606));
#112895=CARTESIAN_POINT('Ctrl Pts',(2.17117843492911,-31.6638531943162,
55.0867930224263));
#112896=CARTESIAN_POINT('Ctrl Pts',(2.16984721069288,-31.6627164115778,
55.1063704500606));
#112897=CARTESIAN_POINT('Ctrl Pts',(2.16773047312117,-31.6603404632456,
55.137714807446));
#112898=CARTESIAN_POINT('Ctrl Pts',(2.16693817966036,-31.6593211783186,
55.1494960258417));
#112899=CARTESIAN_POINT('Ctrl Pts',(2.16543399423523,-31.6571372362708,
55.1719519001914));
#112900=CARTESIAN_POINT('Ctrl Pts',(2.16472145024848,-31.6559946498985,
55.1826280496733));
#112901=CARTESIAN_POINT('Ctrl Pts',(2.16308906981575,-31.6531279019413,
55.2071698451742));
#112902=CARTESIAN_POINT('Ctrl Pts',(2.1621715195509,-31.6513323492107,55.2210264623908));
#112903=CARTESIAN_POINT('Ctrl Pts',(2.15926315580417,-31.6450529981877,
55.2651249119903));
#112904=CARTESIAN_POINT('Ctrl Pts',(2.1572929572791,-31.6399109089102,55.2952676489055));
#112905=CARTESIAN_POINT('Ctrl Pts',(2.1526398152762,-31.6256540345434,55.3668884381332));
#112906=CARTESIAN_POINT('Ctrl Pts',(2.14997937236171,-31.6157774278917,
55.408193395815));
#112907=CARTESIAN_POINT('Ctrl Pts',(2.14277554881109,-31.5844576153759,
55.520083496558));
#112908=CARTESIAN_POINT('Ctrl Pts',(2.13829996551363,-31.5598897025359,
55.5896925150088));
#112909=CARTESIAN_POINT('Ctrl Pts',(2.13295527386606,-31.5254128186204,
55.6699682736316));
#112910=CARTESIAN_POINT('Ctrl Pts',(2.13212035963713,-31.5198809678143,
55.6824247892904));
#112911=CARTESIAN_POINT('Ctrl Pts',(2.12675007713731,-31.4834142531925,
55.7618963491714));
#112912=CARTESIAN_POINT('Ctrl Pts',(2.12216235501318,-31.4482111809464,
55.8268527713405));
#112913=CARTESIAN_POINT('Ctrl Pts',(2.11654027588311,-31.4022709623842,
55.8996348563199));
#112914=CARTESIAN_POINT('Ctrl Pts',(2.11573202235905,-31.395603561099,55.9099436274539));
#112915=CARTESIAN_POINT('Ctrl Pts',(2.11445506685338,-31.3849851264321,
55.9259700232764));
#112916=CARTESIAN_POINT('Ctrl Pts',(2.11399124124554,-31.3811110526101,
55.9317384506558));
#112917=CARTESIAN_POINT('Ctrl Pts',(2.11311885789158,-31.3737954245023,
55.9424854168378));
#112918=CARTESIAN_POINT('Ctrl Pts',(2.11271087473568,-31.3703626813043,
55.9474696545795));
#112919=CARTESIAN_POINT('Ctrl Pts',(2.11174491645276,-31.3622073660227,
55.9591738907788));
#112920=CARTESIAN_POINT('Ctrl Pts',(2.11118545769657,-31.3574621719033,
55.9658777901899));
#112921=CARTESIAN_POINT('Ctrl Pts',(2.10930165882308,-31.3414052657541,
55.988210569702));
#112922=CARTESIAN_POINT('Ctrl Pts',(2.10796378534965,-31.3298721402424,
56.0036773527398));
#112923=CARTESIAN_POINT('Ctrl Pts',(2.10463352754408,-31.3007896000602,
56.0412977703782));
#112924=CARTESIAN_POINT('Ctrl Pts',(2.1026265789964,-31.2829403714896,56.063211386878));
#112925=CARTESIAN_POINT('Ctrl Pts',(2.09343372188809,-31.1994108899654,
56.1605937453689));
#112926=CARTESIAN_POINT('Ctrl Pts',(2.08607577300004,-31.1275715857393,
56.2305068409151));
#112927=CARTESIAN_POINT('Ctrl Pts',(2.07289754164681,-30.9856695232517,
56.3456795436961));
#112928=CARTESIAN_POINT('Ctrl Pts',(2.06704680935116,-30.9176452464735,
56.3929568406548));
#112929=CARTESIAN_POINT('Ctrl Pts',(2.06004283481689,-30.8294914373563,
56.4449513482183));
#112930=CARTESIAN_POINT('Ctrl Pts',(2.05871167716821,-30.812427847237,56.4546138640165));
#112931=CARTESIAN_POINT('Ctrl Pts',(2.05659501942459,-30.7848064540562,
56.4696171770011));
#112932=CARTESIAN_POINT('Ctrl Pts',(2.05580274011233,-30.7743558871533,
56.4751504295406));
#112933=CARTESIAN_POINT('Ctrl Pts',(2.05429856561854,-30.7543053576852,
56.4854947675108));
#112934=CARTESIAN_POINT('Ctrl Pts',(2.0535860185813,-30.7447161082256,56.4903252008502));
#112935=CARTESIAN_POINT('Ctrl Pts',(2.05195360872115,-30.7225422267729,
56.5012274800501));
#112936=CARTESIAN_POINT('Ctrl Pts',(2.05103603236773,-30.7099264563181,
56.5072344418335));
#112937=CARTESIAN_POINT('Ctrl Pts',(2.04812749185214,-30.6694691962174,
56.5258773621193));
#112938=CARTESIAN_POINT('Ctrl Pts',(2.04615714629515,-30.6413538804128,
56.5379064070614));
#112939=CARTESIAN_POINT('Ctrl Pts',(2.04150358224,-30.5734432120206,56.5647752005727));
#112940=CARTESIAN_POINT('Ctrl Pts',(2.0388428701114,-30.5333800312772,56.5788808273197));
#112941=CARTESIAN_POINT('Ctrl Pts',(2.03163889322003,-30.4223862329931,
56.6132521263377));
#112942=CARTESIAN_POINT('Ctrl Pts',(2.0271634087151,-30.3505811790887,56.6303636887563));
#112943=CARTESIAN_POINT('Ctrl Pts',(2.02181723499935,-30.2644150546329,
56.6449398570226));
#112944=CARTESIAN_POINT('Ctrl Pts',(2.02098074667628,-30.2509241126987,
56.6470517716352));
#112945=CARTESIAN_POINT('Ctrl Pts',(2.0156107855745,-30.1643838527792,56.6595111123436));
#112946=CARTESIAN_POINT('Ctrl Pts',(2.0110249452427,-30.0907500079712,56.6651609107663));
#112947=CARTESIAN_POINT('Ctrl Pts',(2.00540495613297,-30.0047183005893,
56.666038553412));
#112948=CARTESIAN_POINT('Ctrl Pts',(2.00459671004535,-29.9924414094366,
56.666028081927));
#112949=CARTESIAN_POINT('Ctrl Pts',(2.00331976367859,-29.9732180186805,
56.6657992104633));
#112950=CARTESIAN_POINT('Ctrl Pts',(2.00285593965653,-29.9662705776211,
56.6656730188718));
#112951=CARTESIAN_POINT('Ctrl Pts',(2.00198355701048,-29.9532738610787,
56.6653556068995));
#112952=CARTESIAN_POINT('Ctrl Pts',(2.00157557295156,-29.9472245764896,
56.6651748795512));
#112953=CARTESIAN_POINT('Ctrl Pts',(2.00060960959139,-29.9329681142962,
56.6646711951904));
#112954=CARTESIAN_POINT('Ctrl Pts',(2.00005014662097,-29.924762192847,56.6643205001155));
#112955=CARTESIAN_POINT('Ctrl Pts',(1.99816632100341,-29.8972903773353,
56.6629428622291));
#112956=CARTESIAN_POINT('Ctrl Pts',(1.99682842453156,-29.878040582076,56.6616419742938));
#112957=CARTESIAN_POINT('Ctrl Pts',(1.99349809715418,-29.8306597380197,
56.6576123016473));
#112958=CARTESIAN_POINT('Ctrl Pts',(1.99149110134063,-29.8025677331954,
56.6545014314531));
#112959=CARTESIAN_POINT('Ctrl Pts',(1.9822978236645,-29.6754434739068,56.6371403166034));
#112960=CARTESIAN_POINT('Ctrl Pts',(1.97493949047844,-29.577738480749,56.6147015224257));
#112961=CARTESIAN_POINT('Ctrl Pts',(1.96175688810711,-29.4039568504639,
56.5579280046778));
#112962=CARTESIAN_POINT('Ctrl Pts',(1.95590231956057,-29.327293171844,56.5263932489599));
#112963=CARTESIAN_POINT('Ctrl Pts',(1.94889711022973,-29.2357832756456,
56.4805107078214));
#112964=CARTESIAN_POINT('Ctrl Pts',(1.947568230824,-29.2184405232332,56.4714292367417));
#112965=CARTESIAN_POINT('Ctrl Pts',(1.94545430454428,-29.1908904451282,
56.4563781723088));
#112966=CARTESIAN_POINT('Ctrl Pts',(1.9446625095041,-29.1805800547817,56.4506021571734));
#112967=CARTESIAN_POINT('Ctrl Pts',(1.9431587085359,-29.1610195756471,56.4393690156069));
#112968=CARTESIAN_POINT('Ctrl Pts',(1.94244605645959,-29.1517591318772,
56.4339312237316));
#112969=CARTESIAN_POINT('Ctrl Pts',(1.94081263598737,-29.1305603358802,
56.4212059240331));
#112970=CARTESIAN_POINT('Ctrl Pts',(1.93989416397002,-29.1186597745658,
56.4138567943191));
#112971=CARTESIAN_POINT('Ctrl Pts',(1.93697954947175,-29.0809763893301,
56.389924910659));
#112972=CARTESIAN_POINT('Ctrl Pts',(1.93500415124032,-29.055557208528,56.3727795369857));
#112973=CARTESIAN_POINT('Ctrl Pts',(1.93033607971217,-28.9959698514808,
56.3301485203659));
#112974=CARTESIAN_POINT('Ctrl Pts',(1.92766611300871,-28.962277761855,56.3040339581454));
#112975=CARTESIAN_POINT('Ctrl Pts',(1.92045757524315,-28.8731696716777,
56.229323608626));
#112976=CARTESIAN_POINT('Ctrl Pts',(1.91598616736384,-28.8199174860712,
56.1782990893257));
#112977=CARTESIAN_POINT('Ctrl Pts',(1.91060735737232,-28.7606049003929,
56.1133996617428));
#112978=CARTESIAN_POINT('Ctrl Pts',(1.90973439785307,-28.7511279748243,
56.1027591205603));
#112979=CARTESIAN_POINT('Ctrl Pts',(1.90437535863507,-28.6939532131089,
56.036881802974));
#112980=CARTESIAN_POINT('Ctrl Pts',(1.89983659378609,-28.6497967557562,
55.9786882018082));
#112981=CARTESIAN_POINT('Ctrl Pts',(1.8942688632865,-28.6028406309548,55.9075529447326));
#112982=CARTESIAN_POINT('Ctrl Pts',(1.89346081078101,-28.5961925808969,
55.897235397393));
#112983=CARTESIAN_POINT('Ctrl Pts',(1.8921841044149,-28.5859608110775,55.8809639305689));
#112984=CARTESIAN_POINT('Ctrl Pts',(1.89172032384338,-28.5822991612967,
55.8750591993351));
#112985=CARTESIAN_POINT('Ctrl Pts',(1.89084797465748,-28.5755171882501,
55.8639683733889));
#112986=CARTESIAN_POINT('Ctrl Pts',(1.89043998005691,-28.5723880528177,
55.8587879568165));
#112987=CARTESIAN_POINT('Ctrl Pts',(1.88947392559671,-28.5650783935967,
55.8465361566159));
#112988=CARTESIAN_POINT('Ctrl Pts',(1.88891438121063,-28.5609218685731,
55.8394507761383));
#112989=CARTESIAN_POINT('Ctrl Pts',(1.88702998383444,-28.5471755609521,
55.8156161179621));
#112990=CARTESIAN_POINT('Ctrl Pts',(1.88569158620767,-28.5378248627358,
55.7987316765901));
#112991=CARTESIAN_POINT('Ctrl Pts',(1.88235973073603,-28.5155034379875,
55.7567201798113));
#112992=CARTESIAN_POINT('Ctrl Pts',(1.88035169195056,-28.5028753255672,
55.7314184861613));
#112993=CARTESIAN_POINT('Ctrl Pts',(1.87494997068406,-28.4709372529807,
55.6631311780316));
#112994=CARTESIAN_POINT('Ctrl Pts',(1.87153014927533,-28.4528121848193,
55.619660056186));
#112995=CARTESIAN_POINT('Ctrl Pts',(1.86810673741825,-28.4365624617974,
55.5755163456748));
#112996=CARTESIAN_POINT('Origin',(5.,-30.,55.));
#112997=CARTESIAN_POINT('',(1.16624546596858,-28.4365623102019,55.575515933853));
#112998=CARTESIAN_POINT('',(1.36116732170967,-28.4365623080758,55.5755159280775));
#112999=CARTESIAN_POINT('',(5.,-28.4365623102018,55.5755159338528));
#113000=CARTESIAN_POINT('Ctrl Pts',(1.36116732170967,-28.4365623080758,
55.5755159280775));
#113001=CARTESIAN_POINT('Ctrl Pts',(1.36158377376753,-28.4385480585766,
55.5809103872544));
#113002=CARTESIAN_POINT('Ctrl Pts',(1.36199991354639,-28.4405618822783,
55.5862949867732));
#113003=CARTESIAN_POINT('Ctrl Pts',(1.36679795800594,-28.4641243692031,
55.6483163168118));
#113004=CARTESIAN_POINT('Ctrl Pts',(1.37113052084416,-28.4887212500842,
55.7037512298974));
#113005=CARTESIAN_POINT('Ctrl Pts',(1.37811663022607,-28.5341033774531,
55.7926144392078));
#113006=CARTESIAN_POINT('Ctrl Pts',(1.38082054814088,-28.5531462531665,
55.8268647007203));
#113007=CARTESIAN_POINT('Ctrl Pts',(1.38452366318565,-28.5812986814334,
55.8735431494178));
#113008=CARTESIAN_POINT('Ctrl Pts',(1.38555860306899,-28.5893979635029,
55.886562455289));
#113009=CARTESIAN_POINT('Ctrl Pts',(1.38732161837705,-28.6035899400703,
55.9086885762336));
#113010=CARTESIAN_POINT('Ctrl Pts',(1.3880528760382,-28.6095947284154,55.9178503007989));
#113011=CARTESIAN_POINT('Ctrl Pts',(1.38944448722421,-28.6212468563099,
55.9352515864444));
#113012=CARTESIAN_POINT('Ctrl Pts',(1.39010537741692,-28.6268787693484,
55.9435008502789));
#113013=CARTESIAN_POINT('Ctrl Pts',(1.39165339328923,-28.6402996604933,
55.9627841850654));
#113014=CARTESIAN_POINT('Ctrl Pts',(1.39253817562486,-28.6481493740455,
55.9737752836327));
#113015=CARTESIAN_POINT('Ctrl Pts',(1.3956428073009,-28.6763152921145,56.0122158522167));
#113016=CARTESIAN_POINT('Ctrl Pts',(1.39783537785293,-28.6973416669029,
56.0391360159408));
#113017=CARTESIAN_POINT('Ctrl Pts',(1.40782879589833,-28.7981005882645,
56.1602687109848));
#113018=CARTESIAN_POINT('Ctrl Pts',(1.41524524747757,-28.8873147448464,
56.2460813457704));
#113019=CARTESIAN_POINT('Ctrl Pts',(1.42593905146676,-29.025414153285,56.3521504015004));
#113020=CARTESIAN_POINT('Ctrl Pts',(1.42908047856126,-29.0670239356125,
56.3811890635867));
#113021=CARTESIAN_POINT('Ctrl Pts',(1.43413817753778,-29.134254715251,56.4236825118854));
#113022=CARTESIAN_POINT('Ctrl Pts',(1.43599727016874,-29.1590132576931,
56.4384463340088));
#113023=CARTESIAN_POINT('Ctrl Pts',(1.43852209839875,-29.1924695345722,
56.4572377318534));
#113024=CARTESIAN_POINT('Ctrl Pts',(1.43915470291399,-29.2008384826829,
56.4618440813738));
#113025=CARTESIAN_POINT('Ctrl Pts',(1.44021111351293,-29.2147812443813,
56.4693628039732));
#113026=CARTESIAN_POINT('Ctrl Pts',(1.44063239791733,-29.2203329214534,
56.472316130487));
#113027=CARTESIAN_POINT('Ctrl Pts',(1.44143674182715,-29.2309130587344,
56.4778678266063));
#113028=CARTESIAN_POINT('Ctrl Pts',(1.44181940019445,-29.2359382891956,
56.4804721327332));
#113029=CARTESIAN_POINT('Ctrl Pts',(1.44285024496362,-29.2494565464955,
56.4873907589411));
#113030=CARTESIAN_POINT('Ctrl Pts',(1.44350123900518,-29.2579733145221,
56.491657847043));
#113031=CARTESIAN_POINT('Ctrl Pts',(1.44597108186289,-29.2902267666097,
56.5074729660901));
#113032=CARTESIAN_POINT('Ctrl Pts',(1.44781584560412,-29.3141988886506,
56.5185287072503));
#113033=CARTESIAN_POINT('Ctrl Pts',(1.45686863883772,-29.4317108359299,
56.5693742619728));
#113034=CARTESIAN_POINT('Ctrl Pts',(1.46433887448437,-29.528493799993,56.6011148018832));
#113035=CARTESIAN_POINT('Ctrl Pts',(1.47864601908454,-29.7208336424597,
56.6452293062189));
#113036=CARTESIAN_POINT('Ctrl Pts',(1.48546807433489,-29.81578817088,56.658549001633));
#113037=CARTESIAN_POINT('Ctrl Pts',(1.49351610959751,-29.9328893440817,
56.6647871745137));
#113038=CARTESIAN_POINT('Ctrl Pts',(1.49498194168079,-29.9544246297646,
56.6655158773369));
#113039=CARTESIAN_POINT('Ctrl Pts',(1.49725990951138,-29.9882037641785,
56.6660031728523));
#113040=CARTESIAN_POINT('Ctrl Pts',(1.49808075620676,-30.0004404784882,
56.666044880234));
#113041=CARTESIAN_POINT('Ctrl Pts',(1.49960948678899,-30.023346292887,56.6658705815975));
#113042=CARTESIAN_POINT('Ctrl Pts',(1.5003183405736,-30.0340149354649,56.6656868965212));
#113043=CARTESIAN_POINT('Ctrl Pts',(1.50190320405074,-30.0579697901595,
56.6650442080287));
#113044=CARTESIAN_POINT('Ctrl Pts',(1.50277740667697,-30.0712538532933,
56.6645286470046));
#113045=CARTESIAN_POINT('Ctrl Pts',(1.50501327182793,-30.1053975453121,
56.6627940066699));
#113046=CARTESIAN_POINT('Ctrl Pts',(1.50636767301957,-30.1262433519794,
56.661341394616));
#113047=CARTESIAN_POINT('Ctrl Pts',(1.51738141038033,-30.296878431497,56.6462204887977));
#113048=CARTESIAN_POINT('Ctrl Pts',(1.52635033113338,-30.4442044229351,
56.6127190239061));
#113049=CARTESIAN_POINT('Ctrl Pts',(1.53935047374397,-30.6416530600251,
56.538666105376));
#113050=CARTESIAN_POINT('Ctrl Pts',(1.54312811204966,-30.69706373042,56.5143687270485));
#113051=CARTESIAN_POINT('Ctrl Pts',(1.5480401612387,-30.7645766858779,56.4802732766343));
#113052=CARTESIAN_POINT('Ctrl Pts',(1.54903529964396,-30.7780334669659,
56.4732448427409));
#113053=CARTESIAN_POINT('Ctrl Pts',(1.5505364217496,-30.7979677990191,56.4624839274267));
#113054=CARTESIAN_POINT('Ctrl Pts',(1.55103421669152,-30.8045197453253,
56.458889927402));
#113055=CARTESIAN_POINT('Ctrl Pts',(1.55193689319192,-30.8162902601501,
56.4523299350908));
#113056=CARTESIAN_POINT('Ctrl Pts',(1.55234079135825,-30.8215172802137,
56.4493796550496));
#113057=CARTESIAN_POINT('Ctrl Pts',(1.5532546393959,-30.8332545330335,56.4426709221335));
#113058=CARTESIAN_POINT('Ctrl Pts',(1.5537655575938,-30.8397552866358,56.4388966465526));
#113059=CARTESIAN_POINT('Ctrl Pts',(1.55533170968354,-30.8595029812325,
56.4272519227815));
#113060=CARTESIAN_POINT('Ctrl Pts',(1.5563951593331,-30.8726660450193,56.4192418248951));
#113061=CARTESIAN_POINT('Ctrl Pts',(1.56484260049718,-30.975447404128,56.3547260380023));
#113062=CARTESIAN_POINT('Ctrl Pts',(1.57261173086794,-31.0595945916183,
56.2899752531431));
#113063=CARTESIAN_POINT('Ctrl Pts',(1.58824998057803,-31.2168488490078,
56.143138002274));
#113064=CARTESIAN_POINT('Ctrl Pts',(1.59607195954014,-31.2891686879162,
56.0609136030713));
#113065=CARTESIAN_POINT('Ctrl Pts',(1.60496450033353,-31.3648933195608,
55.9555327181075));
#113066=CARTESIAN_POINT('Ctrl Pts',(1.60635818377756,-31.3765521821325,
55.9386589924853));
#113067=CARTESIAN_POINT('Ctrl Pts',(1.60854991746957,-31.3945448132776,
55.9115619512726));
#113068=CARTESIAN_POINT('Ctrl Pts',(1.60935561873642,-31.4010842605642,
55.9014784163549));
#113069=CARTESIAN_POINT('Ctrl Pts',(1.6108709861859,-31.4132387076742,55.8822850121191));
#113070=CARTESIAN_POINT('Ctrl Pts',(1.61158145570637,-31.4188761307601,
55.8731901408965));
#113071=CARTESIAN_POINT('Ctrl Pts',(1.61318963616946,-31.4314941809594,
55.852388505316));
#113072=CARTESIAN_POINT('Ctrl Pts',(1.61408530408609,-31.4384196131465,
55.8406490284063));
#113073=CARTESIAN_POINT('Ctrl Pts',(1.6164167855927,-31.4561698107631,55.8096984972154));
#113074=CARTESIAN_POINT('Ctrl Pts',(1.61784422097093,-31.4667588284361,
55.7903548481227));
#113075=CARTESIAN_POINT('Ctrl Pts',(1.62641717429374,-31.5285556132645,
55.6719444359103));
#113076=CARTESIAN_POINT('Ctrl Pts',(1.63321815399214,-31.5700957679772,
55.5681499806008));
#113077=CARTESIAN_POINT('Ctrl Pts',(1.64434109877295,-31.6204936921444,
55.3931185874683));
#113078=CARTESIAN_POINT('Ctrl Pts',(1.64865250916417,-31.6356965734774,
55.3240946915944));
#113079=CARTESIAN_POINT('Ctrl Pts',(1.65460713659497,-31.6500970577635,
55.2308656271097));
#113080=CARTESIAN_POINT('Ctrl Pts',(1.65612113009439,-31.6532181480619,
55.2073375929617));
#113081=CARTESIAN_POINT('Ctrl Pts',(1.65875532433683,-31.6577067397094,
55.1668898026132));
#113082=CARTESIAN_POINT('Ctrl Pts',(1.65986459893477,-31.6593202220615,
55.1500006248846));
#113083=CARTESIAN_POINT('Ctrl Pts',(1.66150401994203,-31.661299293818,55.1253061928711));
#113084=CARTESIAN_POINT('Ctrl Pts',(1.66202361951538,-31.6618683953676,
55.1175177264249));
#113085=CARTESIAN_POINT('Ctrl Pts',(1.66291046489379,-31.6627411269317,
55.1042955431842));
#113086=CARTESIAN_POINT('Ctrl Pts',(1.66327614922529,-31.6630729238847,
55.0988638669398));
#113087=CARTESIAN_POINT('Ctrl Pts',(1.66411376151794,-31.6637690586954,
55.0864703220316));
#113088=CARTESIAN_POINT('Ctrl Pts',(1.66458659609144,-31.6641163084086,
55.0795078921204));
#113089=CARTESIAN_POINT('Ctrl Pts',(1.66590489407934,-31.6649585498489,
55.0601837556508));
#113090=CARTESIAN_POINT('Ctrl Pts',(1.66675519481662,-31.6653595428168,
55.0478186962362));
#113091=CARTESIAN_POINT('Ctrl Pts',(1.67329071850763,-31.6673681631933,
54.9534454968093));
#113092=CARTESIAN_POINT('Ctrl Pts',(1.67922873497755,-31.6630547889557,
54.8714319950975));
#113093=CARTESIAN_POINT('Ctrl Pts',(1.68952751499371,-31.645217831155,54.7309999733622));
#113094=CARTESIAN_POINT('Ctrl Pts',(1.69386917297553,-31.634551075954,54.6723630773916));
#113095=CARTESIAN_POINT('Ctrl Pts',(1.70203870642488,-31.6083004137768,
54.5620191174013));
#113096=CARTESIAN_POINT('Ctrl Pts',(1.70587163033355,-31.5932988559749,
54.5102478536596));
#113097=CARTESIAN_POINT('Ctrl Pts',(1.71135976433464,-31.5677848162377,
54.4358911910482));
#113098=CARTESIAN_POINT('Ctrl Pts',(1.71307124944709,-31.5592353788256,
54.4126729003733));
#113099=CARTESIAN_POINT('Ctrl Pts',(1.7161581454993,-31.542727846442,54.3707467680355));
#113100=CARTESIAN_POINT('Ctrl Pts',(1.71753870266278,-31.5349385846823,
54.3519780537993));
#113101=CARTESIAN_POINT('Ctrl Pts',(1.71971472260656,-31.5220147298226,
54.3223786968741));
#113102=CARTESIAN_POINT('Ctrl Pts',(1.7205176495593,-31.5171034984931,54.3114533740682));
#113103=CARTESIAN_POINT('Ctrl Pts',(1.72203068432302,-31.5075796754232,
54.2908637887608));
#113104=CARTESIAN_POINT('Ctrl Pts',(1.72274156417849,-31.5029909297819,
54.2811892335459));
#113105=CARTESIAN_POINT('Ctrl Pts',(1.72435458142107,-31.4923199847364,
54.2592404646978));
#113106=CARTESIAN_POINT('Ctrl Pts',(1.7252546276115,-31.4861789862258,54.2469955740609));
#113107=CARTESIAN_POINT('Ctrl Pts',(1.72804513691277,-31.4665624730002,
54.2090561119216));
#113108=CARTESIAN_POINT('Ctrl Pts',(1.72991734886921,-31.452565930064,54.1836360480317));
#113109=CARTESIAN_POINT('Ctrl Pts',(1.74004413338332,-31.3724407003726,
54.0467070077865));
#113110=CARTESIAN_POINT('Ctrl Pts',(1.74783797284851,-31.2941362849517,
53.9428460046709));
#113111=CARTESIAN_POINT('Ctrl Pts',(1.75900569603257,-31.1684067593939,
53.8112514110225));
#113112=CARTESIAN_POINT('Ctrl Pts',(1.762244451456,-31.1304737551301,53.7751220930884));
#113113=CARTESIAN_POINT('Ctrl Pts',(1.7674401334203,-31.0686766339808,53.7215825064583));
#113114=CARTESIAN_POINT('Ctrl Pts',(1.76933604140751,-31.045942990068,53.702917100652));
#113115=CARTESIAN_POINT('Ctrl Pts',(1.7719035484822,-31.0151338353942,53.6789580366621));
#113116=CARTESIAN_POINT('Ctrl Pts',(1.77254058547048,-31.0074878766252,
53.673117661519));
#113117=CARTESIAN_POINT('Ctrl Pts',(1.77360239123595,-30.9947504309796,
53.6635617099247));
#113118=CARTESIAN_POINT('Ctrl Pts',(1.77402458427284,-30.9896875355378,
53.6598081098155));
#113119=CARTESIAN_POINT('Ctrl Pts',(1.7748810234561,-30.9794239757351,53.6522886422584));
#113120=CARTESIAN_POINT('Ctrl Pts',(1.77531532900213,-30.9742226225317,
53.6485239527666));
#113121=CARTESIAN_POINT('Ctrl Pts',(1.77644280925468,-30.9607249784893,
53.6388728957903));
#113122=CARTESIAN_POINT('Ctrl Pts',(1.7771389361446,-30.9523964487101,53.6330323816554));
#113123=CARTESIAN_POINT('Ctrl Pts',(1.78001289075266,-30.9180127465532,
53.6093870127789));
#113124=CARTESIAN_POINT('Ctrl Pts',(1.78222819415428,-30.8915093582224,
53.5922490831907));
#113125=CARTESIAN_POINT('Ctrl Pts',(1.79220598298561,-30.7715131215519,
53.5194034597294));
#113126=CARTESIAN_POINT('Ctrl Pts',(1.80022484751124,-30.6731817972066,
53.4721830317116));
#113127=CARTESIAN_POINT('Ctrl Pts',(1.81221881958467,-30.5170898176883,
53.4152410410755));
#113128=CARTESIAN_POINT('Ctrl Pts',(1.81630861242007,-30.4622483300041,
53.3983850611159));
#113129=CARTESIAN_POINT('Ctrl Pts',(1.82295747958886,-30.3700317537936,
53.3751745533046));
#113130=CARTESIAN_POINT('Ctrl Pts',(1.8255607791396,-30.333116416724,53.367206357309));
#113131=CARTESIAN_POINT('Ctrl Pts',(1.82915186403274,-30.2810740499241,
53.3578117721664));
#113132=CARTESIAN_POINT('Ctrl Pts',(1.83017257370876,-30.2661522825533,
53.3553274532956));
#113133=CARTESIAN_POINT('Ctrl Pts',(1.8319189010864,-30.2404059490489,53.3514005445967));
#113134=CARTESIAN_POINT('Ctrl Pts',(1.83264754870688,-30.2295974517406,
53.3498605499463));
#113135=CARTESIAN_POINT('Ctrl Pts',(1.8340392244325,-30.2088310859813,53.3471097491684));
#113136=CARTESIAN_POINT('Ctrl Pts',(1.83470274295007,-30.1988759289686,
53.3458824176942));
#113137=CARTESIAN_POINT('Ctrl Pts',(1.83643933543539,-30.1726833119128,
53.3428931198305));
#113138=CARTESIAN_POINT('Ctrl Pts',(1.83750771980573,-30.1564297106569,
53.3412798562905));
#113139=CARTESIAN_POINT('Ctrl Pts',(1.84136744435496,-30.0972416953909,
53.3362828696846));
#113140=CARTESIAN_POINT('Ctrl Pts',(1.84411471653995,-30.0542020692733,
53.3343249844645));
#113141=CARTESIAN_POINT('Ctrl Pts',(1.8540445815078,-29.8963276800815,53.3332700731374));
#113142=CARTESIAN_POINT('Ctrl Pts',(1.8609433174609,-29.7817540046521,53.3443714336091));
#113143=CARTESIAN_POINT('Ctrl Pts',(1.87097680323465,-29.6218425238484,
53.3767653787616));
#113144=CARTESIAN_POINT('Ctrl Pts',(1.87397762291709,-29.5748986522819,
53.3884225391352));
#113145=CARTESIAN_POINT('Ctrl Pts',(1.87883478097776,-29.501721712393,53.4100138071475));
#113146=CARTESIAN_POINT('Ctrl Pts',(1.88063928356007,-29.4751169833749,
53.418597158505));
#113147=CARTESIAN_POINT('Ctrl Pts',(1.88310071464198,-29.4398260357812,
53.4309715073326));
#113148=CARTESIAN_POINT('Ctrl Pts',(1.88372657702852,-29.4309364430022,
53.4341737201425));
#113149=CARTESIAN_POINT('Ctrl Pts',(1.88477479559862,-29.4161970469491,
53.4396252416666));
#113150=CARTESIAN_POINT('Ctrl Pts',(1.88519471164361,-29.4103316638861,
53.4418323178598));
#113151=CARTESIAN_POINT('Ctrl Pts',(1.88599904600432,-29.3991746295811,
53.4461025993532));
#113152=CARTESIAN_POINT('Ctrl Pts',(1.88638308493371,-29.3938808279137,
53.4481598651098));
#113153=CARTESIAN_POINT('Ctrl Pts',(1.88742247861135,-29.3796397709683,
53.4537781785265));
#113154=CARTESIAN_POINT('Ctrl Pts',(1.8880807219464,-29.3707128677528,53.4573897352087));
#113155=CARTESIAN_POINT('Ctrl Pts',(1.89061139769923,-29.3367229548156,
53.4714851566882));
#113156=CARTESIAN_POINT('Ctrl Pts',(1.8925113448145,-29.3118878457891,53.4825035335824));
#113157=CARTESIAN_POINT('Ctrl Pts',(1.90232689287817,-29.1865087707893,
53.5418399197771));
#113158=CARTESIAN_POINT('Ctrl Pts',(1.91054975613207,-29.0907330446859,
53.5995601913861));
#113159=CARTESIAN_POINT('Ctrl Pts',(1.92287923202993,-28.9541497866542,
53.7018303857256));
#113160=CARTESIAN_POINT('Ctrl Pts',(1.92709931101957,-28.9087678960131,
53.7397378488051));
#113161=CARTESIAN_POINT('Ctrl Pts',(1.93306883925825,-28.846292181743,53.7978345760744));
#113162=CARTESIAN_POINT('Ctrl Pts',(1.93488620282228,-28.8275151795685,
53.8161406703138));
#113163=CARTESIAN_POINT('Ctrl Pts',(1.93814323006128,-28.7943118953648,
53.8500765214844));
#113164=CARTESIAN_POINT('Ctrl Pts',(1.93958896378713,-28.7797381701592,
53.8655534603913));
#113165=CARTESIAN_POINT('Ctrl Pts',(1.94184293614615,-28.7572882929765,
53.8903280402484));
#113166=CARTESIAN_POINT('Ctrl Pts',(1.94265958481592,-28.7492115339136,
53.8994399281399));
#113167=CARTESIAN_POINT('Ctrl Pts',(1.94418451565449,-28.7342411759457,
53.9167066003439));
#113168=CARTESIAN_POINT('Ctrl Pts',(1.94489372217523,-28.7273247206171,
53.9248406477522));
#113169=CARTESIAN_POINT('Ctrl Pts',(1.94648457654274,-28.7119174661925,
53.9433172541798));
#113170=CARTESIAN_POINT('Ctrl Pts',(1.9473643560252,-28.7034720497542,53.9536968265269));
#113171=CARTESIAN_POINT('Ctrl Pts',(1.94962493590604,-28.6819764386631,
53.9807752986874));
#113172=CARTESIAN_POINT('Ctrl Pts',(1.95099819348587,-28.669117935779,53.9976237752586));
#113173=CARTESIAN_POINT('Ctrl Pts',(1.96048448451935,-28.581819184619,54.11665368373));
#113174=CARTESIAN_POINT('Ctrl Pts',(1.96813527651343,-28.5188990470452,
54.2267722058592));
#113175=CARTESIAN_POINT('Ctrl Pts',(1.9811030231244,-28.435283548501,54.4216031967692));
#113176=CARTESIAN_POINT('Ctrl Pts',(1.98636858792426,-28.4076456044622,
54.5027233223497));
#113177=CARTESIAN_POINT('Ctrl Pts',(1.99285439274383,-28.3828589393575,
54.5992391735961));
#113178=CARTESIAN_POINT('Ctrl Pts',(1.99377933897153,-28.3795281878337,
54.6129269787273));
#113179=CARTESIAN_POINT('Ctrl Pts',(1.99519486431358,-28.3747455891304,
54.6337258630041));
#113180=CARTESIAN_POINT('Ctrl Pts',(1.99567856583511,-28.3731658846417,
54.6408072945396));
#113181=CARTESIAN_POINT('Ctrl Pts',(1.99656783200992,-28.3703621506975,
54.6537737577348));
#113182=CARTESIAN_POINT('Ctrl Pts',(1.99697257868926,-28.3691236488181,
54.6596553891418));
#113183=CARTESIAN_POINT('Ctrl Pts',(1.99790425559076,-28.366358485514,54.6731488548685));
#113184=CARTESIAN_POINT('Ctrl Pts',(1.99843233794233,-28.3648531863368,
54.6807647252102));
#113185=CARTESIAN_POINT('Ctrl Pts',(2.00006589113265,-28.3603848585366,
54.7042327622797));
#113186=CARTESIAN_POINT('Ctrl Pts',(2.00118036224702,-28.3575988311037,
54.7201171251284));
#113187=CARTESIAN_POINT('Ctrl Pts',(2.00843431037383,-28.3411136633396,
54.8228495109306));
#113188=CARTESIAN_POINT('Ctrl Pts',(2.01483590118353,-28.3340785096767,
54.9106190072649));
#113189=CARTESIAN_POINT('Ctrl Pts',(2.02993613776549,-28.3338947857698,
55.1180568449114));
#113190=CARTESIAN_POINT('Ctrl Pts',(2.03856942696008,-28.3466535323101,
55.2372744075942));
#113191=CARTESIAN_POINT('Ctrl Pts',(2.04830033618961,-28.3766865549533,
55.3753416420334));
#113192=CARTESIAN_POINT('Ctrl Pts',(2.0497835389115,-28.3817187648502,55.3964767460031));
#113193=CARTESIAN_POINT('Ctrl Pts',(2.05216951937095,-28.3905550413753,
55.4306113334118));
#113194=CARTESIAN_POINT('Ctrl Pts',(2.0530802414723,-28.3941066103615,55.4436728921056));
#113195=CARTESIAN_POINT('Ctrl Pts',(2.05470106395927,-28.400747566364,55.4669710265837));
#113196=CARTESIAN_POINT('Ctrl Pts',(2.05541305864357,-28.4037770236732,
55.4772237474747));
#113197=CARTESIAN_POINT('Ctrl Pts',(2.05692245471112,-28.4104380414905,
55.498993577318));
#113198=CARTESIAN_POINT('Ctrl Pts',(2.05771893068484,-28.4140965693085,
55.5105018428584));
#113199=CARTESIAN_POINT('Ctrl Pts',(2.05975208248151,-28.4238030084701,
55.5399226223487));
#113200=CARTESIAN_POINT('Ctrl Pts',(2.06098279722393,-28.4300313320395,
55.557773979529));
#113201=CARTESIAN_POINT('Ctrl Pts',(2.06220428404731,-28.4365623101862,
55.5755159338105));
#113202=CARTESIAN_POINT('',(1.82701798699663,-28.334000473818,54.999675424517));
#113203=CARTESIAN_POINT('Ctrl Pts',(1.86810673741825,-28.4365624617974,
55.5755163456748));
#113204=CARTESIAN_POINT('Ctrl Pts',(1.86162183563071,-28.4057809308945,
55.4918957825778));
#113205=CARTESIAN_POINT('Ctrl Pts',(1.85513252908068,-28.3817289129791,
55.405861033452));
#113206=CARTESIAN_POINT('Ctrl Pts',(1.84519626206848,-28.3549112155355,
55.2680536719336));
#113207=CARTESIAN_POINT('Ctrl Pts',(1.84163835190104,-28.3474595851737,
55.2174419664774));
#113208=CARTESIAN_POINT('Ctrl Pts',(1.83699847475443,-28.3406553066266,
55.1497249555348));
#113209=CARTESIAN_POINT('Ctrl Pts',(1.83585277227586,-28.339220020485,55.1328618458178));
#113210=CARTESIAN_POINT('Ctrl Pts',(1.83394918425833,-28.3372487394932,
55.1046138034724));
#113211=CARTESIAN_POINT('Ctrl Pts',(1.83318696520669,-28.3365721954689,
55.0932402941342));
#113212=CARTESIAN_POINT('Ctrl Pts',(1.83175229460624,-28.3355134147814,
55.0717183369838));
#113213=CARTESIAN_POINT('Ctrl Pts',(1.83107912628968,-28.3351071949762,
55.0615716475465));
#113214=CARTESIAN_POINT('Ctrl Pts',(1.82982343023142,-28.3345200432967,
55.0425577109211));
#113215=CARTESIAN_POINT('Ctrl Pts',(1.82924024488316,-28.3343170982553,
55.0336915544102));
#113216=CARTESIAN_POINT('Ctrl Pts',(1.82810993935358,-28.3340600375524,
55.0164415288973));
#113217=CARTESIAN_POINT('Ctrl Pts',(1.82756260927594,-28.3339983934517,
55.0080580818904));
#113218=CARTESIAN_POINT('Ctrl Pts',(1.82701715464812,-28.3340000318124,
54.9996744250059));
#113219=CARTESIAN_POINT('Ctrl Pts',(1.82701722290713,-28.3340000316078,
54.9996754741491));
#113220=CARTESIAN_POINT('Ctrl Pts',(1.82545459593269,-28.3340047100833,
54.9756578493269));
#113221=CARTESIAN_POINT('Ctrl Pts',(1.82390764189692,-28.3345287558541,
54.9516419897929));
#113222=CARTESIAN_POINT('Ctrl Pts',(1.81315018159099,-28.3418484033513,
54.7832643812592));
#113223=CARTESIAN_POINT('Ctrl Pts',(1.80453968563037,-28.3668823381416,
54.6403221171576));
#113224=CARTESIAN_POINT('Ctrl Pts',(1.79300176085031,-28.4226849666057,
54.4620188620413));
#113225=CARTESIAN_POINT('Ctrl Pts',(1.79036101234513,-28.4368561165743,
54.4221357064352));
#113226=CARTESIAN_POINT('Ctrl Pts',(1.78602430489043,-28.4620122921717,
54.359059143433));
#113227=CARTESIAN_POINT('Ctrl Pts',(1.78436761316333,-28.4720419925298,
54.3355035531236));
#113228=CARTESIAN_POINT('Ctrl Pts',(1.78207864037288,-28.4863870643553,
54.303856628424));
#113229=CARTESIAN_POINT('Ctrl Pts',(1.78147216978569,-28.490232909638,54.2955548026208));
#113230=CARTESIAN_POINT('Ctrl Pts',(1.78044744986378,-28.4968017594048,
54.2816758642341));
#113231=CARTESIAN_POINT('Ctrl Pts',(1.78003141074779,-28.4994879777933,
54.2760813690753));
#113232=CARTESIAN_POINT('Ctrl Pts',(1.77922668688876,-28.5047191620114,
54.2653407773242));
#113233=CARTESIAN_POINT('Ctrl Pts',(1.77883831547864,-28.5072595651708,
54.2601926266778));
#113234=CARTESIAN_POINT('Ctrl Pts',(1.77777216609402,-28.5142776829682,
54.246153667092));
#113235=CARTESIAN_POINT('Ctrl Pts',(1.77709124111117,-28.5188084708371,
54.2372898724368));
#113236=CARTESIAN_POINT('Ctrl Pts',(1.77435944763071,-28.5371877492326,
54.2021150661963));
#113237=CARTESIAN_POINT('Ctrl Pts',(1.77227541512984,-28.5516592441943,
54.176137848277));
#113238=CARTESIAN_POINT('Ctrl Pts',(1.76236681954623,-28.6228628248663,
54.0560019743048));
#113239=CARTESIAN_POINT('Ctrl Pts',(1.75426551738015,-28.6881281584836,
53.9672217407039));
#113240=CARTESIAN_POINT('Ctrl Pts',(1.74213391251971,-28.8005049419681,
53.8423561157109));
#113241=CARTESIAN_POINT('Ctrl Pts',(1.73798949091869,-28.8415820610622,
53.8012520011758));
#113242=CARTESIAN_POINT('Ctrl Pts',(1.73211361606381,-28.9039918434947,
53.7450120573343));
#113243=CARTESIAN_POINT('Ctrl Pts',(1.73031659305481,-28.9236617508805,
53.7281019242605));
#113244=CARTESIAN_POINT('Ctrl Pts',(1.72749016375896,-28.9555309877658,
53.7019731222036));
#113245=CARTESIAN_POINT('Ctrl Pts',(1.72644902278615,-28.967475491935,53.692451736991));
#113246=CARTESIAN_POINT('Ctrl Pts',(1.72446900398966,-28.9905816965725,
53.6745470681092));
#113247=CARTESIAN_POINT('Ctrl Pts',(1.723529133526,-29.0017210593077,53.6661372022929));
#113248=CARTESIAN_POINT('Ctrl Pts',(1.72187605247386,-29.0216130206805,
53.6515081929718));
#113249=CARTESIAN_POINT('Ctrl Pts',(1.72116065031392,-29.0303223889424,
53.64523191106));
#113250=CARTESIAN_POINT('Ctrl Pts',(1.71966350028497,-29.0487577170484,
53.6322156166884));
#113251=CARTESIAN_POINT('Ctrl Pts',(1.71888248749652,-29.0584960754086,
53.6254941352461));
#113252=CARTESIAN_POINT('Ctrl Pts',(1.71681510708784,-29.0845901064971,
53.6078913120709));
#113253=CARTESIAN_POINT('Ctrl Pts',(1.71553566132635,-29.101068330534,53.5971943189823));
#113254=CARTESIAN_POINT('Ctrl Pts',(1.70892850342153,-29.1877984928466,
53.5430486125507));
#113255=CARTESIAN_POINT('Ctrl Pts',(1.70378418414734,-29.2610249375565,
53.5045746495378));
#113256=CARTESIAN_POINT('Ctrl Pts',(1.69256312457214,-29.4286294051293,
53.4318451480556));
#113257=CARTESIAN_POINT('Ctrl Pts',(1.68654448256831,-29.5238448176661,
53.4003600724119));
#113258=CARTESIAN_POINT('Ctrl Pts',(1.67849823295412,-29.6488286995577,
53.3711864298665));
#113259=CARTESIAN_POINT('Ctrl Pts',(1.67670630962728,-29.6765116430934,
53.3654633588148));
#113260=CARTESIAN_POINT('Ctrl Pts',(1.67364031922123,-29.7233143455223,
53.3570230171086));
#113261=CARTESIAN_POINT('Ctrl Pts',(1.6723825597674,-29.7423606414123,53.353928859136));
#113262=CARTESIAN_POINT('Ctrl Pts',(1.67056493028423,-29.7695846220246,
53.3499902358845));
#113263=CARTESIAN_POINT('Ctrl Pts',(1.67001909855973,-29.7777222584166,
53.3488743031841));
#113264=CARTESIAN_POINT('Ctrl Pts',(1.66906527695937,-29.7918696053892,
53.3470407240329));
#113265=CARTESIAN_POINT('Ctrl Pts',(1.66865881543818,-29.7978755138257,
53.3462955766185));
#113266=CARTESIAN_POINT('Ctrl Pts',(1.66778162367742,-29.8107857417327,
53.3447651989941));
#113267=CARTESIAN_POINT('Ctrl Pts',(1.66731036749063,-29.8176908487408,
53.3439904435792));
#113268=CARTESIAN_POINT('Ctrl Pts',(1.66600025365635,-29.8368083497858,
53.341966469347));
#113269=CARTESIAN_POINT('Ctrl Pts',(1.66515664924455,-29.8490297284857,
53.3408090349567));
#113270=CARTESIAN_POINT('Ctrl Pts',(1.6592169541169,-29.934537538994,53.3336634738373));
#113271=CARTESIAN_POINT('Ctrl Pts',(1.65391681879628,-30.0081299795949,
53.332398651033));
#113272=CARTESIAN_POINT('Ctrl Pts',(1.64756637559429,-30.0954316173639,
53.3366774825345));
#113273=CARTESIAN_POINT('Ctrl Pts',(1.6465556910797,-30.1092979591638,53.3375310699811));
#113274=CARTESIAN_POINT('Ctrl Pts',(1.64017849207702,-30.1966772738093,
53.344007932512));
#113275=CARTESIAN_POINT('Ctrl Pts',(1.63481225275999,-30.2697644061377,
53.3543329137724));
#113276=CARTESIAN_POINT('Ctrl Pts',(1.62652043124555,-30.3834887613324,
53.3781814539819));
#113277=CARTESIAN_POINT('Ctrl Pts',(1.62352679304667,-30.4247011320883,
53.3884825549899));
#113278=CARTESIAN_POINT('Ctrl Pts',(1.61845723681767,-30.4948365980091,
53.4088910587602));
#113279=CARTESIAN_POINT('Ctrl Pts',(1.61635987529078,-30.5239561804558,
53.4182411512532));
#113280=CARTESIAN_POINT('Ctrl Pts',(1.61334194993097,-30.5659846040451,
53.4330243583449));
#113281=CARTESIAN_POINT('Ctrl Pts',(1.6124009718399,-30.5791070675546,53.4378264313719));
#113282=CARTESIAN_POINT('Ctrl Pts',(1.61074663871965,-30.6022036257754,
53.446609491173));
#113283=CARTESIAN_POINT('Ctrl Pts',(1.61003108089109,-30.61220240098,53.4505228271049));
#113284=CARTESIAN_POINT('Ctrl Pts',(1.60853428473231,-30.6331316275402,
53.4589483607161));
#113285=CARTESIAN_POINT('Ctrl Pts',(1.60775377493972,-30.6440533139186,
53.463480831979));
#113286=CARTESIAN_POINT('Ctrl Pts',(1.6056893188338,-30.6729537060661,53.4758367181291));
#113287=CARTESIAN_POINT('Ctrl Pts',(1.60441225858804,-30.6908444744905,
53.483862023093));
#113288=CARTESIAN_POINT('Ctrl Pts',(1.59780144012474,-30.7834256033647,
53.5273705345931));
#113289=CARTESIAN_POINT('Ctrl Pts',(1.592651598315,-30.8555439458057,53.5680641524787));
#113290=CARTESIAN_POINT('Ctrl Pts',(1.58142600451561,-31.007609306604,53.669475746203));
#113291=CARTESIAN_POINT('Ctrl Pts',(1.57540813560007,-31.0856912252472,
53.732386680518));
#113292=CARTESIAN_POINT('Ctrl Pts',(1.56736281516442,-31.1779768935513,
53.8215581169088));
#113293=CARTESIAN_POINT('Ctrl Pts',(1.56557099432716,-31.197798120355,53.8417106076669));
#113294=CARTESIAN_POINT('Ctrl Pts',(1.56250516123563,-31.2302716121272,
53.8764520276478));
#113295=CARTESIAN_POINT('Ctrl Pts',(1.56124745438774,-31.2432006320562,
53.8907748666653));
#113296=CARTESIAN_POINT('Ctrl Pts',(1.55942988734562,-31.2612743516383,
53.9115100019598));
#113297=CARTESIAN_POINT('Ctrl Pts',(1.55888406410575,-31.2666253817316,
53.9177414351029));
#113298=CARTESIAN_POINT('Ctrl Pts',(1.55793025420933,-31.2758387673183,
53.9286326174512));
#113299=CARTESIAN_POINT('Ctrl Pts',(1.55752379583824,-31.2797221643495,
53.9332742576878));
#113300=CARTESIAN_POINT('Ctrl Pts',(1.55664661161026,-31.2880098899131,
53.9432905770505));
#113301=CARTESIAN_POINT('Ctrl Pts',(1.55617535981127,-31.2924058454848,
53.948671598777));
#113302=CARTESIAN_POINT('Ctrl Pts',(1.55486524594626,-31.3044749452165,
53.9636352851151));
#113303=CARTESIAN_POINT('Ctrl Pts',(1.55402163691192,-31.3120758486463,
53.9732752802004));
#113304=CARTESIAN_POINT('Ctrl Pts',(1.5480786297716,-31.3644848040678,54.0412763733764));
#113305=CARTESIAN_POINT('Ctrl Pts',(1.54277491849894,-31.40548547083,54.1024600486782));
#113306=CARTESIAN_POINT('Ctrl Pts',(1.53642362639942,-31.4492389004914,
54.1781395662555));
#113307=CARTESIAN_POINT('Ctrl Pts',(1.53541563133018,-31.4560236223852,
54.1902202948951));
#113308=CARTESIAN_POINT('Ctrl Pts',(1.52904087508932,-31.4979560207691,
54.2671153463555));
#113309=CARTESIAN_POINT('Ctrl Pts',(1.5236744067401,-31.5289213978872,54.3341225103229));
#113310=CARTESIAN_POINT('Ctrl Pts',(1.51538286771513,-31.5705614975592,
54.442599739866));
#113311=CARTESIAN_POINT('Ctrl Pts',(1.51238970901964,-31.5842563859728,
54.4828049963383));
#113312=CARTESIAN_POINT('Ctrl Pts',(1.50732087084965,-31.6051455920761,
54.552788265643));
#113313=CARTESIAN_POINT('Ctrl Pts',(1.50522375552059,-31.613082435228,54.5823207244749));
#113314=CARTESIAN_POINT('Ctrl Pts',(1.50220612315584,-31.6234559173839,
54.6256444245092));
#113315=CARTESIAN_POINT('Ctrl Pts',(1.50126519680947,-31.626538414856,54.6392729310961));
#113316=CARTESIAN_POINT('Ctrl Pts',(1.49961093247191,-31.6316858303462,
54.6634400120583));
#113317=CARTESIAN_POINT('Ctrl Pts',(1.49889539207807,-31.6338209569508,
54.6739626335194));
#113318=CARTESIAN_POINT('Ctrl Pts',(1.49739861112907,-31.6380934496863,
54.6961157064468));
#113319=CARTESIAN_POINT('Ctrl Pts',(1.49661809930098,-31.6402090236074,
54.7077497907877));
#113320=CARTESIAN_POINT('Ctrl Pts',(1.49455358906428,-31.6455028833275,
54.7387325252692));
#113321=CARTESIAN_POINT('Ctrl Pts',(1.49327647768644,-31.6484638307345,
54.7581167971921));
#113322=CARTESIAN_POINT('Ctrl Pts',(1.48666342347386,-31.6621272788716,
54.85953025339));
#113323=CARTESIAN_POINT('Ctrl Pts',(1.48151156671246,-31.6670523059732,
54.9422250182093));
#113324=CARTESIAN_POINT('Ctrl Pts',(1.47028582541274,-31.6643146832485,
55.1249884167226));
#113325=CARTESIAN_POINT('Ctrl Pts',(1.46426964397116,-31.6538084112718,
55.2246794791036));
#113326=CARTESIAN_POINT('Ctrl Pts',(1.45622635190676,-31.628948715306,55.3505434407319));
#113327=CARTESIAN_POINT('Ctrl Pts',(1.45443476177725,-31.6227685955833,
55.3781223692615));
#113328=CARTESIAN_POINT('Ctrl Pts',(1.45136928620479,-31.6111943438156,
55.4242416742124));
#113329=CARTESIAN_POINT('Ctrl Pts',(1.45011170165141,-31.6061737456621,
55.4428702209807));
#113330=CARTESIAN_POINT('Ctrl Pts',(1.44829428500646,-31.5985563452328,
55.4692984877839));
#113331=CARTESIAN_POINT('Ctrl Pts',(1.44774848710103,-31.5962233413036,
55.4771734456194));
#113332=CARTESIAN_POINT('Ctrl Pts',(1.44679470863462,-31.5920702998738,
55.4908205249506));
#113333=CARTESIAN_POINT('Ctrl Pts',(1.44638825612012,-31.590276884126,55.4966005013321));
#113334=CARTESIAN_POINT('Ctrl Pts',(1.44551106694425,-31.5863566544626,
55.5089959214516));
#113335=CARTESIAN_POINT('Ctrl Pts',(1.44503980417734,-31.5842199678471,
55.5156077698054));
#113336=CARTESIAN_POINT('Ctrl Pts',(1.44372963375321,-31.5781938671376,
55.533864063917));
#113337=CARTESIAN_POINT('Ctrl Pts',(1.4428859784995,-31.5742170946578,55.5454789068228));
#113338=CARTESIAN_POINT('Ctrl Pts',(1.43693167733926,-31.545456337168,55.6265448101438));
#113339=CARTESIAN_POINT('Ctrl Pts',(1.43161582018813,-31.5162159050044,
55.6943202488002));
#113340=CARTESIAN_POINT('Ctrl Pts',(1.42526178333954,-31.4763256382389,
55.7721444531892));
#113341=CARTESIAN_POINT('Ctrl Pts',(1.42426305371873,-31.4699132207546,
55.7842828359576));
#113342=CARTESIAN_POINT('Ctrl Pts',(1.41789691160616,-31.4281045777199,
55.8611101992064));
#113343=CARTESIAN_POINT('Ctrl Pts',(1.41252985279945,-31.3885940690259,
55.9234724087597));
#113344=CARTESIAN_POINT('Ctrl Pts',(1.40423951896968,-31.3200424791767,
56.0172729969052));
#113345=CARTESIAN_POINT('Ctrl Pts',(1.40124805728931,-31.2937042856933,
56.0505647139523));
#113346=CARTESIAN_POINT('Ctrl Pts',(1.39618173151308,-31.2462585178706,
56.1060423491436));
#113347=CARTESIAN_POINT('Ctrl Pts',(1.39408546079869,-31.2257590757972,
56.1287182430763));
#113348=CARTESIAN_POINT('Ctrl Pts',(1.39106879197606,-31.1949962423499,
56.1609199531276));
#113349=CARTESIAN_POINT('Ctrl Pts',(1.39012800336942,-31.185219404729,56.1708997139368));
#113350=CARTESIAN_POINT('Ctrl Pts',(1.38847388694842,-31.1677086170226,
56.1883298603443));
#113351=CARTESIAN_POINT('Ctrl Pts',(1.38775835822321,-31.1600261138563,
56.1958305463998));
#113352=CARTESIAN_POINT('Ctrl Pts',(1.38626150947457,-31.1437305898784,
56.2114355866072));
#113353=CARTESIAN_POINT('Ctrl Pts',(1.3854809190765,-31.1351026778822,56.2195235813728));
#113354=CARTESIAN_POINT('Ctrl Pts',(1.38341598425799,-31.1119387311018,
56.2407791504558));
#113355=CARTESIAN_POINT('Ctrl Pts',(1.38213853180769,-31.0972547860331,
56.253783326236));
#113356=CARTESIAN_POINT('Ctrl Pts',(1.37551361237887,-31.0193215770003,
56.3203832809695));
#113357=CARTESIAN_POINT('Ctrl Pts',(1.3703511082947,-30.9523631047568,56.3694654113419));
#113358=CARTESIAN_POINT('Ctrl Pts',(1.35912473791162,-30.7972790047845,
56.4662469516713));
#113359=CARTESIAN_POINT('Ctrl Pts',(1.35311761352187,-30.7079582197976,
56.511398940935));
#113360=CARTESIAN_POINT('Ctrl Pts',(1.34508522170745,-30.5888933548515,
56.5587039859287));
#113361=CARTESIAN_POINT('Ctrl Pts',(1.34329484229251,-30.562389398754,56.568461502123));
#113362=CARTESIAN_POINT('Ctrl Pts',(1.34023122512766,-30.5173927026961,
56.5837400752557));
#113363=CARTESIAN_POINT('Ctrl Pts',(1.33897426179721,-30.4990282418087,
56.589622147231));
#113364=CARTESIAN_POINT('Ctrl Pts',(1.33715758004984,-30.4727039996028,
56.5975526168379));
#113365=CARTESIAN_POINT('Ctrl Pts',(1.33661187967724,-30.4648239866077,
56.5998631470506));
#113366=CARTESIAN_POINT('Ctrl Pts',(1.33565819654879,-30.4511074010679,
56.6037751527371));
#113367=CARTESIAN_POINT('Ctrl Pts',(1.33525174054363,-30.4452786617929,
56.6054032327856));
#113368=CARTESIAN_POINT('Ctrl Pts',(1.33437444193052,-30.4327369789256,
56.6088328104112));
#113369=CARTESIAN_POINT('Ctrl Pts',(1.33390307222236,-30.4260216964146,
56.6106240450719));
#113370=CARTESIAN_POINT('Ctrl Pts',(1.33259240895874,-30.4074084651998,
56.6154643917785));
#113371=CARTESIAN_POINT('Ctrl Pts',(1.33174836305431,-30.395487982673,56.6184239531236));
#113372=CARTESIAN_POINT('Ctrl Pts',(1.32569201328955,-30.310347850174,56.6385653906965));
#113373=CARTESIAN_POINT('Ctrl Pts',(1.32026632864406,-30.2360787506473,
56.6509017665711));
#113374=CARTESIAN_POINT('Ctrl Pts',(1.31071174694016,-30.105230094,56.6636253733694));
#113375=CARTESIAN_POINT('Ctrl Pts',(1.30660505217434,-30.0489791341576,
56.6662304853437));
#113376=CARTESIAN_POINT('Ctrl Pts',(1.29818034983908,-29.9324625332999,
56.6657201918926));
#113377=CARTESIAN_POINT('Ctrl Pts',(1.293874257319,-29.8722753298122,56.6621891322544));
#113378=CARTESIAN_POINT('Ctrl Pts',(1.28692486917766,-29.7736355106187,
56.6510110881028));
#113379=CARTESIAN_POINT('Ctrl Pts',(1.28423188850251,-29.7350282983485,
56.645256493113));
#113380=CARTESIAN_POINT('Ctrl Pts',(1.28054109828775,-29.681604535636,56.6353637637584));
#113381=CARTESIAN_POINT('Ctrl Pts',(1.27950785663442,-29.6665918837104,
56.6323692494965));
#113382=CARTESIAN_POINT('Ctrl Pts',(1.2777469913615,-29.6409172469014,56.626879040463));
#113383=CARTESIAN_POINT('Ctrl Pts',(1.27701620246075,-29.6302349127606,
56.6244844185117));
#113384=CARTESIAN_POINT('Ctrl Pts',(1.27562499871827,-29.6098515305301,
56.6197036624504));
#113385=CARTESIAN_POINT('Ctrl Pts',(1.27496405197059,-29.6001468640776,
56.6173352340937));
#113386=CARTESIAN_POINT('Ctrl Pts',(1.27341518106666,-29.5773607253018,
56.6115566322762));
#113387=CARTESIAN_POINT('Ctrl Pts',(1.27252960892119,-29.5642981700632,
56.6080742111692));
#113388=CARTESIAN_POINT('Ctrl Pts',(1.26941814569736,-29.518301895172,56.5952101729372));
#113389=CARTESIAN_POINT('Ctrl Pts',(1.26721970094342,-29.4856152201851,
56.5849722758909));
#113390=CARTESIAN_POINT('Ctrl Pts',(1.25644329243025,-29.3251037661909,
56.529208605666));
#113391=CARTESIAN_POINT('Ctrl Pts',(1.248346180035,-29.2028665800843,56.4691978589594));
#113392=CARTESIAN_POINT('Ctrl Pts',(1.23734904010953,-29.0537438296414,
56.3718433069069));
#113393=CARTESIAN_POINT('Ctrl Pts',(1.23470237003611,-29.0191304515592,
56.3473118598639));
#113394=CARTESIAN_POINT('Ctrl Pts',(1.23035701783487,-28.9651548660094,
56.3058747946619));
#113395=CARTESIAN_POINT('Ctrl Pts',(1.22869779540035,-28.94518109911,56.2897946913068));
#113396=CARTESIAN_POINT('Ctrl Pts',(1.22640585725787,-28.9185909337418,
56.2673571883539));
#113397=CARTESIAN_POINT('Ctrl Pts',(1.22579903730385,-28.911643200382,56.2613957660774));
#113398=CARTESIAN_POINT('Ctrl Pts',(1.22477389829932,-28.9000679651241,
56.2512969456098));
#113399=CARTESIAN_POINT('Ctrl Pts',(1.22435779357978,-28.8954136839243,
56.2471902806685));
#113400=CARTESIAN_POINT('Ctrl Pts',(1.22349866152291,-28.8858970352757,
56.23869829113));
#113401=CARTESIAN_POINT('Ctrl Pts',(1.22305544590985,-28.8810374233475,
56.2343101801323));
#113402=CARTESIAN_POINT('Ctrl Pts',(1.22187836034643,-28.8682593442517,
56.2226344100305));
#113403=CARTESIAN_POINT('Ctrl Pts',(1.22114105218907,-28.860385560112,56.2152986158212));
#113404=CARTESIAN_POINT('Ctrl Pts',(1.21782200567632,-28.8254954723313,
56.1821552449488));
#113405=CARTESIAN_POINT('Ctrl Pts',(1.21518739896034,-28.7992827764792,
56.1555213468577));
#113406=CARTESIAN_POINT('Ctrl Pts',(1.20585345298221,-28.7108156574795,
56.0593701281318));
#113407=CARTESIAN_POINT('Ctrl Pts',(1.19900163014399,-28.6535225746133,
55.9855249726162));
#113408=CARTESIAN_POINT('Ctrl Pts',(1.18770474561607,-28.5685446476298,
55.8546509067454));
#113409=CARTESIAN_POINT('Ctrl Pts',(1.18321236827063,-28.5373735321406,
55.8001360995782));
#113410=CARTESIAN_POINT('Ctrl Pts',(1.17690866172103,-28.4972007095769,
55.7196460339274));
#113411=CARTESIAN_POINT('Ctrl Pts',(1.17502064751211,-28.4856491628171,
55.6950092144419));
#113412=CARTESIAN_POINT('Ctrl Pts',(1.17165090234293,-28.4659090902918,
55.6500764368256));
#113413=CARTESIAN_POINT('Ctrl Pts',(1.17016244036602,-28.4575073397739,
55.629881548414));
#113414=CARTESIAN_POINT('Ctrl Pts',(1.16786921729795,-28.4450673872868,
55.5982371668454));
#113415=CARTESIAN_POINT('Ctrl Pts',(1.16705527994685,-28.440752793604,55.5868997362884));
#113416=CARTESIAN_POINT('Ctrl Pts',(1.16624546596859,-28.4365623102019,
55.575515933853));
#113417=CARTESIAN_POINT('Origin',(5.,-30.,55.));
#113418=CARTESIAN_POINT('',(0.468131487137801,-28.4365623373493,55.5755160076012));
#113419=CARTESIAN_POINT('',(0.659214745210771,-28.4365623102018,55.5755159338528));
#113420=CARTESIAN_POINT('',(5.,-28.4365623102018,55.5755159338528));
#113421=CARTESIAN_POINT('',(0.428519636557289,-28.3340004401721,55.0012110545587));
#113422=CARTESIAN_POINT('Ctrl Pts',(0.468131487137799,-28.4365623373493,
55.5755160076012));
#113423=CARTESIAN_POINT('Ctrl Pts',(0.464559665450955,-28.4163576335939,
55.5206282296826));
#113424=CARTESIAN_POINT('Ctrl Pts',(0.460978297772835,-28.3990503155309,
55.4646953498218));
#113425=CARTESIAN_POINT('Ctrl Pts',(0.454816291795371,-28.3750168253862,
55.369534079064));
#113426=CARTESIAN_POINT('Ctrl Pts',(0.452288494775125,-28.3666894253552,
55.3307896060807));
#113427=CARTESIAN_POINT('Ctrl Pts',(0.448975349890733,-28.3578371707525,
55.2810279403499));
#113428=CARTESIAN_POINT('Ctrl Pts',(0.448253722146548,-28.3560288899956,
55.2702488384788));
#113429=CARTESIAN_POINT('Ctrl Pts',(0.447089391460057,-28.3533044885334,
55.2529683566067));
#113430=CARTESIAN_POINT('Ctrl Pts',(0.446650389253277,-28.3523204816432,
55.2464777839124));
#113431=CARTESIAN_POINT('Ctrl Pts',(0.44582750414188,-28.3505568582534,
55.2343620528578));
#113432=CARTESIAN_POINT('Ctrl Pts',(0.445444173184423,-28.3497675964323,
55.2287384104872));
#113433=CARTESIAN_POINT('Ctrl Pts',(0.44464178135063,-28.3481822399086,
55.2170069741934));
#113434=CARTESIAN_POINT('Ctrl Pts',(0.444222447831723,-28.3473912330323,
55.2108985532282));
#113435=CARTESIAN_POINT('Ctrl Pts',(0.443221768061731,-28.3455919301614,
55.1963716527654));
#113436=CARTESIAN_POINT('Ctrl Pts',(0.442638889947717,-28.3446140027119,
55.1879496748707));
#113437=CARTESIAN_POINT('Ctrl Pts',(0.440656114804364,-28.3415220427165,
55.1594225538021));
#113438=CARTESIAN_POINT('Ctrl Pts',(0.439242468058708,-28.3397097701379,
55.1392873099145));
#113439=CARTESIAN_POINT('Ctrl Pts',(0.435037745367989,-28.3354495891085,
55.0798599353537));
#113440=CARTESIAN_POINT('Ctrl Pts',(0.432212098543957,-28.3340275642907,
55.0405100936272));
#113441=CARTESIAN_POINT('Ctrl Pts',(0.429364773524748,-28.3340003968516,
55.0011499171688));
#113442=CARTESIAN_POINT('',(0.,-31.2690708798524,56.0793586530485));
#113443=CARTESIAN_POINT('Ctrl Pts',(0.428519636557289,-28.3340004401721,
55.0012110545587));
#113444=CARTESIAN_POINT('Ctrl Pts',(0.424501125412418,-28.3339569165041,
54.9413372767136));
#113445=CARTESIAN_POINT('Ctrl Pts',(0.420482614267547,-28.3371452968995,
54.8813422610129));
#113446=CARTESIAN_POINT('Ctrl Pts',(0.416464103122675,-28.3435783380043,
54.821609199589));
#113447=CARTESIAN_POINT('Ctrl Pts',(0.412450057461902,-28.3500042305304,
54.7619425152452));
#113448=CARTESIAN_POINT('Ctrl Pts',(0.408436011801128,-28.3596675898715,
54.7025377291128));
#113449=CARTESIAN_POINT('Ctrl Pts',(0.404421966140355,-28.3725291627882,
54.643777212934));
#113450=CARTESIAN_POINT('Ctrl Pts',(0.400410795178421,-28.3853815247612,
54.5850587786851));
#113451=CARTESIAN_POINT('Ctrl Pts',(0.396399624216488,-28.4014274513206,
54.5269842136769));
#113452=CARTESIAN_POINT('Ctrl Pts',(0.392388453254553,-28.4205762710958,
54.4699276609986));
#113453=CARTESIAN_POINT('Ctrl Pts',(0.388378570694002,-28.4397189402068,
54.4128894350737));
#113454=CARTESIAN_POINT('Ctrl Pts',(0.384368688133449,-28.4619623584441,
54.3568690721377));
#113455=CARTESIAN_POINT('Ctrl Pts',(0.380358805572897,-28.4871661075506,
54.3022252413161));
#113456=CARTESIAN_POINT('Ctrl Pts',(0.376345831298646,-28.51238928934,54.2475392788167));
#113457=CARTESIAN_POINT('Ctrl Pts',(0.372332857024395,-28.5405771449676,
54.1942324502499));
#113458=CARTESIAN_POINT('Ctrl Pts',(0.368319882750144,-28.5715418157655,
54.1426417225608));
#113459=CARTESIAN_POINT('Ctrl Pts',(0.364305505297722,-28.6025173136824,
54.0910329556375));
#113460=CARTESIAN_POINT('Ctrl Pts',(0.3602911278453,-28.6362712667164,54.0411419232217));
#113461=CARTESIAN_POINT('Ctrl Pts',(0.356276750392879,-28.6725724488726,
53.9932765541084));
#113462=CARTESIAN_POINT('Ctrl Pts',(0.352255019302422,-28.7089401284513,
53.9453235040028));
#113463=CARTESIAN_POINT('Ctrl Pts',(0.348233288211964,-28.7478640170129,
53.899403933109));
#113464=CARTESIAN_POINT('Ctrl Pts',(0.344211557121507,-28.7890732686805,
53.8557917797114));
#113465=CARTESIAN_POINT('Ctrl Pts',(0.340609642252897,-28.8259808124639,
53.8167321657687));
#113466=CARTESIAN_POINT('Ctrl Pts',(0.337007727384288,-28.86472077612,53.7795230582427));
#113467=CARTESIAN_POINT('Ctrl Pts',(0.333405812515678,-28.9050764107094,
53.7443335101966));
#113468=CARTESIAN_POINT('Ctrl Pts',(0.329325377332539,-28.9507933577289,
53.7044689728148));
#113469=CARTESIAN_POINT('Ctrl Pts',(0.325244942149401,-28.9987826271463,
53.6670238660387));
#113470=CARTESIAN_POINT('Ctrl Pts',(0.321164506966262,-29.0487579722144,
53.6322666178767));
#113471=CARTESIAN_POINT('Ctrl Pts',(0.317043925079215,-29.0992250161556,
53.5971673990945));
#113472=CARTESIAN_POINT('Ctrl Pts',(0.312923343192167,-29.1517170913018,
53.5648096294597));
#113473=CARTESIAN_POINT('Ctrl Pts',(0.308802761305119,-29.2059030293678,
53.5354297554461));
#113474=CARTESIAN_POINT('Ctrl Pts',(0.304733346342263,-29.2594161188262,
53.5064147031561));
#113475=CARTESIAN_POINT('Ctrl Pts',(0.300663931379406,-29.314580782465,
53.4803042617932));
#113476=CARTESIAN_POINT('Ctrl Pts',(0.29659451641655,-29.3710489165639,
53.45728274313));
#113477=CARTESIAN_POINT('Ctrl Pts',(0.29252752005979,-29.4274834895307,
53.4342749070196));
#113478=CARTESIAN_POINT('Ctrl Pts',(0.288460523703031,-29.4852195246385,
53.4143525458554));
#113479=CARTESIAN_POINT('Ctrl Pts',(0.28439352734627,-29.5438872246229,
53.3976526168968));
#113480=CARTESIAN_POINT('Ctrl Pts',(0.280327444740207,-29.6025417434664,
53.3809564399877));
#113481=CARTESIAN_POINT('Ctrl Pts',(0.276261362134141,-29.6621270203941,
53.3674813976669));
#113482=CARTESIAN_POINT('Ctrl Pts',(0.272195279528077,-29.7222583109853,
53.3573145297461));
#113483=CARTESIAN_POINT('Ctrl Pts',(0.268034884707164,-29.7837843384146,
53.3469118427521));
#113484=CARTESIAN_POINT('Ctrl Pts',(0.263874489886252,-29.8458814862898,
53.339972864249));
#113485=CARTESIAN_POINT('Ctrl Pts',(0.259714095065338,-29.9081292883171,
53.3365350101866));
#113486=CARTESIAN_POINT('Ctrl Pts',(0.255642712986453,-29.9690452822391,
53.3331707099165));
#113487=CARTESIAN_POINT('Ctrl Pts',(0.251571330907568,-30.0301050229311,
53.3331591191531));
#113488=CARTESIAN_POINT('Ctrl Pts',(0.247499948828683,-30.0909144776033,
53.336482474465));
#113489=CARTESIAN_POINT('Ctrl Pts',(0.243295047636755,-30.1537181505274,
53.3399148176942));
#113490=CARTESIAN_POINT('Ctrl Pts',(0.239090146444827,-30.2162542433769,
53.3469046314213));
#113491=CARTESIAN_POINT('Ctrl Pts',(0.2348852452529,-30.2780973747092,53.3573747079203));
#113492=CARTESIAN_POINT('Ctrl Pts',(0.230680344060973,-30.3399405060415,
53.3678447844194));
#113493=CARTESIAN_POINT('Ctrl Pts',(0.226475442869046,-30.4010901142077,
53.3817949221457));
#113494=CARTESIAN_POINT('Ctrl Pts',(0.222270541677118,-30.4611382343937,
53.3990916550969));
#113495=CARTESIAN_POINT('Ctrl Pts',(0.218232105035426,-30.5188091564334,
53.4157036411921));
#113496=CARTESIAN_POINT('Ctrl Pts',(0.214193668393735,-30.5757132364291,
53.4354740797279));
#113497=CARTESIAN_POINT('Ctrl Pts',(0.210155231752043,-30.6314753353094,
53.458314266494));
#113498=CARTESIAN_POINT('Ctrl Pts',(0.206029400047314,-30.688444171494,
53.4816487335323));
#113499=CARTESIAN_POINT('Ctrl Pts',(0.201903568342585,-30.7442204617963,
53.508187329055));
#113500=CARTESIAN_POINT('Ctrl Pts',(0.197777736637857,-30.7984179174006,
53.5377808546002));
#113501=CARTESIAN_POINT('Ctrl Pts',(0.193750411658712,-30.8513213759957,
53.5666678168368));
#113502=CARTESIAN_POINT('Ctrl Pts',(0.189723086679567,-30.9027200696696,
53.5984651822622));
#113503=CARTESIAN_POINT('Ctrl Pts',(0.185695761700423,-30.9522751223287,
53.6329857018327));
#113504=CARTESIAN_POINT('Ctrl Pts',(0.181670784440974,-31.0018012869855,
53.6674860977468));
#113505=CARTESIAN_POINT('Ctrl Pts',(0.177645807181524,-31.049485511849,
53.7047062047229));
#113506=CARTESIAN_POINT('Ctrl Pts',(0.173620829922075,-31.0950167085855,
53.744414714996));
#113507=CARTESIAN_POINT('Ctrl Pts',(0.169596634189296,-31.1405390645653,
53.7841155150989));
#113508=CARTESIAN_POINT('Ctrl Pts',(0.165572438456518,-31.1839088281068,
53.8263034164061));
#113509=CARTESIAN_POINT('Ctrl Pts',(0.16154824272374,-31.2248486564817,
53.8707074034091));
#113510=CARTESIAN_POINT('Ctrl Pts',(0.157347161733308,-31.2675880126558,
53.9170631867966));
#113511=CARTESIAN_POINT('Ctrl Pts',(0.153146080742876,-31.3076784050157,
53.965833974631));
#113512=CARTESIAN_POINT('Ctrl Pts',(0.148944999752445,-31.3448498765588,
54.0166715657931));
#113513=CARTESIAN_POINT('Ctrl Pts',(0.144914712435887,-31.380510153197,
54.0654423701008));
#113514=CARTESIAN_POINT('Ctrl Pts',(0.140884425119329,-31.4134840489688,
54.1161146630918));
#113515=CARTESIAN_POINT('Ctrl Pts',(0.136854137802771,-31.4435782915124,
54.1683524086043));
#113516=CARTESIAN_POINT('Ctrl Pts',(0.132820591304928,-31.4736968704331,
54.2206323973291));
#113517=CARTESIAN_POINT('Ctrl Pts',(0.128787044807085,-31.5009309364345,
54.2744798873931));
#113518=CARTESIAN_POINT('Ctrl Pts',(0.124753498309242,-31.5251345724958,
54.3295370735245));
#113519=CARTESIAN_POINT('Ctrl Pts',(0.120712473306291,-31.5493830839579,
54.3846963399091));
#113520=CARTESIAN_POINT('Ctrl Pts',(0.116671448303339,-31.5705897898519,
54.4410692839238));
#113521=CARTESIAN_POINT('Ctrl Pts',(0.112630423300388,-31.5886584275105,
54.4982825489384));
#113522=CARTESIAN_POINT('Ctrl Pts',(0.112132039146445,-31.5908868528941,
54.5053387251951));
#113523=CARTESIAN_POINT('Ctrl Pts',(0.111633654992502,-31.5930676105852,
54.5124076720023));
#113524=CARTESIAN_POINT('Ctrl Pts',(0.11113527083856,-31.5952005742277,
54.5194886806913));
#113525=CARTESIAN_POINT('Ctrl Pts',(0.10694773985886,-31.6131221940476,
54.5789848404677));
#113526=CARTESIAN_POINT('Ctrl Pts',(0.102760208879161,-31.6277416901261,
54.6395863054358));
#113527=CARTESIAN_POINT('Ctrl Pts',(0.0985726778994609,-31.6389317870598,
54.7009036988445));
#113528=CARTESIAN_POINT('Ctrl Pts',(0.0943940903940186,-31.6500979848644,
54.7620901342896));
#113529=CARTESIAN_POINT('Ctrl Pts',(0.090215502888577,-31.6578492651913,
54.8239889898453));
#113530=CARTESIAN_POINT('Ctrl Pts',(0.0860369153831346,-31.6621086094138,
54.8861976691256));
#113531=CARTESIAN_POINT('Ctrl Pts',(0.0818635996917905,-31.6663625799375,
54.9483278643268));
#113532=CARTESIAN_POINT('Ctrl Pts',(0.077690284000446,-31.6671333299212,
55.0107666325594));
#113533=CARTESIAN_POINT('Ctrl Pts',(0.0735169683091019,-31.6643953215423,
55.0731041286663));
#113534=CARTESIAN_POINT('Ctrl Pts',(0.0693476782178636,-31.6616599542593,
55.1353814937289));
#113535=CARTESIAN_POINT('Ctrl Pts',(0.0651783881266246,-31.6554225724169,
55.1975573043719));
#113536=CARTESIAN_POINT('Ctrl Pts',(0.0610090980353863,-31.6457096786985,
55.2592212441872));
#113537=CARTESIAN_POINT('Ctrl Pts',(0.0568425928731666,-31.636003272828,
55.3208439948092));
#113538=CARTESIAN_POINT('Ctrl Pts',(0.0526760877109474,-31.6228260427918,
55.3819550822746));
#113539=CARTESIAN_POINT('Ctrl Pts',(0.0485095825487276,-31.6062561827473,
55.4421505121406));
#113540=CARTESIAN_POINT('Ctrl Pts',(0.0443433163955318,-31.5896872732227,
55.5023424889324));
#113541=CARTESIAN_POINT('Ctrl Pts',(0.0401770502423353,-31.569726233976,
55.5616184474993));
#113542=CARTESIAN_POINT('Ctrl Pts',(0.0360107840891395,-31.5465018284697,
55.619587035484));
#113543=CARTESIAN_POINT('Ctrl Pts',(0.0318450104360858,-31.5232801683529,
55.6775487709208));
#113544=CARTESIAN_POINT('Ctrl Pts',(0.0276792367830336,-31.4967960926715,
55.734203000793));
#113545=CARTESIAN_POINT('Ctrl Pts',(0.02351346312998,-31.4672267106425,
55.7891779137668));
#113546=CARTESIAN_POINT('Ctrl Pts',(0.0193444149573671,-31.4376340855072,
55.8441960399448));
#113547=CARTESIAN_POINT('Ctrl Pts',(0.0151753667847533,-31.4049515381844,
55.8975317907779));
#113548=CARTESIAN_POINT('Ctrl Pts',(0.0110063186121403,-31.3694019533152,
55.9488383899572));
#113549=CARTESIAN_POINT('Ctrl Pts',(0.00733754574142688,-31.3381182292772,
55.993988326193));
#113550=CARTESIAN_POINT('Ctrl Pts',(0.00366877287071343,-31.3046150543095,
56.0375670978278));
#113551=CARTESIAN_POINT('Ctrl Pts',(0.,-31.2690708798524,56.0793586530485));
#113552=CARTESIAN_POINT('',(0.,-28.7475028281235,56.0985476022646));
#113553=CARTESIAN_POINT('Origin',(0.,-30.,55.));
#113554=CARTESIAN_POINT('Ctrl Pts',(1.62023172656234E-14,-28.7475028281236,
56.0985476022648));
#113555=CARTESIAN_POINT('Ctrl Pts',(3.75357402200702E-5,-28.7478625803039,
56.0989577698236));
#113556=CARTESIAN_POINT('Ctrl Pts',(7.48508279364976E-5,-28.7482202958009,
56.0993652087435));
#113557=CARTESIAN_POINT('Ctrl Pts',(0.000932278812672465,-28.7564416618929,
56.1087202727867));
#113558=CARTESIAN_POINT('Ctrl Pts',(0.00175868013715661,-28.7644030580975,
56.1175858633979));
#113559=CARTESIAN_POINT('Ctrl Pts',(0.0107130193140845,-28.8511361178773,
56.2121097718193));
#113560=CARTESIAN_POINT('Ctrl Pts',(0.0192885215002732,-28.9385755977656,
56.2893695022278));
#113561=CARTESIAN_POINT('Ctrl Pts',(0.0346719272342822,-29.1113734614591,
56.4124720618206));
#113562=CARTESIAN_POINT('Ctrl Pts',(0.0415003586744818,-29.1940618415998,
56.4612335904689));
#113563=CARTESIAN_POINT('Ctrl Pts',(0.0495712580011992,-29.3001267556719,
56.5120208776402));
#113564=CARTESIAN_POINT('Ctrl Pts',(0.0510520476430112,-29.3199399305453,
56.5210351973345));
#113565=CARTESIAN_POINT('Ctrl Pts',(0.0533548169406772,-29.3512950504097,
56.534565489637));
#113566=CARTESIAN_POINT('Ctrl Pts',(0.0541855673846926,-29.362719818038,
56.5393451001824));
#113567=CARTESIAN_POINT('Ctrl Pts',(0.0557339708160195,-29.3842215115695,
56.5480600280857));
#113568=CARTESIAN_POINT('Ctrl Pts',(0.0564525915581555,-29.3942854618892,
56.5520254202119));
#113569=CARTESIAN_POINT('Ctrl Pts',(0.0580613783573555,-29.4170021737305,
56.5607216226821));
#113570=CARTESIAN_POINT('Ctrl Pts',(0.0589496921570372,-29.4296753804327,
56.565397168395));
#113571=CARTESIAN_POINT('Ctrl Pts',(0.061227793507911,-29.4624979999319,
56.5770549412087));
#113572=CARTESIAN_POINT('Ctrl Pts',(0.0626101184269552,-29.482727475378,
56.5838055080911));
#113573=CARTESIAN_POINT('Ctrl Pts',(0.0731854464751945,-29.6397047570472,
56.6328600575719));
#113574=CARTESIAN_POINT('Ctrl Pts',(0.0817782006599408,-29.781254490794,
56.6577686126975));
#113575=CARTESIAN_POINT('Ctrl Pts',(0.0943890865181255,-29.9850953182022,
56.6670463540227));
#113576=CARTESIAN_POINT('Ctrl Pts',(0.0981994555451711,-30.0460397150593,
56.666476680097));
#113577=CARTESIAN_POINT('Ctrl Pts',(0.103152500170303,-30.1221192704565,
56.661589072911));
#113578=CARTESIAN_POINT('Ctrl Pts',(0.10415830102058,-30.1374143067386,
56.6603941194457));
#113579=CARTESIAN_POINT('Ctrl Pts',(0.105679039932593,-30.160266827608,
56.6582908184455));
#113580=CARTESIAN_POINT('Ctrl Pts',(0.106185867033484,-30.1678386050706,
56.6575415806849));
#113581=CARTESIAN_POINT('Ctrl Pts',(0.107104957588992,-30.181483254212,
56.6560969748654));
#113582=CARTESIAN_POINT('Ctrl Pts',(0.107516219708491,-30.1875578043628,
56.6554200160817));
#113583=CARTESIAN_POINT('Ctrl Pts',(0.108447945740051,-30.2012487235869,
56.653817950112));
#113584=CARTESIAN_POINT('Ctrl Pts',(0.108969405992014,-30.2088623772444,
56.6528736680248));
#113585=CARTESIAN_POINT('Ctrl Pts',(0.110585995213957,-30.2323241071582,
56.6497991420235));
#113586=CARTESIAN_POINT('Ctrl Pts',(0.111689953793306,-30.2481477225314,
56.6474933569477));
#113587=CARTESIAN_POINT('Ctrl Pts',(0.119511069272,-30.3590326351629,56.6297017996245));
#113588=CARTESIAN_POINT('Ctrl Pts',(0.126541406312297,-30.4526197329216,
56.6062268309948));
#113589=CARTESIAN_POINT('Ctrl Pts',(0.141905327855665,-30.6523773093463,
56.5372674590541));
#113590=CARTESIAN_POINT('Ctrl Pts',(0.150172738911815,-30.7569468805903,
56.4885656596627));
#113591=CARTESIAN_POINT('Ctrl Pts',(0.159565076372559,-30.8743405843089,
56.4182939421622));
#113592=CARTESIAN_POINT('Ctrl Pts',(0.161045410770459,-30.8927847011483,
56.4067568084943));
#113593=CARTESIAN_POINT('Ctrl Pts',(0.16334364918861,-30.9213143126495,
56.3881238235734));
#113594=CARTESIAN_POINT('Ctrl Pts',(0.164170395069581,-30.9315554393837,
56.3812719825102));
#113595=CARTESIAN_POINT('Ctrl Pts',(0.165709004674219,-30.9505690861189,
56.3682432133675));
#113596=CARTESIAN_POINT('Ctrl Pts',(0.166421855639546,-30.9593597174167,
56.3620939836012));
#113597=CARTESIAN_POINT('Ctrl Pts',(0.168014349531454,-30.9789515544843,
56.3481053198735));
#113598=CARTESIAN_POINT('Ctrl Pts',(0.168892189568057,-30.989719271434,
56.3402200865601));
#113599=CARTESIAN_POINT('Ctrl Pts',(0.171134944282373,-31.0171347972556,
56.3196329911025));
#113600=CARTESIAN_POINT('Ctrl Pts',(0.172492615266876,-31.0336402935467,
56.3067448997139));
#113601=CARTESIAN_POINT('Ctrl Pts',(0.183562612263131,-31.1672891739787,
56.1982697855029));
#113602=CARTESIAN_POINT('Ctrl Pts',(0.19257856866068,-31.2711586006143,
56.087461188863));
#113603=CARTESIAN_POINT('Ctrl Pts',(0.205633605993383,-31.3936879586553,
55.9147969208517));
#113604=CARTESIAN_POINT('Ctrl Pts',(0.209416025636807,-31.4259969972004,
55.8635684960944));
#113605=CARTESIAN_POINT('Ctrl Pts',(0.214334831993184,-31.4628461254091,
55.7974136858428));
#113606=CARTESIAN_POINT('Ctrl Pts',(0.215332049689358,-31.470065360942,
55.784024979009));
#113607=CARTESIAN_POINT('Ctrl Pts',(0.21683648963492,-31.4805643848506,
55.7638986909951));
#113608=CARTESIAN_POINT('Ctrl Pts',(0.217335518587385,-31.4839839024865,
55.7572343623819));
#113609=CARTESIAN_POINT('Ctrl Pts',(0.218239093383336,-31.4900597795696,
55.7451938083046));
#113610=CARTESIAN_POINT('Ctrl Pts',(0.218642638681212,-31.4927322136535,
55.7398259894008));
#113611=CARTESIAN_POINT('Ctrl Pts',(0.219553678015184,-31.4986730022683,
55.7277301540787));
#113612=CARTESIAN_POINT('Ctrl Pts',(0.220062113914561,-31.5019250134053,
55.7209945863529));
#113613=CARTESIAN_POINT('Ctrl Pts',(0.221620217123942,-31.5117017353367,
55.7003918433673));
#113614=CARTESIAN_POINT('Ctrl Pts',(0.222678048221896,-31.5180803414009,
55.6864567766573));
#113615=CARTESIAN_POINT('Ctrl Pts',(0.231187528639727,-31.5674149526258,
55.5746260460575));
#113616=CARTESIAN_POINT('Ctrl Pts',(0.239033421441629,-31.6010462240505,
55.472897739143));
#113617=CARTESIAN_POINT('Ctrl Pts',(0.25454182033073,-31.6482501071324,
55.2648675104554));
#113618=CARTESIAN_POINT('Ctrl Pts',(0.262166353587474,-31.661805049623,
55.15904262621));
#113619=CARTESIAN_POINT('Ctrl Pts',(0.27095201622974,-31.6658489648646,
55.0311009220826));
#113620=CARTESIAN_POINT('Ctrl Pts',(0.272417672274158,-31.6661118691617,
55.0095580556456));
#113621=CARTESIAN_POINT('Ctrl Pts',(0.274692181369376,-31.6658692077285,
54.9758265970315));
#113622=CARTESIAN_POINT('Ctrl Pts',(0.275509829500226,-31.6656477607705,
54.9636390116038));
#113623=CARTESIAN_POINT('Ctrl Pts',(0.277030712186308,-31.6649836824572,
54.9408585589592));
#113624=CARTESIAN_POINT('Ctrl Pts',(0.277734932829164,-31.6645736608853,
54.9302654366796));
#113625=CARTESIAN_POINT('Ctrl Pts',(0.279306851781938,-31.6634276760127,
54.9065239900043));
#113626=CARTESIAN_POINT('Ctrl Pts',(0.280172784135655,-31.6626368700546,
54.89337892894));
#113627=CARTESIAN_POINT('Ctrl Pts',(0.282705833005443,-31.6598526530429,
54.8547460586797));
#113628=CARTESIAN_POINT('Ctrl Pts',(0.28435944189621,-31.6574283051908,
54.8292924608546));
#113629=CARTESIAN_POINT('Ctrl Pts',(0.296517854340955,-31.635083120541,
54.6407714281719));
#113630=CARTESIAN_POINT('Ctrl Pts',(0.306191047854637,-31.5917304354458,
54.4814125429551));
#113631=CARTESIAN_POINT('Ctrl Pts',(0.318502913361422,-31.5122874053803,
54.3002362145878));
#113632=CARTESIAN_POINT('Ctrl Pts',(0.320615923008884,-31.4978838293999,
54.2699134934715));
#113633=CARTESIAN_POINT('Ctrl Pts',(0.324169684140878,-31.4726294239121,
54.2206451466195));
#113634=CARTESIAN_POINT('Ctrl Pts',(0.325586297798577,-31.4623041448519,
54.2014401178944));
#113635=CARTESIAN_POINT('Ctrl Pts',(0.327590724173834,-31.4473961563363,
54.1749703355599));
#113636=CARTESIAN_POINT('Ctrl Pts',(0.328160045905645,-31.4431291732388,
54.1675291224502));
#113637=CARTESIAN_POINT('Ctrl Pts',(0.329139310499817,-31.4357387001571,
54.1548684238715));
#113638=CARTESIAN_POINT('Ctrl Pts',(0.329547435343278,-31.4326437677014,
54.1496325325326));
#113639=CARTESIAN_POINT('Ctrl Pts',(0.330411739038064,-31.4260597131908,
54.13863184582));
#113640=CARTESIAN_POINT('Ctrl Pts',(0.330868283351245,-31.422564320962,
54.1328713179069));
#113641=CARTESIAN_POINT('Ctrl Pts',(0.33211830593615,-31.4129437626281,
54.1172310317389));
#113642=CARTESIAN_POINT('Ctrl Pts',(0.332915978117594,-31.4067501158323,
54.1073941405651));
#113643=CARTESIAN_POINT('Ctrl Pts',(0.337072936175573,-31.3741680925198,
54.056828086171));
#113644=CARTESIAN_POINT('Ctrl Pts',(0.340521544944614,-31.3461143916216,
54.0172048407093));
#113645=CARTESIAN_POINT('Ctrl Pts',(0.351235652704874,-31.2548821998936,
53.8995946118062));
#113646=CARTESIAN_POINT('Ctrl Pts',(0.358610955290783,-31.1863544693423,
53.826038462252));
#113647=CARTESIAN_POINT('Ctrl Pts',(0.369452580184512,-31.0739700808081,
53.7253629304253));
#113648=CARTESIAN_POINT('Ctrl Pts',(0.37304047129974,-31.0347993219239,
53.6933621194328));
#113649=CARTESIAN_POINT('Ctrl Pts',(0.378979569212961,-30.9664288754677,
53.6425127227984));
#113650=CARTESIAN_POINT('Ctrl Pts',(0.381363495022356,-30.9379872362941,
53.6227067374863));
#113651=CARTESIAN_POINT('Ctrl Pts',(0.384709398161686,-30.8966532279324,
53.5957976753192));
#113652=CARTESIAN_POINT('Ctrl Pts',(0.385698478023701,-30.8842543038273,
53.5879569660136));
#113653=CARTESIAN_POINT('Ctrl Pts',(0.387409121334323,-30.8625007400884,
53.5745995805627));
#113654=CARTESIAN_POINT('Ctrl Pts',(0.388133366006338,-30.8531928943661,
53.5690088131035));
#113655=CARTESIAN_POINT('Ctrl Pts',(0.389622336670036,-30.8338578731183,
53.5576509338085));
#113656=CARTESIAN_POINT('Ctrl Pts',(0.390386577941943,-30.8238239363243,
53.5518964420303));
#113657=CARTESIAN_POINT('Ctrl Pts',(0.392351109702528,-30.7977534769141,
53.5373036403333));
#113658=CARTESIAN_POINT('Ctrl Pts',(0.393545729129202,-30.7816294527555,
53.5286242178936));
#113659=CARTESIAN_POINT('Ctrl Pts',(0.398667264531292,-30.7113889561795,
53.4922949417827));
#113660=CARTESIAN_POINT('Ctrl Pts',(0.402500690228721,-30.6559223034154,
53.4673500339213));
#113661=CARTESIAN_POINT('Ctrl Pts',(0.413730943686305,-30.4871627820572,
53.4022989049097));
#113662=CARTESIAN_POINT('Ctrl Pts',(0.420900872275422,-30.3707808667734,
53.3713517363182));
#113663=CARTESIAN_POINT('Ctrl Pts',(0.431234977027151,-30.2074115523137,
53.3463436296408));
#113664=CARTESIAN_POINT('Ctrl Pts',(0.434107958570272,-30.1624774325154,
53.3413260598535));
#113665=CARTESIAN_POINT('Ctrl Pts',(0.437794345600006,-30.1063698172342,
53.3373624194594));
#113666=CARTESIAN_POINT('Ctrl Pts',(0.438524247324552,-30.0953329595042,
53.3366930911864));
#113667=CARTESIAN_POINT('Ctrl Pts',(0.439701051414267,-30.0776712032297,
53.3357983555512));
#113668=CARTESIAN_POINT('Ctrl Pts',(0.440144194818643,-30.0710499832864,
53.3355025307177));
#113669=CARTESIAN_POINT('Ctrl Pts',(0.441000630524023,-30.0583147198418,
53.3350096657094));
#113670=CARTESIAN_POINT('Ctrl Pts',(0.441413603588024,-30.0522010996308,
53.3348067799563));
#113671=CARTESIAN_POINT('Ctrl Pts',(0.442338965069219,-30.0385602267756,
53.3344292871092));
#113672=CARTESIAN_POINT('Ctrl Pts',(0.442852275525089,-30.0310326363063,
53.334272032771));
#113673=CARTESIAN_POINT('Ctrl Pts',(0.444639979192116,-30.0049427669413,
53.3339039125524));
#113674=CARTESIAN_POINT('Ctrl Pts',(0.445927102676751,-29.9863789654471,
53.3339522814767));
#113675=CARTESIAN_POINT('Ctrl Pts',(0.454821841236573,-29.8593408374988,
53.3364065098491));
#113676=CARTESIAN_POINT('Ctrl Pts',(0.462797073776145,-29.7513322394771,
53.3490941794592));
#113677=CARTESIAN_POINT('Ctrl Pts',(0.476889661467134,-29.5615685736355,
53.3904400938668));
#113678=CARTESIAN_POINT('Ctrl Pts',(0.48302888112474,-29.4793301556177,
53.41513036437));
#113679=CARTESIAN_POINT('Ctrl Pts',(0.491051378892342,-29.3714337221862,
53.4568356911214));
#113680=CARTESIAN_POINT('Ctrl Pts',(0.493103164567633,-29.3438134259284,
53.4683763420509));
#113681=CARTESIAN_POINT('Ctrl Pts',(0.496069104295478,-29.3038727409577,
53.4863438025928));
#113682=CARTESIAN_POINT('Ctrl Pts',(0.497002663246154,-29.2912992262281,
53.4921898401472));
#113683=CARTESIAN_POINT('Ctrl Pts',(0.498649156748737,-29.2691264770014,
53.502837668713));
#113684=CARTESIAN_POINT('Ctrl Pts',(0.499364212908342,-29.2594980512346,
53.5075764589182));
#113685=CARTESIAN_POINT('Ctrl Pts',(0.500865110186966,-29.2392944549664,
53.5177636588023));
#113686=CARTESIAN_POINT('Ctrl Pts',(0.501650172003646,-29.2287304620333,
53.5232329873811));
#113687=CARTESIAN_POINT('Ctrl Pts',(0.503738921525196,-29.2006427511085,
53.5381585417489));
#113688=CARTESIAN_POINT('Ctrl Pts',(0.505035436693089,-29.1832281218627,
53.5478167420967));
#113689=CARTESIAN_POINT('Ctrl Pts',(0.512573733888914,-29.082206352273,
53.6062360177406));
#113690=CARTESIAN_POINT('Ctrl Pts',(0.518554975603383,-29.0027990410851,
53.6618980286231));
#113691=CARTESIAN_POINT('Ctrl Pts',(0.529880515505819,-28.8610237036824,
53.7809468026903));
#113692=CARTESIAN_POINT('Ctrl Pts',(0.535220759653745,-28.7980097953967,
53.8430318666004));
#113693=CARTESIAN_POINT('Ctrl Pts',(0.543256131918304,-28.7143304190063,
53.9397288976512));
#113694=CARTESIAN_POINT('Ctrl Pts',(0.545782499591792,-28.6895186927909,
53.9705539015747));
#113695=CARTESIAN_POINT('Ctrl Pts',(0.549073921677668,-28.6594732815697,
54.0107291766534));
#113696=CARTESIAN_POINT('Ctrl Pts',(0.54977512792125,-28.6531984528712,
54.0192889197349));
#113697=CARTESIAN_POINT('Ctrl Pts',(0.550915700674219,-28.6432033011031,
54.0332005418519));
#113698=CARTESIAN_POINT('Ctrl Pts',(0.551351676551874,-28.6394317372136,
54.0385154847581));
#113699=CARTESIAN_POINT('Ctrl Pts',(0.552203489425921,-28.6321601877708,
54.0488911165766));
#113700=CARTESIAN_POINT('Ctrl Pts',(0.552619097602689,-28.628656897173,
54.0539492879644));
#113701=CARTESIAN_POINT('Ctrl Pts',(0.55366065604612,-28.6199861054858,
54.0666178312412));
#113702=CARTESIAN_POINT('Ctrl Pts',(0.554288852055143,-28.6148535176734,
54.0742517433201));
#113703=CARTESIAN_POINT('Ctrl Pts',(0.556572629816215,-28.5965334536372,
54.1019933836642));
#113704=CARTESIAN_POINT('Ctrl Pts',(0.558249525702292,-28.5837191447751,
54.1223425361972));
#113705=CARTESIAN_POINT('Ctrl Pts',(0.567251634879455,-28.5180457917415,
54.2318173097701));
#113706=CARTESIAN_POINT('Ctrl Pts',(0.574868118399485,-28.4731497831658,
54.3254486004659));
#113707=CARTESIAN_POINT('Ctrl Pts',(0.588424553480013,-28.4083725499691,
54.5007825568729));
#113708=CARTESIAN_POINT('Ctrl Pts',(0.594384960335272,-28.3854007867015,
54.5809907471399));
#113709=CARTESIAN_POINT('Ctrl Pts',(0.602235533419829,-28.3624744736332,
54.6918463944742));
#113710=CARTESIAN_POINT('Ctrl Pts',(0.604283616471256,-28.3572117588969,
54.7212608960795));
#113711=CARTESIAN_POINT('Ctrl Pts',(0.60724453931131,-28.3506716616341,
54.7644926035828));
#113712=CARTESIAN_POINT('Ctrl Pts',(0.608176741524404,-28.348771343716,
54.7782081014048));
#113713=CARTESIAN_POINT('Ctrl Pts',(0.609820926989279,-28.3457038117893,
54.8025791898692));
#113714=CARTESIAN_POINT('Ctrl Pts',(0.610535028087741,-28.3444680509492,
54.8132251903913));
#113715=CARTESIAN_POINT('Ctrl Pts',(0.612033979505358,-28.3420791336145,
54.8356967654067));
#113716=CARTESIAN_POINT('Ctrl Pts',(0.612818051047757,-28.3409495725663,
54.8475242850854));
#113717=CARTESIAN_POINT('Ctrl Pts',(0.614904240245468,-28.338267729879,
54.8791802963705));
#113718=CARTESIAN_POINT('Ctrl Pts',(0.616199193150838,-28.3369437888853,
54.8990265781233));
#113719=CARTESIAN_POINT('Ctrl Pts',(0.623783176792384,-28.3312278387557,
55.0162966637291));
#113720=CARTESIAN_POINT('Ctrl Pts',(0.629806890393584,-28.3350410166939,
55.1139348987395));
#113721=CARTESIAN_POINT('Ctrl Pts',(0.640245363638023,-28.356624779606,
55.2832355454365));
#113722=CARTESIAN_POINT('Ctrl Pts',(0.644678590323032,-28.3706400013324,
55.3550910777214));
#113723=CARTESIAN_POINT('Ctrl Pts',(0.652476636674378,-28.4027065631766,
55.4763917838337));
#113724=CARTESIAN_POINT('Ctrl Pts',(0.655783585865192,-28.4184591678063,
55.526329641042));
#113725=CARTESIAN_POINT('Ctrl Pts',(0.659211111289602,-28.4365431355012,
55.5754638423972));
#113726=CARTESIAN_POINT('Ctrl Pts',(0.659212928209264,-28.4365527225674,
55.5754898882335));
#113727=CARTESIAN_POINT('Ctrl Pts',(0.659214745210768,-28.4365623102018,
55.5755159338528));
#113728=CARTESIAN_POINT('Origin',(5.,-30.,125.));
#113729=CARTESIAN_POINT('',(9.56913309254615,-28.4365599842513,125.575509615172));
#113730=CARTESIAN_POINT('',(9.75970369730367,-28.4365599837282,125.575509613751));
#113731=CARTESIAN_POINT('',(5.,-28.4365599837785,125.575509613888));
#113732=CARTESIAN_POINT('',(10.,-31.3346917155535,125.997072727755));
#113733=CARTESIAN_POINT('Ctrl Pts',(9.75970369730367,-28.4365599837282,
125.575509613751));
#113734=CARTESIAN_POINT('Ctrl Pts',(9.75994451571396,-28.4379065492441,
125.579167718432));
#113735=CARTESIAN_POINT('Ctrl Pts',(9.76018561618856,-28.439266103374,125.582821504279));
#113736=CARTESIAN_POINT('Ctrl Pts',(9.76396616505077,-28.4607604410501,
125.639972574818));
#113737=CARTESIAN_POINT('Ctrl Pts',(9.76756188217567,-28.4836202388558,
125.6923974909));
#113738=CARTESIAN_POINT('Ctrl Pts',(9.77207491623637,-28.5144274149677,
125.754169230963));
#113739=CARTESIAN_POINT('Ctrl Pts',(9.77285759273999,-28.5198428497737,
125.764743045133));
#113740=CARTESIAN_POINT('Ctrl Pts',(9.77410232503199,-28.5285590500868,
125.781322261152));
#113741=CARTESIAN_POINT('Ctrl Pts',(9.77455987107205,-28.5317847034412,
125.78736699422));
#113742=CARTESIAN_POINT('Ctrl Pts',(9.7754118944931,-28.5378290951926,125.798527621339));
#113743=CARTESIAN_POINT('Ctrl Pts',(9.77580572358126,-28.5406376614943,
125.803648978627));
#113744=CARTESIAN_POINT('Ctrl Pts',(9.77672967135821,-28.5472593623224,
125.815574320486));
#113745=CARTESIAN_POINT('Ctrl Pts',(9.77726113849169,-28.5510933601628,
125.822366326629));
#113746=CARTESIAN_POINT('Ctrl Pts',(9.77905624837008,-28.5641318539652,
125.845090060905));
#113747=CARTESIAN_POINT('Ctrl Pts',(9.7803331085325,-28.5735521639723,125.860895487567));
#113748=CARTESIAN_POINT('Ctrl Pts',(9.78350149743746,-28.5973271953013,
125.89932348826));
#113749=CARTESIAN_POINT('Ctrl Pts',(9.78540724587401,-28.6119693144433,
125.921761561951));
#113750=CARTESIAN_POINT('Ctrl Pts',(9.79378251429947,-28.6780255606532,
126.017843607809));
#113751=CARTESIAN_POINT('Ctrl Pts',(9.80041826342814,-28.7348055181594,
126.08761403733));
#113752=CARTESIAN_POINT('Ctrl Pts',(9.81454454270551,-28.8686960009257,
126.227383426841));
#113753=CARTESIAN_POINT('Ctrl Pts',(9.8219702729316,-28.947313719987,126.295445072283));
#113754=CARTESIAN_POINT('Ctrl Pts',(9.83042357402043,-29.0477427120753,
126.367167655443));
#113755=CARTESIAN_POINT('Ctrl Pts',(9.8317569649978,-29.0639182836909,126.378293299996));
#113756=CARTESIAN_POINT('Ctrl Pts',(9.83385413702969,-29.0898827351996,
126.395483785136));
#113757=CARTESIAN_POINT('Ctrl Pts',(9.83462524832458,-29.0995438831628,
126.401737216424));
#113758=CARTESIAN_POINT('Ctrl Pts',(9.83607463095884,-29.1179157793364,
126.413360574966));
#113759=CARTESIAN_POINT('Ctrl Pts',(9.83675368055385,-29.1266126615979,
126.418751300482));
#113760=CARTESIAN_POINT('Ctrl Pts',(9.8382884089348,-29.1464682625006,126.430806937075));
#113761=CARTESIAN_POINT('Ctrl Pts',(9.83914217914352,-29.1576565085309,
126.43742212901));
#113762=CARTESIAN_POINT('Ctrl Pts',(9.84176038765198,-29.1923941659267,
126.457416318034));
#113763=CARTESIAN_POINT('Ctrl Pts',(9.84350852502053,-29.2161940004395,
126.470352950626));
#113764=CARTESIAN_POINT('Ctrl Pts',(9.85217889303779,-29.3370203882264,
126.532261338954));
#113765=CARTESIAN_POINT('Ctrl Pts',(9.85878029389206,-29.4383597227391,
126.572237248646));
#113766=CARTESIAN_POINT('Ctrl Pts',(9.87101604579307,-29.6313419490597,
126.627301443516));
#113767=CARTESIAN_POINT('Ctrl Pts',(9.8766300372631,-29.7217317355538,126.645168986635));
#113768=CARTESIAN_POINT('Ctrl Pts',(9.88352498252932,-29.8273483986049,
126.657091565063));
#113769=CARTESIAN_POINT('Ctrl Pts',(9.88446223307119,-29.8415964405245,
126.658514187078));
#113770=CARTESIAN_POINT('Ctrl Pts',(9.88588934250875,-29.8630909875837,
126.660380859115));
#113771=CARTESIAN_POINT('Ctrl Pts',(9.88637190756385,-29.870325381615,126.660961517718));
#113772=CARTESIAN_POINT('Ctrl Pts',(9.88726167851064,-29.8835968076819,
126.661939499302));
#113773=CARTESIAN_POINT('Ctrl Pts',(9.88766807118888,-29.889632499381,126.662351230676));
#113774=CARTESIAN_POINT('Ctrl Pts',(9.88852639150201,-29.9023254722685,
126.663147663766));
#113775=CARTESIAN_POINT('Ctrl Pts',(9.88897867336083,-29.9089828816488,
126.663525276355));
#113776=CARTESIAN_POINT('Ctrl Pts',(9.89019244811108,-29.9267710924219,
126.6644271378));
#113777=CARTESIAN_POINT('Ctrl Pts',(9.89095770818538,-29.9379049575182,
126.664879682921));
#113778=CARTESIAN_POINT('Ctrl Pts',(9.8948510116117,-29.9941790262757,126.66660174095));
#113779=CARTESIAN_POINT('Ctrl Pts',(9.89805839363356,-30.0393490765158,
126.666147076887));
#113780=CARTESIAN_POINT('Ctrl Pts',(9.90936116946916,-30.1960286472457,
126.658195662987));
#113781=CARTESIAN_POINT('Ctrl Pts',(9.91764203974498,-30.3067643456311,
126.641321646206));
#113782=CARTESIAN_POINT('Ctrl Pts',(9.93203831717597,-30.4993665145325,
126.591785582919));
#113783=CARTESIAN_POINT('Ctrl Pts',(9.93821217710515,-30.5819314146435,
126.563492354797));
#113784=CARTESIAN_POINT('Ctrl Pts',(9.94565819888396,-30.6815914325746,
126.520344977419));
#113785=CARTESIAN_POINT('Ctrl Pts',(9.94711621840112,-30.7011022622152,
126.511446796632));
#113786=CARTESIAN_POINT('Ctrl Pts',(9.94944303030874,-30.7322104700222,
126.496527425594));
#113787=CARTESIAN_POINT('Ctrl Pts',(9.9503192101316,-30.7439177602343,126.490742395386));
#113788=CARTESIAN_POINT('Ctrl Pts',(9.95199065133982,-30.766230001092,126.479388731336));
#113789=CARTESIAN_POINT('Ctrl Pts',(9.95278655215591,-30.7768452374353,
126.473842230897));
#113790=CARTESIAN_POINT('Ctrl Pts',(9.95462617365112,-30.8013502788028,
126.460699941063));
#113791=CARTESIAN_POINT('Ctrl Pts',(9.95566714467698,-30.815193594718,126.453019619794));
#113792=CARTESIAN_POINT('Ctrl Pts',(9.95908941541234,-30.8605932621434,
126.426978631489));
#113793=CARTESIAN_POINT('Ctrl Pts',(9.961444339829,-30.8916566270398,126.407777503271));
#113794=CARTESIAN_POINT('Ctrl Pts',(9.96910762261717,-30.9916281706381,
126.341344598547));
#113795=CARTESIAN_POINT('Ctrl Pts',(9.97429816414406,-31.0576177915449,
126.289952476888));
#113796=CARTESIAN_POINT('Ctrl Pts',(9.98457090092396,-31.1795816150135,
126.179292029512));
#113797=CARTESIAN_POINT('Ctrl Pts',(9.98964040694053,-31.2356155639976,
126.120443806729));
#113798=CARTESIAN_POINT('Ctrl Pts',(9.995854392969,-31.2962772040964,126.046627351688));
#113799=CARTESIAN_POINT('Ctrl Pts',(9.99679738131947,-31.3052758614811,
126.03538316696));
#113800=CARTESIAN_POINT('Ctrl Pts',(9.99815926204356,-31.3179580649797,
126.019108129792));
#113801=CARTESIAN_POINT('Ctrl Pts',(9.99857202460429,-31.3217611232338,
126.014170780477));
#113802=CARTESIAN_POINT('Ctrl Pts',(9.99932318648219,-31.3286066166782,
126.005179658991));
#113803=CARTESIAN_POINT('Ctrl Pts',(9.99966107564483,-31.3316584429384,
126.001133097393));
#113804=CARTESIAN_POINT('Ctrl Pts',(10.,-31.3346917155535,125.997072727755));
#113805=CARTESIAN_POINT('',(10.,-30.7923075365013,123.534460929349));
#113806=CARTESIAN_POINT('Origin',(10.,-30.,125.));
#113807=CARTESIAN_POINT('Ctrl Pts',(9.99999999999994,-30.7923075365013,
123.534460929349));
#113808=CARTESIAN_POINT('Ctrl Pts',(9.99926708496121,-30.8016756586983,
123.539525573458));
#113809=CARTESIAN_POINT('Ctrl Pts',(9.99852930854555,-30.8109947629585,
123.544679796411));
#113810=CARTESIAN_POINT('Ctrl Pts',(9.99204966954295,-30.8919287972562,
123.590461664261));
#113811=CARTESIAN_POINT('Ctrl Pts',(9.98606976217558,-30.9604834673963,
123.636253610317));
#113812=CARTESIAN_POINT('Ctrl Pts',(9.97464534962519,-31.0841521385255,
123.732824677345));
#113813=CARTESIAN_POINT('Ctrl Pts',(9.9692155793381,-31.1397932651847,123.782629121173));
#113814=CARTESIAN_POINT('Ctrl Pts',(9.96087158743111,-31.2215068019947,
123.866301916725));
#113815=CARTESIAN_POINT('Ctrl Pts',(9.95788607305659,-31.2499370011715,
123.89772589531));
#113816=CARTESIAN_POINT('Ctrl Pts',(9.95282145460603,-31.2968042730688,
123.95367671475));
#113817=CARTESIAN_POINT('Ctrl Pts',(9.95072128046115,-31.3158181625168,
123.977690596857));
#113818=CARTESIAN_POINT('Ctrl Pts',(9.94769358097189,-31.3425896985432,
124.013487460142));
#113819=CARTESIAN_POINT('Ctrl Pts',(9.94674581584978,-31.3508760673856,
124.024865157323));
#113820=CARTESIAN_POINT('Ctrl Pts',(9.94507701084002,-31.3652948307072,
124.045199600773));
#113821=CARTESIAN_POINT('Ctrl Pts',(9.94435378369102,-31.3714856496421,
124.054113696361));
#113822=CARTESIAN_POINT('Ctrl Pts',(9.94283810955629,-31.3843342124285,
124.073005583975));
#113823=CARTESIAN_POINT('Ctrl Pts',(9.94204642672205,-31.3909722185667,
124.082996096683));
#113824=CARTESIAN_POINT('Ctrl Pts',(9.93994450295174,-31.40839393213,124.109841108067));
#113825=CARTESIAN_POINT('Ctrl Pts',(9.93864137206597,-31.418983087874,124.126819965796));
#113826=CARTESIAN_POINT('Ctrl Pts',(9.93128242964598,-31.47749510852,124.2245159632));
#113827=CARTESIAN_POINT('Ctrl Pts',(9.92546528087725,-31.5188366449002,
124.30898220434));
#113828=CARTESIAN_POINT('Ctrl Pts',(9.91546646844782,-31.5778393588891,
124.460797771252));
#113829=CARTESIAN_POINT('Ctrl Pts',(9.91126613611847,-31.5988125887474,
124.52659341407));
#113830=CARTESIAN_POINT('Ctrl Pts',(9.90469624315624,-31.6245855734625,
124.629028198606));
#113831=CARTESIAN_POINT('Ctrl Pts',(9.90239307114696,-31.6323502358026,
124.664842213327));
#113832=CARTESIAN_POINT('Ctrl Pts',(9.89855311395586,-31.6431009015141,
124.723747014169));
#113833=CARTESIAN_POINT('Ctrl Pts',(9.89704430793271,-31.6467949659221,
124.746696826641));
#113834=CARTESIAN_POINT('Ctrl Pts',(9.8949225422075,-31.6512420537353,124.778560511889));
#113835=CARTESIAN_POINT('Ctrl Pts',(9.89433002993274,-31.6524054017544,
124.787415554464));
#113836=CARTESIAN_POINT('Ctrl Pts',(9.89331615589468,-31.6542620781662,
124.802485252524));
#113837=CARTESIAN_POINT('Ctrl Pts',(9.89289675076957,-31.6549917358788,
124.808695397122));
#113838=CARTESIAN_POINT('Ctrl Pts',(9.89201864101834,-31.6564393303941,
124.821644531724));
#113839=CARTESIAN_POINT('Ctrl Pts',(9.89155962314301,-31.657151132115,124.828384005428));
#113840=CARTESIAN_POINT('Ctrl Pts',(9.89030675651547,-31.6589731106979,
124.846704316409));
#113841=CARTESIAN_POINT('Ctrl Pts',(9.88950875995965,-31.6600031060348,
124.858292492427));
#113842=CARTESIAN_POINT('Ctrl Pts',(9.88541804075691,-31.6646282137652,
124.917334077948));
#113843=CARTESIAN_POINT('Ctrl Pts',(9.88204024862677,-31.6663098884451,
124.964911150791));
#113844=CARTESIAN_POINT('Ctrl Pts',(9.87138706030857,-31.6651989797993,
125.11308774233));
#113845=CARTESIAN_POINT('Ctrl Pts',(9.8639970731756,-31.6553348053409,125.213411225608));
#113846=CARTESIAN_POINT('Ctrl Pts',(9.85314568841142,-31.6270179378176,
125.361824975351));
#113847=CARTESIAN_POINT('Ctrl Pts',(9.84956356623129,-31.6153065176612,
125.410962673781));
#113848=CARTESIAN_POINT('Ctrl Pts',(9.84363234818514,-31.5918340521378,
125.492766015986));
#113849=CARTESIAN_POINT('Ctrl Pts',(9.84125091452813,-31.5812527360129,
125.525731951912));
#113850=CARTESIAN_POINT('Ctrl Pts',(9.8379055887241,-31.5647272725196,125.572189154445));
#113851=CARTESIAN_POINT('Ctrl Pts',(9.83691482977229,-31.5596202099386,
125.585966458468));
#113852=CARTESIAN_POINT('Ctrl Pts',(9.83520016874323,-31.5504112729223,
125.609835629471));
#113853=CARTESIAN_POINT('Ctrl Pts',(9.83447359869569,-31.5463915142819,
125.619957985975));
#113854=CARTESIAN_POINT('Ctrl Pts',(9.83297878814657,-31.5378790884301,
125.640795509862));
#113855=CARTESIAN_POINT('Ctrl Pts',(9.83221104427392,-31.5333730031845,
125.651504582234));
#113856=CARTESIAN_POINT('Ctrl Pts',(9.83023519456374,-31.5214312643373,
125.679074705769));
#113857=CARTESIAN_POINT('Ctrl Pts',(9.8290328316294,-31.5138271127673,125.695861383162));
#113858=CARTESIAN_POINT('Ctrl Pts',(9.82385531164028,-31.4796386149013,
125.768120541713));
#113859=CARTESIAN_POINT('Ctrl Pts',(9.81997596267147,-31.4502706515343,
125.822226168476));
#113860=CARTESIAN_POINT('Ctrl Pts',(9.80868217627455,-31.3547531666863,
125.977089155921));
#113861=CARTESIAN_POINT('Ctrl Pts',(9.80149390773205,-31.2806090285349,
126.072425797119));
#113862=CARTESIAN_POINT('Ctrl Pts',(9.7911298764295,-31.1652975344011,126.191509063384));
#113863=CARTESIAN_POINT('Ctrl Pts',(9.78824757627212,-31.1324397928708,
126.222780238562));
#113864=CARTESIAN_POINT('Ctrl Pts',(9.78455035449333,-31.0900275382096,
126.259967663639));
#113865=CARTESIAN_POINT('Ctrl Pts',(9.78381951595969,-31.0816316308882,
126.267182522886));
#113866=CARTESIAN_POINT('Ctrl Pts',(9.78264157686225,-31.0680935572103,
126.27858363382));
#113867=CARTESIAN_POINT('Ctrl Pts',(9.78219824618454,-31.062997047823,126.28282392717));
#113868=CARTESIAN_POINT('Ctrl Pts',(9.78134369140809,-31.0531741136247,
126.290897874293));
#113869=CARTESIAN_POINT('Ctrl Pts',(9.78093280515532,-31.048451813452,126.294736199133));
#113870=CARTESIAN_POINT('Ctrl Pts',(9.77991766498423,-31.0367848042294,
126.304113561151));
#113871=CARTESIAN_POINT('Ctrl Pts',(9.77931139296962,-31.0298166945629,
126.309623028735));
#113872=CARTESIAN_POINT('Ctrl Pts',(9.77717984611495,-31.0053059946969,
126.328686308018));
#113873=CARTESIAN_POINT('Ctrl Pts',(9.77563654795875,-30.9875380349221,
126.341944842871));
#113874=CARTESIAN_POINT('Ctrl Pts',(9.76558283681481,-30.8713418957222,
126.4250935548));
#113875=CARTESIAN_POINT('Ctrl Pts',(9.75666116340628,-30.7658316028005,
126.484462632965));
#113876=CARTESIAN_POINT('Ctrl Pts',(9.74379121782298,-30.6019536338763,
126.554514488182));
#113877=CARTESIAN_POINT('Ctrl Pts',(9.73968728152694,-30.5479327926763,
126.574367884202));
#113878=CARTESIAN_POINT('Ctrl Pts',(9.73302212813713,-30.4568910276268,
126.602571267814));
#113879=CARTESIAN_POINT('Ctrl Pts',(9.7304160144128,-30.4204211770606,126.612523026939));
#113880=CARTESIAN_POINT('Ctrl Pts',(9.72682554439009,-30.3689667297245,
126.624699038706));
#113881=CARTESIAN_POINT('Ctrl Pts',(9.72580795972714,-30.3542448790846,
126.627972360263));
#113882=CARTESIAN_POINT('Ctrl Pts',(9.72406854753942,-30.328846868538,126.633258614709));
#113883=CARTESIAN_POINT('Ctrl Pts',(9.72334367629279,-30.3181919573441,
126.635367803717));
#113884=CARTESIAN_POINT('Ctrl Pts',(9.72196035843565,-30.2977265666011,
126.63921143368));
#113885=CARTESIAN_POINT('Ctrl Pts',(9.72130141341689,-30.2879197031116,
126.640962365404));
#113886=CARTESIAN_POINT('Ctrl Pts',(9.71957957789169,-30.2621464061597,
126.645325801574));
#113887=CARTESIAN_POINT('Ctrl Pts',(9.71852130296157,-30.2461563396241,
126.647793924736));
#113888=CARTESIAN_POINT('Ctrl Pts',(9.71471939950037,-30.1882072611637,
126.655876183282));
#113889=CARTESIAN_POINT('Ctrl Pts',(9.71201851712529,-30.1460721221638,
126.660123883524));
#113890=CARTESIAN_POINT('Ctrl Pts',(9.70135702509057,-29.976919647339,126.67068526608));
#113891=CARTESIAN_POINT('Ctrl Pts',(9.69376943843848,-29.8495372173957,
126.664056046763));
#113892=CARTESIAN_POINT('Ctrl Pts',(9.68335700841577,-29.6832518572427,
126.636137609831));
#113893=CARTESIAN_POINT('Ctrl Pts',(9.68076828175081,-29.6426286992141,
126.627747203136));
#113894=CARTESIAN_POINT('Ctrl Pts',(9.67650822926257,-29.5778575876894,
126.61182772459));
#113895=CARTESIAN_POINT('Ctrl Pts',(9.67487490877224,-29.553493017766,126.605248946307));
#113896=CARTESIAN_POINT('Ctrl Pts',(9.67261535893484,-29.5205920247129,
126.595558269083));
#113897=CARTESIAN_POINT('Ctrl Pts',(9.67201438451142,-29.5119164787226,
126.592925818661));
#113898=CARTESIAN_POINT('Ctrl Pts',(9.67099780997606,-29.4973767537795,
126.588384053768));
#113899=CARTESIAN_POINT('Ctrl Pts',(9.67058438312519,-29.4915007504997,
126.586512698332));
#113900=CARTESIAN_POINT('Ctrl Pts',(9.66972743422822,-29.4794004140336,
126.582584923653));
#113901=CARTESIAN_POINT('Ctrl Pts',(9.66928370309871,-29.473177682019,126.580524346861));
#113902=CARTESIAN_POINT('Ctrl Pts',(9.66810411914285,-29.4567442585325,
126.574974803239));
#113903=CARTESIAN_POINT('Ctrl Pts',(9.66736480496803,-29.4465552234503,
126.57142333425));
#113904=CARTESIAN_POINT('Ctrl Pts',(9.66402282935719,-29.4009598221346,
126.555032259623));
#113905=CARTESIAN_POINT('Ctrl Pts',(9.66136644399632,-29.3659630504794,
126.541094132434));
#113906=CARTESIAN_POINT('Ctrl Pts',(9.65113870839662,-29.2348569551235,
126.483656995352));
#113907=CARTESIAN_POINT('Ctrl Pts',(9.64337156100733,-29.1424811795041,
126.432251327956));
#113908=CARTESIAN_POINT('Ctrl Pts',(9.63180784087054,-29.0103148238149,
126.341304978151));
#113909=CARTESIAN_POINT('Ctrl Pts',(9.62789452512773,-28.9666102920846,
126.307930612521));
#113910=CARTESIAN_POINT('Ctrl Pts',(9.62149233049919,-28.8966010984201,
126.248764895171));
#113911=CARTESIAN_POINT('Ctrl Pts',(9.61896349987556,-28.8693590389266,
126.224154516576));
#113912=CARTESIAN_POINT('Ctrl Pts',(9.61545480067594,-28.8321708862205,
126.188257389433));
#113913=CARTESIAN_POINT('Ctrl Pts',(9.61444407248696,-28.8215320587777,
126.177707009184));
#113914=CARTESIAN_POINT('Ctrl Pts',(9.61270859179761,-28.8033982516775,
126.1592321436));
#113915=CARTESIAN_POINT('Ctrl Pts',(9.61198092727424,-28.7958362496777,
126.151375081794));
#113916=CARTESIAN_POINT('Ctrl Pts',(9.61058688283756,-28.7814320304424,
126.136111681118));
#113917=CARTESIAN_POINT('Ctrl Pts',(9.60992005080986,-28.7745788611619,
126.128716389728));
#113918=CARTESIAN_POINT('Ctrl Pts',(9.60816507076817,-28.7566447788359,
126.109007744648));
#113919=CARTESIAN_POINT('Ctrl Pts',(9.60708178667373,-28.7456794655501,
126.096590357779));
#113920=CARTESIAN_POINT('Ctrl Pts',(9.60310258716954,-28.7058205602204,
126.050072876008));
#113921=CARTESIAN_POINT('Ctrl Pts',(9.60025437984429,-28.6781160208182,
126.014976229816));
#113922=CARTESIAN_POINT('Ctrl Pts',(9.59035504899481,-28.5855318754205,
125.887456594161));
#113923=CARTESIAN_POINT('Ctrl Pts',(9.58356758144573,-28.528666386121,125.78960572766));
#113924=CARTESIAN_POINT('Ctrl Pts',(9.57415340819301,-28.4656058209318,
125.650228987696));
#113925=CARTESIAN_POINT('Ctrl Pts',(9.57166688472001,-28.4504056391673,
125.613122976217));
#113926=CARTESIAN_POINT('Ctrl Pts',(9.56913309254614,-28.4365599842513,
125.575509615172));
#113927=CARTESIAN_POINT('Origin',(5.,-30.,125.));
#113928=CARTESIAN_POINT('',(8.86798217145003,-28.436560143385,125.575510047478));
#113929=CARTESIAN_POINT('',(9.06223779754793,-28.4365599835583,125.57550961329));
#113930=CARTESIAN_POINT('',(5.,-28.4365599837785,125.575509613888));
#113931=CARTESIAN_POINT('Ctrl Pts',(9.06223779754793,-28.4365599835583,
125.57550961329));
#113932=CARTESIAN_POINT('Ctrl Pts',(9.06389059933002,-28.4453428407573,
125.599369284938));
#113933=CARTESIAN_POINT('Ctrl Pts',(9.06552590189583,-28.4546713138373,
125.623026366844));
#113934=CARTESIAN_POINT('Ctrl Pts',(9.06986227677821,-28.4810815118922,
125.68575523031));
#113935=CARTESIAN_POINT('Ctrl Pts',(9.07253365247076,-28.499127595394,125.724400453568));
#113936=CARTESIAN_POINT('Ctrl Pts',(9.07974290865302,-28.5523418183504,
125.827808846025));
#113937=CARTESIAN_POINT('Ctrl Pts',(9.08421372303455,-28.5903535329045,
125.890998817763));
#113938=CARTESIAN_POINT('Ctrl Pts',(9.0895973824134,-28.6406101871138,125.963234591888));
#113939=CARTESIAN_POINT('Ctrl Pts',(9.09047576512338,-28.6489495266976,
125.974896996808));
#113940=CARTESIAN_POINT('Ctrl Pts',(9.09583344681536,-28.7005825621802,
126.045169713907));
#113941=CARTESIAN_POINT('Ctrl Pts',(9.10036545821814,-28.7475274932461,
126.100988353071));
#113942=CARTESIAN_POINT('Ctrl Pts',(9.10592591400627,-28.8064683343981,
126.162406510963));
#113943=CARTESIAN_POINT('Ctrl Pts',(9.10673418688796,-28.815066603373,126.171170165829));
#113944=CARTESIAN_POINT('Ctrl Pts',(9.10801130200919,-28.8286830919664,
126.184745126469));
#113945=CARTESIAN_POINT('Ctrl Pts',(9.10847526922015,-28.8336361085751,
126.18962161301));
#113946=CARTESIAN_POINT('Ctrl Pts',(9.1093477861865,-28.8429585073051,126.198685785176));
#113947=CARTESIAN_POINT('Ctrl Pts',(9.10975575974265,-28.8473203780158,
126.20288083858));
#113948=CARTESIAN_POINT('Ctrl Pts',(9.11072168512997,-28.8576554453067,
126.212712815134));
#113949=CARTESIAN_POINT('Ctrl Pts',(9.11128112062213,-28.8636475715681,
126.218329432031));
#113950=CARTESIAN_POINT('Ctrl Pts',(9.11316534606356,-28.8838586605985,
126.236995136783));
#113951=CARTESIAN_POINT('Ctrl Pts',(9.11450369092158,-28.8982622088678,
126.249840877123));
#113952=CARTESIAN_POINT('Ctrl Pts',(9.11783548206529,-28.9343097006044,
126.280882350314));
#113953=CARTESIAN_POINT('Ctrl Pts',(9.11984352247364,-28.9561995799827,
126.298782472974));
#113954=CARTESIAN_POINT('Ctrl Pts',(9.12904500388289,-29.0576419177724,
126.37751414196));
#113955=CARTESIAN_POINT('Ctrl Pts',(9.13641092388408,-29.1421247782131,
126.43165446924));
#113956=CARTESIAN_POINT('Ctrl Pts',(9.14959464477476,-29.3043084007384,
126.516049526275));
#113957=CARTESIAN_POINT('Ctrl Pts',(9.15544338239801,-29.3804062666587,
126.548709232751));
#113958=CARTESIAN_POINT('Ctrl Pts',(9.16244526156718,-29.4771676818996,
126.581956619876));
#113959=CARTESIAN_POINT('Ctrl Pts',(9.16377630918558,-29.4958209598727,
126.587999978756));
#113960=CARTESIAN_POINT('Ctrl Pts',(9.16589271451769,-29.5258867656511,
126.597157603824));
#113961=CARTESIAN_POINT('Ctrl Pts',(9.16668485541362,-29.5372328399044,
126.600481908193));
#113962=CARTESIAN_POINT('Ctrl Pts',(9.16818871277626,-29.5589462469017,
126.606593541876));
#113963=CARTESIAN_POINT('Ctrl Pts',(9.16890108177321,-29.5693069628799,
126.609401981762));
#113964=CARTESIAN_POINT('Ctrl Pts',(9.1705329997968,-29.5932099264239,126.61563390805));
#113965=CARTESIAN_POINT('Ctrl Pts',(9.17145026311751,-29.6067696512427,
126.618987647053));
#113966=CARTESIAN_POINT('Ctrl Pts',(9.17435741631522,-29.6501237576559,
126.629133624891));
#113967=CARTESIAN_POINT('Ctrl Pts',(9.17632669996584,-29.6800645233558,
126.635277111439));
#113968=CARTESIAN_POINT('Ctrl Pts',(9.18097738764118,-29.7519404547603,
126.647975316782));
#113969=CARTESIAN_POINT('Ctrl Pts',(9.18363630873181,-29.7939906266829,
126.653758355772));
#113970=CARTESIAN_POINT('Ctrl Pts',(9.19083902256052,-29.9096040396609,
126.665179456619));
#113971=CARTESIAN_POINT('Ctrl Pts',(9.19531490061675,-29.9833920116409,
126.667548678803));
#113972=CARTESIAN_POINT('Ctrl Pts',(9.20064313679382,-30.0704430943989,
126.664563657246));
#113973=CARTESIAN_POINT('Ctrl Pts',(9.20146128200233,-30.0837857593542,
126.663945413749));
#113974=CARTESIAN_POINT('Ctrl Pts',(9.2068326810085,-30.1711080730042,126.658846289221));
#113975=CARTESIAN_POINT('Ctrl Pts',(9.21143820699762,-30.2447169095172,
126.649593836059));
#113976=CARTESIAN_POINT('Ctrl Pts',(9.21708018019915,-30.3295075734238,
126.633135479342));
#113977=CARTESIAN_POINT('Ctrl Pts',(9.21788845555639,-30.3415333703881,
126.630662954129));
#113978=CARTESIAN_POINT('Ctrl Pts',(9.21916541540654,-30.3603203827648,
126.626583382721));
#113979=CARTESIAN_POINT('Ctrl Pts',(9.21962921976291,-30.3671010165151,
126.625066496633));
#113980=CARTESIAN_POINT('Ctrl Pts',(9.22050173671547,-30.3797718203926,
126.622148581547));
#113981=CARTESIAN_POINT('Ctrl Pts',(9.22090987601783,-30.3856640991398,
126.620757802419));
#113982=CARTESIAN_POINT('Ctrl Pts',(9.22187628250806,-30.3995360148918,
126.617403629936));
#113983=CARTESIAN_POINT('Ctrl Pts',(9.22243603601175,-30.4075088535818,
126.615413277307));
#113984=CARTESIAN_POINT('Ctrl Pts',(9.22432068300024,-30.4341571944914,
126.608550913612));
#113985=CARTESIAN_POINT('Ctrl Pts',(9.22565911926247,-30.4527619309364,
126.603413566659));
#113986=CARTESIAN_POINT('Ctrl Pts',(9.22899068390954,-30.4983872675725,
126.589957643326));
#113987=CARTESIAN_POINT('Ctrl Pts',(9.23099838462509,-30.5252929153879,
126.581272382818));
#113988=CARTESIAN_POINT('Ctrl Pts',(9.24019357069396,-30.6463715918789,
126.538756552732));
#113989=CARTESIAN_POINT('Ctrl Pts',(9.24755316658955,-30.7376010584079,
126.497168354391));
#113990=CARTESIAN_POINT('Ctrl Pts',(9.260738185935,-30.896480138873,126.406674143785));
#113991=CARTESIAN_POINT('Ctrl Pts',(9.26659387469504,-30.965266892046,126.360394184085));
#113992=CARTESIAN_POINT('Ctrl Pts',(9.27360364815253,-31.0457561850253,
126.297048589284));
#113993=CARTESIAN_POINT('Ctrl Pts',(9.27493587962849,-31.060960949827,126.284641180069));
#113994=CARTESIAN_POINT('Ctrl Pts',(9.27705432048739,-31.0849792795904,
126.264324335906));
#113995=CARTESIAN_POINT('Ctrl Pts',(9.27784731605055,-31.0939335112525,
126.256584875355));
#113996=CARTESIAN_POINT('Ctrl Pts',(9.27935291402748,-31.1108602494669,
126.241636423269));
#113997=CARTESIAN_POINT('Ctrl Pts',(9.28006616848645,-31.1188469138541,
126.234444447523));
#113998=CARTESIAN_POINT('Ctrl Pts',(9.28170031317826,-31.1370666739329,
126.217715494352));
#113999=CARTESIAN_POINT('Ctrl Pts',(9.28261891221082,-31.1472504658255,
126.20812583557));
#114000=CARTESIAN_POINT('Ctrl Pts',(9.28553136420732,-31.1793366056851,
126.177140005287));
#114001=CARTESIAN_POINT('Ctrl Pts',(9.28750454801023,-31.2007711915046,
126.155267136093));
#114002=CARTESIAN_POINT('Ctrl Pts',(9.29216586624923,-31.2505134483854,
126.101626647788));
#114003=CARTESIAN_POINT('Ctrl Pts',(9.29483141592322,-31.2782313613824,
126.069340975862));
#114004=CARTESIAN_POINT('Ctrl Pts',(9.30203587260516,-31.3504928408421,
125.97834107053));
#114005=CARTESIAN_POINT('Ctrl Pts',(9.30650750206485,-31.3924256232248,
125.917678271393));
#114006=CARTESIAN_POINT('Ctrl Pts',(9.31185900726484,-31.4372839428721,
125.842592026091));
#114007=CARTESIAN_POINT('Ctrl Pts',(9.31270455652755,-31.4442142736856,
125.830657318496));
#114008=CARTESIAN_POINT('Ctrl Pts',(9.3180653150418,-31.4870942822952,125.754654616862));
#114009=CARTESIAN_POINT('Ctrl Pts',(9.32263291722558,-31.5189170355347,
125.688361320747));
#114010=CARTESIAN_POINT('Ctrl Pts',(9.32823297603165,-31.5508320274583,
125.608791401724));
#114011=CARTESIAN_POINT('Ctrl Pts',(9.32904181279348,-31.5552792746956,
125.597338517201));
#114012=CARTESIAN_POINT('Ctrl Pts',(9.33031988017727,-31.5620455872949,
125.579325452338));
#114013=CARTESIAN_POINT('Ctrl Pts',(9.33078423533308,-31.5644510154057,
125.572797881044));
#114014=CARTESIAN_POINT('Ctrl Pts',(9.33165835073149,-31.5688786352828,
125.560546764479));
#114015=CARTESIAN_POINT('Ctrl Pts',(9.33206754265318,-31.5709105207891,
125.554826980509));
#114016=CARTESIAN_POINT('Ctrl Pts',(9.3330371624904,-31.575630104756,125.541307520354));
#114017=CARTESIAN_POINT('Ctrl Pts',(9.33359908930249,-31.5782911797907,
125.53349883155));
#114018=CARTESIAN_POINT('Ctrl Pts',(9.33549396820274,-31.5870212102404,
125.507244280964));
#114019=CARTESIAN_POINT('Ctrl Pts',(9.33684058618207,-31.5928253841288,
125.488712898948));
#114020=CARTESIAN_POINT('Ctrl Pts',(9.34019636727919,-31.6063450960727,
125.442745478243));
#114021=CARTESIAN_POINT('Ctrl Pts',(9.34222028491288,-31.6136829011744,
125.415205295821));
#114022=CARTESIAN_POINT('Ctrl Pts',(9.35156962251807,-31.6440319446479,
125.288299826575));
#114023=CARTESIAN_POINT('Ctrl Pts',(9.35907015794566,-31.6585950088456,
125.187139251635));
#114024=CARTESIAN_POINT('Ctrl Pts',(9.37216406600614,-31.6679040950355,
125.0055192896));
#114025=CARTESIAN_POINT('Ctrl Pts',(9.37780517404365,-31.6662521772768,
124.925558278909));
#114026=CARTESIAN_POINT('Ctrl Pts',(9.38460671077072,-31.657064149822,124.826577323893));
#114027=CARTESIAN_POINT('Ctrl Pts',(9.38593173746895,-31.6549184496565,
124.80717364725));
#114028=CARTESIAN_POINT('Ctrl Pts',(9.38804210089221,-31.6509265233338,
124.776086264705));
#114029=CARTESIAN_POINT('Ctrl Pts',(9.38883411121953,-31.6492961101253,
124.764377208505));
#114030=CARTESIAN_POINT('Ctrl Pts',(9.39033996624531,-31.6459428838921,
124.742038871597));
#114031=CARTESIAN_POINT('Ctrl Pts',(9.39105444144772,-31.6442413922971,
124.731407047884));
#114032=CARTESIAN_POINT('Ctrl Pts',(9.39269443897607,-31.6400807316658,
124.706932001561));
#114033=CARTESIAN_POINT('Ctrl Pts',(9.3936176271612,-31.6375491352972,124.693101796001));
#114034=CARTESIAN_POINT('Ctrl Pts',(9.39655772892414,-31.6288799828841,
124.648908098807));
#114035=CARTESIAN_POINT('Ctrl Pts',(9.39855342602875,-31.6220703891944,
124.618682063026));
#114036=CARTESIAN_POINT('Ctrl Pts',(9.40992510334145,-31.5779885409697,
124.445669446299));
#114037=CARTESIAN_POINT('Ctrl Pts',(9.41868980673958,-31.5227236440366,
124.308160350397));
#114038=CARTESIAN_POINT('Ctrl Pts',(9.43132944099916,-31.4222745625069,
124.130587281867));
#114039=CARTESIAN_POINT('Ctrl Pts',(9.43488291763592,-31.3920003381725,
124.082897461114));
#114040=CARTESIAN_POINT('Ctrl Pts',(9.43935225533778,-31.3524773652413,
124.027116120467));
#114041=CARTESIAN_POINT('Ctrl Pts',(9.4401374574757,-31.3454826528222,124.017465279244));
#114042=CARTESIAN_POINT('Ctrl Pts',(9.44138594402702,-31.3342939762659,
124.002371419115));
#114043=CARTESIAN_POINT('Ctrl Pts',(9.4418447011448,-31.3301686997754,123.9968776613));
#114044=CARTESIAN_POINT('Ctrl Pts',(9.44271162772101,-31.3223498553831,
123.986598102644));
#114045=CARTESIAN_POINT('Ctrl Pts',(9.44311927172541,-31.3186640759014,
123.981806700079));
#114046=CARTESIAN_POINT('Ctrl Pts',(9.44409127822239,-31.3098529446529,
123.970480580788));
#114047=CARTESIAN_POINT('Ctrl Pts',(9.44465720653217,-31.3047047343026,
123.963964035327));
#114048=CARTESIAN_POINT('Ctrl Pts',(9.44659894595935,-31.2869722515712,
123.941860240634));
#114049=CARTESIAN_POINT('Ctrl Pts',(9.4479895726608,-31.2741561937267,123.926462282038));
#114050=CARTESIAN_POINT('Ctrl Pts',(9.45148446122763,-31.2415898580862,
123.888739942417));
#114051=CARTESIAN_POINT('Ctrl Pts',(9.45360523614729,-31.2215125710045,
123.866707838631));
#114052=CARTESIAN_POINT('Ctrl Pts',(9.46388437932644,-31.1222786429749,
123.763513752125));
#114053=CARTESIAN_POINT('Ctrl Pts',(9.47224659940962,-31.0355649220604,
123.690032390207));
#114054=CARTESIAN_POINT('Ctrl Pts',(9.48533161008495,-30.8849547222947,
123.586775213546));
#114055=CARTESIAN_POINT('Ctrl Pts',(9.49019755252259,-30.825462663382,123.551220229114));
#114056=CARTESIAN_POINT('Ctrl Pts',(9.49621708007272,-30.747204530449,123.510840740678));
#114057=CARTESIAN_POINT('Ctrl Pts',(9.49749312562583,-30.7303408507461,
123.502498012576));
#114058=CARTESIAN_POINT('Ctrl Pts',(9.49954097883193,-30.7028409503989,
123.489468456255));
#114059=CARTESIAN_POINT('Ctrl Pts',(9.50031888945334,-30.6922910832407,
123.484604337422));
#114060=CARTESIAN_POINT('Ctrl Pts',(9.50180756042947,-30.6719063342073,
123.475463063823));
#114061=CARTESIAN_POINT('Ctrl Pts',(9.50251884739219,-30.6620793764762,
123.47116976084));
#114062=CARTESIAN_POINT('Ctrl Pts',(9.50416526665393,-30.6391347185475,
123.461408188155));
#114063=CARTESIAN_POINT('Ctrl Pts',(9.5050979041059,-30.6259870151238,123.456012231391));
#114064=CARTESIAN_POINT('Ctrl Pts',(9.50812737656557,-30.5828068281466,
123.438932878497));
#114065=CARTESIAN_POINT('Ctrl Pts',(9.5102008008245,-30.5525031341213,123.427952016501));
#114066=CARTESIAN_POINT('Ctrl Pts',(9.51515772415006,-30.4784710356829,
123.403531206414));
#114067=CARTESIAN_POINT('Ctrl Pts',(9.51801409559071,-30.434470366514,123.390999349362));
#114068=CARTESIAN_POINT('Ctrl Pts',(9.52512372644802,-30.3226277650559,
123.364068906182));
#114069=CARTESIAN_POINT('Ctrl Pts',(9.52932924226855,-30.2543003760714,
123.352064693413));
#114070=CARTESIAN_POINT('Ctrl Pts',(9.53431792129586,-30.1732516179027,
123.342987657701));
#114071=CARTESIAN_POINT('Ctrl Pts',(9.53506815284999,-30.1610646414383,
123.341758701882));
#114072=CARTESIAN_POINT('Ctrl Pts',(9.54035796771801,-30.0752469660574,
123.334059672392));
#114073=CARTESIAN_POINT('Ctrl Pts',(9.54495067255575,-30.0012797032774,
123.332362493317));
#114074=CARTESIAN_POINT('Ctrl Pts',(9.5505778095653,-29.9152174870883,123.336113598137));
#114075=CARTESIAN_POINT('Ctrl Pts',(9.5513842367218,-29.9029870138944,123.336781886941));
#114076=CARTESIAN_POINT('Ctrl Pts',(9.55265793484031,-29.8838537580744,
123.338039101398));
#114077=CARTESIAN_POINT('Ctrl Pts',(9.55312032287477,-29.876945104284,123.338536348191));
#114078=CARTESIAN_POINT('Ctrl Pts',(9.5539919168578,-29.8639969877972,123.339549482477));
#114079=CARTESIAN_POINT('Ctrl Pts',(9.5544005661202,-29.8579569586731,123.340055269005));
#114080=CARTESIAN_POINT('Ctrl Pts',(9.55536868591195,-29.8437177275803,
123.341325932042));
#114081=CARTESIAN_POINT('Ctrl Pts',(9.55592965549295,-29.8355212460014,
123.342118657815));
#114082=CARTESIAN_POINT('Ctrl Pts',(9.55781629932395,-29.8081248077636,
123.344973474094));
#114083=CARTESIAN_POINT('Ctrl Pts',(9.55915548848551,-29.7889556700667,
123.347308527785));
#114084=CARTESIAN_POINT('Ctrl Pts',(9.56248722154647,-29.7418430948287,
123.353880422655));
#114085=CARTESIAN_POINT('Ctrl Pts',(9.56449427818051,-29.7139590926442,
123.358496095079));
#114086=CARTESIAN_POINT('Ctrl Pts',(9.57366386920714,-29.5882807641671,
123.382599104441));
#114087=CARTESIAN_POINT('Ctrl Pts',(9.5809974097623,-29.4922384660791,123.410133026382));
#114088=CARTESIAN_POINT('Ctrl Pts',(9.59421679974319,-29.3213071919836,
123.47621776069));
#114089=CARTESIAN_POINT('Ctrl Pts',(9.60012881080644,-29.2457477538774,
123.512168155588));
#114090=CARTESIAN_POINT('Ctrl Pts',(9.60719866112001,-29.1560795089531,
123.563426691946));
#114091=CARTESIAN_POINT('Ctrl Pts',(9.60853738784968,-29.1391384805706,
123.573514049607));
#114092=CARTESIAN_POINT('Ctrl Pts',(9.6106663654073,-29.1122703566486,123.590165422435));
#114093=CARTESIAN_POINT('Ctrl Pts',(9.61146343371866,-29.1022280294976,
123.596538936272));
#114094=CARTESIAN_POINT('Ctrl Pts',(9.61297698854849,-29.0831953322957,
123.608906213186));
#114095=CARTESIAN_POINT('Ctrl Pts',(9.61369412811207,-29.0741933766686,
123.614880933651));
#114096=CARTESIAN_POINT('Ctrl Pts',(9.61533762704353,-29.0536050307787,
123.628836089473));
#114097=CARTESIAN_POINT('Ctrl Pts',(9.61626167655271,-29.0420602272945,
123.636876630982));
#114098=CARTESIAN_POINT('Ctrl Pts',(9.61919439613349,-29.0055370186924,
123.663006937264));
#114099=CARTESIAN_POINT('Ctrl Pts',(9.62118219217877,-28.9809576125359,
123.681645011811));
#114100=CARTESIAN_POINT('Ctrl Pts',(9.62588348790906,-28.9234366565551,
123.72783252063));
#114101=CARTESIAN_POINT('Ctrl Pts',(9.6285740587608,-28.891014572963,123.755994197638));
#114102=CARTESIAN_POINT('Ctrl Pts',(9.63575157497526,-28.8066361848038,
123.835208527477));
#114103=CARTESIAN_POINT('Ctrl Pts',(9.64017526535042,-28.7568799290371,
123.888465386057));
#114104=CARTESIAN_POINT('Ctrl Pts',(9.64536565406243,-28.7031969632477,
123.954055102617));
#114105=CARTESIAN_POINT('Ctrl Pts',(9.64609844104944,-28.695726875889,123.963385096283));
#114106=CARTESIAN_POINT('Ctrl Pts',(9.65143268905923,-28.6421988854006,
124.031735172149));
#114107=CARTESIAN_POINT('Ctrl Pts',(9.65608507259707,-28.6000708598512,
124.093712947131));
#114108=CARTESIAN_POINT('Ctrl Pts',(9.66178032184662,-28.5560187562625,
124.16896049655));
#114109=CARTESIAN_POINT('Ctrl Pts',(9.66259319329784,-28.5498988856904,
124.179685898596));
#114110=CARTESIAN_POINT('Ctrl Pts',(9.66387840151904,-28.5404954779628,
124.196599966775));
#114111=CARTESIAN_POINT('Ctrl Pts',(9.66434587004967,-28.5371306505963,
124.202743250026));
#114112=CARTESIAN_POINT('Ctrl Pts',(9.66523007251182,-28.5308725435921,
124.214341901285));
#114113=CARTESIAN_POINT('Ctrl Pts',(9.66564627335725,-28.5279707042067,
124.219792413206));
#114114=CARTESIAN_POINT('Ctrl Pts',(9.6666366200846,-28.5211680713316,124.23274281235));
#114115=CARTESIAN_POINT('Ctrl Pts',(9.66721234151501,-28.5172939582916,
124.240256456666));
#114116=CARTESIAN_POINT('Ctrl Pts',(9.66916988677307,-28.5043864337242,
124.265764704886));
#114117=CARTESIAN_POINT('Ctrl Pts',(9.67056608814642,-28.4956224834149,
124.28389273905));
#114118=CARTESIAN_POINT('Ctrl Pts',(9.68032290249009,-28.4372644051163,
124.410406683955));
#114119=CARTESIAN_POINT('Ctrl Pts',(9.68909376329002,-28.3991001928916,
124.523679457309));
#114120=CARTESIAN_POINT('Ctrl Pts',(9.70382032119808,-28.3549258039464,
124.723308590907));
#114121=CARTESIAN_POINT('Ctrl Pts',(9.7098524581643,-28.3429193192993,124.807867778118));
#114122=CARTESIAN_POINT('Ctrl Pts',(9.71703355873765,-28.3361764024113,
124.912625356863));
#114123=CARTESIAN_POINT('Ctrl Pts',(9.71836925881555,-28.335260331937,124.932285995));
#114124=CARTESIAN_POINT('Ctrl Pts',(9.72049724830729,-28.3343488790973,
124.963880856001));
#114125=CARTESIAN_POINT('Ctrl Pts',(9.72129623747585,-28.3341329801179,
124.975806326301));
#114126=CARTESIAN_POINT('Ctrl Pts',(9.72281611609816,-28.3339650959009,
124.998606983978));
#114127=CARTESIAN_POINT('Ctrl Pts',(9.72353763388513,-28.3339914898998,
125.009481345367));
#114128=CARTESIAN_POINT('Ctrl Pts',(9.72519522352925,-28.3342981007914,
125.03457485386));
#114129=CARTESIAN_POINT('Ctrl Pts',(9.72612891418908,-28.3346539206633,
125.048792357817));
#114130=CARTESIAN_POINT('Ctrl Pts',(9.72911022938338,-28.3363812386608,
125.0944347978));
#114131=CARTESIAN_POINT('Ctrl Pts',(9.73113605243017,-28.3384606393052,
125.125827142653));
#114132=CARTESIAN_POINT('Ctrl Pts',(9.74228319104025,-28.3549758076651,
125.300136629054));
#114133=CARTESIAN_POINT('Ctrl Pts',(9.75083237414512,-28.3869548981719,
125.440751524718));
#114134=CARTESIAN_POINT('Ctrl Pts',(9.75970369730367,-28.4365599837282,
125.575509613751));
#114135=CARTESIAN_POINT('Ctrl Pts',(9.56913309254614,-28.4365599842513,
125.575509615172));
#114136=CARTESIAN_POINT('Ctrl Pts',(9.56864907652894,-28.4339151269433,
125.568324547117));
#114137=CARTESIAN_POINT('Ctrl Pts',(9.56816332838147,-28.4313196967858,
125.561120966193));
#114138=CARTESIAN_POINT('Ctrl Pts',(9.56590951223272,-28.4195543508702,
125.527746639993));
#114139=CARTESIAN_POINT('Ctrl Pts',(9.56411880548602,-28.4109898327577,
125.501369566884));
#114140=CARTESIAN_POINT('Ctrl Pts',(9.5616726110363,-28.4003989635077,125.465748386525));
#114141=CARTESIAN_POINT('Ctrl Pts',(9.56104756284543,-28.3977868054281,
125.456681403509));
#114142=CARTESIAN_POINT('Ctrl Pts',(9.55999962570631,-28.3935660290641,
125.441548720156));
#114143=CARTESIAN_POINT('Ctrl Pts',(9.55957915432647,-28.3919143628956,
125.435495070804));
#114144=CARTESIAN_POINT('Ctrl Pts',(9.5587733120997,-28.3888293866305,125.423931209732));
#114145=CARTESIAN_POINT('Ctrl Pts',(9.55838831516424,-28.3873900524238,
125.418422717458));
#114146=CARTESIAN_POINT('Ctrl Pts',(9.55734420574154,-28.3835787110721,
125.403524486058));
#114147=CARTESIAN_POINT('Ctrl Pts',(9.55668216604186,-28.3812603439051,
125.394121438962));
#114148=CARTESIAN_POINT('Ctrl Pts',(9.55412129549575,-28.3726629844751,
125.357895423551));
#114149=CARTESIAN_POINT('Ctrl Pts',(9.55219417358964,-28.3669680326369,
125.330939994153));
#114150=CARTESIAN_POINT('Ctrl Pts',(9.54311627988201,-28.3435782332267,
125.20484877221));
#114151=CARTESIAN_POINT('Ctrl Pts',(9.53571699610879,-28.3342272104926,
125.104382936422));
#114152=CARTESIAN_POINT('Ctrl Pts',(9.52129044764897,-28.333786189495,124.905355962508));
#114153=CARTESIAN_POINT('Ctrl Pts',(9.51428778498704,-28.3422749160066,
124.807180107484));
#114154=CARTESIAN_POINT('Ctrl Pts',(9.50620104424878,-28.362816952133,124.690842168768));
#114155=CARTESIAN_POINT('Ctrl Pts',(9.50485849955833,-28.366601233408,124.671434291939));
#114156=CARTESIAN_POINT('Ctrl Pts',(9.50272785511388,-28.3732077457406,
124.640495178933));
#114157=CARTESIAN_POINT('Ctrl Pts',(9.50193282781672,-28.3758091674126,
124.628919271821));
#114158=CARTESIAN_POINT('Ctrl Pts',(9.500425924596,-28.3809997232743,124.606923216332));
#114159=CARTESIAN_POINT('Ctrl Pts',(9.49971337030503,-28.3835663497061,
124.596498429626));
#114160=CARTESIAN_POINT('Ctrl Pts',(9.49809968516449,-28.3896339863144,
124.572841209062));
#114161=CARTESIAN_POINT('Ctrl Pts',(9.49720061826433,-28.3931976836133,
124.559625539693));
#114162=CARTESIAN_POINT('Ctrl Pts',(9.49436252145478,-28.4050268150634,
124.517814924124));
#114163=CARTESIAN_POINT('Ctrl Pts',(9.49244296538531,-28.4138961174369,
124.48939589123));
#114164=CARTESIAN_POINT('Ctrl Pts',(9.4814725659988,-28.4695220239556,124.326631245233));
#114165=CARTESIAN_POINT('Ctrl Pts',(9.47298949485508,-28.5325657372751,
124.198485425495));
#114166=CARTESIAN_POINT('Ctrl Pts',(9.4615463728839,-28.6349691757038,124.043908408253));
#114167=CARTESIAN_POINT('Ctrl Pts',(9.4588538890971,-28.6602038694527,124.008856159938));
#114168=CARTESIAN_POINT('Ctrl Pts',(9.45444160141901,-28.7027388407429,
123.954369582316));
#114169=CARTESIAN_POINT('Ctrl Pts',(9.45276276222877,-28.7191829359519,
123.93429039739));
#114170=CARTESIAN_POINT('Ctrl Pts',(9.45044779106971,-28.7420800491302,
123.907627359893));
#114171=CARTESIAN_POINT('Ctrl Pts',(9.44983821927761,-28.7481294795623,
123.90069986897));
#114172=CARTESIAN_POINT('Ctrl Pts',(9.44880971677453,-28.7583630566993,
123.889174928192));
#114173=CARTESIAN_POINT('Ctrl Pts',(9.44839303204895,-28.7625162569413,
123.884550035595));
#114174=CARTESIAN_POINT('Ctrl Pts',(9.44753432992432,-28.7710873037546,
123.87511233255));
#114175=CARTESIAN_POINT('Ctrl Pts',(9.44709213744048,-28.7755077153033,
123.870302111011));
#114176=CARTESIAN_POINT('Ctrl Pts',(9.44592030073135,-28.7872426498607,
123.85768213506));
#114177=CARTESIAN_POINT('Ctrl Pts',(9.44518726799707,-28.7946041801413,
123.849916786776));
#114178=CARTESIAN_POINT('Ctrl Pts',(9.44191822389892,-28.8275469582656,
123.815830651404));
#114179=CARTESIAN_POINT('Ctrl Pts',(9.43933119501081,-28.8539173218618,
123.790290438666));
#114180=CARTESIAN_POINT('Ctrl Pts',(9.42914507243602,-28.9596135366402,
123.694481166278));
#114181=CARTESIAN_POINT('Ctrl Pts',(9.42134135126428,-29.0447287841113,
123.630970901488));
#114182=CARTESIAN_POINT('Ctrl Pts',(9.40777103491111,-29.2056163465733,
123.533276402163));
#114183=CARTESIAN_POINT('Ctrl Pts',(9.40195325074701,-29.2790071232635,
123.495840289644));
#114184=CARTESIAN_POINT('Ctrl Pts',(9.39498164264185,-29.3729336953591,
123.456391397641));
#114185=CARTESIAN_POINT('Ctrl Pts',(9.39365185614205,-29.3911259752948,
123.449125360777));
#114186=CARTESIAN_POINT('Ctrl Pts',(9.39153712379415,-29.4204917834884,
123.437993005859));
#114187=CARTESIAN_POINT('Ctrl Pts',(9.39074541017417,-29.4315851936955,
123.433922018805));
#114188=CARTESIAN_POINT('Ctrl Pts',(9.38924216635695,-29.4528344412019,
123.426379647442));
#114189=CARTESIAN_POINT('Ctrl Pts',(9.38852998602496,-29.4629822968068,
123.422887715356));
#114190=CARTESIAN_POINT('Ctrl Pts',(9.38689823119501,-29.4864144897609,
123.415076965411));
#114191=CARTESIAN_POINT('Ctrl Pts',(9.38598094467362,-29.4997209358332,
123.410826636408));
#114192=CARTESIAN_POINT('Ctrl Pts',(9.38307267387077,-29.5423190467943,
123.397808082202));
#114193=CARTESIAN_POINT('Ctrl Pts',(9.38110232824733,-29.5718002799732,
123.389678297914));
#114194=CARTESIAN_POINT('Ctrl Pts',(9.37644857239736,-29.642719189676,123.372207193458));
#114195=CARTESIAN_POINT('Ctrl Pts',(9.3737876965006,-29.6843233715002,123.363629735032));
#114196=CARTESIAN_POINT('Ctrl Pts',(9.36658171166315,-29.7989784721036,
123.344527787625));
#114197=CARTESIAN_POINT('Ctrl Pts',(9.36210454696657,-29.8724712589146,
123.337250863823));
#114198=CARTESIAN_POINT('Ctrl Pts',(9.35676857231092,-29.959659213745,123.334434078629));
#114199=CARTESIAN_POINT('Ctrl Pts',(9.35594402320497,-29.9731185752571,
123.334162492568));
#114200=CARTESIAN_POINT('Ctrl Pts',(9.35057190384155,-30.0605995332203,
123.333457772531));
#114201=CARTESIAN_POINT('Ctrl Pts',(9.34597195985089,-30.1345678489389,
123.33779543764));
#114202=CARTESIAN_POINT('Ctrl Pts',(9.34033630074149,-30.2201707949272,
123.348566839258));
#114203=CARTESIAN_POINT('Ctrl Pts',(9.33952823014974,-30.2323315150685,
123.350233741198));
#114204=CARTESIAN_POINT('Ctrl Pts',(9.33825167019404,-30.2513426124542,
123.353053998569));
#114205=CARTESIAN_POINT('Ctrl Pts',(9.33778806013631,-30.2582063648558,
123.354116131301));
#114206=CARTESIAN_POINT('Ctrl Pts',(9.33691594499232,-30.2710375217351,
123.35618392687));
#114207=CARTESIAN_POINT('Ctrl Pts',(9.3365080131288,-30.2770063484849,123.357179225034));
#114208=CARTESIAN_POINT('Ctrl Pts',(9.33554219669211,-30.2910623881309,
123.359601839103));
#114209=CARTESIAN_POINT('Ctrl Pts',(9.33498282827726,-30.2991446201065,
123.361056459406));
#114210=CARTESIAN_POINT('Ctrl Pts',(9.333100012791,-30.3261649799327,123.366126037049));
#114211=CARTESIAN_POINT('Ctrl Pts',(9.33176305338781,-30.3450502734016,
123.370009831118));
#114212=CARTESIAN_POINT('Ctrl Pts',(9.3284356778858,-30.3914140428957,123.380386424095));
#114213=CARTESIAN_POINT('Ctrl Pts',(9.32643073005886,-30.4188025074075,
123.38725161038));
#114214=CARTESIAN_POINT('Ctrl Pts',(9.31725632167081,-30.5421739020631,
123.421530302263));
#114215=CARTESIAN_POINT('Ctrl Pts',(9.30991534878841,-30.6357493821585,
123.456840167597));
#114216=CARTESIAN_POINT('Ctrl Pts',(9.29673260043725,-30.8003028269684,
123.536457087596));
#114217=CARTESIAN_POINT('Ctrl Pts',(9.29086212744621,-30.8722075629032,
123.578134961831));
#114218=CARTESIAN_POINT('Ctrl Pts',(9.28383875660147,-30.9569084544208,
123.636083893992));
#114219=CARTESIAN_POINT('Ctrl Pts',(9.28250673464296,-30.9729047650104,
123.64744785325));
#114220=CARTESIAN_POINT('Ctrl Pts',(9.2803888512693,-30.9982186861673,123.66611267322));
#114221=CARTESIAN_POINT('Ctrl Pts',(9.27959620221406,-31.0076653179181,
123.673234547663));
#114222=CARTESIAN_POINT('Ctrl Pts',(9.2780914076956,-31.025542395378,123.687013270293));
#114223=CARTESIAN_POINT('Ctrl Pts',(9.27737860923445,-31.0339858475429,
123.693652177482));
#114224=CARTESIAN_POINT('Ctrl Pts',(9.275745726344,-31.0532666418938,123.709116314394));
#114225=CARTESIAN_POINT('Ctrl Pts',(9.274827928131,-31.0640584155899,123.717997263415));
#114226=CARTESIAN_POINT('Ctrl Pts',(9.27191901945845,-31.0981000399246,
123.746737394697));
#114227=CARTESIAN_POINT('Ctrl Pts',(9.26994852185422,-31.1209163030937,
123.767101916279));
#114228=CARTESIAN_POINT('Ctrl Pts',(9.26529460691424,-31.1740465702702,
123.817217941104));
#114229=CARTESIAN_POINT('Ctrl Pts',(9.26263368789692,-31.2038092043832,
123.847523307756));
#114230=CARTESIAN_POINT('Ctrl Pts',(9.25543144447707,-31.2819757327842,
123.933451474673));
#114231=CARTESIAN_POINT('Ctrl Pts',(9.2509577468347,-31.3278973198496,123.991200411082));
#114232=CARTESIAN_POINT('Ctrl Pts',(9.2456057615673,-31.3776860342753,124.063129131166));
#114233=CARTESIAN_POINT('Ctrl Pts',(9.24476165889348,-31.3853868652131,
124.074554668351));
#114234=CARTESIAN_POINT('Ctrl Pts',(9.23939448547394,-31.4333197340001,
124.147610774164));
#114235=CARTESIAN_POINT('Ctrl Pts',(9.23481904682353,-31.4695673785132,
124.211747610035));
#114236=CARTESIAN_POINT('Ctrl Pts',(9.22921055783351,-31.5067734932096,
124.289127006863));
#114237=CARTESIAN_POINT('Ctrl Pts',(9.22840217872281,-31.5119717115942,
124.300251263814));
#114238=CARTESIAN_POINT('Ctrl Pts',(9.22712493159828,-31.5199192813636,
124.317761260788));
#114239=CARTESIAN_POINT('Ctrl Pts',(9.22666093853779,-31.5227525474073,
124.324108740897));
#114240=CARTESIAN_POINT('Ctrl Pts',(9.22578823132324,-31.5279791158545,
124.336017711999));
#114241=CARTESIAN_POINT('Ctrl Pts',(9.22538009188315,-31.5303819303747,
124.341574757637));
#114242=CARTESIAN_POINT('Ctrl Pts',(9.22441366196081,-31.5359747770561,
124.354705477475));
#114243=CARTESIAN_POINT('Ctrl Pts',(9.22385388600149,-31.5391391169627,
124.362289793001));
#114244=CARTESIAN_POINT('Ctrl Pts',(9.22196833959125,-31.5495517990776,
124.387775990224));
#114245=CARTESIAN_POINT('Ctrl Pts',(9.22062900664261,-31.5565446294652,
124.405779709907));
#114246=CARTESIAN_POINT('Ctrl Pts',(9.21729441983968,-31.5730086491381,
124.450454112424));
#114247=CARTESIAN_POINT('Ctrl Pts',(9.21528456002422,-31.5821160283495,
124.477251891612));
#114248=CARTESIAN_POINT('Ctrl Pts',(9.20606642334074,-31.6203960571586,
124.600071562395));
#114249=CARTESIAN_POINT('Ctrl Pts',(9.19868545122572,-31.6415390275105,
124.698377334602));
#114250=CARTESIAN_POINT('Ctrl Pts',(9.1855137419008,-31.6636920637042,124.879727323645));
#114251=CARTESIAN_POINT('Ctrl Pts',(9.17969015143798,-31.6676043530301,
124.962102909666));
#114252=CARTESIAN_POINT('Ctrl Pts',(9.17271225983601,-31.6648843659895,
125.064032142613));
#114253=CARTESIAN_POINT('Ctrl Pts',(9.17138176776003,-31.6640159353249,
125.083612745987));
#114254=CARTESIAN_POINT('Ctrl Pts',(9.16926582094754,-31.6620699455326,
125.114975194841));
#114255=CARTESIAN_POINT('Ctrl Pts',(9.16847359734726,-31.661212090601,125.126768299615));
#114256=CARTESIAN_POINT('Ctrl Pts',(9.16696931233731,-31.6593356193819,
125.149253588732));
#114257=CARTESIAN_POINT('Ctrl Pts',(9.16625660116129,-31.658339021785,125.159946958506));
#114258=CARTESIAN_POINT('Ctrl Pts',(9.16462350646613,-31.655807256875,125.184536630692));
#114259=CARTESIAN_POINT('Ctrl Pts',(9.16370541409725,-31.6542004209905,
125.198424864662));
#114260=CARTESIAN_POINT('Ctrl Pts',(9.16079391990177,-31.6485182629067,
125.242653209634));
#114261=CARTESIAN_POINT('Ctrl Pts',(9.15882119412287,-31.6437813747341,
125.27290295694));
#114262=CARTESIAN_POINT('Ctrl Pts',(9.15416095088509,-31.6304788127535,
125.344823618399));
#114263=CARTESIAN_POINT('Ctrl Pts',(9.15149602891097,-31.6211456337839,
125.386331077069));
#114264=CARTESIAN_POINT('Ctrl Pts',(9.14428942280601,-31.5913215126241,
125.498683700995));
#114265=CARTESIAN_POINT('Ctrl Pts',(9.13981526786953,-31.5677012878763,
125.568597068817));
#114266=CARTESIAN_POINT('Ctrl Pts',(9.13445109923829,-31.5341903013582,
125.649623905231));
#114267=CARTESIAN_POINT('Ctrl Pts',(9.13359539420121,-31.5286899816869,
125.662463608741));
#114268=CARTESIAN_POINT('Ctrl Pts',(9.12822988086904,-31.4932880070493,
125.742314961656));
#114269=CARTESIAN_POINT('Ctrl Pts',(9.12366753319143,-31.4591511726609,
125.80735104298));
#114270=CARTESIAN_POINT('Ctrl Pts',(9.11807355409343,-31.4144346422765,
125.88038705076));
#114271=CARTESIAN_POINT('Ctrl Pts',(9.11726532568212,-31.4079089687935,
125.890785625307));
#114272=CARTESIAN_POINT('Ctrl Pts',(9.11598836799763,-31.3975105639601,
125.906955629354));
#114273=CARTESIAN_POINT('Ctrl Pts',(9.11552451437639,-31.3937154673444,
125.912776797311));
#114274=CARTESIAN_POINT('Ctrl Pts',(9.11465206218794,-31.3865468481967,
125.923623556525));
#114275=CARTESIAN_POINT('Ctrl Pts',(9.11424403813389,-31.3831822127602,
125.92865472488));
#114276=CARTESIAN_POINT('Ctrl Pts',(9.1132779456481,-31.3751865206967,125.94047090122));
#114277=CARTESIAN_POINT('Ctrl Pts',(9.11271839285482,-31.3705326132634,
125.94724011299));
#114278=CARTESIAN_POINT('Ctrl Pts',(9.11083406479607,-31.3547780050052,
125.969796377645));
#114279=CARTESIAN_POINT('Ctrl Pts',(9.10949574629724,-31.3434535369851,
125.985424259676));
#114280=CARTESIAN_POINT('Ctrl Pts',(9.10616416475786,-31.3148762880254,
126.023452812909));
#114281=CARTESIAN_POINT('Ctrl Pts',(9.10415632369449,-31.2973201302102,
126.045617335541));
#114282=CARTESIAN_POINT('Ctrl Pts',(9.09495578448027,-31.2150584476086,
126.144209722006));
#114283=CARTESIAN_POINT('Ctrl Pts',(9.08759083604433,-31.1441066983528,
126.21515564163));
#114284=CARTESIAN_POINT('Ctrl Pts',(9.07441425822697,-31.0037799005452,
126.33221838848));
#114285=CARTESIAN_POINT('Ctrl Pts',(9.06857146151652,-30.9364915102122,
126.38035041791));
#114286=CARTESIAN_POINT('Ctrl Pts',(9.06157511407242,-30.8491509219734,
126.433486328067));
#114287=CARTESIAN_POINT('Ctrl Pts',(9.06024413815668,-30.8322231672953,
126.443379713669));
#114288=CARTESIAN_POINT('Ctrl Pts',(9.05812767127939,-30.8048117235281,
126.458757657672));
#114289=CARTESIAN_POINT('Ctrl Pts',(9.05733540338543,-30.7944378455855,
126.46443311084));
#114290=CARTESIAN_POINT('Ctrl Pts',(9.05583118930943,-30.7745299231472,
126.47505074231));
#114291=CARTESIAN_POINT('Ctrl Pts',(9.05511859180318,-30.7650068464543,
126.480012104115));
#114292=CARTESIAN_POINT('Ctrl Pts',(9.05348597866258,-30.7429811213187,
126.491217736126));
#114293=CARTESIAN_POINT('Ctrl Pts',(9.05256825105334,-30.730446430936,126.497397513828));
#114294=CARTESIAN_POINT('Ctrl Pts',(9.04965885607282,-30.6902354266995,
126.516596999777));
#114295=CARTESIAN_POINT('Ctrl Pts',(9.04768782563769,-30.6622767929369,
126.529013094004));
#114296=CARTESIAN_POINT('Ctrl Pts',(9.04303234529681,-30.5947098508056,
126.556817415281));
#114297=CARTESIAN_POINT('Ctrl Pts',(9.04037042920156,-30.5548233946614,
126.571474355906));
#114298=CARTESIAN_POINT('Ctrl Pts',(9.03316567933843,-30.4442925020958,
126.607356845071));
#114299=CARTESIAN_POINT('Ctrl Pts',(9.02869056061395,-30.3727314978194,
126.62544254042));
#114300=CARTESIAN_POINT('Ctrl Pts',(9.02333971540549,-30.2866961602502,
126.641203826451));
#114301=CARTESIAN_POINT('Ctrl Pts',(9.022498226784,-30.2731546356077,126.643511858074));
#114302=CARTESIAN_POINT('Ctrl Pts',(9.01712959590003,-30.1868139379441,
126.657131295132));
#114303=CARTESIAN_POINT('Ctrl Pts',(9.01255003170936,-30.1133691972112,
126.663769290262));
#114304=CARTESIAN_POINT('Ctrl Pts',(9.00693696281334,-30.027463160572,126.66581886804));
#114305=CARTESIAN_POINT('Ctrl Pts',(9.00612871172942,-30.0151871692735,
126.665976006561));
#114306=CARTESIAN_POINT('Ctrl Pts',(9.00485174531684,-29.9959621186229,
126.666009598637));
#114307=CARTESIAN_POINT('Ctrl Pts',(9.00438790659187,-29.9890133767509,
126.665978264256));
#114308=CARTESIAN_POINT('Ctrl Pts',(9.00351545960601,-29.9760125771056,
126.665838300057));
#114309=CARTESIAN_POINT('Ctrl Pts',(9.003107425652,-29.9699606533227,126.665740157217));
#114310=CARTESIAN_POINT('Ctrl Pts',(9.0021413106944,-29.9556964194323,126.665431079037));
#114311=CARTESIAN_POINT('Ctrl Pts',(9.00158174520495,-29.9474849864777,
126.665192377042));
#114312=CARTESIAN_POINT('Ctrl Pts',(8.99969748271359,-29.9199906239966,
126.664189567124));
#114313=CARTESIAN_POINT('Ctrl Pts',(8.99835924538192,-29.9007200598256,
126.663151174646));
#114314=CARTESIAN_POINT('Ctrl Pts',(8.99502795234815,-29.8532752075023,
126.659767150037));
#114315=CARTESIAN_POINT('Ctrl Pts',(8.99302032323471,-29.8251347733289,
126.657038662555));
#114316=CARTESIAN_POINT('Ctrl Pts',(8.98382188715087,-29.6977154067481,
126.641402399791));
#114317=CARTESIAN_POINT('Ctrl Pts',(8.97645890361031,-29.5996537396147,
126.6202781039));
#114318=CARTESIAN_POINT('Ctrl Pts',(8.96327727135493,-29.4251281942028,
126.565860126711));
#114319=CARTESIAN_POINT('Ctrl Pts',(8.95742785399945,-29.3481088389755,
126.535394789005));
#114320=CARTESIAN_POINT('Ctrl Pts',(8.95042765424983,-29.2560471219849,
126.490796152483));
#114321=CARTESIAN_POINT('Ctrl Pts',(8.94909896203622,-29.2385845019613,
126.481953288398));
#114322=CARTESIAN_POINT('Ctrl Pts',(8.94698517657294,-29.2108334308248,
126.467280407598));
#114323=CARTESIAN_POINT('Ctrl Pts',(8.94619333879618,-29.2004446155483,
126.461645260682));
#114324=CARTESIAN_POINT('Ctrl Pts',(8.94468935663384,-29.1807302927506,
126.450678636941));
#114325=CARTESIAN_POINT('Ctrl Pts',(8.94397656697666,-29.1713947079991,
126.445366610994));
#114326=CARTESIAN_POINT('Ctrl Pts',(8.94234268517443,-29.1500182190073,
126.432928023052));
#114327=CARTESIAN_POINT('Ctrl Pts',(8.94142389195574,-29.1380143048349,
126.425739256799));
#114328=CARTESIAN_POINT('Ctrl Pts',(8.93850761017328,-29.0999862349143,
126.402309580254));
#114329=CARTESIAN_POINT('Ctrl Pts',(8.93653089643965,-29.0743185702054,
126.385500276577));
#114330=CARTESIAN_POINT('Ctrl Pts',(8.93185913279897,-29.0141084881935,
126.343649076758));
#114331=CARTESIAN_POINT('Ctrl Pts',(8.92918683710026,-28.9800346423822,
126.31797039676));
#114332=CARTESIAN_POINT('Ctrl Pts',(8.92200100880832,-28.8902056538236,
126.244701031015));
#114333=CARTESIAN_POINT('Ctrl Pts',(8.91755341277782,-28.8365448712948,
126.194695220975));
#114334=CARTESIAN_POINT('Ctrl Pts',(8.9122688064988,-28.7773653248804,126.131765195463));
#114335=CARTESIAN_POINT('Ctrl Pts',(8.91146544165359,-28.7684937983376,
126.122105376911));
#114336=CARTESIAN_POINT('Ctrl Pts',(8.90609014291122,-28.7100458568767,
126.056935844696));
#114337=CARTESIAN_POINT('Ctrl Pts',(8.90146615293136,-28.6641290480692,
125.998269026665));
#114338=CARTESIAN_POINT('Ctrl Pts',(8.8958037174643,-28.6153879818003,125.926583169957));
#114339=CARTESIAN_POINT('Ctrl Pts',(8.89499523942802,-28.6085957710182,
125.916352040206));
#114340=CARTESIAN_POINT('Ctrl Pts',(8.89371795615981,-28.5981376803837,
125.9002146091));
#114341=CARTESIAN_POINT('Ctrl Pts',(8.89325402995178,-28.594394451634,125.894358621373));
#114342=CARTESIAN_POINT('Ctrl Pts',(8.89238148360055,-28.5874599118728,
125.883359009665));
#114343=CARTESIAN_POINT('Ctrl Pts',(8.89197343850685,-28.584259850916,125.878221194301));
#114344=CARTESIAN_POINT('Ctrl Pts',(8.89100735056332,-28.5767831340685,
125.866069991195));
#114345=CARTESIAN_POINT('Ctrl Pts',(8.89044782392765,-28.5725302735253,
125.859042286531));
#114346=CARTESIAN_POINT('Ctrl Pts',(8.88856383190261,-28.5584624455144,
125.835402756564));
#114347=CARTESIAN_POINT('Ctrl Pts',(8.88722583127268,-28.5488845276075,
125.818652608353));
#114348=CARTESIAN_POINT('Ctrl Pts',(8.88389525848572,-28.525999143992,125.776966057176));
#114349=CARTESIAN_POINT('Ctrl Pts',(8.88188812044822,-28.5130314891505,
125.751850546977));
#114350=CARTESIAN_POINT('Ctrl Pts',(8.87594100326836,-28.4768414696524,
125.677156251079));
#114351=CARTESIAN_POINT('Ctrl Pts',(8.87195997478123,-28.4554367586926,
125.626790564402));
#114352=CARTESIAN_POINT('Ctrl Pts',(8.86798217145003,-28.4365601433851,
125.575510047478));
#114353=CARTESIAN_POINT('Origin',(5.,-30.,125.));
#114354=CARTESIAN_POINT('',(8.16626341820841,-28.4365599837785,125.575509613888));
#114355=CARTESIAN_POINT('',(8.36102756272879,-28.4365599800807,125.575509603842));
#114356=CARTESIAN_POINT('',(5.,-28.4365599837785,125.575509613888));
#114357=CARTESIAN_POINT('Ctrl Pts',(8.36102756272879,-28.4365599800807,
125.575509603842));
#114358=CARTESIAN_POINT('Ctrl Pts',(8.36145770696862,-28.4386070099079,
125.581070602881));
#114359=CARTESIAN_POINT('Ctrl Pts',(8.36188760913549,-28.4406839228182,
125.586621259518));
#114360=CARTESIAN_POINT('Ctrl Pts',(8.36819138196828,-28.4715968984599,
125.667913252586));
#114361=CARTESIAN_POINT('Ctrl Pts',(8.3739849424497,-28.5058953475837,125.741470545045));
#114362=CARTESIAN_POINT('Ctrl Pts',(8.38168331840411,-28.5600129458592,
125.838385065995));
#114363=CARTESIAN_POINT('Ctrl Pts',(8.3837357830561,-28.5753112481217,125.864126376972));
#114364=CARTESIAN_POINT('Ctrl Pts',(8.38670227849407,-28.598697583844,125.901165772368));
#114365=CARTESIAN_POINT('Ctrl Pts',(8.38763574447603,-28.6062455229821,
125.912796082803));
#114366=CARTESIAN_POINT('Ctrl Pts',(8.38928189758351,-28.6198897564361,
125.933256016873));
#114367=CARTESIAN_POINT('Ctrl Pts',(8.38999670869459,-28.6259277256678,
125.942123384479));
#114368=CARTESIAN_POINT('Ctrl Pts',(8.39149691209831,-28.6388369564555,
125.960693764744));
#114369=CARTESIAN_POINT('Ctrl Pts',(8.39228152708727,-28.6457273066304,
125.970382823967));
#114370=CARTESIAN_POINT('Ctrl Pts',(8.39436865484977,-28.6644230631664,
125.996085339622));
#114371=CARTESIAN_POINT('Ctrl Pts',(8.39566400793597,-28.6764127919527,
126.011962803471));
#114372=CARTESIAN_POINT('Ctrl Pts',(8.40340709727707,-28.7503497877074,
126.10631141169));
#114373=CARTESIAN_POINT('Ctrl Pts',(8.40957459561342,-28.8189757604072,
126.179294686223));
#114374=CARTESIAN_POINT('Ctrl Pts',(8.42058850569829,-28.9536663980121,
126.29890927781));
#114375=CARTESIAN_POINT('Ctrl Pts',(8.42544476690868,-29.0173510923646,
126.347731077068));
#114376=CARTESIAN_POINT('Ctrl Pts',(8.43230669257294,-29.1089407382553,
126.407991321287));
#114377=CARTESIAN_POINT('Ctrl Pts',(8.43417384748565,-29.1340087992832,
126.423546700542));
#114378=CARTESIAN_POINT('Ctrl Pts',(8.43735537156928,-29.1766599513997,
126.448469303392));
#114379=CARTESIAN_POINT('Ctrl Pts',(8.43865179517252,-29.1940225292612,
126.458201765976));
#114380=CARTESIAN_POINT('Ctrl Pts',(8.44051571475404,-29.2188803277021,
126.471556053164));
#114381=CARTESIAN_POINT('Ctrl Pts',(8.44106818664587,-29.2262354935232,
126.475436762904));
#114382=CARTESIAN_POINT('Ctrl Pts',(8.44202968137124,-29.2390069042951,
126.482053415615));
#114383=CARTESIAN_POINT('Ctrl Pts',(8.44243710258017,-29.244409552681,126.484815104019));
#114384=CARTESIAN_POINT('Ctrl Pts',(8.44331174683502,-29.2559862385061,
126.490653246658));
#114385=CARTESIAN_POINT('Ctrl Pts',(8.44377945191003,-29.2621642379322,
126.493720845059));
#114386=CARTESIAN_POINT('Ctrl Pts',(8.44506982522805,-29.2791796717585,
126.502038303693));
#114387=CARTESIAN_POINT('Ctrl Pts',(8.44589701834114,-29.2900550103824,
126.507209043946));
#114388=CARTESIAN_POINT('Ctrl Pts',(8.45102183791747,-29.3572903797278,
126.538287357102));
#114389=CARTESIAN_POINT('Ctrl Pts',(8.45546527715576,-29.414999519399,126.561145869374));
#114390=CARTESIAN_POINT('Ctrl Pts',(8.46974303275754,-29.6020544615563,
126.623408517052));
#114391=CARTESIAN_POINT('Ctrl Pts',(8.47965820117329,-29.7350088150674,
126.650335252346));
#114392=CARTESIAN_POINT('Ctrl Pts',(8.49150670112938,-29.9043325929816,
126.663612346825));
#114393=CARTESIAN_POINT('Ctrl Pts',(8.49389458874195,-29.9389788086658,
126.665243230035));
#114394=CARTESIAN_POINT('Ctrl Pts',(8.49717168016257,-29.9872360426982,
126.666006490485));
#114395=CARTESIAN_POINT('Ctrl Pts',(8.4980889041296,-30.0008215326724,126.666055187869));
#114396=CARTESIAN_POINT('Ctrl Pts',(8.49967283470738,-30.0244139784297,
126.665851168518));
#114397=CARTESIAN_POINT('Ctrl Pts',(8.50034187447292,-30.0344207015195,
126.665674452242));
#114398=CARTESIAN_POINT('Ctrl Pts',(8.5017362461051,-30.0553596647767,126.665115896981));
#114399=CARTESIAN_POINT('Ctrl Pts',(8.50246099746376,-30.0662909907093,
126.664716539569));
#114400=CARTESIAN_POINT('Ctrl Pts',(8.50418756080041,-30.0924411594482,
126.663503195412));
#114401=CARTESIAN_POINT('Ctrl Pts',(8.50518617047491,-30.1076544924927,
126.662587978036));
#114402=CARTESIAN_POINT('Ctrl Pts',(8.5086871853002,-30.161273441952,126.658623234945));
#114403=CARTESIAN_POINT('Ctrl Pts',(8.51115475382142,-30.1995853021649,
126.65445042986));
#114404=CARTESIAN_POINT('Ctrl Pts',(8.517324472727,-30.2962062008685,126.640521123376));
#114405=CARTESIAN_POINT('Ctrl Pts',(8.52097708010476,-30.3542048991576,
126.628983525005));
#114406=CARTESIAN_POINT('Ctrl Pts',(8.53143349804796,-30.5194756534759,
126.586859746785));
#114407=CARTESIAN_POINT('Ctrl Pts',(8.53812306285762,-30.6244340137254,
126.54856582347));
#114408=CARTESIAN_POINT('Ctrl Pts',(8.54695407241359,-30.7492968912502,
126.488237894541));
#114409=CARTESIAN_POINT('Ctrl Pts',(8.54871242000477,-30.7735256449567,
126.475789869132));
#114410=CARTESIAN_POINT('Ctrl Pts',(8.55113800532702,-30.805900510132,126.45814035454));
#114411=CARTESIAN_POINT('Ctrl Pts',(8.55177622972547,-30.8143238361179,
126.453452993632));
#114412=CARTESIAN_POINT('Ctrl Pts',(8.55279783590509,-30.8276465154202,
126.445887108063));
#114413=CARTESIAN_POINT('Ctrl Pts',(8.55317826351522,-30.832572790982,126.443056072724));
#114414=CARTESIAN_POINT('Ctrl Pts',(8.55398171053166,-30.8429011889788,
126.437050051014));
#114415=CARTESIAN_POINT('Ctrl Pts',(8.55440508917953,-30.8483000099712,
126.433869712394));
#114416=CARTESIAN_POINT('Ctrl Pts',(8.5554711854043,-30.8617885321296,126.425821051457));
#114417=CARTESIAN_POINT('Ctrl Pts',(8.55611629030951,-30.8698549398162,
126.420914324672));
#114418=CARTESIAN_POINT('Ctrl Pts',(8.55868225842405,-30.9015808691078,
126.401244326766));
#114419=CARTESIAN_POINT('Ctrl Pts',(8.56063261557264,-30.9249084335177,
126.385957393763));
#114420=CARTESIAN_POINT('Ctrl Pts',(8.56601614850504,-30.9874577232244,
126.342685381898));
#114421=CARTESIAN_POINT('Ctrl Pts',(8.56949274009445,-31.0258659620074,
126.313573463172));
#114422=CARTESIAN_POINT('Ctrl Pts',(8.58127918681224,-31.1508695917134,
126.20999596664));
#114423=CARTESIAN_POINT('Ctrl Pts',(8.58962954009622,-31.2310737857826,
126.128297093791));
#114424=CARTESIAN_POINT('Ctrl Pts',(8.60074104305059,-31.3295720190128,
126.004841848937));
#114425=CARTESIAN_POINT('Ctrl Pts',(8.6037714646891,-31.3554942382202,125.969590053118));
#114426=CARTESIAN_POINT('Ctrl Pts',(8.60786746237645,-31.389203368946,125.919749860271));
#114427=CARTESIAN_POINT('Ctrl Pts',(8.60897807989324,-31.3982042510058,
125.906008119057));
#114428=CARTESIAN_POINT('Ctrl Pts',(8.61075585636904,-31.412381248504,125.883649345891));
#114429=CARTESIAN_POINT('Ctrl Pts',(8.61142770806204,-31.417685001841,125.875114964341));
#114430=CARTESIAN_POINT('Ctrl Pts',(8.61282284294003,-31.4285835791482,
125.857218692879));
#114431=CARTESIAN_POINT('Ctrl Pts',(8.61354558812298,-31.4341643546033,
125.847848774036));
#114432=CARTESIAN_POINT('Ctrl Pts',(8.61525806876907,-31.4472282967277,
125.825416771546));
#114433=CARTESIAN_POINT('Ctrl Pts',(8.61624474050465,-31.4546273099731,
125.812306594301));
#114434=CARTESIAN_POINT('Ctrl Pts',(8.61965193810057,-31.4797153038824,
125.766411286217));
#114435=CARTESIAN_POINT('Ctrl Pts',(8.62204015231128,-31.4964824288276,
125.733133212663));
#114436=CARTESIAN_POINT('Ctrl Pts',(8.62795432106819,-31.535713954565,125.648303806195));
#114437=CARTESIAN_POINT('Ctrl Pts',(8.63143620982289,-31.5567115990926,
125.596124878231));
#114438=CARTESIAN_POINT('Ctrl Pts',(8.64146547144384,-31.6099530610728,
125.441686777283));
#114439=CARTESIAN_POINT('Ctrl Pts',(8.64789702667453,-31.6350176433205,
125.337268236808));
#114440=CARTESIAN_POINT('Ctrl Pts',(8.65683367474016,-31.6546591846119,
125.197088219706));
#114441=CARTESIAN_POINT('Ctrl Pts',(8.6590402273004,-31.6583774982597,125.162863370849));
#114442=CARTESIAN_POINT('Ctrl Pts',(8.66198709830412,-31.6618421828736,
125.118095422794));
#114443=CARTESIAN_POINT('Ctrl Pts',(8.66268009871064,-31.6625525854659,
125.107632970125));
#114444=CARTESIAN_POINT('Ctrl Pts',(8.66381059374463,-31.6635426584482,
125.090685956784));
#114445=CARTESIAN_POINT('Ctrl Pts',(8.6642448059996,-31.6638832965665,125.084205053423));
#114446=CARTESIAN_POINT('Ctrl Pts',(8.66510147008029,-31.6644776698322,
125.071478389391));
#114447=CARTESIAN_POINT('Ctrl Pts',(8.66552377080596,-31.6647341337085,
125.065232913471));
#114448=CARTESIAN_POINT('Ctrl Pts',(8.66658353726255,-31.6652870367743,
125.049626599976));
#114449=CARTESIAN_POINT('Ctrl Pts',(8.66722333292179,-31.6655396939478,
125.040264523982));
#114450=CARTESIAN_POINT('Ctrl Pts',(8.66974085755674,-31.6662191445097,
125.003638962121));
#114451=CARTESIAN_POINT('Ctrl Pts',(8.67164673455173,-31.6660554953507,
124.976370359353));
#114452=CARTESIAN_POINT('Ctrl Pts',(8.67686677678667,-31.6638016864866,
124.902606669074));
#114453=CARTESIAN_POINT('Ctrl Pts',(8.68022154841539,-31.6604323670643,
124.856176053179));
#114454=CARTESIAN_POINT('Ctrl Pts',(8.68858056675474,-31.6472905409691,
124.741725024608));
#114455=CARTESIAN_POINT('Ctrl Pts',(8.69360024140499,-31.6352453148678,
124.674047129665));
#114456=CARTESIAN_POINT('Ctrl Pts',(8.70469005641908,-31.5990268085286,
124.52472031556));
#114457=CARTESIAN_POINT('Ctrl Pts',(8.71070706558514,-31.572704481169,124.443778701327));
#114458=CARTESIAN_POINT('Ctrl Pts',(8.71787117024162,-31.5328192040067,
124.347000557882));
#114459=CARTESIAN_POINT('Ctrl Pts',(8.7192068155053,-31.5250016211873,124.328946278973));
#114460=CARTESIAN_POINT('Ctrl Pts',(8.72132909676774,-31.5119686888015,
124.300252251159));
#114461=CARTESIAN_POINT('Ctrl Pts',(8.72212257058555,-31.5069566563289,
124.289522782629));
#114462=CARTESIAN_POINT('Ctrl Pts',(8.72362810178253,-31.4971820201652,
124.269166692261));
#114463=CARTESIAN_POINT('Ctrl Pts',(8.72434082110673,-31.4924399209179,
124.259530948068));
#114464=CARTESIAN_POINT('Ctrl Pts',(8.72597235829699,-31.4813217974705,
124.237480167335));
#114465=CARTESIAN_POINT('Ctrl Pts',(8.72688890380039,-31.4748822248631,
124.225097938261));
#114466=CARTESIAN_POINT('Ctrl Pts',(8.72978896865646,-31.4538960487608,
124.185954574458));
#114467=CARTESIAN_POINT('Ctrl Pts',(8.73175205306949,-31.4387703709172,
124.159509856633));
#114468=CARTESIAN_POINT('Ctrl Pts',(8.73638448146635,-31.4009625006906,
124.097423950052));
#114469=CARTESIAN_POINT('Ctrl Pts',(8.73903161606981,-31.377633150419,124.062201124308));
#114470=CARTESIAN_POINT('Ctrl Pts',(8.74634984147412,-31.3087737864522,
123.966361124478));
#114471=CARTESIAN_POINT('Ctrl Pts',(8.75094660920688,-31.2604112096926,
123.907909299828));
#114472=CARTESIAN_POINT('Ctrl Pts',(8.75616197691216,-31.2017358639728,
123.84610396226));
#114473=CARTESIAN_POINT('Ctrl Pts',(8.756740416765,-31.1951768934233,123.839311693734));
#114474=CARTESIAN_POINT('Ctrl Pts',(8.76200330791184,-31.1350764746444,
123.778123160089));
#114475=CARTESIAN_POINT('Ctrl Pts',(8.76673908697932,-31.077920185203,123.72741731741));
#114476=CARTESIAN_POINT('Ctrl Pts',(8.7725261499066,-31.007766949544,123.673307559569));
#114477=CARTESIAN_POINT('Ctrl Pts',(8.77333526805991,-30.9979525769807,
123.665909415232));
#114478=CARTESIAN_POINT('Ctrl Pts',(8.77461342140452,-30.9824589323018,
123.65449682322));
#114479=CARTESIAN_POINT('Ctrl Pts',(8.77507756830051,-30.9768346165369,
123.650408032056));
#114480=CARTESIAN_POINT('Ctrl Pts',(8.77595041269201,-30.966265809128,123.642825346319));
#114481=CARTESIAN_POINT('Ctrl Pts',(8.77635853348204,-30.9613276566661,
123.639323041152));
#114482=CARTESIAN_POINT('Ctrl Pts',(8.77732466610054,-30.9496448243202,
123.631132520136));
#114483=CARTESIAN_POINT('Ctrl Pts',(8.77788416071585,-30.9428844415474,
123.626467185465));
#114484=CARTESIAN_POINT('Ctrl Pts',(8.77976750109632,-30.9201364819341,
123.61101591297));
#114485=CARTESIAN_POINT('Ctrl Pts',(8.78110486883277,-30.9039968209665,
123.600458072118));
#114486=CARTESIAN_POINT('Ctrl Pts',(8.78443339708765,-30.8637785118332,
123.575134974258));
#114487=CARTESIAN_POINT('Ctrl Pts',(8.78643910137207,-30.8395011064841,
123.560697609492));
#114488=CARTESIAN_POINT('Ctrl Pts',(8.7956196274884,-30.7277457099274,123.498028019629));
#114489=CARTESIAN_POINT('Ctrl Pts',(8.80296613486707,-30.6364048238903,
123.457105650151));
#114490=CARTESIAN_POINT('Ctrl Pts',(8.8161466944176,-30.4635686265864,123.397648489073));
#114491=CARTESIAN_POINT('Ctrl Pts',(8.82201005164917,-30.3832775355713,
123.376568971746));
#114492=CARTESIAN_POINT('Ctrl Pts',(8.82902649887282,-30.2824471380455,
123.357999870828));
#114493=CARTESIAN_POINT('Ctrl Pts',(8.83035830359465,-30.2630930625698,
123.354787883739));
#114494=CARTESIAN_POINT('Ctrl Pts',(8.83247592321245,-30.2319840472416,
123.350188091914));
#114495=CARTESIAN_POINT('Ctrl Pts',(8.83326852473787,-30.2202637135715,
123.348582475806));
#114496=CARTESIAN_POINT('Ctrl Pts',(8.83477327834336,-30.1978708635722,
123.345757429507));
#114497=CARTESIAN_POINT('Ctrl Pts',(8.83548608309976,-30.1872017630164,
123.34451612215));
#114498=CARTESIAN_POINT('Ctrl Pts',(8.83711904754025,-30.1626233001798,
123.341897166478));
#114499=CARTESIAN_POINT('Ctrl Pts',(8.83803691933775,-30.1487069903583,
123.340591191106));
#114500=CARTESIAN_POINT('Ctrl Pts',(8.8409463129405,-30.1042935960718,123.336986435659));
#114501=CARTESIAN_POINT('Ctrl Pts',(8.84291720362924,-30.0737479136646,
123.335352078473));
#114502=CARTESIAN_POINT('Ctrl Pts',(8.84757209503965,-30.0007176856076,
123.333458928047));
#114503=CARTESIAN_POINT('Ctrl Pts',(8.8502335747362,-29.9582339355169,123.333982102552));
#114504=CARTESIAN_POINT('Ctrl Pts',(8.85743770377063,-29.8421837670007,
123.339853813939));
#114505=CARTESIAN_POINT('Ctrl Pts',(8.86191263519807,-29.7688801425367,
123.348462746118));
#114506=CARTESIAN_POINT('Ctrl Pts',(8.86726034163982,-29.6829284990999,
123.364393374043));
#114507=CARTESIAN_POINT('Ctrl Pts',(8.86809888772666,-29.6695007055871,
123.367053711127));
#114508=CARTESIAN_POINT('Ctrl Pts',(8.87346749486712,-29.5839739241192,
123.385096566236));
#114509=CARTESIAN_POINT('Ctrl Pts',(8.8780499484194,-29.5129388937597,123.405083224761));
#114510=CARTESIAN_POINT('Ctrl Pts',(8.88366636573933,-29.43189618427,123.433805617918));
#114511=CARTESIAN_POINT('Ctrl Pts',(8.8844747809977,-29.4203681357607,123.438035317908));
#114512=CARTESIAN_POINT('Ctrl Pts',(8.88575204124957,-29.4023897340531,
123.444858114584));
#114513=CARTESIAN_POINT('Ctrl Pts',(8.88621600803788,-29.3959067982081,
123.447364913152));
#114514=CARTESIAN_POINT('Ctrl Pts',(8.88708871705689,-29.3838062349024,
123.452131172887));
#114515=CARTESIAN_POINT('Ctrl Pts',(8.88749688485231,-29.3781849939084,
123.454380785702));
#114516=CARTESIAN_POINT('Ctrl Pts',(8.88846337037872,-29.3649628894959,
123.459756054751));
#114517=CARTESIAN_POINT('Ctrl Pts',(8.88902317416903,-29.357372754441,123.462907368186));
#114518=CARTESIAN_POINT('Ctrl Pts',(8.89090852735885,-29.3320274878815,
123.473650888658));
#114519=CARTESIAN_POINT('Ctrl Pts',(8.89224763517326,-29.314381828731,123.481495297868));
#114520=CARTESIAN_POINT('Ctrl Pts',(8.89558141882648,-29.2712289204826,
123.501584459649));
#114521=CARTESIAN_POINT('Ctrl Pts',(8.89759069203603,-29.2458900926084,
123.514175486556));
#114522=CARTESIAN_POINT('Ctrl Pts',(8.90680243132826,-29.1322573003871,
123.574295837154));
#114523=CARTESIAN_POINT('Ctrl Pts',(8.91417742840122,-29.0480436727267,
123.629091772331));
#114524=CARTESIAN_POINT('Ctrl Pts',(8.92735212823738,-28.9044852908043,
123.742143564441));
#114525=CARTESIAN_POINT('Ctrl Pts',(8.93318399979611,-28.8435723673284,
123.797904286862));
#114526=CARTESIAN_POINT('Ctrl Pts',(8.94017018094361,-28.7735927445204,
123.872229806077));
#114527=CARTESIAN_POINT('Ctrl Pts',(8.94150120287582,-28.7604058538469,
123.886740472133));
#114528=CARTESIAN_POINT('Ctrl Pts',(8.94361794419042,-28.739678799933,123.910373290353));
#114529=CARTESIAN_POINT('Ctrl Pts',(8.9444104382666,-28.7319746775606,123.919348489172));
#114530=CARTESIAN_POINT('Ctrl Pts',(8.94591521416387,-28.7174568379781,
123.936630618989));
#114531=CARTESIAN_POINT('Ctrl Pts',(8.94662814636664,-28.7106266467982,
123.944922861496));
#114532=CARTESIAN_POINT('Ctrl Pts',(8.94826172465711,-28.6950910938163,
123.964160099813));
#114533=CARTESIAN_POINT('Ctrl Pts',(8.94918007843716,-28.6864422986704,
123.975149895211));
#114534=CARTESIAN_POINT('Ctrl Pts',(8.9520923738276,-28.6593008148525,124.0105459818));
#114535=CARTESIAN_POINT('Ctrl Pts',(8.95406562903356,-28.6413415073779,
124.035354547882));
#114536=CARTESIAN_POINT('Ctrl Pts',(8.95872726382163,-28.6000894251401,
124.095778755504));
#114537=CARTESIAN_POINT('Ctrl Pts',(8.96139303398346,-28.577456933059,124.131819557973));
#114538=CARTESIAN_POINT('Ctrl Pts',(8.96859914867215,-28.5194565331449,
124.232551293325));
#114539=CARTESIAN_POINT('Ctrl Pts',(8.97307208223782,-28.4869622831259,
124.298784123701));
#114540=CARTESIAN_POINT('Ctrl Pts',(8.97843591740039,-28.4536471547153,
124.379883592678));
#114541=CARTESIAN_POINT('Ctrl Pts',(8.97929248196261,-28.4484975178083,
124.392882612287));
#114542=CARTESIAN_POINT('Ctrl Pts',(8.98465558066968,-28.4173666473452,
124.474448806567));
#114543=CARTESIAN_POINT('Ctrl Pts',(8.98921465188718,-28.3957753455328,
124.544595864343));
#114544=CARTESIAN_POINT('Ctrl Pts',(8.99480513081464,-28.3760449815618,
124.627875181981));
#114545=CARTESIAN_POINT('Ctrl Pts',(8.99561353105724,-28.3733464392908,
124.639854260382));
#114546=CARTESIAN_POINT('Ctrl Pts',(8.9968908195505,-28.3693280228528,124.658659662157));
#114547=CARTESIAN_POINT('Ctrl Pts',(8.99735483134072,-28.3679179873674,
124.665466559286));
#114548=CARTESIAN_POINT('Ctrl Pts',(8.99822773302511,-28.3653591270608,
124.678220719373));
#114549=CARTESIAN_POINT('Ctrl Pts',(8.99863604950941,-28.3642000834639,
124.684165680641));
#114550=CARTESIAN_POINT('Ctrl Pts',(8.99960301584995,-28.3615439219884,
124.698196580603));
#114551=CARTESIAN_POINT('Ctrl Pts',(9.00016315392076,-28.3600742262815,
124.706287431088));
#114552=CARTESIAN_POINT('Ctrl Pts',(9.0020501190838,-28.3553508627016,124.733431391799));
#114553=CARTESIAN_POINT('Ctrl Pts',(9.00339052502644,-28.3523690250318,
124.752529398956));
#114554=CARTESIAN_POINT('Ctrl Pts',(9.00672814727556,-28.3458379487924,
124.799734265238));
#114555=CARTESIAN_POINT('Ctrl Pts',(9.0087399910164,-28.3426721571202,124.827887547695));
#114556=CARTESIAN_POINT('Ctrl Pts',(9.01797556390105,-28.3315398552732,
124.956295463057));
#114557=CARTESIAN_POINT('Ctrl Pts',(9.02537231383394,-28.33194321021,125.05706476187));
#114558=CARTESIAN_POINT('Ctrl Pts',(9.03853419354012,-28.3491703078742,
125.238841313797));
#114559=CARTESIAN_POINT('Ctrl Pts',(9.04433408946599,-28.3629297385434,
125.319825626506));
#114560=CARTESIAN_POINT('Ctrl Pts',(9.05128940886092,-28.3873006207887,
125.41849797493));
#114561=CARTESIAN_POINT('Ctrl Pts',(9.05261949376751,-28.3923337298054,
125.437434638829));
#114562=CARTESIAN_POINT('Ctrl Pts',(9.05473521130915,-28.4009388470119,
125.46765295942));
#114563=CARTESIAN_POINT('Ctrl Pts',(9.05552760338496,-28.404298886696,125.47899251657));
#114564=CARTESIAN_POINT('Ctrl Pts',(9.0570324786278,-28.4109418706488,125.50056541187));
#114565=CARTESIAN_POINT('Ctrl Pts',(9.05774560923411,-28.414203624293,125.510804594771));
#114566=CARTESIAN_POINT('Ctrl Pts',(9.05938006241585,-28.4219407943758,
125.534304209144));
#114567=CARTESIAN_POINT('Ctrl Pts',(9.06029908669143,-28.4264847238471,
125.547541359049));
#114568=CARTESIAN_POINT('Ctrl Pts',(9.06155524212669,-28.4329600900784,
125.565658398423));
#114569=CARTESIAN_POINT('Ctrl Pts',(9.06189689051117,-28.4347484306822,
125.570588315377));
#114570=CARTESIAN_POINT('Ctrl Pts',(9.06223779754793,-28.4365599835583,
125.57550961329));
#114571=CARTESIAN_POINT('',(8.82706574074257,-28.3340000603266,124.999551660593));
#114572=CARTESIAN_POINT('Ctrl Pts',(8.86798217145003,-28.4365601433851,
125.575510047478));
#114573=CARTESIAN_POINT('Ctrl Pts',(8.86185962239668,-28.4075056644279,
125.496580182371));
#114574=CARTESIAN_POINT('Ctrl Pts',(8.85575036351493,-28.3844406215789,
125.415482508081));
#114575=CARTESIAN_POINT('Ctrl Pts',(8.84633165537642,-28.3578042058915,
125.284872792836));
#114576=CARTESIAN_POINT('Ctrl Pts',(8.84292409524228,-28.3501319539516,
125.236422943428));
#114577=CARTESIAN_POINT('Ctrl Pts',(8.83842238551622,-28.3426894408775,
125.170785037085));
#114578=CARTESIAN_POINT('Ctrl Pts',(8.83727034630692,-28.341030750582,125.153840453454));
#114579=CARTESIAN_POINT('Ctrl Pts',(8.83536839463526,-28.3387051589693,
125.125629325156));
#114580=CARTESIAN_POINT('Ctrl Pts',(8.83461397978074,-28.3378925069161,
125.114376432987));
#114581=CARTESIAN_POINT('Ctrl Pts',(8.83319044802623,-28.3365686097304,
125.093027798251));
#114582=CARTESIAN_POINT('Ctrl Pts',(8.83252065816331,-28.3360348207541,
125.082934017713));
#114583=CARTESIAN_POINT('Ctrl Pts',(8.83106752375674,-28.3350720243024,
125.060932680886));
#114584=CARTESIAN_POINT('Ctrl Pts',(8.83028532486699,-28.3346788267911,
125.049024056637));
#114585=CARTESIAN_POINT('Ctrl Pts',(8.82868900352269,-28.3341344862232,
125.024594036931));
#114586=CARTESIAN_POINT('Ctrl Pts',(8.82787533746247,-28.3339966906545,
125.012073141787));
#114587=CARTESIAN_POINT('Ctrl Pts',(8.82706574074257,-28.3340000603266,
124.999551660593));
#114588=CARTESIAN_POINT('Ctrl Pts',(8.82706582501452,-28.3340000599764,
124.99955296397));
#114589=CARTESIAN_POINT('Ctrl Pts',(8.82552293670077,-28.3340064630552,
124.975690169399));
#114590=CARTESIAN_POINT('Ctrl Pts',(8.82399512451827,-28.3345255587479,
124.951829175653));
#114591=CARTESIAN_POINT('Ctrl Pts',(8.8139693057654,-28.3413530734983,124.794025566948));
#114592=CARTESIAN_POINT('Ctrl Pts',(8.80595594332984,-28.3632988322378,
124.661259729756));
#114593=CARTESIAN_POINT('Ctrl Pts',(8.79398870050104,-28.4177504440931,
124.474985621226));
#114594=CARTESIAN_POINT('Ctrl Pts',(8.79023980714995,-28.4376750408818,
124.41837042761));
#114595=CARTESIAN_POINT('Ctrl Pts',(8.78536234457686,-28.4663889185449,
124.348984026802));
#114596=CARTESIAN_POINT('Ctrl Pts',(8.78437087525542,-28.4723619244685,
124.335089015429));
#114597=CARTESIAN_POINT('Ctrl Pts',(8.78287427379261,-28.4815625950485,
124.314464068068));
#114598=CARTESIAN_POINT('Ctrl Pts',(8.78237725978755,-28.4846478491526,
124.307670945061));
#114599=CARTESIAN_POINT('Ctrl Pts',(8.78147543525583,-28.4902968726483,
124.295451575151));
#114600=CARTESIAN_POINT('Ctrl Pts',(8.78107159982884,-28.49284447342,124.290018147171));
#114601=CARTESIAN_POINT('Ctrl Pts',(8.78015718461895,-28.4986532435748,
124.277801578143));
#114602=CARTESIAN_POINT('Ctrl Pts',(8.7796456288921,-28.5019310283025,124.271026753521));
#114603=CARTESIAN_POINT('Ctrl Pts',(8.77807525536332,-28.5120820218852,
124.25040336544));
#114604=CARTESIAN_POINT('Ctrl Pts',(8.77700815827029,-28.5191019771699,
124.236628512749));
#114605=CARTESIAN_POINT('Ctrl Pts',(8.76863194953328,-28.5752199948783,
124.130199253173));
#114606=CARTESIAN_POINT('Ctrl Pts',(8.76094569801021,-28.6327712984183,
124.04227682885));
#114607=CARTESIAN_POINT('Ctrl Pts',(8.74537603323542,-28.7664233159057,
123.874923256554));
#114608=CARTESIAN_POINT('Ctrl Pts',(8.73754138196926,-28.8429040124052,
123.79640292199));
#114609=CARTESIAN_POINT('Ctrl Pts',(8.72899729874516,-28.9381855270799,
123.716123894898));
#114610=CARTESIAN_POINT('Ctrl Pts',(8.72795953209783,-28.9499637290812,
123.706473160498));
#114611=CARTESIAN_POINT('Ctrl Pts',(8.72598517823142,-28.9727626091331,
123.688309030333));
#114612=CARTESIAN_POINT('Ctrl Pts',(8.72504761257469,-28.9837609029819,
123.679769726437));
#114613=CARTESIAN_POINT('Ctrl Pts',(8.7233970517507,-29.0034237573007,123.664894400473));
#114614=CARTESIAN_POINT('Ctrl Pts',(8.72268188913507,-29.0120447906744,
123.658502447624));
#114615=CARTESIAN_POINT('Ctrl Pts',(8.72118373294742,-29.0303151053736,
123.645227818769));
#114616=CARTESIAN_POINT('Ctrl Pts',(8.72040148920367,-29.0399773118707,
123.638363885468));
#114617=CARTESIAN_POINT('Ctrl Pts',(8.71832728964169,-29.0659178584358,
123.620349380235));
#114618=CARTESIAN_POINT('Ctrl Pts',(8.71704233780558,-29.0823227321151,
123.609383674257));
#114619=CARTESIAN_POINT('Ctrl Pts',(8.7104526164313,-29.1681057082518,123.554222010733));
#114620=CARTESIAN_POINT('Ctrl Pts',(8.70532934453711,-29.2404965211612,
123.514914469575));
#114621=CARTESIAN_POINT('Ctrl Pts',(8.69411968592561,-29.4068882977375,
123.439928897928));
#114622=CARTESIAN_POINT('Ctrl Pts',(8.6880926206815,-29.50179762959,123.407079603888));
#114623=CARTESIAN_POINT('Ctrl Pts',(8.68003620877506,-29.6265301752924,
123.376153855184));
#114624=CARTESIAN_POINT('Ctrl Pts',(8.67824311719694,-29.6541508031264,
123.370047802957));
#114625=CARTESIAN_POINT('Ctrl Pts',(8.67517530208143,-29.700862167431,123.36096209351));
#114626=CARTESIAN_POINT('Ctrl Pts',(8.67391691030504,-29.7198741584461,
123.35760597397));
#114627=CARTESIAN_POINT('Ctrl Pts',(8.67209848650151,-29.747053801267,123.353293673558));
#114628=CARTESIAN_POINT('Ctrl Pts',(8.67155250820096,-29.7551776472432,
123.352066289686));
#114629=CARTESIAN_POINT('Ctrl Pts',(8.67059847890346,-29.769301739739,123.350039105652));
#114630=CARTESIAN_POINT('Ctrl Pts',(8.67019195752396,-29.7752978053332,
123.349211835961));
#114631=CARTESIAN_POINT('Ctrl Pts',(8.66931468778569,-29.7881870900808,
123.347505044789));
#114632=CARTESIAN_POINT('Ctrl Pts',(8.66884341385409,-29.7950812388545,
123.346635979969));
#114633=CARTESIAN_POINT('Ctrl Pts',(8.66753335845075,-29.8141684803774,
123.344351087112));
#114634=CARTESIAN_POINT('Ctrl Pts',(8.66668983160653,-29.8263718078877,
123.343026884577));
#114635=CARTESIAN_POINT('Ctrl Pts',(8.66078865563074,-29.9112203821212,
123.334767402788));
#114636=CARTESIAN_POINT('Ctrl Pts',(8.65553002066224,-29.9842309334713,
123.332477766137));
#114637=CARTESIAN_POINT('Ctrl Pts',(8.64288099834985,-30.1582473398906,
123.338450412223));
#114638=CARTESIAN_POINT('Ctrl Pts',(8.63548791381896,-30.2588318271421,
123.35112189794));
#114639=CARTESIAN_POINT('Ctrl Pts',(8.62457909681576,-30.4092647338153,
123.384187167215));
#114640=CARTESIAN_POINT('Ctrl Pts',(8.62090051317587,-30.4603142394905,
123.397982339724));
#114641=CARTESIAN_POINT('Ctrl Pts',(8.616140548432,-30.5268040293666,123.419391775582));
#114642=CARTESIAN_POINT('Ctrl Pts',(8.61499049166957,-30.5429013245915,
123.42484825068));
#114643=CARTESIAN_POINT('Ctrl Pts',(8.61309090891086,-30.5695351975844,
123.434333112344));
#114644=CARTESIAN_POINT('Ctrl Pts',(8.61233690392399,-30.5801190980823,
123.438223771718));
#114645=CARTESIAN_POINT('Ctrl Pts',(8.61086399930962,-30.6008134435513,
123.446070448043));
#114646=CARTESIAN_POINT('Ctrl Pts',(8.61014487534427,-30.610926313427,123.450018420937));
#114647=CARTESIAN_POINT('Ctrl Pts',(8.60841344476983,-30.6352912295891,
123.459805776321));
#114648=CARTESIAN_POINT('Ctrl Pts',(8.60740452813876,-30.6495024668347,
123.465744556872));
#114649=CARTESIAN_POINT('Ctrl Pts',(8.60398822907375,-30.6976404115853,
123.486649828974));
#114650=CARTESIAN_POINT('Ctrl Pts',(8.6016124394286,-30.7311503151428,123.502552030318));
#114651=CARTESIAN_POINT('Ctrl Pts',(8.59088850788345,-30.8818178038314,
123.580316482313));
#114652=CARTESIAN_POINT('Ctrl Pts',(8.58297964008849,-30.9918606323425,
123.654891688397));
#114653=CARTESIAN_POINT('Ctrl Pts',(8.57220093315785,-31.1236541146117,
123.769258812822));
#114654=CARTESIAN_POINT('Ctrl Pts',(8.56957720492188,-31.154341771547,123.797994574212));
#114655=CARTESIAN_POINT('Ctrl Pts',(8.56526531006402,-31.2018386734637,
123.845968240012));
#114656=CARTESIAN_POINT('Ctrl Pts',(8.56361585415679,-31.2193502032082,
123.864486718003));
#114657=CARTESIAN_POINT('Ctrl Pts',(8.56133529690855,-31.2425515427887,
123.89017789152));
#114658=CARTESIAN_POINT('Ctrl Pts',(8.56072975989833,-31.2486180747974,
123.897007550888));
#114659=CARTESIAN_POINT('Ctrl Pts',(8.55970611857505,-31.2587096693473,
123.90855854209));
#114660=CARTESIAN_POINT('Ctrl Pts',(8.5592902130915,-31.2627651945177,123.913253226494));
#114661=CARTESIAN_POINT('Ctrl Pts',(8.55843070622539,-31.2710523731426,
123.922955504012));
#114662=CARTESIAN_POINT('Ctrl Pts',(8.5579869098732,-31.2752808161903,123.927965570644));
#114663=CARTESIAN_POINT('Ctrl Pts',(8.55680691887714,-31.2863933945528,
123.941291082138));
#114664=CARTESIAN_POINT('Ctrl Pts',(8.55606725849165,-31.2932263310104,
123.949648544672));
#114665=CARTESIAN_POINT('Ctrl Pts',(8.55272065672722,-31.3235702235797,
123.987507547628));
#114666=CARTESIAN_POINT('Ctrl Pts',(8.55005981193214,-31.3461545558332,
124.017733983163));
#114667=CARTESIAN_POINT('Ctrl Pts',(8.53983105719722,-31.4278908573883,
124.135246671807));
#114668=CARTESIAN_POINT('Ctrl Pts',(8.53206803216505,-31.4797384613907,
124.227313033232));
#114669=CARTESIAN_POINT('Ctrl Pts',(8.52051604782475,-31.5448063504319,
124.373790739904));
#114670=CARTESIAN_POINT('Ctrl Pts',(8.51661011256681,-31.5645866171088,
124.424991831235));
#114671=CARTESIAN_POINT('Ctrl Pts',(8.51103072563614,-31.5896603680191,
124.500838622117));
#114672=CARTESIAN_POINT('Ctrl Pts',(8.50929887529829,-31.5969786858944,
124.524772309841));
#114673=CARTESIAN_POINT('Ctrl Pts',(8.50617920746973,-31.6093064321642,
124.568596437648));
#114674=CARTESIAN_POINT('Ctrl Pts',(8.50478607108701,-31.6144929945769,
124.588431461658));
#114675=CARTESIAN_POINT('Ctrl Pts',(8.50259508822357,-31.6221367611784,
124.620035947924));
#114676=CARTESIAN_POINT('Ctrl Pts',(8.5017895976725,-31.6248348184241,124.631744411082));
#114677=CARTESIAN_POINT('Ctrl Pts',(8.50027456753053,-31.6296953744908,
124.653931461807));
#114678=CARTESIAN_POINT('Ctrl Pts',(8.49956422553636,-31.6318840430296,
124.664403626383));
#114679=CARTESIAN_POINT('Ctrl Pts',(8.49795625940507,-31.6366310732582,
124.688262212454));
#114680=CARTESIAN_POINT('Ctrl Pts',(8.49706067837911,-31.6391263787626,
124.701660510648));
#114681=CARTESIAN_POINT('Ctrl Pts',(8.49472928081337,-31.6452278498938,
124.73681281002));
#114682=CARTESIAN_POINT('Ctrl Pts',(8.49330184338597,-31.6485671119436,
124.758610843183));
#114683=CARTESIAN_POINT('Ctrl Pts',(8.48473219217271,-31.6661604373065,
124.890961061172));
#114684=CARTESIAN_POINT('Ctrl Pts',(8.4779341523219,-31.6697235097824,125.002650670489));
#114685=CARTESIAN_POINT('Ctrl Pts',(8.46681184918821,-31.6572749674427,
125.184357105146));
#114686=CARTESIAN_POINT('Ctrl Pts',(8.4624980195575,-31.6479671603043,125.254461620818));
#114687=CARTESIAN_POINT('Ctrl Pts',(8.45654042125751,-31.6296255397651,
125.347044887742));
#114688=CARTESIAN_POINT('Ctrl Pts',(8.45502601485619,-31.6245152515883,
125.370229166802));
#114689=CARTESIAN_POINT('Ctrl Pts',(8.45239121013011,-31.6149057962378,
125.40978434658));
#114690=CARTESIAN_POINT('Ctrl Pts',(8.45128174588971,-31.6106484358086,
125.426210632598));
#114691=CARTESIAN_POINT('Ctrl Pts',(8.44964215357477,-31.6040666987849,
125.450096663259));
#114692=CARTESIAN_POINT('Ctrl Pts',(8.4491225770084,-31.6019394062509,125.457610219579));
#114693=CARTESIAN_POINT('Ctrl Pts',(8.44823581653339,-31.5982403949592,
125.470333121899));
#114694=CARTESIAN_POINT('Ctrl Pts',(8.4478701943089,-31.5966958480847,125.475550179448));
#114695=CARTESIAN_POINT('Ctrl Pts',(8.44703279875574,-31.5931147039456,
125.487432155117));
#114696=CARTESIAN_POINT('Ctrl Pts',(8.44656011987035,-31.5910618745412,
125.494091765476));
#114697=CARTESIAN_POINT('Ctrl Pts',(8.44524243188948,-31.5852508900668,
125.5125314725));
#114698=CARTESIAN_POINT('Ctrl Pts',(8.44439259132426,-31.5814033638846,
125.524282626921));
#114699=CARTESIAN_POINT('Ctrl Pts',(8.43787001537452,-31.5510942786992,
125.613482754506));
#114700=CARTESIAN_POINT('Ctrl Pts',(8.43194553276739,-31.5190911362583,
125.688922152097));
#114701=CARTESIAN_POINT('Ctrl Pts',(8.42576263423915,-31.4802346283364,
125.764507317313));
#114702=CARTESIAN_POINT('Ctrl Pts',(8.42553261645292,-31.478781331009,125.767314647441));
#114703=CARTESIAN_POINT('Ctrl Pts',(8.42036077280776,-31.4459293078638,
125.830334812944));
#114704=CARTESIAN_POINT('Ctrl Pts',(8.41541389751153,-31.4108845771325,
125.888579233453));
#114705=CARTESIAN_POINT('Ctrl Pts',(8.40717200905783,-31.34567703784,125.983324932337));
#114706=CARTESIAN_POINT('Ctrl Pts',(8.4038380267175,-31.3173376050465,126.020978406953));
#114707=CARTESIAN_POINT('Ctrl Pts',(8.39826772126613,-31.2665284780896,
126.082842090486));
#114708=CARTESIAN_POINT('Ctrl Pts',(8.39600375305034,-31.2448670212946,
126.107676732343));
#114709=CARTESIAN_POINT('Ctrl Pts',(8.39279521128459,-31.2127156672078,
126.142402448857));
#114710=CARTESIAN_POINT('Ctrl Pts',(8.39182641095768,-31.2028130528618,
126.152824109311));
#114711=CARTESIAN_POINT('Ctrl Pts',(8.39014036328775,-31.1852409873848,
126.170844269367));
#114712=CARTESIAN_POINT('Ctrl Pts',(8.38942062880467,-31.1776303920657,
126.178498693424));
#114713=CARTESIAN_POINT('Ctrl Pts',(8.38793130047828,-31.1616566632953,
126.194255148347));
#114714=CARTESIAN_POINT('Ctrl Pts',(8.3871622811226,-31.1532818811087,126.202344575004));
#114715=CARTESIAN_POINT('Ctrl Pts',(8.38516464951079,-31.13120143802,126.223229677761));
#114716=CARTESIAN_POINT('Ctrl Pts',(8.38394212636076,-31.1173631253853,
126.235883178226));
#114717=CARTESIAN_POINT('Ctrl Pts',(8.37839671643114,-31.0531544979173,
126.292634128942));
#114718=CARTESIAN_POINT('Ctrl Pts',(8.37418970793322,-31.0003655186899,
126.333906948898));
#114719=CARTESIAN_POINT('Ctrl Pts',(8.36295581817705,-30.8508071343742,
126.436952156236));
#114720=CARTESIAN_POINT('Ctrl Pts',(8.35610045906975,-30.7499261126979,
126.492083246674));
#114721=CARTESIAN_POINT('Ctrl Pts',(8.34705591980557,-30.6165818596045,
126.547991926128));
#114722=CARTESIAN_POINT('Ctrl Pts',(8.34516208627364,-30.5886684558691,
126.558820526579));
#114723=CARTESIAN_POINT('Ctrl Pts',(8.34193984248377,-30.541537474199,126.575657890066));
#114724=CARTESIAN_POINT('Ctrl Pts',(8.34062998071377,-30.5224747480987,
126.582081120766));
#114725=CARTESIAN_POINT('Ctrl Pts',(8.33875014869806,-30.4953425455757,
126.590679561886));
#114726=CARTESIAN_POINT('Ctrl Pts',(8.33819555479961,-30.4873649934236,
126.593141883801));
#114727=CARTESIAN_POINT('Ctrl Pts',(8.33723174466375,-30.4735554231775,
126.597290867606));
#114728=CARTESIAN_POINT('Ctrl Pts',(8.33682415486096,-30.4677321314326,
126.599005786909));
#114729=CARTESIAN_POINT('Ctrl Pts',(8.33595078186691,-30.4552921359627,
126.602595508025));
#114730=CARTESIAN_POINT('Ctrl Pts',(8.33548453244945,-30.4486732571209,
126.604461154245));
#114731=CARTESIAN_POINT('Ctrl Pts',(8.3342016428989,-30.4305167608695,126.609457746696));
#114732=CARTESIAN_POINT('Ctrl Pts',(8.33338055829408,-30.4189569526958,
126.612505494897));
#114733=CARTESIAN_POINT('Ctrl Pts',(8.32844967808664,-30.3498399263896,
126.629934871194));
#114734=CARTESIAN_POINT('Ctrl Pts',(8.32420638531486,-30.2915861159059,
126.64135666306));
#114735=CARTESIAN_POINT('Ctrl Pts',(8.3124039159444,-30.1300562869054,126.664157245159));
#114736=CARTESIAN_POINT('Ctrl Pts',(8.30478438900738,-30.0261175441198,
126.669028062859));
#114737=CARTESIAN_POINT('Ctrl Pts',(8.29440852544147,-29.8807623930906,
126.662250227872));
#114738=CARTESIAN_POINT('Ctrl Pts',(8.29147189746632,-29.8392101024742,
126.658746669104));
#114739=CARTESIAN_POINT('Ctrl Pts',(8.28648713322641,-29.7678857257353,
126.650026977369));
#114740=CARTESIAN_POINT('Ctrl Pts',(8.28441851695031,-29.7380448280005,
126.64555332789));
#114741=CARTESIAN_POINT('Ctrl Pts',(8.28143359034581,-29.6946528216197,
126.637837710602));
#114742=CARTESIAN_POINT('Ctrl Pts',(8.28049749407267,-29.6809961659564,
126.635232656175));
#114743=CARTESIAN_POINT('Ctrl Pts',(8.27884857909498,-29.6568602126853,
126.63031475525));
#114744=CARTESIAN_POINT('Ctrl Pts',(8.27813360795498,-29.6463678081762,
126.62807106632));
#114745=CARTESIAN_POINT('Ctrl Pts',(8.27663492649095,-29.6243217382988,
126.623133563683));
#114746=CARTESIAN_POINT('Ctrl Pts',(8.27585197495847,-29.6127736569231,
126.620417382449));
#114747=CARTESIAN_POINT('Ctrl Pts',(8.27377370492735,-29.5820480380202,
126.612843295144));
#114748=CARTESIAN_POINT('Ctrl Pts',(8.27248544026783,-29.5629259874137,
126.607766680447));
#114749=CARTESIAN_POINT('Ctrl Pts',(8.26533875559389,-29.4565354583767,
126.57748309987));
#114750=CARTESIAN_POINT('Ctrl Pts',(8.25970675943806,-29.3713474206997,
126.545511438966));
#114751=CARTESIAN_POINT('Ctrl Pts',(8.24843378544306,-29.2049260288125,
126.467001142149));
#114752=CARTESIAN_POINT('Ctrl Pts',(8.24281433605841,-29.1241582531405,
126.420258450694));
#114753=CARTESIAN_POINT('Ctrl Pts',(8.23441941445586,-29.0144255121978,
126.343817671257));
#114754=CARTESIAN_POINT('Ctrl Pts',(8.23183010945709,-28.9819870817916,
126.319413547021));
#114755=CARTESIAN_POINT('Ctrl Pts',(8.22846711326601,-28.942169566976,126.287115045455));
#114756=CARTESIAN_POINT('Ctrl Pts',(8.22776070308026,-28.9339295688024,
126.280298475448));
#114757=CARTESIAN_POINT('Ctrl Pts',(8.22661379182093,-28.9207618367548,
126.269190166702));
#114758=CARTESIAN_POINT('Ctrl Pts',(8.22617675178774,-28.9157925776939,
126.264947806824));
#114759=CARTESIAN_POINT('Ctrl Pts',(8.22532448641645,-28.9061989371415,
126.256659456414));
#114760=CARTESIAN_POINT('Ctrl Pts',(8.22490950596848,-28.9015717771517,
126.252616936301));
#114761=CARTESIAN_POINT('Ctrl Pts',(8.2239724693165,-28.8912200668231,126.243471700029));
#114762=CARTESIAN_POINT('Ctrl Pts',(8.22344940399404,-28.8855081814775,
126.238354872295));
#114763=CARTESIAN_POINT('Ctrl Pts',(8.22159070833133,-28.865438307072,126.220124535378));
#114764=CARTESIAN_POINT('Ctrl Pts',(8.22024101243933,-28.8512754051141,
126.206799834927));
#114765=CARTESIAN_POINT('Ctrl Pts',(8.21132992198955,-28.7602258823685,
126.118083778963));
#114766=CARTESIAN_POINT('Ctrl Pts',(8.20341412264587,-28.6905741590765,
126.035641207627));
#114767=CARTESIAN_POINT('Ctrl Pts',(8.18941166089258,-28.5808753524287,
125.876879753582));
#114768=CARTESIAN_POINT('Ctrl Pts',(8.18330323894413,-28.5378390236045,
125.803070198172));
#114769=CARTESIAN_POINT('Ctrl Pts',(8.17530625105535,-28.4875743270153,
125.699301885762));
#114770=CARTESIAN_POINT('Ctrl Pts',(8.17325108324174,-28.4752364448803,
125.6719753311));
#114771=CARTESIAN_POINT('Ctrl Pts',(8.17028164887843,-28.4582784058146,
125.63154006513));
#114772=CARTESIAN_POINT('Ctrl Pts',(8.16934788677825,-28.4530745996968,
125.618684211802));
#114773=CARTESIAN_POINT('Ctrl Pts',(8.16770159193498,-28.4441321197757,
125.595773585964));
#114774=CARTESIAN_POINT('Ctrl Pts',(8.16698693047251,-28.440328942492,125.585745019665));
#114775=CARTESIAN_POINT('Ctrl Pts',(8.16627145758177,-28.4366018553033,
125.575623353271));
#114776=CARTESIAN_POINT('Ctrl Pts',(8.16626743784335,-28.436580917989,125.57556648415));
#114777=CARTESIAN_POINT('Ctrl Pts',(8.16626341820841,-28.4365599837785,
125.575509613888));
#114778=CARTESIAN_POINT('Origin',(5.,-30.,125.));
#114779=CARTESIAN_POINT('',(7.46828914249572,-28.4365600390074,125.575509763924));
#114780=CARTESIAN_POINT('',(7.65924494691568,-28.4365599837121,125.575509613707));
#114781=CARTESIAN_POINT('',(5.,-28.4365599837785,125.575509613888));
#114782=CARTESIAN_POINT('Ctrl Pts',(7.65924494691568,-28.4365599837121,
125.575509613707));
#114783=CARTESIAN_POINT('Ctrl Pts',(7.66000437687175,-28.4406054932687,
125.586499719479));
#114784=CARTESIAN_POINT('Ctrl Pts',(7.66076922565613,-28.4447668020627,
125.597446945435));
#114785=CARTESIAN_POINT('Ctrl Pts',(7.66215647700585,-28.4524612023065,
125.617063437286));
#114786=CARTESIAN_POINT('Ctrl Pts',(7.66277660823055,-28.4559524641237,
125.625748202422));
#114787=CARTESIAN_POINT('Ctrl Pts',(7.66381792132597,-28.4618964043691,
125.640181525617));
#114788=CARTESIAN_POINT('Ctrl Pts',(7.66423673220792,-28.4643086518056,
125.645946698855));
#114789=CARTESIAN_POINT('Ctrl Pts',(7.66504125856129,-28.4689822593511,
125.656942271152));
#114790=CARTESIAN_POINT('Ctrl Pts',(7.66542661388327,-28.4712381138844,
125.662174873351));
#114791=CARTESIAN_POINT('Ctrl Pts',(7.66647392120915,-28.4774167327331,
125.676306719916));
#114792=CARTESIAN_POINT('Ctrl Pts',(7.66713883665129,-28.4813905789815,
125.685183187278));
#114793=CARTESIAN_POINT('Ctrl Pts',(7.66972642803558,-28.4970601637743,
125.719378684095));
#114794=CARTESIAN_POINT('Ctrl Pts',(7.67167815781493,-28.5093125957213,
125.744435818369));
#114795=CARTESIAN_POINT('Ctrl Pts',(7.68151928548853,-28.5734708238799,
125.867703271747));
#114796=CARTESIAN_POINT('Ctrl Pts',(7.68970708961808,-28.6344781316498,
125.960855783906));
#114797=CARTESIAN_POINT('Ctrl Pts',(7.70197988037505,-28.7412590674603,
126.092970378632));
#114798=CARTESIAN_POINT('Ctrl Pts',(7.7061785023585,-28.7806157559364,126.136712898359));
#114799=CARTESIAN_POINT('Ctrl Pts',(7.71212159124836,-28.8406942322164,
126.196766241463));
#114800=CARTESIAN_POINT('Ctrl Pts',(7.71393329980538,-28.8596150626884,
126.214809295234));
#114801=CARTESIAN_POINT('Ctrl Pts',(7.71718130508527,-28.8946409844701,
126.246670434491));
#114802=CARTESIAN_POINT('Ctrl Pts',(7.7186236199752,-28.9105999999297,126.260640090308));
#114803=CARTESIAN_POINT('Ctrl Pts',(7.72087357102241,-28.9361278205838,
126.282138838925));
#114804=CARTESIAN_POINT('Ctrl Pts',(7.7216895657369,-28.9455193633209,126.289873876349));
#114805=CARTESIAN_POINT('Ctrl Pts',(7.72321400907695,-28.9633122119621,
126.30420415486));
#114806=CARTESIAN_POINT('Ctrl Pts',(7.72392337402123,-28.9716937855505,
126.310822789633));
#114807=CARTESIAN_POINT('Ctrl Pts',(7.72551554159998,-28.9907331496529,
126.325562500279));
#114808=CARTESIAN_POINT('Ctrl Pts',(7.72639646404369,-29.0014265145047,
126.333636580506));
#114809=CARTESIAN_POINT('Ctrl Pts',(7.72866192503662,-29.0293285735346,
126.354180399429));
#114810=CARTESIAN_POINT('Ctrl Pts',(7.73003886593481,-29.0466808411547,
126.366451689241));
#114811=CARTESIAN_POINT('Ctrl Pts',(7.7409594064645,-29.187286200686,126.461903418399));
#114812=CARTESIAN_POINT('Ctrl Pts',(7.74983288404353,-29.3209286143421,
126.528570914357));
#114813=CARTESIAN_POINT('Ctrl Pts',(7.76277512159135,-29.5197027483694,
126.596444099852));
#114814=CARTESIAN_POINT('Ctrl Pts',(7.76660500095504,-29.5788013268332,
126.613043486413));
#114815=CARTESIAN_POINT('Ctrl Pts',(7.77157981327122,-29.6535932176645,
126.629660065105));
#114816=CARTESIAN_POINT('Ctrl Pts',(7.77258148058685,-29.6685572380419,
126.632769194257));
#114817=CARTESIAN_POINT('Ctrl Pts',(7.77409057973926,-29.6909182437501,
126.63709517713));
#114818=CARTESIAN_POINT('Ctrl Pts',(7.77458969599311,-29.6982845737826,
126.638468781275));
#114819=CARTESIAN_POINT('Ctrl Pts',(7.77549373189191,-29.7115684346454,
126.640853213922));
#114820=CARTESIAN_POINT('Ctrl Pts',(7.77589765335625,-29.7174825042249,
126.641881816439));
#114821=CARTESIAN_POINT('Ctrl Pts',(7.77681024290389,-29.7307965028565,
126.644123384841));
#114822=CARTESIAN_POINT('Ctrl Pts',(7.77731986480762,-29.7381990743511,
126.645318357439));
#114823=CARTESIAN_POINT('Ctrl Pts',(7.77887788073116,-29.7607395687476,
126.648801030067));
#114824=CARTESIAN_POINT('Ctrl Pts',(7.77993437047395,-29.7759007061343,
126.650929997241));
#114825=CARTESIAN_POINT('Ctrl Pts',(7.78847933956808,-29.8977055023577,
126.666325494422));
#114826=CARTESIAN_POINT('Ctrl Pts',(7.79636454579978,-30.0053676162317,
126.669452772226));
#114827=CARTESIAN_POINT('Ctrl Pts',(7.81188321619623,-30.2184360115704,
126.655022786106));
#114828=CARTESIAN_POINT('Ctrl Pts',(7.81948051818708,-30.3233897372144,
126.637754883678));
#114829=CARTESIAN_POINT('Ctrl Pts',(7.82823765499373,-30.4467600627743,
126.605123817649));
#114830=CARTESIAN_POINT('Ctrl Pts',(7.8296983865248,-30.4674104259716,126.599232500944));
#114831=CARTESIAN_POINT('Ctrl Pts',(7.83197032956753,-30.4996277824114,
126.589363850631));
#114832=CARTESIAN_POINT('Ctrl Pts',(7.83279017451538,-30.5112740880835,
126.585655760655));
#114833=CARTESIAN_POINT('Ctrl Pts',(7.83431808891986,-30.5330123233518,
126.578470073101));
#114834=CARTESIAN_POINT('Ctrl Pts',(7.83502711655958,-30.543113611665,126.575023022818));
#114835=CARTESIAN_POINT('Ctrl Pts',(7.83661372121867,-30.5657432301982,
126.567057099743));
#114836=CARTESIAN_POINT('Ctrl Pts',(7.8374894748619,-30.5782519976698,126.562484560147));
#114837=CARTESIAN_POINT('Ctrl Pts',(7.83973201163526,-30.6103158649109,
126.550325912969));
#114838=CARTESIAN_POINT('Ctrl Pts',(7.84109145927099,-30.6297853127081,
126.54251950204));
#114839=CARTESIAN_POINT('Ctrl Pts',(7.85071025735473,-30.7675865123462,
126.484222948799));
#114840=CARTESIAN_POINT('Ctrl Pts',(7.85848751998315,-30.8798661069955,
126.420544315833));
#114841=CARTESIAN_POINT('Ctrl Pts',(7.87148636541487,-31.0513226072828,
126.295104554463));
#114842=CARTESIAN_POINT('Ctrl Pts',(7.87664729544417,-31.1151021462972,
126.240612190912));
#114843=CARTESIAN_POINT('Ctrl Pts',(7.88301531431186,-31.1844898286138,
126.171639041958));
#114844=CARTESIAN_POINT('Ctrl Pts',(7.8839396881213,-31.1943478660608,126.161588283968));
#114845=CARTESIAN_POINT('Ctrl Pts',(7.88535454869376,-31.2090905776309,
126.146171278649));
#114846=CARTESIAN_POINT('Ctrl Pts',(7.88583816855855,-31.214069792629,126.140895770265));
#114847=CARTESIAN_POINT('Ctrl Pts',(7.88672741656866,-31.2231120765137,
126.131189192866));
#114848=CARTESIAN_POINT('Ctrl Pts',(7.88713222824153,-31.2271858215076,
126.126768431189));
#114849=CARTESIAN_POINT('Ctrl Pts',(7.88806423387845,-31.2364680019656,
126.11658551333));
#114850=CARTESIAN_POINT('Ctrl Pts',(7.88859258235956,-31.2416601150417,
126.11080893098));
#114851=CARTESIAN_POINT('Ctrl Pts',(7.89022755541026,-31.2575188109682,
126.092914931793));
#114852=CARTESIAN_POINT('Ctrl Pts',(7.89134320069149,-31.2680494545389,
126.080679018488));
#114853=CARTESIAN_POINT('Ctrl Pts',(7.89779499688969,-31.3273880940981,
126.009669891017));
#114854=CARTESIAN_POINT('Ctrl Pts',(7.90332903467554,-31.3722811430271,
125.947752432297));
#114855=CARTESIAN_POINT('Ctrl Pts',(7.91550006698255,-31.4609421525688,
125.805895369061));
#114856=CARTESIAN_POINT('Ctrl Pts',(7.92212219944983,-31.5027352138685,
125.724988980278));
#114857=CARTESIAN_POINT('Ctrl Pts',(7.93233305350001,-31.5581957147618,
125.591957370601));
#114858=CARTESIAN_POINT('Ctrl Pts',(7.93603780869256,-31.5763081381189,
125.5418866475));
#114859=CARTESIAN_POINT('Ctrl Pts',(7.94082573787058,-31.5970154400235,
125.474750368841));
#114860=CARTESIAN_POINT('Ctrl Pts',(7.94197860831124,-31.6017867418814,
125.458394480075));
#114861=CARTESIAN_POINT('Ctrl Pts',(7.94388171486389,-31.60930065671,125.431085586249));
#114862=CARTESIAN_POINT('Ctrl Pts',(7.94463646168098,-31.6121842311618,
125.420173061941));
#114863=CARTESIAN_POINT('Ctrl Pts',(7.94611002326954,-31.6176229532318,
125.398710164754));
#114864=CARTESIAN_POINT('Ctrl Pts',(7.94682907005252,-31.6201863206409,
125.3881624791));
#114865=CARTESIAN_POINT('Ctrl Pts',(7.94855898392565,-31.6261319955883,
125.362611692892));
#114866=CARTESIAN_POINT('Ctrl Pts',(7.94956647928676,-31.6294100417488,
125.347585167669));
#114867=CARTESIAN_POINT('Ctrl Pts',(7.95297067585508,-31.6398471340722,
125.2963443465));
#114868=CARTESIAN_POINT('Ctrl Pts',(7.95533610573655,-31.6460108411502,
125.259936959417));
#114869=CARTESIAN_POINT('Ctrl Pts',(7.96531081243936,-31.6671504769284,
125.103678655359));
#114870=CARTESIAN_POINT('Ctrl Pts',(7.97256764901129,-31.670280963747,124.982601434739));
#114871=CARTESIAN_POINT('Ctrl Pts',(7.98305894509792,-31.6561609203659,
124.812418379638));
#114872=CARTESIAN_POINT('Ctrl Pts',(7.9861577038636,-31.6497860554771,124.762805698741));
#114873=CARTESIAN_POINT('Ctrl Pts',(7.99115473589603,-31.6362799452474,
124.685421298988));
#114874=CARTESIAN_POINT('Ctrl Pts',(7.99299747899562,-31.6306466453361,
124.657417008517));
#114875=CARTESIAN_POINT('Ctrl Pts',(7.9955033767907,-31.6221794629302,124.620288960294));
#114876=CARTESIAN_POINT('Ctrl Pts',(7.99613402677024,-31.619982614706,124.611023135585));
#114877=CARTESIAN_POINT('Ctrl Pts',(7.99718809379577,-31.6162047844782,
124.595676409116));
#114878=CARTESIAN_POINT('Ctrl Pts',(7.99760901319832,-31.6146685763034,
124.589584530164));
#114879=CARTESIAN_POINT('Ctrl Pts',(7.99846598969639,-31.6114862086979,
124.577259223798));
#114880=CARTESIAN_POINT('Ctrl Pts',(7.99890213248015,-31.6098382609255,
124.571026417159));
#114881=CARTESIAN_POINT('Ctrl Pts',(8.00003959029246,-31.6054661577713,
124.554870460968));
#114882=CARTESIAN_POINT('Ctrl Pts',(8.00074395204116,-31.6026862138655,
124.544962884227));
#114883=CARTESIAN_POINT('Ctrl Pts',(8.00369842596939,-31.5907183554662,
124.50378066051));
#114884=CARTESIAN_POINT('Ctrl Pts',(8.00598857808518,-31.5807059464587,
124.47275537061));
#114885=CARTESIAN_POINT('Ctrl Pts',(8.0151938016667,-31.537375166918,124.350845152625));
#114886=CARTESIAN_POINT('Ctrl Pts',(8.0223044474517,-31.4970744495799,124.262645456113));
#114887=CARTESIAN_POINT('Ctrl Pts',(8.03396386060595,-31.4177073146066,
124.122629857593));
#114888=CARTESIAN_POINT('Ctrl Pts',(8.03856192451762,-31.3828681528981,
124.068683991876));
#114889=CARTESIAN_POINT('Ctrl Pts',(8.04591207161824,-31.3210041081768,
123.984048353026));
#114890=CARTESIAN_POINT('Ctrl Pts',(8.04872170209543,-31.2958120642838,
123.952106308627));
#114891=CARTESIAN_POINT('Ctrl Pts',(8.05254195012938,-31.2594097257565,
123.909273324487));
#114892=CARTESIAN_POINT('Ctrl Pts',(8.05359138800184,-31.2491797150288,
123.89757194974));
#114893=CARTESIAN_POINT('Ctrl Pts',(8.05537152884012,-31.2314366506489,
123.87784108989));
#114894=CARTESIAN_POINT('Ctrl Pts',(8.05610557031029,-31.2240052778759,
123.869739882231));
#114895=CARTESIAN_POINT('Ctrl Pts',(8.05749757399433,-31.2096955902363,
123.854447038344));
#114896=CARTESIAN_POINT('Ctrl Pts',(8.05815611827572,-31.2028319954567,
123.847242346812));
#114897=CARTESIAN_POINT('Ctrl Pts',(8.05969135825602,-31.1866139799571,
123.830520920362));
#114898=CARTESIAN_POINT('Ctrl Pts',(8.0605658108241,-31.1772088669591,123.821054133674));
#114899=CARTESIAN_POINT('Ctrl Pts',(8.06359536363938,-31.144052615423,123.788472894193));
#114900=CARTESIAN_POINT('Ctrl Pts',(8.06572493619712,-31.1197254532927,
123.765954028922));
#114901=CARTESIAN_POINT('Ctrl Pts',(8.07749848007033,-30.9799485525973,
123.644106237465));
#114902=CARTESIAN_POINT('Ctrl Pts',(8.08650217796176,-30.8519889151635,
123.560257356629));
#114903=CARTESIAN_POINT('Ctrl Pts',(8.09804410529499,-30.6846874278325,
123.480841452316));
#114904=CARTESIAN_POINT('Ctrl Pts',(8.1001190462817,-30.6545400475449,123.467610809832));
#114905=CARTESIAN_POINT('Ctrl Pts',(8.10361637507494,-30.60406152731,123.447218902795));
#114906=CARTESIAN_POINT('Ctrl Pts',(8.10501588074681,-30.5839472294856,
123.439543338569));
#114907=CARTESIAN_POINT('Ctrl Pts',(8.10700231137587,-30.5556238076518,
123.429359468825));
#114908=CARTESIAN_POINT('Ctrl Pts',(8.10757141894178,-30.5475345268512,
123.426521233759));
#114909=CARTESIAN_POINT('Ctrl Pts',(8.1085520634946,-30.5336470861384,123.421768690094));
#114910=CARTESIAN_POINT('Ctrl Pts',(8.10896182186858,-30.5278595287723,
123.419823555145));
#114911=CARTESIAN_POINT('Ctrl Pts',(8.10983015602446,-30.5156298130903,
123.415787967065));
#114912=CARTESIAN_POINT('Ctrl Pts',(8.11028911923891,-30.5091854915316,
123.413704945302));
#114913=CARTESIAN_POINT('Ctrl Pts',(8.11155262025018,-30.491493708333,123.408105277584));
#114914=CARTESIAN_POINT('Ctrl Pts',(8.11236149926928,-30.4802216033861,
123.404668666235));
#114915=CARTESIAN_POINT('Ctrl Pts',(8.1167573412069,-30.4192038931694,123.386770990382));
#114916=CARTESIAN_POINT('Ctrl Pts',(8.12044612402867,-30.3688451313495,
123.374517941011));
#114917=CARTESIAN_POINT('Ctrl Pts',(8.13130096307024,-30.2210730302732,
123.34578314236));
#114918=CARTESIAN_POINT('Ctrl Pts',(8.1385553547343,-30.122657798709,123.335589232585));
#114919=CARTESIAN_POINT('Ctrl Pts',(8.1491802482279,-29.974661944702,123.333464566189));
#114920=CARTESIAN_POINT('Ctrl Pts',(8.15267294200117,-29.9253982768887,
123.334942134734));
#114921=CARTESIAN_POINT('Ctrl Pts',(8.15847357563449,-29.8423562670606,
123.34112662357));
#114922=CARTESIAN_POINT('Ctrl Pts',(8.16081231774195,-29.8085272436336,
123.344690089323));
#114923=CARTESIAN_POINT('Ctrl Pts',(8.16410594938206,-29.7604117114463,
123.351253454494));
#114924=CARTESIAN_POINT('Ctrl Pts',(8.16508687295615,-29.7460206465406,
123.353408906049));
#114925=CARTESIAN_POINT('Ctrl Pts',(8.16678703625533,-29.7209776680386,
123.357495913684));
#114926=CARTESIAN_POINT('Ctrl Pts',(8.16750888694876,-29.7103131046261,
123.359343226796));
#114927=CARTESIAN_POINT('Ctrl Pts',(8.16899619163889,-29.6882781544591,
123.363381670807));
#114928=CARTESIAN_POINT('Ctrl Pts',(8.16976113115143,-29.6769110635224,
123.365587685135));
#114929=CARTESIAN_POINT('Ctrl Pts',(8.17173429317091,-29.6475091856344,
123.371612445821));
#114930=CARTESIAN_POINT('Ctrl Pts',(8.17293671189603,-29.6295128260624,
123.375612392682));
#114931=CARTESIAN_POINT('Ctrl Pts',(8.17821635309224,-29.550214806565,123.394623972619));
#114932=CARTESIAN_POINT('Ctrl Pts',(8.18219163219968,-29.4897251942165,
123.412813855749));
#114933=CARTESIAN_POINT('Ctrl Pts',(8.19511354842859,-29.2938358495133,
123.484081471318));
#114934=CARTESIAN_POINT('Ctrl Pts',(8.20369107127314,-29.1643719335063,
123.55141715803));
#114935=CARTESIAN_POINT('Ctrl Pts',(8.2144747122442,-29.0265129832222,123.647814896298));
#114936=CARTESIAN_POINT('Ctrl Pts',(8.21596258752668,-29.0080002473793,
123.661337274887));
#114937=CARTESIAN_POINT('Ctrl Pts',(8.21805347439158,-28.9827908967551,
123.680561198768));
#114938=CARTESIAN_POINT('Ctrl Pts',(8.21863608796822,-28.9758506744648,
123.685940921998));
#114939=CARTESIAN_POINT('Ctrl Pts',(8.21963255000446,-28.9641302862768,
123.695175245265));
#114940=CARTESIAN_POINT('Ctrl Pts',(8.22004446622471,-28.9593281941136,
123.699001961707));
#114941=CARTESIAN_POINT('Ctrl Pts',(8.22090890415184,-28.9493423766639,
123.707050175428));
#114942=CARTESIAN_POINT('Ctrl Pts',(8.22136173714491,-28.9441627934153,
123.711276414596));
#114943=CARTESIAN_POINT('Ctrl Pts',(8.22259120594472,-28.9302345479803,
123.722781382444));
#114944=CARTESIAN_POINT('Ctrl Pts',(8.2233718160776,-28.9215349904661,123.730118617861));
#114945=CARTESIAN_POINT('Ctrl Pts',(8.22725424727641,-28.8789392164369,
123.766797422974));
#114946=CARTESIAN_POINT('Ctrl Pts',(8.2304323118313,-28.8461645595898,123.797407427969));
#114947=CARTESIAN_POINT('Ctrl Pts',(8.23996918740608,-28.7528544772965,
123.891883681567));
#114948=CARTESIAN_POINT('Ctrl Pts',(8.24642377711056,-28.6960961697525,
123.959265375396));
#114949=CARTESIAN_POINT('Ctrl Pts',(8.25716882936448,-28.6096611677064,
124.08011520575));
#114950=CARTESIAN_POINT('Ctrl Pts',(8.26150268712672,-28.5771132068232,
124.131308724844));
#114951=CARTESIAN_POINT('Ctrl Pts',(8.26761239925455,-28.5343810256616,
124.207392527624));
#114952=CARTESIAN_POINT('Ctrl Pts',(8.26945976700469,-28.5218948344833,
124.230928586426));
#114953=CARTESIAN_POINT('Ctrl Pts',(8.2727648135219,-28.5003519183986,124.274000902871));
#114954=CARTESIAN_POINT('Ctrl Pts',(8.27422883713139,-28.4910994270867,
124.293432102383));
#114955=CARTESIAN_POINT('Ctrl Pts',(8.27650470944068,-28.4771819893589,
124.324181296994));
#114956=CARTESIAN_POINT('Ctrl Pts',(8.2773252411017,-28.4722611314191,124.3353801266));
#114957=CARTESIAN_POINT('Ctrl Pts',(8.27885378060327,-28.4632787287989,
124.356449209166));
#114958=CARTESIAN_POINT('Ctrl Pts',(8.27956275405594,-28.4591878580258,
124.366306195432));
#114959=CARTESIAN_POINT('Ctrl Pts',(8.28114839612405,-28.4502107048298,
124.388537717765));
#114960=CARTESIAN_POINT('Ctrl Pts',(8.28202325124273,-28.4453773282874,
124.400932935555));
#114961=CARTESIAN_POINT('Ctrl Pts',(8.28426181045815,-28.4333247079794,
124.432970537949));
#114962=CARTESIAN_POINT('Ctrl Pts',(8.2856182241134,-28.426326000243,124.452693790982));
#114963=CARTESIAN_POINT('Ctrl Pts',(8.2966237809029,-28.3721289735597,124.615072452251));
#114964=CARTESIAN_POINT('Ctrl Pts',(8.30558432046893,-28.3440583939598,
124.763373237726));
#114965=CARTESIAN_POINT('Ctrl Pts',(8.31760122228488,-28.333929230156,124.958047270103));
#114966=CARTESIAN_POINT('Ctrl Pts',(8.32038311470479,-28.3334035203741,
125.002734166932));
#114967=CARTESIAN_POINT('Ctrl Pts',(8.3249251277759,-28.335429007757,125.073919232414));
#114968=CARTESIAN_POINT('Ctrl Pts',(8.32664125314046,-28.336818028131,125.100429981403));
#114969=CARTESIAN_POINT('Ctrl Pts',(8.32899981068632,-28.339546028376,125.13614192483));
#114970=CARTESIAN_POINT('Ctrl Pts',(8.32961437993956,-28.340329624558,125.145383116617));
#114971=CARTESIAN_POINT('Ctrl Pts',(8.33064897671064,-28.3417687262063,
125.160822528058));
#114972=CARTESIAN_POINT('Ctrl Pts',(8.33106669954043,-28.3423819486823,
125.167024660113));
#114973=CARTESIAN_POINT('Ctrl Pts',(8.33187140242276,-28.3436243188825,
125.178908581248));
#114974=CARTESIAN_POINT('Ctrl Pts',(8.33225804133579,-28.3442479330186,
125.184590811351));
#114975=CARTESIAN_POINT('Ctrl Pts',(8.33331315286667,-28.3460222784039,
125.200025318645));
#114976=CARTESIAN_POINT('Ctrl Pts',(8.33398466373152,-28.3472299904756,
125.209770625929));
#114977=CARTESIAN_POINT('Ctrl Pts',(8.33663011011154,-28.3522954838519,
125.247881673198));
#114978=CARTESIAN_POINT('Ctrl Pts',(8.33863471079156,-28.3567977482924,
125.276155070562));
#114979=CARTESIAN_POINT('Ctrl Pts',(8.34732083498592,-28.3791834713274,
125.396653522729));
#114980=CARTESIAN_POINT('Ctrl Pts',(8.35421071389529,-28.4041190181944,
125.487379887572));
#114981=CARTESIAN_POINT('Ctrl Pts',(8.36102756272879,-28.4365599800807,
125.575509603842));
#114982=CARTESIAN_POINT('Ctrl Pts',(8.16626341820841,-28.4365599837785,
125.575509613888));
#114983=CARTESIAN_POINT('Ctrl Pts',(8.16547942547945,-28.4324769590612,
125.564417593744));
#114984=CARTESIAN_POINT('Ctrl Pts',(8.16469937320103,-28.4285120041026,
125.553282201909));
#114985=CARTESIAN_POINT('Ctrl Pts',(8.1626186044127,-28.4182017872195,125.523321164882));
#114986=CARTESIAN_POINT('Ctrl Pts',(8.16132506106394,-28.4120740470098,
125.504422293387));
#114987=CARTESIAN_POINT('Ctrl Pts',(8.15401452785318,-28.3791009035015,
125.39616547033));
#114988=CARTESIAN_POINT('Ctrl Pts',(8.14823771962926,-28.3594598761445,
125.304782308935));
#114989=CARTESIAN_POINT('Ctrl Pts',(8.13815381465029,-28.338478564275,125.141417546437));
#114990=CARTESIAN_POINT('Ctrl Pts',(8.13382720892913,-28.333945478382,125.070101000919));
#114991=CARTESIAN_POINT('Ctrl Pts',(8.1258696786412,-28.3340445101056,124.941605154235));
#114992=CARTESIAN_POINT('Ctrl Pts',(8.12227689942226,-28.3370251665466,
124.884540405244));
#114993=CARTESIAN_POINT('Ctrl Pts',(8.11776286945087,-28.3441647769812,
124.815857010106));
#114994=CARTESIAN_POINT('Ctrl Pts',(8.11697534779172,-28.3455287698328,
124.803979963053));
#114995=CARTESIAN_POINT('Ctrl Pts',(8.11572407869919,-28.3478785085063,
124.785295855632));
#114996=CARTESIAN_POINT('Ctrl Pts',(8.11526489406306,-28.3487788220798,
124.778478196097));
#114997=CARTESIAN_POINT('Ctrl Pts',(8.11439583277433,-28.3505533421466,
124.765652867563));
#114998=CARTESIAN_POINT('Ctrl Pts',(8.1139864698656,-28.3514182109223,124.759644148285));
#114999=CARTESIAN_POINT('Ctrl Pts',(8.11300979062025,-28.3535504749372,
124.745383296907));
#115000=CARTESIAN_POINT('Ctrl Pts',(8.11244089225243,-28.3548470860646,
124.737135802287));
#115001=CARTESIAN_POINT('Ctrl Pts',(8.11049068977032,-28.3594787420168,
124.709052248364));
#115002=CARTESIAN_POINT('Ctrl Pts',(8.10909457544795,-28.3631108672285,
124.689267848386));
#115003=CARTESIAN_POINT('Ctrl Pts',(8.10558542532627,-28.373037526978,124.640215053393));
#115004=CARTESIAN_POINT('Ctrl Pts',(8.10345589762585,-28.3797643675872,
124.611041924188));
#115005=CARTESIAN_POINT('Ctrl Pts',(8.09307956532922,-28.4160314348977,
124.471093734306));
#115006=CARTESIAN_POINT('Ctrl Pts',(8.08462915601719,-28.4561674029286,
124.363382620243));
#115007=CARTESIAN_POINT('Ctrl Pts',(8.07163710921463,-28.5367638877434,
124.200638129734));
#115008=CARTESIAN_POINT('Ctrl Pts',(8.06693700100534,-28.5700724169644,
124.142475376262));
#115009=CARTESIAN_POINT('Ctrl Pts',(8.06107839197189,-28.6170776229805,
124.070788901293));
#115010=CARTESIAN_POINT('Ctrl Pts',(8.05980672125489,-28.6276233442741,
124.055283147441));
#115011=CARTESIAN_POINT('Ctrl Pts',(8.05776136156508,-28.6451384948061,
124.030442436719));
#115012=CARTESIAN_POINT('Ctrl Pts',(8.05698168664499,-28.6519477334164,
124.020997106625));
#115013=CARTESIAN_POINT('Ctrl Pts',(8.05548658681987,-28.6652589860843,
124.002934843657));
#115014=CARTESIAN_POINT('Ctrl Pts',(8.05477066377694,-28.6717467994374,
123.994308225768));
#115015=CARTESIAN_POINT('Ctrl Pts',(8.05310884323275,-28.6870694278685,
123.974341213398));
#115016=CARTESIAN_POINT('Ctrl Pts',(8.05216551819546,-28.6959681772884,
123.963050791733));
#115017=CARTESIAN_POINT('Ctrl Pts',(8.04907873652986,-28.7257373928665,
123.926270033047));
#115018=CARTESIAN_POINT('Ctrl Pts',(8.04695975395307,-28.7472185535769,
123.901282514337));
#115019=CARTESIAN_POINT('Ctrl Pts',(8.04187247679382,-28.8011767256037,
123.842158475678));
#115020=CARTESIAN_POINT('Ctrl Pts',(8.03893313996667,-28.8343880669925,
123.808730281568));
#115021=CARTESIAN_POINT('Ctrl Pts',(8.03182964268563,-28.9188421181164,
123.730643236722));
#115022=CARTESIAN_POINT('Ctrl Pts',(8.02770660979172,-28.9714839982173,
123.687626584171));
#115023=CARTESIAN_POINT('Ctrl Pts',(8.02333105031825,-29.0295008712684,
123.645858141884));
#115024=CARTESIAN_POINT('Ctrl Pts',(8.02311257283382,-29.0324032148564,
123.64378276369));
#115025=CARTESIAN_POINT('Ctrl Pts',(8.01790381433809,-29.1017223679453,
123.594550513803));
#115026=CARTESIAN_POINT('Ctrl Pts',(8.01286811306646,-29.1714937959449,
123.552324310014));
#115027=CARTESIAN_POINT('Ctrl Pts',(8.00674276202954,-29.2550727596199,
123.509767776961));
#115028=CARTESIAN_POINT('Ctrl Pts',(8.0059294233641,-29.2661452647006,123.504284158882));
#115029=CARTESIAN_POINT('Ctrl Pts',(8.00464612531833,-29.2835545550346,
123.495902110174));
#115030=CARTESIAN_POINT('Ctrl Pts',(8.00418112007286,-29.2898505320337,
123.492919289974));
#115031=CARTESIAN_POINT('Ctrl Pts',(8.0033077663485,-29.3016478447872,123.487420461107));
#115032=CARTESIAN_POINT('Ctrl Pts',(8.00290000687352,-29.3071444133693,
123.484894813681));
#115033=CARTESIAN_POINT('Ctrl Pts',(8.00193626362902,-29.3201100772512,
123.479022458936));
#115034=CARTESIAN_POINT('Ctrl Pts',(8.0013788177423,-29.3275902106154,123.475700798524));
#115035=CARTESIAN_POINT('Ctrl Pts',(7.99950926179686,-29.3526223541858,
123.464805020734));
#115036=CARTESIAN_POINT('Ctrl Pts',(7.99818388648282,-29.3702795010093,
123.457478215209));
#115037=CARTESIAN_POINT('Ctrl Pts',(7.99489170691469,-29.41401192889,123.440207496968));
#115038=CARTESIAN_POINT('Ctrl Pts',(7.99291073520473,-29.44021803352,123.430612015065));
#115039=CARTESIAN_POINT('Ctrl Pts',(7.98394489144086,-29.5588073172379,
123.39053811178));
#115040=CARTESIAN_POINT('Ctrl Pts',(7.9767942255221,-29.6535127139069,123.367527859017));
#115041=CARTESIAN_POINT('Ctrl Pts',(7.96356668136652,-29.8346409159076,
123.340001031527));
#115042=CARTESIAN_POINT('Ctrl Pts',(7.95747970818973,-29.9204789632291,
123.33368048114));
#115043=CARTESIAN_POINT('Ctrl Pts',(7.95024903481309,-30.0261227812028,
123.334088458429));
#115044=CARTESIAN_POINT('Ctrl Pts',(7.94891218700895,-30.0458096207103,
123.334513524405));
#115045=CARTESIAN_POINT('Ctrl Pts',(7.94678863913994,-30.0773187574682,
123.335753004221));
#115046=CARTESIAN_POINT('Ctrl Pts',(7.94599508283325,-30.0891474164829,
123.336344685974));
#115047=CARTESIAN_POINT('Ctrl Pts',(7.94448979560155,-30.1116832310394,
123.337712999148));
#115048=CARTESIAN_POINT('Ctrl Pts',(7.94377739893271,-30.1223911023939,
123.338467079907));
#115049=CARTESIAN_POINT('Ctrl Pts',(7.94214717200413,-30.1469871171889,
123.340438273105));
#115050=CARTESIAN_POINT('Ctrl Pts',(7.94123160522727,-30.1608688902596,
123.341726332081));
#115051=CARTESIAN_POINT('Ctrl Pts',(7.93833707832414,-30.2049525104772,
123.346375547093));
#115052=CARTESIAN_POINT('Ctrl Pts',(7.93637844587613,-30.2350803351481,
123.350388899318));
#115053=CARTESIAN_POINT('Ctrl Pts',(7.93175853781775,-30.3066464127872,
123.361922969449));
#115054=CARTESIAN_POINT('Ctrl Pts',(7.92911930605668,-30.3479427795192,
123.370194927597));
#115055=CARTESIAN_POINT('Ctrl Pts',(7.9218396038667,-30.462077105722,123.397593453428));
#115056=CARTESIAN_POINT('Ctrl Pts',(7.91727239400856,-30.5339959481434,
123.420104213306));
#115057=CARTESIAN_POINT('Ctrl Pts',(7.91183715133302,-30.6167785394866,
123.452316590263));
#115058=CARTESIAN_POINT('Ctrl Pts',(7.91100664316762,-30.6293491455522,
123.457385546901));
#115059=CARTESIAN_POINT('Ctrl Pts',(7.90569050749756,-30.7091992493756,
123.49072270242));
#115060=CARTESIAN_POINT('Ctrl Pts',(7.9011519654138,-30.7746138627548,123.523229125894));
#115061=CARTESIAN_POINT('Ctrl Pts',(7.89558442436585,-30.848288926322,123.566084879981));
#115062=CARTESIAN_POINT('Ctrl Pts',(7.89477630857707,-30.8588304348841,
123.572373670629));
#115063=CARTESIAN_POINT('Ctrl Pts',(7.89349948739961,-30.8752289248917,
123.582403931149));
#115064=CARTESIAN_POINT('Ctrl Pts',(7.89303565586442,-30.8811338647551,
123.586066694147));
#115065=CARTESIAN_POINT('Ctrl Pts',(7.89216319647963,-30.8921395265004,
123.592989087817));
#115066=CARTESIAN_POINT('Ctrl Pts',(7.89175514263403,-30.8972456191498,
123.596239715626));
#115067=CARTESIAN_POINT('Ctrl Pts',(7.89078892106941,-30.9092405956053,
123.603968107052));
#115068=CARTESIAN_POINT('Ctrl Pts',(7.89022926811205,-30.916114193393,123.608469086074));
#115069=CARTESIAN_POINT('Ctrl Pts',(7.888344374703,-30.9390265986613,123.623715957769));
#115070=CARTESIAN_POINT('Ctrl Pts',(7.88700558181857,-30.9549111982721,
123.634689324039));
#115071=CARTESIAN_POINT('Ctrl Pts',(7.8836725896048,-30.9935898775746,123.662414410329));
#115072=CARTESIAN_POINT('Ctrl Pts',(7.88166379887218,-31.0161544425717,
123.679475095754));
#115073=CARTESIAN_POINT('Ctrl Pts',(7.87245499813857,-31.1166619364988,
123.759568910331));
#115074=CARTESIAN_POINT('Ctrl Pts',(7.86508252586005,-31.1892534186918,
123.828983374719));
#115075=CARTESIAN_POINT('Ctrl Pts',(7.85190793376787,-31.3094070397529,
123.966649377347));
#115076=CARTESIAN_POINT('Ctrl Pts',(7.84607386977252,-31.3589642359754,
124.032746053603));
#115077=CARTESIAN_POINT('Ctrl Pts',(7.83908588263193,-31.4139889545182,
124.118764804695));
#115078=CARTESIAN_POINT('Ctrl Pts',(7.83775509849655,-31.4242598199741,
124.135462982231));
#115079=CARTESIAN_POINT('Ctrl Pts',(7.83563882127667,-31.4402501886613,
124.162518532701));
#115080=CARTESIAN_POINT('Ctrl Pts',(7.83484655480527,-31.4461579802632,
124.172761870677));
#115081=CARTESIAN_POINT('Ctrl Pts',(7.83334227108706,-31.4572220766442,
124.192426389377));
#115082=CARTESIAN_POINT('Ctrl Pts',(7.83262960322967,-31.4623972947206,
124.201836182956));
#115083=CARTESIAN_POINT('Ctrl Pts',(7.83099672465691,-31.4740983186649,
124.223607371765));
#115084=CARTESIAN_POINT('Ctrl Pts',(7.83007880347991,-31.4805603226038,
124.236002279373));
#115085=CARTESIAN_POINT('Ctrl Pts',(7.82716834081315,-31.5006682525393,
124.27578523552));
#115086=CARTESIAN_POINT('Ctrl Pts',(7.82519645511471,-31.5137164783339,
124.303469425794));
#115087=CARTESIAN_POINT('Ctrl Pts',(7.82053855599107,-31.543049812716,124.370428966258));
#115088=CARTESIAN_POINT('Ctrl Pts',(7.81787510659863,-31.558608981378,124.409999293157));
#115089=CARTESIAN_POINT('Ctrl Pts',(7.81066971969658,-31.596968769538,124.519707737668));
#115090=CARTESIAN_POINT('Ctrl Pts',(7.80619538013148,-31.6166543896218,
124.590831504046));
#115091=CARTESIAN_POINT('Ctrl Pts',(7.80083666926066,-31.6343716467981,
124.676614972478));
#115092=CARTESIAN_POINT('Ctrl Pts',(7.79998656953,-31.6370084600261,124.690239040858));
#115093=CARTESIAN_POINT('Ctrl Pts',(7.79461998770719,-31.6525367813739,
124.776216091977));
#115094=CARTESIAN_POINT('Ctrl Pts',(7.79005102148958,-31.6607974236268,
124.849314116242));
#115095=CARTESIAN_POINT('Ctrl Pts',(7.78444971239173,-31.6647756820226,
124.934971923929));
#115096=CARTESIAN_POINT('Ctrl Pts',(7.78364147022368,-31.6652096554362,
124.947241078298));
#115097=CARTESIAN_POINT('Ctrl Pts',(7.78236449233671,-31.6656768597908,
124.966460616492));
#115098=CARTESIAN_POINT('Ctrl Pts',(7.78190063240834,-31.6658022645961,
124.973408603235));
#115099=CARTESIAN_POINT('Ctrl Pts',(7.78102815158764,-31.6659555652293,
124.986409737236));
#115100=CARTESIAN_POINT('Ctrl Pts',(7.78062010506356,-31.6659939442218,
124.992462513743));
#115101=CARTESIAN_POINT('Ctrl Pts',(7.77965394435065,-31.666006659998,125.006730743812));
#115102=CARTESIAN_POINT('Ctrl Pts',(7.77909434548976,-31.6659532123358,
125.01494594611));
#115103=CARTESIAN_POINT('Ctrl Pts',(7.77720982911279,-31.6655706896432,
125.04245957913));
#115104=CARTESIAN_POINT('Ctrl Pts',(7.77587136626035,-31.6649670177052,
125.061751831152));
#115105=CARTESIAN_POINT('Ctrl Pts',(7.7725393798046,-31.6626531408596,125.109270567233));
#115106=CARTESIAN_POINT('Ctrl Pts',(7.77053127531928,-31.6605591952488,
125.137471823562));
#115107=CARTESIAN_POINT('Ctrl Pts',(7.76132856963111,-31.6477925620909,
125.265269538704));
#115108=CARTESIAN_POINT('Ctrl Pts',(7.75396167292581,-31.6288690136447,
125.363832992559));
#115109=CARTESIAN_POINT('Ctrl Pts',(7.74078581811461,-31.5784023305153,
125.539463151853));
#115110=CARTESIAN_POINT('Ctrl Pts',(7.73494548422716,-31.5497265639478,
125.617029726385));
#115111=CARTESIAN_POINT('Ctrl Pts',(7.7279514412154,-31.5072661236998,125.70999237117));
#115112=CARTESIAN_POINT('Ctrl Pts',(7.72662047674095,-31.4988068007017,
125.727680263514));
#115113=CARTESIAN_POINT('Ctrl Pts',(7.72450398327123,-31.4847475651856,
125.755791303693));
#115114=CARTESIAN_POINT('Ctrl Pts',(7.72371167843047,-31.479345651537,125.766310826506));
#115115=CARTESIAN_POINT('Ctrl Pts',(7.72220736501307,-31.4688252736245,
125.78627198206));
#115116=CARTESIAN_POINT('Ctrl Pts',(7.72149470537442,-31.4637266469606,
125.795723335335));
#115117=CARTESIAN_POINT('Ctrl Pts',(7.71986190644102,-31.4517826150671,
125.817360736742));
#115118=CARTESIAN_POINT('Ctrl Pts',(7.71894405590255,-31.4448744725493,
125.82951137043));
#115119=CARTESIAN_POINT('Ctrl Pts',(7.71603407230868,-31.4223608703319,
125.867975457935));
#115120=CARTESIAN_POINT('Ctrl Pts',(7.71406258513979,-31.4061827120815,
125.89394754291));
#115121=CARTESIAN_POINT('Ctrl Pts',(7.70940583001876,-31.3658476543687,
125.95489348398));
#115122=CARTESIAN_POINT('Ctrl Pts',(7.70674311032931,-31.3410496734596,
125.989417775061));
#115123=CARTESIAN_POINT('Ctrl Pts',(7.69953811031672,-31.2696919709715,
126.081144248231));
#115124=CARTESIAN_POINT('Ctrl Pts',(7.69506347539834,-31.2206134033656,
126.136263117505));
#115125=CARTESIAN_POINT('Ctrl Pts',(7.68970794153499,-31.1581908575605,
126.197639735466));
#115126=CARTESIAN_POINT('Ctrl Pts',(7.68886129530606,-31.148216161876,126.207206129174));
#115127=CARTESIAN_POINT('Ctrl Pts',(7.68349384736662,-31.0844009071469,
126.266902687337));
#115128=CARTESIAN_POINT('Ctrl Pts',(7.67892059112954,-31.0274149761528,
126.313538531284));
#115129=CARTESIAN_POINT('Ctrl Pts',(7.67331451884676,-30.9575484231261,
126.363380998167));
#115130=CARTESIAN_POINT('Ctrl Pts',(7.67250625920492,-30.9474757254317,
126.370400108274));
#115131=CARTESIAN_POINT('Ctrl Pts',(7.67122925964101,-30.9315816785885,
126.381216807186));
#115132=CARTESIAN_POINT('Ctrl Pts',(7.67076539577713,-30.9258123381129,
126.38509053948));
#115133=CARTESIAN_POINT('Ctrl Pts',(7.66989291196878,-30.9149726262504,
126.392270711324));
#115134=CARTESIAN_POINT('Ctrl Pts',(7.66948486644286,-30.9099082525484,
126.395585757904));
#115135=CARTESIAN_POINT('Ctrl Pts',(7.6685187140959,-30.8979278907113,126.403334954812));
#115136=CARTESIAN_POINT('Ctrl Pts',(7.66795912268106,-30.8909970451717,
126.407745627142));
#115137=CARTESIAN_POINT('Ctrl Pts',(7.66607465823961,-30.8676748186116,
126.422346273744));
#115138=CARTESIAN_POINT('Ctrl Pts',(7.66473624085459,-30.8511397077952,
126.432302213832));
#115139=CARTESIAN_POINT('Ctrl Pts',(7.66140439296249,-30.8099638976418,
126.456129779611));
#115140=CARTESIAN_POINT('Ctrl Pts',(7.65939638302319,-30.7851362865985,
126.469665363804));
#115141=CARTESIAN_POINT('Ctrl Pts',(7.65019451669854,-30.6708541981889,
126.528247639604));
#115142=CARTESIAN_POINT('Ctrl Pts',(7.64282838778472,-30.5777933509493,
126.565803787186));
#115143=CARTESIAN_POINT('Ctrl Pts',(7.62965235893061,-30.4028672185788,
126.618664374487));
#115144=CARTESIAN_POINT('Ctrl Pts',(7.62381116140066,-30.3221361288222,
126.636645461328));
#115145=CARTESIAN_POINT('Ctrl Pts',(7.61681628438287,-30.2209931574098,
126.6513940696));
#115146=CARTESIAN_POINT('Ctrl Pts',(7.61548529519009,-30.2015444046224,
126.653880364072));
#115147=CARTESIAN_POINT('Ctrl Pts',(7.61336877207036,-30.1703014436118,
126.657315071783));
#115148=CARTESIAN_POINT('Ctrl Pts',(7.61257646196115,-30.1585336554849,
126.658482113685));
#115149=CARTESIAN_POINT('Ctrl Pts',(7.61107214444826,-30.1360574884488,
126.660469714761));
#115150=CARTESIAN_POINT('Ctrl Pts',(7.61035948592068,-30.1253517022893,
126.661312214409));
#115151=CARTESIAN_POINT('Ctrl Pts',(7.60872669785634,-30.100695335414,126.663012862423));
#115152=CARTESIAN_POINT('Ctrl Pts',(7.60780885696898,-30.0867404816529,
126.663799098365));
#115153=CARTESIAN_POINT('Ctrl Pts',(7.60489893888342,-30.042215576272,126.665745968945));
#115154=CARTESIAN_POINT('Ctrl Pts',(7.60292750621691,-30.0116217133338,
126.666240352381));
#115155=CARTESIAN_POINT('Ctrl Pts',(7.59827090755342,-29.938544610728,126.665408200689));
#115156=CARTESIAN_POINT('Ctrl Pts',(7.59560828766221,-29.8960913656353,
126.663299316137));
#115157=CARTESIAN_POINT('Ctrl Pts',(7.58840334126734,-29.7803270874141,
126.653098451153));
#115158=CARTESIAN_POINT('Ctrl Pts',(7.58392866662734,-29.7074002054776,
126.641760154257));
#115159=CARTESIAN_POINT('Ctrl Pts',(7.57446014648976,-29.5563768260499,
126.60789420372));
#115160=CARTESIAN_POINT('Ctrl Pts',(7.56947081470208,-29.4786984847162,
126.584413729969));
#115161=CARTESIAN_POINT('Ctrl Pts',(7.56317443575743,-29.3879893331913,
126.549599652459));
#115162=CARTESIAN_POINT('Ctrl Pts',(7.56211908234472,-29.3730168390307,
126.543602347795));
#115163=CARTESIAN_POINT('Ctrl Pts',(7.56053784015299,-29.3509708518339,
126.534398066715));
#115164=CARTESIAN_POINT('Ctrl Pts',(7.56002125403971,-29.3438284157962,
126.531357276545));
#115165=CARTESIAN_POINT('Ctrl Pts',(7.55909941258379,-29.3311947700974,
126.525874071297));
#115166=CARTESIAN_POINT('Ctrl Pts',(7.55869535611452,-29.3256951451234,
126.523451698449));
#115167=CARTESIAN_POINT('Ctrl Pts',(7.55779954987719,-29.3135867348158,
126.518039998779));
#115168=CARTESIAN_POINT('Ctrl Pts',(7.55730703257641,-29.3069843959243,
126.515037285367));
#115169=CARTESIAN_POINT('Ctrl Pts',(7.55585127908362,-29.2876241795882,
126.506079320415));
#115170=CARTESIAN_POINT('Ctrl Pts',(7.55488136958126,-29.2749223076002,
126.500005512053));
#115171=CARTESIAN_POINT('Ctrl Pts',(7.5480422291824,-29.1866225044816,126.456398573499));
#115172=CARTESIAN_POINT('Ctrl Pts',(7.54191663462614,-29.1139025864465,
126.413332312008));
#115173=CARTESIAN_POINT('Ctrl Pts',(7.52646891785952,-28.9400105864096,
126.291637216763));
#115174=CARTESIAN_POINT('Ctrl Pts',(7.51720686455405,-28.8440226685185,
126.206495914544));
#115175=CARTESIAN_POINT('Ctrl Pts',(7.50695850663711,-28.744671498522,126.095513320632));
#115176=CARTESIAN_POINT('Ctrl Pts',(7.50552236270976,-28.7309297559286,
126.079564666007));
#115177=CARTESIAN_POINT('Ctrl Pts',(7.50319643927016,-28.7089803982537,
126.053091771589));
#115178=CARTESIAN_POINT('Ctrl Pts',(7.5022993597384,-28.7005907968368,126.042722221962));
#115179=CARTESIAN_POINT('Ctrl Pts',(7.50069354247894,-28.6857144652872,
126.023876657793));
#115180=CARTESIAN_POINT('Ctrl Pts',(7.49998304725718,-28.6791830212844,
126.015437046281));
#115181=CARTESIAN_POINT('Ctrl Pts',(7.49846705315504,-28.665358742141,125.997214908737));
#115182=CARTESIAN_POINT('Ctrl Pts',(7.4976625770582,-28.6580913391826,125.987413804187));
#115183=CARTESIAN_POINT('Ctrl Pts',(7.49545942954509,-28.6383853515719,
125.960218097117));
#115184=CARTESIAN_POINT('Ctrl Pts',(7.49406941880257,-28.6261726995768,
125.942662113951));
#115185=CARTESIAN_POINT('Ctrl Pts',(7.48820579676779,-28.5756697713551,
125.866995841285));
#115186=CARTESIAN_POINT('Ctrl Pts',(7.48385361238211,-28.5407003449968,
125.80674934718));
#115187=CARTESIAN_POINT('Ctrl Pts',(7.47577564638596,-28.4821412597061,
125.689518808267));
#115188=CARTESIAN_POINT('Ctrl Pts',(7.47204379419599,-28.457761504673,125.633106038967));
#115189=CARTESIAN_POINT('Ctrl Pts',(7.46828914249572,-28.4365600390074,
125.575509763924));
#115190=CARTESIAN_POINT('Origin',(5.,-30.,125.));
#115191=CARTESIAN_POINT('',(6.7689357756443,-28.4365600093868,125.575509683456));
#115192=CARTESIAN_POINT('',(6.96167308954663,-28.4365599688247,125.575509573264));
#115193=CARTESIAN_POINT('',(5.,-28.4365599837785,125.575509613888));
#115194=CARTESIAN_POINT('Ctrl Pts',(6.96167308954662,-28.4365599688247,
125.575509573264));
#115195=CARTESIAN_POINT('Ctrl Pts',(6.96619326604114,-28.461605418403,125.643548508303));
#115196=CARTESIAN_POINT('Ctrl Pts',(6.97060995840626,-28.49107241895,125.709898686597));
#115197=CARTESIAN_POINT('Ctrl Pts',(6.98041879830601,-28.5656959162624,
125.852103833634));
#115198=CARTESIAN_POINT('Ctrl Pts',(6.98580004343452,-28.6127230432211,
125.926697481698));
#115199=CARTESIAN_POINT('Ctrl Pts',(6.99272049307737,-28.6769792923376,
126.012692150223));
#115200=CARTESIAN_POINT('Ctrl Pts',(6.99397967804428,-28.6888101283685,
126.027964117312));
#115201=CARTESIAN_POINT('Ctrl Pts',(6.99579915129659,-28.7060493096574,
126.049435646233));
#115202=CARTESIAN_POINT('Ctrl Pts',(6.99634536729574,-28.7112426605574,
126.05580683728));
#115203=CARTESIAN_POINT('Ctrl Pts',(6.9972997737851,-28.7203432178703,126.066804192495));
#115204=CARTESIAN_POINT('Ctrl Pts',(6.9977064329797,-28.7242288438188,126.071447908622));
#115205=CARTESIAN_POINT('Ctrl Pts',(6.99858396809871,-28.7326292603818,
126.081376770711));
#115206=CARTESIAN_POINT('Ctrl Pts',(6.99905536960203,-28.737151767051,126.086654797074));
#115207=CARTESIAN_POINT('Ctrl Pts',(7.00036573562785,-28.7497539111416,
126.101177305723));
#115208=CARTESIAN_POINT('Ctrl Pts',(7.00120944724854,-28.7579027283144,
126.110360791321));
#115209=CARTESIAN_POINT('Ctrl Pts',(7.00711659039268,-28.8152430606139,
126.173560633232));
#115210=CARTESIAN_POINT('Ctrl Pts',(7.01238145257386,-28.8678349230907,
126.224374713504));
#115211=CARTESIAN_POINT('Ctrl Pts',(7.01866721911848,-28.933874431748,126.280278891081));
#115212=CARTESIAN_POINT('Ctrl Pts',(7.01964797433931,-28.9442698815991,
126.288864492452));
#115213=CARTESIAN_POINT('Ctrl Pts',(7.02603794076691,-29.0126394783319,
126.343948747429));
#115214=CARTESIAN_POINT('Ctrl Pts',(7.03144851220877,-29.0735692764677,
126.386652977837));
#115215=CARTESIAN_POINT('Ctrl Pts',(7.0397952601921,-29.1736113126269,126.447223022306));
#115216=CARTESIAN_POINT('Ctrl Pts',(7.0428007017934,-29.210908576136,126.467892356308));
#115217=CARTESIAN_POINT('Ctrl Pts',(7.04788795810297,-29.2763309864504,
126.500932839584));
#115218=CARTESIAN_POINT('Ctrl Pts',(7.04999141354889,-29.304079488496,126.513998377334));
#115219=CARTESIAN_POINT('Ctrl Pts',(7.05301658893146,-29.3449925089903,
126.531899782452));
#115220=CARTESIAN_POINT('Ctrl Pts',(7.05395885418,-29.3578809947853,126.537346727527));
#115221=CARTESIAN_POINT('Ctrl Pts',(7.05561489945898,-29.3807845566007,
126.546687961624));
#115222=CARTESIAN_POINT('Ctrl Pts',(7.05633089303632,-29.3907714001008,
126.550648876547));
#115223=CARTESIAN_POINT('Ctrl Pts',(7.05782807308561,-29.4118281901591,
126.558765445241));
#115224=CARTESIAN_POINT('Ctrl Pts',(7.05860853541367,-29.4229055041951,
126.562900427479));
#115225=CARTESIAN_POINT('Ctrl Pts',(7.06067165743154,-29.4524474931904,
126.573571057137));
#115226=CARTESIAN_POINT('Ctrl Pts',(7.06194745217296,-29.4709853442732,
126.579899732921));
#115227=CARTESIAN_POINT('Ctrl Pts',(7.06853355814901,-29.5679949117098,
126.611119011648));
#115228=CARTESIAN_POINT('Ctrl Pts',(7.07366172258311,-29.6481250676711,
126.630496663849));
#115229=CARTESIAN_POINT('Ctrl Pts',(7.08488649056641,-29.8284384768893,
126.660181791797));
#115230=CARTESIAN_POINT('Ctrl Pts',(7.09092319526859,-29.9287736694686,
126.667501543961));
#115231=CARTESIAN_POINT('Ctrl Pts',(7.09899127111867,-30.0574534116637,
126.665249653017));
#115232=CARTESIAN_POINT('Ctrl Pts',(7.10078575072611,-30.0857375596243,
126.664033110103));
#115233=CARTESIAN_POINT('Ctrl Pts',(7.10385577202603,-30.1332479948339,
126.660775166727));
#115234=CARTESIAN_POINT('Ctrl Pts',(7.10511495455522,-30.1524952218776,
126.659118534576));
#115235=CARTESIAN_POINT('Ctrl Pts',(7.10693442489503,-30.1798842568459,
126.656280537426));
#115236=CARTESIAN_POINT('Ctrl Pts',(7.10748064048046,-30.1880536526125,
126.655372882842));
#115237=CARTESIAN_POINT('Ctrl Pts',(7.10843504650317,-30.2022288180361,
126.653691679341));
#115238=CARTESIAN_POINT('Ctrl Pts',(7.10884170564949,-30.2082376293783,
126.652945780579));
#115239=CARTESIAN_POINT('Ctrl Pts',(7.10971924096942,-30.221135385906,126.651273282356));
#115240=CARTESIAN_POINT('Ctrl Pts',(7.11019064272452,-30.2280225345039,
126.650336338834));
#115241=CARTESIAN_POINT('Ctrl Pts',(7.11150101011798,-30.2470584964309,
126.647625212566));
#115242=CARTESIAN_POINT('Ctrl Pts',(7.1123447228701,-30.2591935843518,126.645759826177));
#115243=CARTESIAN_POINT('Ctrl Pts',(7.11825216250102,-30.3433940836757,
126.631862338454));
#115244=CARTESIAN_POINT('Ctrl Pts',(7.12351734343573,-30.4146132440537,
126.615236106916));
#115245=CARTESIAN_POINT('Ctrl Pts',(7.12985706691742,-30.498108591718,126.589857242714));
#115246=CARTESIAN_POINT('Ctrl Pts',(7.13089161018272,-30.5116608441542,
126.58554766501));
#115247=CARTESIAN_POINT('Ctrl Pts',(7.13728951150637,-30.5950835079316,
126.557838541981));
#115248=CARTESIAN_POINT('Ctrl Pts',(7.14265284876418,-30.6633973025621,
126.529996938432));
#115249=CARTESIAN_POINT('Ctrl Pts',(7.15094946853164,-30.7679086970577,
126.479082041508));
#115250=CARTESIAN_POINT('Ctrl Pts',(7.15395036909879,-30.8054449652055,
126.458981276297));
#115251=CARTESIAN_POINT('Ctrl Pts',(7.15903088243546,-30.8686017285939,
126.421979352316));
#115252=CARTESIAN_POINT('Ctrl Pts',(7.16113205814459,-30.8945999687192,
126.405768598104));
#115253=CARTESIAN_POINT('Ctrl Pts',(7.16415461381213,-30.9317970226308,
126.381124870327));
#115254=CARTESIAN_POINT('Ctrl Pts',(7.16509648884991,-30.9433586433093,
126.373253832919));
#115255=CARTESIAN_POINT('Ctrl Pts',(7.16675209401653,-30.9636232207307,
126.359081192915));
#115256=CARTESIAN_POINT('Ctrl Pts',(7.1674680337163,-30.9723667688724,126.35283933878));
#115257=CARTESIAN_POINT('Ctrl Pts',(7.16896534069072,-30.9906077675845,
126.339549218365));
#115258=CARTESIAN_POINT('Ctrl Pts',(7.16974598151359,-31.0000918031732,
126.332483491451));
#115259=CARTESIAN_POINT('Ctrl Pts',(7.17181013579085,-31.0250915219491,
126.313441094717));
#115260=CARTESIAN_POINT('Ctrl Pts',(7.17308677172273,-31.0404727551062,
126.301290373489));
#115261=CARTESIAN_POINT('Ctrl Pts',(7.17967257876229,-31.119311036206,126.236718671754));
#115262=CARTESIAN_POINT('Ctrl Pts',(7.18479971111164,-31.179037516089,126.179916639213));
#115263=CARTESIAN_POINT('Ctrl Pts',(7.19602299766147,-31.301754702461,126.044542998536));
#115264=CARTESIAN_POINT('Ctrl Pts',(7.20205925630102,-31.3623170540397,
125.964222628287));
#115265=CARTESIAN_POINT('Ctrl Pts',(7.21012679584731,-31.4302114809766,
125.854899038405));
#115266=CARTESIAN_POINT('Ctrl Pts',(7.21192121591318,-31.4445291713042,
125.830477295724));
#115267=CARTESIAN_POINT('Ctrl Pts',(7.21499114563072,-31.4675592278534,
125.788795966392));
#115268=CARTESIAN_POINT('Ctrl Pts',(7.21625029738875,-31.4766061834217,
125.771727455041));
#115269=CARTESIAN_POINT('Ctrl Pts',(7.21806973095802,-31.4890764227335,
125.747178004529));
#115270=CARTESIAN_POINT('Ctrl Pts',(7.21861594131848,-31.4927446113176,
125.739822331082));
#115271=CARTESIAN_POINT('Ctrl Pts',(7.219570341449,-31.4990202169218,125.727001412862));
#115272=CARTESIAN_POINT('Ctrl Pts',(7.2199769999868,-31.5016525127705,125.721548608612));
#115273=CARTESIAN_POINT('Ctrl Pts',(7.22085453784462,-31.5072426669158,
125.709805505463));
#115274=CARTESIAN_POINT('Ctrl Pts',(7.22132594278407,-31.5101908596986,
125.703511105409));
#115275=CARTESIAN_POINT('Ctrl Pts',(7.22263632745684,-31.5182376458712,
125.686047518329));
#115276=CARTESIAN_POINT('Ctrl Pts',(7.2234800544977,-31.5232521673389,125.674840395447));
#115277=CARTESIAN_POINT('Ctrl Pts',(7.22939124540841,-31.5572651286404,
125.596512693993));
#115278=CARTESIAN_POINT('Ctrl Pts',(7.23466045948267,-31.581938280695,125.527608739796));
#115279=CARTESIAN_POINT('Ctrl Pts',(7.24100152105412,-31.6058978594324,
125.443676965507));
#115280=CARTESIAN_POINT('Ctrl Pts',(7.24203341270642,-31.6096169901336,
125.429988750864));
#115281=CARTESIAN_POINT('Ctrl Pts',(7.24842908470747,-31.6315724094788,
125.344902346293));
#115282=CARTESIAN_POINT('Ctrl Pts',(7.25379281108063,-31.6452307940476,
125.272402458721));
#115283=CARTESIAN_POINT('Ctrl Pts',(7.26208879086746,-31.6591324128804,
125.156990316707));
#115284=CARTESIAN_POINT('Ctrl Pts',(7.26508872035481,-31.662600834382,125.114565667326));
#115285=CARTESIAN_POINT('Ctrl Pts',(7.27016779150484,-31.6657656411109,
125.04145654363));
#115286=CARTESIAN_POINT('Ctrl Pts',(7.27226847948869,-31.6662463085384,
125.01082909845));
#115287=CARTESIAN_POINT('Ctrl Pts',(7.27529047464868,-31.6657162157421,
124.966220514559));
#115288=CARTESIAN_POINT('Ctrl Pts',(7.27623226616479,-31.6653739834145,
124.952239335256));
#115289=CARTESIAN_POINT('Ctrl Pts',(7.27788777714381,-31.664457666796,124.927528815414));
#115290=CARTESIAN_POINT('Ctrl Pts',(7.27860370532655,-31.6639557676617,
124.916797778223));
#115291=CARTESIAN_POINT('Ctrl Pts',(7.28010103954658,-31.6626833165531,
124.894264193733));
#115292=CARTESIAN_POINT('Ctrl Pts',(7.28088171863763,-31.6618908035528,
124.882463447901));
#115293=CARTESIAN_POINT('Ctrl Pts',(7.28294609422568,-31.6594509950476,
124.851128767655));
#115294=CARTESIAN_POINT('Ctrl Pts',(7.28422291050307,-31.6575844636793,
124.831613399686));
#115295=CARTESIAN_POINT('Ctrl Pts',(7.29081479276253,-31.6460823826263,
124.730262817037));
#115296=CARTESIAN_POINT('Ctrl Pts',(7.29594737289473,-31.6307294451463,
124.649187639915));
#115297=CARTESIAN_POINT('Ctrl Pts',(7.30717101264205,-31.5835197207545,
124.47266269227));
#115298=CARTESIAN_POINT('Ctrl Pts',(7.31320267380424,-31.5489039131112,
124.378297769228));
#115299=CARTESIAN_POINT('Ctrl Pts',(7.32126468549303,-31.4939147787945,
124.262046538924));
#115300=CARTESIAN_POINT('Ctrl Pts',(7.32305849152792,-31.4811663901989,
124.236781406804));
#115301=CARTESIAN_POINT('Ctrl Pts',(7.32612747677053,-31.4586453461783,
124.194839938157));
#115302=CARTESIAN_POINT('Ctrl Pts',(7.32738631117671,-31.4492143872971,
124.177986281896));
#115303=CARTESIAN_POINT('Ctrl Pts',(7.32920536552759,-31.4353555740465,
124.154199831174));
#115304=CARTESIAN_POINT('Ctrl Pts',(7.32975152200273,-31.4311656482883,
124.147129300723));
#115305=CARTESIAN_POINT('Ctrl Pts',(7.33070586137993,-31.4237983543817,
124.134904103676));
#115306=CARTESIAN_POINT('Ctrl Pts',(7.33111251365515,-31.4206449218808,
124.129735288336));
#115307=CARTESIAN_POINT('Ctrl Pts',(7.33199007775181,-31.4138107125555,
124.118669421745));
#115308=CARTESIAN_POINT('Ctrl Pts',(7.33246151557791,-31.4101212419726,
124.11277827031));
#115309=CARTESIAN_POINT('Ctrl Pts',(7.33377207864045,-31.3998121816725,
124.096544049527));
#115310=CARTESIAN_POINT('Ctrl Pts',(7.33461595318881,-31.3931150888306,
124.086251059891));
#115311=CARTESIAN_POINT('Ctrl Pts',(7.34056679290618,-31.3454380539383,
124.014717178169));
#115312=CARTESIAN_POINT('Ctrl Pts',(7.34587865060716,-31.3005523478014,
123.956186328974));
#115313=CARTESIAN_POINT('Ctrl Pts',(7.35215028781879,-31.2436017988192,
123.891320361461));
#115314=CARTESIAN_POINT('Ctrl Pts',(7.35307038129763,-31.2351490313212,
123.881911075728));
#115315=CARTESIAN_POINT('Ctrl Pts',(7.35947775295334,-31.1755717840124,
123.817092209638));
#115316=CARTESIAN_POINT('Ctrl Pts',(7.36496666235236,-31.1208413238072,
123.765108914887));
#115317=CARTESIAN_POINT('Ctrl Pts',(7.37335111413028,-31.0303287238141,
123.690132118193));
#115318=CARTESIAN_POINT('Ctrl Pts',(7.37632065589549,-30.9968724566929,
123.6644937505));
#115319=CARTESIAN_POINT('Ctrl Pts',(7.38135455556256,-30.9376591394278,
123.622583627847));
#115320=CARTESIAN_POINT('Ctrl Pts',(7.38343994298495,-30.9123631164856,
123.605699359097));
#115321=CARTESIAN_POINT('Ctrl Pts',(7.38644434586241,-30.8748101400577,
123.582093895129));
#115322=CARTESIAN_POINT('Ctrl Pts',(7.38738351006768,-30.8629096404324,
123.574820195075));
#115323=CARTESIAN_POINT('Ctrl Pts',(7.38903606105674,-30.8416875795425,
123.56221235493));
#115324=CARTESIAN_POINT('Ctrl Pts',(7.3897516298043,-30.8324032894817,123.556817382723));
#115325=CARTESIAN_POINT('Ctrl Pts',(7.39124983564941,-30.8127680189271,
123.545660124952));
#115326=CARTESIAN_POINT('Ctrl Pts',(7.39203173014164,-30.8024063961036,
123.53991770354));
#115327=CARTESIAN_POINT('Ctrl Pts',(7.39410313441399,-30.7746592887629,
123.52492482474));
#115328=CARTESIAN_POINT('Ctrl Pts',(7.39538567809875,-30.7571692211627,
123.515871093816));
#115329=CARTESIAN_POINT('Ctrl Pts',(7.40221086126839,-30.6625199597613,
123.468984768642));
#115330=CARTESIAN_POINT('Ctrl Pts',(7.40755326618122,-30.5826772649763,
123.436852453945));
#115331=CARTESIAN_POINT('Ctrl Pts',(7.41879401586944,-30.407923474442,123.381785807161));
#115332=CARTESIAN_POINT('Ctrl Pts',(7.42465069980157,-30.3127680694217,
123.360734124953));
#115333=CARTESIAN_POINT('Ctrl Pts',(7.4325019441944,-30.1886570919505,123.344480978544));
#115334=CARTESIAN_POINT('Ctrl Pts',(7.43427189498057,-30.160902477878,123.341553453677));
#115335=CARTESIAN_POINT('Ctrl Pts',(7.43730415572979,-30.1140320690139,
123.337797187808));
#115336=CARTESIAN_POINT('Ctrl Pts',(7.43855062547048,-30.0949511785318,
123.336598154541));
#115337=CARTESIAN_POINT('Ctrl Pts',(7.44035489873692,-30.0676770247961,
123.335355041839));
#115338=CARTESIAN_POINT('Ctrl Pts',(7.44089894804567,-30.0594967343944,
123.335042598718));
#115339=CARTESIAN_POINT('Ctrl Pts',(7.44185091585677,-30.0452665246496,
123.334604084087));
#115340=CARTESIAN_POINT('Ctrl Pts',(7.44225732740366,-30.0392176863733,
123.33445066519));
#115341=CARTESIAN_POINT('Ctrl Pts',(7.44313593620846,-30.0261995315224,
123.334191438699));
#115342=CARTESIAN_POINT('Ctrl Pts',(7.44360867468025,-30.0192304516878,
123.334096412261));
#115343=CARTESIAN_POINT('Ctrl Pts',(7.44492630011381,-29.9998981815117,
123.333954130075));
#115344=CARTESIAN_POINT('Ctrl Pts',(7.44577601603251,-29.9875350422296,
123.334000764306));
#115345=CARTESIAN_POINT('Ctrl Pts',(7.45228787447881,-29.8934910367533,
123.335402320559));
#115346=CARTESIAN_POINT('Ctrl Pts',(7.4582008533018,-29.8120168919971,123.342625867577));
#115347=CARTESIAN_POINT('Ctrl Pts',(7.46848348868089,-29.6725219105499,
123.365413023157));
#115348=CARTESIAN_POINT('Ctrl Pts',(7.47283385869959,-29.614190015485,123.378190028458));
#115349=CARTESIAN_POINT('Ctrl Pts',(7.48102255727653,-29.5046100153875,
123.408440596109));
#115350=CARTESIAN_POINT('Ctrl Pts',(7.48486584250961,-29.4532776781101,
123.425335522503));
#115351=CARTESIAN_POINT('Ctrl Pts',(7.49036700591859,-29.3797193267496,
123.453577703023));
#115352=CARTESIAN_POINT('Ctrl Pts',(7.49208145596446,-29.3567861375947,
123.46297492795));
#115353=CARTESIAN_POINT('Ctrl Pts',(7.49517316506172,-29.3154207105719,
123.48101312359));
#115354=CARTESIAN_POINT('Ctrl Pts',(7.49655559460631,-29.2969212194321,
123.4894867673));
#115355=CARTESIAN_POINT('Ctrl Pts',(7.49873391844987,-29.2677782856679,
123.503487057141));
#115356=CARTESIAN_POINT('Ctrl Pts',(7.49953730276435,-29.2570317907059,
123.508793146455));
#115357=CARTESIAN_POINT('Ctrl Pts',(7.50105082283565,-29.2367939691114,
123.519058675857));
#115358=CARTESIAN_POINT('Ctrl Pts',(7.50176173486675,-29.2272914329899,
123.523994535665));
#115359=CARTESIAN_POINT('Ctrl Pts',(7.50337431742757,-29.2057491287152,
123.535449222082));
#115360=CARTESIAN_POINT('Ctrl Pts',(7.50427390254093,-29.1937407040056,
123.542025585331));
#115361=CARTESIAN_POINT('Ctrl Pts',(7.50662277965274,-29.162424195563,123.559681196279));
#115362=CARTESIAN_POINT('Ctrl Pts',(7.50806348355918,-29.1432543395918,
123.571000898366));
#115363=CARTESIAN_POINT('Ctrl Pts',(7.51904980360839,-28.997596454177,123.660996236589));
#115364=CARTESIAN_POINT('Ctrl Pts',(7.52792892745521,-28.8819547580372,
123.755926061958));
#115365=CARTESIAN_POINT('Ctrl Pts',(7.54078984904522,-28.7398984062878,
123.908557759468));
#115366=CARTESIAN_POINT('Ctrl Pts',(7.54451308157894,-28.7016979975512,
123.954288467086));
#115367=CARTESIAN_POINT('Ctrl Pts',(7.54935985009843,-28.6569998292364,
124.014031528025));
#115368=CARTESIAN_POINT('Ctrl Pts',(7.55034822099687,-28.6481329918666,
124.026224440762));
#115369=CARTESIAN_POINT('Ctrl Pts',(7.55184114426868,-28.6351320442016,
124.044622059117));
#115370=CARTESIAN_POINT('Ctrl Pts',(7.55233763938041,-28.6308718612701,
124.05073729605));
#115371=CARTESIAN_POINT('Ctrl Pts',(7.55323909002869,-28.6232544544476,
124.061829576595));
#115372=CARTESIAN_POINT('Ctrl Pts',(7.55364307773244,-28.6198829069617,
124.066796460053));
#115373=CARTESIAN_POINT('Ctrl Pts',(7.55455858030701,-28.6123374276834,
124.078042607479));
#115374=CARTESIAN_POINT('Ctrl Pts',(7.55507108010478,-28.6081792649811,
124.084332001072));
#115375=CARTESIAN_POINT('Ctrl Pts',(7.55664676956547,-28.5955908428902,
124.103656371831));
#115376=CARTESIAN_POINT('Ctrl Pts',(7.55771831451886,-28.5873002316814,
124.116780717));
#115377=CARTESIAN_POINT('Ctrl Pts',(7.56600866908977,-28.5251211143859,
124.218328180392));
#115378=CARTESIAN_POINT('Ctrl Pts',(7.57359506488849,-28.4794031811977,
124.311479489786));
#115379=CARTESIAN_POINT('Ctrl Pts',(7.58919660152276,-28.4031904057528,
124.512060742581));
#115380=CARTESIAN_POINT('Ctrl Pts',(7.59715701738913,-28.3742206318665,
124.61955899875));
#115381=CARTESIAN_POINT('Ctrl Pts',(7.60619182603659,-28.352793720861,124.749606347116));
#115382=CARTESIAN_POINT('Ctrl Pts',(7.60760061138425,-28.3498062521622,
124.77011705312));
#115383=CARTESIAN_POINT('Ctrl Pts',(7.60981047905332,-28.3456863192798,
124.802648026804));
#115384=CARTESIAN_POINT('Ctrl Pts',(7.61061942888788,-28.3443005084163,
124.814633437821));
#115385=CARTESIAN_POINT('Ctrl Pts',(7.61213767996794,-28.3419321814745,
124.837268737546));
#115386=CARTESIAN_POINT('Ctrl Pts',(7.61284781990361,-28.3409217848343,
124.847915024808));
#115387=CARTESIAN_POINT('Ctrl Pts',(7.61445094883416,-28.3388631484173,
124.872077651338));
#115388=CARTESIAN_POINT('Ctrl Pts',(7.61534194689051,-28.3378772261518,
124.885598646541));
#115389=CARTESIAN_POINT('Ctrl Pts',(7.61765231313363,-28.3357369428939,
124.920883550426));
#115390=CARTESIAN_POINT('Ctrl Pts',(7.61906355764825,-28.3348443731604,
124.942661143777));
#115391=CARTESIAN_POINT('Ctrl Pts',(7.62983741626248,-28.3312639782071,
125.110416882985));
#115392=CARTESIAN_POINT('Ctrl Pts',(7.6385608707445,-28.3473477973736,125.256153014513));
#115393=CARTESIAN_POINT('Ctrl Pts',(7.65040919414744,-28.3933123002938,
125.443019724587));
#115394=CARTESIAN_POINT('Ctrl Pts',(7.65329581305405,-28.4062818674135,
125.487620514038));
#115395=CARTESIAN_POINT('Ctrl Pts',(7.65724268492099,-28.4260463842847,
125.546321056607));
#115396=CARTESIAN_POINT('Ctrl Pts',(7.65823906327717,-28.4312016068929,
125.56095294855));
#115397=CARTESIAN_POINT('Ctrl Pts',(7.65924494691568,-28.4365599837121,
125.575509613707));
#115398=CARTESIAN_POINT('',(7.42925547773031,-28.3340002666303,125.00126447839));
#115399=CARTESIAN_POINT('Ctrl Pts',(7.46828914249572,-28.4365600390074,
125.575509763924));
#115400=CARTESIAN_POINT('Ctrl Pts',(7.46566403364243,-28.4217367851707,
125.535240651473));
#115401=CARTESIAN_POINT('Ctrl Pts',(7.46302721323805,-28.4084671937405,
125.4943930358));
#115402=CARTESIAN_POINT('Ctrl Pts',(7.45746219409187,-28.3842248370625,
125.408607547837));
#115403=CARTESIAN_POINT('Ctrl Pts',(7.45453113574382,-28.3735189901549,
125.363659456007));
#115404=CARTESIAN_POINT('Ctrl Pts',(7.45075731402903,-28.3625047376426,
125.307077621908));
#115405=CARTESIAN_POINT('Ctrl Pts',(7.45000126478169,-28.3604307183729,
125.295803909537));
#115406=CARTESIAN_POINT('Ctrl Pts',(7.44879320517343,-28.3573287892267,
125.277906829833));
#115407=CARTESIAN_POINT('Ctrl Pts',(7.44834534534316,-28.3562241901259,
125.271296877405));
#115408=CARTESIAN_POINT('Ctrl Pts',(7.44748341995341,-28.3541855607317,
125.258627946203));
#115409=CARTESIAN_POINT('Ctrl Pts',(7.44706971401807,-28.3532450518384,
125.252570225264));
#115410=CARTESIAN_POINT('Ctrl Pts',(7.44623518833265,-28.3514234566647,
125.240394645433));
#115411=CARTESIAN_POINT('Ctrl Pts',(7.44581434796839,-28.3505429368899,
125.234276756687));
#115412=CARTESIAN_POINT('Ctrl Pts',(7.4448067979077,-28.3485247804576,125.219678865607));
#115413=CARTESIAN_POINT('Ctrl Pts',(7.44421850973425,-28.3474183988451,
125.211194812517));
#115414=CARTESIAN_POINT('Ctrl Pts',(7.44213373575981,-28.343748285315,125.181254517956));
#115415=CARTESIAN_POINT('Ctrl Pts',(7.44062121653562,-28.341536808702,125.159758208545));
#115416=CARTESIAN_POINT('Ctrl Pts',(7.4358635283949,-28.3359510074493,125.092666290553));
#115417=CARTESIAN_POINT('Ctrl Pts',(7.43257070150379,-28.3340351188065,
125.046972984103));
#115418=CARTESIAN_POINT('Ctrl Pts',(7.42925570628143,-28.3340004783878,
125.001262532282));
#115419=CARTESIAN_POINT('Ctrl Pts',(7.42925584547015,-28.3340004798433,
125.001264451555));
#115420=CARTESIAN_POINT('Ctrl Pts',(7.41937356250201,-28.3338970568045,
124.864997678517));
#115421=CARTESIAN_POINT('Ctrl Pts',(7.40939540494581,-28.3505132779832,
124.729197461488));
#115422=CARTESIAN_POINT('Ctrl Pts',(7.39773132741014,-28.3911308944978,
124.566304272887));
#115423=CARTESIAN_POINT('Ctrl Pts',(7.39556511349714,-28.3996344491601,
124.535907207785));
#115424=CARTESIAN_POINT('Ctrl Pts',(7.39246814011792,-28.4131923344622,
124.492262430278));
#115425=CARTESIAN_POINT('Ctrl Pts',(7.3915154280401,-28.4175596931546,124.478810299596));
#115426=CARTESIAN_POINT('Ctrl Pts',(7.38984774049602,-28.4255507270181,
124.455223648547));
#115427=CARTESIAN_POINT('Ctrl Pts',(7.38913044314721,-28.4291022414426,
124.445065744617));
#115428=CARTESIAN_POINT('Ctrl Pts',(7.3876370005742,-28.4367355615591,124.42389389732));
#115429=CARTESIAN_POINT('Ctrl Pts',(7.38686151707715,-28.4408359388719,
124.412887243857));
#115430=CARTESIAN_POINT('Ctrl Pts',(7.38482643944949,-28.4519554683061,
124.383977367569));
#115431=CARTESIAN_POINT('Ctrl Pts',(7.38357337554834,-28.4591689007725,
124.366150389133));
#115432=CARTESIAN_POINT('Ctrl Pts',(7.37751434511364,-28.4958143138997,
124.279911516966));
#115433=CARTESIAN_POINT('Ctrl Pts',(7.37285459654274,-28.5295037414308,
124.213396714037));
#115434=CARTESIAN_POINT('Ctrl Pts',(7.36165100731372,-28.6223364616383,
124.057069095073));
#115435=CARTESIAN_POINT('Ctrl Pts',(7.35521642813294,-28.6859235125185,
123.9703029597));
#115436=CARTESIAN_POINT('Ctrl Pts',(7.34666551916549,-28.7768993101918,
123.868436096094));
#115437=CARTESIAN_POINT('Ctrl Pts',(7.34481288550097,-28.7969603816424,
123.847130689847));
#115438=CARTESIAN_POINT('Ctrl Pts',(7.34167301274474,-28.8312979142142,
123.812535837829));
#115439=CARTESIAN_POINT('Ctrl Pts',(7.34040383027099,-28.8452658892386,
123.798948479201));
#115440=CARTESIAN_POINT('Ctrl Pts',(7.33859563195503,-28.8652266594629,
123.780201707463));
#115441=CARTESIAN_POINT('Ctrl Pts',(7.33807115532862,-28.8710233718836,
123.77483463326));
#115442=CARTESIAN_POINT('Ctrl Pts',(7.33753990228832,-28.8768990011261,
123.769471597473));
#115443=CARTESIAN_POINT('Ctrl Pts',(7.3375361850848,-28.8769401133886,123.769434075646));
#115444=CARTESIAN_POINT('Ctrl Pts',(7.33752867773757,-28.8770231450277,
123.769358302991));
#115445=CARTESIAN_POINT('Ctrl Pts',(7.33752488757879,-28.8770650645789,
123.769320052154));
#115446=CARTESIAN_POINT('Ctrl Pts',(7.3375172304766,-28.8771497533367,123.769242783113));
#115447=CARTESIAN_POINT('Ctrl Pts',(7.33751336352829,-28.8771925226056,
123.769203765013));
#115448=CARTESIAN_POINT('Ctrl Pts',(7.3375055487759,-28.8772789558496,123.769124920833));
#115449=CARTESIAN_POINT('Ctrl Pts',(7.33750160096349,-28.8773226199255,
123.769085094833));
#115450=CARTESIAN_POINT('Ctrl Pts',(7.33749362014911,-28.8774108907405,
123.769004591635));
#115451=CARTESIAN_POINT('Ctrl Pts',(7.33748958715301,-28.877455497424,123.768963914672));
#115452=CARTESIAN_POINT('Ctrl Pts',(7.33748143137279,-28.8775457043416,
123.768881663703));
#115453=CARTESIAN_POINT('Ctrl Pts',(7.3374773085818,-28.8775913046616,123.768840089819));
#115454=CARTESIAN_POINT('Ctrl Pts',(7.33746896833499,-28.8776835528198,
123.768755996411));
#115455=CARTESIAN_POINT('Ctrl Pts',(7.33746475083882,-28.8777302011151,
123.768713476686));
#115456=CARTESIAN_POINT('Ctrl Pts',(7.33745621592777,-28.8778246033652,
123.768627439252));
#115457=CARTESIAN_POINT('Ctrl Pts',(7.33745189852428,-28.8778723572058,
123.76858392188));
#115458=CARTESIAN_POINT('Ctrl Pts',(7.3374431582116,-28.8779690323747,123.768495833515));
#115459=CARTESIAN_POINT('Ctrl Pts',(7.33743873528734,-28.8780179538823,
123.768451262609));
#115460=CARTESIAN_POINT('Ctrl Pts',(7.33742977795473,-28.8781170305464,
123.76836100766));
#115461=CARTESIAN_POINT('Ctrl Pts',(7.33742524354762,-28.8781671857026,
123.768315323888));
#115462=CARTESIAN_POINT('Ctrl Pts',(7.33741605686236,-28.8782688003468,
123.768222779652));
#115463=CARTESIAN_POINT('Ctrl Pts',(7.33741140455526,-28.8783202601695,
123.768175919176));
#115464=CARTESIAN_POINT('Ctrl Pts',(7.33740197519525,-28.8784245602297,
123.768080953143));
#115465=CARTESIAN_POINT('Ctrl Pts',(7.33739719814064,-28.8784774005015,
123.768032847873));
#115466=CARTESIAN_POINT('Ctrl Pts',(7.33738751191134,-28.8785845430714,
123.767935318925));
#115467=CARTESIAN_POINT('Ctrl Pts',(7.33738260271761,-28.8786388455971,
123.767885895386));
#115468=CARTESIAN_POINT('Ctrl Pts',(7.33737264427328,-28.878749000513,123.767785651012));
#115469=CARTESIAN_POINT('Ctrl Pts',(7.33736759501287,-28.8788048530301,
123.767734830439));
#115470=CARTESIAN_POINT('Ctrl Pts',(7.33735734788781,-28.8789182025261,
123.767631707072));
#115471=CARTESIAN_POINT('Ctrl Pts',(7.33735215000152,-28.8789756997641,
123.767579404456));
#115472=CARTESIAN_POINT('Ctrl Pts',(7.33734159640269,-28.879092440767,123.767473225416));
#115473=CARTESIAN_POINT('Ctrl Pts',(7.3373362406618,-28.8791516848669,123.767419349139));
#115474=CARTESIAN_POINT('Ctrl Pts',(7.33732536135549,-28.8792720302513,
123.767309923524));
#115475=CARTESIAN_POINT('Ctrl Pts',(7.3373198377936,-28.8793331315201,123.767254374694));
#115476=CARTESIAN_POINT('Ctrl Pts',(7.33730861205778,-28.8794573106368,
123.767141496935));
#115477=CARTESIAN_POINT('Ctrl Pts',(7.33730290984146,-28.8795203889788,
123.767084168099));
#115478=CARTESIAN_POINT('Ctrl Pts',(7.33729131506578,-28.8796486520813,
123.76696761398));
#115479=CARTESIAN_POINT('Ctrl Pts',(7.33728542249567,-28.8797138369881,
123.766908389161));
#115480=CARTESIAN_POINT('Ctrl Pts',(7.33727343427613,-28.8798464541867,
123.76678791682));
#115481=CARTESIAN_POINT('Ctrl Pts',(7.33726733858723,-28.8799138869453,
123.766726669533));
#115482=CARTESIAN_POINT('Ctrl Pts',(7.33725493025597,-28.8800511534114,
123.766602014789));
#115483=CARTESIAN_POINT('Ctrl Pts',(7.33724861758046,-28.8801209875185,
123.766538607698));
#115484=CARTESIAN_POINT('Ctrl Pts',(7.33723576012546,-28.8802632243746,
123.766409483308));
#115485=CARTESIAN_POINT('Ctrl Pts',(7.33722921531702,-28.8803356274802,
123.766343766493));
#115486=CARTESIAN_POINT('Ctrl Pts',(7.33721587703332,-28.8804831856614,
123.766209858723));
#115487=CARTESIAN_POINT('Ctrl Pts',(7.33720908352888,-28.8805583410998,
123.766141668336));
#115488=CARTESIAN_POINT('Ctrl Pts',(7.33719522971353,-28.8807116047312,
123.766002633983));
#115489=CARTESIAN_POINT('Ctrl Pts',(7.33718816935918,-28.8807897134486,
123.765931790541));
#115490=CARTESIAN_POINT('Ctrl Pts',(7.33717376191652,-28.8809491042154,
123.765787253071));
#115491=CARTESIAN_POINT('Ctrl Pts',(7.3371664147823,-28.8810303868209,123.765713559655));
#115492=CARTESIAN_POINT('Ctrl Pts',(7.33715141183802,-28.8811963682422,
123.765563105448));
#115493=CARTESIAN_POINT('Ctrl Pts',(7.33714375597763,-28.8812810676682,
123.765486345354));
#115494=CARTESIAN_POINT('Ctrl Pts',(7.33712811137022,-28.8814541507277,
123.765329518739));
#115495=CARTESIAN_POINT('Ctrl Pts',(7.3371201225614,-28.8815425351041,123.76524945295));
#115496=CARTESIAN_POINT('Ctrl Pts',(7.33710378526031,-28.8817232846925,
123.765085750537));
#115497=CARTESIAN_POINT('Ctrl Pts',(7.33709543670959,-28.8818156506169,
123.765002114852));
#115498=CARTESIAN_POINT('Ctrl Pts',(7.33707835020737,-28.8820046922629,
123.764830979631));
#115499=CARTESIAN_POINT('Ctrl Pts',(7.33706961217501,-28.8821013689524,
123.764743481011));
#115500=CARTESIAN_POINT('Ctrl Pts',(7.33705171364309,-28.88229939817,123.764564294126));
#115501=CARTESIAN_POINT('Ctrl Pts',(7.33704255305717,-28.8824007517355,
123.764472606958));
#115502=CARTESIAN_POINT('Ctrl Pts',(7.33663053392987,-28.8869594097029,
123.76034974194));
#115503=CARTESIAN_POINT('Ctrl Pts',(7.33622585682368,-28.8914382500251,
123.756342908708));
#115504=CARTESIAN_POINT('Ctrl Pts',(7.33529423576552,-28.9017526234754,
123.747215512634));
#115505=CARTESIAN_POINT('Ctrl Pts',(7.33476613887717,-28.9076023211805,
123.742111460775));
#115506=CARTESIAN_POINT('Ctrl Pts',(7.33313221068919,-28.9257165314535,
123.726527868962));
#115507=CARTESIAN_POINT('Ctrl Pts',(7.33201737203806,-28.9380973441982,
123.716185784042));
#115508=CARTESIAN_POINT('Ctrl Pts',(7.32524300079625,-29.0135665541961,
123.654982531475));
#115509=CARTESIAN_POINT('Ctrl Pts',(7.31936060053549,-29.0801418395196,
123.608604505391));
#115510=CARTESIAN_POINT('Ctrl Pts',(7.30809840553617,-29.2132134421988,
123.529640580684));
#115511=CARTESIAN_POINT('Ctrl Pts',(7.30273296111614,-29.2790383951908,
123.496269443176));
#115512=CARTESIAN_POINT('Ctrl Pts',(7.29443954209551,-29.3859518810057,
123.450707724317));
#115513=CARTESIAN_POINT('Ctrl Pts',(7.29144364339463,-29.4256686705819,
123.435549401915));
#115514=CARTESIAN_POINT('Ctrl Pts',(7.28637067906987,-29.4949032954147,
123.412117991926));
#115515=CARTESIAN_POINT('Ctrl Pts',(7.28427213274951,-29.5241482047487,
123.403110136906));
#115516=CARTESIAN_POINT('Ctrl Pts',(7.2812527744722,-29.5670919198683,123.391167523035));
#115517=CARTESIAN_POINT('Ctrl Pts',(7.28031152315644,-29.5806044218695,
123.38759226171));
#115518=CARTESIAN_POINT('Ctrl Pts',(7.27865680691216,-29.6045756792918,
123.38157146536));
#115519=CARTESIAN_POINT('Ctrl Pts',(7.27794113709066,-29.6150159289277,
123.379056265799));
#115520=CARTESIAN_POINT('Ctrl Pts',(7.27644419888003,-29.6370020031624,
123.373983924632));
#115521=CARTESIAN_POINT('Ctrl Pts',(7.27566365833539,-29.6485522407399,
123.371448401889));
#115522=CARTESIAN_POINT('Ctrl Pts',(7.27359932949598,-29.6793201674347,
123.365036774304));
#115523=CARTESIAN_POINT('Ctrl Pts',(7.27232242428435,-29.6985812996632,
123.361376454428));
#115524=CARTESIAN_POINT('Ctrl Pts',(7.26572003761559,-29.7992701004747,
123.344077448166));
#115525=CARTESIAN_POINT('Ctrl Pts',(7.26057783867157,-29.8815687264981,
123.336164517924));
#115526=CARTESIAN_POINT('Ctrl Pts',(7.24935299960241,-30.0642848271456,
123.332228919761));
#115527=CARTESIAN_POINT('Ctrl Pts',(7.24332891776974,-30.1644297034915,
123.339110646512));
#115528=CARTESIAN_POINT('Ctrl Pts',(7.2352760958641,-30.291265492037,123.359414721593));
#115529=CARTESIAN_POINT('Ctrl Pts',(7.23348340206691,-30.3190680616087,
123.364594535179));
#115530=CARTESIAN_POINT('Ctrl Pts',(7.23041619746381,-30.3656033433355,
123.374496147947));
#115531=CARTESIAN_POINT('Ctrl Pts',(7.22915800970899,-30.3844107486517,
123.378840885009));
#115532=CARTESIAN_POINT('Ctrl Pts',(7.22733982705669,-30.411108918281,123.385499162527));
#115533=CARTESIAN_POINT('Ctrl Pts',(7.22679388058043,-30.419065389015,123.387546065891));
#115534=CARTESIAN_POINT('Ctrl Pts',(7.22583988544353,-30.43285706367,123.391203119674));
#115535=CARTESIAN_POINT('Ctrl Pts',(7.22543336601706,-30.4386991592339,
123.392786359547));
#115536=CARTESIAN_POINT('Ctrl Pts',(7.22455607664872,-30.4512298385684,
123.396255655373));
#115537=CARTESIAN_POINT('Ctrl Pts',(7.22408478089844,-30.4579151878881,
123.398151703052));
#115538=CARTESIAN_POINT('Ctrl Pts',(7.22277460481303,-30.4763777855145,
123.403512944941));
#115539=CARTESIAN_POINT('Ctrl Pts',(7.22193097773102,-30.4881286172494,
123.407066497805));
#115540=CARTESIAN_POINT('Ctrl Pts',(7.21600304099805,-30.5698194900865,
123.432759272902));
#115541=CARTESIAN_POINT('Ctrl Pts',(7.21071563021698,-30.6382626970609,
123.459365035987));
#115542=CARTESIAN_POINT('Ctrl Pts',(7.2043685736538,-30.7174246406035,123.49631971207));
#115543=CARTESIAN_POINT('Ctrl Pts',(7.20334869084487,-30.7300519515729,
123.502409713044));
#115544=CARTESIAN_POINT('Ctrl Pts',(7.19696317027417,-30.8085877946221,
123.541515964453));
#115545=CARTESIAN_POINT('Ctrl Pts',(7.19159772852778,-30.8723254076313,
123.578719028349));
#115546=CARTESIAN_POINT('Ctrl Pts',(7.18330430391382,-30.9685899044678,
123.643830669137));
#115547=CARTESIAN_POINT('Ctrl Pts',(7.18030839739543,-31.0028661240677,
123.668977199263));
#115548=CARTESIAN_POINT('Ctrl Pts',(7.17523542145845,-31.0601023804654,
123.714435960794));
#115549=CARTESIAN_POINT('Ctrl Pts',(7.1731368712097,-31.0835317051256,123.734120379615));
#115550=CARTESIAN_POINT('Ctrl Pts',(7.17011750841782,-31.1168563945396,
123.763722062387));
#115551=CARTESIAN_POINT('Ctrl Pts',(7.16917625642977,-31.1271888306669,
123.773135416704));
#115552=CARTESIAN_POINT('Ctrl Pts',(7.16752153942846,-31.1452483215704,
123.790009257428));
#115553=CARTESIAN_POINT('Ctrl Pts',(7.16680586951508,-31.1530238678371,
123.797416412614));
#115554=CARTESIAN_POINT('Ctrl Pts',(7.16530893152689,-31.1692098174702,
123.813136812569));
#115555=CARTESIAN_POINT('Ctrl Pts',(7.16452839129268,-31.1776044514178,
123.821465490075));
#115556=CARTESIAN_POINT('Ctrl Pts',(7.16246406424493,-31.1996785387533,
123.843837508329));
#115557=CARTESIAN_POINT('Ctrl Pts',(7.16118716049282,-31.2132002642859,
123.858034381055));
#115558=CARTESIAN_POINT('Ctrl Pts',(7.15458482406676,-31.2823433796613,
123.93324448832));
#115559=CARTESIAN_POINT('Ctrl Pts',(7.14944267019436,-31.3336267731865,
123.998094823561));
#115560=CARTESIAN_POINT('Ctrl Pts',(7.13821783412521,-31.4360320549009,
124.149467822659));
#115561=CARTESIAN_POINT('Ctrl Pts',(7.13219371430047,-31.484565796549,124.237336837175));
#115562=CARTESIAN_POINT('Ctrl Pts',(7.12414084670429,-31.5362989646492,
124.354909976433));
#115563=CARTESIAN_POINT('Ctrl Pts',(7.1223481478214,-31.5470263291784,124.38107754618));
#115564=CARTESIAN_POINT('Ctrl Pts',(7.11928093539525,-31.5639466675181,
124.425544257186));
#115565=CARTESIAN_POINT('Ctrl Pts',(7.11802274501155,-31.5704969411154,
124.443701645393));
#115566=CARTESIAN_POINT('Ctrl Pts',(7.11620455921831,-31.5793831768821,
124.469743196566));
#115567=CARTESIAN_POINT('Ctrl Pts',(7.11565861229608,-31.5819787905467,
124.477537947534));
#115568=CARTESIAN_POINT('Ctrl Pts',(7.1147046166567,-31.5863864520248,124.491108396063));
#115569=CARTESIAN_POINT('Ctrl Pts',(7.11429809717877,-31.5882248464276,
124.496875288251));
#115570=CARTESIAN_POINT('Ctrl Pts',(7.11342080802908,-31.5921063296269,
124.509284476255));
#115571=CARTESIAN_POINT('Ctrl Pts',(7.11294951255185,-31.5941392697469,
124.515929473807));
#115572=CARTESIAN_POINT('Ctrl Pts',(7.1116393379471,-31.59964850111,124.534348430723));
#115573=CARTESIAN_POINT('Ctrl Pts',(7.11079571208955,-31.6030362313227,
124.546148118841));
#115574=CARTESIAN_POINT('Ctrl Pts',(7.10486810396721,-31.6257555532954,
124.62871044262));
#115575=CARTESIAN_POINT('Ctrl Pts',(7.09958104660358,-31.6405233864013,
124.700637864255));
#115576=CARTESIAN_POINT('Ctrl Pts',(7.09323408216949,-31.6524113279818,
124.787186876037));
#115577=CARTESIAN_POINT('Ctrl Pts',(7.09221394195506,-31.6541439652191,
124.801102133685));
#115578=CARTESIAN_POINT('Ctrl Pts',(7.08582818790081,-31.6638846674983,
124.888296515404));
#115579=CARTESIAN_POINT('Ctrl Pts',(7.0804627678863,-31.6671979128064,124.962022529068));
#115580=CARTESIAN_POINT('Ctrl Pts',(7.07216929790442,-31.6647055032124,
125.078213287153));
#115581=CARTESIAN_POINT('Ctrl Pts',(7.06917332793634,-31.6621690309992,
125.120649678821));
#115582=CARTESIAN_POINT('Ctrl Pts',(7.06410025774465,-31.6550199938247,
125.193392874174));
#115583=CARTESIAN_POINT('Ctrl Pts',(7.06200167560689,-31.6511894478119,
125.223753445864));
#115584=CARTESIAN_POINT('Ctrl Pts',(7.05898227616285,-31.6443938353568,
125.267806388092));
#115585=CARTESIAN_POINT('Ctrl Pts',(7.05804101871024,-31.6420892000036,
125.281592661778));
#115586=CARTESIAN_POINT('Ctrl Pts',(7.05638629554762,-31.6377075609206,
125.305917080741));
#115587=CARTESIAN_POINT('Ctrl Pts',(7.05567062488179,-31.6357016648871,
125.316467041181));
#115588=CARTESIAN_POINT('Ctrl Pts',(7.05417368868203,-31.6312729607665,
125.33859171503));
#115589=CARTESIAN_POINT('Ctrl Pts',(7.05339315095625,-31.6288286352117,
125.350161550237));
#115590=CARTESIAN_POINT('Ctrl Pts',(7.05132883841502,-31.6220051785355,
125.380840513879));
#115591=CARTESIAN_POINT('Ctrl Pts',(7.0500519464842,-31.6174115181461,125.399900399846));
#115592=CARTESIAN_POINT('Ctrl Pts',(7.04345001705135,-31.5917266271684,
125.498775696548));
#115593=CARTESIAN_POINT('Ctrl Pts',(7.03830822828367,-31.5650597775483,
125.577027929199));
#115594=CARTESIAN_POINT('Ctrl Pts',(7.02708341661256,-31.4934279498487,
125.745162450392));
#115595=CARTESIAN_POINT('Ctrl Pts',(7.02105898912504,-31.445926384267,125.833599824145));
#115596=CARTESIAN_POINT('Ctrl Pts',(7.01300575153124,-31.3752031879176,
125.940835733467));
#115597=CARTESIAN_POINT('Ctrl Pts',(7.01121301146626,-31.3590364583208,
125.964041186931));
#115598=CARTESIAN_POINT('Ctrl Pts',(7.00814573569051,-31.3308544565283,
126.002374684314));
#115599=CARTESIAN_POINT('Ctrl Pts',(7.00688752401667,-31.3191520825185,
126.017726042458));
#115600=CARTESIAN_POINT('Ctrl Pts',(7.0050693127822,-31.302092779623,126.039316068949));
#115601=CARTESIAN_POINT('Ctrl Pts',(7.00452336224373,-31.2969518038483,
126.045724394579));
#115602=CARTESIAN_POINT('Ctrl Pts',(7.00356936252713,-31.2879411982705,
126.056787636949));
#115603=CARTESIAN_POINT('Ctrl Pts',(7.00316284262883,-31.2840932562691,
126.061459913361));
#115604=CARTESIAN_POINT('Ctrl Pts',(7.00228555524054,-31.2757729511287,
126.071451196654));
#115605=CARTESIAN_POINT('Ctrl Pts',(7.00181426197055,-31.2712928142239,
126.076763142823));
#115606=CARTESIAN_POINT('Ctrl Pts',(7.00050409934027,-31.2588063705757,
126.091381339864));
#115607=CARTESIAN_POINT('Ctrl Pts',(6.99966048338448,-31.250730417711,126.10062714291));
#115608=CARTESIAN_POINT('Ctrl Pts',(6.99373552866349,-31.1937139035421,
126.164464929997));
#115609=CARTESIAN_POINT('Ctrl Pts',(6.98845132493557,-31.1413232049315,
126.215857893132));
#115610=CARTESIAN_POINT('Ctrl Pts',(6.98210511512545,-31.0750684962294,
126.272784801032));
#115611=CARTESIAN_POINT('Ctrl Pts',(6.98108290718335,-31.0642959778432,
126.2818063384));
#115612=CARTESIAN_POINT('Ctrl Pts',(6.97469528415801,-30.9963042459605,
126.337298509323));
#115613=CARTESIAN_POINT('Ctrl Pts',(6.96933004491224,-30.9361638930803,
126.380068089586));
#115614=CARTESIAN_POINT('Ctrl Pts',(6.96103620405767,-30.8371928219746,
126.440996362045));
#115615=CARTESIAN_POINT('Ctrl Pts',(6.95803971253382,-30.8001585946025,
126.461885447702));
#115616=CARTESIAN_POINT('Ctrl Pts',(6.95296586758419,-30.7351571617461,
126.495338142216));
#115617=CARTESIAN_POINT('Ctrl Pts',(6.95086702333251,-30.7075690942456,
126.508588214968));
#115618=CARTESIAN_POINT('Ctrl Pts',(6.94784732262703,-30.666868660664,126.526773576812));
#115619=CARTESIAN_POINT('Ctrl Pts',(6.94690602026148,-30.6540356781177,
126.532314823348));
#115620=CARTESIAN_POINT('Ctrl Pts',(6.9452512464592,-30.631222573742,126.541826637324));
#115621=CARTESIAN_POINT('Ctrl Pts',(6.94453556960922,-30.6212710976615,
126.545863367073));
#115622=CARTESIAN_POINT('Ctrl Pts',(6.94303864810687,-30.6002814658965,
126.554142199428));
#115623=CARTESIAN_POINT('Ctrl Pts',(6.94225813099632,-30.5892357413782,
126.558363586445));
#115624=CARTESIAN_POINT('Ctrl Pts',(6.94019393767106,-30.5597619733041,
126.569269501898));
#115625=CARTESIAN_POINT('Ctrl Pts',(6.93891714288803,-30.5412589630261,
126.575747131965));
#115626=CARTESIAN_POINT('Ctrl Pts',(6.93231854793044,-30.4443083444405,
126.607778791493));
#115627=CARTESIAN_POINT('Ctrl Pts',(6.92717975028263,-30.3641521168646,
126.627807810239));
#115628=CARTESIAN_POINT('Ctrl Pts',(6.91595513760539,-30.18405382767,126.658833050549));
#115629=CARTESIAN_POINT('Ctrl Pts',(6.90992818902548,-30.0839471097344,
126.666899348882));
#115630=CARTESIAN_POINT('Ctrl Pts',(6.90187191962886,-29.9554464691717,
126.66564431401));
#115631=CARTESIAN_POINT('Ctrl Pts',(6.9000788422117,-29.9271767683142,126.664647889031));
#115632=CARTESIAN_POINT('Ctrl Pts',(6.89701104750156,-29.8796779515927,
126.661761505974));
#115633=CARTESIAN_POINT('Ctrl Pts',(6.89575266143302,-29.8604309189347,
126.660255730827));
#115634=CARTESIAN_POINT('Ctrl Pts',(6.89393424180196,-29.8330366551162,
126.657632874581));
#115635=CARTESIAN_POINT('Ctrl Pts',(6.89338826164524,-29.8248640052282,
126.656789329324));
#115636=CARTESIAN_POINT('Ctrl Pts',(6.892434228536,-29.8106817515041,126.655219393704));
#115637=CARTESIAN_POINT('Ctrl Pts',(6.89202770519594,-29.8046693250667,
126.654520645563));
#115638=CARTESIAN_POINT('Ctrl Pts',(6.89115043223224,-29.7917627761054,
126.652949347267));
#115639=CARTESIAN_POINT('Ctrl Pts',(6.89067915704018,-29.7848703689007,
126.652066440391));
#115640=CARTESIAN_POINT('Ctrl Pts',(6.88936909248049,-29.7658181847186,
126.649504639765));
#115641=CARTESIAN_POINT('Ctrl Pts',(6.88852555761921,-29.7536714157406,
126.647734470626));
#115642=CARTESIAN_POINT('Ctrl Pts',(6.88262203406951,-29.6694203980064,
126.634504047185));
#115643=CARTESIAN_POINT('Ctrl Pts',(6.87736087397863,-29.598125213307,126.618450075721));
#115644=CARTESIAN_POINT('Ctrl Pts',(6.87107459106674,-29.5151362300872,
126.593940539202));
#115645=CARTESIAN_POINT('Ctrl Pts',(6.87008966013403,-29.50219848629,126.589947473144));
#115646=CARTESIAN_POINT('Ctrl Pts',(6.86362724625123,-29.417678652807,126.562728761375));
#115647=CARTESIAN_POINT('Ctrl Pts',(6.85814858885033,-29.347687078278,126.534831778095));
#115648=CARTESIAN_POINT('Ctrl Pts',(6.84977682634256,-29.2418592223927,
126.48409924935));
#115649=CARTESIAN_POINT('Ctrl Pts',(6.84681000740223,-29.2046011283282,
126.464468895143));
#115650=CARTESIAN_POINT('Ctrl Pts',(6.8417802780461,-29.1417982028294,126.428274802709));
#115651=CARTESIAN_POINT('Ctrl Pts',(6.83969638087453,-29.1158909670876,
126.412384743522));
#115652=CARTESIAN_POINT('Ctrl Pts',(6.83669386733622,-29.0787521044276,
126.388183216752));
#115653=CARTESIAN_POINT('Ctrl Pts',(6.8357551326363,-29.0671685556515,126.38042596517));
#115654=CARTESIAN_POINT('Ctrl Pts',(6.83410325132563,-29.0468403746469,
126.366439879747));
#115655=CARTESIAN_POINT('Ctrl Pts',(6.83338792544044,-29.0380561584206,
126.360270293465));
#115656=CARTESIAN_POINT('Ctrl Pts',(6.83189015047112,-29.0197067624715,
126.347115965969));
#115657=CARTESIAN_POINT('Ctrl Pts',(6.83110844423959,-29.0101551691849,
126.340113234175));
#115658=CARTESIAN_POINT('Ctrl Pts',(6.82903737442185,-28.9849243587417,
126.321198372519));
#115659=CARTESIAN_POINT('Ctrl Pts',(6.82775497627883,-28.9693799756157,
126.309108901373));
#115660=CARTESIAN_POINT('Ctrl Pts',(6.82092612384948,-28.8871211774187,
126.242759497642));
#115661=CARTESIAN_POINT('Ctrl Pts',(6.81558021507435,-28.8244652367482,
126.18366852511));
#115662=CARTESIAN_POINT('Ctrl Pts',(6.80433857306496,-28.7012775650826,
126.048012769568));
#115663=CARTESIAN_POINT('Ctrl Pts',(6.79848425521836,-28.6423411790938,
125.970448862313));
#115664=CARTESIAN_POINT('Ctrl Pts',(6.79063594300864,-28.5756346710899,
125.864591084913));
#115665=CARTESIAN_POINT('Ctrl Pts',(6.78886641990585,-28.5613571208815,
125.840619311241));
#115666=CARTESIAN_POINT('Ctrl Pts',(6.78583488723391,-28.5383237954122,
125.79963991741));
#115667=CARTESIAN_POINT('Ctrl Pts',(6.78458871081901,-28.529246546389,125.782818962133));
#115668=CARTESIAN_POINT('Ctrl Pts',(6.78278488693997,-28.5166990017146,
125.758578359584));
#115669=CARTESIAN_POINT('Ctrl Pts',(6.78224098759198,-28.5129905523876,
125.751282819538));
#115670=CARTESIAN_POINT('Ctrl Pts',(6.78128929646074,-28.5066348190222,
125.738547918945));
#115671=CARTESIAN_POINT('Ctrl Pts',(6.78088301092258,-28.5039631655978,
125.733120986649));
#115672=CARTESIAN_POINT('Ctrl Pts',(6.78000470670348,-28.4982778978357,
125.721411997249));
#115673=CARTESIAN_POINT('Ctrl Pts',(6.77953214744316,-28.4952741615286,
125.715125645257));
#115674=CARTESIAN_POINT('Ctrl Pts',(6.77821511087333,-28.4870524111867,
125.697637655391));
#115675=CARTESIAN_POINT('Ctrl Pts',(6.77736580947579,-28.4819195884693,
125.686396784898));
#115676=CARTESIAN_POINT('Ctrl Pts',(6.77402887620946,-28.4623887797075,
125.642333507151));
#115677=CARTESIAN_POINT('Ctrl Pts',(6.77149707433844,-28.4489317881972,
125.609119081009));
#115678=CARTESIAN_POINT('Ctrl Pts',(6.7689357756443,-28.4365600093868,125.575509683456));
#115679=CARTESIAN_POINT('Origin',(5.,-30.,125.));
#115680=CARTESIAN_POINT('',(6.06644913825629,-28.4365599905855,125.57550963238));
#115681=CARTESIAN_POINT('',(6.2618827045692,-28.4365599067946,125.575509404752));
#115682=CARTESIAN_POINT('',(5.,-28.4365599837785,125.575509613888));
#115683=CARTESIAN_POINT('',(6.92206959391605,-28.3340008189938,124.998531925366));
#115684=CARTESIAN_POINT('Ctrl Pts',(6.2618827045692,-28.4365599067946,125.575509404752));
#115685=CARTESIAN_POINT('Ctrl Pts',(6.26453319938667,-28.4494969610584,
125.610654459128));
#115686=CARTESIAN_POINT('Ctrl Pts',(6.26715307047973,-28.4636223241704,
125.645372127239));
#115687=CARTESIAN_POINT('Ctrl Pts',(6.27126995743702,-28.4879893075809,
125.699910307995));
#115688=CARTESIAN_POINT('Ctrl Pts',(6.27278955539158,-28.4974691391647,
125.720036018624));
#115689=CARTESIAN_POINT('Ctrl Pts',(6.27522184522568,-28.5134282592118,
125.752228530355));
#115690=CARTESIAN_POINT('Ctrl Pts',(6.27614299564413,-28.5196579464052,
125.764415283831));
#115691=CARTESIAN_POINT('Ctrl Pts',(6.27777541001437,-28.5310278216,125.785997060839));
#115692=CARTESIAN_POINT('Ctrl Pts',(6.27848867307505,-28.5361096813697,
125.795421765339));
#115693=CARTESIAN_POINT('Ctrl Pts',(6.27999366462139,-28.5470727723749,
125.81529268462));
#115694=CARTESIAN_POINT('Ctrl Pts',(6.28078453734769,-28.5529766250115,
125.825725774838));
#115695=CARTESIAN_POINT('Ctrl Pts',(6.28290789256535,-28.5692094452626,
125.853703011054));
#115696=CARTESIAN_POINT('Ctrl Pts',(6.28423276079966,-28.579748426927,125.871123395666));
#115697=CARTESIAN_POINT('Ctrl Pts',(6.29281959222204,-28.6506788814484,
125.983657215931));
#115698=CARTESIAN_POINT('Ctrl Pts',(6.29971676160355,-28.7202679858104,
126.072631895048));
#115699=CARTESIAN_POINT('Ctrl Pts',(6.31285660422745,-28.869308642933,126.227843451257));
#115700=CARTESIAN_POINT('Ctrl Pts',(6.31908333450307,-28.9469656087316,
126.295058065134));
#115701=CARTESIAN_POINT('Ctrl Pts',(6.32674536027513,-29.0429755123075,
126.363782769096));
#115702=CARTESIAN_POINT('Ctrl Pts',(6.32776719432771,-29.0557856711485,
126.37268298221));
#115703=CARTESIAN_POINT('Ctrl Pts',(6.32930079888376,-29.0749820401044,
126.38562435));
#115704=CARTESIAN_POINT('Ctrl Pts',(6.32980385475558,-29.0812742455049,
126.389804320019));
#115705=CARTESIAN_POINT('Ctrl Pts',(6.33071183219028,-29.0926176796934,
126.397229175008));
#115706=CARTESIAN_POINT('Ctrl Pts',(6.33111571019184,-29.0976583218239,
126.400489748536));
#115707=CARTESIAN_POINT('Ctrl Pts',(6.33202416789549,-29.1089846153035,
126.407729706354));
#115708=CARTESIAN_POINT('Ctrl Pts',(6.33252965653828,-29.115279296855,126.411694235309));
#115709=CARTESIAN_POINT('Ctrl Pts',(6.33406249443389,-29.1343507452311,
126.423528202029));
#115710=CARTESIAN_POINT('Ctrl Pts',(6.33509757646537,-29.1472070915657,
126.431267057696));
#115711=CARTESIAN_POINT('Ctrl Pts',(6.33754361639287,-29.1775755955892,
126.448992916798));
#115712=CARTESIAN_POINT('Ctrl Pts',(6.33896136022004,-29.1951677578577,
126.45883767407));
#115713=CARTESIAN_POINT('Ctrl Pts',(6.3441679257121,-29.2598762787358,126.49352256554));
#115714=CARTESIAN_POINT('Ctrl Pts',(6.34802308250029,-29.3079961382248,
126.51641773694));
#115715=CARTESIAN_POINT('Ctrl Pts',(6.36157881677038,-29.479994884436,126.588360321446));
#115716=CARTESIAN_POINT('Ctrl Pts',(6.3712730371265,-29.608607765328,126.62484414707));
#115717=CARTESIAN_POINT('Ctrl Pts',(6.38223429718041,-29.7654675838344,
126.649607367618));
#115718=CARTESIAN_POINT('Ctrl Pts',(6.38398169376901,-29.7908162471649,
126.653013068482));
#115719=CARTESIAN_POINT('Ctrl Pts',(6.38660460147052,-29.8293711843941,
126.657291918874));
#115720=CARTESIAN_POINT('Ctrl Pts',(6.3874933582728,-29.8425250357522,126.658593485513));
#115721=CARTESIAN_POINT('Ctrl Pts',(6.38909041106804,-29.8663188666728,
126.660662250527));
#115722=CARTESIAN_POINT('Ctrl Pts',(6.38980037860481,-29.8769532460782,
126.661484053838));
#115723=CARTESIAN_POINT('Ctrl Pts',(6.39132185615373,-29.8998610367381,
126.663033172167));
#115724=CARTESIAN_POINT('Ctrl Pts',(6.39213227568952,-29.9121361457776,
126.663726870733));
#115725=CARTESIAN_POINT('Ctrl Pts',(6.3943693927692,-29.9462132249856,126.665274448983));
#115726=CARTESIAN_POINT('Ctrl Pts',(6.39578697157501,-29.9680264713172,
126.665836058176));
#115727=CARTESIAN_POINT('Ctrl Pts',(6.39893926136341,-30.0169624392807,
126.666134340882));
#115728=CARTESIAN_POINT('Ctrl Pts',(6.40066686821204,-30.044080590703,126.665637532037));
#115729=CARTESIAN_POINT('Ctrl Pts',(6.40631730562073,-30.1335205402861,
126.6618129418));
#115730=CARTESIAN_POINT('Ctrl Pts',(6.41016538120923,-30.1956695284297,
126.655646177167));
#115731=CARTESIAN_POINT('Ctrl Pts',(6.4196488368188,-30.348702894728,126.631721641554));
#115732=CARTESIAN_POINT('Ctrl Pts',(6.42523114005937,-30.4387221513904,
126.609853990699));
#115733=CARTESIAN_POINT('Ctrl Pts',(6.4334649209599,-30.5629835375019,126.568466721425));
#115734=CARTESIAN_POINT('Ctrl Pts',(6.43592404130443,-30.5990758195875,
126.555038896514));
#115735=CARTESIAN_POINT('Ctrl Pts',(6.4391603060366,-30.6447134498778,126.536235211082));
#115736=CARTESIAN_POINT('Ctrl Pts',(6.43987777696164,-30.6547184479179,
126.531997974782));
#115737=CARTESIAN_POINT('Ctrl Pts',(6.44103839619328,-30.6707078416453,
126.525041045625));
#115738=CARTESIAN_POINT('Ctrl Pts',(6.44147793490054,-30.6767190256917,
126.522383183106));
#115739=CARTESIAN_POINT('Ctrl Pts',(6.44233620694843,-30.6883673546834,
126.517150221002));
#115740=CARTESIAN_POINT('Ctrl Pts',(6.44275470492931,-30.6940060996796,
126.51457912859));
#115741=CARTESIAN_POINT('Ctrl Pts',(6.4437918939359,-30.7078830558456,126.508157906864));
#115742=CARTESIAN_POINT('Ctrl Pts',(6.44441271237697,-30.716104267001,126.504271704889));
#115743=CARTESIAN_POINT('Ctrl Pts',(6.44676505233764,-30.7469521745781,
126.48937958442));
#115744=CARTESIAN_POINT('Ctrl Pts',(6.44852038672317,-30.7693591700143,
126.477929429874));
#115745=CARTESIAN_POINT('Ctrl Pts',(6.45320553925439,-30.8277805917852,
126.446387076662));
#115746=CARTESIAN_POINT('Ctrl Pts',(6.45616736969528,-30.8633224172604,
126.425457913083));
#115747=CARTESIAN_POINT('Ctrl Pts',(6.46827432337109,-31.0042098561678,
126.335292007246));
#115748=CARTESIAN_POINT('Ctrl Pts',(6.47752956685181,-31.1023346033881,
126.255511168682));
#115749=CARTESIAN_POINT('Ctrl Pts',(6.4893893111207,-31.2203660844488,126.134937154781));
#115750=CARTESIAN_POINT('Ctrl Pts',(6.49234296369616,-31.2490271784583,
126.103316544031));
#115751=CARTESIAN_POINT('Ctrl Pts',(6.49635425942368,-31.2869047943292,
126.058157346815));
#115752=CARTESIAN_POINT('Ctrl Pts',(6.49745453764131,-31.2971815376834,
126.045533840314));
#115753=CARTESIAN_POINT('Ctrl Pts',(6.49922021503165,-31.3134840836536,
126.024898036044));
#115754=CARTESIAN_POINT('Ctrl Pts',(6.49989018589651,-31.3196252470397,
126.016978680825));
#115755=CARTESIAN_POINT('Ctrl Pts',(6.50128479102593,-31.3323125993615,
126.000309221005));
#115756=CARTESIAN_POINT('Ctrl Pts',(6.50200885903743,-31.3388449260318,
125.99154912826));
#115757=CARTESIAN_POINT('Ctrl Pts',(6.50373065270819,-31.3542429075739,
125.970470233193));
#115758=CARTESIAN_POINT('Ctrl Pts',(6.50472522313699,-31.3630274473054,
125.958093173536));
#115759=CARTESIAN_POINT('Ctrl Pts',(6.50819419780949,-31.3932607329634,
125.914238105718));
#115760=CARTESIAN_POINT('Ctrl Pts',(6.51063463981055,-31.4137989571279,
125.882144909165));
#115761=CARTESIAN_POINT('Ctrl Pts',(6.51671632950467,-31.4628378040119,
125.799397515676));
#115762=CARTESIAN_POINT('Ctrl Pts',(6.52030996584898,-31.4898226486207,
125.747903768538));
#115763=CARTESIAN_POINT('Ctrl Pts',(6.5306130663636,-31.5599071729842,125.595246586069));
#115764=CARTESIAN_POINT('Ctrl Pts',(6.53720786217767,-31.5957554721044,
125.491109977333));
#115765=CARTESIAN_POINT('Ctrl Pts',(6.54606922763657,-31.6279484766227,
125.355280140688));
#115766=CARTESIAN_POINT('Ctrl Pts',(6.54798403109222,-31.6340298106704,
125.326169501329));
#115767=CARTESIAN_POINT('Ctrl Pts',(6.5505925204446,-31.6411032107873,125.28711566778));
#115768=CARTESIAN_POINT('Ctrl Pts',(6.55125131463722,-31.6427899269998,
125.277301999324));
#115769=CARTESIAN_POINT('Ctrl Pts',(6.55229767160672,-31.6453105760916,
125.261805446907));
#115770=CARTESIAN_POINT('Ctrl Pts',(6.5526820208343,-31.6462032962194,125.256132170632));
#115771=CARTESIAN_POINT('Ctrl Pts',(6.55348542643119,-31.6480001160509,
125.244315724879));
#115772=CARTESIAN_POINT('Ctrl Pts',(6.55390477425739,-31.648899225091,125.238171989441));
#115773=CARTESIAN_POINT('Ctrl Pts',(6.55494710838994,-31.6510390707485,
125.222956981187));
#115774=CARTESIAN_POINT('Ctrl Pts',(6.55557226829297,-31.6522393985809,
125.213880314075));
#115775=CARTESIAN_POINT('Ctrl Pts',(6.5579614695847,-31.6565153810407,125.179359075986));
#115776=CARTESIAN_POINT('Ctrl Pts',(6.55975025928964,-31.6590783718404,
125.153855997126));
#115777=CARTESIAN_POINT('Ctrl Pts',(6.56455193761555,-31.664315894548,125.086050778279));
#115778=CARTESIAN_POINT('Ctrl Pts',(6.56759863363915,-31.665966066748,125.043689216899));
#115779=CARTESIAN_POINT('Ctrl Pts',(6.58047350559178,-31.6661062488206,
124.865917736589));
#115780=CARTESIAN_POINT('Ctrl Pts',(6.59040798074068,-31.6497063668685,
124.730986984933));
#115781=CARTESIAN_POINT('Ctrl Pts',(6.60225665207569,-31.6088689371866,
124.56608364022));
#115782=CARTESIAN_POINT('Ctrl Pts',(6.60462858419402,-31.5995526368281,
124.532908651128));
#115783=CARTESIAN_POINT('Ctrl Pts',(6.60788787289367,-31.5851467686922,
124.487116597681));
#115784=CARTESIAN_POINT('Ctrl Pts',(6.60880284621934,-31.5809221451636,
124.474238787605));
#115785=CARTESIAN_POINT('Ctrl Pts',(6.61038399442401,-31.5733079049395,
124.451950515089));
#115786=CARTESIAN_POINT('Ctrl Pts',(6.61105248224384,-31.5699898703658,
124.44251653286));
#115787=CARTESIAN_POINT('Ctrl Pts',(6.61244674602053,-31.5628627273512,
124.422820744788));
#115788=CARTESIAN_POINT('Ctrl Pts',(6.61317193274186,-31.5590370175724,
124.41256542088));
#115789=CARTESIAN_POINT('Ctrl Pts',(6.61490146548797,-31.5496293665892,
124.388086385591));
#115790=CARTESIAN_POINT('Ctrl Pts',(6.61590258005776,-31.5439522131185,
124.373900140193));
#115791=CARTESIAN_POINT('Ctrl Pts',(6.61942355040095,-31.5231720155337,
124.32397621279));
#115792=CARTESIAN_POINT('Ctrl Pts',(6.62190801953996,-31.5070161152784,
124.288688574357));
#115793=CARTESIAN_POINT('Ctrl Pts',(6.62813293145819,-31.4629013726425,
124.200599140311));
#115794=CARTESIAN_POINT('Ctrl Pts',(6.63182259687753,-31.4333080699181,
124.148676960642));
#115795=CARTESIAN_POINT('Ctrl Pts',(6.64237913559423,-31.3401040996549,
124.003839500944));
#115796=CARTESIAN_POINT('Ctrl Pts',(6.64913194514274,-31.2697983494857,
123.915646887389));
#115797=CARTESIAN_POINT('Ctrl Pts',(6.65794791548176,-31.1732156821294,
123.816877362549));
#115798=CARTESIAN_POINT('Ctrl Pts',(6.65960692389917,-31.1548584334054,
123.798952107329));
#115799=CARTESIAN_POINT('Ctrl Pts',(6.66191575738511,-31.1292029041182,
123.775032402144));
#115800=CARTESIAN_POINT('Ctrl Pts',(6.66254001999159,-31.1222557180147,
123.768664583661));
#115801=CARTESIAN_POINT('Ctrl Pts',(6.66354492540437,-31.1110640106714,
123.758579606982));
#115802=CARTESIAN_POINT('Ctrl Pts',(6.66392278602291,-31.1068538585194,
123.754824365202));
#115803=CARTESIAN_POINT('Ctrl Pts',(6.66472686477968,-31.0978930675363,
123.746913150258));
#115804=CARTESIAN_POINT('Ctrl Pts',(6.66515349106686,-31.0931377583651,
123.742762680333));
#115805=CARTESIAN_POINT('Ctrl Pts',(6.66623812964722,-31.0810429026558,
123.732326690308));
#115806=CARTESIAN_POINT('Ctrl Pts',(6.66689869691037,-31.0736721395653,
123.726077905448));
#115807=CARTESIAN_POINT('Ctrl Pts',(6.66961085642554,-31.0433737036929,
123.700841221238));
#115808=CARTESIAN_POINT('Ctrl Pts',(6.67169619280759,-31.0199948213183,
123.68240654186));
#115809=CARTESIAN_POINT('Ctrl Pts',(6.67759242938557,-30.9533535359595,
123.632695379766));
#115810=CARTESIAN_POINT('Ctrl Pts',(6.68145604984246,-30.9090640498384,
123.60285764462));
#115811=CARTESIAN_POINT('Ctrl Pts',(6.69505368842306,-30.7491287746903,
123.505937712207));
#115812=CARTESIAN_POINT('Ctrl Pts',(6.70477986328375,-30.6268932145498,
123.450666696313));
#115813=CARTESIAN_POINT('Ctrl Pts',(6.71558872697801,-30.4774265375474,
123.403708044208));
#115814=CARTESIAN_POINT('Ctrl Pts',(6.71715990626993,-30.4553614562229,
123.397274152549));
#115815=CARTESIAN_POINT('Ctrl Pts',(6.71964746889766,-30.4198950015234,
123.387724225972));
#115816=CARTESIAN_POINT('Ctrl Pts',(6.72057318091282,-30.4065766013591,
123.384314241345));
#115817=CARTESIAN_POINT('Ctrl Pts',(6.72221275884133,-30.3827788450401,
123.378534076148));
#115818=CARTESIAN_POINT('Ctrl Pts',(6.72292864974069,-30.372316045031,123.37609970801));
#115819=CARTESIAN_POINT('Ctrl Pts',(6.72442607246351,-30.3502838645565,
123.371197638648));
#115820=CARTESIAN_POINT('Ctrl Pts',(6.72520687573671,-30.3387102359802,
123.368751611096));
#115821=CARTESIAN_POINT('Ctrl Pts',(6.72727196947351,-30.3078815593857,
123.362578382068));
#115822=CARTESIAN_POINT('Ctrl Pts',(6.72854937096296,-30.2885847211309,
123.359067484357));
#115823=CARTESIAN_POINT('Ctrl Pts',(6.73583250017285,-30.177367094609,123.340855056472));
#115824=CARTESIAN_POINT('Ctrl Pts',(6.74159860185873,-30.0843999756339,
123.333536416551));
#115825=CARTESIAN_POINT('Ctrl Pts',(6.75291404096309,-29.899610665351,123.334501647568));
#115826=CARTESIAN_POINT('Ctrl Pts',(6.75844863262275,-29.8081255883498,
123.342548676133));
#115827=CARTESIAN_POINT('Ctrl Pts',(6.76669327797358,-29.6787340016579,
123.3647895315));
#115828=CARTESIAN_POINT('Ctrl Pts',(6.76922090942779,-29.6399495437974,
123.372889606036));
#115829=CARTESIAN_POINT('Ctrl Pts',(6.77253559312887,-29.5908493472666,
123.384985470093));
#115830=CARTESIAN_POINT('Ctrl Pts',(6.77325937274455,-29.5802310440417,
123.387712743889));
#115831=CARTESIAN_POINT('Ctrl Pts',(6.77442776287269,-29.5632705911494,
123.39224787228));
#115832=CARTESIAN_POINT('Ctrl Pts',(6.7748686775115,-29.5569107077642,123.393988992545));
#115833=CARTESIAN_POINT('Ctrl Pts',(6.77572748713438,-29.54460539846,123.397436423727));
#115834=CARTESIAN_POINT('Ctrl Pts',(6.77614512583801,-29.5386588863692,
123.399138159927));
#115835=CARTESIAN_POINT('Ctrl Pts',(6.77717705264136,-29.5240548550127,
123.403405575777));
#115836=CARTESIAN_POINT('Ctrl Pts',(6.77779342092862,-29.5154085291638,
123.406008584202));
#115837=CARTESIAN_POINT('Ctrl Pts',(6.78010853803244,-29.4832013957348,
123.415990918984));
#115838=CARTESIAN_POINT('Ctrl Pts',(6.78183017395441,-29.4597856269238,
123.423823030178));
#115839=CARTESIAN_POINT('Ctrl Pts',(6.78639924812052,-29.3988196238663,
123.445732987378));
#115840=CARTESIAN_POINT('Ctrl Pts',(6.78927695477294,-29.3615892951226,
123.460651059185));
#115841=CARTESIAN_POINT('Ctrl Pts',(6.80068390173899,-29.2174159488322,
123.524551022688));
#115842=CARTESIAN_POINT('Ctrl Pts',(6.80932329822938,-29.1152304523408,
123.583463511025));
#115843=CARTESIAN_POINT('Ctrl Pts',(6.82123600089791,-28.9790678616202,
123.682491876728));
#115844=CARTESIAN_POINT('Ctrl Pts',(6.82476601493298,-28.9394176715411,
123.714194360977));
#115845=CARTESIAN_POINT('Ctrl Pts',(6.8294003253749,-28.888317161365,123.759026870483));
#115846=CARTESIAN_POINT('Ctrl Pts',(6.83056696496207,-28.8755383640317,
123.770594001194));
#115847=CARTESIAN_POINT('Ctrl Pts',(6.83248654397586,-28.8546619422436,
123.790088827657));
#115848=CARTESIAN_POINT('Ctrl Pts',(6.83324415767988,-28.8464618409549,
123.797904314091));
#115849=CARTESIAN_POINT('Ctrl Pts',(6.83472718553359,-28.8304914096011,
123.8134395907));
#115850=CARTESIAN_POINT('Ctrl Pts',(6.83545279700059,-28.8227162478945,
123.821153561868));
#115851=CARTESIAN_POINT('Ctrl Pts',(6.83619066777848,-28.8148515459285,
123.829111791164));
#115852=CARTESIAN_POINT('Ctrl Pts',(6.83620624170887,-28.8146855680861,
123.829279814269));
#115853=CARTESIAN_POINT('Ctrl Pts',(6.83623583013961,-28.8143702683017,
123.829599135125));
#115854=CARTESIAN_POINT('Ctrl Pts',(6.83624984493426,-28.8142209395846,
123.829750426162));
#115855=CARTESIAN_POINT('Ctrl Pts',(6.83627655291757,-28.8139363935831,
123.830038821749));
#115856=CARTESIAN_POINT('Ctrl Pts',(6.83628924632489,-28.8138011711808,
123.830175921094));
#115857=CARTESIAN_POINT('Ctrl Pts',(6.83631350256281,-28.8135427947668,
123.83043797474));
#115858=CARTESIAN_POINT('Ctrl Pts',(6.83632506558081,-28.8134196365894,
123.830562925186));
#115859=CARTESIAN_POINT('Ctrl Pts',(6.83634721640795,-28.8131837275465,
123.830802342948));
#115860=CARTESIAN_POINT('Ctrl Pts',(6.83635780434501,-28.8130709736074,
123.830916807014));
#115861=CARTESIAN_POINT('Ctrl Pts',(6.83637813275086,-28.8128545077565,
123.831136619574));
#115862=CARTESIAN_POINT('Ctrl Pts',(6.83638787332317,-28.812750793376,123.831241965493));
#115863=CARTESIAN_POINT('Ctrl Pts',(6.83643223615479,-28.8122784670355,
123.831721849778));
#115864=CARTESIAN_POINT('Ctrl Pts',(6.83646685136234,-28.8119100179505,
123.832096549064));
#115865=CARTESIAN_POINT('Ctrl Pts',(6.83653604626115,-28.8111736889653,
123.832846077836));
#115866=CARTESIAN_POINT('Ctrl Pts',(6.83657062595841,-28.8108058088897,
123.833220907085));
#115867=CARTESIAN_POINT('Ctrl Pts',(6.83767795873292,-28.7990283896695,
123.845232155369));
#115868=CARTESIAN_POINT('Ctrl Pts',(6.83874329689679,-28.7877897099164,
123.857035509234));
#115869=CARTESIAN_POINT('Ctrl Pts',(6.84301520154557,-28.7431301836051,
123.905338743654));
#115870=CARTESIAN_POINT('Ctrl Pts',(6.84616095838745,-28.7111682803419,
123.943156345533));
#115871=CARTESIAN_POINT('Ctrl Pts',(6.85485758441965,-28.6263125093629,
124.053144652801));
#115872=CARTESIAN_POINT('Ctrl Pts',(6.86028018796973,-28.5774782027905,
124.128228780105));
#115873=CARTESIAN_POINT('Ctrl Pts',(6.87077987473199,-28.4957493985147,
124.279201320023));
#115874=CARTESIAN_POINT('Ctrl Pts',(6.87583847403425,-28.4620086311546,
124.354322141641));
#115875=CARTESIAN_POINT('Ctrl Pts',(6.88222971323214,-28.4283560689041,
124.447043659558));
#115876=CARTESIAN_POINT('Ctrl Pts',(6.88330360939275,-28.4229853013396,
124.462552373413));
#115877=CARTESIAN_POINT('Ctrl Pts',(6.88490031704324,-28.4154303061508,
124.485457195498));
#115878=CARTESIAN_POINT('Ctrl Pts',(6.88541334322756,-28.4130667369984,
124.492793705419));
#115879=CARTESIAN_POINT('Ctrl Pts',(6.88633156415561,-28.408951467608,124.505877879494));
#115880=CARTESIAN_POINT('Ctrl Pts',(6.88673560149617,-28.4071798291052,
124.511618997854));
#115881=CARTESIAN_POINT('Ctrl Pts',(6.88763478572709,-28.4033237748579,
124.524359003226));
#115882=CARTESIAN_POINT('Ctrl Pts',(6.88813073693747,-28.4012543254014,
124.531361985501));
#115883=CARTESIAN_POINT('Ctrl Pts',(6.88960635955107,-28.3952640490912,
124.552134505304));
#115884=CARTESIAN_POINT('Ctrl Pts',(6.89059296867327,-28.3914747200839,
124.565940829975));
#115885=CARTESIAN_POINT('Ctrl Pts',(6.89290428349614,-28.3830838604319,
124.598132652908));
#115886=CARTESIAN_POINT('Ctrl Pts',(6.89423485063796,-28.3786172580569,
124.616551038582));
#115887=CARTESIAN_POINT('Ctrl Pts',(6.90423166997339,-28.3476777675406,
124.754355990659));
#115888=CARTESIAN_POINT('Ctrl Pts',(6.91327216383534,-28.3341084014325,
124.876251723394));
#115889=CARTESIAN_POINT('Ctrl Pts',(6.92206989104865,-28.3340006468508,
124.99853190384));
#115890=CARTESIAN_POINT('Ctrl Pts',(6.92206979048547,-28.3340006480831,
124.998530506106));
#115891=CARTESIAN_POINT('Ctrl Pts',(6.92753177905078,-28.3339336859568,
125.074447023654));
#115892=CARTESIAN_POINT('Ctrl Pts',(6.93289216561482,-28.3390557540501,
125.150289817465));
#115893=CARTESIAN_POINT('Ctrl Pts',(6.93911162664111,-28.3513445759967,
125.240232116867));
#115894=CARTESIAN_POINT('Ctrl Pts',(6.94012218279109,-28.353549658344,125.254906795077));
#115895=CARTESIAN_POINT('Ctrl Pts',(6.94186359326972,-28.3577121892431,
125.280295014377));
#115896=CARTESIAN_POINT('Ctrl Pts',(6.94259723577587,-28.3595791353605,
125.291022241554));
#115897=CARTESIAN_POINT('Ctrl Pts',(6.94406284090429,-28.3635365850972,
125.312511870141));
#115898=CARTESIAN_POINT('Ctrl Pts',(6.94479472140027,-28.3656284244834,
125.323273476083));
#115899=CARTESIAN_POINT('Ctrl Pts',(6.94618651850421,-28.3698274805669,
125.343792349891));
#115900=CARTESIAN_POINT('Ctrl Pts',(6.94684698110349,-28.3719164533771,
125.353552818573));
#115901=CARTESIAN_POINT('Ctrl Pts',(6.9485622490246,-28.377592885062,125.378957441186));
#115902=CARTESIAN_POINT('Ctrl Pts',(6.94961259269553,-28.381318968508,125.394569812067));
#115903=CARTESIAN_POINT('Ctrl Pts',(6.95332698054743,-28.3953833556236,
125.449943441757));
#115904=CARTESIAN_POINT('Ctrl Pts',(6.95595133756798,-28.4069663656086,
125.4893750524));
#115905=CARTESIAN_POINT('Ctrl Pts',(6.95959035233196,-28.4252824963323,
125.544149468564));
#115906=CARTESIAN_POINT('Ctrl Pts',(6.96063434584027,-28.4308044849064,
125.5598741184));
#115907=CARTESIAN_POINT('Ctrl Pts',(6.96167308954662,-28.4365599688247,
125.575509573264));
#115908=CARTESIAN_POINT('Ctrl Pts',(6.7689357756443,-28.4365600093868,125.575509683456));
#115909=CARTESIAN_POINT('Ctrl Pts',(6.76566848506476,-28.420778095137,125.532636250435));
#115910=CARTESIAN_POINT('Ctrl Pts',(6.76235350240954,-28.4067621010019,
125.489120073969));
#115911=CARTESIAN_POINT('Ctrl Pts',(6.75469878842849,-28.378651974293,125.38772188101));
#115912=CARTESIAN_POINT('Ctrl Pts',(6.75035980893607,-28.3658371653365,
125.329560227213));
#115913=CARTESIAN_POINT('Ctrl Pts',(6.74216812851736,-28.3473522964619,
125.217366497062));
#115914=CARTESIAN_POINT('Ctrl Pts',(6.73831113630137,-28.341156118264,125.163494805165));
#115915=CARTESIAN_POINT('Ctrl Pts',(6.73198983938758,-28.3352104610111,
125.073156967422));
#115916=CARTESIAN_POINT('Ctrl Pts',(6.729486824718,-28.3340108073496,125.036830930799));
#115917=CARTESIAN_POINT('Ctrl Pts',(6.72610900406875,-28.3339961064373,
124.9870664239));
#115918=CARTESIAN_POINT('Ctrl Pts',(6.72520278314316,-28.3341544305092,
124.973640804401));
#115919=CARTESIAN_POINT('Ctrl Pts',(6.72363259450369,-28.3347130475935,
124.950253447738));
#115920=CARTESIAN_POINT('Ctrl Pts',(6.72296639062987,-28.3350404882023,
124.940290831137));
#115921=CARTESIAN_POINT('Ctrl Pts',(6.72157292296929,-28.3359160260347,
124.919372174836));
#115922=CARTESIAN_POINT('Ctrl Pts',(6.7208462812632,-28.3364829577567,124.908417367689));
#115923=CARTESIAN_POINT('Ctrl Pts',(6.71910585380683,-28.3381073583385,
124.882072999952));
#115924=CARTESIAN_POINT('Ctrl Pts',(6.71809541042726,-28.3392704585849,
124.866690786944));
#115925=CARTESIAN_POINT('Ctrl Pts',(6.71449765318875,-28.3442028793999,
124.811639768621));
#115926=CARTESIAN_POINT('Ctrl Pts',(6.71194789671585,-28.34918152188,124.77209118515));
#115927=CARTESIAN_POINT('Ctrl Pts',(6.70550674341121,-28.3655498553303,
124.671372101888));
#115928=CARTESIAN_POINT('Ctrl Pts',(6.70167115359441,-28.3789555107175,
124.610591255652));
#115929=CARTESIAN_POINT('Ctrl Pts',(6.69223211632216,-28.4205291939749,
124.46214848252));
#115930=CARTESIAN_POINT('Ctrl Pts',(6.68668135806102,-28.4526164707771,
124.375809040903));
#115931=CARTESIAN_POINT('Ctrl Pts',(6.67844004874595,-28.5083229885934,
124.257035943605));
#115932=CARTESIAN_POINT('Ctrl Pts',(6.67593524040467,-28.526234795142,124.222110883728));
#115933=CARTESIAN_POINT('Ctrl Pts',(6.67264687822897,-28.5506879960217,
124.17831263442));
#115934=CARTESIAN_POINT('Ctrl Pts',(6.67192539151807,-28.5561085634468,
124.168824377533));
#115935=CARTESIAN_POINT('Ctrl Pts',(6.67075991272595,-28.5649444428561,
124.153705187675));
#115936=CARTESIAN_POINT('Ctrl Pts',(6.6703195858635,-28.5683005963175,124.148039804224));
#115937=CARTESIAN_POINT('Ctrl Pts',(6.66946123327384,-28.5748751627257,
124.137090109082));
#115938=CARTESIAN_POINT('Ctrl Pts',(6.66904345692316,-28.5780895614228,
124.131803604381));
#115939=CARTESIAN_POINT('Ctrl Pts',(6.66801020449228,-28.586076454115,124.118831427133));
#115940=CARTESIAN_POINT('Ctrl Pts',(6.6673926346831,-28.5908822091461,124.111166556878));
#115941=CARTESIAN_POINT('Ctrl Pts',(6.66506668193613,-28.6091098437405,
124.082614032058));
#115942=CARTESIAN_POINT('Ctrl Pts',(6.66333513962677,-28.6229349829396,
124.061989221668));
#115943=CARTESIAN_POINT('Ctrl Pts',(6.65873182740592,-28.6604729417816,
124.008607990808));
#115944=CARTESIAN_POINT('Ctrl Pts',(6.65582927364801,-28.6849259992527,
123.976393230019));
#115945=CARTESIAN_POINT('Ctrl Pts',(6.64422750792679,-28.7864659750026,
123.85227386869));
#115946=CARTESIAN_POINT('Ctrl Pts',(6.63541794614295,-28.8722199805286,
123.767904940636));
#115947=CARTESIAN_POINT('Ctrl Pts',(6.62352598431755,-29.0042637056442,
123.663433766239));
#115948=CARTESIAN_POINT('Ctrl Pts',(6.62016185090898,-29.0435269750317,
123.635060356369));
#115949=CARTESIAN_POINT('Ctrl Pts',(6.61570424466294,-29.0981664409287,
123.599092818538));
#115950=CARTESIAN_POINT('Ctrl Pts',(6.61455448351329,-29.1125012202855,
123.589967854092));
#115951=CARTESIAN_POINT('Ctrl Pts',(6.61273094015243,-29.1356170530476,
123.575745418554));
#115952=CARTESIAN_POINT('Ctrl Pts',(6.61205199631276,-29.1443091173042,
123.570506343875));
#115953=CARTESIAN_POINT('Ctrl Pts',(6.61065440296462,-29.1623761000877,
123.559840451813));
#115954=CARTESIAN_POINT('Ctrl Pts',(6.60993618910334,-29.1717571804574,
123.554424971422));
#115955=CARTESIAN_POINT('Ctrl Pts',(6.60825606070921,-29.1939251968672,
123.54191453245));
#115956=CARTESIAN_POINT('Ctrl Pts',(6.60729689706585,-29.2067541799568,
123.534895597441));
#115957=CARTESIAN_POINT('Ctrl Pts',(6.60409583263791,-29.2501321935008,
123.51189964288));
#115958=CARTESIAN_POINT('Ctrl Pts',(6.60188106785313,-29.2810854776876,
123.496701435788));
#115959=CARTESIAN_POINT('Ctrl Pts',(6.59650605610566,-29.3582430179661,
123.461745473911));
#115960=CARTESIAN_POINT('Ctrl Pts',(6.59337959913883,-29.4049122626889,
123.443095972488));
#115961=CARTESIAN_POINT('Ctrl Pts',(6.58628634375605,-29.5136340053649,
123.405254234714));
#115962=CARTESIAN_POINT('Ctrl Pts',(6.58234749730337,-29.5761059118787,
123.387523694431));
#115963=CARTESIAN_POINT('Ctrl Pts',(6.57368799047526,-29.7141547719017,
123.35692268656));
#115964=CARTESIAN_POINT('Ctrl Pts',(6.56896412098794,-29.7899001867891,
123.345531539426));
#115965=CARTESIAN_POINT('Ctrl Pts',(6.56296075072051,-29.8822425262484,
123.33808850214));
#115966=CARTESIAN_POINT('Ctrl Pts',(6.56190438691834,-29.8983522551874,
123.337025454719));
#115967=CARTESIAN_POINT('Ctrl Pts',(6.56032191091518,-29.9222299153552,
123.335798051685));
#115968=CARTESIAN_POINT('Ctrl Pts',(6.55980512214208,-29.9299881816379,
123.335453620304));
#115969=CARTESIAN_POINT('Ctrl Pts',(6.55888306643245,-29.9437541129448,
123.334938884169));
#115970=CARTESIAN_POINT('Ctrl Pts',(6.55847900066332,-29.9497607046222,
123.334746826969));
#115971=CARTESIAN_POINT('Ctrl Pts',(6.55758335627051,-29.9630164713693,
123.334394767318));
#115972=CARTESIAN_POINT('Ctrl Pts',(6.55709101203843,-29.9702656164729,
123.334249588323));
#115973=CARTESIAN_POINT('Ctrl Pts',(6.5556362788004,-29.9915811577864,123.333961882986));
#115974=CARTESIAN_POINT('Ctrl Pts',(6.55466723003914,-30.0056482792319,
123.333950196247));
#115975=CARTESIAN_POINT('Ctrl Pts',(6.54798406726279,-30.101878269984,123.335088936061));
#115976=CARTESIAN_POINT('Ctrl Pts',(6.54202674199773,-30.183850511154,123.342138653558));
#115977=CARTESIAN_POINT('Ctrl Pts',(6.52653932635934,-30.3939658285482,
123.375985950159));
#115978=CARTESIAN_POINT('Ctrl Pts',(6.51706480653485,-30.5201058514035,
123.411877491657));
#115979=CARTESIAN_POINT('Ctrl Pts',(6.50664773052694,-30.6599278677778,
123.470136603068));
#115980=CARTESIAN_POINT('Ctrl Pts',(6.50523209566115,-30.6789369387628,
123.478477241566));
#115981=CARTESIAN_POINT('Ctrl Pts',(6.50293236403428,-30.7098190625436,
123.492721492463));
#115982=CARTESIAN_POINT('Ctrl Pts',(6.50204124124716,-30.7217858200303,
123.498415221026));
#115983=CARTESIAN_POINT('Ctrl Pts',(6.50044185124528,-30.7432587058715,
123.508947943201));
#115984=CARTESIAN_POINT('Ctrl Pts',(6.4997318867413,-30.752788602039,123.513736540968));
#115985=CARTESIAN_POINT('Ctrl Pts',(6.49821248466088,-30.7731752236963,
123.524226836731));
#115986=CARTESIAN_POINT('Ctrl Pts',(6.49740411579749,-30.7840163596878,
123.5299575798));
#115987=CARTESIAN_POINT('Ctrl Pts',(6.49517823416996,-30.813843142863,123.546148166046));
#115988=CARTESIAN_POINT('Ctrl Pts',(6.49376968994446,-30.8326898564463,
123.556859851032));
#115989=CARTESIAN_POINT('Ctrl Pts',(6.49064055108185,-30.8744377913088,
123.581677868949));
#115990=CARTESIAN_POINT('Ctrl Pts',(6.48892690102477,-30.8972174735286,
123.59597719349));
#115991=CARTESIAN_POINT('Ctrl Pts',(6.4833420696504,-30.9709730480013,123.644803720927));
#115992=CARTESIAN_POINT('Ctrl Pts',(6.47954362482003,-31.0203838273396,
123.68160579439));
#115993=CARTESIAN_POINT('Ctrl Pts',(6.47023692267696,-31.1370369912806,
123.778986745744));
#115994=CARTESIAN_POINT('Ctrl Pts',(6.46478012548521,-31.2015936094042,
123.84246063489));
#115995=CARTESIAN_POINT('Ctrl Pts',(6.45651942298891,-31.2877405891338,
123.942175069479));
#115996=CARTESIAN_POINT('Ctrl Pts',(6.45388232485946,-31.3136223248683,
123.974492723018));
#115997=CARTESIAN_POINT('Ctrl Pts',(6.45044103592729,-31.344904517884,124.016683233437));
#115998=CARTESIAN_POINT('Ctrl Pts',(6.44970604635026,-31.3514473891593,
124.025695138365));
#115999=CARTESIAN_POINT('Ctrl Pts',(6.44852393290883,-31.3617407716749,
124.040176039178));
#116000=CARTESIAN_POINT('Ctrl Pts',(6.44808066098892,-31.3655499588191,
124.045603189895));
#116001=CARTESIAN_POINT('Ctrl Pts',(6.44722104596509,-31.3728370379993,
124.056118412725));
#116002=CARTESIAN_POINT('Ctrl Pts',(6.44680499624314,-31.376319241199,124.061203256842));
#116003=CARTESIAN_POINT('Ctrl Pts',(6.44578248167053,-31.384770143057,124.073691653643));
#116004=CARTESIAN_POINT('Ctrl Pts',(6.44517401946421,-31.3897077297389,
124.081115938429));
#116005=CARTESIAN_POINT('Ctrl Pts',(6.44292288200507,-31.4076503349595,
124.108570322492));
#116006=CARTESIAN_POINT('Ctrl Pts',(6.44125886223176,-31.4202831634038,
124.128838747474));
#116007=CARTESIAN_POINT('Ctrl Pts',(6.43688510372683,-31.4519771114395,
124.182211909521));
#116008=CARTESIAN_POINT('Ctrl Pts',(6.43414792421252,-31.4703426829046,
124.21571247241));
#116009=CARTESIAN_POINT('Ctrl Pts',(6.42636814161454,-31.5188303104101,
124.31185809634));
#116010=CARTESIAN_POINT('Ctrl Pts',(6.4212844975024,-31.5462082224433,124.37580054661));
#116011=CARTESIAN_POINT('Ctrl Pts',(6.40925870486,-31.6018701258222,124.532157712738));
#116012=CARTESIAN_POINT('Ctrl Pts',(6.40239231032963,-31.6262750023347,
124.625701162495));
#116013=CARTESIAN_POINT('Ctrl Pts',(6.39442228899993,-31.6457805472773,
124.740464988821));
#116014=CARTESIAN_POINT('Ctrl Pts',(6.39307076223008,-31.6487633962984,
124.760143054257));
#116015=CARTESIAN_POINT('Ctrl Pts',(6.39092961805284,-31.6529637974901,
124.791654127011));
#116016=CARTESIAN_POINT('Ctrl Pts',(6.39013294220872,-31.6544083989397,
124.803454379842));
#116017=CARTESIAN_POINT('Ctrl Pts',(6.38862518575324,-31.656915636688,124.825926559411));
#116018=CARTESIAN_POINT('Ctrl Pts',(6.38791340311213,-31.6580017705635,
124.836595202634));
#116019=CARTESIAN_POINT('Ctrl Pts',(6.38628937938659,-31.6602548754232,
124.861069503379));
#116020=CARTESIAN_POINT('Ctrl Pts',(6.38537934069859,-31.6613528069016,
124.874880838876));
#116021=CARTESIAN_POINT('Ctrl Pts',(6.38252197418721,-31.6642754973892,
124.91853336968));
#116022=CARTESIAN_POINT('Ctrl Pts',(6.3805942197333,-31.6654694771846,124.948411823421));
#116023=CARTESIAN_POINT('Ctrl Pts',(6.37342763472322,-31.6669328141901,
125.060789075925));
#116024=CARTESIAN_POINT('Ctrl Pts',(6.3683461659369,-31.6618798136474,125.143240126127));
#116025=CARTESIAN_POINT('Ctrl Pts',(6.35705023005063,-31.6369343992204,
125.326267763607));
#116026=CARTESIAN_POINT('Ctrl Pts',(6.35088117107393,-31.6138393747341,
125.42605534833));
#116027=CARTESIAN_POINT('Ctrl Pts',(6.34271788078855,-31.5736725685779,
125.547514990068));
#116028=CARTESIAN_POINT('Ctrl Pts',(6.34105421172018,-31.5650297130898,
125.57175155696));
#116029=CARTESIAN_POINT('Ctrl Pts',(6.33873999859542,-31.5524564706115,
125.604585713514));
#116030=CARTESIAN_POINT('Ctrl Pts',(6.33811517573018,-31.5490085523667,
125.61336569229));
#116031=CARTESIAN_POINT('Ctrl Pts',(6.33710968377548,-31.5433795310543,
125.627349548043));
#116032=CARTESIAN_POINT('Ctrl Pts',(6.33673180434864,-31.5412461635949,
125.632572599087));
#116033=CARTESIAN_POINT('Ctrl Pts',(6.33592803487865,-31.5366718060309,
125.643611327701));
#116034=CARTESIAN_POINT('Ctrl Pts',(6.33550173973639,-31.5342242572817,
125.64942413331));
#116035=CARTESIAN_POINT('Ctrl Pts',(6.3344185612339,-31.5279498091341,125.664092194107));
#116036=CARTESIAN_POINT('Ctrl Pts',(6.33375913461186,-31.5240789420989,
125.672928249213));
#116037=CARTESIAN_POINT('Ctrl Pts',(6.33105697484544,-31.5080021169505,
125.708776596779));
#116038=CARTESIAN_POINT('Ctrl Pts',(6.32898079148647,-31.4951537457605,
125.735492805451));
#116039=CARTESIAN_POINT('Ctrl Pts',(6.32311980225455,-31.4573567763721,
125.808998103495));
#116040=CARTESIAN_POINT('Ctrl Pts',(6.319282930209,-31.4308775663393,125.854959309563));
#116041=CARTESIAN_POINT('Ctrl Pts',(6.305817962956,-31.3308762716336,126.010840622041));
#116042=CARTESIAN_POINT('Ctrl Pts',(6.29619306128808,-31.2464947843344,
126.113235510768));
#116043=CARTESIAN_POINT('Ctrl Pts',(6.28520854980733,-31.1315499810503,
126.223055818523));
#116044=CARTESIAN_POINT('Ctrl Pts',(6.28338036365473,-31.1117749281198,
126.241059042647));
#116045=CARTESIAN_POINT('Ctrl Pts',(6.28067435487289,-31.0815458536922,
126.26727691448));
#116046=CARTESIAN_POINT('Ctrl Pts',(6.2797816399537,-31.071413820254,126.275854480371));
#116047=CARTESIAN_POINT('Ctrl Pts',(6.27818053670851,-31.0529573126989,
126.291104439105));
#116048=CARTESIAN_POINT('Ctrl Pts',(6.27747043499808,-31.0446693175428,
126.297819633503));
#116049=CARTESIAN_POINT('Ctrl Pts',(6.27595196692837,-31.0267292877109,
126.312071994415));
#116050=CARTESIAN_POINT('Ctrl Pts',(6.27514465683307,-31.0170574464703,
126.319583310284));
#116051=CARTESIAN_POINT('Ctrl Pts',(6.27292496469938,-30.9901022018194,
126.340044777561));
#116052=CARTESIAN_POINT('Ctrl Pts',(6.2715214669039,-30.9726480943924,126.352766842425));
#116053=CARTESIAN_POINT('Ctrl Pts',(6.26342092083833,-30.8696349798483,
126.424826851887));
#116054=CARTESIAN_POINT('Ctrl Pts',(6.25702543657572,-30.778908785925,126.476381153419));
#116055=CARTESIAN_POINT('Ctrl Pts',(6.24397338457015,-30.5840757522166,
126.564100105994));
#116056=CARTESIAN_POINT('Ctrl Pts',(6.23734732374487,-30.4800207197973,
126.59910194209));
#116057=CARTESIAN_POINT('Ctrl Pts',(6.22925225068398,-30.3585575131978,
126.627028396531));
#116058=CARTESIAN_POINT('Ctrl Pts',(6.22826047036556,-30.3437681206091,
126.630217265675));
#116059=CARTESIAN_POINT('Ctrl Pts',(6.22676348905146,-30.3216229043059,
126.634677457065));
#116060=CARTESIAN_POINT('Ctrl Pts',(6.22626641215246,-30.314298171416,126.636101566321));
#116061=CARTESIAN_POINT('Ctrl Pts',(6.22536452278877,-30.3010657002205,
126.638582149385));
#116062=CARTESIAN_POINT('Ctrl Pts',(6.22496068611918,-30.2951614856038,
126.639655973216));
#116063=CARTESIAN_POINT('Ctrl Pts',(6.22404633030813,-30.2818405099807,
126.642004432791));
#116064=CARTESIAN_POINT('Ctrl Pts',(6.22353483591524,-30.2744208960654,
126.643260720841));
#116065=CARTESIAN_POINT('Ctrl Pts',(6.2219648526068,-30.2517373153726,126.646943593896));
#116066=CARTESIAN_POINT('Ctrl Pts',(6.22089809026885,-30.2364483615836,
126.649207993917));
#116067=CARTESIAN_POINT('Ctrl Pts',(6.21544461656102,-30.158805719062,126.659605622754));
#116068=CARTESIAN_POINT('Ctrl Pts',(6.21092192441388,-30.0960638788738,
126.664415893714));
#116069=CARTESIAN_POINT('Ctrl Pts',(6.20137953052586,-29.9645776445958,
126.667037234323));
#116070=CARTESIAN_POINT('Ctrl Pts',(6.19636205424312,-29.8959270886012,
126.664162592765));
#116071=CARTESIAN_POINT('Ctrl Pts',(6.18526919213416,-29.7430576156658,
126.648262647192));
#116072=CARTESIAN_POINT('Ctrl Pts',(6.17924716673526,-29.6592535197048,
126.632998773393));
#116073=CARTESIAN_POINT('Ctrl Pts',(6.1720785295216,-29.5579450683226,126.606402919354));
#116074=CARTESIAN_POINT('Ctrl Pts',(6.17074302629156,-29.5390091900488,
126.601071651302));
#116075=CARTESIAN_POINT('Ctrl Pts',(6.1686210905763,-29.5088343485104,126.591996375173));
#116076=CARTESIAN_POINT('Ctrl Pts',(6.16782782025468,-29.4975336760191,
126.588465851555));
#116077=CARTESIAN_POINT('Ctrl Pts',(6.1663227564773,-29.4760595092905,126.581504853401));
#116078=CARTESIAN_POINT('Ctrl Pts',(6.16561030062586,-29.4658797137806,
126.578095931237));
#116079=CARTESIAN_POINT('Ctrl Pts',(6.16397949045133,-29.442550089541,126.570031898233));
#116080=CARTESIAN_POINT('Ctrl Pts',(6.16306340534582,-29.4294242362088,
126.565309516204));
#116081=CARTESIAN_POINT('Ctrl Pts',(6.16016537561502,-29.3878542613355,
126.549761200043));
#116082=CARTESIAN_POINT('Ctrl Pts',(6.15820383055342,-29.3596458006872,
126.53832014464));
#116083=CARTESIAN_POINT('Ctrl Pts',(6.1535755828014,-29.2931196045941,126.509190486473));
#116084=CARTESIAN_POINT('Ctrl Pts',(6.15093103753098,-29.255129008656,126.490806291018));
#116085=CARTESIAN_POINT('Ctrl Pts',(6.14362504959845,-29.1511081797027,
126.435498780649));
#116086=CARTESIAN_POINT('Ctrl Pts',(6.13903760215144,-29.086835209857,126.395494359554));
#116087=CARTESIAN_POINT('Ctrl Pts',(6.13372869077102,-29.0164700688166,
126.344748618992));
#116088=CARTESIAN_POINT('Ctrl Pts',(6.1330465013984,-29.007504775263,126.338145432928));
#116089=CARTESIAN_POINT('Ctrl Pts',(6.12776556764452,-28.9387599463996,
126.286442041436));
#116090=CARTESIAN_POINT('Ctrl Pts',(6.12311457543217,-28.8820236671828,
126.237452880374));
#116091=CARTESIAN_POINT('Ctrl Pts',(6.11742211172923,-28.8200469106952,
126.176187721045));
#116092=CARTESIAN_POINT('Ctrl Pts',(6.11661353930724,-28.8114082721725,
126.167457292948));
#116093=CARTESIAN_POINT('Ctrl Pts',(6.1153361518231,-28.7980335833544,126.153638175816));
#116094=CARTESIAN_POINT('Ctrl Pts',(6.11487221761166,-28.7932313154153,
126.148613792785));
#116095=CARTESIAN_POINT('Ctrl Pts',(6.11399968056643,-28.7843059688965,
126.139157873265));
#116096=CARTESIAN_POINT('Ctrl Pts',(6.11359165305245,-28.7801754214001,
126.134733726586));
#116097=CARTESIAN_POINT('Ctrl Pts',(6.11262565089614,-28.7704967715143,
126.124253206343));
#116098=CARTESIAN_POINT('Ctrl Pts',(6.11206619305883,-28.7649692482964,
126.118178204093));
#116099=CARTESIAN_POINT('Ctrl Pts',(6.11027255066844,-28.7474875722705,
126.0986772845));
#116100=CARTESIAN_POINT('Ctrl Pts',(6.10902700859033,-28.7357061518161,
126.085099146581));
#116101=CARTESIAN_POINT('Ctrl Pts',(6.1025554996016,-28.6762057392147,126.014240032712));
#116102=CARTESIAN_POINT('Ctrl Pts',(6.09715138893323,-28.632154729726,125.953997603251));
#116103=CARTESIAN_POINT('Ctrl Pts',(6.08526294993754,-28.5447743063688,
125.815945593676));
#116104=CARTESIAN_POINT('Ctrl Pts',(6.07879307504246,-28.5033359053839,
125.737189425107));
#116105=CARTESIAN_POINT('Ctrl Pts',(6.07046004283884,-28.4570812673408,
125.629111752382));
#116106=CARTESIAN_POINT('Ctrl Pts',(6.06844399518573,-28.4464731093221,
125.602439792326));
#116107=CARTESIAN_POINT('Ctrl Pts',(6.06644913825629,-28.4365599905855,
125.57550963238));
#116108=CARTESIAN_POINT('Origin',(5.,-30.,125.));
#116109=CARTESIAN_POINT('',(5.3678724416903,-28.4365599837785,125.575509613888));
#116110=CARTESIAN_POINT('',(5.55934601859666,-28.436559980232,125.575509604253));
#116111=CARTESIAN_POINT('',(5.,-28.4365599837785,125.575509613888));
#116112=CARTESIAN_POINT('Ctrl Pts',(5.55934601859666,-28.436559980232,125.575509604253));
#116113=CARTESIAN_POINT('Ctrl Pts',(5.56387671087001,-28.4589277274792,
125.636274239526));
#116114=CARTESIAN_POINT('Ctrl Pts',(5.56855161395396,-28.4848198285364,
125.695685446484));
#116115=CARTESIAN_POINT('Ctrl Pts',(5.5740981650682,-28.5193379989006,125.763760391978));
#116116=CARTESIAN_POINT('Ctrl Pts',(5.5749399462272,-28.5246784771278,125.774026033106));
#116117=CARTESIAN_POINT('Ctrl Pts',(5.58242649944295,-28.5731019919598,
125.864785151984));
#116118=CARTESIAN_POINT('Ctrl Pts',(5.58906862584462,-28.6226313221648,
125.941673974154));
#116119=CARTESIAN_POINT('Ctrl Pts',(5.59905977370649,-28.7086796213221,
126.053827427168));
#116120=CARTESIAN_POINT('Ctrl Pts',(5.6025380965924,-28.7409192708118,126.092143388595));
#116121=CARTESIAN_POINT('Ctrl Pts',(5.60706181648059,-28.7859235576508,
126.14098290456));
#116122=CARTESIAN_POINT('Ctrl Pts',(5.60816858031253,-28.79718560053,126.152849144488));
#116123=CARTESIAN_POINT('Ctrl Pts',(5.60930315698163,-28.8089881810292,
126.164923655471));
#116124=CARTESIAN_POINT('Ctrl Pts',(5.60933845108678,-28.8093555914467,
126.165299175485));
#116125=CARTESIAN_POINT('Ctrl Pts',(5.60940902617381,-28.8100907933492,
126.166049894289));
#116126=CARTESIAN_POINT('Ctrl Pts',(5.60944430715177,-28.810458584829,126.166425093025));
#116127=CARTESIAN_POINT('Ctrl Pts',(5.60948912068581,-28.8109260786037,
126.166901550967));
#116128=CARTESIAN_POINT('Ctrl Pts',(5.60949866045186,-28.811025616166,126.167002971196));
#116129=CARTESIAN_POINT('Ctrl Pts',(5.60951854566114,-28.811233137171,126.167214363172));
#116130=CARTESIAN_POINT('Ctrl Pts',(5.60952889101054,-28.8113411229734,
126.167324332746));
#116131=CARTESIAN_POINT('Ctrl Pts',(5.60955050534072,-28.8115667820757,
126.167554073577));
#116132=CARTESIAN_POINT('Ctrl Pts',(5.60956177419511,-28.8116844582179,
126.167673842026));
#116133=CARTESIAN_POINT('Ctrl Pts',(5.60958537820657,-28.8119310008479,
126.167924692368));
#116134=CARTESIAN_POINT('Ctrl Pts',(5.60959771320737,-28.8120598709518,
126.168055770752));
#116135=CARTESIAN_POINT('Ctrl Pts',(5.60962362388296,-28.8123306396708,
126.168331088123));
#116136=CARTESIAN_POINT('Ctrl Pts',(5.60963719934727,-28.8124725427914,
126.16847532251));
#116137=CARTESIAN_POINT('Ctrl Pts',(5.6096658065174,-28.8127716518829,126.168779234774));
#116138=CARTESIAN_POINT('Ctrl Pts',(5.60968083796983,-28.8129288638965,
126.16893890689));
#116139=CARTESIAN_POINT('Ctrl Pts',(5.60971262712999,-28.8132614421574,
126.169276553155));
#116140=CARTESIAN_POINT('Ctrl Pts',(5.6097293844874,-28.8134368161937,126.169454519536));
#116141=CARTESIAN_POINT('Ctrl Pts',(5.60976496866988,-28.8138093465418,
126.169832386489));
#116142=CARTESIAN_POINT('Ctrl Pts',(5.60978379502933,-28.8140065133557,
126.170032276678));
#116143=CARTESIAN_POINT('Ctrl Pts',(5.6098239608815,-28.8144273244565,126.17045868459));
#116144=CARTESIAN_POINT('Ctrl Pts',(5.60984529974307,-28.8146509832175,
126.170685188144));
#116145=CARTESIAN_POINT('Ctrl Pts',(5.60989107542949,-28.8151309751109,
126.171171006646));
#116146=CARTESIAN_POINT('Ctrl Pts',(5.60991551135984,-28.8153873285028,
126.171430301588));
#116147=CARTESIAN_POINT('Ctrl Pts',(5.60996826986791,-28.8159410784756,
126.171990037956));
#116148=CARTESIAN_POINT('Ctrl Pts',(5.60999659115661,-28.8162385044083,
126.172290450471));
#116149=CARTESIAN_POINT('Ctrl Pts',(5.61005821318731,-28.8168860140822,
126.172943964375));
#116150=CARTESIAN_POINT('Ctrl Pts',(5.61009151199381,-28.8172361416954,
126.173297022381));
#116151=CARTESIAN_POINT('Ctrl Pts',(5.61084441121101,-28.8251579027286,
126.181277935234));
#116152=CARTESIAN_POINT('Ctrl Pts',(5.61156074400305,-28.8328031636369,
126.188832649401));
#116153=CARTESIAN_POINT('Ctrl Pts',(5.61305714493872,-28.8489987124434,
126.204529541568));
#116154=CARTESIAN_POINT('Ctrl Pts',(5.61383650325648,-28.8575635475978,
126.212655905345));
#116155=CARTESIAN_POINT('Ctrl Pts',(5.61589324046518,-28.8805052743641,
126.233964335834));
#116156=CARTESIAN_POINT('Ctrl Pts',(5.61716383197746,-28.8950287745099,
126.246986393483));
#116157=CARTESIAN_POINT('Ctrl Pts',(5.62375586413986,-28.9721473883346,
126.313726892015));
#116158=CARTESIAN_POINT('Ctrl Pts',(5.62889417640534,-29.0384428790275,
126.363000267641));
#116159=CARTESIAN_POINT('Ctrl Pts',(5.64012856737408,-29.1929248389875,
126.460912683838));
#116160=CARTESIAN_POINT('Ctrl Pts',(5.64616505641996,-29.2824057093656,
126.506881637926));
#116161=CARTESIAN_POINT('Ctrl Pts',(5.65423287298559,-29.4017163655147,
126.555125064875));
#116162=CARTESIAN_POINT('Ctrl Pts',(5.65602732380753,-29.4282237334719,
126.565065172765));
#116163=CARTESIAN_POINT('Ctrl Pts',(5.65909730083182,-29.4732245688206,
126.580644431431));
#116164=CARTESIAN_POINT('Ctrl Pts',(5.66035646848474,-29.4915868580442,
126.586645887563));
#116165=CARTESIAN_POINT('Ctrl Pts',(5.66217592104807,-29.5179045951558,
126.594743736312));
#116166=CARTESIAN_POINT('Ctrl Pts',(5.66272213410759,-29.5257784073134,
126.597102826339));
#116167=CARTESIAN_POINT('Ctrl Pts',(5.66367653728221,-29.5394822716513,
126.601098400157));
#116168=CARTESIAN_POINT('Ctrl Pts',(5.66408319613472,-29.5453043114087,
126.602761521419));
#116169=CARTESIAN_POINT('Ctrl Pts',(5.66496073268302,-29.5578291318377,
126.606265618003));
#116170=CARTESIAN_POINT('Ctrl Pts',(5.6654321359787,-29.5645343039123,126.608096370046));
#116171=CARTESIAN_POINT('Ctrl Pts',(5.66674251172949,-29.583114826629,126.61304479057));
#116172=CARTESIAN_POINT('Ctrl Pts',(5.66758623139195,-29.595013208627,126.616073148363));
#116173=CARTESIAN_POINT('Ctrl Pts',(5.6734954828419,-29.67796922657,126.636213365583));
#116174=CARTESIAN_POINT('Ctrl Pts',(5.67876261169556,-29.7500451611886,
126.648762629497));
#116175=CARTESIAN_POINT('Ctrl Pts',(5.68510299049547,-29.836825261145,126.658050580784));
#116176=CARTESIAN_POINT('Ctrl Pts',(5.68613626212294,-29.8509662411422,
126.659381408442));
#116177=CARTESIAN_POINT('Ctrl Pts',(5.69253310073032,-29.9385672252456,
126.666496846603));
#116178=CARTESIAN_POINT('Ctrl Pts',(5.69789663062693,-30.0123315240616,
126.667583571493));
#116179=CARTESIAN_POINT('Ctrl Pts',(5.70619293750442,-30.1284269870043,
126.661587616317));
#116180=CARTESIAN_POINT('Ctrl Pts',(5.70919336109643,-30.170827989108,126.657765121979));
#116181=CARTESIAN_POINT('Ctrl Pts',(5.71427316607011,-30.2434150200868,
126.648406248613));
#116182=CARTESIAN_POINT('Ctrl Pts',(5.71637410222801,-30.2736787240765,
126.643652701305));
#116183=CARTESIAN_POINT('Ctrl Pts',(5.71939638259966,-30.3175465571194,
126.635516972178));
#116184=CARTESIAN_POINT('Ctrl Pts',(5.72033821661738,-30.3312648437227,
126.632793681469));
#116185=CARTESIAN_POINT('Ctrl Pts',(5.72199377552585,-30.3554571823847,
126.627673674398));
#116186=CARTESIAN_POINT('Ctrl Pts',(5.72270970956948,-30.3659452277947,
126.625347808435));
#116187=CARTESIAN_POINT('Ctrl Pts',(5.72420702992422,-30.3879308874943,
126.620248589306));
#116188=CARTESIAN_POINT('Ctrl Pts',(5.72498768954085,-30.3994229807926,
126.617453912535));
#116189=CARTESIAN_POINT('Ctrl Pts',(5.72705195250144,-30.429879945526,126.609702899502));
#116190=CARTESIAN_POINT('Ctrl Pts',(5.72832867699853,-30.4487891203636,
126.604533754795));
#116191=CARTESIAN_POINT('Ctrl Pts',(5.73491745995534,-30.5466439093596,
126.575918174931));
#116192=CARTESIAN_POINT('Ctrl Pts',(5.74004726074812,-30.6238670634926,
126.546974472556));
#116193=CARTESIAN_POINT('Ctrl Pts',(5.75127071968234,-30.7897471518108,
126.47034926399));
#116194=CARTESIAN_POINT('Ctrl Pts',(5.75730472599273,-30.8768584874213,
126.420121250978));
#116195=CARTESIAN_POINT('Ctrl Pts',(5.765369557475,-30.9820587448928,126.346074882379));
#116196=CARTESIAN_POINT('Ctrl Pts',(5.76716367680494,-31.0047819481238,
126.329199015752));
#116197=CARTESIAN_POINT('Ctrl Pts',(5.77023314394908,-31.0422710021246,
126.299846232284));
#116198=CARTESIAN_POINT('Ctrl Pts',(5.77149214028249,-31.057269986804,126.287675877856));
#116199=CARTESIAN_POINT('Ctrl Pts',(5.77331138812889,-31.0783446967249,
126.26995916137));
#116200=CARTESIAN_POINT('Ctrl Pts',(5.77385757210018,-31.0845967939543,
126.264623795458));
#116201=CARTESIAN_POINT('Ctrl Pts',(5.7748119424772,-31.095385740118,126.255277955183));
#116202=CARTESIAN_POINT('Ctrl Pts',(5.77521859794716,-31.0999406187617,
126.251288655058));
#116203=CARTESIAN_POINT('Ctrl Pts',(5.77609614865013,-31.1096777138217,
126.242666361985));
#116204=CARTESIAN_POINT('Ctrl Pts',(5.77656756969137,-31.1148526357052,
126.238025812338));
#116205=CARTESIAN_POINT('Ctrl Pts',(5.77787804170919,-31.1290884354201,
126.22509839484));
#116206=CARTESIAN_POINT('Ctrl Pts',(5.77872184097471,-31.1380867558584,
126.216743722423));
#116207=CARTESIAN_POINT('Ctrl Pts',(5.78465224986635,-31.2002211056147,
126.157761577216));
#116208=CARTESIAN_POINT('Ctrl Pts',(5.78994213002371,-31.2500478152111,
126.103775631436));
#116209=CARTESIAN_POINT('Ctrl Pts',(5.79628915138742,-31.3049340404179,
126.035808245437));
#116210=CARTESIAN_POINT('Ctrl Pts',(5.79730656214647,-31.3135827305999,
126.024818021595));
#116211=CARTESIAN_POINT('Ctrl Pts',(5.80368943377926,-31.3669443041776,
125.955223962102));
#116212=CARTESIAN_POINT('Ctrl Pts',(5.80905469631131,-31.4078677272737,
125.89381168292));
#116213=CARTESIAN_POINT('Ctrl Pts',(5.81734777316818,-31.465756668967,125.793044031523));
#116214=CARTESIAN_POINT('Ctrl Pts',(5.82034350862756,-31.485506661922,125.755401818718));
#116215=CARTESIAN_POINT('Ctrl Pts',(5.825416350126,-31.5169645549511,125.689427674944));
#116216=CARTESIAN_POINT('Ctrl Pts',(5.82751493078528,-31.5293695850263,
125.661453600573));
#116217=CARTESIAN_POINT('Ctrl Pts',(5.83053450396068,-31.5463105872289,
125.620221723893));
#116218=CARTESIAN_POINT('Ctrl Pts',(5.83147593444493,-31.5514604800356,
125.607224685383));
#116219=CARTESIAN_POINT('Ctrl Pts',(5.83313103835407,-31.5602772227666,
125.584128728075));
#116220=CARTESIAN_POINT('Ctrl Pts',(5.83384691682046,-31.5640110636554,
125.574056430066));
#116221=CARTESIAN_POINT('Ctrl Pts',(5.83534436914983,-31.5716515929452,
125.55281751416));
#116222=CARTESIAN_POINT('Ctrl Pts',(5.8361252139267,-31.5755372999715,125.541643944042));
#116223=CARTESIAN_POINT('Ctrl Pts',(5.8381905476821,-31.5855487314031,125.51183586277));
#116224=CARTESIAN_POINT('Ctrl Pts',(5.83946814475944,-31.5914650557284,
125.493132597964));
#116225=CARTESIAN_POINT('Ctrl Pts',(5.84608704699126,-31.620625500087,125.39495026224));
#116226=CARTESIAN_POINT('Ctrl Pts',(5.85124386845245,-31.6382520012093,
125.313919743571));
#116227=CARTESIAN_POINT('Ctrl Pts',(5.86246913978206,-31.6636950448597,
125.132917490952));
#116228=CARTESIAN_POINT('Ctrl Pts',(5.86848038039449,-31.6686714861518,
125.032884592881));
#116229=CARTESIAN_POINT('Ctrl Pts',(5.87651783294262,-31.6635169570918,
124.904787197624));
#116230=CARTESIAN_POINT('Ctrl Pts',(5.87830890381491,-31.6616632716858,
124.8765936146));
#116231=CARTESIAN_POINT('Ctrl Pts',(5.88137368146036,-31.6573392221696,
124.829252187381));
#116232=CARTESIAN_POINT('Ctrl Pts',(5.88263110168593,-31.6552511806857,
124.810074846506));
#116233=CARTESIAN_POINT('Ctrl Pts',(5.88444846607165,-31.6517998740989,
124.782788894));
#116234=CARTESIAN_POINT('Ctrl Pts',(5.88499438230133,-31.6507087391817,
124.774646632965));
#116235=CARTESIAN_POINT('Ctrl Pts',(5.88594845086659,-31.6487089190083,
124.760518145733));
#116236=CARTESIAN_POINT('Ctrl Pts',(5.88635507527444,-31.6478277469296,
124.754528263866));
#116237=CARTESIAN_POINT('Ctrl Pts',(5.88723275659524,-31.6458644240482,
124.741669502414));
#116238=CARTESIAN_POINT('Ctrl Pts',(5.88770434123275,-31.6447719336788,
124.734802658193));
#116239=CARTESIAN_POINT('Ctrl Pts',(5.88901570084698,-31.6416296636297,
124.715818584914));
#116240=CARTESIAN_POINT('Ctrl Pts',(5.88986023408982,-31.6394887905003,
124.703717174243));
#116241=CARTESIAN_POINT('Ctrl Pts',(5.89598295086757,-31.6231181001006,
124.616797935887));
#116242=CARTESIAN_POINT('Ctrl Pts',(5.90147988936187,-31.6039079215513,
124.543017509895));
#116243=CARTESIAN_POINT('Ctrl Pts',(5.90771780544969,-31.5766499887535,
124.46164660416));
#116244=CARTESIAN_POINT('Ctrl Pts',(5.90842150588969,-31.5734977018988,
124.45250155542));
#116245=CARTESIAN_POINT('Ctrl Pts',(5.91463667402113,-31.5449648643984,
124.372007670209));
#116246=CARTESIAN_POINT('Ctrl Pts',(5.92015091202742,-31.5148248629015,
124.3024343415));
#116247=CARTESIAN_POINT('Ctrl Pts',(5.92856624835229,-31.4606718669075,
124.197643409191));
#116248=CARTESIAN_POINT('Ctrl Pts',(5.9315420805563,-31.4398697219119,124.160884943123));
#116249=CARTESIAN_POINT('Ctrl Pts',(5.93658533760329,-31.4016978052337,
124.099041323859));
#116250=CARTESIAN_POINT('Ctrl Pts',(5.93867389843221,-31.3849954304947,
124.073570757555));
#116251=CARTESIAN_POINT('Ctrl Pts',(5.94168195137679,-31.3596340961814,
124.037115869749));
#116252=CARTESIAN_POINT('Ctrl Pts',(5.94262166163607,-31.3515211574746,
124.025761166212));
#116253=CARTESIAN_POINT('Ctrl Pts',(5.94427482736665,-31.3369141438955,
124.005851174607));
#116254=CARTESIAN_POINT('Ctrl Pts',(5.94499047036058,-31.3304783062755,
123.99725436875));
#116255=CARTESIAN_POINT('Ctrl Pts',(5.94648849271052,-31.3167715243964,
123.97930955603));
#116256=CARTESIAN_POINT('Ctrl Pts',(5.94727013273233,-31.3094831004363,
123.969975606245));
#116257=CARTESIAN_POINT('Ctrl Pts',(5.9493400654138,-31.2898229747473,123.94534378201));
#116258=CARTESIAN_POINT('Ctrl Pts',(5.95062140999309,-31.2772785396692,
123.930185703219));
#116259=CARTESIAN_POINT('Ctrl Pts',(5.95738993451073,-31.2090775466254,
123.850685167063));
#116260=CARTESIAN_POINT('Ctrl Pts',(5.96268129293519,-31.1488195097103,
123.790450709512));
#116261=CARTESIAN_POINT('Ctrl Pts',(5.97211489582155,-31.0321022020777,
123.690407567738));
#116262=CARTESIAN_POINT('Ctrl Pts',(5.97627484188539,-30.9772778145826,
123.649002173353));
#116263=CARTESIAN_POINT('Ctrl Pts',(5.98437098580799,-30.8676481578466,
123.576379748542));
#116264=CARTESIAN_POINT('Ctrl Pts',(5.98829093449839,-30.8133219704435,
123.544660308136));
#116265=CARTESIAN_POINT('Ctrl Pts',(5.9933738649866,-30.7435740464345,123.509063209239));
#116266=CARTESIAN_POINT('Ctrl Pts',(5.9943865547912,-30.7297111673908,123.502229507906));
#116267=CARTESIAN_POINT('Ctrl Pts',(5.99590905208018,-30.7089591788538,
123.492356297438));
#116268=CARTESIAN_POINT('Ctrl Pts',(5.99641032695816,-30.7021408462258,
123.489168812293));
#116269=CARTESIAN_POINT('Ctrl Pts',(5.99731651449941,-30.6898458835086,
123.48352227317));
#116270=CARTESIAN_POINT('Ctrl Pts',(5.99772040408426,-30.6843772391891,
123.481046468587));
#116271=CARTESIAN_POINT('Ctrl Pts',(5.99863069424564,-30.672077620677,123.475558001356));
#116272=CARTESIAN_POINT('Ctrl Pts',(5.99913802378278,-30.6652397721613,
123.472561694998));
#116273=CARTESIAN_POINT('Ctrl Pts',(6.00068204607961,-30.6444738457948,
123.463628070545));
#116274=CARTESIAN_POINT('Ctrl Pts',(6.00172663185114,-30.6304851862709,
123.457834758111));
#116275=CARTESIAN_POINT('Ctrl Pts',(6.01039377130432,-30.5147596914464,
123.411745435089));
#116276=CARTESIAN_POINT('Ctrl Pts',(6.01842867603435,-30.409365919462,123.381375223097));
#116277=CARTESIAN_POINT('Ctrl Pts',(6.03394527829849,-30.199303985209,123.342686399179));
#116278=CARTESIAN_POINT('Ctrl Pts',(6.04139989670306,-30.095283035604,123.333465123683));
#116279=CARTESIAN_POINT('Ctrl Pts',(6.05003539576169,-29.969467437326,123.33413977014));
#116280=CARTESIAN_POINT('Ctrl Pts',(6.05150504361922,-29.9478716090723,
123.334675632282));
#116281=CARTESIAN_POINT('Ctrl Pts',(6.05378762748829,-29.9140548488339,
123.33617324886));
#116282=CARTESIAN_POINT('Ctrl Pts',(6.05460933133339,-29.9018243733904,
123.33685010085));
#116283=CARTESIAN_POINT('Ctrl Pts',(6.05613894212797,-29.8789556658657,
123.338368838315));
#116284=CARTESIAN_POINT('Ctrl Pts',(6.05684782734328,-29.8683159780741,
123.339178162555));
#116285=CARTESIAN_POINT('Ctrl Pts',(6.05843184712057,-29.8444534132373,
123.34122406272));
#116286=CARTESIAN_POINT('Ctrl Pts',(6.05930518487314,-29.8312359708868,
123.342516645566));
#116287=CARTESIAN_POINT('Ctrl Pts',(6.06153703149892,-29.7973150966523,
123.346243872056));
#116288=CARTESIAN_POINT('Ctrl Pts',(6.06288832566957,-29.7766389808975,
123.348909324813));
#116289=CARTESIAN_POINT('Ctrl Pts',(6.07257998852718,-29.6275345315832,
123.370983372838));
#116290=CARTESIAN_POINT('Ctrl Pts',(6.08042704077471,-29.5017165019639,
123.404963027084));
#116291=CARTESIAN_POINT('Ctrl Pts',(6.09344431203597,-29.3042387870999,
123.483976163813));
#116292=CARTESIAN_POINT('Ctrl Pts',(6.09854832142122,-29.229772869255,123.520419457875));
#116293=CARTESIAN_POINT('Ctrl Pts',(6.10485235763993,-29.1461892512382,
123.569349360332));
#116294=CARTESIAN_POINT('Ctrl Pts',(6.10577638650614,-29.1341353518918,
123.576612341434));
#116295=CARTESIAN_POINT('Ctrl Pts',(6.10719082544782,-29.1160107174131,
123.587848606771));
#116296=CARTESIAN_POINT('Ctrl Pts',(6.10767437480609,-29.1098712051099,
123.591710494001));
#116297=CARTESIAN_POINT('Ctrl Pts',(6.1085635586109,-29.0986894110263,123.598846416347));
#116298=CARTESIAN_POINT('Ctrl Pts',(6.10896837742722,-29.0936393785891,
123.602107814244));
#116299=CARTESIAN_POINT('Ctrl Pts',(6.10990048498639,-29.0821041072831,
123.609646275242));
#116300=CARTESIAN_POINT('Ctrl Pts',(6.11042892926396,-29.0756310736528,
123.613941403914));
#116301=CARTESIAN_POINT('Ctrl Pts',(6.11206447971331,-29.0557940126292,
123.627304882392));
#116302=CARTESIAN_POINT('Ctrl Pts',(6.11318061534033,-29.0425320701174,
123.636522113214));
#116303=CARTESIAN_POINT('Ctrl Pts',(6.12028371876759,-28.9597281500227,
123.695875715826));
#116304=CARTESIAN_POINT('Ctrl Pts',(6.12651987594059,-28.8940149442416,
123.751120491557));
#116305=CARTESIAN_POINT('Ctrl Pts',(6.13647447605889,-28.7964324388262,
123.846923358677));
#116306=CARTESIAN_POINT('Ctrl Pts',(6.14018735931351,-28.7616753258736,
123.884332955355));
#116307=CARTESIAN_POINT('Ctrl Pts',(6.14767734478265,-28.6944288972366,
123.963732527376));
#116308=CARTESIAN_POINT('Ctrl Pts',(6.15144707800656,-28.6621160872555,
124.005799963437));
#116309=CARTESIAN_POINT('Ctrl Pts',(6.15764471505079,-28.6114389279093,
124.078731794292));
#116310=CARTESIAN_POINT('Ctrl Pts',(6.16010934781647,-28.591967208349,124.108775587284));
#116311=CARTESIAN_POINT('Ctrl Pts',(6.16354511030201,-28.5658158918386,
124.152125057064));
#116312=CARTESIAN_POINT('Ctrl Pts',(6.16454545768899,-28.5583243549196,
124.164926749288));
#116313=CARTESIAN_POINT('Ctrl Pts',(6.16626810636348,-28.5456411601574,
124.187279580959));
#116314=CARTESIAN_POINT('Ctrl Pts',(6.16699322149103,-28.5403702800372,
124.196784459317));
#116315=CARTESIAN_POINT('Ctrl Pts',(6.16838576952037,-28.5303815074185,
124.215220105879));
#116316=CARTESIAN_POINT('Ctrl Pts',(6.16905362342998,-28.525651092268,124.224143504363));
#116317=CARTESIAN_POINT('Ctrl Pts',(6.1708190435125,-28.5133096692025,124.247944738807));
#116318=CARTESIAN_POINT('Ctrl Pts',(6.17191160988917,-28.5058407407028,
124.262895260788));
#116319=CARTESIAN_POINT('Ctrl Pts',(6.17597884358671,-28.4786947299313,
124.319342077429));
#116320=CARTESIAN_POINT('Ctrl Pts',(6.17890271693425,-28.4605101785177,
124.361535749782));
#116321=CARTESIAN_POINT('Ctrl Pts',(6.18882374878948,-28.4039846192959,
124.509207109504));
#116322=CARTESIAN_POINT('Ctrl Pts',(6.19556586069116,-28.374564794865,124.617764990719));
#116323=CARTESIAN_POINT('Ctrl Pts',(6.20539762039084,-28.3485178108549,
124.77543452399));
#116324=CARTESIAN_POINT('Ctrl Pts',(6.20835465869034,-28.3427751774363,
124.822719603926));
#116325=CARTESIAN_POINT('Ctrl Pts',(6.21314911311099,-28.3369089056542,
124.897774693167));
#116326=CARTESIAN_POINT('Ctrl Pts',(6.21493631096052,-28.3354403449275,
124.925414848332));
#116327=CARTESIAN_POINT('Ctrl Pts',(6.21737766336993,-28.3343957306038,
124.962488970179));
#116328=CARTESIAN_POINT('Ctrl Pts',(6.21800139367624,-28.3342103356652,
124.971902962946));
#116329=CARTESIAN_POINT('Ctrl Pts',(6.21904706341704,-28.3340345460499,
124.98757811068));
#116330=CARTESIAN_POINT('Ctrl Pts',(6.21946658871795,-28.3339996297195,
124.993838730686));
#116331=CARTESIAN_POINT('Ctrl Pts',(6.22032415080722,-28.3340003890238,
125.00657498276));
#116332=CARTESIAN_POINT('Ctrl Pts',(6.220762302291,-28.3340385309373,125.013050446491));
#116333=CARTESIAN_POINT('Ctrl Pts',(6.22191082718516,-28.3342365605299,
125.029946127955));
#116334=CARTESIAN_POINT('Ctrl Pts',(6.2226243540981,-28.3344564712401,125.040365167481));
#116335=CARTESIAN_POINT('Ctrl Pts',(6.22591359864517,-28.3359113208777,
125.088072924458));
#116336=CARTESIAN_POINT('Ctrl Pts',(6.22854275201821,-28.3383008200076,
125.125312927896));
#116337=CARTESIAN_POINT('Ctrl Pts',(6.23683045955873,-28.3496178692986,
125.240830095917));
#116338=CARTESIAN_POINT('Ctrl Pts',(6.24259339284647,-28.3628473382319,
125.318576038942));
#116339=CARTESIAN_POINT('Ctrl Pts',(6.25289099295345,-28.3964544071425,
125.456245786719));
#116340=CARTESIAN_POINT('Ctrl Pts',(6.2574309774459,-28.4148310450808,125.516480354484));
#116341=CARTESIAN_POINT('Ctrl Pts',(6.2618827045692,-28.4365599067946,125.575509404752));
#116342=CARTESIAN_POINT('',(6.02851963656825,-28.3340006962934,124.998476829274));
#116343=CARTESIAN_POINT('Ctrl Pts',(6.06644913825629,-28.4365599905855,
125.57550963238));
#116344=CARTESIAN_POINT('Ctrl Pts',(6.0647519761627,-28.4281262181678,125.552598291741));
#116345=CARTESIAN_POINT('Ctrl Pts',(6.06307012626867,-28.4201955224898,
125.529500065226));
#116346=CARTESIAN_POINT('Ctrl Pts',(6.06021111114331,-28.4074578948752,
125.489562813823));
#116347=CARTESIAN_POINT('Ctrl Pts',(6.05902639191263,-28.4024043292916,
125.472810975716));
#116348=CARTESIAN_POINT('Ctrl Pts',(6.0570853241414,-28.3945009537609,125.445037411799));
#116349=CARTESIAN_POINT('Ctrl Pts',(6.056324082195,-28.3914986397866,125.434060906635));
#116350=CARTESIAN_POINT('Ctrl Pts',(6.05483979642889,-28.3858373294429,
125.412497278553));
#116351=CARTESIAN_POINT('Ctrl Pts',(6.05411649930734,-28.3831694592067,
125.401913104826));
#116352=CARTESIAN_POINT('Ctrl Pts',(6.0526836420675,-28.3780674746594,125.380798727961));
#116353=CARTESIAN_POINT('Ctrl Pts',(6.05197405189187,-28.3756314279088,
125.370269549237));
#116354=CARTESIAN_POINT('Ctrl Pts',(6.05031190153342,-28.3701410357475,
125.345441067135));
#116355=CARTESIAN_POINT('Ctrl Pts',(6.04936204384721,-28.3671721072557,
125.331123645304));
#116356=CARTESIAN_POINT('Ctrl Pts',(6.04151867578899,-28.3440813688305,
125.211896568066));
#116357=CARTESIAN_POINT('Ctrl Pts',(6.03495492927364,-28.3339033738713,
125.105313603942));
#116358=CARTESIAN_POINT('Ctrl Pts',(6.02842899135889,-28.3340006912401,
124.99848236646));
#116359=CARTESIAN_POINT('Ctrl Pts',(6.02851963656825,-28.3340006962934,
124.998476829274));
#116360=CARTESIAN_POINT('Ctrl Pts',(6.02319560875472,-28.3340734949187,
124.918851835839));
#116361=CARTESIAN_POINT('Ctrl Pts',(6.01787158094119,-28.3398584615601,
124.839481023852));
#116362=CARTESIAN_POINT('Ctrl Pts',(6.01254755312766,-28.3512247099835,
124.761052216937));
#116363=CARTESIAN_POINT('Ctrl Pts',(6.00879991051251,-28.359225539141,124.705845304173));
#116364=CARTESIAN_POINT('Ctrl Pts',(6.00505226789736,-28.3699908306089,
124.651104499726));
#116365=CARTESIAN_POINT('Ctrl Pts',(6.00130462528221,-28.3834612365898,
124.597062751297));
#116366=CARTESIAN_POINT('Ctrl Pts',(5.99722727558203,-28.3981167311039,
124.538266561431));
#116367=CARTESIAN_POINT('Ctrl Pts',(5.99314992588185,-28.4160144422315,
124.480149579522));
#116368=CARTESIAN_POINT('Ctrl Pts',(5.98907257618167,-28.4370742327457,
124.423095288585));
#116369=CARTESIAN_POINT('Ctrl Pts',(5.98495160860925,-28.4583593125581,
124.365430653441));
#116370=CARTESIAN_POINT('Ctrl Pts',(5.98083064103684,-28.4828744868681,
124.308852114328));
#116371=CARTESIAN_POINT('Ctrl Pts',(5.97670967346442,-28.5104841015508,
124.253743751606));
#116372=CARTESIAN_POINT('Ctrl Pts',(5.97264355643894,-28.5377262291229,
124.199368887458));
#116373=CARTESIAN_POINT('Ctrl Pts',(5.96857743941347,-28.5679806888366,
124.146425773315));
#116374=CARTESIAN_POINT('Ctrl Pts',(5.96451132238799,-28.6010683663941,
124.095264522362));
#116375=CARTESIAN_POINT('Ctrl Pts',(5.96044769316854,-28.634135799644,124.04413457382));
#116376=CARTESIAN_POINT('Ctrl Pts',(5.9563840639491,-28.6700327363219,123.994784755901));
#116377=CARTESIAN_POINT('Ctrl Pts',(5.95232043472965,-28.7085351232899,
123.947538850017));
#116378=CARTESIAN_POINT('Ctrl Pts',(5.9482577821129,-28.7470282570674,123.900304298633));
#116379=CARTESIAN_POINT('Ctrl Pts',(5.94419512949615,-28.7881252748384,
123.855173052227));
#116380=CARTESIAN_POINT('Ctrl Pts',(5.94013247687939,-28.8315612467258,
123.8124365786));
#116381=CARTESIAN_POINT('Ctrl Pts',(5.93596888334308,-28.876076431472,123.768638271891));
#116382=CARTESIAN_POINT('Ctrl Pts',(5.93180528980677,-28.9230479927252,
123.727355765403));
#116383=CARTESIAN_POINT('Ctrl Pts',(5.92764169627046,-28.9721516994952,
123.68886161251));
#116384=CARTESIAN_POINT('Ctrl Pts',(5.92357385644441,-29.0201261264568,
123.65125274247));
#116385=CARTESIAN_POINT('Ctrl Pts',(5.91950601661836,-29.0701351964431,
123.616305575435));
#116386=CARTESIAN_POINT('Ctrl Pts',(5.91543817679231,-29.121846243511,123.584230958113));
#116387=CARTESIAN_POINT('Ctrl Pts',(5.91122670640087,-29.1753831458841,
123.551023824366));
#116388=CARTESIAN_POINT('Ctrl Pts',(5.90701523600943,-29.2307439592215,
123.520896213987));
#116389=CARTESIAN_POINT('Ctrl Pts',(5.90280376561798,-29.2875334118873,
123.494029428965));
#116390=CARTESIAN_POINT('Ctrl Pts',(5.89859229522654,-29.3443228645532,
123.467162643943));
#116391=CARTESIAN_POINT('Ctrl Pts',(5.8943808248351,-29.4025403724686,123.443556842906));
#116392=CARTESIAN_POINT('Ctrl Pts',(5.89016935444365,-29.4617725659751,
123.423336678532));
#116393=CARTESIAN_POINT('Ctrl Pts',(5.88609200474355,-29.5191184200315,
123.4037604561));
#116394=CARTESIAN_POINT('Ctrl Pts',(5.88201465504344,-29.5776521037458,
123.387276539074));
#116395=CARTESIAN_POINT('Ctrl Pts',(5.87793730534333,-29.6370079727795,
123.374025588094));
#116396=CARTESIAN_POINT('Ctrl Pts',(5.8738163377709,-29.696998807393,123.360632883687));
#116397=CARTESIAN_POINT('Ctrl Pts',(5.86969537019848,-29.7578290526703,
123.350542981847));
#116398=CARTESIAN_POINT('Ctrl Pts',(5.86557440262605,-29.8191024520453,
123.343850225027));
#116399=CARTESIAN_POINT('Ctrl Pts',(5.86150828560065,-29.8795602955066,
123.337246549561));
#116400=CARTESIAN_POINT('Ctrl Pts',(5.85744216857525,-29.9404490441904,
123.333950195322));
#116401=CARTESIAN_POINT('Ctrl Pts',(5.85337605154985,-30.0013774075983,
123.334000569403));
#116402=CARTESIAN_POINT('Ctrl Pts',(5.84931242233048,-30.0622684927014,
123.334050912664));
#116403=CARTESIAN_POINT('Ctrl Pts',(5.84524879311111,-30.1231986335682,
123.33744392392));
#116404=CARTESIAN_POINT('Ctrl Pts',(5.84118516389174,-30.1837742889544,
123.34416697378));
#116405=CARTESIAN_POINT('Ctrl Pts',(5.83712251127506,-30.2443353863322,
123.350888407906));
#116406=CARTESIAN_POINT('Ctrl Pts',(5.83305985865839,-30.3045416587418,
123.360938235477));
#116407=CARTESIAN_POINT('Ctrl Pts',(5.82899720604172,-30.3640045429381,
123.374251959029));
#116408=CARTESIAN_POINT('Ctrl Pts',(5.82483361250533,-30.4249448456552,
123.387896476186));
#116409=CARTESIAN_POINT('Ctrl Pts',(5.82067001896895,-30.4851037654203,
123.404969181928));
#116410=CARTESIAN_POINT('Ctrl Pts',(5.81650642543256,-30.544076467027,123.425345498839));
#116411=CARTESIAN_POINT('Ctrl Pts',(5.81243858560659,-30.601692923135,123.445253204217));
#116412=CARTESIAN_POINT('Ctrl Pts',(5.80837074578062,-30.6581766839114,
123.468313913943));
#116413=CARTESIAN_POINT('Ctrl Pts',(5.80430290595464,-30.7131701817936,
123.494362496548));
#116414=CARTESIAN_POINT('Ctrl Pts',(5.80009143556305,-30.7701054344017,
123.521330823493));
#116415=CARTESIAN_POINT('Ctrl Pts',(5.79587996517146,-30.82544266909,123.551501720361));
#116416=CARTESIAN_POINT('Ctrl Pts',(5.79166849477987,-30.8788151850225,
123.584641433921));
#116417=CARTESIAN_POINT('Ctrl Pts',(5.78745702438828,-30.932187700955,123.617781147481));
#116418=CARTESIAN_POINT('Ctrl Pts',(5.78324555399669,-30.9835950480775,
123.653889273056));
#116419=CARTESIAN_POINT('Ctrl Pts',(5.7790340836051,-31.0327083033886,123.692686127928));
#116420=CARTESIAN_POINT('Ctrl Pts',(5.77495673390501,-31.0802574722521,
123.730247437842));
#116421=CARTESIAN_POINT('Ctrl Pts',(5.77087938420491,-31.1258528967944,
123.770483850586));
#116422=CARTESIAN_POINT('Ctrl Pts',(5.76680203450482,-31.1691780895278,
123.813164461702));
#116423=CARTESIAN_POINT('Ctrl Pts',(5.76268106693239,-31.212966758015,123.856301653092));
#116424=CARTESIAN_POINT('Ctrl Pts',(5.75856009935996,-31.2544358643982,
123.901935391438));
#116425=CARTESIAN_POINT('Ctrl Pts',(5.75443913178754,-31.2932912321427,
123.949783932296));
#116426=CARTESIAN_POINT('Ctrl Pts',(5.75037301476215,-31.3316294305236,
123.996995603634));
#116427=CARTESIAN_POINT('Ctrl Pts',(5.74630689773677,-31.3674227117968,
124.046363069472));
#116428=CARTESIAN_POINT('Ctrl Pts',(5.74224078071139,-31.4004257464336,
124.097578962609));
#116429=CARTESIAN_POINT('Ctrl Pts',(5.73817715149204,-31.4334085885506,
124.148763519902));
#116430=CARTESIAN_POINT('Ctrl Pts',(5.73411352227268,-31.4636042921268,
124.201793832714));
#116431=CARTESIAN_POINT('Ctrl Pts',(5.73004989305333,-31.4908100250261,
124.256332420176));
#116432=CARTESIAN_POINT('Ctrl Pts',(5.72598724043667,-31.518009219634,124.310857900503));
#116433=CARTESIAN_POINT('Ctrl Pts',(5.72192458782002,-31.5422196416099,
124.366890477986));
#116434=CARTESIAN_POINT('Ctrl Pts',(5.71786193520336,-31.5632847353325,
124.42406872261));
#116435=CARTESIAN_POINT('Ctrl Pts',(5.71369834166696,-31.5848732136847,
124.482667621457));
#116436=CARTESIAN_POINT('Ctrl Pts',(5.70953474813056,-31.6031577274293,
124.542469372818));
#116437=CARTESIAN_POINT('Ctrl Pts',(5.70537115459415,-31.6180233714039,
124.603066290685));
#116438=CARTESIAN_POINT('Ctrl Pts',(5.7013033147682,-31.6325471374895,124.662269609566));
#116439=CARTESIAN_POINT('Ctrl Pts',(5.69723547494225,-31.643807594015,124.72223137808));
#116440=CARTESIAN_POINT('Ctrl Pts',(5.6931676351163,-31.651749543316,124.782561626764));
#116441=CARTESIAN_POINT('Ctrl Pts',(5.68895616472467,-31.659971913361,124.845022064472));
#116442=CARTESIAN_POINT('Ctrl Pts',(5.68474469433304,-31.6646369573864,
124.907876896626));
#116443=CARTESIAN_POINT('Ctrl Pts',(5.68053322394141,-31.6657421763008,
124.970691262523));
#116444=CARTESIAN_POINT('Ctrl Pts',(5.67632175354978,-31.6668473952153,
125.03350562842));
#116445=CARTESIAN_POINT('Ctrl Pts',(5.67211028315816,-31.6643928849113,
125.096278930468));
#116446=CARTESIAN_POINT('Ctrl Pts',(5.66789881276653,-31.6584352230018,
125.158583136263));
#116447=CARTESIAN_POINT('Ctrl Pts',(5.66382146306639,-31.6526672919133,
125.218903169694));
#116448=CARTESIAN_POINT('Ctrl Pts',(5.65974411336626,-31.6435922496629,
125.279032657119));
#116449=CARTESIAN_POINT('Ctrl Pts',(5.65566676366613,-31.6312324376956,
125.338580469327));
#116450=CARTESIAN_POINT('Ctrl Pts',(5.6515457960937,-31.6187404053549,125.398765300447));
#116451=CARTESIAN_POINT('Ctrl Pts',(5.64742482852128,-31.6028928679922,
125.458355403813));
#116452=CARTESIAN_POINT('Ctrl Pts',(5.64330386094886,-31.5837669805991,
125.516950820837));
#116453=CARTESIAN_POINT('Ctrl Pts',(5.63923774392343,-31.564895660942,125.574766326198));
#116454=CARTESIAN_POINT('Ctrl Pts',(5.63517162689801,-31.542832892783,125.631612961355));
#116455=CARTESIAN_POINT('Ctrl Pts',(5.63110550987258,-31.5177038507697,
125.687117909357));
#116456=CARTESIAN_POINT('Ctrl Pts',(5.62704188065318,-31.4925901836661,
125.742588897307));
#116457=CARTESIAN_POINT('Ctrl Pts',(5.62297825143379,-31.4644141731075,
125.796719360269));
#116458=CARTESIAN_POINT('Ctrl Pts',(5.61891462221439,-31.4333493426061,
125.849155852627));
#116459=CARTESIAN_POINT('Ctrl Pts',(5.61485196959769,-31.4022919778441,
125.901579743043));
#116460=CARTESIAN_POINT('Ctrl Pts',(5.61078931698099,-31.3683474321801,
125.952310030756));
#116461=CARTESIAN_POINT('Ctrl Pts',(5.60672666436429,-31.3317344485663,
126.001019159907));
#116462=CARTESIAN_POINT('Ctrl Pts',(5.60256307082793,-31.2942117764839,
126.050938519112));
#116463=CARTESIAN_POINT('Ctrl Pts',(5.59839947729157,-31.2538865838682,
126.098734457738));
#116464=CARTESIAN_POINT('Ctrl Pts',(5.59423588375521,-31.2110390650589,
126.144089324704));
#116465=CARTESIAN_POINT('Ctrl Pts',(5.59016804392921,-31.1691769471707,
126.188401127125));
#116466=CARTESIAN_POINT('Ctrl Pts',(5.58610020410322,-31.1249077208041,
126.230382636882));
#116467=CARTESIAN_POINT('Ctrl Pts',(5.58203236427722,-31.0785290790597,
126.269775974581));
#116468=CARTESIAN_POINT('Ctrl Pts',(5.57782089388568,-31.030512862871,126.310560243982));
#116469=CARTESIAN_POINT('Ctrl Pts',(5.57360942349414,-30.9802359328558,
126.348569754225));
#116470=CARTESIAN_POINT('Ctrl Pts',(5.5693979531026,-30.9280622790153,126.383566552888));
#116471=CARTESIAN_POINT('Ctrl Pts',(5.56518648271105,-30.8758886251748,
126.41856335155));
#116472=CARTESIAN_POINT('Ctrl Pts',(5.56097501231951,-30.8218188015804,
126.450547195083));
#116473=CARTESIAN_POINT('Ctrl Pts',(5.55676354192797,-30.7662431025642,
126.479333467401));
#116474=CARTESIAN_POINT('Ctrl Pts',(5.55268619222786,-30.7124372963612,
126.507202997017));
#116475=CARTESIAN_POINT('Ctrl Pts',(5.54860884252774,-30.6569979178379,
126.532190733182));
#116476=CARTESIAN_POINT('Ctrl Pts',(5.54453149282763,-30.6002656888768,
126.554103311481));
#116477=CARTESIAN_POINT('Ctrl Pts',(5.5404105252552,-30.5429265609983,126.576250301866));
#116478=CARTESIAN_POINT('Ctrl Pts',(5.53628955768278,-30.484267184399,126.595255627346));
#116479=CARTESIAN_POINT('Ctrl Pts',(5.53216859011035,-30.4246654278064,
126.610967186018));
#116480=CARTESIAN_POINT('Ctrl Pts',(5.52810247308495,-30.3658569773718,
126.626469622057));
#116481=CARTESIAN_POINT('Ctrl Pts',(5.52403635605954,-30.3061315899492,
126.638765302794));
#116482=CARTESIAN_POINT('Ctrl Pts',(5.51997023903413,-30.2458703755337,
126.647757190376));
#116483=CARTESIAN_POINT('Ctrl Pts',(5.51590660981476,-30.1856460312358,
126.656743576377));
#116484=CARTESIAN_POINT('Ctrl Pts',(5.51184298059538,-30.124887015264,126.662430101641));
#116485=CARTESIAN_POINT('Ctrl Pts',(5.507779351376,-30.0639843855967,126.664770854622));
#116486=CARTESIAN_POINT('Ctrl Pts',(5.50371669875932,-30.0030963925188,
126.667111045055));
#116487=CARTESIAN_POINT('Ctrl Pts',(5.49965404614264,-29.942065365614,126.66610703977));
#116488=CARTESIAN_POINT('Ctrl Pts',(5.49559139352596,-29.8812851371463,
126.661764959715));
#116489=CARTESIAN_POINT('Ctrl Pts',(5.49142779998959,-29.8189947593402,
126.65731499607));
#116490=CARTESIAN_POINT('Ctrl Pts',(5.48726420645321,-29.7569683731697,
126.64935884579));
#116491=CARTESIAN_POINT('Ctrl Pts',(5.48310061291683,-29.6956248184908,
126.637959629808));
#116492=CARTESIAN_POINT('Ctrl Pts',(5.47903277309085,-29.6356920338398,
126.626822571315));
#116493=CARTESIAN_POINT('Ctrl Pts',(5.47496493326487,-29.5764115003722,
126.612399329089));
#116494=CARTESIAN_POINT('Ctrl Pts',(5.47089709343889,-29.5181613318449,
126.594800143551));
#116495=CARTESIAN_POINT('Ctrl Pts',(5.46668562304731,-29.4578544194412,
126.576579551792));
#116496=CARTESIAN_POINT('Ctrl Pts',(5.46247415265573,-29.3986525730831,
126.554954706161));
#116497=CARTESIAN_POINT('Ctrl Pts',(5.45826268226415,-29.3409531220702,
126.530102353665));
#116498=CARTESIAN_POINT('Ctrl Pts',(5.45405121187257,-29.2832536710573,
126.505250001169));
#116499=CARTESIAN_POINT('Ctrl Pts',(5.44983974148099,-29.2270571205141,
126.477170475215));
#116500=CARTESIAN_POINT('Ctrl Pts',(5.44562827108941,-29.1727302560843,
126.446091549938));
#116501=CARTESIAN_POINT('Ctrl Pts',(5.44155183031644,-29.1201452383499,
126.4160090879));
#116502=CARTESIAN_POINT('Ctrl Pts',(5.43747538954347,-29.0690946646957,
126.382992519672));
#116503=CARTESIAN_POINT('Ctrl Pts',(5.43339894877049,-29.0199255545782,
126.347223100096));
#116504=CARTESIAN_POINT('Ctrl Pts',(5.42932840898429,-28.9708276208335,
126.311505459726));
#116505=CARTESIAN_POINT('Ctrl Pts',(5.42525786919808,-28.9236061619891,
126.273043165973));
#116506=CARTESIAN_POINT('Ctrl Pts',(5.42118732941187,-28.8785820263563,
126.232062388188));
#116507=CARTESIAN_POINT('Ctrl Pts',(5.41712116917619,-28.8336063328189,
126.191125702195));
#116508=CARTESIAN_POINT('Ctrl Pts',(5.41305500894051,-28.7908236503885,
126.147676249286));
#116509=CARTESIAN_POINT('Ctrl Pts',(5.40898884870483,-28.7505226465905,
126.101981099346));
#116510=CARTESIAN_POINT('Ctrl Pts',(5.40492500380744,-28.7102445908447,
126.056311968974));
#116511=CARTESIAN_POINT('Ctrl Pts',(5.40086115891004,-28.6724457521372,
126.008400058139));
#116512=CARTESIAN_POINT('Ctrl Pts',(5.39679731401265,-28.6373773381303,
125.958548632756));
#116513=CARTESIAN_POINT('Ctrl Pts',(5.392734798567,-28.602320396452,125.908713515837));
#116514=CARTESIAN_POINT('Ctrl Pts',(5.38867228312134,-28.5699923969535,
125.856940565118));
#116515=CARTESIAN_POINT('Ctrl Pts',(5.38460976767569,-28.54060233297,125.803563593916));
#116516=CARTESIAN_POINT('Ctrl Pts',(5.38054576390131,-28.5112015017471,
125.750167067717));
#116517=CARTESIAN_POINT('Ctrl Pts',(5.37648176012692,-28.4847409988668,
125.695165798197));
#116518=CARTESIAN_POINT('Ctrl Pts',(5.37241775635254,-28.4613839509542,
125.638918346597));
#116519=CARTESIAN_POINT('Ctrl Pts',(5.37090265146513,-28.4526761890001,
125.617948683783));
#116520=CARTESIAN_POINT('Ctrl Pts',(5.36938754657771,-28.4443992926494,
125.596806024743));
#116521=CARTESIAN_POINT('Ctrl Pts',(5.3678724416903,-28.4365599837785,125.575509613888));
#116522=CARTESIAN_POINT('Origin',(5.,-30.,125.));
#116523=CARTESIAN_POINT('',(4.66781556895434,-28.4339562630661,125.576468403481));
#116524=CARTESIAN_POINT('',(4.86075486118656,-28.4365599784656,125.575509599455));
#116525=CARTESIAN_POINT('',(5.,-28.4365599837785,125.575509613888));
#116526=CARTESIAN_POINT('',(5.52205821453768,-28.3340005850234,125.001396172494));
#116527=CARTESIAN_POINT('Ctrl Pts',(4.86075486118656,-28.4365599784656,
125.575509599455));
#116528=CARTESIAN_POINT('Ctrl Pts',(4.86238043919705,-28.4457530879321,
125.600483770652));
#116529=CARTESIAN_POINT('Ctrl Pts',(4.86400410782707,-28.4555447508684,
125.625238079615));
#116530=CARTESIAN_POINT('Ctrl Pts',(4.86651230638005,-28.471533401758,125.662987554203));
#116531=CARTESIAN_POINT('Ctrl Pts',(4.86739308927612,-28.4773107607449,
125.676150954234));
#116532=CARTESIAN_POINT('Ctrl Pts',(4.87273750404912,-28.5132941123096,
125.755336207118));
#116533=CARTESIAN_POINT('Ctrl Pts',(4.87725398811927,-28.547615579312,125.819392473812));
#116534=CARTESIAN_POINT('Ctrl Pts',(4.88279718916779,-28.592490550416,125.891416759702));
#116535=CARTESIAN_POINT('Ctrl Pts',(4.88360534816387,-28.5990967308248,
125.901763105706));
#116536=CARTESIAN_POINT('Ctrl Pts',(4.88488230900459,-28.6096212186161,
125.917851376678));
#116537=CARTESIAN_POINT('Ctrl Pts',(4.88534623716257,-28.6134623137335,
125.923643624771));
#116538=CARTESIAN_POINT('Ctrl Pts',(4.88621893813826,-28.6207175626951,
125.934437063524));
#116539=CARTESIAN_POINT('Ctrl Pts',(4.88662713725671,-28.6241228851158,
125.939443892735));
#116540=CARTESIAN_POINT('Ctrl Pts',(4.88759380217016,-28.6322155109139,
125.951204063062));
#116541=CARTESIAN_POINT('Ctrl Pts',(4.88815375538808,-28.6369255886961,
125.957941397128));
#116542=CARTESIAN_POINT('Ctrl Pts',(4.89004013162794,-28.6528735222028,
125.98039768879));
#116543=CARTESIAN_POINT('Ctrl Pts',(4.89138013178083,-28.6643344913381,
125.995955292534));
#116544=CARTESIAN_POINT('Ctrl Pts',(4.89471664534451,-28.6932522011111,
126.033812390676));
#116545=CARTESIAN_POINT('Ctrl Pts',(4.89672778407849,-28.7110116039955,
126.055872436836));
#116546=CARTESIAN_POINT('Ctrl Pts',(4.90595650221888,-28.7943058631281,
126.154102798447));
#116547=CARTESIAN_POINT('Ctrl Pts',(4.91334705981141,-28.8660872086386,
126.22470155148));
#116548=CARTESIAN_POINT('Ctrl Pts',(4.92651682306763,-29.0073635626406,
126.340517048636));
#116549=CARTESIAN_POINT('Ctrl Pts',(4.93232985908405,-29.0747113701787,
126.387860820313));
#116550=CARTESIAN_POINT('Ctrl Pts',(4.93929776894664,-29.1621105600168,
126.440097673046));
#116551=CARTESIAN_POINT('Ctrl Pts',(4.94062817726602,-29.1791082423171,
126.449854061832));
#116552=CARTESIAN_POINT('Ctrl Pts',(4.94274416254166,-29.206633147188,126.465013610755));
#116553=CARTESIAN_POINT('Ctrl Pts',(4.94353650619432,-29.2170522097914,
126.470608245974));
#116554=CARTESIAN_POINT('Ctrl Pts',(4.94504113085666,-29.2370482583143,
126.481072599086));
#116555=CARTESIAN_POINT('Ctrl Pts',(4.94575406081811,-29.2466144604934,
126.485961521032));
#116556=CARTESIAN_POINT('Ctrl Pts',(4.94738782273622,-29.2687431492796,
126.497002021461));
#116557=CARTESIAN_POINT('Ctrl Pts',(4.94830636003383,-29.2813372668548,
126.503088663298));
#116558=CARTESIAN_POINT('Ctrl Pts',(4.9512200213547,-29.3217579626969,126.521999484024));
#116559=CARTESIAN_POINT('Ctrl Pts',(4.95319442882247,-29.3498632007468,
126.534215441782));
#116560=CARTESIAN_POINT('Ctrl Pts',(4.95785936667107,-29.4177907695341,
126.561538051706));
#116561=CARTESIAN_POINT('Ctrl Pts',(4.96052724007215,-29.4578870085852,
126.575906901092));
#116562=CARTESIAN_POINT('Ctrl Pts',(4.96773457412782,-29.568755230396,126.610904347099));
#116563=CARTESIAN_POINT('Ctrl Pts',(4.9722067458145,-29.6404140538691,126.628398960873));
#116564=CARTESIAN_POINT('Ctrl Pts',(4.97757843672751,-29.7269056389501,
126.643525136016));
#116565=CARTESIAN_POINT('Ctrl Pts',(4.97844356417774,-29.7408457863712,
126.645780814707));
#116566=CARTESIAN_POINT('Ctrl Pts',(4.98380457014615,-29.8271614618932,
126.658623842087));
#116567=CARTESIAN_POINT('Ctrl Pts',(4.98835306559782,-29.9001317687946,
126.664611019222));
#116568=CARTESIAN_POINT('Ctrl Pts',(4.99393179432279,-29.985525347942,126.665982362427));
#116569=CARTESIAN_POINT('Ctrl Pts',(4.99474010364641,-29.9978030533051,
126.66604378668));
#116570=CARTESIAN_POINT('Ctrl Pts',(4.99601725093119,-30.0170304720378,
126.665927452106));
#116571=CARTESIAN_POINT('Ctrl Pts',(4.99648121290226,-30.0239805867628,
126.665841901184));
#116572=CARTESIAN_POINT('Ctrl Pts',(4.99735393942934,-30.0369840179344,
126.665600446852));
#116573=CARTESIAN_POINT('Ctrl Pts',(4.99776212985249,-30.043037281797,126.665455029062));
#116574=CARTESIAN_POINT('Ctrl Pts',(4.99872872240624,-30.0573056249283,
126.665034422571));
#116575=CARTESIAN_POINT('Ctrl Pts',(4.9992886112851,-30.065519608345,126.664731430842));
#116576=CARTESIAN_POINT('Ctrl Pts',(5.00117453888885,-30.0930292488551,
126.663512765216));
#116577=CARTESIAN_POINT('Ctrl Pts',(5.0025141462926,-30.1123103650977,126.662322310361));
#116578=CARTESIAN_POINT('Ctrl Pts',(5.00584946262772,-30.1597830797899,
126.658561606865));
#116579=CARTESIAN_POINT('Ctrl Pts',(5.00785978434464,-30.1879377026819,
126.655607584944));
#116580=CARTESIAN_POINT('Ctrl Pts',(5.01708122616136,-30.3155424992718,
126.638922420814));
#116581=CARTESIAN_POINT('Ctrl Pts',(5.02446512550131,-30.4137024591961,
126.616936771744));
#116582=CARTESIAN_POINT('Ctrl Pts',(5.03763638152116,-30.5876504326763,
126.561088328707));
#116583=CARTESIAN_POINT('Ctrl Pts',(5.04345688619681,-30.6640509648988,
126.530153515268));
#116584=CARTESIAN_POINT('Ctrl Pts',(5.05043201840522,-30.7554342714904,
126.485011517827));
#116585=CARTESIAN_POINT('Ctrl Pts',(5.05176264828876,-30.7728528799514,
126.476021215801));
#116586=CARTESIAN_POINT('Ctrl Pts',(5.05387889924891,-30.8005210812038,
126.46111664744));
#116587=CARTESIAN_POINT('Ctrl Pts',(5.05467129004169,-30.8108729231281,
126.455397187677));
#116588=CARTESIAN_POINT('Ctrl Pts',(5.05617595113781,-30.8305101034968,
126.444272954867));
#116589=CARTESIAN_POINT('Ctrl Pts',(5.05688887094814,-30.8398057360168,
126.438887672872));
#116590=CARTESIAN_POINT('Ctrl Pts',(5.05852253475496,-30.8610818807263,
126.426285241668));
#116591=CARTESIAN_POINT('Ctrl Pts',(5.0594409850558,-30.8730250084303,126.419006324978));
#116592=CARTESIAN_POINT('Ctrl Pts',(5.06235405598912,-30.9108279266776,
126.395308818645));
#116593=CARTESIAN_POINT('Ctrl Pts',(5.0643279722908,-30.936328077378,126.378326569357));
#116594=CARTESIAN_POINT('Ctrl Pts',(5.06899149950454,-30.9961067443332,
126.336090848631));
#116595=CARTESIAN_POINT('Ctrl Pts',(5.07165847292855,-31.029914401008,126.310207658955));
#116596=CARTESIAN_POINT('Ctrl Pts',(5.0788653922523,-31.1194453933778,126.236053341707));
#116597=CARTESIAN_POINT('Ctrl Pts',(5.08333798792775,-31.1730155419773,
126.185335713181));
#116598=CARTESIAN_POINT('Ctrl Pts',(5.08870730168159,-31.2326097943606,
126.120904645166));
#116599=CARTESIAN_POINT('Ctrl Pts',(5.08956965213516,-31.2420360638132,
126.110450601654));
#116600=CARTESIAN_POINT('Ctrl Pts',(5.09493172130901,-31.2996610953757,
126.044890763764));
#116601=CARTESIAN_POINT('Ctrl Pts',(5.09948403184024,-31.3443105863923,
125.986783670037));
#116602=CARTESIAN_POINT('Ctrl Pts',(5.10506699466941,-31.3918132310617,
125.91573068278));
#116603=CARTESIAN_POINT('Ctrl Pts',(5.10587531991308,-31.398523963689,125.905448758776));
#116604=CARTESIAN_POINT('Ctrl Pts',(5.10715248694237,-31.4088546555001,
125.889231619491));
#116605=CARTESIAN_POINT('Ctrl Pts',(5.10761645249436,-31.4125523042486,
125.883346079864));
#116606=CARTESIAN_POINT('Ctrl Pts',(5.10848918172814,-31.4194020673945,
125.872290339888));
#116607=CARTESIAN_POINT('Ctrl Pts',(5.10889737123119,-31.4225629633968,
125.867125871183));
#116608=CARTESIAN_POINT('Ctrl Pts',(5.10986395612519,-31.4299481768046,
125.854910388895));
#116609=CARTESIAN_POINT('Ctrl Pts',(5.11042383819312,-31.4341485424474,
125.847845217301));
#116610=CARTESIAN_POINT('Ctrl Pts',(5.11230971830816,-31.448044594566,125.824072806649));
#116611=CARTESIAN_POINT('Ctrl Pts',(5.11364928413995,-31.4575015556837,
125.807228761969));
#116612=CARTESIAN_POINT('Ctrl Pts',(5.11698447375815,-31.4800887441408,
125.765306787422));
#116613=CARTESIAN_POINT('Ctrl Pts',(5.11899470900334,-31.4928765283363,
125.740051795234));
#116614=CARTESIAN_POINT('Ctrl Pts',(5.12821538114816,-31.5480627377876,
125.623805773471));
#116615=CARTESIAN_POINT('Ctrl Pts',(5.13559857624145,-31.5828279437222,
125.529422384309));
#116616=CARTESIAN_POINT('Ctrl Pts',(5.1487699904762,-31.6302543442041,125.352990577226));
#116617=CARTESIAN_POINT('Ctrl Pts',(5.15459128551917,-31.6457044703404,
125.272014770313));
#116618=CARTESIAN_POINT('Ctrl Pts',(5.16156718184215,-31.6573431207567,
125.170745248412));
#116619=CARTESIAN_POINT('Ctrl Pts',(5.16289783502591,-31.6592372530369,
125.151234767285));
#116620=CARTESIAN_POINT('Ctrl Pts',(5.16501411392607,-31.6617215638531,
125.119905399332));
#116621=CARTESIAN_POINT('Ctrl Pts',(5.16580650967613,-31.6625308744097,
125.10810626569));
#116622=CARTESIAN_POINT('Ctrl Pts',(5.16731117460445,-31.6638354357006,
125.085574778323));
#116623=CARTESIAN_POINT('Ctrl Pts',(5.1680240933481,-31.6643526467217,125.074844347471));
#116624=CARTESIAN_POINT('Ctrl Pts',(5.16965774684138,-31.6653042169947,
125.050134387123));
#116625=CARTESIAN_POINT('Ctrl Pts',(5.17057618799685,-31.6656664099426,
125.036152765577));
#116626=CARTESIAN_POINT('Ctrl Pts',(5.1734891968717,-31.6662600665422,124.991541176395));
#116627=CARTESIAN_POINT('Ctrl Pts',(5.17546306154493,-31.6658229611774,
124.960907648763));
#116628=CARTESIAN_POINT('Ctrl Pts',(5.18012644049014,-31.6627609546134,
124.887780233753));
#116629=CARTESIAN_POINT('Ctrl Pts',(5.18279331932223,-31.6593516971863,
124.845340392403));
#116630=CARTESIAN_POINT('Ctrl Pts',(5.1900001943174,-31.645610503253,124.729903673284));
#116631=CARTESIAN_POINT('Ctrl Pts',(5.19447283384993,-31.6320551303181,
124.65738889661));
#116632=CARTESIAN_POINT('Ctrl Pts',(5.19984188142381,-31.6102469581482,
124.572380166922));
#116633=CARTESIAN_POINT('Ctrl Pts',(5.20070392437248,-31.6065779481966,
124.558795650451));
#116634=CARTESIAN_POINT('Ctrl Pts',(5.20606610542568,-31.5827525323426,
124.474822766881));
#116635=CARTESIAN_POINT('Ctrl Pts',(5.21061883258998,-31.5581485787204,
124.405788754817));
#116636=CARTESIAN_POINT('Ctrl Pts',(5.21620225783166,-31.5242147919116,
124.32733662035));
#116637=CARTESIAN_POINT('Ctrl Pts',(5.217010584809,-31.5192161497886,124.316122070349));
#116638=CARTESIAN_POINT('Ctrl Pts',(5.21828775398837,-31.5111944078119,
124.298647182006));
#116639=CARTESIAN_POINT('Ctrl Pts',(5.21875171993036,-31.5082551791437,
124.292348515355));
#116640=CARTESIAN_POINT('Ctrl Pts',(5.219624449459,-31.5026818342507,124.280597490286));
#116641=CARTESIAN_POINT('Ctrl Pts',(5.2200326388619,-31.5000572963385,124.275140862658));
#116642=CARTESIAN_POINT('Ctrl Pts',(5.22099922292171,-31.4938000177251,
124.262310994892));
#116643=CARTESIAN_POINT('Ctrl Pts',(5.22155910424794,-31.4901423918131,
124.254950198812));
#116644=CARTESIAN_POINT('Ctrl Pts',(5.22344497919173,-31.4777069085841,
124.23038228427));
#116645=CARTESIAN_POINT('Ctrl Pts',(5.22478454049656,-31.4686846406716,
124.213301529963));
#116646=CARTESIAN_POINT('Ctrl Pts',(5.22811971631613,-31.4457147433573,
124.171588240694));
#116647=CARTESIAN_POINT('Ctrl Pts',(5.23012994214515,-31.4314326310571,
124.14714737267));
#116648=CARTESIAN_POINT('Ctrl Pts',(5.23935053048307,-31.3637009524461,
124.037736319938));
#116649=CARTESIAN_POINT('Ctrl Pts',(5.24673364889391,-31.3032614797006,
123.957339139325));
#116650=CARTESIAN_POINT('Ctrl Pts',(5.25990508035964,-31.1807560127768,
123.821803494397));
#116651=CARTESIAN_POINT('Ctrl Pts',(5.26572646146689,-31.1211035184108,
123.764903917407));
#116652=CARTESIAN_POINT('Ctrl Pts',(5.27270244099332,-31.0423340409034,
123.700200050631));
#116653=CARTESIAN_POINT('Ctrl Pts',(5.27403309671259,-31.0269697176762,
123.688026899243));
#116654=CARTESIAN_POINT('Ctrl Pts',(5.27614937865315,-31.0019959179074,
123.668947769153));
#116655=CARTESIAN_POINT('Ctrl Pts',(5.27694177494266,-30.9925218869149,
123.661868400633));
#116656=CARTESIAN_POINT('Ctrl Pts',(5.27844644028799,-30.9742997460758,
123.648552108096));
#116657=CARTESIAN_POINT('Ctrl Pts',(5.2791593589156,-30.9655651623088,123.642297777018));
#116658=CARTESIAN_POINT('Ctrl Pts',(5.28079301128667,-30.9453213609007,
123.628096535429));
#116659=CARTESIAN_POINT('Ctrl Pts',(5.28171145144698,-30.9337712454245,
123.620209120028));
#116660=CARTESIAN_POINT('Ctrl Pts',(5.28462445356896,-30.8966131735221,
123.595514694759));
#116661=CARTESIAN_POINT('Ctrl Pts',(5.28659831262428,-30.8706396207975,
123.579267444194));
#116662=CARTESIAN_POINT('Ctrl Pts',(5.29126167543586,-30.8075416051257,
123.542178402699));
#116663=CARTESIAN_POINT('Ctrl Pts',(5.29392854397502,-30.770037145724,123.522024888971));
#116664=CARTESIAN_POINT('Ctrl Pts',(5.30113541413808,-30.6656011137827,
123.470960719107));
#116665=CARTESIAN_POINT('Ctrl Pts',(5.30560805843472,-30.597326287486,123.44301970664));
#116666=CARTESIAN_POINT('Ctrl Pts',(5.3109770768539,-30.5140792409551,123.41523613542));
#116667=CARTESIAN_POINT('Ctrl Pts',(5.31183908615908,-30.5006768831049,
123.410951031273));
#116668=CARTESIAN_POINT('Ctrl Pts',(5.31720127938764,-30.4172053775509,
123.385423742675));
#116669=CARTESIAN_POINT('Ctrl Pts',(5.32175405207011,-30.3458618548013,
123.368652799818));
#116670=CARTESIAN_POINT('Ctrl Pts',(5.32733752783174,-30.261545568793,123.35461230413));
#116671=CARTESIAN_POINT('Ctrl Pts',(5.32814585499848,-30.2494126499903,
123.352729511422));
#116672=CARTESIAN_POINT('Ctrl Pts',(5.32942302441272,-30.2303805268127,
123.349991173847));
#116673=CARTESIAN_POINT('Ctrl Pts',(5.32988699039733,-30.2234946098815,
123.349044377187));
#116674=CARTESIAN_POINT('Ctrl Pts',(5.33075971995818,-30.2105992792555,
123.347353452929));
#116675=CARTESIAN_POINT('Ctrl Pts',(5.33116790935014,-30.2045914737466,
123.346598962697));
#116676=CARTESIAN_POINT('Ctrl Pts',(5.33213449331878,-30.1904188211004,
123.344897515631));
#116677=CARTESIAN_POINT('Ctrl Pts',(5.33269437456398,-30.1822509319145,
123.343978215141));
#116678=CARTESIAN_POINT('Ctrl Pts',(5.33458024894301,-30.1548658053897,
123.341101052477));
#116679=CARTESIAN_POINT('Ctrl Pts',(5.33591980975339,-30.1356221725721,
123.339417065443));
#116680=CARTESIAN_POINT('Ctrl Pts',(5.33925498406594,-30.0881189949893,
123.336091287347));
#116681=CARTESIAN_POINT('Ctrl Pts',(5.34126520886653,-30.059839066475,123.334834462726));
#116682=CARTESIAN_POINT('Ctrl Pts',(5.35048578805117,-29.9311829713013,
123.33239816749));
#116683=CARTESIAN_POINT('Ctrl Pts',(5.35786889808692,-29.8308577096969,
123.339571435432));
#116684=CARTESIAN_POINT('Ctrl Pts',(5.37104209114812,-29.650521632075,123.368987836374));
#116685=CARTESIAN_POINT('Ctrl Pts',(5.37686516662464,-29.5703409067214,
123.388251713395));
#116686=CARTESIAN_POINT('Ctrl Pts',(5.3838418129469,-29.4732488167275,123.419344170878));
#116687=CARTESIAN_POINT('Ctrl Pts',(5.38517157920922,-29.4547009015659,
123.425646605975));
#116688=CARTESIAN_POINT('Ctrl Pts',(5.38728679456708,-29.4251416407104,
123.436275707448));
#116689=CARTESIAN_POINT('Ctrl Pts',(5.38807900161115,-29.4140582086348,
123.440394913458));
#116690=CARTESIAN_POINT('Ctrl Pts',(5.38958352077166,-29.3929895943905,
123.448481459267));
#116691=CARTESIAN_POINT('Ctrl Pts',(5.3902964802308,-29.3829971488306,123.452428061243));
#116692=CARTESIAN_POINT('Ctrl Pts',(5.39193052687161,-29.3600810017637,
123.461736231927));
#116693=CARTESIAN_POINT('Ctrl Pts',(5.39284931659802,-29.3471851515069,
123.467164543131));
#116694=CARTESIAN_POINT('Ctrl Pts',(5.39576469149395,-29.3062517407561,
123.485005137055));
#116695=CARTESIAN_POINT('Ctrl Pts',(5.39774052460512,-29.2784868415909,
123.498029616269));
#116696=CARTESIAN_POINT('Ctrl Pts',(5.40240955778406,-29.2130255967973,
123.530971864591));
#116697=CARTESIAN_POINT('Ctrl Pts',(5.40508004422706,-29.1757028321056,
123.551584681367));
#116698=CARTESIAN_POINT('Ctrl Pts',(5.41233686025362,-29.0754755121674,
123.612069231686));
#116699=CARTESIAN_POINT('Ctrl Pts',(5.41685382822784,-29.0143905616757,
123.654759599325));
#116700=CARTESIAN_POINT('Ctrl Pts',(5.42221445115768,-28.9461024652947,
123.709639854212));
#116701=CARTESIAN_POINT('Ctrl Pts',(5.4230211358357,-28.9359387851882,123.718008172611));
#116702=CARTESIAN_POINT('Ctrl Pts',(5.42833055829348,-28.8698708299322,
123.773732547345));
#116703=CARTESIAN_POINT('Ctrl Pts',(5.43288614633392,-28.8170499867948,
123.824606295463));
#116704=CARTESIAN_POINT('Ctrl Pts',(5.43847274690479,-28.759491573965,123.887864395107));
#116705=CARTESIAN_POINT('Ctrl Pts',(5.4392810857625,-28.7513291738461,123.897036761771));
#116706=CARTESIAN_POINT('Ctrl Pts',(5.44055826967646,-28.738706087534,123.911541465898));
#116707=CARTESIAN_POINT('Ctrl Pts',(5.44102223829059,-28.7341759407456,
123.916813145981));
#116708=CARTESIAN_POINT('Ctrl Pts',(5.44189496983914,-28.7257613351789,
123.926730000916));
#116709=CARTESIAN_POINT('Ctrl Pts',(5.44230315855554,-28.7218690420643,
123.931368203944));
#116710=CARTESIAN_POINT('Ctrl Pts',(5.44326973689955,-28.7127528939033,
123.94235239902));
#116711=CARTESIAN_POINT('Ctrl Pts',(5.44382961314334,-28.7075506235169,
123.948715946017));
#116712=CARTESIAN_POINT('Ctrl Pts',(5.44571545265216,-28.6902809929302,
123.970162516875));
#116713=CARTESIAN_POINT('Ctrl Pts',(5.4470549829368,-28.6784294002208,123.985416248211));
#116714=CARTESIAN_POINT('Ctrl Pts',(5.45450747594605,-28.6146156901012,
124.070563956309));
#116715=CARTESIAN_POINT('Ctrl Pts',(5.46085766180495,-28.567934519736,124.144238879998));
#116716=CARTESIAN_POINT('Ctrl Pts',(5.47370801870482,-28.4854054804999,
124.300311162647));
#116717=CARTESIAN_POINT('Ctrl Pts',(5.4801850158172,-28.4500167530918,124.382653781712));
#116718=CARTESIAN_POINT('Ctrl Pts',(5.48939016492012,-28.4081136754622,
124.50686285228));
#116719=CARTESIAN_POINT('Ctrl Pts',(5.49226834727872,-28.3962967092375,
124.546764304565));
#116720=CARTESIAN_POINT('Ctrl Pts',(5.49619599336575,-28.3819883320362,
124.602691235687));
#116721=CARTESIAN_POINT('Ctrl Pts',(5.49728578887273,-28.3782185524634,
124.618370624752));
#116722=CARTESIAN_POINT('Ctrl Pts',(5.49903921563436,-28.372481873467,124.643853071922));
#116723=CARTESIAN_POINT('Ctrl Pts',(5.49970729688571,-28.3703745997395,
124.65362311146));
#116724=CARTESIAN_POINT('Ctrl Pts',(5.50110147936075,-28.3661429895898,
124.674136255641));
#116725=CARTESIAN_POINT('Ctrl Pts',(5.5018269849342,-28.36403639343,124.684882564649));
#116726=CARTESIAN_POINT('Ctrl Pts',(5.50326582985179,-28.3600506634912,
124.706333075816));
#116727=CARTESIAN_POINT('Ctrl Pts',(5.50397918423974,-28.3581700086626,
124.717036437893));
#116728=CARTESIAN_POINT('Ctrl Pts',(5.50565525387928,-28.3539788256483,
124.742339822065));
#116729=CARTESIAN_POINT('Ctrl Pts',(5.50661517444864,-28.3517575830418,
124.756953850244));
#116730=CARTESIAN_POINT('Ctrl Pts',(5.51253201801181,-28.3391927720227,
124.847737316833));
#116731=CARTESIAN_POINT('Ctrl Pts',(5.51732909613142,-28.3339361594531,
124.924519595377));
#116732=CARTESIAN_POINT('Ctrl Pts',(5.52205821453768,-28.3340005850234,
125.001396172494));
#116733=CARTESIAN_POINT('Ctrl Pts',(5.52205812845195,-28.3340005838512,
125.001394773084));
#116734=CARTESIAN_POINT('Ctrl Pts',(5.53023876175647,-28.3341119182617,
125.134379173918));
#116735=CARTESIAN_POINT('Ctrl Pts',(5.538148581464,-28.3501451314225,125.266857640374));
#116736=CARTESIAN_POINT('Ctrl Pts',(5.54796471122472,-28.3863380832262,
125.414757645535));
#116737=CARTESIAN_POINT('Ctrl Pts',(5.5492230763142,-28.3912522236007,125.43342727207));
#116738=CARTESIAN_POINT('Ctrl Pts',(5.55104156984201,-28.3987189244339,
125.459915694842));
#116739=CARTESIAN_POINT('Ctrl Pts',(5.55158764660967,-28.401006898531,125.467808276731));
#116740=CARTESIAN_POINT('Ctrl Pts',(5.55254189612542,-28.4050819304441,
125.481486254538));
#116741=CARTESIAN_POINT('Ctrl Pts',(5.55294853914217,-28.4068422903595,
125.48727935804));
#116742=CARTESIAN_POINT('Ctrl Pts',(5.55382614207314,-28.4106916992212,
125.499703365874));
#116743=CARTESIAN_POINT('Ctrl Pts',(5.55429762856221,-28.412790651181,125.506330729269));
#116744=CARTESIAN_POINT('Ctrl Pts',(5.55560845564577,-28.4187128176287,
125.524631033915));
#116745=CARTESIAN_POINT('Ctrl Pts',(5.55645254851924,-28.4226236546171,
125.536274852816));
#116746=CARTESIAN_POINT('Ctrl Pts',(5.55798021472545,-28.4298810537396,
125.557116027919));
#116747=CARTESIAN_POINT('Ctrl Pts',(5.55866144585198,-28.433180286975,125.566328267133));
#116748=CARTESIAN_POINT('Ctrl Pts',(5.55934601859666,-28.436559980232,125.575509604253));
#116749=CARTESIAN_POINT('',(5.32851907197511,-28.3320235394521,125.000530942666));
#116750=CARTESIAN_POINT('Ctrl Pts',(5.3678724416903,-28.4365599837785,125.575509613888));
#116751=CARTESIAN_POINT('Ctrl Pts',(5.36380377119692,-28.41550826323,125.518320122137));
#116752=CARTESIAN_POINT('Ctrl Pts',(5.35973510070354,-28.3976158268008,
125.460021074581));
#116753=CARTESIAN_POINT('Ctrl Pts',(5.35566643021015,-28.3829781651687,
125.400994246441));
#116754=CARTESIAN_POINT('Ctrl Pts',(5.35159020293631,-28.3683133168683,
125.341857787211));
#116755=CARTESIAN_POINT('Ctrl Pts',(5.34751397566247,-28.3569154130502,
125.28199135154));
#116756=CARTESIAN_POINT('Ctrl Pts',(5.34343774838862,-28.348828605094,125.221785988385));
#116757=CARTESIAN_POINT('Ctrl Pts',(5.34045616567603,-28.3429134572912,
125.177748387455));
#116758=CARTESIAN_POINT('Ctrl Pts',(5.33747458296344,-28.3387687514707,
125.133529630053));
#116759=CARTESIAN_POINT('Ctrl Pts',(5.33449300025085,-28.3363941013021,
125.089282774473));
#116760=CARTESIAN_POINT('Ctrl Pts',(5.33250187903717,-28.3348082937691,
125.059734423387));
#116761=CARTESIAN_POINT('Ctrl Pts',(5.33051075782348,-28.3340096599776,
125.030143448947));
#116762=CARTESIAN_POINT('Ctrl Pts',(5.32851963660979,-28.3340000870979,
125.000538711647));
#116763=CARTESIAN_POINT('Ctrl Pts',(5.32851890483142,-28.3314384399868,
125.000528642885));
#116764=CARTESIAN_POINT('Ctrl Pts',(5.29346517969172,-28.3336501290359,
124.47853450853));
#116765=CARTESIAN_POINT('Ctrl Pts',(5.22136636427249,-28.8783523852238,
123.400922781091));
#116766=CARTESIAN_POINT('Ctrl Pts',(5.11222245857373,-30.7133320434846,
123.164583819203));
#116767=CARTESIAN_POINT('Ctrl Pts',(5.00108718773517,-31.9288987627743,
124.603837503091));
#116768=CARTESIAN_POINT('Ctrl Pts',(4.88995191689662,-31.3789987832528,
126.405687560155));
#116769=CARTESIAN_POINT('Ctrl Pts',(4.77886137730299,-29.5676694072103,
126.920744002413));
#116770=CARTESIAN_POINT('Ctrl Pts',(4.70481592798891,-28.6242856685622,
126.09333226611));
#116771=CARTESIAN_POINT('Ctrl Pts',(4.66781556895434,-28.4339562630661,
125.576468403481));
#116772=CARTESIAN_POINT('Origin',(5.,-30.,125.));
#116773=CARTESIAN_POINT('',(3.96713564162385,-28.4365599852621,125.575509617918));
#116774=CARTESIAN_POINT('',(4.16231116930939,-28.436559983762,125.575509613843));
#116775=CARTESIAN_POINT('',(5.,-28.4365599837785,125.575509613888));
#116776=CARTESIAN_POINT('Ctrl Pts',(4.16231116930939,-28.436559983762,125.575509613843));
#116777=CARTESIAN_POINT('Ctrl Pts',(4.16317922697514,-28.4409822920616,
125.587523338016));
#116778=CARTESIAN_POINT('Ctrl Pts',(4.16404268008447,-28.4455430622354,
125.599486059615));
#116779=CARTESIAN_POINT('Ctrl Pts',(4.16563891938588,-28.4542751614591,
125.621620092053));
#116780=CARTESIAN_POINT('Ctrl Pts',(4.16637286785923,-28.4584100737857,
125.631804815354));
#116781=CARTESIAN_POINT('Ctrl Pts',(4.16776485836637,-28.4664801403983,
125.651131226606));
#116782=CARTESIAN_POINT('Ctrl Pts',(4.16842348095199,-28.4703969876596,
125.660279990594));
#116783=CARTESIAN_POINT('Ctrl Pts',(4.17012589727787,-28.4807758879012,
125.683934389042));
#116784=CARTESIAN_POINT('Ctrl Pts',(4.17116536468675,-28.4873638687723,
125.698383930497));
#116785=CARTESIAN_POINT('Ctrl Pts',(4.17479569757736,-28.5112448409967,
125.748838663549));
#116786=CARTESIAN_POINT('Ctrl Pts',(4.17734928696242,-28.5296256928894,
125.784315662723));
#116787=CARTESIAN_POINT('Ctrl Pts',(4.18801181564254,-28.6127404528174,
125.931522928704));
#116788=CARTESIAN_POINT('Ctrl Pts',(4.195723419553,-28.6890648901925,126.036181896769));
#116789=CARTESIAN_POINT('Ctrl Pts',(4.20627235726083,-28.8049600963661,
126.161536737027));
#116790=CARTESIAN_POINT('Ctrl Pts',(4.20887139195282,-28.8343453468672,
126.19102339734));
#116791=CARTESIAN_POINT('Ctrl Pts',(4.21263383407759,-28.8774501499696,
126.231152502855));
#116792=CARTESIAN_POINT('Ctrl Pts',(4.21374791304859,-28.8902807566091,
126.242729979486));
#116793=CARTESIAN_POINT('Ctrl Pts',(4.21550022286791,-28.9105152726094,
126.260425004797));
#116794=CARTESIAN_POINT('Ctrl Pts',(4.21612984725988,-28.9177962573231,
126.266681970031));
#116795=CARTESIAN_POINT('Ctrl Pts',(4.21728735702848,-28.9311906267264,
126.277992735665));
#116796=CARTESIAN_POINT('Ctrl Pts',(4.21781389315024,-28.9372868591462,
126.283066515352));
#116797=CARTESIAN_POINT('Ctrl Pts',(4.21834735396957,-28.9434634153534,
126.288132931266));
#116798=CARTESIAN_POINT('Ctrl Pts',(4.21835119581947,-28.9435078973568,
126.288169414465));
#116799=CARTESIAN_POINT('Ctrl Pts',(4.21835894487734,-28.9435976181108,
126.288242993756));
#116800=CARTESIAN_POINT('Ctrl Pts',(4.21836285207824,-28.9436428567798,
126.288280089651));
#116801=CARTESIAN_POINT('Ctrl Pts',(4.21837073555032,-28.9437341338438,
126.288354929178));
#116802=CARTESIAN_POINT('Ctrl Pts',(4.21837471184787,-28.9437801725446,
126.28839267292));
#116803=CARTESIAN_POINT('Ctrl Pts',(4.21877605287532,-28.9484270132244,
126.292201859092));
#116804=CARTESIAN_POINT('Ctrl Pts',(4.21917515494819,-28.9530479165009,
126.295948581132));
#116805=CARTESIAN_POINT('Ctrl Pts',(4.22002521016993,-28.9628876238562,
126.303839840958));
#116806=CARTESIAN_POINT('Ctrl Pts',(4.22047658143271,-28.968111321352,126.307977890708));
#116807=CARTESIAN_POINT('Ctrl Pts',(4.22169796302618,-28.982247085991,126.31903841948));
#116808=CARTESIAN_POINT('Ctrl Pts',(4.2224718624188,-28.9912047083257,126.325901726405));
#116809=CARTESIAN_POINT('Ctrl Pts',(4.22624720919268,-29.0349388505564,
126.35871099675));
#116810=CARTESIAN_POINT('Ctrl Pts',(4.22932004107227,-29.0706475086381,
126.38338058524));
#116811=CARTESIAN_POINT('Ctrl Pts',(4.23881210239701,-29.1823387683896,
126.45426624988));
#116812=CARTESIAN_POINT('Ctrl Pts',(4.24533677897331,-29.2610949036596,
126.495820653806));
#116813=CARTESIAN_POINT('Ctrl Pts',(4.256183647702,-29.3988872592886,126.554974692873));
#116814=CARTESIAN_POINT('Ctrl Pts',(4.26054976332195,-29.4562698463316,
126.575957365829));
#116815=CARTESIAN_POINT('Ctrl Pts',(4.26758220213828,-29.5523386448093,
126.605211824967));
#116816=CARTESIAN_POINT('Ctrl Pts',(4.27029977497475,-29.590394516047,126.615341910125));
#116817=CARTESIAN_POINT('Ctrl Pts',(4.27401811929543,-29.6437505532854,
126.627537486277));
#116818=CARTESIAN_POINT('Ctrl Pts',(4.27505502323509,-29.6587716727772,
126.630752952986));
#116819=CARTESIAN_POINT('Ctrl Pts',(4.27682040968263,-29.6845832739236,
126.635905989399));
#116820=CARTESIAN_POINT('Ctrl Pts',(4.27755209498397,-29.6953521120446,
126.637945600897));
#116821=CARTESIAN_POINT('Ctrl Pts',(4.27894388251059,-29.7159680330845,
126.641639888374));
#116822=CARTESIAN_POINT('Ctrl Pts',(4.27960452739117,-29.7258113555464,
126.643312592277));
#116823=CARTESIAN_POINT('Ctrl Pts',(4.28132105893931,-29.7515320906149,
126.647445848561));
#116824=CARTESIAN_POINT('Ctrl Pts',(4.28237247059705,-29.7674313551585,
126.649765432095));
#116825=CARTESIAN_POINT('Ctrl Pts',(4.28609523790505,-29.8242076784766,
126.657211547177));
#116826=CARTESIAN_POINT('Ctrl Pts',(4.2887266612414,-29.8652401110334,126.661051851689));
#116827=CARTESIAN_POINT('Ctrl Pts',(4.29936671143038,-30.0338614361575,
126.670542892513));
#116828=CARTESIAN_POINT('Ctrl Pts',(4.30699527934091,-30.1617439648984,
126.663039006415));
#116829=CARTESIAN_POINT('Ctrl Pts',(4.31744725702816,-30.3283331185741,
126.633851479204));
#116830=CARTESIAN_POINT('Ctrl Pts',(4.32003570993169,-30.3688679108526,
126.625179775387));
#116831=CARTESIAN_POINT('Ctrl Pts',(4.32429611365685,-30.4335076314715,
126.608808407346));
#116832=CARTESIAN_POINT('Ctrl Pts',(4.32593049324473,-30.4578352375551,
126.602054958244));
#116833=CARTESIAN_POINT('Ctrl Pts',(4.32819351345414,-30.4907138987437,
126.592117699225));
#116834=CARTESIAN_POINT('Ctrl Pts',(4.32879709762664,-30.4994074009803,
126.589412198611));
#116835=CARTESIAN_POINT('Ctrl Pts',(4.32981849029757,-30.5139821578055,
126.584745018771));
#116836=CARTESIAN_POINT('Ctrl Pts',(4.33023412369842,-30.5198755954111,
126.582821467148));
#116837=CARTESIAN_POINT('Ctrl Pts',(4.33109424879399,-30.5319913820317,
126.578792044713));
#116838=CARTESIAN_POINT('Ctrl Pts',(4.33153894578492,-30.5382121919578,
126.576682207571));
#116839=CARTESIAN_POINT('Ctrl Pts',(4.33272350719992,-30.5546730627074,
126.570990605243));
#116840=CARTESIAN_POINT('Ctrl Pts',(4.33346688174507,-30.5648906928265,
126.567345583404));
#116841=CARTESIAN_POINT('Ctrl Pts',(4.33685771742829,-30.6110233497129,
126.550378607468));
#116842=CARTESIAN_POINT('Ctrl Pts',(4.33956077585401,-30.6465053273742,
126.535921129286));
#116843=CARTESIAN_POINT('Ctrl Pts',(4.34892012649131,-30.765969748107,126.482371208142));
#116844=CARTESIAN_POINT('Ctrl Pts',(4.35572099626238,-30.8471770134883,
126.437506458466));
#116845=CARTESIAN_POINT('Ctrl Pts',(4.36694606887245,-30.9761988225833,
126.35147796924));
#116846=CARTESIAN_POINT('Ctrl Pts',(4.37141715323246,-31.0261779801031,
126.313931864512));
#116847=CARTESIAN_POINT('Ctrl Pts',(4.37859384109451,-31.1044841786287,
126.247905241694));
#116848=CARTESIAN_POINT('Ctrl Pts',(4.3813534991082,-31.1340990713949,126.22105387124));
#116849=CARTESIAN_POINT('Ctrl Pts',(4.38511849018135,-31.1737824707877,
126.182382858021));
#116850=CARTESIAN_POINT('Ctrl Pts',(4.3861611731732,-31.1846929800073,126.17145084519));
#116851=CARTESIAN_POINT('Ctrl Pts',(4.3879333567846,-31.2030942913225,126.152493200084));
#116852=CARTESIAN_POINT('Ctrl Pts',(4.38866612261558,-31.210660505082,126.14454252932));
#116853=CARTESIAN_POINT('Ctrl Pts',(4.39014604037217,-31.2258517883746,
126.128260133651));
#116854=CARTESIAN_POINT('Ctrl Pts',(4.39089295493148,-31.2334718142169,
126.119924475314));
#116855=CARTESIAN_POINT('Ctrl Pts',(4.39275988297913,-31.2523942840735,
126.098797474278));
#116856=CARTESIAN_POINT('Ctrl Pts',(4.39387526280677,-31.263586180322,126.085908528559));
#116857=CARTESIAN_POINT('Ctrl Pts',(4.39817085703018,-31.3062127915342,
126.035266794887));
#116858=CARTESIAN_POINT('Ctrl Pts',(4.4012921114574,-31.3361714257897,125.996301061924));
#116859=CARTESIAN_POINT('Ctrl Pts',(4.41182898467989,-31.4327874951286,
125.858423723178));
#116860=CARTESIAN_POINT('Ctrl Pts',(4.41896233633882,-31.4905269490875,
125.753724112213));
#116861=CARTESIAN_POINT('Ctrl Pts',(4.42883229370567,-31.5521821057682,
125.60655874918));
#116862=CARTESIAN_POINT('Ctrl Pts',(4.43135439936957,-31.5664103778371,
125.568806563515));
#116863=CARTESIAN_POINT('Ctrl Pts',(4.4355175105843,-31.587148284961,125.507080634077));
#116864=CARTESIAN_POINT('Ctrl Pts',(4.43712303788963,-31.5945167435998,
125.483411466825));
#116865=CARTESIAN_POINT('Ctrl Pts',(4.43935225454763,-31.6038486740857,
125.450896007729));
#116866=CARTESIAN_POINT('Ctrl Pts',(4.43995184251413,-31.6062724715152,
125.442183804796));
#116867=CARTESIAN_POINT('Ctrl Pts',(4.440968454533,-31.6102350609335,125.427477878964));
#116868=CARTESIAN_POINT('Ctrl Pts',(4.44138335021321,-31.6118116473372,
125.421494365992));
#116869=CARTESIAN_POINT('Ctrl Pts',(4.44218897272962,-31.614793987893,125.409914227204));
#116870=CARTESIAN_POINT('Ctrl Pts',(4.44257941218681,-31.616204051675,125.404318881318));
#116871=CARTESIAN_POINT('Ctrl Pts',(4.44365744131983,-31.6200014388658,
125.388912953585));
#116872=CARTESIAN_POINT('Ctrl Pts',(4.44434829230354,-31.6223286389151,
125.37908801357));
#116873=CARTESIAN_POINT('Ctrl Pts',(4.44717123920904,-31.6314148973058,
125.339110990885));
#116874=CARTESIAN_POINT('Ctrl Pts',(4.44933922696244,-31.6374233377766,
125.308796627838));
#116875=CARTESIAN_POINT('Ctrl Pts',(4.45929174660197,-31.6608311006076,
125.170656546464));
#116876=CARTESIAN_POINT('Ctrl Pts',(4.46733985017474,-31.6684446471276,
125.061447481425));
#116877=CARTESIAN_POINT('Ctrl Pts',(4.47938274580057,-31.6636667543472,
124.894710334348));
#116878=CARTESIAN_POINT('Ctrl Pts',(4.48349201426374,-31.6590328438972,
124.837260600529));
#116879=CARTESIAN_POINT('Ctrl Pts',(4.49016815258423,-31.6464347523035,
124.742623473705));
#116880=CARTESIAN_POINT('Ctrl Pts',(4.49277972340893,-31.6401589568326,
124.705264414348));
#116881=CARTESIAN_POINT('Ctrl Pts',(4.49638011527232,-31.6295981471039,
124.653308163883));
#116882=CARTESIAN_POINT('Ctrl Pts',(4.49740208683874,-31.6263792444703,
124.63850874182));
#116883=CARTESIAN_POINT('Ctrl Pts',(4.4991499583045,-31.6204924376931,124.613115603815));
#116884=CARTESIAN_POINT('Ctrl Pts',(4.49987890092369,-31.6179213734383,
124.602500671963));
#116885=CARTESIAN_POINT('Ctrl Pts',(4.50127073123814,-31.6127897165635,
124.582189171061));
#116886=CARTESIAN_POINT('Ctrl Pts',(4.50193411319018,-31.6102455989487,
124.572488974244));
#116887=CARTESIAN_POINT('Ctrl Pts',(4.50366943743377,-31.6033327614527,
124.54706929583));
#116888=CARTESIAN_POINT('Ctrl Pts',(4.50473670485607,-31.5988203827969,
124.531389734225));
#116889=CARTESIAN_POINT('Ctrl Pts',(4.50858671764909,-31.5816002536884,
124.474700316751));
#116890=CARTESIAN_POINT('Ctrl Pts',(4.51132569969776,-31.5675383663796,
124.434117441358));
#116891=CARTESIAN_POINT('Ctrl Pts',(4.5212560676488,-31.5101261917827,124.287059710301));
#116892=CARTESIAN_POINT('Ctrl Pts',(4.52816221625505,-31.4573642478251,
124.184613529117));
#116893=CARTESIAN_POINT('Ctrl Pts',(4.53820516738287,-31.3680019493107,
124.04791406236));
#116894=CARTESIAN_POINT('Ctrl Pts',(4.54120798632575,-31.3397779754479,
124.008591256163));
#116895=CARTESIAN_POINT('Ctrl Pts',(4.54549759964524,-31.2981416882681,
123.955612451002));
#116896=CARTESIAN_POINT('Ctrl Pts',(4.54671908262832,-31.2861438318098,
123.940872446406));
#116897=CARTESIAN_POINT('Ctrl Pts',(4.54888866438222,-31.2646505962483,
123.915370696626));
#116898=CARTESIAN_POINT('Ctrl Pts',(4.54983032932422,-31.2552632263514,
123.904520171332));
#116899=CARTESIAN_POINT('Ctrl Pts',(4.55126631461466,-31.2408844249614,
123.888327719142));
#116900=CARTESIAN_POINT('Ctrl Pts',(4.55175345507476,-31.2359957700664,
123.882894871786));
#116901=CARTESIAN_POINT('Ctrl Pts',(4.55264595044027,-31.2270234779623,
123.873054800333));
#116902=CARTESIAN_POINT('Ctrl Pts',(4.55305044705163,-31.2229515390824,
123.868637269474));
#116903=CARTESIAN_POINT('Ctrl Pts',(4.55397754462481,-31.2136061141802,
123.858608087518));
#116904=CARTESIAN_POINT('Ctrl Pts',(4.55450125068896,-31.2083175786257,
123.853010932244));
#116905=CARTESIAN_POINT('Ctrl Pts',(4.55614692958504,-31.1916639969083,
123.835628506113));
#116906=CARTESIAN_POINT('Ctrl Pts',(4.55727832479877,-31.1801642913592,
123.823974382642));
#116907=CARTESIAN_POINT('Ctrl Pts',(4.56383934253566,-31.1130903657118,
123.75797434218));
#116908=CARTESIAN_POINT('Ctrl Pts',(4.56947347362756,-31.0539431093971,
123.707405895845));
#116909=CARTESIAN_POINT('Ctrl Pts',(4.57996511771871,-30.9380733036565,
123.621597831199));
#116910=CARTESIAN_POINT('Ctrl Pts',(4.5848085495672,-30.8823353489816,123.585270636609));
#116911=CARTESIAN_POINT('Ctrl Pts',(4.59481078997831,-30.7611922637512,
123.516267214959));
#116912=CARTESIAN_POINT('Ctrl Pts',(4.59994275309543,-30.6955010452258,
123.484362325228));
#116913=CARTESIAN_POINT('Ctrl Pts',(4.60620255939373,-30.6106485002079,
123.449834800201));
#116914=CARTESIAN_POINT('Ctrl Pts',(4.60746712552473,-30.5932586344661,
123.443096669935));
#116915=CARTESIAN_POINT('Ctrl Pts',(4.60950411867562,-30.5648509195995,
123.432634517634));
#116916=CARTESIAN_POINT('Ctrl Pts',(4.61028243792012,-30.5539011922207,
123.428731532237));
#116917=CARTESIAN_POINT('Ctrl Pts',(4.61177693114594,-30.5326957796855,
123.421422171251));
#116918=CARTESIAN_POINT('Ctrl Pts',(4.61249358342784,-30.5224460773789,
123.418000360077));
#116919=CARTESIAN_POINT('Ctrl Pts',(4.61414356097127,-30.4986649796156,
123.410317494367));
#116920=CARTESIAN_POINT('Ctrl Pts',(4.61507447354788,-30.485110879281,123.406129024676));
#116921=CARTESIAN_POINT('Ctrl Pts',(4.61804825830917,-30.441391910178,123.393228420271));
#116922=CARTESIAN_POINT('Ctrl Pts',(4.62006929800454,-30.4110326720846,
123.385195345504));
#116923=CARTESIAN_POINT('Ctrl Pts',(4.63094836414409,-30.2445843243034,
123.346151952231));
#116924=CARTESIAN_POINT('Ctrl Pts',(4.63927417250506,-30.1052460073446,
123.331480130998));
#116925=CARTESIAN_POINT('Ctrl Pts',(4.65053548342524,-29.9228527188195,
123.335235272053));
#116926=CARTESIAN_POINT('Ctrl Pts',(4.65320915825484,-29.8800508211849,
123.337771073136));
#116927=CARTESIAN_POINT('Ctrl Pts',(4.65759399957326,-29.8116959010801,
123.344474558685));
#116928=CARTESIAN_POINT('Ctrl Pts',(4.6592648233259,-29.7860581394499,123.347592173183));
#116929=CARTESIAN_POINT('Ctrl Pts',(4.66157047847722,-29.7514188744154,
123.352623988826));
#116930=CARTESIAN_POINT('Ctrl Pts',(4.66217902060251,-29.7423441578602,
123.35401890788));
#116931=CARTESIAN_POINT('Ctrl Pts',(4.66320636170562,-29.72714768124,123.356483578421));
#116932=CARTESIAN_POINT('Ctrl Pts',(4.66362292730653,-29.7210193634386,
123.357512734094));
#116933=CARTESIAN_POINT('Ctrl Pts',(4.66448229276276,-29.7084490508006,
123.359696103062));
#116934=CARTESIAN_POINT('Ctrl Pts',(4.66492527469808,-29.702007901545,123.360854022418));
#116935=CARTESIAN_POINT('Ctrl Pts',(4.66610039206937,-29.685018117183,123.364011709505));
#116936=CARTESIAN_POINT('Ctrl Pts',(4.6668359428259,-29.6744819062216,123.366075513184));
#116937=CARTESIAN_POINT('Ctrl Pts',(4.67013111700079,-29.6276841847637,
123.375712714981));
#116938=CARTESIAN_POINT('Ctrl Pts',(4.67274268786714,-29.5916638930089,
123.384391937964));
#116939=CARTESIAN_POINT('Ctrl Pts',(4.68206712786217,-29.4658281804642,
123.419189261915));
#116940=CARTESIAN_POINT('Ctrl Pts',(4.68893509065443,-29.3779514092269,
123.45165984287));
#116941=CARTESIAN_POINT('Ctrl Pts',(4.70025433355752,-29.2363703406212,
123.517983458252));
#116942=CARTESIAN_POINT('Ctrl Pts',(4.70475305418314,-29.1810247568318,
123.547834649225));
#116943=CARTESIAN_POINT('Ctrl Pts',(4.71196759048416,-29.0933198112044,
123.601752450571));
#116944=CARTESIAN_POINT('Ctrl Pts',(4.71473821155468,-29.0599141254374,
123.623989754725));
#116945=CARTESIAN_POINT('Ctrl Pts',(4.7185153371643,-29.0147853061878,123.656442340097));
#116946=CARTESIAN_POINT('Ctrl Pts',(4.71955951191594,-29.0023552929254,
123.665646132072));
#116947=CARTESIAN_POINT('Ctrl Pts',(4.72133345166069,-28.981323282175,123.681677474529));
#116948=CARTESIAN_POINT('Ctrl Pts',(4.72206649802086,-28.9726575237358,
123.688419280786));
#116949=CARTESIAN_POINT('Ctrl Pts',(4.72354633329308,-28.9552188643451,
123.702265132343));
#116950=CARTESIAN_POINT('Ctrl Pts',(4.72429289088067,-28.9464502473169,
123.709373664694));
#116951=CARTESIAN_POINT('Ctrl Pts',(4.72615767511359,-28.9246267143451,
123.727436176202));
#116952=CARTESIAN_POINT('Ctrl Pts',(4.7272712908582,-28.9116661605151,123.73850252555));
#116953=CARTESIAN_POINT('Ctrl Pts',(4.73154804558759,-28.8622119478054,
123.782058502115));
#116954=CARTESIAN_POINT('Ctrl Pts',(4.73465292780016,-28.826982656787,123.815950111589));
#116955=CARTESIAN_POINT('Ctrl Pts',(4.74606647368828,-28.7012718377728,
123.948014299602));
#116956=CARTESIAN_POINT('Ctrl Pts',(4.75399658311775,-28.6212084871078,
124.055383808113));
#116957=CARTESIAN_POINT('Ctrl Pts',(4.76430153766584,-28.5390722115101,
124.198596740525));
#116958=CARTESIAN_POINT('Ctrl Pts',(4.76629905873587,-28.5241163033265,
124.226485770754));
#116959=CARTESIAN_POINT('Ctrl Pts',(4.76967922578871,-28.5006015582395,
124.273502622169));
#116960=CARTESIAN_POINT('Ctrl Pts',(4.77104089798658,-28.4915928572346,
124.292397059673));
#116961=CARTESIAN_POINT('Ctrl Pts',(4.7729824502807,-28.4794381113972,124.319177365008));
#116962=CARTESIAN_POINT('Ctrl Pts',(4.77354556525418,-28.4759923298395,
124.326926058278));
#116963=CARTESIAN_POINT('Ctrl Pts',(4.77451926779054,-28.470173387285,124.340285182138));
#116964=CARTESIAN_POINT('Ctrl Pts',(4.77492813381232,-28.4677715825235,
124.345882899312));
#116965=CARTESIAN_POINT('Ctrl Pts',(4.77579853489,-28.4627475079176,124.357771672162));
#116966=CARTESIAN_POINT('Ctrl Pts',(4.77626048300065,-28.4601331616044,
124.364065596676));
#116967=CARTESIAN_POINT('Ctrl Pts',(4.77754063810094,-28.4530291819928,
124.38146878718));
#116968=CARTESIAN_POINT('Ctrl Pts',(4.77836337070612,-28.4486207721539,
124.392610467891));
#116969=CARTESIAN_POINT('Ctrl Pts',(4.78298345315674,-28.4247140732948,
124.454990131926));
#116970=CARTESIAN_POINT('Ctrl Pts',(4.78689457477958,-28.4076357984436,
124.507114096948));
#116971=CARTESIAN_POINT('Ctrl Pts',(4.80156354832864,-28.3539853336534,
124.703031438508));
#116972=CARTESIAN_POINT('Ctrl Pts',(4.81248202844361,-28.3340822986218,
124.850709193547));
#116973=CARTESIAN_POINT('Ctrl Pts',(4.82498050555705,-28.3339828214303,
125.030605074958));
#116974=CARTESIAN_POINT('Ctrl Pts',(4.82714463543918,-28.3348602620568,
125.062127258076));
#116975=CARTESIAN_POINT('Ctrl Pts',(4.83022909206343,-28.3374177715957,
125.10757319661));
#116976=CARTESIAN_POINT('Ctrl Pts',(4.83117144314779,-28.3383795779757,
125.121528814164));
#116977=CARTESIAN_POINT('Ctrl Pts',(4.83282998096261,-28.3403932604248,
125.14621073381));
#116978=CARTESIAN_POINT('Ctrl Pts',(4.83354835881832,-28.3413736517119,
125.156941883741));
#116979=CARTESIAN_POINT('Ctrl Pts',(4.83504069871296,-28.3436366818982,
125.179314545688));
#116980=CARTESIAN_POINT('Ctrl Pts',(4.83581403054194,-28.3449381027186,
125.190953595979));
#116981=CARTESIAN_POINT('Ctrl Pts',(4.83783589563745,-28.348679511804,125.221494568576));
#116982=CARTESIAN_POINT('Ctrl Pts',(4.83907805904064,-28.3513213373572,
125.240370369404));
#116983=CARTESIAN_POINT('Ctrl Pts',(4.84549040007951,-28.3667454337356,
125.338302097014));
#116984=CARTESIAN_POINT('Ctrl Pts',(4.85048818984653,-28.3848922241868,
125.416410867518));
#116985=CARTESIAN_POINT('Ctrl Pts',(4.8572016034264,-28.4171923328068,125.520693063046));
#116986=CARTESIAN_POINT('Ctrl Pts',(4.85897938281318,-28.4265191394924,
125.548232470602));
#116987=CARTESIAN_POINT('Ctrl Pts',(4.86075486118656,-28.4365599784656,
125.575509599455));
#116988=CARTESIAN_POINT('',(4.62852042919292,-28.3357497203589,125.001193953836));
#116989=CARTESIAN_POINT('Ctrl Pts',(4.66781556895434,-28.4339562630661,
125.576468403481));
#116990=CARTESIAN_POINT('Ctrl Pts',(4.66777083770939,-28.4337261660757,
125.575843545651));
#116991=CARTESIAN_POINT('Ctrl Pts',(4.65467245778892,-28.3664685496906,
125.392825950738));
#116992=CARTESIAN_POINT('Ctrl Pts',(4.64157407786846,-28.334468402925,125.196877811068));
#116993=CARTESIAN_POINT('Ctrl Pts',(4.62852042919292,-28.3357497203589,
125.001193953836));
#116994=CARTESIAN_POINT('Ctrl Pts',(4.6275136190416,-28.3340004723798,125.00125457927));
#116995=CARTESIAN_POINT('Ctrl Pts',(4.6239375618158,-28.3339624568575,124.950772442624));
#116996=CARTESIAN_POINT('Ctrl Pts',(4.62041976511974,-28.3362189480784,
124.900309774701));
#116997=CARTESIAN_POINT('Ctrl Pts',(4.61604554105104,-28.3419851644348,
124.836517043977));
#116998=CARTESIAN_POINT('Ctrl Pts',(4.61512462459214,-28.3433707318118,
124.823027237963));
#116999=CARTESIAN_POINT('Ctrl Pts',(4.61350377315945,-28.3461143487295,
124.799183530003));
#117000=CARTESIAN_POINT('Ctrl Pts',(4.61280178313282,-28.3474053112998,
124.788822809959));
#117001=CARTESIAN_POINT('Ctrl Pts',(4.61141212000764,-28.3501656184413,
124.768248018594));
#117002=CARTESIAN_POINT('Ctrl Pts',(4.61072440635864,-28.3516326308489,
124.758034109817));
#117003=CARTESIAN_POINT('Ctrl Pts',(4.60926076993725,-28.3549710616375,
124.736231993051));
#117004=CARTESIAN_POINT('Ctrl Pts',(4.60848576349747,-28.3568702538317,
124.724648554252));
#117005=CARTESIAN_POINT('Ctrl Pts',(4.60645344662114,-28.36219723033,124.694178998796));
#117006=CARTESIAN_POINT('Ctrl Pts',(4.60520263348851,-28.3658293058874,
124.675330030457));
#117007=CARTESIAN_POINT('Ctrl Pts',(4.59880832819561,-28.3862140855227,
124.578572740266));
#117008=CARTESIAN_POINT('Ctrl Pts',(4.59383504404583,-28.408215857731,124.501872029714));
#117009=CARTESIAN_POINT('Ctrl Pts',(4.58390751218169,-28.4637340275011,
124.350290617888));
#117010=CARTESIAN_POINT('Ctrl Pts',(4.57896992556178,-28.4974497369693,
124.275722699557));
#117011=CARTESIAN_POINT('Ctrl Pts',(4.57132676090821,-28.5565738161393,
124.16702842421));
#117012=CARTESIAN_POINT('Ctrl Pts',(4.56870420584042,-28.5780346285061,
124.130900001632));
#117013=CARTESIAN_POINT('Ctrl Pts',(4.5643940250378,-28.6146663041366,124.074227001829));
#117014=CARTESIAN_POINT('Ctrl Pts',(4.56274507237488,-28.6289845852772,
124.053151724226));
#117015=CARTESIAN_POINT('Ctrl Pts',(4.56046510581799,-28.64908431832,124.024978846363));
#117016=CARTESIAN_POINT('Ctrl Pts',(4.55985963947971,-28.6544500766305,
124.017587243912));
#117017=CARTESIAN_POINT('Ctrl Pts',(4.5588360844876,-28.6635617174338,124.005250181324));
#117018=CARTESIAN_POINT('Ctrl Pts',(4.55842019385935,-28.6672750409911,
124.000280705919));
#117019=CARTESIAN_POINT('Ctrl Pts',(4.55756067966869,-28.6749697654381,
123.990102053023));
#117020=CARTESIAN_POINT('Ctrl Pts',(4.55711686081514,-28.6789542769691,
123.984895483346));
#117021=CARTESIAN_POINT('Ctrl Pts',(4.55593674459495,-28.6895814628421,
123.971177455592));
#117022=CARTESIAN_POINT('Ctrl Pts',(4.55519698022075,-28.6962761955396,
123.962706986091));
#117023=CARTESIAN_POINT('Ctrl Pts',(4.55184909975054,-28.7267413816829,
123.924921924913));
#117024=CARTESIAN_POINT('Ctrl Pts',(4.54918703129522,-28.7514197832095,
123.896357244628));
#117025=CARTESIAN_POINT('Ctrl Pts',(4.53895755579082,-28.8486307895759,
123.791274337358));
#117026=CARTESIAN_POINT('Ctrl Pts',(4.53119518671602,-28.9273993093324,
123.720860840384));
#117027=CARTESIAN_POINT('Ctrl Pts',(4.51964436242677,-29.0564608674606,
123.625846490869));
#117028=CARTESIAN_POINT('Ctrl Pts',(4.51573892437174,-29.1022096527089,
123.595529483357));
#117029=CARTESIAN_POINT('Ctrl Pts',(4.51016015832971,-29.1708887879186,
123.554746849849));
#117030=CARTESIAN_POINT('Ctrl Pts',(4.50842844620163,-29.1926889401731,
123.542457192206));
#117031=CARTESIAN_POINT('Ctrl Pts',(4.50530900082085,-29.2328371772173,
123.521001224076));
#117032=CARTESIAN_POINT('Ctrl Pts',(4.50391594985222,-29.2510930955652,
123.511673863228));
#117033=CARTESIAN_POINT('Ctrl Pts',(4.50172506914042,-29.2803151867611,
123.497417517666));
#117034=CARTESIAN_POINT('Ctrl Pts',(4.5009195965488,-29.2911700440651,123.492266451494));
#117035=CARTESIAN_POINT('Ctrl Pts',(4.49940458149445,-29.3117939833515,
123.482751527787));
#117036=CARTESIAN_POINT('Ctrl Pts',(4.4986942368313,-29.3215511712721,123.478363498172));
#117037=CARTESIAN_POINT('Ctrl Pts',(4.49708623948698,-29.3438326293942,
123.468599950394));
#117038=CARTESIAN_POINT('Ctrl Pts',(4.49619063022583,-29.3563820535877,
123.463283471956));
#117039=CARTESIAN_POINT('Ctrl Pts',(4.49385910617347,-29.3894036755574,
123.449769574818));
#117040=CARTESIAN_POINT('Ctrl Pts',(4.4924315720158,-29.4099762526942,123.441823407701));
#117041=CARTESIAN_POINT('Ctrl Pts',(4.48374083056788,-29.5372268509231,
123.395554627666));
#117042=CARTESIAN_POINT('Ctrl Pts',(4.47683512781077,-29.6474296374407,
123.367792400218));
#117043=CARTESIAN_POINT('Ctrl Pts',(4.46400861349008,-29.85525008001,123.337488221073));
#117044=CARTESIAN_POINT('Ctrl Pts',(4.45810741105641,-29.951911980061,123.331893169279));
#117045=CARTESIAN_POINT('Ctrl Pts',(4.45088911827662,-30.0628214707039,
123.335123191926));
#117046=CARTESIAN_POINT('Ctrl Pts',(4.44994864637216,-30.0771379380591,
123.335725074394));
#117047=CARTESIAN_POINT('Ctrl Pts',(4.44851420767756,-30.0987368028933,
123.3369123939));
#117048=CARTESIAN_POINT('Ctrl Pts',(4.44802739989435,-30.1060264536135,
123.337361215442));
#117049=CARTESIAN_POINT('Ctrl Pts',(4.44713535547297,-30.1193052726517,
123.338266468655));
#117050=CARTESIAN_POINT('Ctrl Pts',(4.44673097448782,-30.1252952329037,
123.338707377272));
#117051=CARTESIAN_POINT('Ctrl Pts',(4.44580395327426,-30.1389598320813,
123.339787522105));
#117052=CARTESIAN_POINT('Ctrl Pts',(4.44528020639347,-30.1466324788901,
123.34044758536));
#117053=CARTESIAN_POINT('Ctrl Pts',(4.44363375921617,-30.1706126452903,
123.342678146121));
#117054=CARTESIAN_POINT('Ctrl Pts',(4.44250162191485,-30.1869011910927,
123.34443595813));
#117055=CARTESIAN_POINT('Ctrl Pts',(4.43589087854303,-30.28100575181,123.355997827549));
#117056=CARTESIAN_POINT('Ctrl Pts',(4.43020408697857,-30.3580713563141,
123.371046365756));
#117057=CARTESIAN_POINT('Ctrl Pts',(4.41966015512029,-30.4979667454167,
123.408772692479));
#117058=CARTESIAN_POINT('Ctrl Pts',(4.41481697701063,-30.5610605802085,
123.429908587048));
#117059=CARTESIAN_POINT('Ctrl Pts',(4.40659821662898,-30.6673515701857,
123.472743352658));
#117060=CARTESIAN_POINT('Ctrl Pts',(4.40318977590103,-30.7111813621061,
123.492653737976));
#117061=CARTESIAN_POINT('Ctrl Pts',(4.39751122011841,-30.783914391932,123.529573928426));
#117062=CARTESIAN_POINT('Ctrl Pts',(4.39521199812144,-30.8132767202812,
123.545608079141));
#117063=CARTESIAN_POINT('Ctrl Pts',(4.39196337816406,-30.8546124657938,
123.569824296462));
#117064=CARTESIAN_POINT('Ctrl Pts',(4.39098890782616,-30.8669912957543,
123.577294434659));
#117065=CARTESIAN_POINT('Ctrl Pts',(4.38929635097504,-30.888450015477,123.590628034534));
#117066=CARTESIAN_POINT('Ctrl Pts',(4.38857571876595,-30.8975728427396,
123.596420373301));
#117067=CARTESIAN_POINT('Ctrl Pts',(4.38708763826762,-30.9163789119354,
123.608619219607));
#117068=CARTESIAN_POINT('Ctrl Pts',(4.38632073511994,-30.9260528612506,
123.615039027277));
#117069=CARTESIAN_POINT('Ctrl Pts',(4.38433539213345,-30.9510419395565,
123.632001137973));
#117070=CARTESIAN_POINT('Ctrl Pts',(4.38312289914863,-30.9662493708966,
123.642699791613));
#117071=CARTESIAN_POINT('Ctrl Pts',(4.37775649630183,-31.0332488655607,
123.691531809118));
#117072=CARTESIAN_POINT('Ctrl Pts',(4.37370870515379,-31.0829891046085,
123.732392722253));
#117073=CARTESIAN_POINT('Ctrl Pts',(4.36078349152526,-31.2362894563955,
123.873954533147));
#117074=CARTESIAN_POINT('Ctrl Pts',(4.35225951593735,-31.329141929386,123.985228350538));
#117075=CARTESIAN_POINT('Ctrl Pts',(4.34155843054311,-31.4185612684161,
124.126073541137));
#117076=CARTESIAN_POINT('Ctrl Pts',(4.34009559672282,-31.430248340487,124.145334514263));
#117077=CARTESIAN_POINT('Ctrl Pts',(4.33803436412337,-31.4459127944192,
124.172371908705));
#117078=CARTESIAN_POINT('Ctrl Pts',(4.33745561601757,-31.4502255397583,
124.179952475699));
#117079=CARTESIAN_POINT('Ctrl Pts',(4.33646380079489,-31.4574671518285,
124.192916941977));
#117080=CARTESIAN_POINT('Ctrl Pts',(4.33605262262066,-31.4604262612337,
124.198283905885));
#117081=CARTESIAN_POINT('Ctrl Pts',(4.33518750371661,-31.4665608975553,
124.209557023808));
#117082=CARTESIAN_POINT('Ctrl Pts',(4.33473323193015,-31.4697304457395,
124.215466139844));
#117083=CARTESIAN_POINT('Ctrl Pts',(4.33349540021967,-31.4782297501892,
124.231544005287));
#117084=CARTESIAN_POINT('Ctrl Pts',(4.33270777533694,-31.4834900892777,
124.241748757439));
#117085=CARTESIAN_POINT('Ctrl Pts',(4.32870343820016,-31.5095142975284,
124.293541722267));
#117086=CARTESIAN_POINT('Ctrl Pts',(4.32540472585382,-31.5286348485165,
124.33592818055));
#117087=CARTESIAN_POINT('Ctrl Pts',(4.32117889486761,-31.5505428244502,
124.390472023849));
#117088=CARTESIAN_POINT('Ctrl Pts',(4.32029137841869,-31.5550022663463,
124.401940348357));
#117089=CARTESIAN_POINT('Ctrl Pts',(4.31119280338278,-31.5993052171702,
124.519720439028));
#117090=CARTESIAN_POINT('Ctrl Pts',(4.30285176938574,-31.628313544663,124.629804183977));
#117091=CARTESIAN_POINT('Ctrl Pts',(4.29083621630954,-31.6545315070307,
124.797051188914));
#117092=CARTESIAN_POINT('Ctrl Pts',(4.28695000220397,-31.660395617532,124.852520020277));
#117093=CARTESIAN_POINT('Ctrl Pts',(4.28197072407766,-31.6644205951122,
124.92544241941));
#117094=CARTESIAN_POINT('Ctrl Pts',(4.28080065422388,-31.6651045619957,
124.942714862513));
#117095=CARTESIAN_POINT('Ctrl Pts',(4.27887713041502,-31.6657918151533,
124.971327414729));
#117096=CARTESIAN_POINT('Ctrl Pts',(4.27811895961906,-31.6659483480288,
124.982662144019));
#117097=CARTESIAN_POINT('Ctrl Pts',(4.27664430148294,-31.6660281607841,
125.004815346992));
#117098=CARTESIAN_POINT('Ctrl Pts',(4.27592752877229,-31.6659617740972,
125.015633192928));
#117099=CARTESIAN_POINT('Ctrl Pts',(4.274212422453,-31.6655489446354,125.041632860686));
#117100=CARTESIAN_POINT('Ctrl Pts',(4.27321731690479,-31.665100289338,125.056812266337));
#117101=CARTESIAN_POINT('Ctrl Pts',(4.26992389061443,-31.6629151975043,
125.107336985913));
#117102=CARTESIAN_POINT('Ctrl Pts',(4.26765394037276,-31.660260202349,125.142634234797));
#117103=CARTESIAN_POINT('Ctrl Pts',(4.25594730946091,-31.6405356194274,
125.326376338418));
#117104=CARTESIAN_POINT('Ctrl Pts',(4.24710776268307,-31.6046805705133,
125.472097272328));
#117105=CARTESIAN_POINT('Ctrl Pts',(4.23575366586114,-31.5378713234268,
125.641545058589));
#117106=CARTESIAN_POINT('Ctrl Pts',(4.23368914925321,-31.5249655788896,
125.671645734975));
#117107=CARTESIAN_POINT('Ctrl Pts',(4.23020763861349,-31.5021534629487,
125.72079883118));
#117108=CARTESIAN_POINT('Ctrl Pts',(4.22881326754233,-31.4927504221238,
125.740075708319));
#117109=CARTESIAN_POINT('Ctrl Pts',(4.22683302510541,-31.4790783596106,
125.766783189641));
#117110=CARTESIAN_POINT('Ctrl Pts',(4.22626482784102,-31.4751197107079,
125.774371412831));
#117111=CARTESIAN_POINT('Ctrl Pts',(4.22528533890743,-31.4682388932838,
125.787316828047));
#117112=CARTESIAN_POINT('Ctrl Pts',(4.22487582712739,-31.4653454544112,
125.792689052272));
#117113=CARTESIAN_POINT('Ctrl Pts',(4.22400753710567,-31.4591769182905,
125.803992927678));
#117114=CARTESIAN_POINT('Ctrl Pts',(4.22354837816044,-31.45589517375,125.809920456328));
#117115=CARTESIAN_POINT('Ctrl Pts',(4.22228338892511,-31.4467975385827,
125.826118754195));
#117116=CARTESIAN_POINT('Ctrl Pts',(4.22147319932365,-31.4409086411515,
125.83634776362));
#117117=CARTESIAN_POINT('Ctrl Pts',(4.21704433047729,-31.4083572570148,
125.891525139464));
#117118=CARTESIAN_POINT('Ctrl Pts',(4.21332202333584,-31.3797020102034,
125.93525851543));
#117119=CARTESIAN_POINT('Ctrl Pts',(4.20252035818099,-31.291821509232,126.056533442922));
#117120=CARTESIAN_POINT('Ctrl Pts',(4.19535735206574,-31.2277738738686,
126.130326679629));
#117121=CARTESIAN_POINT('Ctrl Pts',(4.1829910097119,-31.1039288223965,126.249990126512));
#117122=CARTESIAN_POINT('Ctrl Pts',(4.17773177839953,-31.046783184364,126.298222604811));
#117123=CARTESIAN_POINT('Ctrl Pts',(4.17134452873138,-30.9714748825422,
126.353567208739));
#117124=CARTESIAN_POINT('Ctrl Pts',(4.17007273007814,-30.9561776380079,
126.364416362567));
#117125=CARTESIAN_POINT('Ctrl Pts',(4.16802721681029,-30.9310899839611,
126.381579899126));
#117126=CARTESIAN_POINT('Ctrl Pts',(4.16724751458468,-30.9214111797332,
126.388053682562));
#117127=CARTESIAN_POINT('Ctrl Pts',(4.16575239607922,-30.9026311239892,
126.400331943234));
#117128=CARTESIAN_POINT('Ctrl Pts',(4.1650364813213,-30.8935398041171,126.406150463156));
#117129=CARTESIAN_POINT('Ctrl Pts',(4.16339109487335,-30.8724210997654,
126.419379078216));
#117130=CARTESIAN_POINT('Ctrl Pts',(4.16246399573286,-30.8603546234547,
126.426725441425));
#117131=CARTESIAN_POINT('Ctrl Pts',(4.15943007726731,-30.8203337315293,
126.450398736041));
#117132=CARTESIAN_POINT('Ctrl Pts',(4.15734689018052,-30.7919958340841,
126.46606505455));
#117133=CARTESIAN_POINT('Ctrl Pts',(4.14727366930413,-30.651196338731,126.538629670035));
#117134=CARTESIAN_POINT('Ctrl Pts',(4.13969898072987,-30.5329881880253,
126.583465614267));
#117135=CARTESIAN_POINT('Ctrl Pts',(4.12880549058354,-30.3610194039377,
126.627226121469));
#117136=CARTESIAN_POINT('Ctrl Pts',(4.1256225041865,-30.3106319928343,126.637591795652));
#117137=CARTESIAN_POINT('Ctrl Pts',(4.12050586464599,-30.2311307506781,
126.65014542667));
#117138=CARTESIAN_POINT('Ctrl Pts',(4.11863101967559,-30.2022998654994,
126.653927409427));
#117139=CARTESIAN_POINT('Ctrl Pts',(4.11608799650355,-30.1638576399227,
126.657950082375));
#117140=CARTESIAN_POINT('Ctrl Pts',(4.11545355900496,-30.1543202001754,
126.658864993546));
#117141=CARTESIAN_POINT('Ctrl Pts',(4.11439497470346,-30.1385060590429,
126.660244463591));
#117142=CARTESIAN_POINT('Ctrl Pts',(4.1139733723927,-30.1322334888595,126.66075582468));
#117143=CARTESIAN_POINT('Ctrl Pts',(4.1131169529277,-30.1195475435465,126.661717701202));
#117144=CARTESIAN_POINT('Ctrl Pts',(4.11268206649378,-30.1131341958608,
126.66216665345));
#117145=CARTESIAN_POINT('Ctrl Pts',(4.11155114247452,-30.0965256544854,
126.663232732119));
#117146=CARTESIAN_POINT('Ctrl Pts',(4.11085211903813,-30.0863272766544,
126.663793229741));
#117147=CARTESIAN_POINT('Ctrl Pts',(4.10794928637258,-30.0442270075574,
126.665718933189));
#117148=CARTESIAN_POINT('Ctrl Pts',(4.10570708694556,-30.0122963143604,
126.666260507857));
#117149=CARTESIAN_POINT('Ctrl Pts',(4.09571478728842,-29.8717746359347,
126.664604866642));
#117150=CARTESIAN_POINT('Ctrl Pts',(4.08771233275723,-29.7635647252818,
126.652709689751));
#117151=CARTESIAN_POINT('Ctrl Pts',(4.07574585805454,-29.6013226152742,
126.618605039537));
#117152=CARTESIAN_POINT('Ctrl Pts',(4.07166703450062,-29.5460008205429,
126.603967506771));
#117153=CARTESIAN_POINT('Ctrl Pts',(4.06503359477111,-29.4556492874781,
126.575010635209));
#117154=CARTESIAN_POINT('Ctrl Pts',(4.06243501874747,-29.4201601198509,
126.56229392441));
#117155=CARTESIAN_POINT('Ctrl Pts',(4.05884932327329,-29.3710827959981,
126.542805107416));
#117156=CARTESIAN_POINT('Ctrl Pts',(4.05782940784878,-29.3571115029106,
126.537035736547));
#117157=CARTESIAN_POINT('Ctrl Pts',(4.05608411417787,-29.3331905109617,
126.526774446916));
#117158=CARTESIAN_POINT('Ctrl Pts',(4.05535571354866,-29.3232030915294,
126.522373495853));
#117159=CARTESIAN_POINT('Ctrl Pts',(4.05396429482689,-29.3041211614648,
126.513740150738));
#117160=CARTESIAN_POINT('Ctrl Pts',(4.05330078846113,-29.2950202509714,
126.50952315742));
#117161=CARTESIAN_POINT('Ctrl Pts',(4.0515637535685,-29.2711954313356,126.498221235096));
#117162=CARTESIAN_POINT('Ctrl Pts',(4.05049492103353,-29.256536464309,126.491001331569));
#117163=CARTESIAN_POINT('Ctrl Pts',(4.04663067059832,-29.2035794786347,
126.463943461823));
#117164=CARTESIAN_POINT('Ctrl Pts',(4.04387946595003,-29.1659475932882,
126.442835117309));
#117165=CARTESIAN_POINT('Ctrl Pts',(4.03394974542766,-29.0313492304479,
126.360308465389));
#117166=CARTESIAN_POINT('Ctrl Pts',(4.02705443893515,-28.9399840379235,
126.290383762643));
#117167=CARTESIAN_POINT('Ctrl Pts',(4.01702527179702,-28.8213762301946,
126.178447413574));
#117168=CARTESIAN_POINT('Ctrl Pts',(4.01402531442402,-28.7876864617562,
126.143760262708));
#117169=CARTESIAN_POINT('Ctrl Pts',(4.00916944944701,-28.7369742924151,
126.086785648973));
#117170=CARTESIAN_POINT('Ctrl Pts',(4.00736534809849,-28.71892344232,126.065448084705));
#117171=CARTESIAN_POINT('Ctrl Pts',(4.00490445364709,-28.6955009042766,
126.036304663281));
#117172=CARTESIAN_POINT('Ctrl Pts',(4.00427871249933,-28.6896457259004,
126.028891107864));
#117173=CARTESIAN_POINT('Ctrl Pts',(4.00323069623234,-28.6800125485721,
126.016478424503));
#117174=CARTESIAN_POINT('Ctrl Pts',(4.00281086026394,-28.6761990253808,
126.011506913893));
#117175=CARTESIAN_POINT('Ctrl Pts',(4.00195378036007,-28.6685083570726,
126.001362966315));
#117176=CARTESIAN_POINT('Ctrl Pts',(4.00151643124816,-28.6646331247064,
125.996189284355));
#117177=CARTESIAN_POINT('Ctrl Pts',(4.00037193420677,-28.6546169296553,
125.982653565336));
#117178=CARTESIAN_POINT('Ctrl Pts',(3.99966167019552,-28.6485239077102,
125.974256636452));
#117179=CARTESIAN_POINT('Ctrl Pts',(3.99664638996665,-28.6231559708506,
125.93860060631));
#117180=CARTESIAN_POINT('Ctrl Pts',(3.99429932888321,-28.6046255831409,
125.910824057031));
#117181=CARTESIAN_POINT('Ctrl Pts',(3.98424977189428,-28.5298567213915,
125.791106001401));
#117182=CARTESIAN_POINT('Ctrl Pts',(3.97631022084783,-28.4817745581952,
125.694378489058));
#117183=CARTESIAN_POINT('Ctrl Pts',(3.96806748132605,-28.4410652415147,
125.587639587124));
#117184=CARTESIAN_POINT('Ctrl Pts',(3.96760122759222,-28.4387948763755,
125.581580964228));
#117185=CARTESIAN_POINT('Ctrl Pts',(3.96713564162385,-28.4365599852621,
125.575509617918));
#117186=CARTESIAN_POINT('Origin',(5.,-30.,125.));
#117187=CARTESIAN_POINT('',(3.26654944485247,-28.4365599843055,125.57550961532));
#117188=CARTESIAN_POINT('',(3.46014888220092,-28.4365599331867,125.575509476449));
#117189=CARTESIAN_POINT('',(5.,-28.4365599837785,125.575509613888));
#117190=CARTESIAN_POINT('',(4.12030991028152,-28.3340002413346,124.999103268726));
#117191=CARTESIAN_POINT('Ctrl Pts',(3.46014888220092,-28.4365599331867,
125.575509476449));
#117192=CARTESIAN_POINT('Ctrl Pts',(3.46532991775447,-28.4612287593674,
125.642525282149));
#117193=CARTESIAN_POINT('Ctrl Pts',(3.47055310032042,-28.4901913607366,
125.707913999253));
#117194=CARTESIAN_POINT('Ctrl Pts',(3.48167381485054,-28.5615879239327,
125.844614835882));
#117195=CARTESIAN_POINT('Ctrl Pts',(3.48752709335552,-28.6053125474045,
125.915015928909));
#117196=CARTESIAN_POINT('Ctrl Pts',(3.49453388119038,-28.6656551191771,
125.997729631814));
#117197=CARTESIAN_POINT('Ctrl Pts',(3.49586545408808,-28.6774938168255,
126.013369691517));
#117198=CARTESIAN_POINT('Ctrl Pts',(3.49798283583202,-28.6969111525982,
126.038101817227));
#117199=CARTESIAN_POINT('Ctrl Pts',(3.49877542725244,-28.7043149569333,
126.047328128534));
#117200=CARTESIAN_POINT('Ctrl Pts',(3.5002802435704,-28.7186283026569,126.064780708679));
#117201=CARTESIAN_POINT('Ctrl Pts',(3.50099312033602,-28.7255203366588,
126.073020494341));
#117202=CARTESIAN_POINT('Ctrl Pts',(3.50262636737665,-28.7415642556874,
126.091829158633));
#117203=CARTESIAN_POINT('Ctrl Pts',(3.50354444804996,-28.7507705234206,
126.102350746716));
#117204=CARTESIAN_POINT('Ctrl Pts',(3.50645501158062,-28.7805447547872,
126.135526786545));
#117205=CARTESIAN_POINT('Ctrl Pts',(3.50842684198261,-28.8016055044676,
126.157731833981));
#117206=CARTESIAN_POINT('Ctrl Pts',(3.51308438016914,-28.8533503061446,
126.209362014637));
#117207=CARTESIAN_POINT('Ctrl Pts',(3.51574753310864,-28.88457245638,126.238217984662));
#117208=CARTESIAN_POINT('Ctrl Pts',(3.5229525464642,-28.9728743250068,126.313774157698));
#117209=CARTESIAN_POINT('Ctrl Pts',(3.52742680294526,-29.0320031187659,
126.357929340266));
#117210=CARTESIAN_POINT('Ctrl Pts',(3.53278268559425,-29.1054688779818,
126.405546651875));
#117211=CARTESIAN_POINT('Ctrl Pts',(3.53363004522545,-29.1171689882141,
126.412924880407));
#117212=CARTESIAN_POINT('Ctrl Pts',(3.53899665000148,-29.1916463202109,
126.458604895782));
#117213=CARTESIAN_POINT('Ctrl Pts',(3.5435683560016,-29.256802455335,126.492855848905));
#117214=CARTESIAN_POINT('Ctrl Pts',(3.54917284952906,-29.3352211517049,
126.527670077878));
#117215=CARTESIAN_POINT('Ctrl Pts',(3.54998125458917,-29.3464986056246,
126.532528201948));
#117216=CARTESIAN_POINT('Ctrl Pts',(3.55125852061003,-29.364242243006,126.539940385763));
#117217=CARTESIAN_POINT('Ctrl Pts',(3.55172250411449,-29.3706727284248,
126.542579494923));
#117218=CARTESIAN_POINT('Ctrl Pts',(3.55259524691991,-29.3827354427691,
126.547442125453));
#117219=CARTESIAN_POINT('Ctrl Pts',(3.55300343181197,-29.388363521192,126.549675281582));
#117220=CARTESIAN_POINT('Ctrl Pts',(3.55396997831247,-29.4016596287601,
126.55486731057));
#117221=CARTESIAN_POINT('Ctrl Pts',(3.55452982624035,-29.4093375182824,
126.557800172983));
#117222=CARTESIAN_POINT('Ctrl Pts',(3.55641546833364,-29.4351294277933,
126.567434292581));
#117223=CARTESIAN_POINT('Ctrl Pts',(3.5577548258011,-29.4533374744489,126.573877069074));
#117224=CARTESIAN_POINT('Ctrl Pts',(3.56108938031962,-29.4984906209931,
126.588976141008));
#117225=CARTESIAN_POINT('Ctrl Pts',(3.56309918218078,-29.5255516882073,
126.597264991331));
#117226=CARTESIAN_POINT('Ctrl Pts',(3.57231599811235,-29.6494586680582,
126.631791410014));
#117227=CARTESIAN_POINT('Ctrl Pts',(3.57969566492214,-29.7483427282499,
126.649936823387));
#117228=CARTESIAN_POINT('Ctrl Pts',(3.59286787274552,-29.9302851552353,
126.666577422531));
#117229=CARTESIAN_POINT('Ctrl Pts',(3.59869312869536,-30.0127638957753,
126.667987175944));
#117230=CARTESIAN_POINT('Ctrl Pts',(3.60567285382405,-30.1145896885818,
126.66217009621));
#117231=CARTESIAN_POINT('Ctrl Pts',(3.60700362335552,-30.1341388844873,
126.660706789916));
#117232=CARTESIAN_POINT('Ctrl Pts',(3.60912004177136,-30.1654346609528,
126.657807962926));
#117233=CARTESIAN_POINT('Ctrl Pts',(3.60991246227526,-30.1771991782469,
126.656591782154));
#117234=CARTESIAN_POINT('Ctrl Pts',(3.61141714634194,-30.1996230396647,
126.654032055268));
#117235=CARTESIAN_POINT('Ctrl Pts',(3.61213005976159,-30.2102842377848,
126.652710484742));
#117236=CARTESIAN_POINT('Ctrl Pts',(3.61376366176776,-30.2347933147538,
126.64943131754));
#117237=CARTESIAN_POINT('Ctrl Pts',(3.61468205726588,-30.2486309416167,
126.647402272233));
#117238=CARTESIAN_POINT('Ctrl Pts',(3.61759475633636,-30.2926846761326,
126.640374832179));
#117239=CARTESIAN_POINT('Ctrl Pts',(3.61956836327565,-30.3227902324913,
126.634717273503));
#117240=CARTESIAN_POINT('Ctrl Pts',(3.62423100207547,-30.3943108343342,
126.61922375425));
#117241=CARTESIAN_POINT('Ctrl Pts',(3.62689740871858,-30.4355388687808,
126.608624528928));
#117242=CARTESIAN_POINT('Ctrl Pts',(3.63410406030919,-30.5469337260266,
126.575388827143));
#117243=CARTESIAN_POINT('Ctrl Pts',(3.63857691673909,-30.6160751916339,
126.549657439062));
#117244=CARTESIAN_POINT('Ctrl Pts',(3.6439445879609,-30.6960954875547,126.513672466843));
#117245=CARTESIAN_POINT('Ctrl Pts',(3.64480505028118,-30.708831504118,126.50775036306));
#117246=CARTESIAN_POINT('Ctrl Pts',(3.65016779017718,-30.7875183002385,
126.469944525175));
#117247=CARTESIAN_POINT('Ctrl Pts',(3.65472264274787,-30.8513734072728,
126.433904665862));
#117248=CARTESIAN_POINT('Ctrl Pts',(3.66030842699278,-30.9229138819223,
126.387060461597));
#117249=CARTESIAN_POINT('Ctrl Pts',(3.66111676280043,-30.9331109793367,
126.380221227214));
#117250=CARTESIAN_POINT('Ctrl Pts',(3.66239394293167,-30.9489606881828,
126.3693348481));
#117251=CARTESIAN_POINT('Ctrl Pts',(3.66285791085971,-30.9546653803884,
126.365363805382));
#117252=CARTESIAN_POINT('Ctrl Pts',(3.66373064188961,-30.9652929101285,
126.35786680626));
#117253=CARTESIAN_POINT('Ctrl Pts',(3.66413883078226,-30.9702215891158,
126.354349559463));
#117254=CARTESIAN_POINT('Ctrl Pts',(3.66510541059366,-30.9817953481934,
126.34599459679));
#117255=CARTESIAN_POINT('Ctrl Pts',(3.66566528814227,-30.9884239203541,
126.34113448502));
#117256=CARTESIAN_POINT('Ctrl Pts',(3.66755113674812,-31.0105089247112,
126.324688958416));
#117257=CARTESIAN_POINT('Ctrl Pts',(3.66889067499644,-31.0257991423795,
126.312884291714));
#117258=CARTESIAN_POINT('Ctrl Pts',(3.67222578053739,-31.0629797880686,
126.283133311526));
#117259=CARTESIAN_POINT('Ctrl Pts',(3.67423595840849,-31.0846242931938,
126.264890148074));
#117260=CARTESIAN_POINT('Ctrl Pts',(3.68345611992189,-31.1808671940163,
126.179484337047));
#117261=CARTESIAN_POINT('Ctrl Pts',(3.69083884779448,-31.2497674287165,
126.106215386806));
#117262=CARTESIAN_POINT('Ctrl Pts',(3.70401036702836,-31.3624104493522,
125.962377534351));
#117263=CARTESIAN_POINT('Ctrl Pts',(3.70983218646979,-31.408298938585,125.893885068763));
#117264=CARTESIAN_POINT('Ctrl Pts',(3.71680858975323,-31.4586141220279,
125.805223578588));
#117265=CARTESIAN_POINT('Ctrl Pts',(3.71813925838095,-31.4679867582043,
125.78800704512));
#117266=CARTESIAN_POINT('Ctrl Pts',(3.72025555580035,-31.4825241516162,
125.760143408546));
#117267=CARTESIAN_POINT('Ctrl Pts',(3.72104795483627,-31.4878828749239,
125.749600176543));
#117268=CARTESIAN_POINT('Ctrl Pts',(3.72255262230491,-31.4978940955259,
125.729372797756));
#117269=CARTESIAN_POINT('Ctrl Pts',(3.72326554034158,-31.5025660537777,
125.719699008456));
#117270=CARTESIAN_POINT('Ctrl Pts',(3.72489918699927,-31.5131041798168,
125.697328710352));
#117271=CARTESIAN_POINT('Ctrl Pts',(3.72581762209329,-31.5189047473797,
125.684602057698));
#117272=CARTESIAN_POINT('Ctrl Pts',(3.72873058983711,-31.5368954121266,
125.643775286773));
#117273=CARTESIAN_POINT('Ctrl Pts',(3.73070442029226,-31.5484715910502,
125.615410471343));
#117274=CARTESIAN_POINT('Ctrl Pts',(3.73536770096955,-31.5742480175744,
125.546909826777));
#117275=CARTESIAN_POINT('Ctrl Pts',(3.73803451710919,-31.5877052751456,
125.506517047856));
#117276=CARTESIAN_POINT('Ctrl Pts',(3.74524136264681,-31.6201977354068,
125.394899125859));
#117277=CARTESIAN_POINT('Ctrl Pts',(3.74971403117173,-31.6360775111014,
125.3228571845));
#117278=CARTESIAN_POINT('Ctrl Pts',(3.75508290058745,-31.6492465947405,
125.236092277556));
#117279=CARTESIAN_POINT('Ctrl Pts',(3.75594473806314,-31.6511813048847,
125.22215802037));
#117280=CARTESIAN_POINT('Ctrl Pts',(3.76130699327965,-31.6620898394809,
125.1355535307));
#117281=CARTESIAN_POINT('Ctrl Pts',(3.76585999824478,-31.6664399486111,
125.062390575192));
#117282=CARTESIAN_POINT('Ctrl Pts',(3.77144373181391,-31.6658852474748,
124.976911108947));
#117283=CARTESIAN_POINT('Ctrl Pts',(3.77225205994675,-31.6656698468975,
124.964634847378));
#117284=CARTESIAN_POINT('Ctrl Pts',(3.77352923055926,-31.6651200394101,
124.945414581429));
#117285=CARTESIAN_POINT('Ctrl Pts',(3.77399319676115,-31.6648778135567,
124.938468096763));
#117286=CARTESIAN_POINT('Ctrl Pts',(3.77486592648628,-31.6643432477886,
124.925473363823));
#117287=CARTESIAN_POINT('Ctrl Pts',(3.77527411582245,-31.6640613929902,
124.919424931681));
#117288=CARTESIAN_POINT('Ctrl Pts',(3.77624069932617,-31.6633192115683,
124.90516982799));
#117289=CARTESIAN_POINT('Ctrl Pts',(3.77680058015803,-31.6628311152389,
124.896964878775));
#117290=CARTESIAN_POINT('Ctrl Pts',(3.77868645165528,-31.660992597261,124.869490512831));
#117291=CARTESIAN_POINT('Ctrl Pts',(3.78002600994291,-31.6593678146676,
124.850241826587));
#117292=CARTESIAN_POINT('Ctrl Pts',(3.7833611765657,-31.6545380464134,124.80286803854));
#117293=CARTESIAN_POINT('Ctrl Pts',(3.78537139611885,-31.650950265369,124.774788549093));
#117294=CARTESIAN_POINT('Ctrl Pts',(3.79459192860026,-31.6313948185806,
124.647604644421));
#117295=CARTESIAN_POINT('Ctrl Pts',(3.80197499590304,-31.6072057302879,
124.549975824683));
#117296=CARTESIAN_POINT('Ctrl Pts',(3.81514643885347,-31.5474533217331,
124.377328245949));
#117297=CARTESIAN_POINT('Ctrl Pts',(3.82096787732227,-31.514799756558,124.301632433047));
#117298=CARTESIAN_POINT('Ctrl Pts',(3.82794391230333,-31.4676029552573,
124.211278421824));
#117299=CARTESIAN_POINT('Ctrl Pts',(3.82927456971232,-31.4582220471357,
124.194066578225));
#117300=CARTESIAN_POINT('Ctrl Pts',(3.83139085367901,-31.4426972420499,
124.16674101946));
#117301=CARTESIAN_POINT('Ctrl Pts',(3.83218325032808,-31.4367458075771,
124.156520683263));
#117302=CARTESIAN_POINT('Ctrl Pts',(3.83368791595135,-31.4251816412912,
124.137139241225));
#117303=CARTESIAN_POINT('Ctrl Pts',(3.83440083450162,-31.4195881653953,
124.127967403364));
#117304=CARTESIAN_POINT('Ctrl Pts',(3.83603448612494,-31.4065093590034,
124.106980955285));
#117305=CARTESIAN_POINT('Ctrl Pts',(3.83695292562201,-31.3989631228259,
124.095205110582));
#117306=CARTESIAN_POINT('Ctrl Pts',(3.83986592324375,-31.3744199963634,
124.057947015548));
#117307=CARTESIAN_POINT('Ctrl Pts',(3.84183977855529,-31.3568677387098,
124.03283699387));
#117308=CARTESIAN_POINT('Ctrl Pts',(3.84650313061535,-31.3132968234182,
123.974027925592));
#117309=CARTESIAN_POINT('Ctrl Pts',(3.84916999229536,-31.2866592920587,
123.940813759968));
#117310=CARTESIAN_POINT('Ctrl Pts',(3.85637685923743,-31.2105064667283,
123.852977739293));
#117311=CARTESIAN_POINT('Ctrl Pts',(3.86084950670794,-31.1585936370154,
123.800563832764));
#117312=CARTESIAN_POINT('Ctrl Pts',(3.86621850567641,-31.0928394189226,
123.742440471932));
#117313=CARTESIAN_POINT('Ctrl Pts',(3.86708049254056,-31.0821800812025,
123.733256052763));
#117314=CARTESIAN_POINT('Ctrl Pts',(3.87244269388305,-31.0153366855485,
123.677121204314));
#117315=CARTESIAN_POINT('Ctrl Pts',(3.87699549691995,-30.9562312757209,
123.633787742421));
#117316=CARTESIAN_POINT('Ctrl Pts',(3.88257900637132,-30.8841182976005,
123.587894624976));
#117317=CARTESIAN_POINT('Ctrl Pts',(3.8833873336643,-30.8736876608711,123.5814173962));
#117318=CARTESIAN_POINT('Ctrl Pts',(3.88466450323518,-30.8572416958763,
123.571454940026));
#117319=CARTESIAN_POINT('Ctrl Pts',(3.88512846924817,-30.8512742793772,
123.567890922304));
#117320=CARTESIAN_POINT('Ctrl Pts',(3.88600119883046,-30.8400669108008,
123.561292159143));
#117321=CARTESIAN_POINT('Ctrl Pts',(3.88640938821511,-30.834832490976,123.558248505014));
#117322=CARTESIAN_POINT('Ctrl Pts',(3.88737597212307,-30.8224536197502,
123.551140584963));
#117323=CARTESIAN_POINT('Ctrl Pts',(3.88793585331422,-30.8152955540348,
123.547100583774));
#117324=CARTESIAN_POINT('Ctrl Pts',(3.88982172731652,-30.7912159644553,
123.533744076505));
#117325=CARTESIAN_POINT('Ctrl Pts',(3.89116128779708,-30.7741630531813,
123.524669317359));
#117326=CARTESIAN_POINT('Ctrl Pts',(3.89449646110404,-30.7317426926238,
123.503033135777));
#117327=CARTESIAN_POINT('Ctrl Pts',(3.89650668521849,-30.7062059489065,
123.490818056826));
#117328=CARTESIAN_POINT('Ctrl Pts',(3.90572725829652,-30.5887465190894,
123.438267251891));
#117329=CARTESIAN_POINT('Ctrl Pts',(3.91311036274472,-30.4936045096298,
123.405639091831));
#117330=CARTESIAN_POINT('Ctrl Pts',(3.92628179734783,-30.3161482211605,
123.36220205613));
#117331=CARTESIAN_POINT('Ctrl Pts',(3.93210319412599,-30.2348433056025,
123.348581189028));
#117332=CARTESIAN_POINT('Ctrl Pts',(3.9390791888024,-30.1333356982793,123.339228566891));
#117333=CARTESIAN_POINT('Ctrl Pts',(3.94040984498329,-30.1137874286749,
123.337774792795));
#117334=CARTESIAN_POINT('Ctrl Pts',(3.9425261274773,-30.0824099611487,123.33599745821));
#117335=CARTESIAN_POINT('Ctrl Pts',(3.94331852386509,-30.0705955709546,
123.335454374724));
#117336=CARTESIAN_POINT('Ctrl Pts',(3.94482318928658,-30.0480403915748,
123.334658137047));
#117337=CARTESIAN_POINT('Ctrl Pts',(3.94553610789297,-30.0373010296701,
123.334382984557));
#117338=CARTESIAN_POINT('Ctrl Pts',(3.94716976005973,-30.0125759171249,
123.333988764232));
#117339=CARTESIAN_POINT('Ctrl Pts',(3.9480882000388,-29.9985897020255,123.333941891105));
#117340=CARTESIAN_POINT('Ctrl Pts',(3.9510012009313,-29.9539761922974,123.334354190202));
#117341=CARTESIAN_POINT('Ctrl Pts',(3.95297505896388,-29.9233604119264,
123.335481836395));
#117342=CARTESIAN_POINT('Ctrl Pts',(3.95763841883828,-29.8503209270508,
123.34019175022));
#117343=CARTESIAN_POINT('Ctrl Pts',(3.96030528550364,-29.8079689377568,
123.344556946585));
#117344=CARTESIAN_POINT('Ctrl Pts',(3.96751215478685,-29.6928714715943,
123.360897186192));
#117345=CARTESIAN_POINT('Ctrl Pts',(3.97198479995059,-29.6206806504457,
123.37608400442));
#117346=CARTESIAN_POINT('Ctrl Pts',(3.98144490244575,-29.4718021718128,
123.417876513893));
#117347=CARTESIAN_POINT('Ctrl Pts',(3.98642785149998,-29.3955789386686,
123.445400466576));
#117348=CARTESIAN_POINT('Ctrl Pts',(3.99271754940338,-29.3069297739578,
123.484919135945));
#117349=CARTESIAN_POINT('Ctrl Pts',(3.99377334547296,-29.2922889685515,
123.491702479008));
#117350=CARTESIAN_POINT('Ctrl Pts',(3.99535521992618,-29.2707517182,123.50206367003));
#117351=CARTESIAN_POINT('Ctrl Pts',(3.99587198756371,-29.2637775704583,
123.505479062234));
#117352=CARTESIAN_POINT('Ctrl Pts',(3.9967941408829,-29.2514473301767,123.511624697639));
#117353=CARTESIAN_POINT('Ctrl Pts',(3.99719832673008,-29.246081766641,123.514335355673));
#117354=CARTESIAN_POINT('Ctrl Pts',(3.99809442097233,-29.2342726764778,
123.520381701839));
#117355=CARTESIAN_POINT('Ctrl Pts',(3.99858709737131,-29.22783629977,123.523730425256));
#117356=CARTESIAN_POINT('Ctrl Pts',(4.00004334439385,-29.2089705797939,
123.533703024247));
#117357=CARTESIAN_POINT('Ctrl Pts',(4.0010135927777,-29.1966034770277,123.540442409874));
#117358=CARTESIAN_POINT('Ctrl Pts',(4.00788448135043,-29.1103358552988,
123.588882046302));
#117359=CARTESIAN_POINT('Ctrl Pts',(4.01404416544292,-29.0396373519479,
123.636014360602));
#117360=CARTESIAN_POINT('Ctrl Pts',(4.02948371415978,-28.8726242102543,
123.766799735977));
#117361=CARTESIAN_POINT('Ctrl Pts',(4.0387027844885,-28.7817102821561,123.856522496258));
#117362=CARTESIAN_POINT('Ctrl Pts',(4.04891683104113,-28.6886644222319,
123.972186528897));
#117363=CARTESIAN_POINT('Ctrl Pts',(4.05035702854925,-28.6757473174831,
123.988883571246));
#117364=CARTESIAN_POINT('Ctrl Pts',(4.05268827165657,-28.655179906664,124.016540128322));
#117365=CARTESIAN_POINT('Ctrl Pts',(4.05358667030016,-28.6473383166857,
124.027353717342));
#117366=CARTESIAN_POINT('Ctrl Pts',(4.05519411568284,-28.6334645112329,
124.046978105102));
#117367=CARTESIAN_POINT('Ctrl Pts',(4.05590493145794,-28.6273854188557,
124.055754695563));
#117368=CARTESIAN_POINT('Ctrl Pts',(4.05742083903453,-28.6145441314777,
124.074680194685));
#117369=CARTESIAN_POINT('Ctrl Pts',(4.05822491512972,-28.6078081264228,
124.084846184434));
#117370=CARTESIAN_POINT('Ctrl Pts',(4.06042496870552,-28.5895921877436,
124.113004360132));
#117371=CARTESIAN_POINT('Ctrl Pts',(4.06181233070301,-28.5783451597669,
124.131144980734));
#117372=CARTESIAN_POINT('Ctrl Pts',(4.06803814907085,-28.5290376122545,
124.214196528902));
#117373=CARTESIAN_POINT('Ctrl Pts',(4.07273134890063,-28.4950504888545,
124.281427564177));
#117374=CARTESIAN_POINT('Ctrl Pts',(4.08222523325239,-28.4348971950192,
124.42357532095));
#117375=CARTESIAN_POINT('Ctrl Pts',(4.08700717862264,-28.4092993999039,
124.498518771395));
#117376=CARTESIAN_POINT('Ctrl Pts',(4.09532078163864,-28.3749114021091,
124.628858268459));
#117377=CARTESIAN_POINT('Ctrl Pts',(4.09880027393672,-28.3634123427282,
124.683394885247));
#117378=CARTESIAN_POINT('Ctrl Pts',(4.10354692297196,-28.3518817806926,
124.75591613204));
#117379=CARTESIAN_POINT('Ctrl Pts',(4.10470540968413,-28.3493767186088,
124.773475562353));
#117380=CARTESIAN_POINT('Ctrl Pts',(4.10639857849468,-28.3461663881126,
124.798872613458));
#117381=CARTESIAN_POINT('Ctrl Pts',(4.10692154951149,-28.3452354674114,
124.806681152133));
#117382=CARTESIAN_POINT('Ctrl Pts',(4.10785098795096,-28.3436884188277,
124.820488686389));
#117383=CARTESIAN_POINT('Ctrl Pts',(4.10825619117933,-28.3430495279652,
124.826484879077));
#117384=CARTESIAN_POINT('Ctrl Pts',(4.10904746182334,-28.3418709276439,
124.838147070533));
#117385=CARTESIAN_POINT('Ctrl Pts',(4.10943327520248,-28.3413276967457,
124.84381235849));
#117386=CARTESIAN_POINT('Ctrl Pts',(4.11030142907303,-28.3401752523307,
124.856515805792));
#117387=CARTESIAN_POINT('Ctrl Pts',(4.1107845878385,-28.3395817608714,124.863555235486));
#117388=CARTESIAN_POINT('Ctrl Pts',(4.11237843502179,-28.3377798553157,
124.886683990698));
#117389=CARTESIAN_POINT('Ctrl Pts',(4.11349822041555,-28.3367604410981,
124.902786569273));
#117390=CARTESIAN_POINT('Ctrl Pts',(4.11649924622742,-28.3346730304706,
124.945616809692));
#117391=CARTESIAN_POINT('Ctrl Pts',(4.11839629444807,-28.334014636662,124.972358788451));
#117392=CARTESIAN_POINT('Ctrl Pts',(4.12030991028152,-28.3340002413346,
124.999103268726));
#117393=CARTESIAN_POINT('Ctrl Pts',(4.12030973512622,-28.3340002426541,
124.999100820774));
#117394=CARTESIAN_POINT('Ctrl Pts',(4.12666726406915,-28.333952287056,125.08795297888));
#117395=CARTESIAN_POINT('Ctrl Pts',(4.13318681829467,-28.3410123763757,
125.176667750711));
#117396=CARTESIAN_POINT('Ctrl Pts',(4.14426204756692,-28.3652763865857,
125.327620293619));
#117397=CARTESIAN_POINT('Ctrl Pts',(4.14885076896109,-28.3790760497282,
125.390209339223));
#117398=CARTESIAN_POINT('Ctrl Pts',(4.15618819211529,-28.4074615666325,
125.490944771156));
#117399=CARTESIAN_POINT('Ctrl Pts',(4.15899418050003,-28.4199031649118,
125.52962242359));
#117400=CARTESIAN_POINT('Ctrl Pts',(4.16194038544885,-28.4346784063753,
125.570378624622));
#117401=CARTESIAN_POINT('Ctrl Pts',(4.16212588216124,-28.435616040836,125.572945281105));
#117402=CARTESIAN_POINT('Ctrl Pts',(4.16231116930939,-28.436559983762,125.575509613843));
#117403=CARTESIAN_POINT('Ctrl Pts',(3.96713564162385,-28.4365599852621,
125.575509617918));
#117404=CARTESIAN_POINT('Ctrl Pts',(3.96352864762869,-28.4192458061984,
125.528473600573));
#117405=CARTESIAN_POINT('Ctrl Pts',(3.95996290866004,-28.4040607105344,
125.480673858322));
#117406=CARTESIAN_POINT('Ctrl Pts',(3.9538426667242,-28.3813426200198,125.396112216372));
#117407=CARTESIAN_POINT('Ctrl Pts',(3.95126254740571,-28.3728525443762,
125.359650031383));
#117408=CARTESIAN_POINT('Ctrl Pts',(3.94769747204483,-28.3626750665644,
125.308140141014));
#117409=CARTESIAN_POINT('Ctrl Pts',(3.94668022427208,-28.3599536216725,
125.293310734621));
#117410=CARTESIAN_POINT('Ctrl Pts',(3.94493805013225,-28.3556108522336,
125.267692530268));
#117411=CARTESIAN_POINT('Ctrl Pts',(3.94421012975797,-28.3538935446072,
125.256921208376));
#117412=CARTESIAN_POINT('Ctrl Pts',(3.94272867798882,-28.3505989262102,
125.234865697589));
#117413=CARTESIAN_POINT('Ctrl Pts',(3.9419754895445,-28.3490313406727,125.22358062291));
#117414=CARTESIAN_POINT('Ctrl Pts',(3.94007040858907,-28.3453418994321,
125.194861456443));
#117415=CARTESIAN_POINT('Ctrl Pts',(3.93892356348225,-28.3433796873595,
125.177407990238));
#117416=CARTESIAN_POINT('Ctrl Pts',(3.93429800904611,-28.3365315365952,
125.106398168395));
#117417=CARTESIAN_POINT('Ctrl Pts',(3.93089121430676,-28.3339637011001,
125.052648173956));
#117418=CARTESIAN_POINT('Ctrl Pts',(3.92157743179926,-28.3340655593804,
124.903317728497));
#117419=CARTESIAN_POINT('Ctrl Pts',(3.91580908409069,-28.3423497631894,
124.807955221799));
#117420=CARTESIAN_POINT('Ctrl Pts',(3.90525577943598,-28.37189304426,124.638520869716));
#117421=CARTESIAN_POINT('Ctrl Pts',(3.90051314394173,-28.3901895479928,
124.564217127033));
#117422=CARTESIAN_POINT('Ctrl Pts',(3.89471857364882,-28.4172692269698,
124.479740151251));
#117423=CARTESIAN_POINT('Ctrl Pts',(3.89390957665405,-28.421149634481,124.468080352304));
#117424=CARTESIAN_POINT('Ctrl Pts',(3.89263166261146,-28.4274265704979,
124.449893522324));
#117425=CARTESIAN_POINT('Ctrl Pts',(3.89216763292323,-28.4297356740866,
124.443336483732));
#117426=CARTESIAN_POINT('Ctrl Pts',(3.89129502354381,-28.4341318165259,
124.431098017651));
#117427=CARTESIAN_POINT('Ctrl Pts',(3.8908870203951,-28.4362088654996,124.425413264577));
#117428=CARTESIAN_POINT('Ctrl Pts',(3.88992122171976,-28.4411766137068,
124.412043310677));
#117429=CARTESIAN_POINT('Ctrl Pts',(3.88936194489439,-28.4440932030299,
124.404368024486));
#117430=CARTESIAN_POINT('Ctrl Pts',(3.88747967205802,-28.4540455820203,
124.378749320774));
#117431=CARTESIAN_POINT('Ctrl Pts',(3.88614317290184,-28.4613357025898,
124.360907229159));
#117432=CARTESIAN_POINT('Ctrl Pts',(3.88281716880542,-28.4800587435126,
124.317262168115));
#117433=CARTESIAN_POINT('Ctrl Pts',(3.88081314549017,-28.4918407476356,
124.29161602209));
#117434=CARTESIAN_POINT('Ctrl Pts',(3.87164657880397,-28.5481849909733,
124.176754425839));
#117435=CARTESIAN_POINT('Ctrl Pts',(3.86431272939907,-28.6000513117406,
124.091350356092));
#117436=CARTESIAN_POINT('Ctrl Pts',(3.85112931401377,-28.7085597220535,
123.944234629508));
#117437=CARTESIAN_POINT('Ctrl Pts',(3.84525172148636,-28.7628133358153,
123.881147271579));
#117438=CARTESIAN_POINT('Ctrl Pts',(3.83822173658365,-28.8354248298719,
123.80848600785));
#117439=CARTESIAN_POINT('Ctrl Pts',(3.83688973546746,-28.8495376276999,
123.794853823229));
#117440=CARTESIAN_POINT('Ctrl Pts',(3.83477199894841,-28.8725395918999,
123.773407594073));
#117441=CARTESIAN_POINT('Ctrl Pts',(3.83397947356079,-28.8812765472154,
123.765433780314));
#117442=CARTESIAN_POINT('Ctrl Pts',(3.83247498925245,-28.8981056482833,
123.750400010187));
#117443=CARTESIAN_POINT('Ctrl Pts',(3.83176237667684,-28.9061825426724,
123.743323957362));
#117444=CARTESIAN_POINT('Ctrl Pts',(3.83013003461322,-28.9249237256984,
123.727222657881));
#117445=CARTESIAN_POINT('Ctrl Pts',(3.82921258939444,-28.9356343465705,
123.718252390808));
#117446=CARTESIAN_POINT('Ctrl Pts',(3.82630535355008,-28.9701266212994,
123.690095255444));
#117447=CARTESIAN_POINT('Ctrl Pts',(3.82433615205136,-28.9943246121907,
123.671426773606));
#117448=CARTESIAN_POINT('Ctrl Pts',(3.81968595623702,-29.0533104293303,
123.628455492344));
#117449=CARTESIAN_POINT('Ctrl Pts',(3.81702741989229,-29.0885402237399,
123.604795020764));
#117450=CARTESIAN_POINT('Ctrl Pts',(3.8098248175971,-29.1873802507635,123.543757166018));
#117451=CARTESIAN_POINT('Ctrl Pts',(3.80534866127199,-29.2526285159713,
123.509218230986));
#117452=CARTESIAN_POINT('Ctrl Pts',(3.80001615027389,-29.3322036468676,
123.473636941602));
#117453=CARTESIAN_POINT('Ctrl Pts',(3.79919394292238,-29.3445223859449,
123.468306411996));
#117454=CARTESIAN_POINT('Ctrl Pts',(3.79382151976482,-29.4252238015701,
123.434537392432));
#117455=CARTESIAN_POINT('Ctrl Pts',(3.78921906393103,-29.4953654259717,
123.410540339049));
#117456=CARTESIAN_POINT('Ctrl Pts',(3.78358055975889,-29.5787170185263,
123.38809819681));
#117457=CARTESIAN_POINT('Ctrl Pts',(3.78277218261997,-29.5906082617706,
123.385037103674));
#117458=CARTESIAN_POINT('Ctrl Pts',(3.78149503733048,-29.6092808166135,
123.380449810057));
#117459=CARTESIAN_POINT('Ctrl Pts',(3.78103114703818,-29.616039968685,123.378834065251));
#117460=CARTESIAN_POINT('Ctrl Pts',(3.78015864323567,-29.6287047408907,
123.375890253134));
#117461=CARTESIAN_POINT('Ctrl Pts',(3.77975060448261,-29.6346077444194,
123.374552020461));
#117462=CARTESIAN_POINT('Ctrl Pts',(3.77878450858412,-29.6485389539525,
123.371473483915));
#117463=CARTESIAN_POINT('Ctrl Pts',(3.77822496737115,-29.6565728831131,
123.369760358476));
#117464=CARTESIAN_POINT('Ctrl Pts',(3.7763408527856,-29.6835201823927,123.364222242629));
#117465=CARTESIAN_POINT('Ctrl Pts',(3.7750027416377,-29.702486500201,123.360666603587));
#117466=CARTESIAN_POINT('Ctrl Pts',(3.77167182689829,-29.7493773842434,
123.352716398822));
#117467=CARTESIAN_POINT('Ctrl Pts',(3.76966445363248,-29.7773597339886,
123.348701695674));
#117468=CARTESIAN_POINT('Ctrl Pts',(3.76046823664936,-29.9048260302872,
123.333712416959));
#117469=CARTESIAN_POINT('Ctrl Pts',(3.7531072750159,-30.0050733627839,123.331004163876));
#117470=CARTESIAN_POINT('Ctrl Pts',(3.73993007223488,-30.187459174884,123.342517418871));
#117471=CARTESIAN_POINT('Ctrl Pts',(3.7340830592895,-30.2694675356135,123.353858935357));
#117472=CARTESIAN_POINT('Ctrl Pts',(3.72708256762523,-30.3694749307159,
123.37536812854));
#117473=CARTESIAN_POINT('Ctrl Pts',(3.72575141293428,-30.3885701861821,
123.379829110991));
#117474=CARTESIAN_POINT('Ctrl Pts',(3.72363469136726,-30.4190490512539,
123.387519385085));
#117475=CARTESIAN_POINT('Ctrl Pts',(3.7228423460522,-30.4304842523267,123.390534510524));
#117476=CARTESIAN_POINT('Ctrl Pts',(3.72133800128878,-30.4522403237117,
123.396519410584));
#117477=CARTESIAN_POINT('Ctrl Pts',(3.72062535030276,-30.4625664281834,
123.39946770737));
#117478=CARTESIAN_POINT('Ctrl Pts',(3.71899263530128,-30.486263856021,123.406482267074));
#117479=CARTESIAN_POINT('Ctrl Pts',(3.71807485921755,-30.4996140826859,
123.410617386871));
#117480=CARTESIAN_POINT('Ctrl Pts',(3.71516538054259,-30.5420103226763,
123.424336253497));
#117481=CARTESIAN_POINT('Ctrl Pts',(3.71319431340135,-30.5708461291343,
123.434552358949));
#117482=CARTESIAN_POINT('Ctrl Pts',(3.70853876390975,-30.6390185278826,
123.46083931436));
#117483=CARTESIAN_POINT('Ctrl Pts',(3.70587681320953,-30.6780540780491,
123.477632323725));
#117484=CARTESIAN_POINT('Ctrl Pts',(3.6986722306304,-30.7829671285244,123.527602718632));
#117485=CARTESIAN_POINT('Ctrl Pts',(3.6941972937502,-30.847350731505,123.563689315279));
#117486=CARTESIAN_POINT('Ctrl Pts',(3.68884536145513,-30.9206605933198,
123.611429034442));
#117487=CARTESIAN_POINT('Ctrl Pts',(3.68800259901805,-30.9320951823863,
123.619078633755));
#117488=CARTESIAN_POINT('Ctrl Pts',(3.68263423726541,-31.0041327414484,
123.668573293278));
#117489=CARTESIAN_POINT('Ctrl Pts',(3.67805621681543,-31.0619923647512,
123.714251538116));
#117490=CARTESIAN_POINT('Ctrl Pts',(3.67244485434571,-31.1257450231763,
123.771828644301));
#117491=CARTESIAN_POINT('Ctrl Pts',(3.67163657537568,-31.1347650147263,
123.780157766036));
#117492=CARTESIAN_POINT('Ctrl Pts',(3.67035955183838,-31.1487449382285,
123.793356158528));
#117493=CARTESIAN_POINT('Ctrl Pts',(3.66989568362529,-31.1537680617216,
123.798158268055));
#117494=CARTESIAN_POINT('Ctrl Pts',(3.66902319652695,-31.1631099995716,
123.807201706442));
#117495=CARTESIAN_POINT('Ctrl Pts',(3.66861515211598,-31.1674359316296,
123.811435327346));
#117496=CARTESIAN_POINT('Ctrl Pts',(3.66764900905809,-31.1775785968597,
123.821470348873));
#117497=CARTESIAN_POINT('Ctrl Pts',(3.66708942590384,-31.1833755946098,
123.827291304127));
#117498=CARTESIAN_POINT('Ctrl Pts',(3.66520501902391,-31.2026465510491,
123.846930288713));
#117499=CARTESIAN_POINT('Ctrl Pts',(3.66386665202302,-31.2159228483038,
123.860938968508));
#117500=CARTESIAN_POINT('Ctrl Pts',(3.6605349576626,-31.2480411180231,123.896030463615));
#117501=CARTESIAN_POINT('Ctrl Pts',(3.65852705247634,-31.2665951050291,
123.917368008497));
#117502=CARTESIAN_POINT('Ctrl Pts',(3.64932611594672,-31.3483604993028,
124.016380208844));
#117503=CARTESIAN_POINT('Ctrl Pts',(3.64196083751902,-31.4050329845057,
124.099185538469));
#117504=CARTESIAN_POINT('Ctrl Pts',(3.62878461566318,-31.4942554506541,
124.25866393905));
#117505=CARTESIAN_POINT('Ctrl Pts',(3.62294246124247,-31.5291722871855,
124.333656002243));
#117506=CARTESIAN_POINT('Ctrl Pts',(3.61594666024645,-31.5653171195069,
124.429278807524));
#117507=CARTESIAN_POINT('Ctrl Pts',(3.61461564372652,-31.571925071051,124.447739199168));
#117508=CARTESIAN_POINT('Ctrl Pts',(3.61249908784277,-31.5819939093794,
124.477514496356));
#117509=CARTESIAN_POINT('Ctrl Pts',(3.61170677192388,-31.5856626502827,
124.488756610987));
#117510=CARTESIAN_POINT('Ctrl Pts',(3.61020244992106,-31.5924340390956,
124.510280545138));
#117511=CARTESIAN_POINT('Ctrl Pts',(3.60948979264503,-31.595557559744,124.52055511673));
#117512=CARTESIAN_POINT('Ctrl Pts',(3.60785701666444,-31.6025171618662,
124.544269737237));
#117513=CARTESIAN_POINT('Ctrl Pts',(3.6069391864906,-31.6062839330776,124.557729412545));
#117514=CARTESIAN_POINT('Ctrl Pts',(3.60402934103103,-31.6177536012827,
124.600794520789));
#117515=CARTESIAN_POINT('Ctrl Pts',(3.60205796877612,-31.6248109782942,
124.630566376625));
#117516=CARTESIAN_POINT('Ctrl Pts',(3.59740154351628,-31.6397023786624,
124.702112113262));
#117517=CARTESIAN_POINT('Ctrl Pts',(3.59473903422782,-31.6467659725939,
124.744024816263));
#117518=CARTESIAN_POINT('Ctrl Pts',(3.58753414740038,-31.6616820781218,
124.85927527001));
#117519=CARTESIAN_POINT('Ctrl Pts',(3.58305942888017,-31.6662813395355,
124.932935537576));
#117520=CARTESIAN_POINT('Ctrl Pts',(3.57770485414219,-31.6659315276349,
125.020461602146));
#117521=CARTESIAN_POINT('Ctrl Pts',(3.57685924522518,-31.6657048173855,
125.034263500966));
#117522=CARTESIAN_POINT('Ctrl Pts',(3.57149154731326,-31.6631838030986,
125.121616499952));
#117523=CARTESIAN_POINT('Ctrl Pts',(3.56691701269625,-31.6561901805754,
125.194941733526));
#117524=CARTESIAN_POINT('Ctrl Pts',(3.56130952094965,-31.6424037617841,
125.279672333373));
#117525=CARTESIAN_POINT('Ctrl Pts',(3.56050125611048,-31.6402982548054,
125.291767620381));
#117526=CARTESIAN_POINT('Ctrl Pts',(3.55922425009882,-31.6367919619569,
125.310670832005));
#117527=CARTESIAN_POINT('Ctrl Pts',(3.55876038506388,-31.6354818698118,
125.317495420012));
#117528=CARTESIAN_POINT('Ctrl Pts',(3.55788790036956,-31.6329508195242,
125.330248787076));
#117529=CARTESIAN_POINT('Ctrl Pts',(3.55747985514373,-31.6317401968368,
125.336179365369));
#117530=CARTESIAN_POINT('Ctrl Pts',(3.55651370529558,-31.62881033213,125.350143390252));
#117531=CARTESIAN_POINT('Ctrl Pts',(3.55595411610255,-31.6270639564911,
125.358170861749));
#117532=CARTESIAN_POINT('Ctrl Pts',(3.55406966713526,-31.6210161208298,
125.385013300963));
#117533=CARTESIAN_POINT('Ctrl Pts',(3.5527312632936,-31.6164472662686,125.403765602707));
#117534=CARTESIAN_POINT('Ctrl Pts',(3.54939945666924,-31.6043847099869,
125.449783426928));
#117535=CARTESIAN_POINT('Ctrl Pts',(3.54739147488572,-31.5965207720785,
125.476945146376));
#117536=CARTESIAN_POINT('Ctrl Pts',(3.53818985847344,-31.5576797020486,
125.599349262024));
#117537=CARTESIAN_POINT('Ctrl Pts',(3.53082395815422,-31.5188442387067,
125.69188020891));
#117538=CARTESIAN_POINT('Ctrl Pts',(3.5176478774254,-31.4332481974446,125.853332606013));
#117539=CARTESIAN_POINT('Ctrl Pts',(3.51180642270418,-31.3891861688273,
125.923332236672));
#117540=CARTESIAN_POINT('Ctrl Pts',(3.50481129734239,-31.3284587015546,
126.005553494918));
#117541=CARTESIAN_POINT('Ctrl Pts',(3.50348030080581,-31.3165334018153,
126.021117139094));
#117542=CARTESIAN_POINT('Ctrl Pts',(3.50136376888445,-31.2969790596035,
126.045725178207));
#117543=CARTESIAN_POINT('Ctrl Pts',(3.50057145721713,-31.2895238974997,
126.054904715906));
#117544=CARTESIAN_POINT('Ctrl Pts',(3.49906713850575,-31.2751132838785,
126.072267423245));
#117545=CARTESIAN_POINT('Ctrl Pts',(3.49835448031952,-31.2681752410406,
126.080464196953));
#117546=CARTESIAN_POINT('Ctrl Pts',(3.49672169551722,-31.2520260962374,
126.099173318561));
#117547=CARTESIAN_POINT('Ctrl Pts',(3.49580385751861,-31.2427609118106,
126.109638078695));
#117548=CARTESIAN_POINT('Ctrl Pts',(3.49289395899629,-31.2128001999143,
126.142631807354));
#117549=CARTESIAN_POINT('Ctrl Pts',(3.49092254260018,-31.1916147206059,
126.164708683709));
#117550=CARTESIAN_POINT('Ctrl Pts',(3.48626599063703,-31.1395810391596,
126.216024774802));
#117551=CARTESIAN_POINT('Ctrl Pts',(3.4836034005325,-31.1081983106632,126.244691962512));
#117552=CARTESIAN_POINT('Ctrl Pts',(3.47639847013452,-31.0194603774264,
126.31973150444));
#117553=CARTESIAN_POINT('Ctrl Pts',(3.47192378363465,-30.9600698863122,
126.363545703123));
#117554=CARTESIAN_POINT('Ctrl Pts',(3.46656883816062,-30.8863404659918,
126.41072580271));
#117555=CARTESIAN_POINT('Ctrl Pts',(3.46572282856574,-30.8746163232636,
126.418024327502));
#117556=CARTESIAN_POINT('Ctrl Pts',(3.46035522666701,-30.7998608440643,
126.463281358925));
#117557=CARTESIAN_POINT('Ctrl Pts',(3.45578118530074,-30.734471221513,126.497170327168));
#117558=CARTESIAN_POINT('Ctrl Pts',(3.45017424124447,-30.6558157807406,
126.531539223051));
#117559=CARTESIAN_POINT('Ctrl Pts',(3.44936597840817,-30.6445120802031,
126.536330331253));
#117560=CARTESIAN_POINT('Ctrl Pts',(3.44808897488056,-30.6267290162988,
126.543636949745));
#117561=CARTESIAN_POINT('Ctrl Pts',(3.44762511029616,-30.6202848420764,
126.546237692855));
#117562=CARTESIAN_POINT('Ctrl Pts',(3.44675262594267,-30.6081974370016,
126.551028213152));
#117563=CARTESIAN_POINT('Ctrl Pts',(3.44634458060134,-30.602558300073,126.55322764935));
#117564=CARTESIAN_POINT('Ctrl Pts',(3.44537842979062,-30.5892374480436,
126.558339732477));
#117565=CARTESIAN_POINT('Ctrl Pts',(3.44481883974155,-30.5815460365203,
126.56122634244));
#117566=CARTESIAN_POINT('Ctrl Pts',(3.44293438480842,-30.5557143240098,
126.570703695432));
#117567=CARTESIAN_POINT('Ctrl Pts',(3.44159597574447,-30.5374816454557,
126.577035798642));
#117568=CARTESIAN_POINT('Ctrl Pts',(3.4382641532061,-30.4922775556296,126.59185999554));
#117569=CARTESIAN_POINT('Ctrl Pts',(3.43625616056449,-30.4651925495935,
126.599984733842));
#117570=CARTESIAN_POINT('Ctrl Pts',(3.42705444776999,-30.3412882249394,
126.633740547108));
#117571=CARTESIAN_POINT('Ctrl Pts',(3.41968845928897,-30.2424847931028,
126.651298702795));
#117572=CARTESIAN_POINT('Ctrl Pts',(3.40651239856147,-30.0604175165886,
126.666951238755));
#117573=CARTESIAN_POINT('Ctrl Pts',(3.40067104302616,-29.9777114721474,
126.667897967212));
#117574=CARTESIAN_POINT('Ctrl Pts',(3.39367601344119,-29.875698805718,126.661472107613));
#117575=CARTESIAN_POINT('Ctrl Pts',(3.39234501973915,-29.8561552968963,
126.659894306766));
#117576=CARTESIAN_POINT('Ctrl Pts',(3.39022849121663,-29.8248754878884,
126.656812371525));
#117577=CARTESIAN_POINT('Ctrl Pts',(3.38943618015248,-29.8131199549463,
126.655527616931));
#117578=CARTESIAN_POINT('Ctrl Pts',(3.38793186190808,-29.7907169954979,
126.652837541245));
#117579=CARTESIAN_POINT('Ctrl Pts',(3.3872192035928,-29.7800675814883,126.651454224076));
#117580=CARTESIAN_POINT('Ctrl Pts',(3.38558641753944,-29.7555904981363,
126.648033775679));
#117581=CARTESIAN_POINT('Ctrl Pts',(3.3846685784309,-29.7417734770215,126.645925397134));
#117582=CARTESIAN_POINT('Ctrl Pts',(3.38175867238197,-29.6978042794605,
126.638648688608));
#117583=CARTESIAN_POINT('Ctrl Pts',(3.37978724972477,-29.6677661939915,
126.632823525222));
#117584=CARTESIAN_POINT('Ctrl Pts',(3.3751306797895,-29.5964318315708,126.616939685752));
#117585=CARTESIAN_POINT('Ctrl Pts',(3.37246807822157,-29.5553262339756,
126.606121675122));
#117586=CARTESIAN_POINT('Ctrl Pts',(3.36526314165245,-29.4441538842884,
126.572267722166));
#117587=CARTESIAN_POINT('Ctrl Pts',(3.36078845970326,-29.3751324787787,
126.54613441899));
#117588=CARTESIAN_POINT('Ctrl Pts',(3.35133283275612,-29.2345305104796,
126.481940490019));
#117589=CARTESIAN_POINT('Ctrl Pts',(3.34635652891028,-29.1635420043293,
126.443061348241));
#117590=CARTESIAN_POINT('Ctrl Pts',(3.34005347758473,-29.0818343203882,
126.390251401994));
#117591=CARTESIAN_POINT('Ctrl Pts',(3.33897605130137,-29.0681380819878,
126.381108428689));
#117592=CARTESIAN_POINT('Ctrl Pts',(3.33737516673439,-29.0482263438027,
126.367385262525));
#117593=CARTESIAN_POINT('Ctrl Pts',(3.33686156950279,-29.0419030929203,
126.362962163664));
#117594=CARTESIAN_POINT('Ctrl Pts',(3.33594287299062,-29.0307125584315,
126.355018059597));
#117595=CARTESIAN_POINT('Ctrl Pts',(3.33553893870879,-29.0258332618245,
126.351514428391));
#117596=CARTESIAN_POINT('Ctrl Pts',(3.33464067964683,-29.0150740699191,
126.343700139059));
#117597=CARTESIAN_POINT('Ctrl Pts',(3.33414555844965,-29.0092035435339,
126.339377291231));
#117598=CARTESIAN_POINT('Ctrl Pts',(3.3326744102038,-28.9919313533606,126.326482970932));
#117599=CARTESIAN_POINT('Ctrl Pts',(3.33169150373857,-28.9806115199769,
126.317803688489));
#117600=CARTESIAN_POINT('Ctrl Pts',(3.3293903085834,-28.9545851807178,126.297312462731));
#117601=CARTESIAN_POINT('Ctrl Pts',(3.32806622371377,-28.9399652336104,
126.285394102995));
#117602=CARTESIAN_POINT('Ctrl Pts',(3.32334839010026,-28.8890179718232,
126.24240094211));
#117603=CARTESIAN_POINT('Ctrl Pts',(3.31989939184916,-28.8538305107332,
126.210014918448));
#117604=CARTESIAN_POINT('Ctrl Pts',(3.30823783897726,-28.7404211193762,
126.096243905696));
#117605=CARTESIAN_POINT('Ctrl Pts',(3.29998260206738,-28.6690713312461,
126.008426556909));
#117606=CARTESIAN_POINT('Ctrl Pts',(3.28884869862378,-28.5823529747546,
125.876284658765));
#117607=CARTESIAN_POINT('Ctrl Pts',(3.2857149161221,-28.5591060801767,125.837510160612));
#117608=CARTESIAN_POINT('Ctrl Pts',(3.28150576136979,-28.529505610907,125.783248574592));
#117609=CARTESIAN_POINT('Ctrl Pts',(3.28038200205312,-28.5217669450595,
125.768543523804));
#117610=CARTESIAN_POINT('Ctrl Pts',(3.27858897635145,-28.5096890640931,
125.744735467308));
#117611=CARTESIAN_POINT('Ctrl Pts',(3.27791486065339,-28.505210403529,125.735704881014));
#117612=CARTESIAN_POINT('Ctrl Pts',(3.27651932666431,-28.496070304631,125.716847094642));
#117613=CARTESIAN_POINT('Ctrl Pts',(3.27579841013671,-28.4914225744092,
125.707013752518));
#117614=CARTESIAN_POINT('Ctrl Pts',(3.2740979973745,-28.4806387795556,125.683607583983));
#117615=CARTESIAN_POINT('Ctrl Pts',(3.27312145001788,-28.4745877174355,
125.669996447003));
#117616=CARTESIAN_POINT('Ctrl Pts',(3.27026165608738,-28.4572987162818,
125.629658068445));
#117617=CARTESIAN_POINT('Ctrl Pts',(3.26839564415477,-28.4465751377881,
125.602716965642));
#117618=CARTESIAN_POINT('Ctrl Pts',(3.26654944485247,-28.4365599843055,
125.575509615319));
#117619=CARTESIAN_POINT('Origin',(5.,-30.,125.));
#117620=CARTESIAN_POINT('',(2.56904935605388,-28.4365599852179,125.575509617798));
#117621=CARTESIAN_POINT('',(2.75979328931693,-28.4365599629713,125.575509557363));
#117622=CARTESIAN_POINT('',(5.,-28.4365599837785,125.575509613888));
#117623=CARTESIAN_POINT('Ctrl Pts',(2.75979328931693,-28.4365599629713,
125.575509557363));
#117624=CARTESIAN_POINT('Ctrl Pts',(2.76303723577968,-28.4546483265453,
125.624648744461));
#117625=CARTESIAN_POINT('Ctrl Pts',(2.76633054043747,-28.4750492326942,
125.672923875654));
#117626=CARTESIAN_POINT('Ctrl Pts',(2.7706819059645,-28.5039739496871,125.733261737967));
#117627=CARTESIAN_POINT('Ctrl Pts',(2.7716343813265,-28.5104195017411,125.746268466288));
#117628=CARTESIAN_POINT('Ctrl Pts',(2.77308356141338,-28.5203797917236,
125.765724460543));
#117629=CARTESIAN_POINT('Ctrl Pts',(2.77357288732662,-28.5237687615016,
125.77223781026));
#117630=CARTESIAN_POINT('Ctrl Pts',(2.77446743413919,-28.5300081696669,
125.784038326005));
#117631=CARTESIAN_POINT('Ctrl Pts',(2.77487177096086,-28.5328442928684,
125.789332759664));
#117632=CARTESIAN_POINT('Ctrl Pts',(2.77579597963266,-28.5393629527035,
125.801345185537));
#117633=CARTESIAN_POINT('Ctrl Pts',(2.77631692712918,-28.5430632194322,
125.808053155397));
#117634=CARTESIAN_POINT('Ctrl Pts',(2.77794519969519,-28.5547128226005,
125.828831799026));
#117635=CARTESIAN_POINT('Ctrl Pts',(2.77906167589533,-28.562820457572,125.842812013932));
#117636=CARTESIAN_POINT('Ctrl Pts',(2.78665470255186,-28.6188382658271,
125.936245944434));
#117637=CARTESIAN_POINT('Ctrl Pts',(2.79342359513652,-28.6731064091108,
126.011688978999));
#117638=CARTESIAN_POINT('Ctrl Pts',(2.80888647816696,-28.8111140384918,
126.173214271089));
#117639=CARTESIAN_POINT('Ctrl Pts',(2.81750623029459,-28.8984566979736,
126.255585129596));
#117640=CARTESIAN_POINT('Ctrl Pts',(2.82718609808875,-29.0109076803959,
126.340786439122));
#117641=CARTESIAN_POINT('Ctrl Pts',(2.82863849244357,-29.0281730411125,
126.353352994413));
#117642=CARTESIAN_POINT('Ctrl Pts',(2.83090048200251,-29.0556732312801,
126.372571204452));
#117643=CARTESIAN_POINT('Ctrl Pts',(2.8317185857514,-29.0657471791156,126.379447874255));
#117644=CARTESIAN_POINT('Ctrl Pts',(2.8332449232388,-29.0847787417583,126.39213505717));
#117645=CARTESIAN_POINT('Ctrl Pts',(2.83395409627308,-29.0937183949588,
126.397971255201));
#117646=CARTESIAN_POINT('Ctrl Pts',(2.83554318125725,-29.1139651043763,
126.410913351021));
#117647=CARTESIAN_POINT('Ctrl Pts',(2.83642124444281,-29.1253028258325,
126.417970095287));
#117648=CARTESIAN_POINT('Ctrl Pts',(2.83867401517774,-29.1547682521237,
126.435821847576));
#117649=CARTESIAN_POINT('Ctrl Pts',(2.8400412707289,-29.1730186891746,126.446410405486));
#117650=CARTESIAN_POINT('Ctrl Pts',(2.85100218251702,-29.322122896621,126.529172794167));
#117651=CARTESIAN_POINT('Ctrl Pts',(2.85991699057071,-29.4619359898843,
126.583785188738));
#117652=CARTESIAN_POINT('Ctrl Pts',(2.87288408100499,-29.6664043028776,
126.63339711441));
#117653=CARTESIAN_POINT('Ctrl Pts',(2.8766911564648,-29.7263844408796,126.644507576731));
#117654=CARTESIAN_POINT('Ctrl Pts',(2.88163859224958,-29.8019455984172,
126.654255934489));
#117655=CARTESIAN_POINT('Ctrl Pts',(2.88263743899645,-29.8170852406489,
126.655998307196));
#117656=CARTESIAN_POINT('Ctrl Pts',(2.88414310800062,-29.8396927948922,
126.658286351301));
#117657=CARTESIAN_POINT('Ctrl Pts',(2.88464166978938,-29.8471444153487,
126.658989809426));
#117658=CARTESIAN_POINT('Ctrl Pts',(2.88554515627021,-29.8605805798354,
126.660166938295));
#117659=CARTESIAN_POINT('Ctrl Pts',(2.88594908919052,-29.8665632881203,
126.66065850754));
#117660=CARTESIAN_POINT('Ctrl Pts',(2.88686228370704,-29.8800336942816,
126.661692041892));
#117661=CARTESIAN_POINT('Ctrl Pts',(2.88737250561811,-29.8875224131172,
126.662215733161));
#117662=CARTESIAN_POINT('Ctrl Pts',(2.88893419636274,-29.910337954678,126.663656355837));
#117663=CARTESIAN_POINT('Ctrl Pts',(2.88999381456226,-29.9256736535506,
126.664411999825));
#117664=CARTESIAN_POINT('Ctrl Pts',(2.89849926954696,-30.0477938556502,
126.668738257653));
#117665=CARTESIAN_POINT('Ctrl Pts',(2.90633703524342,-30.1546782396629,
126.662240304402));
#117666=CARTESIAN_POINT('Ctrl Pts',(2.92182256375358,-30.3651432359935,
126.628961598417));
#117667=CARTESIAN_POINT('Ctrl Pts',(2.92943272492981,-30.4682792175521,
126.602363042429));
#117668=CARTESIAN_POINT('Ctrl Pts',(2.93821829738369,-30.5885916222314,
126.558713180971));
#117669=CARTESIAN_POINT('Ctrl Pts',(2.93969491328196,-30.6088445811729,
126.550914321091));
#117670=CARTESIAN_POINT('Ctrl Pts',(2.94198580975405,-30.6403018166897,
126.538089764389));
#117671=CARTESIAN_POINT('Ctrl Pts',(2.9428089637918,-30.6516121229509,126.533332382412));
#117672=CARTESIAN_POINT('Ctrl Pts',(2.94433990679496,-30.6726562443397,
126.524205819835));
#117673=CARTESIAN_POINT('Ctrl Pts',(2.94504868964055,-30.682402574858,126.519867276819));
#117674=CARTESIAN_POINT('Ctrl Pts',(2.94663073617421,-30.7041599715204,
126.509930566909));
#117675=CARTESIAN_POINT('Ctrl Pts',(2.94750222340795,-30.7161473621253,
126.504282072947));
#117676=CARTESIAN_POINT('Ctrl Pts',(2.94972589219146,-30.7467265634955,
126.489424667644));
#117677=CARTESIAN_POINT('Ctrl Pts',(2.95107095081675,-30.7652163918327,
126.480010248559));
#117678=CARTESIAN_POINT('Ctrl Pts',(2.96212269049807,-30.9168808117756,
126.399185326102));
#117679=CARTESIAN_POINT('Ctrl Pts',(2.97113055886323,-31.0399406938127,
126.310310959368));
#117680=CARTESIAN_POINT('Ctrl Pts',(2.98415461116663,-31.192850805905,126.164592670322));
#117681=CARTESIAN_POINT('Ctrl Pts',(2.98791110691808,-31.2340849480302,
126.120804152586));
#117682=CARTESIAN_POINT('Ctrl Pts',(2.9927978158539,-31.2826277639255,126.063320871063));
#117683=CARTESIAN_POINT('Ctrl Pts',(2.9937903628562,-31.2922381549223,126.051620543336));
#117684=CARTESIAN_POINT('Ctrl Pts',(2.99528836821473,-31.3063468530237,
126.03395823717));
#117685=CARTESIAN_POINT('Ctrl Pts',(2.99578568858537,-31.310967002989,126.02809398809));
#117686=CARTESIAN_POINT('Ctrl Pts',(2.99668794986928,-31.3192308556153,
126.017458593071));
#117687=CARTESIAN_POINT('Ctrl Pts',(2.99709191338061,-31.3228883961609,
126.012698537217));
#117688=CARTESIAN_POINT('Ctrl Pts',(2.99800648412334,-31.3310737207185,
126.001925845536));
#117689=CARTESIAN_POINT('Ctrl Pts',(2.99851806637632,-31.3355864978393,
125.995902279951));
#117690=CARTESIAN_POINT('Ctrl Pts',(3.00008810806472,-31.3492408612435,
125.977416984754));
#117691=CARTESIAN_POINT('Ctrl Pts',(3.00115483941066,-31.3582496934169,
125.964858845395));
#117692=CARTESIAN_POINT('Ctrl Pts',(3.00954132285919,-31.4271006533988,
125.866006594887));
#117693=CARTESIAN_POINT('Ctrl Pts',(3.01723931917393,-31.4788324081438,
125.774361024761));
#117694=CARTESIAN_POINT('Ctrl Pts',(3.03286601043087,-31.566374232507,125.578031377637));
#117695=CARTESIAN_POINT('Ctrl Pts',(3.04074435836625,-31.6011104510511,
125.473394065915));
#117696=CARTESIAN_POINT('Ctrl Pts',(3.04969298501259,-31.6298020047711,
125.346012365552));
#117697=CARTESIAN_POINT('Ctrl Pts',(3.05109103788851,-31.6339501264954,
125.325862212821));
#117698=CARTESIAN_POINT('Ctrl Pts',(3.05328806407711,-31.6399315242076,
125.293811785721));
#117699=CARTESIAN_POINT('Ctrl Pts',(3.05409475028053,-31.6420107357334,
125.281960150391));
#117700=CARTESIAN_POINT('Ctrl Pts',(3.05561105901622,-31.6456959110216,
125.259529261526));
#117701=CARTESIAN_POINT('Ctrl Pts',(3.05632149497792,-31.6473286971399,
125.248955100047));
#117702=CARTESIAN_POINT('Ctrl Pts',(3.05792837934829,-31.6508067561278,
125.224896143383));
#117703=CARTESIAN_POINT('Ctrl Pts',(3.05882279918665,-31.6525888963804,
125.211402883611));
#117704=CARTESIAN_POINT('Ctrl Pts',(3.06114848406786,-31.6568161582198,
125.176066097184));
#117705=CARTESIAN_POINT('Ctrl Pts',(3.06257144218391,-31.6589947738764,
125.154192946908));
#117706=CARTESIAN_POINT('Ctrl Pts',(3.07129303488564,-31.669782835021,125.018754025983));
#117707=CARTESIAN_POINT('Ctrl Pts',(3.07823001012504,-31.6671616317556,
124.904595001293));
#117708=CARTESIAN_POINT('Ctrl Pts',(3.09106482445217,-31.6408724091839,
124.696097335447));
#117709=CARTESIAN_POINT('Ctrl Pts',(3.09694266222433,-31.6205819418205,
124.601843979847));
#117710=CARTESIAN_POINT('Ctrl Pts',(3.10413444886149,-31.5880596548816,
124.496186641115));
#117711=CARTESIAN_POINT('Ctrl Pts',(3.10507502122013,-31.5836673728014,
124.482545667123));
#117712=CARTESIAN_POINT('Ctrl Pts',(3.10650967241133,-31.5767713247972,
124.462039448031));
#117713=CARTESIAN_POINT('Ctrl Pts',(3.10699659132192,-31.5743973297258,
124.455130832859));
#117714=CARTESIAN_POINT('Ctrl Pts',(3.10788888020944,-31.5699881132764,
124.442568905563));
#117715=CARTESIAN_POINT('Ctrl Pts',(3.10829339451344,-31.5679676445182,
124.43691069709));
#117716=CARTESIAN_POINT('Ctrl Pts',(3.10922079153111,-31.5632864158377,
124.424021751059));
#117717=CARTESIAN_POINT('Ctrl Pts',(3.10974478238464,-31.5606060849227,
124.416798488511));
#117718=CARTESIAN_POINT('Ctrl Pts',(3.11139226506257,-31.5520658880556,
124.394263873374));
#117719=CARTESIAN_POINT('Ctrl Pts',(3.11252520759992,-31.546030253153,124.37902078772));
#117720=CARTESIAN_POINT('Ctrl Pts',(3.11968339923107,-31.5068308287761,
124.284137456742));
#117721=CARTESIAN_POINT('Ctrl Pts',(3.1259604110031,-31.4677503881054,124.207091174072));
#117722=CARTESIAN_POINT('Ctrl Pts',(3.13853769810426,-31.3778793126392,
124.059526098402));
#117723=CARTESIAN_POINT('Ctrl Pts',(3.14481785445178,-31.3271802787721,
123.989238982583));
#117724=CARTESIAN_POINT('Ctrl Pts',(3.15436579044093,-31.2397668605522,
123.886040319072));
#117725=CARTESIAN_POINT('Ctrl Pts',(3.15774782496874,-31.2066710245822,
123.850272246344));
#117726=CARTESIAN_POINT('Ctrl Pts',(3.16219141597261,-31.1602912437535,
123.804360383796));
#117727=CARTESIAN_POINT('Ctrl Pts',(3.16331054781866,-31.1483571435837,
123.79289363879));
#117728=CARTESIAN_POINT('Ctrl Pts',(3.16517336737757,-31.1280718939009,
123.773975951726));
#117729=CARTESIAN_POINT('Ctrl Pts',(3.16592117269069,-31.1198131836275,
123.766428109485));
#117730=CARTESIAN_POINT('Ctrl Pts',(3.16739244875795,-31.1033386864626,
123.751673457782));
#117731=CARTESIAN_POINT('Ctrl Pts',(3.16811604407364,-31.0951267901952,
123.744463168161));
#117732=CARTESIAN_POINT('Ctrl Pts',(3.16987650177474,-31.074883982123,123.727039096408));
#117733=CARTESIAN_POINT('Ctrl Pts',(3.17090968656239,-31.0627775933392,
123.716914323882));
#117734=CARTESIAN_POINT('Ctrl Pts',(3.17449247680874,-31.0200285212339,
123.682182815405));
#117735=CARTESIAN_POINT('Ctrl Pts',(3.17700613153684,-30.9886593561573,
123.65848840083));
#117736=CARTESIAN_POINT('Ctrl Pts',(3.18695772998778,-30.859551855189,123.567959220499));
#117737=CARTESIAN_POINT('Ctrl Pts',(3.19407110799303,-30.7556585173268,
123.510519760892));
#117738=CARTESIAN_POINT('Ctrl Pts',(3.20543037199233,-30.5853175200925,
123.438790895298));
#117739=CARTESIAN_POINT('Ctrl Pts',(3.20956163794169,-30.5226023275228,
123.416694806712));
#117740=CARTESIAN_POINT('Ctrl Pts',(3.21489817815105,-30.4435076682524,
123.394039813981));
#117741=CARTESIAN_POINT('Ctrl Pts',(3.21593601011778,-30.4282111414821,
123.389893685387));
#117742=CARTESIAN_POINT('Ctrl Pts',(3.21748902981047,-30.4054937158935,
123.384082726381));
#117743=CARTESIAN_POINT('Ctrl Pts',(3.21799518012268,-30.3981163137638,
123.382249344336));
#117744=CARTESIAN_POINT('Ctrl Pts',(3.21890629753049,-30.3848897441146,
123.379058317125));
#117745=CARTESIAN_POINT('Ctrl Pts',(3.21931018559243,-30.3790454227592,
123.377681714563));
#117746=CARTESIAN_POINT('Ctrl Pts',(3.22021559204696,-30.3659867841699,
123.374680229223));
#117747=CARTESIAN_POINT('Ctrl Pts',(3.22071798560091,-30.358769098873,123.373071786491));
#117748=CARTESIAN_POINT('Ctrl Pts',(3.22223212381146,-30.3370935583827,
123.368392696824));
#117749=CARTESIAN_POINT('Ctrl Pts',(3.22325133687287,-30.3226057435778,
123.365466440969));
#117750=CARTESIAN_POINT('Ctrl Pts',(3.23212354858208,-30.1972125092384,
123.341871417778));
#117751=CARTESIAN_POINT('Ctrl Pts',(3.24041737436664,-30.0845200328496,
123.332326168378));
#117752=CARTESIAN_POINT('Ctrl Pts',(3.25503508915634,-29.8832117013865,
123.335741756485));
#117753=CARTESIAN_POINT('Ctrl Pts',(3.26138040624311,-29.7949363292103,
123.344298365489));
#117754=CARTESIAN_POINT('Ctrl Pts',(3.26956477278181,-29.6787015467723,
123.365009530248));
#117755=CARTESIAN_POINT('Ctrl Pts',(3.27158688540903,-29.6497954147557,
123.370956270561));
#117756=CARTESIAN_POINT('Ctrl Pts',(3.27451836075723,-29.6076350878411,
123.380803946309));
#117757=CARTESIAN_POINT('Ctrl Pts',(3.27544651154424,-29.5942484564904,
123.384106504325));
#117758=CARTESIAN_POINT('Ctrl Pts',(3.27708671680372,-29.5705303573283,
123.390271231361));
#117759=CARTESIAN_POINT('Ctrl Pts',(3.27780084133571,-29.5601827666061,
123.393067614056));
#117760=CARTESIAN_POINT('Ctrl Pts',(3.2793030203289,-29.5383763515598,123.399187102454));
#117761=CARTESIAN_POINT('Ctrl Pts',(3.2800902642641,-29.526924742605,123.402533837904));
#117762=CARTESIAN_POINT('Ctrl Pts',(3.28219261162426,-29.4962893596308,
123.411845364699));
#117763=CARTESIAN_POINT('Ctrl Pts',(3.28350036576453,-29.4771755042877,
123.418034716562));
#117764=CARTESIAN_POINT('Ctrl Pts',(3.29110903947386,-29.3657587148261,
123.456353179857));
#117765=CARTESIAN_POINT('Ctrl Pts',(3.29714414454831,-29.2763107966007,
123.496209819013));
#117766=CARTESIAN_POINT('Ctrl Pts',(3.30753287686947,-29.1278328355663,
123.578704881674));
#117767=CARTESIAN_POINT('Ctrl Pts',(3.31190565576419,-29.0671441417323,
123.617779124584));
#117768=CARTESIAN_POINT('Ctrl Pts',(3.31965788762433,-28.9668560906495,
123.691970440996));
#117769=CARTESIAN_POINT('Ctrl Pts',(3.32298359356863,-28.9260444377097,
123.725266327141));
#117770=CARTESIAN_POINT('Ctrl Pts',(3.32718149695955,-28.8783324892821,
123.768111196788));
#117771=CARTESIAN_POINT('Ctrl Pts',(3.32793931228265,-28.8698631883654,
123.775876314673));
#117772=CARTESIAN_POINT('Ctrl Pts',(3.32914963445409,-28.8565772762266,
123.788312959258));
#117773=CARTESIAN_POINT('Ctrl Pts',(3.32959796612986,-28.8517072234968,
123.792927216193));
#117774=CARTESIAN_POINT('Ctrl Pts',(3.33046034977326,-28.8424407088608,
123.801813842122));
#117775=CARTESIAN_POINT('Ctrl Pts',(3.33087403725293,-28.838039774063,123.806081238236));
#117776=CARTESIAN_POINT('Ctrl Pts',(3.33188076421478,-28.8274346961004,
123.816478695595));
#117777=CARTESIAN_POINT('Ctrl Pts',(3.33247565728877,-28.8212550014351,
123.822633323954));
#117778=CARTESIAN_POINT('Ctrl Pts',(3.33450925422983,-28.8004148341158,
123.843717486912));
#117779=CARTESIAN_POINT('Ctrl Pts',(3.33596378607817,-28.7859880532031,
123.858873926947));
#117780=CARTESIAN_POINT('Ctrl Pts',(3.34490328341289,-28.6999851259749,
123.9527036415));
#117781=CARTESIAN_POINT('Ctrl Pts',(3.35272158264864,-28.6357965609123,
124.037807141351));
#117782=CARTESIAN_POINT('Ctrl Pts',(3.36756449678118,-28.5287667472807,
124.212167569368));
#117783=CARTESIAN_POINT('Ctrl Pts',(3.37457575800662,-28.4848717773251,
124.300286083396));
#117784=CARTESIAN_POINT('Ctrl Pts',(3.38280003822794,-28.4411231274983,
124.411847118787));
#117785=CARTESIAN_POINT('Ctrl Pts',(3.38426706216923,-28.4336414058478,
124.432072411769));
#117786=CARTESIAN_POINT('Ctrl Pts',(3.38654651510395,-28.4225309915491,
124.463998730343));
#117787=CARTESIAN_POINT('Ctrl Pts',(3.38736767229037,-28.4186353134346,
124.475603608291));
#117788=CARTESIAN_POINT('Ctrl Pts',(3.3888967829006,-28.4115836232334,124.49740346241));
#117789=CARTESIAN_POINT('Ctrl Pts',(3.38960570869245,-28.408397003706,124.507587797854));
#117790=CARTESIAN_POINT('Ctrl Pts',(3.39119048212472,-28.4014615886841,
124.530524130972));
#117791=CARTESIAN_POINT('Ctrl Pts',(3.39206452519877,-28.3977670719286,
124.54329188173));
#117792=CARTESIAN_POINT('Ctrl Pts',(3.39429949116731,-28.3886616688604,
124.576230189131));
#117793=CARTESIAN_POINT('Ctrl Pts',(3.39565316420881,-28.38347642017,124.596461094854));
#117794=CARTESIAN_POINT('Ctrl Pts',(3.40532389064964,-28.3488784010632,
124.742840270653));
#117795=CARTESIAN_POINT('Ctrl Pts',(3.41315087624358,-28.3338853611642,
124.871939983007));
#117796=CARTESIAN_POINT('Ctrl Pts',(3.42169050166202,-28.3340095611656,
125.011483767236));
#117797=CARTESIAN_POINT('Ctrl Pts',(3.42230320369506,-28.3341085155098,
125.021484389441));
#117798=CARTESIAN_POINT('Ctrl Pts',(3.42757183754949,-28.3357308221565,
125.107316137673));
#117799=CARTESIAN_POINT('Ctrl Pts',(3.43227943676868,-28.3423408481876,
125.182953074876));
#117800=CARTESIAN_POINT('Ctrl Pts',(3.43803507207486,-28.355979408971,125.270006104254));
#117801=CARTESIAN_POINT('Ctrl Pts',(3.4388440434325,-28.3580155855769,125.282124371585));
#117802=CARTESIAN_POINT('Ctrl Pts',(3.44012201179036,-28.3614134660585,
125.301062311549));
#117803=CARTESIAN_POINT('Ctrl Pts',(3.44058612265394,-28.3626841874184,
125.307898148971));
#117804=CARTESIAN_POINT('Ctrl Pts',(3.44145896183371,-28.3651414399192,
125.320671402663));
#117805=CARTESIAN_POINT('Ctrl Pts',(3.44186711410878,-28.3663175964764,
125.326610562742));
#117806=CARTESIAN_POINT('Ctrl Pts',(3.44283338866173,-28.3691659644831,
125.340593371787));
#117807=CARTESIAN_POINT('Ctrl Pts',(3.44339299472492,-28.3708653306969,
125.348631207018));
#117808=CARTESIAN_POINT('Ctrl Pts',(3.4452769512217,-28.3767542662811,125.375501676292));
#117809=CARTESIAN_POINT('Ctrl Pts',(3.44661483323226,-28.3812113386784,
125.394273270264));
#117810=CARTESIAN_POINT('Ctrl Pts',(3.44994489161394,-28.3929973763394,
125.44033740325));
#117811=CARTESIAN_POINT('Ctrl Pts',(3.45195162577028,-28.4006965880919,
125.467528477889));
#117812=CARTESIAN_POINT('Ctrl Pts',(3.45602015148294,-28.4175507825368,
125.521751199743));
#117813=CARTESIAN_POINT('Ctrl Pts',(3.45808086076826,-28.4267133184061,
125.548759974138));
#117814=CARTESIAN_POINT('Ctrl Pts',(3.46014888220092,-28.4365599331867,
125.575509476449));
#117815=CARTESIAN_POINT('',(3.23000357748363,-28.3339996803007,124.999395781857));
#117816=CARTESIAN_POINT('Ctrl Pts',(3.26654944485247,-28.4365599843055,
125.575509615319));
#117817=CARTESIAN_POINT('Ctrl Pts',(3.26608922769779,-28.4340634253296,
125.568727417246));
#117818=CARTESIAN_POINT('Ctrl Pts',(3.26563023416981,-28.4316108879902,
125.561928675024));
#117819=CARTESIAN_POINT('Ctrl Pts',(3.26175558114333,-28.4112291570977,
125.504254788388));
#117820=CARTESIAN_POINT('Ctrl Pts',(3.2584081392242,-28.3957355881006,125.452550575385));
#117821=CARTESIAN_POINT('Ctrl Pts',(3.25136299090292,-28.3682060469397,
125.341297853109));
#117822=CARTESIAN_POINT('Ctrl Pts',(3.24767920080253,-28.356861969498,125.281661433611));
#117823=CARTESIAN_POINT('Ctrl Pts',(3.23940931230418,-28.3389145332975,
125.14789329267));
#117824=CARTESIAN_POINT('Ctrl Pts',(3.23481638056788,-28.3339731665333,
125.073679451112));
#117825=CARTESIAN_POINT('Ctrl Pts',(3.23000431809184,-28.334000109585,124.999395734044));
#117826=CARTESIAN_POINT('Ctrl Pts',(3.23000443222266,-28.3340001089469,
124.99939749588));
#117827=CARTESIAN_POINT('Ctrl Pts',(3.22944765207874,-28.3340032173081,
124.99080248525));
#117828=CARTESIAN_POINT('Ctrl Pts',(3.22888799167503,-28.3340728389642,
124.982207796535));
#117829=CARTESIAN_POINT('Ctrl Pts',(3.22781269690895,-28.334332897955,124.965789723787));
#117830=CARTESIAN_POINT('Ctrl Pts',(3.22729762093207,-28.3345119609543,
124.957966394242));
#117831=CARTESIAN_POINT('Ctrl Pts',(3.22636905139114,-28.3349318006083,
124.943942991113));
#117832=CARTESIAN_POINT('Ctrl Pts',(3.22595661885278,-28.3351521138087,
124.937742392473));
#117833=CARTESIAN_POINT('Ctrl Pts',(3.22516382038836,-28.3356399400738,
124.925880411748));
#117834=CARTESIAN_POINT('Ctrl Pts',(3.22478376786043,-28.3359017200144,
124.920218825853));
#117835=CARTESIAN_POINT('Ctrl Pts',(3.22396282176298,-28.3365268562504,
124.908045476843));
#117836=CARTESIAN_POINT('Ctrl Pts',(3.22352142450034,-28.3368995659726,
124.90153438694));
#117837=CARTESIAN_POINT('Ctrl Pts',(3.22235463998572,-28.337980836864,124.884408105469));
#117838=CARTESIAN_POINT('Ctrl Pts',(3.22162591865072,-28.3387528541982,
124.873797422681));
#117839=CARTESIAN_POINT('Ctrl Pts',(3.21840447577815,-28.3425894175858,
124.827233785174));
#117840=CARTESIAN_POINT('Ctrl Pts',(3.21586248797687,-28.3467197210186,
124.791380994332));
#117841=CARTESIAN_POINT('Ctrl Pts',(3.20675625161801,-28.3654318790196,
124.665156461374));
#117842=CARTESIAN_POINT('Ctrl Pts',(3.20003860255776,-28.3862911370221,
124.575881812017));
#117843=CARTESIAN_POINT('Ctrl Pts',(3.18870595356972,-28.4342797884443,
124.427039702591));
#117844=CARTESIAN_POINT('Ctrl Pts',(3.18405531527007,-28.4577736244841,
124.366515535751));
#117845=CARTESIAN_POINT('Ctrl Pts',(3.17755872570092,-28.4962789591194,
124.282260673336));
#117846=CARTESIAN_POINT('Ctrl Pts',(3.175630798603,-28.5084482323227,124.25730208862));
#117847=CARTESIAN_POINT('Ctrl Pts',(3.17219748904402,-28.5314683041218,
124.212939537316));
#117848=CARTESIAN_POINT('Ctrl Pts',(3.17068499063485,-28.5420941575238,
124.193426909159));
#117849=CARTESIAN_POINT('Ctrl Pts',(3.1683514925556,-28.5592417593999,124.163384905577));
#117850=CARTESIAN_POINT('Ctrl Pts',(3.16752106545981,-28.5654956362802,
124.152706444695));
#117851=CARTESIAN_POINT('Ctrl Pts',(3.16598356732774,-28.5773551536463,
124.132964139113));
#117852=CARTESIAN_POINT('Ctrl Pts',(3.1652754226223,-28.582929862062,124.123882555756));
#117853=CARTESIAN_POINT('Ctrl Pts',(3.16370355342378,-28.5955531094982,
124.103754150159));
#117854=CARTESIAN_POINT('Ctrl Pts',(3.16284150333715,-28.6026456673121,
124.092735663181));
#117855=CARTESIAN_POINT('Ctrl Pts',(3.16065891811887,-28.6210299769782,
124.064902215425));
#117856=CARTESIAN_POINT('Ctrl Pts',(3.159345056047,-28.632499902251,124.04820709676));
#117857=CARTESIAN_POINT('Ctrl Pts',(3.14935022289263,-28.7227633509899,
123.921824962499));
#117858=CARTESIAN_POINT('Ctrl Pts',(3.14121161098739,-28.8143249215306,
123.821877307221));
#117859=CARTESIAN_POINT('Ctrl Pts',(3.12950949166578,-28.9594687004654,
123.697701675156));
#117860=CARTESIAN_POINT('Ctrl Pts',(3.12605852812399,-29.0037845957564,
123.663496988023));
#117861=CARTESIAN_POINT('Ctrl Pts',(3.12056433444249,-29.0749099493234,
123.614105370924));
#117862=CARTESIAN_POINT('Ctrl Pts',(3.11859088267162,-29.1005623311369,
123.597321446204));
#117863=CARTESIAN_POINT('Ctrl Pts',(3.11593372863336,-29.1349728163845,
123.576139319918));
#117864=CARTESIAN_POINT('Ctrl Pts',(3.1152877027733,-29.1433291697959,123.571096104715));
#117865=CARTESIAN_POINT('Ctrl Pts',(3.11421497743865,-29.1571781164444,
123.562903150098));
#117866=CARTESIAN_POINT('Ctrl Pts',(3.11379096471093,-29.1626453600842,
123.559710693161));
#117867=CARTESIAN_POINT('Ctrl Pts',(3.11298645255106,-29.1730026787887,
123.553741706294));
#117868=CARTESIAN_POINT('Ctrl Pts',(3.11260639591673,-29.1778888863421,
123.55095861487));
#117869=CARTESIAN_POINT('Ctrl Pts',(3.11159165561475,-29.1909197475348,
123.543623606031));
#117870=CARTESIAN_POINT('Ctrl Pts',(3.11095431455985,-29.1990885674555,
123.539115362905));
#117871=CARTESIAN_POINT('Ctrl Pts',(3.10859503984988,-29.2292855036084,
123.522779537778));
#117872=CARTESIAN_POINT('Ctrl Pts',(3.10684997113187,-29.2515400644324,
123.511380272746));
#117873=CARTESIAN_POINT('Ctrl Pts',(3.09710823055981,-29.3757527453012,
123.451245228638));
#117874=CARTESIAN_POINT('Ctrl Pts',(3.08877653802414,-29.4822062905465,
123.412481624518));
#117875=CARTESIAN_POINT('Ctrl Pts',(3.0762739792328,-29.6498767610489,123.370103398674));
#117876=CARTESIAN_POINT('Ctrl Pts',(3.07199006260309,-29.708747569502,123.358560858257));
#117877=CARTESIAN_POINT('Ctrl Pts',(3.06507128106493,-29.8066310188968,
123.344803026003));
#117878=CARTESIAN_POINT('Ctrl Pts',(3.06238730485174,-29.8453246685053,
123.340739755491));
#117879=CARTESIAN_POINT('Ctrl Pts',(3.05870646566697,-29.8993808422484,
123.33697096679));
#117880=CARTESIAN_POINT('Ctrl Pts',(3.05767442569999,-29.914648029691,123.336117537671));
#117881=CARTESIAN_POINT('Ctrl Pts',(3.05591492279765,-29.9408601509746,
123.335014035461));
#117882=CARTESIAN_POINT('Ctrl Pts',(3.05518430783682,-29.9517995353801,
123.334661443155));
#117883=CARTESIAN_POINT('Ctrl Pts',(3.05370418021214,-29.9740691671504,
123.334163283902));
#117884=CARTESIAN_POINT('Ctrl Pts',(3.05295494718087,-29.9853990248037,
123.334025451862));
#117885=CARTESIAN_POINT('Ctrl Pts',(3.05107334301465,-30.0139893152647,
123.333969329119));
#117886=CARTESIAN_POINT('Ctrl Pts',(3.04994576544092,-30.0312489693785,
123.334203663239));
#117887=CARTESIAN_POINT('Ctrl Pts',(3.04551733134659,-30.0994837089373,
123.33619102974));
#117888=CARTESIAN_POINT('Ctrl Pts',(3.04228052562196,-30.150373106521,123.340016267766));
#117889=CARTESIAN_POINT('Ctrl Pts',(3.03175858757404,-30.3175008056871,
123.360329421028));
#117890=CARTESIAN_POINT('Ctrl Pts',(3.0247352411413,-30.4321639410099,123.386754836161));
#117891=CARTESIAN_POINT('Ctrl Pts',(3.0149957152648,-30.5809785240957,123.438069938713));
#117892=CARTESIAN_POINT('Ctrl Pts',(3.01248945811593,-30.618373150999,123.4524936875));
#117893=CARTESIAN_POINT('Ctrl Pts',(3.00834972853951,-30.6778966753075,
123.477954989147));
#117894=CARTESIAN_POINT('Ctrl Pts',(3.00675124647266,-30.7003646194376,
123.488161991748));
#117895=CARTESIAN_POINT('Ctrl Pts',(3.00453040013058,-30.7307292238523,
123.502778481542));
#117896=CARTESIAN_POINT('Ctrl Pts',(3.00393190845015,-30.7388301149392,
123.506759387757));
#117897=CARTESIAN_POINT('Ctrl Pts',(3.002916700434,-30.7524250303608,123.513577850802));
#117898=CARTESIAN_POINT('Ctrl Pts',(3.00250210054275,-30.7579364831412,
123.516380602017));
#117899=CARTESIAN_POINT('Ctrl Pts',(3.00164141584703,-30.7692912746533,
123.522234663947));
#117900=CARTESIAN_POINT('Ctrl Pts',(3.00119510237882,-30.7751322643815,
123.525290054752));
#117901=CARTESIAN_POINT('Ctrl Pts',(3.00000124373214,-30.7906357325751,
123.533517388024));
#117902=CARTESIAN_POINT('Ctrl Pts',(2.99925009251312,-30.8002653759703,
123.53875004711));
#117903=CARTESIAN_POINT('Ctrl Pts',(2.99576166307805,-30.8444458914135,
123.563325012214));
#117904=CARTESIAN_POINT('Ctrl Pts',(2.99296494096236,-30.8783492785341,
123.583798786644));
#117905=CARTESIAN_POINT('Ctrl Pts',(2.98356991448956,-30.9882449259592,
123.655627833474));
#117906=CARTESIAN_POINT('Ctrl Pts',(2.97683741232306,-31.0607272402754,
123.712047354065));
#117907=CARTESIAN_POINT('Ctrl Pts',(2.96570787016637,-31.1738806301788,
123.816186362098));
#117908=CARTESIAN_POINT('Ctrl Pts',(2.96126455456212,-31.2171805883191,
123.860753227679));
#117909=CARTESIAN_POINT('Ctrl Pts',(2.95502073909017,-31.2756190494248,
123.928047229529));
#117910=CARTESIAN_POINT('Ctrl Pts',(2.95314517855461,-31.2928444983341,
123.948886330292));
#117911=CARTESIAN_POINT('Ctrl Pts',(2.94979521966981,-31.3230090925628,
123.987243088179));
#117912=CARTESIAN_POINT('Ctrl Pts',(2.94831421059811,-31.3361261673319,
124.004612354817));
#117913=CARTESIAN_POINT('Ctrl Pts',(2.94601823454732,-31.356106917401,124.032177271664));
#117914=CARTESIAN_POINT('Ctrl Pts',(2.94519432558859,-31.3632041392255,
124.042199763156));
#117915=CARTESIAN_POINT('Ctrl Pts',(2.94366292850998,-31.376255777431,124.061069897053));
#117916=CARTESIAN_POINT('Ctrl Pts',(2.94295443620894,-31.3822372742697,
124.069897946572));
#117917=CARTESIAN_POINT('Ctrl Pts',(2.94137425400026,-31.3954472966771,
124.089803438395));
#117918=CARTESIAN_POINT('Ctrl Pts',(2.9405043252574,-31.4026295443798,124.100910840577));
#117919=CARTESIAN_POINT('Ctrl Pts',(2.93828704686988,-31.4206954743156,
124.129593398409));
#117920=CARTESIAN_POINT('Ctrl Pts',(2.93694675193302,-31.4313859126302,
124.147288025016));
#117921=CARTESIAN_POINT('Ctrl Pts',(2.92587605213686,-31.5176403004289,
124.296250024484));
#117922=CARTESIAN_POINT('Ctrl Pts',(2.91684869953472,-31.5753053454347,
124.437051863492));
#117923=CARTESIAN_POINT('Ctrl Pts',(2.90381231805844,-31.6281289826934,
124.641747977118));
#117924=CARTESIAN_POINT('Ctrl Pts',(2.90006603072716,-31.6399613368566,
124.700544168891));
#117925=CARTESIAN_POINT('Ctrl Pts',(2.89519169770525,-31.6507790765647,
124.774804455902));
#117926=CARTESIAN_POINT('Ctrl Pts',(2.89420055436652,-31.6527546880626,
124.789794161532));
#117927=CARTESIAN_POINT('Ctrl Pts',(2.89270434814951,-31.6553999760959,
124.812216690311));
#117928=CARTESIAN_POINT('Ctrl Pts',(2.89220739704106,-31.6562242173595,
124.819630965089));
#117929=CARTESIAN_POINT('Ctrl Pts',(2.89130563139368,-31.6576216264516,
124.833019282977));
#117930=CARTESIAN_POINT('Ctrl Pts',(2.89090179119244,-31.6582123470696,
124.838991225973));
#117931=CARTESIAN_POINT('Ctrl Pts',(2.88998729403304,-31.6594712673837,
124.852460943545));
#117932=CARTESIAN_POINT('Ctrl Pts',(2.88947566031924,-31.6601209215356,
124.859960074218));
#117933=CARTESIAN_POINT('Ctrl Pts',(2.88790482011062,-31.6619501026632,
124.882880171667));
#117934=CARTESIAN_POINT('Ctrl Pts',(2.88683732756775,-31.662965690117,124.898312887684));
#117935=CARTESIAN_POINT('Ctrl Pts',(2.87846947113451,-31.6691878791066,
125.018348647222));
#117936=CARTESIAN_POINT('Ctrl Pts',(2.87079289439822,-31.6647344414331,
125.123209914435));
#117937=CARTESIAN_POINT('Ctrl Pts',(2.85515229486171,-31.6354264593641,
125.336349294407));
#117938=CARTESIAN_POINT('Ctrl Pts',(2.84724021019601,-31.609541227926,125.443999776096));
#117939=CARTESIAN_POINT('Ctrl Pts',(2.83826869110657,-31.5664504405343,
125.567633418755));
#117940=CARTESIAN_POINT('Ctrl Pts',(2.83687817705804,-31.5593604804076,
125.58683016078));
#117941=CARTESIAN_POINT('Ctrl Pts',(2.83469033306039,-31.5475517718996,
125.617076716792));
#117942=CARTESIAN_POINT('Ctrl Pts',(2.83388539649639,-31.5430642847155,
125.628213966274));
#117943=CARTESIAN_POINT('Ctrl Pts',(2.83237083530556,-31.5343509574631,
125.649182267367));
#117944=CARTESIAN_POINT('Ctrl Pts',(2.83166041450026,-31.530150066814,125.659022957931));
#117945=CARTESIAN_POINT('Ctrl Pts',(2.83005149781574,-31.5203782097541,
125.681316508919));
#117946=CARTESIAN_POINT('Ctrl Pts',(2.82915505453099,-31.5147484645711,
125.693742887154));
#117947=CARTESIAN_POINT('Ctrl Pts',(2.82681978764157,-31.4996015547241,
125.726112540495));
#117948=CARTESIAN_POINT('Ctrl Pts',(2.82538938994307,-31.4898389617098,
125.745938459639));
#117949=CARTESIAN_POINT('Ctrl Pts',(2.81693112508418,-31.4292794145189,
125.862987976907));
#117950=CARTESIAN_POINT('Ctrl Pts',(2.81023497601403,-31.3693750838475,
125.95519801829));
#117951=CARTESIAN_POINT('Ctrl Pts',(2.79744385927754,-31.2385046022361,
126.118756259709));
#117952=CARTESIAN_POINT('Ctrl Pts',(2.79136696910473,-31.1693115083733,
126.190888054312));
#117953=CARTESIAN_POINT('Ctrl Pts',(2.78393195888616,-31.0830734200047,
126.26598640281));
#117954=CARTESIAN_POINT('Ctrl Pts',(2.78297312960808,-31.0719261967078,
126.275438668985));
#117955=CARTESIAN_POINT('Ctrl Pts',(2.78151628894705,-31.0549802816593,
126.289428860244));
#117956=CARTESIAN_POINT('Ctrl Pts',(2.78102577539371,-31.0492731662119,
126.294077276615));
#117957=CARTESIAN_POINT('Ctrl Pts',(2.78013024060899,-31.0388555439189,
126.302448157598));
#117958=CARTESIAN_POINT('Ctrl Pts',(2.77972611867871,-31.0341554706231,
126.306183181476));
#117959=CARTESIAN_POINT('Ctrl Pts',(2.77880394364658,-31.0234326070543,
126.314610202835));
#117960=CARTESIAN_POINT('Ctrl Pts',(2.77828483342275,-31.0173977200388,
126.319286231299));
#117961=CARTESIAN_POINT('Ctrl Pts',(2.77666758969991,-30.9985938969649,
126.333650303977));
#117962=CARTESIAN_POINT('Ctrl Pts',(2.77556047243615,-30.9857175611156,
126.343195349507));
#117963=CARTESIAN_POINT('Ctrl Pts',(2.76778914102209,-30.8951772161083,
126.408308634197));
#117964=CARTESIAN_POINT('Ctrl Pts',(2.76081459039106,-30.8130047831794,
126.457290485201));
#117965=CARTESIAN_POINT('Ctrl Pts',(2.75117948116407,-30.6938751103934,
126.515076509239));
#117966=CARTESIAN_POINT('Ctrl Pts',(2.7484973952017,-30.6601244382253,126.530083447696));
#117967=CARTESIAN_POINT('Ctrl Pts',(2.74179567226525,-30.5740148055645,
126.564991295717));
#117968=CARTESIAN_POINT('Ctrl Pts',(2.73780545641421,-30.5210961787657,
126.583398419821));
#117969=CARTESIAN_POINT('Ctrl Pts',(2.73212095964041,-30.4430147266682,
126.606218091231));
#117970=CARTESIAN_POINT('Ctrl Pts',(2.73036578829342,-30.4185227321709,
126.612773215769));
#117971=CARTESIAN_POINT('Ctrl Pts',(2.72720859277426,-30.3737698827831,
126.623662785618));
#117972=CARTESIAN_POINT('Ctrl Pts',(2.72580104947853,-30.3535599892662,
126.6281830879));
#117973=CARTESIAN_POINT('Ctrl Pts',(2.72359282670168,-30.3214554943502,
126.634737829919));
#117974=CARTESIAN_POINT('Ctrl Pts',(2.72278429605972,-30.3096146280348,
126.637021747798));
#117975=CARTESIAN_POINT('Ctrl Pts',(2.72126666514748,-30.2872311877455,
126.641087607402));
#117976=CARTESIAN_POINT('Ctrl Pts',(2.72055672850573,-30.2766942917686,
126.642897004801));
#117977=CARTESIAN_POINT('Ctrl Pts',(2.71895384483305,-30.2527591156964,
126.646770348281));
#117978=CARTESIAN_POINT('Ctrl Pts',(2.71806289004406,-30.2393514887902,
126.648772462592));
#117979=CARTESIAN_POINT('Ctrl Pts',(2.71575221448119,-30.2043234528106,
126.653566781445));
#117980=CARTESIAN_POINT('Ctrl Pts',(2.71434062435975,-30.1826696365118,
126.656098743493));
#117981=CARTESIAN_POINT('Ctrl Pts',(2.70356851059332,-30.0156865390077,
126.67230875617));
#117982=CARTESIAN_POINT('Ctrl Pts',(2.69484679753411,-29.869184328285,126.667258761376));
#117983=CARTESIAN_POINT('Ctrl Pts',(2.68299947068425,-29.6793974205192,
126.635520530801));
#117984=CARTESIAN_POINT('Ctrl Pts',(2.68011183035185,-29.6339290017304,
126.625947371667));
#117985=CARTESIAN_POINT('Ctrl Pts',(2.67541721334043,-29.5625335777578,
126.607768855673));
#117986=CARTESIAN_POINT('Ctrl Pts',(2.67365794842134,-29.5363143869195,
126.600404015855));
#117987=CARTESIAN_POINT('Ctrl Pts',(2.67124922143442,-29.5013435437212,
126.589649437266));
#117988=CARTESIAN_POINT('Ctrl Pts',(2.67062916534392,-29.4924213995331,
126.586823099472));
#117989=CARTESIAN_POINT('Ctrl Pts',(2.66958803473497,-29.4775836727864,
126.581984898113));
#117990=CARTESIAN_POINT('Ctrl Pts',(2.66916933113692,-29.4716545704037,
126.580014601789));
#117991=CARTESIAN_POINT('Ctrl Pts',(2.66836506858315,-29.4603416462313,
126.576184413364));
#117992=CARTESIAN_POINT('Ctrl Pts',(2.66797987001052,-29.4549560404357,
126.574330182458));
#117993=CARTESIAN_POINT('Ctrl Pts',(2.66693311404226,-29.4404061907541,
126.569237153005));
#117994=CARTESIAN_POINT('Ctrl Pts',(2.66626859713171,-29.4312607821679,
126.565945773137));
#117995=CARTESIAN_POINT('Ctrl Pts',(2.66368354362812,-29.396015323223,126.552911666027));
#117996=CARTESIAN_POINT('Ctrl Pts',(2.66173401726768,-29.3701339332928,
126.542595427654));
#117997=CARTESIAN_POINT('Ctrl Pts',(2.65189391475221,-29.2423859207266,
126.487924735122));
#117998=CARTESIAN_POINT('Ctrl Pts',(2.64370454372534,-29.144878354173,126.434107886226));
#117999=CARTESIAN_POINT('Ctrl Pts',(2.63142898803704,-29.0050566248126,
126.337573385563));
#118000=CARTESIAN_POINT('Ctrl Pts',(2.62722918029416,-28.9584583119658,
126.301617055311));
#118001=CARTESIAN_POINT('Ctrl Pts',(2.62128476376028,-28.8940325753155,
126.246224494745));
#118002=CARTESIAN_POINT('Ctrl Pts',(2.61947287141277,-28.8746126106295,
126.228715910518));
#118003=CARTESIAN_POINT('Ctrl Pts',(2.61622465596887,-28.8401996363471,
126.196189307542));
#118004=CARTESIAN_POINT('Ctrl Pts',(2.61478231155967,-28.8250664269051,
126.181328452982));
#118005=CARTESIAN_POINT('Ctrl Pts',(2.61253248466898,-28.8017058533694,
126.157495183164));
#118006=CARTESIAN_POINT('Ctrl Pts',(2.61171664156733,-28.7932864457656,
126.148715096323));
#118007=CARTESIAN_POINT('Ctrl Pts',(2.61019258419445,-28.7776596370705,
126.132057422774));
#118008=CARTESIAN_POINT('Ctrl Pts',(2.60948345299235,-28.7704303825584,
126.12420128813));
#118009=CARTESIAN_POINT('Ctrl Pts',(2.60789195184058,-28.7543040693199,
126.106334934564));
#118010=CARTESIAN_POINT('Ctrl Pts',(2.60701145917471,-28.745451121731,126.096285760466));
#118011=CARTESIAN_POINT('Ctrl Pts',(2.60434700526554,-28.7188837744712,
126.065385246686));
#118012=CARTESIAN_POINT('Ctrl Pts',(2.60257894104523,-28.7015604300619,
126.044202723347));
#118013=CARTESIAN_POINT('Ctrl Pts',(2.59241916691543,-28.604052602405,125.918791653858));
#118014=CARTESIAN_POINT('Ctrl Pts',(2.58451199478791,-28.5359139983762,
125.805792754862));
#118015=CARTESIAN_POINT('Ctrl Pts',(2.57400318728507,-28.4653822822955,
125.649683244292));
#118016=CARTESIAN_POINT('Ctrl Pts',(2.57154703270053,-28.4503035415831,
125.612845615846));
#118017=CARTESIAN_POINT('Ctrl Pts',(2.56904935605388,-28.4365599852179,
125.575509617798));
#118018=CARTESIAN_POINT('Origin',(5.,-30.,125.));
#118019=CARTESIAN_POINT('',(1.86811697181266,-28.4365600386127,125.575509762851));
#118020=CARTESIAN_POINT('',(2.06219309044095,-28.4365599837628,125.575509613845));
#118021=CARTESIAN_POINT('',(5.,-28.4365599837785,125.575509613888));
#118022=CARTESIAN_POINT('',(2.72302673015923,-28.3340004556389,124.999966473191));
#118023=CARTESIAN_POINT('Ctrl Pts',(2.06219309044095,-28.4365599837628,
125.575509613845));
#118024=CARTESIAN_POINT('Ctrl Pts',(2.06231481742157,-28.4372108183064,
125.577277682953));
#118025=CARTESIAN_POINT('Ctrl Pts',(2.06243645299245,-28.4378646585235,
125.579044665562));
#118026=CARTESIAN_POINT('Ctrl Pts',(2.06925163019703,-28.4746946580413,
125.678060174038));
#118027=CARTESIAN_POINT('Ctrl Pts',(2.07563241278995,-28.5198750093322,
125.771722573598));
#118028=CARTESIAN_POINT('Ctrl Pts',(2.08879836885796,-28.6311900822544,
125.95624065934));
#118029=CARTESIAN_POINT('Ctrl Pts',(2.09554809795371,-28.6983657674872,
126.04583843714));
#118030=CARTESIAN_POINT('Ctrl Pts',(2.10377393077897,-28.7840779043172,
126.138995862746));
#118031=CARTESIAN_POINT('Ctrl Pts',(2.10475125216527,-28.7943152577931,
126.14982710997));
#118032=CARTESIAN_POINT('Ctrl Pts',(2.10623072174372,-28.8098641976026,
126.165842105749));
#118033=CARTESIAN_POINT('Ctrl Pts',(2.1067250244591,-28.8150676754099,126.171130404598));
#118034=CARTESIAN_POINT('Ctrl Pts',(2.10762433699979,-28.8245456339976,
126.180635032828));
#118035=CARTESIAN_POINT('Ctrl Pts',(2.10802840448228,-28.8288078176796,
126.184863247879));
#118036=CARTESIAN_POINT('Ctrl Pts',(2.10894645072438,-28.8384996378183,
126.194374437489));
#118037=CARTESIAN_POINT('Ctrl Pts',(2.10946144124541,-28.8439424732035,
126.199643437607));
#118038=CARTESIAN_POINT('Ctrl Pts',(2.11105252360253,-28.860782537141,126.215724628787));
#118039=CARTESIAN_POINT('Ctrl Pts',(2.11213720004111,-28.8722965462877,
126.226412523041));
#118040=CARTESIAN_POINT('Ctrl Pts',(2.11776954070583,-28.9323392160363,
126.280586774353));
#118041=CARTESIAN_POINT('Ctrl Pts',(2.12246251647973,-28.9832338004666,
126.321357966518));
#118042=CARTESIAN_POINT('Ctrl Pts',(2.13552178348418,-29.1299560432527,
126.425390658499));
#118043=CARTESIAN_POINT('Ctrl Pts',(2.14391087005518,-29.2301488679622,
126.481907669679));
#118044=CARTESIAN_POINT('Ctrl Pts',(2.15501351459777,-29.374929441546,126.544896341994));
#118045=CARTESIAN_POINT('Ctrl Pts',(2.1580021549344,-29.4151534589742,126.560568171068));
#118046=CARTESIAN_POINT('Ctrl Pts',(2.16205210126152,-29.4713929261248,
126.579999278967));
#118047=CARTESIAN_POINT('Ctrl Pts',(2.16315713109171,-29.4869200155011,
126.585109498637));
#118048=CARTESIAN_POINT('Ctrl Pts',(2.16492836668002,-29.5120958456072,
126.592986567285));
#118049=CARTESIAN_POINT('Ctrl Pts',(2.16559919963509,-29.5216984476141,
126.595896080581));
#118050=CARTESIAN_POINT('Ctrl Pts',(2.16699403399123,-29.5418030077233,
126.601789841456));
#118051=CARTESIAN_POINT('Ctrl Pts',(2.16771748221308,-29.5523092224007,
126.604757974655));
#118052=CARTESIAN_POINT('Ctrl Pts',(2.16943493757064,-29.5774332733477,
126.611589881155));
#118053=CARTESIAN_POINT('Ctrl Pts',(2.17042583212048,-29.5920761837414,
126.615358402468));
#118054=CARTESIAN_POINT('Ctrl Pts',(2.17386592794236,-29.643400741383,126.627824941497));
#118055=CARTESIAN_POINT('Ctrl Pts',(2.17628194413063,-29.6803260982737,
126.635477302222));
#118056=CARTESIAN_POINT('Ctrl Pts',(2.18228497170247,-29.773858712866,126.651571554493));
#118057=CARTESIAN_POINT('Ctrl Pts',(2.18582605746478,-29.8307008979953,
126.658362751919));
#118058=CARTESIAN_POINT('Ctrl Pts',(2.19599789533564,-29.9960892642132,
126.669528209492));
#118059=CARTESIAN_POINT('Ctrl Pts',(2.202513487661,-30.1048410644254,126.666236523335));
#118060=CARTESIAN_POINT('Ctrl Pts',(2.21140765119618,-30.2441754539222,
126.648318826746));
#118061=CARTESIAN_POINT('Ctrl Pts',(2.21346040468707,-30.2757353487152,
126.643333902262));
#118062=CARTESIAN_POINT('Ctrl Pts',(2.21622928866247,-30.3171723554896,
126.635561706165));
#118063=CARTESIAN_POINT('Ctrl Pts',(2.2169048903658,-30.327196900393,126.633585802203));
#118064=CARTESIAN_POINT('Ctrl Pts',(2.21801398624008,-30.3435004358817,
126.630216185413));
#118065=CARTESIAN_POINT('Ctrl Pts',(2.21844442342664,-30.3497908238771,
126.628878060701));
#118066=CARTESIAN_POINT('Ctrl Pts',(2.21930041417302,-30.3622232327263,
126.626158037645));
#118067=CARTESIAN_POINT('Ctrl Pts',(2.21972587955541,-30.3683654526088,
126.624777684136));
#118068=CARTESIAN_POINT('Ctrl Pts',(2.22080393617889,-30.3838389275887,
126.621208050756));
#118069=CARTESIAN_POINT('Ctrl Pts',(2.22145902274012,-30.3931592707069,
126.618973021103));
#118070=CARTESIAN_POINT('Ctrl Pts',(2.2241183758424,-30.4306863069507,126.609630837722));
#118071=CARTESIAN_POINT('Ctrl Pts',(2.22615481698908,-30.4587222214789,
126.601866351039));
#118072=CARTESIAN_POINT('Ctrl Pts',(2.2318623315178,-30.5357459961899,126.578347041504));
#118073=CARTESIAN_POINT('Ctrl Pts',(2.2355826130043,-30.5842282488699,126.561050885177));
#118074=CARTESIAN_POINT('Ctrl Pts',(2.24848865580523,-30.7485437608804,
126.493703091887));
#118075=CARTESIAN_POINT('Ctrl Pts',(2.25768881958384,-30.8594685118196,
126.432756202053));
#118076=CARTESIAN_POINT('Ctrl Pts',(2.26870369820073,-30.9887774723958,
126.341236268437));
#118077=CARTESIAN_POINT('Ctrl Pts',(2.27091825153586,-31.0145508856175,
126.321848087803));
#118078=CARTESIAN_POINT('Ctrl Pts',(2.27406023594464,-31.0507696648818,
126.292918454136));
#118079=CARTESIAN_POINT('Ctrl Pts',(2.27501085241741,-31.0616804081071,
126.283974201449));
#118080=CARTESIAN_POINT('Ctrl Pts',(2.27667888391339,-31.0807359635062,
126.267944112093));
#118081=CARTESIAN_POINT('Ctrl Pts',(2.27739857301846,-31.0889278513462,
126.260915793462));
#118082=CARTESIAN_POINT('Ctrl Pts',(2.27888877958168,-31.1058242453155,
126.24613186868));
#118083=CARTESIAN_POINT('Ctrl Pts',(2.27965871294223,-31.114516833776,126.238363490476));
#118084=CARTESIAN_POINT('Ctrl Pts',(2.28166088330865,-31.1370170336625,
126.21782671612));
#118085=CARTESIAN_POINT('Ctrl Pts',(2.28288698172451,-31.1506914958848,
126.204914425715));
#118086=CARTESIAN_POINT('Ctrl Pts',(2.28899093174138,-31.2181727752003,
126.138997519325));
#118087=CARTESIAN_POINT('Ctrl Pts',(2.29371702165791,-31.2685531066315,
126.082605807923));
#118088=CARTESIAN_POINT('Ctrl Pts',(2.30236830557441,-31.3547684106108,
125.971785129724));
#118089=CARTESIAN_POINT('Ctrl Pts',(2.30630613785602,-31.3915751445283,
125.918304142636));
#118090=CARTESIAN_POINT('Ctrl Pts',(2.31496273358526,-31.4647802129463,
125.797386090421));
#118091=CARTESIAN_POINT('Ctrl Pts',(2.31968471471535,-31.4998334536118,
125.729316481363));
#118092=CARTESIAN_POINT('Ctrl Pts',(2.32568607543219,-31.5364714998573,
125.644260832969));
#118093=CARTESIAN_POINT('Ctrl Pts',(2.32674252078714,-31.5426428276835,
125.629340726388));
#118094=CARTESIAN_POINT('Ctrl Pts',(2.32832518810266,-31.5514603679344,
125.607113715113));
#118095=CARTESIAN_POINT('Ctrl Pts',(2.32884208597202,-31.554274069415,125.59987369297));
#118096=CARTESIAN_POINT('Ctrl Pts',(2.32976437696333,-31.5591754297697,
125.586995843966));
#118097=CARTESIAN_POINT('Ctrl Pts',(2.3301685687761,-31.5612833518188,125.581366007593));
#118098=CARTESIAN_POINT('Ctrl Pts',(2.33106455896732,-31.5658675558016,
125.568917759249));
#118099=CARTESIAN_POINT('Ctrl Pts',(2.33155712411249,-31.5683297662948,
125.562094616843));
#118100=CARTESIAN_POINT('Ctrl Pts',(2.3330127152157,-31.5754387364072,125.541984253349));
#118101=CARTESIAN_POINT('Ctrl Pts',(2.33398241021494,-31.5799616115333,
125.528654344981));
#118102=CARTESIAN_POINT('Ctrl Pts',(2.34075274720278,-31.6101139538162,
125.435943980549));
#118103=CARTESIAN_POINT('Ctrl Pts',(2.34680388408158,-31.6299164062079,
125.354801012144));
#118104=CARTESIAN_POINT('Ctrl Pts',(2.36226796283999,-31.6646747087329,
125.145179694918));
#118105=CARTESIAN_POINT('Ctrl Pts',(2.37162264222884,-31.6709224711773,
125.015785402748));
#118106=CARTESIAN_POINT('Ctrl Pts',(2.3819450237651,-31.6607400010836,124.866072492029));
#118107=CARTESIAN_POINT('Ctrl Pts',(2.38337259339451,-31.6589266742306,
124.845221813287));
#118108=CARTESIAN_POINT('Ctrl Pts',(2.38568771757015,-31.6553187325703,
124.811180285239));
#118109=CARTESIAN_POINT('Ctrl Pts',(2.38658245541412,-31.6537581113795,
124.797967532445));
#118110=CARTESIAN_POINT('Ctrl Pts',(2.38818594032121,-31.650660696371,124.774192223803));
#118111=CARTESIAN_POINT('Ctrl Pts',(2.38889641941629,-31.6491803707634,
124.763623181936));
#118112=CARTESIAN_POINT('Ctrl Pts',(2.39041436900415,-31.6457856493461,
124.740972581627));
#118113=CARTESIAN_POINT('Ctrl Pts',(2.39122079594665,-31.6438395401406,
124.728896354288));
#118114=CARTESIAN_POINT('Ctrl Pts',(2.39343456569231,-31.6381033701174,
124.695637783608));
#118115=CARTESIAN_POINT('Ctrl Pts',(2.39483310826594,-31.634035578599,124.674505289315));
#118116=CARTESIAN_POINT('Ctrl Pts',(2.40253184634665,-31.6091855082056,
124.557652165559));
#118117=CARTESIAN_POINT('Ctrl Pts',(2.40856905912572,-31.5804019658594,
124.463825998978));
#118118=CARTESIAN_POINT('Ctrl Pts',(2.42101562493036,-31.5037849811704,
124.275192745723));
#118119=CARTESIAN_POINT('Ctrl Pts',(2.42739148430075,-31.4548193755125,
124.181336248532));
#118120=CARTESIAN_POINT('Ctrl Pts',(2.43556571651037,-31.3854594827054,
124.074510198276));
#118121=CARTESIAN_POINT('Ctrl Pts',(2.43697872959875,-31.3732559770193,
124.056497342415));
#118122=CARTESIAN_POINT('Ctrl Pts',(2.43899612297903,-31.3556033068122,
124.031509513785));
#118123=CARTESIAN_POINT('Ctrl Pts',(2.43958255187393,-31.3504453863978,
124.024330282792));
#118124=CARTESIAN_POINT('Ctrl Pts',(2.44057946784205,-31.3416380872528,
124.012275174306));
#118125=CARTESIAN_POINT('Ctrl Pts',(2.44098794219871,-31.3380185674872,
124.007377513695));
#118126=CARTESIAN_POINT('Ctrl Pts',(2.44184592498239,-31.3303953762181,
123.997179846196));
#118127=CARTESIAN_POINT('Ctrl Pts',(2.44229575068526,-31.3263867752225,
123.991883817919));
#118128=CARTESIAN_POINT('Ctrl Pts',(2.44350859264121,-31.3155440201311,
123.977735355829));
#118129=CARTESIAN_POINT('Ctrl Pts',(2.4442754087304,-31.3086523586475,123.968927714065));
#118130=CARTESIAN_POINT('Ctrl Pts',(2.44832063953449,-31.272081365715,123.923146767727));
#118131=CARTESIAN_POINT('Ctrl Pts',(2.45168540501488,-31.2409248864403,
123.887386667002));
#118132=CARTESIAN_POINT('Ctrl Pts',(2.46498909721191,-31.1135505170592,
123.753205232102));
#118133=CARTESIAN_POINT('Ctrl Pts',(2.47515119374629,-31.0067929304287,
123.665508072469));
#118134=CARTESIAN_POINT('Ctrl Pts',(2.4880242878335,-30.8523328001831,123.567826747251));
#118135=CARTESIAN_POINT('Ctrl Pts',(2.49115297688998,-30.813235621971,123.545269813954));
#118136=CARTESIAN_POINT('Ctrl Pts',(2.49535677662772,-30.7585555726385,
123.516616935911));
#118137=CARTESIAN_POINT('Ctrl Pts',(2.49648010337844,-30.7437287618295,
123.509127961513));
#118138=CARTESIAN_POINT('Ctrl Pts',(2.49827276881014,-30.719726819475,123.497451854677));
#118139=CARTESIAN_POINT('Ctrl Pts',(2.49894695043675,-30.7106216759104,
123.493124270177));
#118140=CARTESIAN_POINT('Ctrl Pts',(2.50034287098579,-30.6916083227468,
123.48429807652));
#118141=CARTESIAN_POINT('Ctrl Pts',(2.50106410571186,-30.681694168892,123.479813346136));
#118142=CARTESIAN_POINT('Ctrl Pts',(2.50276572553247,-30.658093888883,123.46941491926));
#118143=CARTESIAN_POINT('Ctrl Pts',(2.5037431532549,-30.6443707709508,123.463587103249));
#118144=CARTESIAN_POINT('Ctrl Pts',(2.50707938351856,-30.5969797601342,
123.444208173712));
#118145=CARTESIAN_POINT('Ctrl Pts',(2.50940771438994,-30.5629470321415,
123.43157276741));
#118146=CARTESIAN_POINT('Ctrl Pts',(2.51513281198041,-30.4772270836863,
123.402897482673));
#118147=CARTESIAN_POINT('Ctrl Pts',(2.51848929427493,-30.4251198576961,
123.388244468241));
#118148=CARTESIAN_POINT('Ctrl Pts',(2.5254767648598,-30.3143158819693,123.362834353216));
#118149=CARTESIAN_POINT('Ctrl Pts',(2.5290957655144,-30.2555704712064,123.352641632794));
#118150=CARTESIAN_POINT('Ctrl Pts',(2.53774699646188,-30.1153322516718,
123.335992804739));
#118151=CARTESIAN_POINT('Ctrl Pts',(2.54279356215285,-30.0336717308764,
123.332341719573));
#118152=CARTESIAN_POINT('Ctrl Pts',(2.54893151189941,-29.9397265177367,
123.335044756533));
#118153=CARTESIAN_POINT('Ctrl Pts',(2.5497453288015,-29.9273729500061,123.335537881227));
#118154=CARTESIAN_POINT('Ctrl Pts',(2.5510293060358,-29.9080656820036,123.336523922599));
#118155=CARTESIAN_POINT('Ctrl Pts',(2.55149450568713,-29.9011073539954,
123.336923086846));
#118156=CARTESIAN_POINT('Ctrl Pts',(2.55236817543867,-29.8881130059662,
123.337750344702));
#118157=CARTESIAN_POINT('Ctrl Pts',(2.55277605558448,-29.8820765503423,
123.338167676521));
#118158=CARTESIAN_POINT('Ctrl Pts',(2.5537400353919,-29.8678789954351,123.33922697052));
#118159=CARTESIAN_POINT('Ctrl Pts',(2.55429759741748,-29.8597202113756,
123.339896211318));
#118160=CARTESIAN_POINT('Ctrl Pts',(2.55616735457015,-29.8325252425241,
123.34232883484));
#118161=CARTESIAN_POINT('Ctrl Pts',(2.55749281551937,-29.8135152947768,
123.344359681681));
#118162=CARTESIAN_POINT('Ctrl Pts',(2.56078509930181,-29.7668536721785,
123.350158349507));
#118163=CARTESIAN_POINT('Ctrl Pts',(2.56276608779761,-29.739254141181,123.354294648412));
#118164=CARTESIAN_POINT('Ctrl Pts',(2.57173114335664,-29.6159755305234,
123.375949032978));
#118165=CARTESIAN_POINT('Ctrl Pts',(2.5788809553325,-29.5218366518924,123.401132799071));
#118166=CARTESIAN_POINT('Ctrl Pts',(2.59208211650717,-29.350011927202,123.463642330184));
#118167=CARTESIAN_POINT('Ctrl Pts',(2.59814461275216,-29.2719553757112,
123.499055468843));
#118168=CARTESIAN_POINT('Ctrl Pts',(2.60536629389388,-29.1795357897617,
123.549900082901));
#118169=CARTESIAN_POINT('Ctrl Pts',(2.60671652400811,-29.1622883831308,
123.559794946468));
#118170=CARTESIAN_POINT('Ctrl Pts',(2.60885627281193,-29.1350191398783,
123.576095019926));
#118171=CARTESIAN_POINT('Ctrl Pts',(2.60965283040887,-29.1248820492152,
123.582302618487));
#118172=CARTESIAN_POINT('Ctrl Pts',(2.61116076684659,-29.1057236703578,
123.594318338043));
#118173=CARTESIAN_POINT('Ctrl Pts',(2.6118728438471,-29.0966904034283,123.600106121719));
#118174=CARTESIAN_POINT('Ctrl Pts',(2.61349810833563,-29.0761089593788,
123.6135752151));
#118175=CARTESIAN_POINT('Ctrl Pts',(2.61440908479322,-29.0645994305063,
123.621314345836));
#118176=CARTESIAN_POINT('Ctrl Pts',(2.61727176942696,-29.0285331656084,
123.646225273701));
#118177=CARTESIAN_POINT('Ctrl Pts',(2.61920380248792,-29.0043415153599,
123.663916851643));
#118178=CARTESIAN_POINT('Ctrl Pts',(2.62656294866053,-28.913051869991,123.734535152209));
#118179=CARTESIAN_POINT('Ctrl Pts',(2.63181896097461,-28.8495841056786,
123.79194253248));
#118180=CARTESIAN_POINT('Ctrl Pts',(2.64363902708161,-28.7165561467008,
123.93230367782));
#118181=CARTESIAN_POINT('Ctrl Pts',(2.65015358676409,-28.6501125172907,
124.017655035499));
#118182=CARTESIAN_POINT('Ctrl Pts',(2.65834846640939,-28.5820754160901,
124.125118240397));
#118183=CARTESIAN_POINT('Ctrl Pts',(2.6596052238993,-28.5720396152025,124.141596085127));
#118184=CARTESIAN_POINT('Ctrl Pts',(2.6613804055424,-28.558456066797,124.164796581569));
#118185=CARTESIAN_POINT('Ctrl Pts',(2.66188442110346,-28.5546643347953,
124.171375554957));
#118186=CARTESIAN_POINT('Ctrl Pts',(2.66280018617779,-28.5478949656625,
124.183308808472));
#118187=CARTESIAN_POINT('Ctrl Pts',(2.66321095049384,-28.5449015863085,
124.188654119309));
#118188=CARTESIAN_POINT('Ctrl Pts',(2.66406626433856,-28.5387591018982,
124.199766153918));
#118189=CARTESIAN_POINT('Ctrl Pts',(2.66451106641684,-28.5356145417786,
124.205535150756));
#118190=CARTESIAN_POINT('Ctrl Pts',(2.66569620664442,-28.5273654130038,
124.220884340886));
#118191=CARTESIAN_POINT('Ctrl Pts',(2.66644006075658,-28.5223203143431,
124.230495894707));
#118192=CARTESIAN_POINT('Ctrl Pts',(2.67013111884252,-28.4979172579362,
124.27811185158));
#118193=CARTESIAN_POINT('Ctrl Pts',(2.67314824164962,-28.4799313031453,
124.316797581612));
#118194=CARTESIAN_POINT('Ctrl Pts',(2.6819460233931,-28.4325012417849,124.429985415987));
#118195=CARTESIAN_POINT('Ctrl Pts',(2.68781168610613,-28.4069179176067,
124.505977696194));
#118196=CARTESIAN_POINT('Ctrl Pts',(2.70097322623689,-28.361566048642,124.681630796932));
#118197=CARTESIAN_POINT('Ctrl Pts',(2.70819996968239,-28.345234088113,124.781869147136));
#118198=CARTESIAN_POINT('Ctrl Pts',(2.71647448556716,-28.3367452754212,
124.902431012962));
#118199=CARTESIAN_POINT('Ctrl Pts',(2.71779853598483,-28.3357174743766,
124.92189931528));
#118200=CARTESIAN_POINT('Ctrl Pts',(2.71988325154906,-28.3346287717819,
124.952822457251));
#118201=CARTESIAN_POINT('Ctrl Pts',(2.72065081836281,-28.3343439074036,
124.964267090192));
#118202=CARTESIAN_POINT('Ctrl Pts',(2.72195415943265,-28.3340591730269,
124.983797565021));
#118203=CARTESIAN_POINT('Ctrl Pts',(2.72249175600273,-28.334000162432,124.991881975512));
#118204=CARTESIAN_POINT('Ctrl Pts',(2.72302752844612,-28.3340000003349,
124.999966596608));
#118205=CARTESIAN_POINT('Ctrl Pts',(2.72302751681176,-28.3340000003384,
124.999966421049));
#118206=CARTESIAN_POINT('Ctrl Pts',(2.72341003707426,-28.3339998839993,
125.005738519388));
#118207=CARTESIAN_POINT('Ctrl Pts',(2.72379162305297,-28.3340297650592,
125.011510654778));
#118208=CARTESIAN_POINT('Ctrl Pts',(2.72478818356262,-28.3341865271217,
125.026621321881));
#118209=CARTESIAN_POINT('Ctrl Pts',(2.72540164493891,-28.3343619356514,
125.035959222548));
#118210=CARTESIAN_POINT('Ctrl Pts',(2.7274071184179,-28.3351952588838,125.066598225843));
#118211=CARTESIAN_POINT('Ctrl Pts',(2.72878894568904,-28.3361833704955,
125.087888788886));
#118212=CARTESIAN_POINT('Ctrl Pts',(2.7379957085408,-28.3455645420212,125.230762699901));
#118213=CARTESIAN_POINT('Ctrl Pts',(2.74539422571528,-28.3668678458642,
125.351128679346));
#118214=CARTESIAN_POINT('Ctrl Pts',(2.75514841777084,-28.4117154118108,
125.504312956938));
#118215=CARTESIAN_POINT('Ctrl Pts',(2.75745803106252,-28.4235384779283,
125.540135147333));
#118216=CARTESIAN_POINT('Ctrl Pts',(2.75979328931693,-28.4365599629713,
125.575509557363));
#118217=CARTESIAN_POINT('Ctrl Pts',(2.56904935605388,-28.4365599852179,
125.575509617798));
#118218=CARTESIAN_POINT('Ctrl Pts',(2.56823105408791,-28.4320572489617,
125.563277401652));
#118219=CARTESIAN_POINT('Ctrl Pts',(2.56740827376691,-28.4276978294066,
125.550991692691));
#118220=CARTESIAN_POINT('Ctrl Pts',(2.56530560429473,-28.4169970304824,
125.519672955597));
#118221=CARTESIAN_POINT('Ctrl Pts',(2.56401862826457,-28.4108550117471,
125.500576182282));
#118222=CARTESIAN_POINT('Ctrl Pts',(2.56174409682684,-28.4007402472956,
125.467062855529));
#118223=CARTESIAN_POINT('Ctrl Pts',(2.5607638775511,-28.3966139292905,125.452694751303));
#118224=CARTESIAN_POINT('Ctrl Pts',(2.55928096941336,-28.3907279549038,
125.431108617603));
#118225=CARTESIAN_POINT('Ctrl Pts',(2.55878618226911,-28.3888222061937,
125.423930733468));
#118226=CARTESIAN_POINT('Ctrl Pts',(2.5578865334742,-28.3854632353537,125.410929504263));
#118227=CARTESIAN_POINT('Ctrl Pts',(2.55748262103918,-28.3839934039219,
125.405110725782));
#118228=CARTESIAN_POINT('Ctrl Pts',(2.55656564180777,-28.380742613805,125.39194222151));
#118229=CARTESIAN_POINT('Ctrl Pts',(2.55605157199553,-28.3789802491961,
125.384588285914));
#118230=CARTESIAN_POINT('Ctrl Pts',(2.55446570287488,-28.3737249873275,
125.361981270724));
#118231=CARTESIAN_POINT('Ctrl Pts',(2.55338539455546,-28.3703969872883,
125.346691266283));
#118232=CARTESIAN_POINT('Ctrl Pts',(2.54519340993738,-28.347000244132,125.231407231135));
#118233=CARTESIAN_POINT('Ctrl Pts',(2.53772584557607,-28.3359379662311,
125.129814135697));
#118234=CARTESIAN_POINT('Ctrl Pts',(2.52221525519045,-28.3323717256583,
124.916563484871));
#118235=CARTESIAN_POINT('Ctrl Pts',(2.51422881501946,-28.341668410633,124.805345556746));
#118236=CARTESIAN_POINT('Ctrl Pts',(2.50512604426723,-28.3658885666801,
124.67489880836));
#118237=CARTESIAN_POINT('Ctrl Pts',(2.50367516624649,-28.3701848784543,
124.654003317728));
#118238=CARTESIAN_POINT('Ctrl Pts',(2.50141514689657,-28.3775652745733,
124.621304674162));
#118239=CARTESIAN_POINT('Ctrl Pts',(2.50059751802699,-28.3803795646112,
124.60944366983));
#118240=CARTESIAN_POINT('Ctrl Pts',(2.4990718571732,-28.3859015830823,124.587257701146));
#118241=CARTESIAN_POINT('Ctrl Pts',(2.49836288880667,-28.3885788282974,
124.576925867953));
#118242=CARTESIAN_POINT('Ctrl Pts',(2.49677399946516,-28.3948289891224,
124.55372614781));
#118243=CARTESIAN_POINT('Ctrl Pts',(2.49589592915852,-28.3984577363053,
124.54087396046));
#118244=CARTESIAN_POINT('Ctrl Pts',(2.49364263217726,-28.4082192282444,
124.507825843319));
#118245=CARTESIAN_POINT('Ctrl Pts',(2.49227486670575,-28.4145820243575,
124.487699958644));
#118246=CARTESIAN_POINT('Ctrl Pts',(2.4813162999072,-28.4690578344515,124.326137863247));
#118247=CARTESIAN_POINT('Ctrl Pts',(2.47240385014623,-28.535609663832,124.191645719875));
#118248=CARTESIAN_POINT('Ctrl Pts',(2.45943795445118,-28.6533260477269,
124.017276925459));
#118249=CARTESIAN_POINT('Ctrl Pts',(2.45562933404548,-28.690196198818,123.968647588215));
#118250=CARTESIAN_POINT('Ctrl Pts',(2.450680162438,-28.7395042671362,123.910532799219));
#118251=CARTESIAN_POINT('Ctrl Pts',(2.44968124960086,-28.7495229629386,
123.899047951195));
#118252=CARTESIAN_POINT('Ctrl Pts',(2.44817559155413,-28.7646937986434,
123.882131226772));
#118253=CARTESIAN_POINT('Ctrl Pts',(2.44767710906758,-28.7697275983366,
123.876593654285));
#118254=CARTESIAN_POINT('Ctrl Pts',(2.44677383246375,-28.7788649428169,
123.866676927444));
#118255=CARTESIAN_POINT('Ctrl Pts',(2.44637003040627,-28.7829550730582,
123.862285775118));
#118256=CARTESIAN_POINT('Ctrl Pts',(2.44545723270482,-28.7922125268839,
123.8524540453));
#118257=CARTESIAN_POINT('Ctrl Pts',(2.44494727845425,-28.7973928890774,
123.847026266711));
#118258=CARTESIAN_POINT('Ctrl Pts',(2.44338674920808,-28.8132764150256,
123.830607640808));
#118259=CARTESIAN_POINT('Ctrl Pts',(2.44232803947089,-28.8240945471019,
123.819729827089));
#118260=CARTESIAN_POINT('Ctrl Pts',(2.4338121221954,-28.9115604862978,123.734177525658));
#118261=CARTESIAN_POINT('Ctrl Pts',(2.42596169614753,-28.9950850129513,
123.666902276812));
#118262=CARTESIAN_POINT('Ctrl Pts',(2.41037437473203,-29.1742816987032,
123.549034862569));
#118263=CARTESIAN_POINT('Ctrl Pts',(2.40267823468151,-29.2696082320333,
123.498785161512));
#118264=CARTESIAN_POINT('Ctrl Pts',(2.39387012274102,-29.3884976536493,
123.450142306569));
#118265=CARTESIAN_POINT('Ctrl Pts',(2.39244717805493,-29.4080156595347,
123.442582715088));
#118266=CARTESIAN_POINT('Ctrl Pts',(2.3902205359124,-29.4390402266528,123.431234029817));
#118267=CARTESIAN_POINT('Ctrl Pts',(2.38940876344116,-29.4504539689033,
123.42719940564));
#118268=CARTESIAN_POINT('Ctrl Pts',(2.38788831217923,-29.4720219512251,
123.41983883121));
#118269=CARTESIAN_POINT('Ctrl Pts',(2.38717876111291,-29.4821661172456,
123.416485485291));
#118270=CARTESIAN_POINT('Ctrl Pts',(2.38558106504151,-29.5051820639366,
123.409121955857));
#118271=CARTESIAN_POINT('Ctrl Pts',(2.38469486008043,-29.5180717746173,
123.405169932399));
#118272=CARTESIAN_POINT('Ctrl Pts',(2.38240539291069,-29.5516791550761,
123.395310473407));
#118273=CARTESIAN_POINT('Ctrl Pts',(2.38101001075511,-29.5724663383989,
123.389647525277));
#118274=CARTESIAN_POINT('Ctrl Pts',(2.37016783612676,-29.7361573683702,
123.348447258276));
#118275=CARTESIAN_POINT('Ctrl Pts',(2.36137449331452,-29.8830845085621,
123.331595990745));
#118276=CARTESIAN_POINT('Ctrl Pts',(2.34847944699122,-30.0924128707277,
123.335406118444));
#118277=CARTESIAN_POINT('Ctrl Pts',(2.3446045348747,-30.1543886036571,123.3400073984));
#118278=CARTESIAN_POINT('Ctrl Pts',(2.33957578283868,-30.2311939476657,
123.35004802096));
#118279=CARTESIAN_POINT('Ctrl Pts',(2.33856870707222,-30.2464033072549,
123.352250764334));
#118280=CARTESIAN_POINT('Ctrl Pts',(2.33705312407168,-30.2689946005218,
123.355842379625));
#118281=CARTESIAN_POINT('Ctrl Pts',(2.33655303955399,-30.2764016192379,
123.357071360284));
#118282=CARTESIAN_POINT('Ctrl Pts',(2.33564817119637,-30.2897134214183,
123.359372635758));
#118283=CARTESIAN_POINT('Ctrl Pts',(2.33524439790885,-30.2956210648319,
123.360426824452));
#118284=CARTESIAN_POINT('Ctrl Pts',(2.33433332917205,-30.3088780243002,
123.362866439439));
#118285=CARTESIAN_POINT('Ctrl Pts',(2.33382509373115,-30.3162237164752,
123.364269433943));
#118286=CARTESIAN_POINT('Ctrl Pts',(2.33227507557799,-30.3384841785334,
123.368676630185));
#118287=CARTESIAN_POINT('Ctrl Pts',(2.33122531097994,-30.3533670004421,
123.371835635345));
#118288=CARTESIAN_POINT('Ctrl Pts',(2.32260864438357,-30.4741294941207,
123.399202173474));
#118289=CARTESIAN_POINT('Ctrl Pts',(2.31463595337783,-30.5774453402395,
123.433505227745));
#118290=CARTESIAN_POINT('Ctrl Pts',(2.29903129538714,-30.7737095874203,
123.520741962037));
#118291=CARTESIAN_POINT('Ctrl Pts',(2.29143363259745,-30.866409045802,123.573054461167));
#118292=CARTESIAN_POINT('Ctrl Pts',(2.28271944799927,-30.9706295582843,
123.645795390551));
#118293=CARTESIAN_POINT('Ctrl Pts',(2.28130003910408,-30.9875239259045,
123.658065415845));
#118294=CARTESIAN_POINT('Ctrl Pts',(2.27907762457224,-31.0138344413362,
123.677940242375));
#118295=CARTESIAN_POINT('Ctrl Pts',(2.27826659553927,-31.0234055454233,
123.685335259418));
#118296=CARTESIAN_POINT('Ctrl Pts',(2.27674679514816,-31.0412792126381,
123.699458661196));
#118297=CARTESIAN_POINT('Ctrl Pts',(2.27603715972085,-31.0495991672993,
123.706163932447));
#118298=CARTESIAN_POINT('Ctrl Pts',(2.27443829424766,-31.0682818947892,
123.721519656968));
#118299=CARTESIAN_POINT('Ctrl Pts',(2.27355101603783,-31.078605285717,123.730217006848));
#118300=CARTESIAN_POINT('Ctrl Pts',(2.27125676268263,-31.1051705655109,
123.753155753816));
#118301=CARTESIAN_POINT('Ctrl Pts',(2.26985772381813,-31.1212435205954,
123.767589520874));
#118302=CARTESIAN_POINT('Ctrl Pts',(2.25903124056536,-31.2444474272381,
123.882634675188));
#118303=CARTESIAN_POINT('Ctrl Pts',(2.2502539445275,-31.338115328509,123.99670351579));
#118304=CARTESIAN_POINT('Ctrl Pts',(2.23736827676881,-31.4484327637146,
124.174485340228));
#118305=CARTESIAN_POINT('Ctrl Pts',(2.23348431139957,-31.4782638916926,
124.229178275905));
#118306=CARTESIAN_POINT('Ctrl Pts',(2.22844469208572,-31.5115611045266,
124.299303394237));
#118307=CARTESIAN_POINT('Ctrl Pts',(2.22743650942295,-31.5179671535999,
124.313291630023));
#118308=CARTESIAN_POINT('Ctrl Pts',(2.22591958102072,-31.5272110812655,
124.33423822638));
#118309=CARTESIAN_POINT('Ctrl Pts',(2.22541927980277,-31.5301972913025,
124.341130763955));
#118310=CARTESIAN_POINT('Ctrl Pts',(2.22451419531994,-31.5354851901925,
124.35356574525));
#118311=CARTESIAN_POINT('Ctrl Pts',(2.22411042510577,-31.5378036833083,
124.359100753839));
#118312=CARTESIAN_POINT('Ctrl Pts',(2.22319958662066,-31.5429430484147,
124.371558571465));
#118313=CARTESIAN_POINT('Ctrl Pts',(2.22269158084853,-31.5457472361146,
124.378487846955));
#118314=CARTESIAN_POINT('Ctrl Pts',(2.22114296374925,-31.5541107451346,
124.399561199408));
#118315=CARTESIAN_POINT('Ctrl Pts',(2.22009439080216,-31.5595230737227,
124.413762246723));
#118316=CARTESIAN_POINT('Ctrl Pts',(2.21146593757035,-31.6020934679014,
124.530223166829));
#118317=CARTESIAN_POINT('Ctrl Pts',(2.2034787453441,-31.6293436541267,124.635816611436));
#118318=CARTESIAN_POINT('Ctrl Pts',(2.18798034707729,-31.6622123776669,
124.846591911234));
#118319=CARTESIAN_POINT('Ctrl Pts',(2.18049848314152,-31.6685646192756,
124.951183019841));
#118320=CARTESIAN_POINT('Ctrl Pts',(2.17183048515137,-31.6643432746323,
125.077385054417));
#118321=CARTESIAN_POINT('Ctrl Pts',(2.17035370169061,-31.6631939893173,
125.099059646083));
#118322=CARTESIAN_POINT('Ctrl Pts',(2.16806276524559,-31.6607326560642,
125.132941862874));
#118323=CARTESIAN_POINT('Ctrl Pts',(2.16723973460431,-31.6597086983541,
125.145167297901));
#118324=CARTESIAN_POINT('Ctrl Pts',(2.16570914858946,-31.6575423523039,
125.167997258063));
#118325=CARTESIAN_POINT('Ctrl Pts',(2.16500059846276,-31.6564329973489,
125.17860420693));
#118326=CARTESIAN_POINT('Ctrl Pts',(2.16341924168835,-31.6537178187908,
125.202358029223));
#118327=CARTESIAN_POINT('Ctrl Pts',(2.16254820835617,-31.6520569106524,
125.215497974481));
#118328=CARTESIAN_POINT('Ctrl Pts',(2.16032605332972,-31.6473948331044,
125.249150515399));
#118329=CARTESIAN_POINT('Ctrl Pts',(2.1589820407665,-31.6441671294819,125.269629795479));
#118330=CARTESIAN_POINT('Ctrl Pts',(2.14922885388604,-31.6177636497037,
125.418974035585));
#118331=CARTESIAN_POINT('Ctrl Pts',(2.14132266935337,-31.5798515228248,
125.544767212036));
#118332=CARTESIAN_POINT('Ctrl Pts',(2.12828874690645,-31.4948802408172,
125.74000725143));
#118333=CARTESIAN_POINT('Ctrl Pts',(2.12323215411156,-31.4566625351929,
125.812655207168));
#118334=CARTESIAN_POINT('Ctrl Pts',(2.11698149246651,-31.4058119570296,
125.894117775523));
#118335=CARTESIAN_POINT('Ctrl Pts',(2.11605790290485,-31.3982131173285,
125.905954690659));
#118336=CARTESIAN_POINT('Ctrl Pts',(2.11464409045213,-31.3864717978894,
125.923744836594));
#118337=CARTESIAN_POINT('Ctrl Pts',(2.11416072132097,-31.3824386013927,
125.929769905908));
#118338=CARTESIAN_POINT('Ctrl Pts',(2.11327184604019,-31.3749905762786,
125.940740684307));
#118339=CARTESIAN_POINT('Ctrl Pts',(2.11286715469574,-31.3715881469888,
125.945694491507));
#118340=CARTESIAN_POINT('Ctrl Pts',(2.11193532804392,-31.3637275080613,
125.957007627283));
#118341=CARTESIAN_POINT('Ctrl Pts',(2.11140703774528,-31.3592515954944,
125.963354248985));
#118342=CARTESIAN_POINT('Ctrl Pts',(2.10977194315397,-31.3453340755478,
125.982798513255));
#118343=CARTESIAN_POINT('Ctrl Pts',(2.10865611384413,-31.3357466221887,
125.995789940629));
#118344=CARTESIAN_POINT('Ctrl Pts',(2.10219031879693,-31.2796001024131,
126.069600991527));
#118345=CARTESIAN_POINT('Ctrl Pts',(2.09664144320763,-31.2290832996542,
126.127286433246));
#118346=CARTESIAN_POINT('Ctrl Pts',(2.08425634874461,-31.1083853806444,
126.247319922864));
#118347=CARTESIAN_POINT('Ctrl Pts',(2.07743596914106,-31.0365309125931,
126.3076436892));
#118348=CARTESIAN_POINT('Ctrl Pts',(2.06721888907106,-30.9184473538711,
126.390896527044));
#118349=CARTESIAN_POINT('Ctrl Pts',(2.06368547969969,-30.8755907895555,
126.418266687986));
#118350=CARTESIAN_POINT('Ctrl Pts',(2.05907999370103,-30.8170045138383,
126.452012817673));
#118351=CARTESIAN_POINT('Ctrl Pts',(2.05794479117482,-30.8023372274195,
126.460168691488));
#118352=CARTESIAN_POINT('Ctrl Pts',(2.05606295950073,-30.7776508851159,
126.473411436188));
#118353=CARTESIAN_POINT('Ctrl Pts',(2.05531202532798,-30.7676993864426,
126.47862091901));
#118354=CARTESIAN_POINT('Ctrl Pts',(2.05384022634437,-30.7480001088232,
126.488680744058));
#118355=CARTESIAN_POINT('Ctrl Pts',(2.05311918385441,-30.7382559790634,
126.493536956175));
#118356=CARTESIAN_POINT('Ctrl Pts',(2.05137473239474,-30.7144595178811,
126.50510667727));
#118357=CARTESIAN_POINT('Ctrl Pts',(2.05035484342123,-30.7003591295661,
126.511719428098));
#118358=CARTESIAN_POINT('Ctrl Pts',(2.04686699878162,-30.6515177542459,
126.533794805252));
#118359=CARTESIAN_POINT('Ctrl Pts',(2.04443245035103,-30.6163399647606,
126.548265894764));
#118360=CARTESIAN_POINT('Ctrl Pts',(2.03446983786867,-30.46856192392,126.603221305574));
#118361=CARTESIAN_POINT('Ctrl Pts',(2.02728095451647,-30.3522652084886,
126.632721399917));
#118362=CARTESIAN_POINT('Ctrl Pts',(2.01687602083308,-30.1846084127871,
126.656485738769));
#118363=CARTESIAN_POINT('Ctrl Pts',(2.01379546927359,-30.1351243690185,
126.661254342302));
#118364=CARTESIAN_POINT('Ctrl Pts',(2.00882447676607,-30.0570939783004,
126.665264422025));
#118365=CARTESIAN_POINT('Ctrl Pts',(2.00698887534482,-30.0286522006169,
126.665996440925));
#118366=CARTESIAN_POINT('Ctrl Pts',(2.0044913845513,-29.9907002587713,126.66600117233));
#118367=CARTESIAN_POINT('Ctrl Pts',(2.003861730469,-29.981193262172,126.665920972743));
#118368=CARTESIAN_POINT('Ctrl Pts',(2.00280896408529,-29.9654105323057,
126.665652719988));
#118369=CARTESIAN_POINT('Ctrl Pts',(2.00238833818513,-29.9591340614226,
126.665510548644));
#118370=CARTESIAN_POINT('Ctrl Pts',(2.0015315809664,-29.9464131118345,126.665150450689));
#118371=CARTESIAN_POINT('Ctrl Pts',(2.00109536080901,-29.9399688436851,
126.664930579547));
#118372=CARTESIAN_POINT('Ctrl Pts',(1.99995708470832,-29.9232333377424,
126.664262296203));
#118373=CARTESIAN_POINT('Ctrl Pts',(1.99925197261299,-29.9129448782246,
126.663755842457));
#118374=CARTESIAN_POINT('Ctrl Pts',(1.99628883654584,-29.8700078801283,
126.661242908119));
#118375=CARTESIAN_POINT('Ctrl Pts',(1.99399048395441,-29.8374194820291,
126.658370643786));
#118376=CARTESIAN_POINT('Ctrl Pts',(1.9847821400071,-29.7088971794409,126.643218630175));
#118377=CARTESIAN_POINT('Ctrl Pts',(1.97767766267397,-29.6140263671326,
126.623555325442));
#118378=CARTESIAN_POINT('Ctrl Pts',(1.96602669877626,-29.4599741942231,
126.577352386796));
#118379=CARTESIAN_POINT('Ctrl Pts',(1.96143096148941,-29.3996591133522,
126.555397273978));
#118380=CARTESIAN_POINT('Ctrl Pts',(1.95408413825634,-29.3034231438573,
126.513931664385));
#118381=CARTESIAN_POINT('Ctrl Pts',(1.95127556320853,-29.2666900433779,
126.496484346559));
#118382=CARTESIAN_POINT('Ctrl Pts',(1.94745667723266,-29.2168485114291,
126.470534301521));
#118383=CARTESIAN_POINT('Ctrl Pts',(1.9464075744234,-29.2031685027838,126.463166764062));
#118384=CARTESIAN_POINT('Ctrl Pts',(1.9446279972284,-29.1799914855315,126.450263012224));
#118385=CARTESIAN_POINT('Ctrl Pts',(1.94389418643111,-29.1704427602291,
126.444822329682));
#118386=CARTESIAN_POINT('Ctrl Pts',(1.94250262176393,-29.1523548397572,
126.434277737483));
#118387=CARTESIAN_POINT('Ctrl Pts',(1.94184428615079,-29.1438061974481,
126.429191073884));
#118388=CARTESIAN_POINT('Ctrl Pts',(1.94014297667687,-29.1217413344862,
126.415792875408));
#118389=CARTESIAN_POINT('Ctrl Pts',(1.93910432035509,-29.1082971724193,
126.407364148115));
#118390=CARTESIAN_POINT('Ctrl Pts',(1.93547895302539,-29.0614959649165,
126.377082519161));
#118391=CARTESIAN_POINT('Ctrl Pts',(1.93292938595661,-29.0288035226204,
126.354224458256));
#118392=CARTESIAN_POINT('Ctrl Pts',(1.92226532871704,-28.8938147118927,
126.252436993267));
#118393=CARTESIAN_POINT('Ctrl Pts',(1.91454912530594,-28.8000690141589,
126.162931517357));
#118394=CARTESIAN_POINT('Ctrl Pts',(1.9039947584171,-28.6910323785338,126.031451693134));
#118395=CARTESIAN_POINT('Ctrl Pts',(1.90139509278425,-28.6656715165416,
125.998426696306));
#118396=CARTESIAN_POINT('Ctrl Pts',(1.8971183709763,-28.6269165740481,125.943842713647));
#118397=CARTESIAN_POINT('Ctrl Pts',(1.89547924924855,-28.6127310450253,
125.922866102869));
#118398=CARTESIAN_POINT('Ctrl Pts',(1.89321078763743,-28.594098223647,125.893912325633));
#118399=CARTESIAN_POINT('Ctrl Pts',(1.89260666460085,-28.5892296013874,
125.886208735957));
#118400=CARTESIAN_POINT('Ctrl Pts',(1.89158472016883,-28.58115555032,125.873198066411));
#118401=CARTESIAN_POINT('Ctrl Pts',(1.89116908103375,-28.5779160102204,
125.867912184542));
#118402=CARTESIAN_POINT('Ctrl Pts',(1.89030935615627,-28.5713079126132,
125.856993578101));
#118403=CARTESIAN_POINT('Ctrl Pts',(1.88986506879942,-28.5679430360797,
125.851358867813));
#118404=CARTESIAN_POINT('Ctrl Pts',(1.88868237142817,-28.5591153662076,
125.836375934526));
#118405=CARTESIAN_POINT('Ctrl Pts',(1.88794046844187,-28.5537103693259,
125.82699426869));
#118406=CARTESIAN_POINT('Ctrl Pts',(1.88456627219145,-28.5297061820507,
125.784374151944));
#118407=CARTESIAN_POINT('Ctrl Pts',(1.88187901589238,-28.5121601141909,
125.750558922616));
#118408=CARTESIAN_POINT('Ctrl Pts',(1.87551696457238,-28.4738981862066,
125.670195938835));
#118409=CARTESIAN_POINT('Ctrl Pts',(1.87181988333564,-28.4541362594963,
125.623257634171));
#118410=CARTESIAN_POINT('Ctrl Pts',(1.86811697181266,-28.4365600386127,
125.575509762851));
#118411=CARTESIAN_POINT('Origin',(5.,-30.,125.));
#118412=CARTESIAN_POINT('',(1.16625578224439,-28.4365599837819,125.575509613897));
#118413=CARTESIAN_POINT('',(1.36115610141821,-28.4365599811973,125.575509606876));
#118414=CARTESIAN_POINT('',(5.,-28.4365599837785,125.575509613888));
#118415=CARTESIAN_POINT('Ctrl Pts',(1.36115610141822,-28.4365599811973,
125.575509606876));
#118416=CARTESIAN_POINT('Ctrl Pts',(1.36788846393626,-28.4686612718869,
125.662716565578));
#118417=CARTESIAN_POINT('Ctrl Pts',(1.37450638750137,-28.5080098087128,
125.747104294689));
#118418=CARTESIAN_POINT('Ctrl Pts',(1.38236658826502,-28.5649155593372,
125.846494758489));
#118419=CARTESIAN_POINT('Ctrl Pts',(1.38383330985978,-28.5759893934428,
125.864993986104));
#118420=CARTESIAN_POINT('Ctrl Pts',(1.38611240424284,-28.5939088699272,
125.893651803653));
#118421=CARTESIAN_POINT('Ctrl Pts',(1.3869335006038,-28.6005124280402,125.903958163869));
#118422=CARTESIAN_POINT('Ctrl Pts',(1.38846255903877,-28.6130846243825,
125.923111916019));
#118423=CARTESIAN_POINT('Ctrl Pts',(1.38917149278923,-28.6190258112384,
125.931976484495));
#118424=CARTESIAN_POINT('Ctrl Pts',(1.39075636246848,-28.6325578833415,
125.95175350691));
#118425=CARTESIAN_POINT('Ctrl Pts',(1.39163049290498,-28.6401950784762,
125.962633509062));
#118426=CARTESIAN_POINT('Ctrl Pts',(1.39386583866521,-28.6601657541862,
125.99037187657));
#118427=CARTESIAN_POINT('Ctrl Pts',(1.39521979993452,-28.6726877511813,
126.007092109214));
#118428=CARTESIAN_POINT('Ctrl Pts',(1.40488791976394,-28.7650752513151,
126.125736692284));
#118429=CARTESIAN_POINT('Ctrl Pts',(1.41271241556014,-28.8562674498513,
126.218278205338));
#118430=CARTESIAN_POINT('Ctrl Pts',(1.42572359794038,-29.022087177955,126.351351409861));
#118431=CARTESIAN_POINT('Ctrl Pts',(1.43084590381139,-29.0907035378142,
126.398442171754));
#118432=CARTESIAN_POINT('Ctrl Pts',(1.43717049648412,-29.1747029688786,
126.4472867398));
#118433=CARTESIAN_POINT('Ctrl Pts',(1.43809463791653,-29.1869588290539,
126.454207041323));
#118434=CARTESIAN_POINT('Ctrl Pts',(1.43950921612305,-29.2056613105414,
126.464457121626));
#118435=CARTESIAN_POINT('Ctrl Pts',(1.43999279022645,-29.2120447812719,
126.467901625791));
#118436=CARTESIAN_POINT('Ctrl Pts',(1.44088199819808,-29.2237596985939,
126.474124532455));
#118437=CARTESIAN_POINT('Ctrl Pts',(1.4412868161592,-29.2290839555731,126.476915905331));
#118438=CARTESIAN_POINT('Ctrl Pts',(1.44221889466395,-29.2413225440079,
126.483248078116));
#118439=CARTESIAN_POINT('Ctrl Pts',(1.44274731042079,-29.2482465935679,
126.486769367908));
#118440=CARTESIAN_POINT('Ctrl Pts',(1.44438268730008,-29.269639468863,126.497461271443));
#118441=CARTESIAN_POINT('Ctrl Pts',(1.44549867523161,-29.2841876430793,
126.504469802498));
#118442=CARTESIAN_POINT('Ctrl Pts',(1.45226602641753,-29.3722362966567,
126.545320773489));
#118443=CARTESIAN_POINT('Ctrl Pts',(1.45813949948361,-29.4480146701336,
126.573980078569));
#118444=CARTESIAN_POINT('Ctrl Pts',(1.46939065190613,-29.5961995291802,
126.61800200194));
#118445=CARTESIAN_POINT('Ctrl Pts',(1.47475398573363,-29.6681511236861,
126.634277494848));
#118446=CARTESIAN_POINT('Ctrl Pts',(1.48305059776605,-29.7829908697459,
126.652354225002));
#118447=CARTESIAN_POINT('Ctrl Pts',(1.48605149397676,-29.8252751271432,
126.657359095166));
#118448=CARTESIAN_POINT('Ctrl Pts',(1.49113200054262,-29.898241701715,126.663171514866));
#118449=CARTESIAN_POINT('Ctrl Pts',(1.4932331737568,-29.9288385499524,126.664761394697));
#118450=CARTESIAN_POINT('Ctrl Pts',(1.49625572646403,-29.9734451812655,
126.66584706387));
#118451=CARTESIAN_POINT('Ctrl Pts',(1.49719760097907,-29.987430784996,126.666011294724));
#118452=CARTESIAN_POINT('Ctrl Pts',(1.49885320545711,-30.0121596317582,
126.665990259205));
#118453=CARTESIAN_POINT('Ctrl Pts',(1.49956914498663,-30.0229019565679,
126.665877219391));
#118454=CARTESIAN_POINT('Ctrl Pts',(1.50106645181812,-30.0454663869723,
126.665421467763));
#118455=CARTESIAN_POINT('Ctrl Pts',(1.50184709266683,-30.0572874877419,
126.665056759849));
#118456=CARTESIAN_POINT('Ctrl Pts',(1.50391124746068,-30.0886865343674,
126.663753237886));
#118457=CARTESIAN_POINT('Ctrl Pts',(1.50518788387196,-30.108253868072,126.66259474635));
#118458=CARTESIAN_POINT('Ctrl Pts',(1.51177369321979,-30.2098603590109,
126.654777599387));
#118459=CARTESIAN_POINT('Ctrl Pts',(1.51690082711429,-30.2913484268968,
126.642391195443));
#118460=CARTESIAN_POINT('Ctrl Pts',(1.52812413300367,-30.4694627902114,
126.601636704204));
#118461=CARTESIAN_POINT('Ctrl Pts',(1.53416040838146,-30.5650989567957,
126.570444607145));
#118462=CARTESIAN_POINT('Ctrl Pts',(1.54222796926133,-30.6833492661583,
126.519668065507));
#118463=CARTESIAN_POINT('Ctrl Pts',(1.54402239215024,-30.7090687950657,
126.507839020593));
#118464=CARTESIAN_POINT('Ctrl Pts',(1.54709232618714,-30.7518119106759,
126.486844987105));
#118465=CARTESIAN_POINT('Ctrl Pts',(1.54835147935201,-30.769000471379,126.478028200564));
#118466=CARTESIAN_POINT('Ctrl Pts',(1.5501709142979,-30.7932782447822,126.465036924288));
#118467=CARTESIAN_POINT('Ctrl Pts',(1.55071712457215,-30.8004965645595,
126.461105337165));
#118468=CARTESIAN_POINT('Ctrl Pts',(1.55167152424277,-30.8129812863723,
126.45418502708));
#118469=CARTESIAN_POINT('Ctrl Pts',(1.55207818240303,-30.8182609667826,
126.451220746086));
#118470=CARTESIAN_POINT('Ctrl Pts',(1.55295571898963,-30.8295666701918,
126.444791836937));
#118471=CARTESIAN_POINT('Ctrl Pts',(1.55342712302998,-30.8355871155184,
126.441318313332));
#118472=CARTESIAN_POINT('Ctrl Pts',(1.5547375040737,-30.8521816641599,126.431605098145));
#118473=CARTESIAN_POINT('Ctrl Pts',(1.55558122835395,-30.8627085477605,
126.425286176622));
#118474=CARTESIAN_POINT('Ctrl Pts',(1.5614918217239,-30.9354270189733,126.380535081448));
#118475=CARTESIAN_POINT('Ctrl Pts',(1.56676039407081,-30.9950935147074,
126.338165665287));
#118476=CARTESIAN_POINT('Ctrl Pts',(1.57310125013654,-31.062782657917,126.283062887893));
#118477=CARTESIAN_POINT('Ctrl Pts',(1.57413357105327,-31.0736722706845,
126.273964365105));
#118478=CARTESIAN_POINT('Ctrl Pts',(1.58052960975855,-31.1403843568098,
126.216761910754));
#118479=CARTESIAN_POINT('Ctrl Pts',(1.5858932786639,-31.1930839691579,126.165134318634));
#118480=CARTESIAN_POINT('Ctrl Pts',(1.59418936030154,-31.2705486823036,
126.078458410821));
#118481=CARTESIAN_POINT('Ctrl Pts',(1.59718944031677,-31.2976789687186,
126.045655916539));
#118482=CARTESIAN_POINT('Ctrl Pts',(1.60226873464178,-31.34212541195,125.987518739219));
#118483=CARTESIAN_POINT('Ctrl Pts',(1.60436949788008,-31.3600520776271,
125.962679823125));
#118484=CARTESIAN_POINT('Ctrl Pts',(1.60739157896747,-31.3851531554695,
125.925798199347));
#118485=CARTESIAN_POINT('Ctrl Pts',(1.60833338284062,-31.3928758001722,
125.914138171189));
#118486=CARTESIAN_POINT('Ctrl Pts',(1.60998890717904,-31.4062694541386,
125.893351901445));
#118487=CARTESIAN_POINT('Ctrl Pts',(1.61070483649738,-31.4120006269298,
125.884265591495));
#118488=CARTESIAN_POINT('Ctrl Pts',(1.61220216491526,-31.4238559820603,
125.865060698267));
#118489=CARTESIAN_POINT('Ctrl Pts',(1.61298283714817,-31.4299611282615,
125.854931022444));
#118490=CARTESIAN_POINT('Ctrl Pts',(1.61504717540823,-31.4458970170011,
125.827841800432));
#118491=CARTESIAN_POINT('Ctrl Pts',(1.61632396165289,-31.4555373799171,
125.810771989272));
#118492=CARTESIAN_POINT('Ctrl Pts',(1.62291485042368,-31.5041143827149,
125.721098339484));
#118493=CARTESIAN_POINT('Ctrl Pts',(1.62804654001342,-31.5379299118089,
125.645845921156));
#118494=CARTESIAN_POINT('Ctrl Pts',(1.63927012383836,-31.6002711740445,
125.474082420563));
#118495=CARTESIAN_POINT('Ctrl Pts',(1.64530253830474,-31.6259093333768,
125.376879907786));
#118496=CARTESIAN_POINT('Ctrl Pts',(1.65336545592648,-31.647368550382,125.250067249801));
#118497=CARTESIAN_POINT('Ctrl Pts',(1.65515936240895,-31.6513780868515,
125.222051804522));
#118498=CARTESIAN_POINT('Ctrl Pts',(1.65822850200758,-31.6569204286489,
125.17476754759));
#118499=CARTESIAN_POINT('Ctrl Pts',(1.65948738815723,-31.6588349678136,
125.155548944385));
#118500=CARTESIAN_POINT('Ctrl Pts',(1.66130650407048,-31.6610873317372,
125.12811099888));
#118501=CARTESIAN_POINT('Ctrl Pts',(1.66185266904523,-31.6616991175698,
125.119914917138));
#118502=CARTESIAN_POINT('Ctrl Pts',(1.66280701784266,-31.6626562465918,
125.105673410175));
#118503=CARTESIAN_POINT('Ctrl Pts',(1.66321367094054,-31.6630293168683,
125.099630085021));
#118504=CARTESIAN_POINT('Ctrl Pts',(1.66409123053968,-31.6637599111632,
125.086644538431));
#118505=CARTESIAN_POINT('Ctrl Pts',(1.66456266298428,-31.6641069305862,
125.079702178145));
#118506=CARTESIAN_POINT('Ctrl Pts',(1.66587319650753,-31.6649467681416,
125.060490074267));
#118507=CARTESIAN_POINT('Ctrl Pts',(1.66671704656343,-31.6653473769055,
125.048217029552));
#118508=CARTESIAN_POINT('Ctrl Pts',(1.67266115851203,-31.6671998582417,
124.962367891315));
#118509=CARTESIAN_POINT('Ctrl Pts',(1.67796577810366,-31.6639107048638,
124.888778109899));
#118510=CARTESIAN_POINT('Ctrl Pts',(1.68431641348504,-31.6542389518277,
124.801906925831));
#118511=CARTESIAN_POINT('Ctrl Pts',(1.68532286335365,-31.6525370415844,
124.78817767238));
#118512=CARTESIAN_POINT('Ctrl Pts',(1.69169564117011,-31.6406841614922,
124.701425412049));
#118513=CARTESIAN_POINT('Ctrl Pts',(1.69706168589184,-31.6258656535747,
124.629117950333));
#118514=CARTESIAN_POINT('Ctrl Pts',(1.70535296391837,-31.5950414206202,
124.517090609858));
#118515=CARTESIAN_POINT('Ctrl Pts',(1.70834625675692,-31.5822165137071,
124.476597652801));
#118516=CARTESIAN_POINT('Ctrl Pts',(1.71341546965152,-31.557517975688,124.407860939935));
#118517=CARTESIAN_POINT('Ctrl Pts',(1.71551282260845,-31.5463877333739,
124.379374426795));
#118518=CARTESIAN_POINT('Ctrl Pts',(1.71853098494236,-31.5290362697914,
124.338335870974));
#118519=CARTESIAN_POINT('Ctrl Pts',(1.71947220528007,-31.523431603388,124.325531687589));
#118520=CARTESIAN_POINT('Ctrl Pts',(1.72112707262475,-31.5132357084331,
124.303014300458));
#118521=CARTESIAN_POINT('Ctrl Pts',(1.72184292252847,-31.5087104824101,
124.293272284258));
#118522=CARTESIAN_POINT('Ctrl Pts',(1.72334044487439,-31.499003658873,124.272893404998));
#118523=CARTESIAN_POINT('Ctrl Pts',(1.7241213869792,-31.4938023175698,124.262266567121));
#118524=CARTESIAN_POINT('Ctrl Pts',(1.72618728224493,-31.4796747643113,
124.234164767091));
#118525=CARTESIAN_POINT('Ctrl Pts',(1.72746533666611,-31.4705521158834,
124.216790232864));
#118526=CARTESIAN_POINT('Ctrl Pts',(1.73410063103621,-31.4212220551095,
124.126740784834));
#118527=CARTESIAN_POINT('Ctrl Pts',(1.73927216798448,-31.3759265373484,
124.056982253318));
#118528=CARTESIAN_POINT('Ctrl Pts',(1.7504984708822,-31.2651939515627,123.911519598761));
#118529=CARTESIAN_POINT('Ctrl Pts',(1.75649733878881,-31.197775103907,123.837744525143));
#118530=CARTESIAN_POINT('Ctrl Pts',(1.76451990582776,-31.1033380194236,
123.75140165755));
#118531=CARTESIAN_POINT('Ctrl Pts',(1.76630931321811,-31.082028329863,123.732890249487));
#118532=CARTESIAN_POINT('Ctrl Pts',(1.76937153156413,-31.0453909336996,
123.702662192452));
#118533=CARTESIAN_POINT('Ctrl Pts',(1.77062809137023,-31.0303108124198,
123.690653925292));
#118534=CARTESIAN_POINT('Ctrl Pts',(1.77244442768709,-31.0085139627873,
123.673906851498));
#118535=CARTESIAN_POINT('Ctrl Pts',(1.77299019788344,-31.0019646339259,
123.668951421994));
#118536=CARTESIAN_POINT('Ctrl Pts',(1.77394410206363,-30.9905241849914,
123.660427495915));
#118537=CARTESIAN_POINT('Ctrl Pts',(1.77435070976286,-30.9856498185388,
123.656836909152));
#118538=CARTESIAN_POINT('Ctrl Pts',(1.77522846308756,-30.9751340403509,
123.649178779574));
#118539=CARTESIAN_POINT('Ctrl Pts',(1.77570013748638,-30.9694867843727,
123.645120028667));
#118540=CARTESIAN_POINT('Ctrl Pts',(1.77701198407323,-30.9537856616645,
123.633983864675));
#118541=CARTESIAN_POINT('Ctrl Pts',(1.77785692000406,-30.9436788409369,
123.626982376905));
#118542=CARTESIAN_POINT('Ctrl Pts',(1.78405502730907,-30.8695188432329,
123.576813719439));
#118543=CARTESIAN_POINT('Ctrl Pts',(1.78963313685824,-30.8026162129568,
123.538040089812));
#118544=CARTESIAN_POINT('Ctrl Pts',(1.79585997646524,-30.7257112831898,
123.500343346361));
#118545=CARTESIAN_POINT('Ctrl Pts',(1.7964727563374,-30.7181201262464,123.496693501344));
#118546=CARTESIAN_POINT('Ctrl Pts',(1.80260485524155,-30.641906087462,123.460758635482));
#118547=CARTESIAN_POINT('Ctrl Pts',(1.80812732608967,-30.5711776929982,
123.43313533958));
#118548=CARTESIAN_POINT('Ctrl Pts',(1.81655269258082,-30.4585014349004,
123.397777422521));
#118549=CARTESIAN_POINT('Ctrl Pts',(1.81953056155232,-30.4177240239027,
123.386665599608));
#118550=CARTESIAN_POINT('Ctrl Pts',(1.82457684760902,-30.3468879632765,
123.37022918647));
#118551=CARTESIAN_POINT('Ctrl Pts',(1.82666643521057,-30.317025763236,123.364158002776));
#118552=CARTESIAN_POINT('Ctrl Pts',(1.82967566896759,-30.2732638543434,
123.356504438408));
#118553=CARTESIAN_POINT('Ctrl Pts',(1.83061555574374,-30.2594856061424,
123.354272794217));
#118554=CARTESIAN_POINT('Ctrl Pts',(1.83226892021003,-30.2350591650315,
123.350630874847));
#118555=CARTESIAN_POINT('Ctrl Pts',(1.83298458722008,-30.224422490641,123.349149953191));
#118556=CARTESIAN_POINT('Ctrl Pts',(1.83448255040342,-30.2020293257339,
123.346252633924));
#118557=CARTESIAN_POINT('Ctrl Pts',(1.83526410829843,-30.1902705182994,
123.344858513205));
#118558=CARTESIAN_POINT('Ctrl Pts',(1.83733356618749,-30.1589434349058,
123.341482653211));
#118559=CARTESIAN_POINT('Ctrl Pts',(1.83861452390815,-30.1393528672581,
123.339721819512));
#118560=CARTESIAN_POINT('Ctrl Pts',(1.84536578976562,-30.035145169582,123.332213019835));
#118561=CARTESIAN_POINT('Ctrl Pts',(1.85064160769523,-29.9502080533539,
123.332585236987));
#118562=CARTESIAN_POINT('Ctrl Pts',(1.86006752721349,-29.7971209348398,
123.344969977609));
#118563=CARTESIAN_POINT('Ctrl Pts',(1.86423485193548,-29.728992509241,123.354752603964));
#118564=CARTESIAN_POINT('Ctrl Pts',(1.87133723664868,-29.6160284193556,
123.378181863404));
#118565=CARTESIAN_POINT('Ctrl Pts',(1.87423435735936,-29.5708126132314,
123.389557254645));
#118566=CARTESIAN_POINT('Ctrl Pts',(1.87894271517298,-29.4999695551892,
123.410575409003));
#118567=CARTESIAN_POINT('Ctrl Pts',(1.88070590574773,-29.4739991571203,
123.418980112047));
#118568=CARTESIAN_POINT('Ctrl Pts',(1.88311931772348,-29.4394087048879,
123.431121045746));
#118569=CARTESIAN_POINT('Ctrl Pts',(1.88373999266335,-29.4305952629905,
123.434298237665));
#118570=CARTESIAN_POINT('Ctrl Pts',(1.88478196336245,-29.4159466653346,
123.439719006075));
#118571=CARTESIAN_POINT('Ctrl Pts',(1.88520088162678,-29.4100963275817,
123.441921461211));
#118572=CARTESIAN_POINT('Ctrl Pts',(1.88600539554548,-29.3989387397343,
123.446193766397));
#118573=CARTESIAN_POINT('Ctrl Pts',(1.88639062922018,-29.3936294732509,
123.448258000827));
#118574=CARTESIAN_POINT('Ctrl Pts',(1.88743719341928,-29.3792930887035,
123.453916774434));
#118575=CARTESIAN_POINT('Ctrl Pts',(1.88810148028092,-29.3702868302251,
123.457563057199));
#118576=CARTESIAN_POINT('Ctrl Pts',(1.8906836233059,-29.3356183124169,123.471953222355));
#118577=CARTESIAN_POINT('Ctrl Pts',(1.89263038386391,-29.3101962941188,
123.483259873022));
#118578=CARTESIAN_POINT('Ctrl Pts',(1.90246903495523,-29.1846998615746,
123.542882969278));
#118579=CARTESIAN_POINT('Ctrl Pts',(1.91066017172317,-29.0893545877398,
123.600489859609));
#118580=CARTESIAN_POINT('Ctrl Pts',(1.92293836202486,-28.9533952033453,
123.702450529702));
#118581=CARTESIAN_POINT('Ctrl Pts',(1.92713903414929,-28.9082333200005,
123.740213148905));
#118582=CARTESIAN_POINT('Ctrl Pts',(1.93308465529382,-28.8460169087158,
123.798100368657));
#118583=CARTESIAN_POINT('Ctrl Pts',(1.93489690987478,-28.8272948395158,
123.816360513253));
#118584=CARTESIAN_POINT('Ctrl Pts',(1.93814578960179,-28.7941773683414,
123.850218407817));
#118585=CARTESIAN_POINT('Ctrl Pts',(1.93958843785458,-28.7796356634218,
123.865664561606));
#118586=CARTESIAN_POINT('Ctrl Pts',(1.94183878705443,-28.7572227873252,
123.890401495792));
#118587=CARTESIAN_POINT('Ctrl Pts',(1.94265485150414,-28.7491521068725,
123.89950756352));
#118588=CARTESIAN_POINT('Ctrl Pts',(1.9441793570525,-28.734186424162,123.916770552509));
#118589=CARTESIAN_POINT('Ctrl Pts',(1.94488871523273,-28.7272687395855,
123.924906891229));
#118590=CARTESIAN_POINT('Ctrl Pts',(1.94648077899595,-28.7118503751862,
123.943398835323));
#118591=CARTESIAN_POINT('Ctrl Pts',(1.94736160544205,-28.7033953461322,
123.953791671745));
#118592=CARTESIAN_POINT('Ctrl Pts',(1.9496266402695,-28.681858800459,123.980926336417));
#118593=CARTESIAN_POINT('Ctrl Pts',(1.95100325590952,-28.6689702771839,
123.997818730983));
#118594=CARTESIAN_POINT('Ctrl Pts',(1.96045592283178,-28.581995373103,124.116451518948));
#118595=CARTESIAN_POINT('Ctrl Pts',(1.96807467217359,-28.5193221244078,
124.226054404614));
#118596=CARTESIAN_POINT('Ctrl Pts',(1.98103479774366,-28.4355857479652,
124.420718322886));
#118597=CARTESIAN_POINT('Ctrl Pts',(1.98632695518618,-28.4077646928326,
124.502263051839));
#118598=CARTESIAN_POINT('Ctrl Pts',(1.99284280428935,-28.3828620791189,
124.599226384169));
#118599=CARTESIAN_POINT('Ctrl Pts',(1.993767970265,-28.3795304253225,124.612917487288));
#118600=CARTESIAN_POINT('Ctrl Pts',(1.99518379916742,-28.3747467083531,
124.633720872586));
#118601=CARTESIAN_POINT('Ctrl Pts',(1.99566758099685,-28.3731667190938,
124.640803490568));
#118602=CARTESIAN_POINT('Ctrl Pts',(1.99655697683751,-28.3703625519003,
124.653771856634));
#118603=CARTESIAN_POINT('Ctrl Pts',(1.99696177244465,-28.3691238937258,
124.659654202665));
#118604=CARTESIAN_POINT('Ctrl Pts',(1.99789354529921,-28.366358440957,124.673149061158));
#118605=CARTESIAN_POINT('Ctrl Pts',(1.99842167473617,-28.3648530103468,
124.680765609844));
#118606=CARTESIAN_POINT('Ctrl Pts',(2.00005532707843,-28.3603844361573,
124.704235063094));
#118607=CARTESIAN_POINT('Ctrl Pts',(2.00116985069899,-28.3575983056336,
124.720120165698));
#118608=CARTESIAN_POINT('Ctrl Pts',(2.00842378542596,-28.3411134208396,
124.822852298433));
#118609=CARTESIAN_POINT('Ctrl Pts',(2.01482529538982,-28.3340784703978,
124.910620762262));
#118610=CARTESIAN_POINT('Ctrl Pts',(2.02992528091123,-28.3338948384011,
125.118055337291));
#118611=CARTESIAN_POINT('Ctrl Pts',(2.03855840379883,-28.3466531596518,
125.237270689548));
#118612=CARTESIAN_POINT('Ctrl Pts',(2.04828924071552,-28.3766854319895,
125.375336843758));
#118613=CARTESIAN_POINT('Ctrl Pts',(2.04977251375399,-28.3817178198129,
125.396472944023));
#118614=CARTESIAN_POINT('Ctrl Pts',(2.05215864167958,-28.3905545774915,
125.430609635674));
#118615=CARTESIAN_POINT('Ctrl Pts',(2.05306944116974,-28.3941064383024,
125.443672304342));
#118616=CARTESIAN_POINT('Ctrl Pts',(2.05469042476507,-28.4007480633653,
125.466972757659));
#118617=CARTESIAN_POINT('Ctrl Pts',(2.05540250324634,-28.4037778943884,
125.477226688204));
#118618=CARTESIAN_POINT('Ctrl Pts',(2.05691210379892,-28.4104398791914,
125.498999476005));
#118619=CARTESIAN_POINT('Ctrl Pts',(2.05770869996323,-28.4140990152609,
125.510509484949));
#118620=CARTESIAN_POINT('Ctrl Pts',(2.05974160437747,-28.4238044731072,
125.539926704309));
#118621=CARTESIAN_POINT('Ctrl Pts',(2.06097195868479,-28.4300309897374,
125.55777282843));
#118622=CARTESIAN_POINT('Ctrl Pts',(2.06219309044095,-28.4365599837628,
125.575509613845));
#118623=CARTESIAN_POINT('Ctrl Pts',(1.86811697181266,-28.4365600386127,
125.575509762851));
#118624=CARTESIAN_POINT('Ctrl Pts',(1.86507380622595,-28.4221153644137,
125.536269106429));
#118625=CARTESIAN_POINT('Ctrl Pts',(1.86202653433009,-28.4091469471883,
125.49648167022));
#118626=CARTESIAN_POINT('Ctrl Pts',(1.85221160981063,-28.3720165764368,
125.366077255002));
#118627=CARTESIAN_POINT('Ctrl Pts',(1.84555050434239,-28.3539977609925,
125.273905982475));
#118628=CARTESIAN_POINT('Ctrl Pts',(1.83779011161915,-28.3416990096445,
125.161180470645));
#118629=CARTESIAN_POINT('Ctrl Pts',(1.83645740575205,-28.3399149612747,
125.14162994074));
#118630=CARTESIAN_POINT('Ctrl Pts',(1.83433882467471,-28.3376101060971,
125.110253315698));
#118631=CARTESIAN_POINT('Ctrl Pts',(1.8335461498498,-28.3368690990637,125.098445781118));
#118632=CARTESIAN_POINT('Ctrl Pts',(1.83204155045042,-28.3356955867723,
125.075908530718));
#118633=CARTESIAN_POINT('Ctrl Pts',(1.8313289704571,-28.3352409240709,125.06518062015));
#118634=CARTESIAN_POINT('Ctrl Pts',(1.82971233006984,-28.3344411814591,
125.04072354665));
#118635=CARTESIAN_POINT('Ctrl Pts',(1.82881036880894,-28.3341620764283,
125.026992894911));
#118636=CARTESIAN_POINT('Ctrl Pts',(1.82595102331795,-28.3338135964352,
124.9832109419));
#118637=CARTESIAN_POINT('Ctrl Pts',(1.82401355860867,-28.3343874538904,
124.953159536054));
#118638=CARTESIAN_POINT('Ctrl Pts',(1.81305815017193,-28.3423150355948,
124.781509306069));
#118639=CARTESIAN_POINT('Ctrl Pts',(1.80460210868433,-28.3669068000732,
124.641301231028));
#118640=CARTESIAN_POINT('Ctrl Pts',(1.79319080210218,-28.4217437194828,
124.464722451907));
#118641=CARTESIAN_POINT('Ctrl Pts',(1.79050206848774,-28.4361236548606,
124.424061444828));
#118642=CARTESIAN_POINT('Ctrl Pts',(1.78609539047946,-28.4616485909794,
124.3599195207));
#118643=CARTESIAN_POINT('Ctrl Pts',(1.78441829244063,-28.4717943011066,
124.336060813831));
#118644=CARTESIAN_POINT('Ctrl Pts',(1.78210541589467,-28.4862855740065,
124.304076769783));
#118645=CARTESIAN_POINT('Ctrl Pts',(1.78149614364694,-28.4901484884623,
124.295735199441));
#118646=CARTESIAN_POINT('Ctrl Pts',(1.78046801842268,-28.4967383658165,
124.281808462095));
#118647=CARTESIAN_POINT('Ctrl Pts',(1.78005140828074,-28.4994279859631,
124.276205654222));
#118648=CARTESIAN_POINT('Ctrl Pts',(1.77924673172392,-28.5046583715688,
124.26546458883));
#118649=CARTESIAN_POINT('Ctrl Pts',(1.77885898841059,-28.5071944037697,
124.26032418903));
#118650=CARTESIAN_POINT('Ctrl Pts',(1.77779679374661,-28.5141856959868,
124.246335622485));
#118651=CARTESIAN_POINT('Ctrl Pts',(1.77711923438104,-28.5186933455285,
124.237514115988));
#118652=CARTESIAN_POINT('Ctrl Pts',(1.77441855530079,-28.5368592990006,
124.202732307009));
#118653=CARTESIAN_POINT('Ctrl Pts',(1.7723631833118,-28.5511227456628,124.177096033721));
#118654=CARTESIAN_POINT('Ctrl Pts',(1.76323958719341,-28.6166122338677,
124.066374415666));
#118655=CARTESIAN_POINT('Ctrl Pts',(1.75594226835794,-28.6747096118142,
123.985592427633));
#118656=CARTESIAN_POINT('Ctrl Pts',(1.74289414544669,-28.7924506631414,
123.849392142191));
#118657=CARTESIAN_POINT('Ctrl Pts',(1.73712358656608,-28.8496239719627,
123.792228526141));
#118658=CARTESIAN_POINT('Ctrl Pts',(1.72944788712227,-28.9333659717816,
123.719865926375));
#118659=CARTESIAN_POINT('Ctrl Pts',(1.72739640814584,-28.9565313351256,
123.700913882034));
#118660=CARTESIAN_POINT('Ctrl Pts',(1.7244312253868,-28.9911550936886,123.674111609039));
#118661=CARTESIAN_POINT('Ctrl Pts',(1.72349810535745,-29.0022198876238,
123.665765036519));
#118662=CARTESIAN_POINT('Ctrl Pts',(1.72185253039298,-29.0220290460688,
123.651206533345));
#118663=CARTESIAN_POINT('Ctrl Pts',(1.72113795325958,-29.0307315363274,
123.644939242323));
#118664=CARTESIAN_POINT('Ctrl Pts',(1.71963821619544,-29.0492051457759,
123.631904096242));
#118665=CARTESIAN_POINT('Ctrl Pts',(1.71885383327985,-29.0589894300226,
123.625155872033));
#118666=CARTESIAN_POINT('Ctrl Pts',(1.71676728307705,-29.0853371754616,
123.607396875484));
#118667=CARTESIAN_POINT('Ctrl Pts',(1.71547227186718,-29.1020273093401,
123.59657681126));
#118668=CARTESIAN_POINT('Ctrl Pts',(1.70786663011725,-29.2019532968336,
123.53430834638));
#118669=CARTESIAN_POINT('Ctrl Pts',(1.70182310428485,-29.2894007701753,
123.489972588029));
#118670=CARTESIAN_POINT('Ctrl Pts',(1.69132001184899,-29.4487947514026,
123.426093190352));
#118671=CARTESIAN_POINT('Ctrl Pts',(1.68684291800265,-29.5190929260357,
123.403210285008));
#118672=CARTESIAN_POINT('Ctrl Pts',(1.68009638892401,-29.6242251188271,
123.376563138935));
#118673=CARTESIAN_POINT('Ctrl Pts',(1.67791885507917,-29.6580311902958,
123.369107287598));
#118674=CARTESIAN_POINT('Ctrl Pts',(1.67426724128406,-29.7139608452303,
123.358587497524));
#118675=CARTESIAN_POINT('Ctrl Pts',(1.67281870032706,-29.7359583037017,
123.354905696476));
#118676=CARTESIAN_POINT('Ctrl Pts',(1.67077435051358,-29.7666177373059,
123.350404836485));
#118677=CARTESIAN_POINT('Ctrl Pts',(1.67019777112628,-29.7752232667888,
123.349210220518));
#118678=CARTESIAN_POINT('Ctrl Pts',(1.669208500349,-29.7899088440469,123.347288531397));
#118679=CARTESIAN_POINT('Ctrl Pts',(1.66879767318598,-29.7959844151418,
123.346527553219));
#118680=CARTESIAN_POINT('Ctrl Pts',(1.6679319489996,-29.8087358772128,123.345001756501));
#118681=CARTESIAN_POINT('Ctrl Pts',(1.667476708849,-29.8154123293023,123.34424381672));
#118682=CARTESIAN_POINT('Ctrl Pts',(1.66623351460583,-29.83357147366,123.342293506081));
#118683=CARTESIAN_POINT('Ctrl Pts',(1.66544143815951,-29.8450620205992,
123.34118009468));
#118684=CARTESIAN_POINT('Ctrl Pts',(1.66137119312437,-29.9037525662682,
123.336108195918));
#118685=CARTESIAN_POINT('Ctrl Pts',(1.65800790581231,-29.9510904001124,
123.334044873267));
#118686=CARTESIAN_POINT('Ctrl Pts',(1.64734994428443,-30.0992582882437,
123.333906739861));
#118687=CARTESIAN_POINT('Ctrl Pts',(1.63993754762206,-30.1998709535915,
123.342962959158));
#118688=CARTESIAN_POINT('Ctrl Pts',(1.62718882987642,-30.3743591862255,
123.374801130531));
#118689=CARTESIAN_POINT('Ctrl Pts',(1.621793337005,-30.4486393844416,123.393717996614));
#118690=CARTESIAN_POINT('Ctrl Pts',(1.6152699581377,-30.5392789919135,123.423583198221));
#118691=CARTESIAN_POINT('Ctrl Pts',(1.61399054570287,-30.5570923822157,
123.42978985722));
#118692=CARTESIAN_POINT('Ctrl Pts',(1.61193589368605,-30.5857478222201,
123.440323235905));
#118693=CARTESIAN_POINT('Ctrl Pts',(1.61115456716329,-30.5966561094524,
123.444463559178));
#118694=CARTESIAN_POINT('Ctrl Pts',(1.60965832785233,-30.6175628961522,
123.452651173079));
#118695=CARTESIAN_POINT('Ctrl Pts',(1.60894289641922,-30.6275673117454,
123.45668162668));
#118696=CARTESIAN_POINT('Ctrl Pts',(1.60728520335356,-30.6507607309003,
123.466288328642));
#118697=CARTESIAN_POINT('Ctrl Pts',(1.60634547388183,-30.6639185159585,
123.471938075514));
#118698=CARTESIAN_POINT('Ctrl Pts',(1.60328416879503,-30.7067917353428,
123.491005504918));
#118699=CARTESIAN_POINT('Ctrl Pts',(1.60118649386411,-30.7361874085937,
123.505126337104));
#118700=CARTESIAN_POINT('Ctrl Pts',(1.59616232716592,-30.8063831766521,
123.541419630566));
#118701=CARTESIAN_POINT('Ctrl Pts',(1.59326379285336,-30.8467079619909,
123.564452503418));
#118702=CARTESIAN_POINT('Ctrl Pts',(1.58617264115953,-30.9438936146995,
123.625485157041));
#118703=CARTESIAN_POINT('Ctrl Pts',(1.58202372174999,-30.9994758592016,
123.66535606554));
#118704=CARTESIAN_POINT('Ctrl Pts',(1.57720953188181,-31.060458843643,123.715052646713));
#118705=CARTESIAN_POINT('Ctrl Pts',(1.57657680197812,-31.0684038611822,
123.721651124768));
#118706=CARTESIAN_POINT('Ctrl Pts',(1.57130492344091,-31.1339656892536,
123.777139540133));
#118707=CARTESIAN_POINT('Ctrl Pts',(1.56661391594483,-31.1882492572264,
123.829817680767));
#118708=CARTESIAN_POINT('Ctrl Pts',(1.56087690935004,-31.2469782870881,
123.895123506874));
#118709=CARTESIAN_POINT('Ctrl Pts',(1.56006816542347,-31.2550911584685,
123.9043481047));
#118710=CARTESIAN_POINT('Ctrl Pts',(1.55879056472725,-31.2676334544057,
123.918931204264));
#118711=CARTESIAN_POINT('Ctrl Pts',(1.55832659142073,-31.2721327971966,
123.924229365635));
#118712=CARTESIAN_POINT('Ctrl Pts',(1.55745402692494,-31.2804877712706,
123.934193402581));
#118713=CARTESIAN_POINT('Ctrl Pts',(1.55704601157548,-31.2843512996369,
123.938852333591));
#118714=CARTESIAN_POINT('Ctrl Pts',(1.55608009878621,-31.2933970186093,
123.949882104392));
#118715=CARTESIAN_POINT('Ctrl Pts',(1.5555207189523,-31.2985575829968,123.956270322833));
#118716=CARTESIAN_POINT('Ctrl Pts',(1.55363771165736,-31.3156765433867,
123.977785221583));
#118717=CARTESIAN_POINT('Ctrl Pts',(1.55230056703928,-31.3274190199453,
123.993080695204));
#118718=CARTESIAN_POINT('Ctrl Pts',(1.54897259289164,-31.3556972302696,
124.031269682337));
#118719=CARTESIAN_POINT('Ctrl Pts',(1.54696722421238,-31.3719210836055,
124.054386035962));
#118720=CARTESIAN_POINT('Ctrl Pts',(1.53778875379205,-31.4428221876711,
124.161076157434));
#118721=CARTESIAN_POINT('Ctrl Pts',(1.53044401739243,-31.4905049128045,
124.249050862079));
#118722=CARTESIAN_POINT('Ctrl Pts',(1.51726303442301,-31.5628314648221,
124.416914521819));
#118723=CARTESIAN_POINT('Ctrl Pts',(1.51139766484842,-31.5899143449385,
124.495414052926));
#118724=CARTESIAN_POINT('Ctrl Pts',(1.50437947005127,-31.6160376457289,
124.594582861553));
#118725=CARTESIAN_POINT('Ctrl Pts',(1.50304780839145,-31.620698918698,124.613637734058));
#118726=CARTESIAN_POINT('Ctrl Pts',(1.50093048344589,-31.6276297275352,
124.644307230836));
#118727=CARTESIAN_POINT('Ctrl Pts',(1.5001380347067,-31.6301138226258,124.655870934442));
#118728=CARTESIAN_POINT('Ctrl Pts',(1.4986336177817,-31.6346179270985,124.677982092531));
#118729=CARTESIAN_POINT('Ctrl Pts',(1.49792099676429,-31.6366594993558,
124.688524491013));
#118730=CARTESIAN_POINT('Ctrl Pts',(1.49628852560322,-31.641122634375,124.712828083852));
#118731=CARTESIAN_POINT('Ctrl Pts',(1.49537096111671,-31.6434733171178,
124.726601598204));
#118732=CARTESIAN_POINT('Ctrl Pts',(1.49246288915985,-31.6504133584525,
124.770596330839));
#118733=CARTESIAN_POINT('Ctrl Pts',(1.4904929884044,-31.6543445967275,124.80091599706));
#118734=CARTESIAN_POINT('Ctrl Pts',(1.48584078088412,-31.6617364871279,
124.873551828445));
#118735=CARTESIAN_POINT('Ctrl Pts',(1.48318096006398,-31.6644185921562,
124.915926095558));
#118736=CARTESIAN_POINT('Ctrl Pts',(1.47597758258143,-31.6673225367432,
125.032072502706));
#118737=CARTESIAN_POINT('Ctrl Pts',(1.47150185678151,-31.6642697272068,
125.105828779475));
#118738=CARTESIAN_POINT('Ctrl Pts',(1.46616138228397,-31.65488286836,125.192620150486));
#118739=CARTESIAN_POINT('Ctrl Pts',(1.46533081335207,-31.6532604815924,
125.206081549259));
#118740=CARTESIAN_POINT('Ctrl Pts',(1.45995991371941,-31.641737361191,125.292770689231));
#118741=CARTESIAN_POINT('Ctrl Pts',(1.4553672672533,-31.6271393720648,125.3652819901));
#118742=CARTESIAN_POINT('Ctrl Pts',(1.44973966190952,-31.6045629908535,
125.448424314081));
#118743=CARTESIAN_POINT('Ctrl Pts',(1.44893132812255,-31.6012146814024,
125.460237199035));
#118744=CARTESIAN_POINT('Ctrl Pts',(1.44765423888298,-31.5957673048699,
125.478676304118));
#118745=CARTESIAN_POINT('Ctrl Pts',(1.44719036069773,-31.5937567357226,
125.485328505634));
#118746=CARTESIAN_POINT('Ctrl Pts',(1.44631786977977,-31.5899172011883,
125.497750873927));
#118747=CARTESIAN_POINT('Ctrl Pts',(1.44590983168935,-31.58809833254,125.503523902745));
#118748=CARTESIAN_POINT('Ctrl Pts',(1.44494372540347,-31.5837368542093,
125.517108363582));
#118749=CARTESIAN_POINT('Ctrl Pts',(1.44438417298862,-31.5811678829483,
125.524911041919));
#118750=CARTESIAN_POINT('Ctrl Pts',(1.44249997093948,-31.572371154149,125.550978531556));
#118751=CARTESIAN_POINT('Ctrl Pts',(1.44116178172606,-31.5658840312772,
125.56915332724));
#118752=CARTESIAN_POINT('Ctrl Pts',(1.43783062883177,-31.5491195024646,
125.61366428117));
#118753=CARTESIAN_POINT('Ctrl Pts',(1.43582309281918,-31.5384848063226,
125.639858893239));
#118754=CARTESIAN_POINT('Ctrl Pts',(1.42662547824706,-31.4871879703489,
125.757527368973));
#118755=CARTESIAN_POINT('Ctrl Pts',(1.41926324016873,-31.4389985613409,
125.845493561222));
#118756=CARTESIAN_POINT('Ctrl Pts',(1.40608610372879,-31.3371370522766,
125.997221735599));
#118757=CARTESIAN_POINT('Ctrl Pts',(1.40024031433766,-31.286022652747,126.062325811389));
#118758=CARTESIAN_POINT('Ctrl Pts',(1.39324099829267,-31.2170577152728,
126.137853656378));
#118759=CARTESIAN_POINT('Ctrl Pts',(1.39190987258097,-31.203581940568,126.152098517906));
#118760=CARTESIAN_POINT('Ctrl Pts',(1.38979318485049,-31.1815802686629,
126.174548384569));
#118761=CARTESIAN_POINT('Ctrl Pts',(1.38900084479733,-31.1732133457474,
126.182905869809));
#118762=CARTESIAN_POINT('Ctrl Pts',(1.38749650259467,-31.1570801498742,
126.198681291522));
#118763=CARTESIAN_POINT('Ctrl Pts',(1.38678384898385,-31.1493297886649,
126.206114570833));
#118764=CARTESIAN_POINT('Ctrl Pts',(1.38515111750396,-31.1313286923256,
126.223048117867));
#118765=CARTESIAN_POINT('Ctrl Pts',(1.3842333277029,-31.1210291115083,126.23249546026));
#118766=CARTESIAN_POINT('Ctrl Pts',(1.38132376112342,-31.0878132640032,
126.262201966602));
#118767=CARTESIAN_POINT('Ctrl Pts',(1.37935262149001,-31.0644567011252,
126.281960850171));
#118768=CARTESIAN_POINT('Ctrl Pts',(1.37469686096672,-31.007393866691,126.32759861474));
#118769=CARTESIAN_POINT('Ctrl Pts',(1.37203477449641,-30.9732154852828,
126.352853459575));
#118770=CARTESIAN_POINT('Ctrl Pts',(1.36483014601865,-30.8771827560328,
126.41828822623));
#118771=CARTESIAN_POINT('Ctrl Pts',(1.36035528791055,-30.8135686718883,
126.455712012325));
#118772=CARTESIAN_POINT('Ctrl Pts',(1.35500291977246,-30.7353836908596,
126.494977026586));
#118773=CARTESIAN_POINT('Ctrl Pts',(1.35415964654401,-30.7230065298141,
126.501002010302));
#118774=CARTESIAN_POINT('Ctrl Pts',(1.34879149638914,-30.6439561367631,
126.538277715496));
#118775=CARTESIAN_POINT('Ctrl Pts',(1.34421419432254,-30.5753553621518,
126.56522883206));
#118776=CARTESIAN_POINT('Ctrl Pts',(1.33860362850015,-30.4935078477781,
126.591275193368));
#118777=CARTESIAN_POINT('Ctrl Pts',(1.33779534773215,-30.4817680948006,
126.594868714949));
#118778=CARTESIAN_POINT('Ctrl Pts',(1.33651831903953,-30.4633230019829,
126.600292501335));
#118779=CARTESIAN_POINT('Ctrl Pts',(1.33605444740146,-30.4566438269569,
126.602211192361));
#118780=CARTESIAN_POINT('Ctrl Pts',(1.33518194067076,-30.4441245916519,
126.605722887128));
#118781=CARTESIAN_POINT('Ctrl Pts',(1.33477387992873,-30.4382876014881,
126.607325921168));
#118782=CARTESIAN_POINT('Ctrl Pts',(1.33380768559873,-30.4245079269523,
126.611029645546));
#118783=CARTESIAN_POINT('Ctrl Pts',(1.33324806727611,-30.4165582965145,
126.613103430473));
#118784=CARTESIAN_POINT('Ctrl Pts',(1.33136350594978,-30.3898817256404,
126.619852089884));
#118785=CARTESIAN_POINT('Ctrl Pts',(1.3300250179637,-30.3710897109862,126.62426010852));
#118786=CARTESIAN_POINT('Ctrl Pts',(1.32669297214444,-30.3245891781903,
126.634318640945));
#118787=CARTESIAN_POINT('Ctrl Pts',(1.32468483402052,-30.2968057496918,
126.63959193741));
#118788=CARTESIAN_POINT('Ctrl Pts',(1.31548177323326,-30.170050631906,126.660322863488));
#118789=CARTESIAN_POINT('Ctrl Pts',(1.30811456342572,-30.0699421225484,
126.667542438152));
#118790=CARTESIAN_POINT('Ctrl Pts',(1.29493956998774,-29.8872451506476,
126.664229037536));
#118791=CARTESIAN_POINT('Ctrl Pts',(1.28910034246893,-29.8049155354336,
126.656598228925));
#118792=CARTESIAN_POINT('Ctrl Pts',(1.28210734922354,-29.7041476141675,
126.639637670252));
#118793=CARTESIAN_POINT('Ctrl Pts',(1.28077640473921,-29.6848736145989,
126.636042707907));
#118794=CARTESIAN_POINT('Ctrl Pts',(1.27865991865501,-29.6540823485395,
126.62973519622));
#118795=CARTESIAN_POINT('Ctrl Pts',(1.27786760187127,-29.6425232182577,
126.627238825245));
#118796=CARTESIAN_POINT('Ctrl Pts',(1.27636324985426,-29.6205192690064,
126.622240949328));
#118797=CARTESIAN_POINT('Ctrl Pts',(1.27565056370567,-29.6100701938365,
126.61976111768));
#118798=CARTESIAN_POINT('Ctrl Pts',(1.27401768056143,-29.5860780685762,
126.613821549831));
#118799=CARTESIAN_POINT('Ctrl Pts',(1.27309977271339,-29.5725529990944,
126.610292035984));
#118800=CARTESIAN_POINT('Ctrl Pts',(1.27018950330272,-29.5295695274094,
126.598495301101));
#118801=CARTESIAN_POINT('Ctrl Pts',(1.26821779246539,-29.5002927490674,
126.589586395517));
#118802=CARTESIAN_POINT('Ctrl Pts',(1.26356042384791,-29.4309771687159,
126.566389138686));
#118803=CARTESIAN_POINT('Ctrl Pts',(1.26089732183558,-29.3912068677028,
126.551364953231));
#118804=CARTESIAN_POINT('Ctrl Pts',(1.25369207673303,-29.2841383915049,
126.506164823711));
#118805=CARTESIAN_POINT('Ctrl Pts',(1.24921755584633,-29.2182006897815,
126.473017489033));
#118806=CARTESIAN_POINT('Ctrl Pts',(1.24385974689897,-29.1427325433927,
126.428579917327));
#118807=CARTESIAN_POINT('Ctrl Pts',(1.24301071820361,-29.1308783650678,
126.421399187487));
#118808=CARTESIAN_POINT('Ctrl Pts',(1.23764363505311,-29.0567142633553,
126.37519924064));
#118809=CARTESIAN_POINT('Ctrl Pts',(1.23307310874791,-28.9969623534156,
126.332243850096));
#118810=CARTESIAN_POINT('Ctrl Pts',(1.22747006464366,-28.9307767818416,
126.27768088221));
#118811=CARTESIAN_POINT('Ctrl Pts',(1.22666180965119,-28.921390696961,126.269767174192));
#118812=CARTESIAN_POINT('Ctrl Pts',(1.225384812915,-28.9068301951148,126.257212818276));
#118813=CARTESIAN_POINT('Ctrl Pts',(1.22492094706501,-28.9015956841964,
126.25264210667));
#118814=CARTESIAN_POINT('Ctrl Pts',(1.2240484838881,-28.891855752849,126.244029325954));
#118815=CARTESIAN_POINT('Ctrl Pts',(1.22364046120809,-28.8873435676677,
126.239995280331));
#118816=CARTESIAN_POINT('Ctrl Pts',(1.2226743783183,-28.8767594002408,126.230428395339));
#118817=CARTESIAN_POINT('Ctrl Pts',(1.22211483383591,-28.8707062487426,
126.224875135393));
#118818=CARTESIAN_POINT('Ctrl Pts',(1.22023053591187,-28.8505705235727,
126.206126164516));
#118819=CARTESIAN_POINT('Ctrl Pts',(1.21889223925896,-28.8366767947949,
126.192731104189));
#118820=CARTESIAN_POINT('Ctrl Pts',(1.21556072260696,-28.8030106663786,
126.159125452884));
#118821=CARTESIAN_POINT('Ctrl Pts',(1.21355292466535,-28.7835144406899,
126.138647436167));
#118822=CARTESIAN_POINT('Ctrl Pts',(1.20435287453867,-28.6973758016848,
126.043432737066));
#118823=CARTESIAN_POINT('Ctrl Pts',(1.19698837360285,-28.6370327986885,
125.963276978598));
#118824=CARTESIAN_POINT('Ctrl Pts',(1.1838111571639,-28.5407003015419,125.807976853129));
#118825=CARTESIAN_POINT('Ctrl Pts',(1.17796734596364,-28.5024267616088,
125.734615752706));
#118826=CARTESIAN_POINT('Ctrl Pts',(1.17097000890308,-28.4619995623678,
125.640698850335));
#118827=CARTESIAN_POINT('Ctrl Pts',(1.16963899419521,-28.4545662236487,
125.622555108296));
#118828=CARTESIAN_POINT('Ctrl Pts',(1.1676281026626,-28.4437346288164,125.594726220909));
#118829=CARTESIAN_POINT('Ctrl Pts',(1.16694046674226,-28.4401029340819,
125.585134457932));
#118830=CARTESIAN_POINT('Ctrl Pts',(1.16625578224439,-28.4365599837819,
125.575509613897));
#118831=CARTESIAN_POINT('Origin',(5.,-30.,125.));
#118832=CARTESIAN_POINT('',(0.468139978699824,-28.4365599867671,125.575509622007));
#118833=CARTESIAN_POINT('',(0.659203971007262,-28.4365599837785,125.575509613888));
#118834=CARTESIAN_POINT('',(5.,-28.4365599837785,125.575509613888));
#118835=CARTESIAN_POINT('',(0.,-31.2690708798524,126.079358653049));
#118836=CARTESIAN_POINT('Ctrl Pts',(0.468139978699828,-28.4365599867671,
125.575509622007));
#118837=CARTESIAN_POINT('Ctrl Pts',(0.467368748069218,-28.4321976756175,
125.563658887387));
#118838=CARTESIAN_POINT('Ctrl Pts',(0.46659689192531,-28.4279697232914,
125.551757515043));
#118839=CARTESIAN_POINT('Ctrl Pts',(0.461140943886784,-28.3990928442639,
125.467443220244));
#118840=CARTESIAN_POINT('Ctrl Pts',(0.456419851168978,-28.3793245969748,
125.393465849614));
#118841=CARTESIAN_POINT('Ctrl Pts',(0.450407026927721,-28.3615908870582,
125.302386837636));
#118842=CARTESIAN_POINT('Ctrl Pts',(0.449339284521711,-28.3587081421932,
125.286327102347));
#118843=CARTESIAN_POINT('Ctrl Pts',(0.447751303682339,-28.3548178634009,
125.26266053574));
#118844=CARTESIAN_POINT('Ctrl Pts',(0.447240785306152,-28.3536261759322,
125.255084388493));
#118845=CARTESIAN_POINT('Ctrl Pts',(0.446325473091858,-28.3515952030916,
125.241565002395));
#118846=CARTESIAN_POINT('Ctrl Pts',(0.445921813156161,-28.3507356650182,
125.235625073383));
#118847=CARTESIAN_POINT('Ctrl Pts',(0.445021439516117,-28.3488983811264,
125.222425493121));
#118848=CARTESIAN_POINT('Ctrl Pts',(0.444523896583313,-28.3479364122372,
125.215164013547));
#118849=CARTESIAN_POINT('Ctrl Pts',(0.443043358912694,-28.3452299649791,
125.193645158876));
#118850=CARTESIAN_POINT('Ctrl Pts',(0.442053398234113,-28.3436220033341,
125.179371720183));
#118851=CARTESIAN_POINT('Ctrl Pts',(0.434511562346096,-28.3328672750034,
125.071368248408));
#118852=CARTESIAN_POINT('Ctrl Pts',(0.427644809121563,-28.3314993061057,
124.97704308329));
#118853=CARTESIAN_POINT('Ctrl Pts',(0.412301175541919,-28.3462867398635,
124.766787187021));
#118854=CARTESIAN_POINT('Ctrl Pts',(0.403887832506857,-28.3666615733685,
124.651617514269));
#118855=CARTESIAN_POINT('Ctrl Pts',(0.394336778889793,-28.4049792138424,
124.518390809573));
#118856=CARTESIAN_POINT('Ctrl Pts',(0.392836116317528,-28.4114694578954,
124.497397257524));
#118857=CARTESIAN_POINT('Ctrl Pts',(0.390425163645169,-28.4226607832197,
124.463583005454));
#118858=CARTESIAN_POINT('Ctrl Pts',(0.389506752829867,-28.4271073096314,
124.450681512634));
#118859=CARTESIAN_POINT('Ctrl Pts',(0.387873944840566,-28.4353402863902,
124.427713706725));
#118860=CARTESIAN_POINT('Ctrl Pts',(0.387157617190256,-28.4390665929141,
124.417626813142));
#118861=CARTESIAN_POINT('Ctrl Pts',(0.38564067839487,-28.4472004636079,
124.396247971283));
#118862=CARTESIAN_POINT('Ctrl Pts',(0.384840982115183,-28.451634147513,
124.384966576334));
#118863=CARTESIAN_POINT('Ctrl Pts',(0.382679879299442,-28.4640094803565,
124.354460107499));
#118864=CARTESIAN_POINT('Ctrl Pts',(0.381326458947623,-28.472188837654,
124.335333359092));
#118865=CARTESIAN_POINT('Ctrl Pts',(0.372837115258115,-28.5261676930721,
124.215373670924));
#118866=CARTESIAN_POINT('Ctrl Pts',(0.366048427726499,-28.5815683830622,
124.119161806243));
#118867=CARTESIAN_POINT('Ctrl Pts',(0.352975786852313,-28.7061986620622,
123.945360216557));
#118868=CARTESIAN_POINT('Ctrl Pts',(0.346709127500906,-28.773924212927,
123.867339647326));
#118869=CARTESIAN_POINT('Ctrl Pts',(0.3390079119112,-28.8596678157877,123.785322642221));
#118870=CARTESIAN_POINT('Ctrl Pts',(0.337987558499198,-28.8710726403485,
123.774715727569));
#118871=CARTESIAN_POINT('Ctrl Pts',(0.336453321402609,-28.8882529839161,
123.75918084932));
#118872=CARTESIAN_POINT('Ctrl Pts',(0.335947999885583,-28.8939165599583,
123.754129617259));
#118873=CARTESIAN_POINT('Ctrl Pts',(0.335031387501064,-28.9041940363187,
123.745088650751));
#118874=CARTESIAN_POINT('Ctrl Pts',(0.334621091419679,-28.9087956159959,
123.741085311536));
#118875=CARTESIAN_POINT('Ctrl Pts',(0.333691633453243,-28.9192227552468,
123.732113899224));
#118876=CARTESIAN_POINT('Ctrl Pts',(0.333171471614641,-28.9250606613696,
123.727160642531));
#118877=CARTESIAN_POINT('Ctrl Pts',(0.331579571740426,-28.94294051283,123.712200955946));
#118878=CARTESIAN_POINT('Ctrl Pts',(0.330499591107477,-28.9550891848959,
123.702324199624));
#118879=CARTESIAN_POINT('Ctrl Pts',(0.324968622064915,-29.0174852076867,
123.653041099372));
#118880=CARTESIAN_POINT('Ctrl Pts',(0.320382356874171,-29.0698254037879,
123.616378914318));
#118881=CARTESIAN_POINT('Ctrl Pts',(0.307594145872618,-29.2201247827609,
123.523489179777));
#118882=CARTESIAN_POINT('Ctrl Pts',(0.299371107691596,-29.32190694204,123.474062568239));
#118883=CARTESIAN_POINT('Ctrl Pts',(0.288538190039219,-29.4669380836437,
123.421035900165));
#118884=CARTESIAN_POINT('Ctrl Pts',(0.28566477727477,-29.506486954433,123.408231166247));
#118885=CARTESIAN_POINT('Ctrl Pts',(0.281736140891163,-29.5620666088561,
123.392507277488));
#118886=CARTESIAN_POINT('Ctrl Pts',(0.280641395479728,-29.5777207845674,
123.388324224919));
#118887=CARTESIAN_POINT('Ctrl Pts',(0.278876966986034,-29.6032151612703,
123.381908679414));
#118888=CARTESIAN_POINT('Ctrl Pts',(0.278202872197144,-29.6130186742796,
123.37953611852));
#118889=CARTESIAN_POINT('Ctrl Pts',(0.276793528398858,-29.6336454703021,
123.374742067139));
#118890=CARTESIAN_POINT('Ctrl Pts',(0.276058904642824,-29.6444726371476,
123.372339318523));
#118891=CARTESIAN_POINT('Ctrl Pts',(0.274300036745198,-29.6705712816732,
123.366820395673));
#118892=CARTESIAN_POINT('Ctrl Pts',(0.273279172806765,-29.6858642494674,
123.363810017885));
#118893=CARTESIAN_POINT('Ctrl Pts',(0.269644912271854,-29.7407968926573,
123.35379528363));
#118894=CARTESIAN_POINT('Ctrl Pts',(0.26706962256692,-29.7806469542651,
123.348013055479));
#118895=CARTESIAN_POINT('Ctrl Pts',(0.260566485341825,-29.8830994927785,
123.336920507761));
#118896=CARTESIAN_POINT('Ctrl Pts',(0.256695438207355,-29.945864358662,
123.333695911863));
#118897=CARTESIAN_POINT('Ctrl Pts',(0.24718554235897,-30.1012499221996,
123.334504061874));
#118898=CARTESIAN_POINT('Ctrl Pts',(0.241599868013843,-30.1936275022724,
123.342702671986));
#118899=CARTESIAN_POINT('Ctrl Pts',(0.233335296901047,-30.3232338269278,
123.365192840516));
#118900=CARTESIAN_POINT('Ctrl Pts',(0.230847500990398,-30.3613798305607,
123.373199876346));
#118901=CARTESIAN_POINT('Ctrl Pts',(0.227579176300134,-30.409780455689,
123.385145642556));
#118902=CARTESIAN_POINT('Ctrl Pts',(0.226860039358787,-30.4203281403454,
123.387858921663));
#118903=CARTESIAN_POINT('Ctrl Pts',(0.225698073261801,-30.437191994417,
123.392373709684));
#118904=CARTESIAN_POINT('Ctrl Pts',(0.22525889397465,-30.4435256372307,
123.394109550851));
#118905=CARTESIAN_POINT('Ctrl Pts',(0.224417262638342,-30.4555826264015,
123.397490738284));
#118906=CARTESIAN_POINT('Ctrl Pts',(0.224015204558463,-30.4613075824727,
123.399129369328));
#118907=CARTESIAN_POINT('Ctrl Pts',(0.223037323746592,-30.4751457723425,
123.403170614169));
#118908=CARTESIAN_POINT('Ctrl Pts',(0.22245970028393,-30.4832493309913,
123.405604293667));
#118909=CARTESIAN_POINT('Ctrl Pts',(0.220318835722793,-30.5130386605514,
123.41479865206));
#118910=CARTESIAN_POINT('Ctrl Pts',(0.218734838832397,-30.5346028945158,
123.421940561418));
#118911=CARTESIAN_POINT('Ctrl Pts',(0.208556855507809,-30.6705895275747,
123.470085303734));
#118912=CARTESIAN_POINT('Ctrl Pts',(0.19951277548354,-30.7803774165809,
123.523064373845));
#118913=CARTESIAN_POINT('Ctrl Pts',(0.183896431781186,-30.9624118037013,
123.636915427585));
#118914=CARTESIAN_POINT('Ctrl Pts',(0.177260327323807,-31.0371295421189,
123.692864231471));
#118915=CARTESIAN_POINT('Ctrl Pts',(0.169541363277904,-31.1213726954637,
123.767741887473));
#118916=CARTESIAN_POINT('Ctrl Pts',(0.168216069356784,-31.1357293849087,
123.780961197852));
#118917=CARTESIAN_POINT('Ctrl Pts',(0.166128770897804,-31.1581587203012,
123.802353900289));
#118918=CARTESIAN_POINT('Ctrl Pts',(0.165359549936311,-31.1663844159419,
123.810363413593));
#118919=CARTESIAN_POINT('Ctrl Pts',(0.163912054030019,-31.1817835519453,
123.825671114083));
#118920=CARTESIAN_POINT('Ctrl Pts',(0.163233019402845,-31.1889737836234,
123.832951566518));
#118921=CARTESIAN_POINT('Ctrl Pts',(0.161696094026265,-31.2051676171977,
123.849653606238));
#118922=CARTESIAN_POINT('Ctrl Pts',(0.160840137624069,-31.2141287390983,
123.85911559188));
#118923=CARTESIAN_POINT('Ctrl Pts',(0.158206827834837,-31.2415056523198,
123.888710600534));
#118924=CARTESIAN_POINT('Ctrl Pts',(0.156446062762316,-31.2595391593644,
123.909192198364));
#118925=CARTESIAN_POINT('Ctrl Pts',(0.149694644171677,-31.327445614566,
123.990247873303));
#118926=CARTESIAN_POINT('Ctrl Pts',(0.144853617646977,-31.3735205912213,
124.053874076849));
#118927=CARTESIAN_POINT('Ctrl Pts',(0.134500700346386,-31.462944085684,
124.197741698956));
#118928=CARTESIAN_POINT('Ctrl Pts',(0.12902276847542,-31.504538618876,124.278761376881));
#118929=CARTESIAN_POINT('Ctrl Pts',(0.120838387311833,-31.5544245244596,
124.399266115525));
#118930=CARTESIAN_POINT('Ctrl Pts',(0.118317679904426,-31.5682311914639,
124.436291599819));
#118931=CARTESIAN_POINT('Ctrl Pts',(0.115021240922941,-31.5841009440153,
124.483961629491));
#118932=CARTESIAN_POINT('Ctrl Pts',(0.114311247484056,-31.5873953367889,
124.494186368444));
#118933=CARTESIAN_POINT('Ctrl Pts',(0.113166954893524,-31.592503463104,
124.510581897636));
#118934=CARTESIAN_POINT('Ctrl Pts',(0.112736358545873,-31.5943808162653,
124.516732816865));
#118935=CARTESIAN_POINT('Ctrl Pts',(0.111886622773607,-31.5979968891285,
124.528830888064));
#118936=CARTESIAN_POINT('Ctrl Pts',(0.111467684181202,-31.5997381022603,
124.534777052739));
#118937=CARTESIAN_POINT('Ctrl Pts',(0.110439249006086,-31.6039122804174,
124.549332238158));
#118938=CARTESIAN_POINT('Ctrl Pts',(0.10982773797051,-31.6063091129287,
124.557951292892));
#118939=CARTESIAN_POINT('Ctrl Pts',(0.107583414180774,-31.6148008910839,
124.589469142002));
#118940=CARTESIAN_POINT('Ctrl Pts',(0.105929425526354,-31.6204762004279,
124.612476783305));
#118941=CARTESIAN_POINT('Ctrl Pts',(0.0954109898203623,-31.6530612283824,
124.75784331079));
#118942=CARTESIAN_POINT('Ctrl Pts',(0.0861013588996853,-31.66658639838,
124.88278541144));
#118943=CARTESIAN_POINT('Ctrl Pts',(0.069786220291986,-31.6655014734882,
125.107103876206));
#118944=CARTESIAN_POINT('Ctrl Pts',(0.0627319670394635,-31.6561907621357,
125.205923910599));
#118945=CARTESIAN_POINT('Ctrl Pts',(0.0544430292549055,-31.6341886360106,
125.324741380724));
#118946=CARTESIAN_POINT('Ctrl Pts',(0.0529628846407981,-31.6298077898648,
125.34605794817));
#118947=CARTESIAN_POINT('Ctrl Pts',(0.0506097543590494,-31.622117493711,
125.380082929194));
#118948=CARTESIAN_POINT('Ctrl Pts',(0.0497290710686916,-31.61907337331,
125.392848092743));
#118949=CARTESIAN_POINT('Ctrl Pts',(0.0480545747151445,-31.6129687432941,
125.417169885291));
#118950=CARTESIAN_POINT('Ctrl Pts',(0.0472600647941401,-31.6099340626304,
125.42873209057));
#118951=CARTESIAN_POINT('Ctrl Pts',(0.0454316673840891,-31.602631992534,
125.455381710269));
#118952=CARTESIAN_POINT('Ctrl Pts',(0.0444004241194634,-31.5982755012176,
125.470443675996));
#118953=CARTESIAN_POINT('Ctrl Pts',(0.0410488349128261,-31.583344462313,
125.519462274029));
#118954=CARTESIAN_POINT('Ctrl Pts',(0.0387533432384561,-31.571894892015,
125.553143229767));
#118955=CARTESIAN_POINT('Ctrl Pts',(0.0310873261977083,-31.5296613810816,
125.66544563161));
#118956=CARTESIAN_POINT('Ctrl Pts',(0.0258405408557333,-31.493984571933,
125.742086931177));
#118957=CARTESIAN_POINT('Ctrl Pts',(0.0154858401155532,-31.4127069888122,
125.886831798866));
#118958=CARTESIAN_POINT('Ctrl Pts',(0.0103909023578657,-31.3675954258118,
125.954930399638));
#118959=CARTESIAN_POINT('Ctrl Pts',(0.00414849682931046,-31.3088624321337,
126.030845732748));
#118960=CARTESIAN_POINT('Ctrl Pts',(0.00320463889004048,-31.2998944321788,
126.042131579948));
#118961=CARTESIAN_POINT('Ctrl Pts',(0.00184163870806128,-31.2868388690884,
126.058130715643));
#118962=CARTESIAN_POINT('Ctrl Pts',(0.00142863808420865,-31.2828692994149,
126.062939906396));
#118963=CARTESIAN_POINT('Ctrl Pts',(0.000677096287041342,-31.2756232242257,
126.071618915495));
#118964=CARTESIAN_POINT('Ctrl Pts',(0.000339066147284323,-31.2723558546131,
126.075496298494));
#118965=CARTESIAN_POINT('Ctrl Pts',(2.16137329388244E-13,-31.2690708798521,
126.079358653049));
#118966=CARTESIAN_POINT('',(0.,-28.7475103790669,126.098556211331));
#118967=CARTESIAN_POINT('Origin',(0.,-30.,125.));
#118968=CARTESIAN_POINT('Ctrl Pts',(-9.99200722162641E-15,-28.7475103790668,
126.098556211331));
#118969=CARTESIAN_POINT('Ctrl Pts',(0.000120204341514316,-28.7486620881253,
126.099869301756));
#118970=CARTESIAN_POINT('Ctrl Pts',(0.000240539935814629,-28.7498158573408,
126.101180575583));
#118971=CARTESIAN_POINT('Ctrl Pts',(0.0019350791672964,-28.7660745390613,
126.119600292189));
#118972=CARTESIAN_POINT('Ctrl Pts',(0.00353091054824124,-28.7815265364712,
126.136397446123));
#118973=CARTESIAN_POINT('Ctrl Pts',(0.013267754718737,-28.8769048167952,
126.235896674939));
#118974=CARTESIAN_POINT('Ctrl Pts',(0.0217551835120301,-28.9648722034378,
126.31045526773));
#118975=CARTESIAN_POINT('Ctrl Pts',(0.0343325086991831,-29.1085621231512,
126.408680644857));
#118976=CARTESIAN_POINT('Ctrl Pts',(0.0385493452439517,-29.1590496255426,
126.439390945862));
#118977=CARTESIAN_POINT('Ctrl Pts',(0.0445220131853722,-29.2342377070862,
126.479816293358));
#118978=CARTESIAN_POINT('Ctrl Pts',(0.0463454003814986,-29.2577024860493,
126.491724734376));
#118979=CARTESIAN_POINT('Ctrl Pts',(0.0496163886690653,-29.3007239761896,
126.512291596447));
#118980=CARTESIAN_POINT('Ctrl Pts',(0.0510700092075192,-29.3201836705438,
126.521138606934));
#118981=CARTESIAN_POINT('Ctrl Pts',(0.0533392675662641,-29.3510894382467,
126.534477772672));
#118982=CARTESIAN_POINT('Ctrl Pts',(0.0541632985448379,-29.362423610862,
126.539221658455));
#118983=CARTESIAN_POINT('Ctrl Pts',(0.0557040059123447,-29.3838205497343,
126.547900382581));
#118984=CARTESIAN_POINT('Ctrl Pts',(0.0564215939495652,-29.3938710611742,
126.551863533987));
#118985=CARTESIAN_POINT('Ctrl Pts',(0.0580342969124515,-29.416645468968,
126.56058900559));
#118986=CARTESIAN_POINT('Ctrl Pts',(0.0589274892305356,-29.4293905930541,
126.565294054114));
#118987=CARTESIAN_POINT('Ctrl Pts',(0.0612305467946988,-29.4625811686856,
126.577087568334));
#118988=CARTESIAN_POINT('Ctrl Pts',(0.0626326217166769,-29.4831100767161,
126.583934680824));
#118989=CARTESIAN_POINT('Ctrl Pts',(0.0713886819164829,-29.6131755552651,
126.624517896457));
#118990=CARTESIAN_POINT('Ctrl Pts',(0.0783816309159184,-29.7258164134769,
126.647276009909));
#118991=CARTESIAN_POINT('Ctrl Pts',(0.0909557853171158,-29.9299645456178,
126.666984180384));
#118992=CARTESIAN_POINT('Ctrl Pts',(0.0965126677234015,-30.0205655419375,
126.668326739641));
#118993=CARTESIAN_POINT('Ctrl Pts',(0.103345882081162,-30.1253657355237,
126.661340457183));
#118994=CARTESIAN_POINT('Ctrl Pts',(0.104302997915769,-30.1399031154778,
126.66017943787));
#118995=CARTESIAN_POINT('Ctrl Pts',(0.105763601487577,-30.161836951895,
126.658137583951));
#118996=CARTESIAN_POINT('Ctrl Pts',(0.106259850560081,-30.1692462386301,
126.65739770478));
#118997=CARTESIAN_POINT('Ctrl Pts',(0.107167828049092,-30.1827191650552,
126.655961037762));
#118998=CARTESIAN_POINT('Ctrl Pts',(0.107578668309061,-30.1887842664221,
126.655280565308));
#118999=CARTESIAN_POINT('Ctrl Pts',(0.108520533122658,-30.2026171334899,
126.653651575062));
#119000=CARTESIAN_POINT('Ctrl Pts',(0.109052678358275,-30.2103819408131,
126.65268165941));
#119001=CARTESIAN_POINT('Ctrl Pts',(0.110697145176755,-30.2342309139984,
126.649531852205));
#119002=CARTESIAN_POINT('Ctrl Pts',(0.111818497343242,-30.2502897539471,
126.647171649622));
#119003=CARTESIAN_POINT('Ctrl Pts',(0.118574562361602,-30.3459805350638,
126.631676186124));
#119004=CARTESIAN_POINT('Ctrl Pts',(0.124428019876327,-30.424600201384,
126.613004011741));
#119005=CARTESIAN_POINT('Ctrl Pts',(0.135602500289087,-30.5711266866351,
126.566746248814));
#119006=CARTESIAN_POINT('Ctrl Pts',(0.140909348804023,-30.6391903173131,
126.54023260657));
#119007=CARTESIAN_POINT('Ctrl Pts',(0.149160123011709,-30.7439571606213,
126.49127612494));
#119008=CARTESIAN_POINT('Ctrl Pts',(0.152168354429658,-30.7819090177159,
126.471732152215));
#119009=CARTESIAN_POINT('Ctrl Pts',(0.15726155955831,-30.8458096511564,
126.435654857519));
#119010=CARTESIAN_POINT('Ctrl Pts',(0.159368004072816,-30.8721270293933,
126.419821641805));
#119011=CARTESIAN_POINT('Ctrl Pts',(0.162399996212021,-30.9098230967158,
126.39569881646));
#119012=CARTESIAN_POINT('Ctrl Pts',(0.163345975461693,-30.9215570243161,
126.387979079584));
#119013=CARTESIAN_POINT('Ctrl Pts',(0.165009689961135,-30.942139661815,
126.374061685756));
#119014=CARTESIAN_POINT('Ctrl Pts',(0.165729631335259,-30.9510282078058,
126.36792471137));
#119015=CARTESIAN_POINT('Ctrl Pts',(0.167236288040144,-30.9695872863125,
126.354842510094));
#119016=CARTESIAN_POINT('Ctrl Pts',(0.168022262852501,-30.9792443504468,
126.347879166459));
#119017=CARTESIAN_POINT('Ctrl Pts',(0.170103074216175,-31.0047367826617,
126.329078939674));
#119018=CARTESIAN_POINT('Ctrl Pts',(0.171390933410031,-31.0204378084636,
126.317062475006));
#119019=CARTESIAN_POINT('Ctrl Pts',(0.17821391475362,-31.1031151901479,
126.251420738147));
#119020=CARTESIAN_POINT('Ctrl Pts',(0.183550467761074,-31.1660915861063,
126.192958548426));
#119021=CARTESIAN_POINT('Ctrl Pts',(0.19481921028437,-31.2906143135585,
126.058033159491));
#119022=CARTESIAN_POINT('Ctrl Pts',(0.200707971409592,-31.3504777518552,
125.980472867717));
#119023=CARTESIAN_POINT('Ctrl Pts',(0.208599612696059,-31.4182912815847,
125.874523028184));
#119024=CARTESIAN_POINT('Ctrl Pts',(0.210376585110017,-31.4327939970555,
125.850553862308));
#119025=CARTESIAN_POINT('Ctrl Pts',(0.213420572835703,-31.4562002149904,
125.809570915041));
#119026=CARTESIAN_POINT('Ctrl Pts',(0.214671685018553,-31.4654266404986,
125.792747638014));
#119027=CARTESIAN_POINT('Ctrl Pts',(0.216482560034626,-31.4781849013655,
125.768500403063));
#119028=CARTESIAN_POINT('Ctrl Pts',(0.217028522218047,-31.4819558884386,
125.761203133127));
#119029=CARTESIAN_POINT('Ctrl Pts',(0.217982960258905,-31.4884141875288,
125.748475725674));
#119030=CARTESIAN_POINT('Ctrl Pts',(0.218389913920641,-31.4911261009793,
125.743058312257));
#119031=CARTESIAN_POINT('Ctrl Pts',(0.219267007427853,-31.4968804830601,
125.731404786));
#119032=CARTESIAN_POINT('Ctrl Pts',(0.21973766624871,-31.4999135191273,
125.725164513949));
#119033=CARTESIAN_POINT('Ctrl Pts',(0.221049079958931,-31.5082157304375,
125.70780833454));
#119034=CARTESIAN_POINT('Ctrl Pts',(0.221894633332486,-31.51340077538,125.696652997369));
#119035=CARTESIAN_POINT('Ctrl Pts',(0.22829599029076,-31.5514373335683,
125.612390462723));
#119036=CARTESIAN_POINT('Ctrl Pts',(0.234094616544042,-31.579094916581,
125.53706264139));
#119037=CARTESIAN_POINT('Ctrl Pts',(0.240287625540146,-31.6025987786272,
125.455255975213));
#119038=CARTESIAN_POINT('Ctrl Pts',(0.240650432153012,-31.6039537630155,
125.450458848506));
#119039=CARTESIAN_POINT('Ctrl Pts',(0.245965032970622,-31.6234827844638,
125.38011376667));
#119040=CARTESIAN_POINT('Ctrl Pts',(0.25092170439923,-31.6376482144507,
125.313515622568));
#119041=CARTESIAN_POINT('Ctrl Pts',(0.259167209986624,-31.6546523477645,
125.199731189429));
#119042=CARTESIAN_POINT('Ctrl Pts',(0.262495760858726,-31.6596306104476,
125.152950442901));
#119043=CARTESIAN_POINT('Ctrl Pts',(0.268055402483936,-31.6647150429517,
125.073214095539));
#119044=CARTESIAN_POINT('Ctrl Pts',(0.270314240050564,-31.6658356270203,
125.040353522546));
#119045=CARTESIAN_POINT('Ctrl Pts',(0.273513716974237,-31.6660474913257,
124.993160975686));
#119046=CARTESIAN_POINT('Ctrl Pts',(0.274478631268238,-31.6659271842176,
124.978842144537));
#119047=CARTESIAN_POINT('Ctrl Pts',(0.276157107376378,-31.6653936232467,
124.953789509818));
#119048=CARTESIAN_POINT('Ctrl Pts',(0.276873158753556,-31.6650611427352,
124.943055026095));
#119049=CARTESIAN_POINT('Ctrl Pts',(0.278353993333672,-31.6641548314609,
124.920762416001));
#119050=CARTESIAN_POINT('Ctrl Pts',(0.279118213419217,-31.6635643273077,
124.909205516887));
#119051=CARTESIAN_POINT('Ctrl Pts',(0.281101127305262,-31.6617108473527,
124.879090911699));
#119052=CARTESIAN_POINT('Ctrl Pts',(0.282313805138082,-31.6602574010555,
124.860546224265));
#119053=CARTESIAN_POINT('Ctrl Pts',(0.287734266903797,-31.6523143985141,
124.777154774385));
#119054=CARTESIAN_POINT('Ctrl Pts',(0.291832029579267,-31.6423336616721,
124.712694490506));
#119055=CARTESIAN_POINT('Ctrl Pts',(0.304768062870247,-31.5982816110112,
124.508310382987));
#119056=CARTESIAN_POINT('Ctrl Pts',(0.313258034757407,-31.5498706940095,
124.372183610993));
#119057=CARTESIAN_POINT('Ctrl Pts',(0.323943474852953,-31.47421009323,124.223608656929));
#119058=CARTESIAN_POINT('Ctrl Pts',(0.325427401204644,-31.4634152842268,
124.20344837163));
#119059=CARTESIAN_POINT('Ctrl Pts',(0.327511557238231,-31.4479269098858,
124.175900473021));
#119060=CARTESIAN_POINT('Ctrl Pts',(0.328091318448439,-31.4435843987947,
124.168317102551));
#119061=CARTESIAN_POINT('Ctrl Pts',(0.329082906064293,-31.4361044052984,
124.155489800982));
#119062=CARTESIAN_POINT('Ctrl Pts',(0.329492796542649,-31.4329973814433,
124.150228358442));
#119063=CARTESIAN_POINT('Ctrl Pts',(0.330354501210045,-31.4264357188536,
124.139255151278));
#119064=CARTESIAN_POINT('Ctrl Pts',(0.330806622722977,-31.4229757247761,
124.133547094536));
#119065=CARTESIAN_POINT('Ctrl Pts',(0.332032104127468,-31.4135487213855,
124.118203847396));
#119066=CARTESIAN_POINT('Ctrl Pts',(0.332809395876531,-31.4075176660362,
124.108608702864));
#119067=CARTESIAN_POINT('Ctrl Pts',(0.336637513100385,-31.3775421894471,
124.061981769726));
#119068=CARTESIAN_POINT('Ctrl Pts',(0.33976209209934,-31.35223369061,124.025852166006));
#119069=CARTESIAN_POINT('Ctrl Pts',(0.349282392928046,-31.2718963871914,
123.920336734674));
#119070=CARTESIAN_POINT('Ctrl Pts',(0.355779027187453,-31.2127399536266,
123.854288437971));
#119071=CARTESIAN_POINT('Ctrl Pts',(0.366584571824769,-31.1045260057245,
123.751287315702));
#119072=CARTESIAN_POINT('Ctrl Pts',(0.370937290428969,-31.058165900498,
123.711765836677));
#119073=CARTESIAN_POINT('Ctrl Pts',(0.377952695974848,-30.9784753914571,
123.651042190002));
#119074=CARTESIAN_POINT('Ctrl Pts',(0.380666211539674,-30.9463729349424,
123.628329493749));
#119075=CARTESIAN_POINT('Ctrl Pts',(0.384381121927475,-30.9006433589569,
123.598346087419));
#119076=CARTESIAN_POINT('Ctrl Pts',(0.385418476396555,-30.8876758896001,
123.590097984554));
#119077=CARTESIAN_POINT('Ctrl Pts',(0.387185294083296,-30.8652551525701,
123.576269000164));
#119078=CARTESIAN_POINT('Ctrl Pts',(0.387917951829374,-30.8558576529953,
123.570600081619));
#119079=CARTESIAN_POINT('Ctrl Pts',(0.389312059920929,-30.8377874922977,
123.559941596044));
#119080=CARTESIAN_POINT('Ctrl Pts',(0.389974049303338,-30.8291245953965,
123.55493650598));
#119081=CARTESIAN_POINT('Ctrl Pts',(0.391695180620037,-30.8063906234806,
123.542073429595));
#119082=CARTESIAN_POINT('Ctrl Pts',(0.392749823247401,-30.7922494692561,
123.534340922807));
#119083=CARTESIAN_POINT('Ctrl Pts',(0.396492028696302,-30.7413490218364,
123.507460095458));
#119084=CARTESIAN_POINT('Ctrl Pts',(0.399139228099406,-30.7039886155014,
123.48947883064));
#119085=CARTESIAN_POINT('Ctrl Pts',(0.409052066066855,-30.559753083363,
123.426574947428));
#119086=CARTESIAN_POINT('Ctrl Pts',(0.416020550711431,-30.4489695066851,
123.391454981954));
#119087=CARTESIAN_POINT('Ctrl Pts',(0.426138482222719,-30.2878392845479,
123.358334498815));
#119088=CARTESIAN_POINT('Ctrl Pts',(0.42915439222678,-30.2398414308243,
123.350638756414));
#119089=CARTESIAN_POINT('Ctrl Pts',(0.433461001687293,-30.1726439262062,
123.342859862002));
#119090=CARTESIAN_POINT('Ctrl Pts',(0.434686160684013,-30.1536729257287,
123.340993089404));
#119091=CARTESIAN_POINT('Ctrl Pts',(0.436861951107176,-30.1203358867991,
123.33828936478));
#119092=CARTESIAN_POINT('Ctrl Pts',(0.437806129845592,-30.105982960015,
123.337312254507));
#119093=CARTESIAN_POINT('Ctrl Pts',(0.439245955362327,-30.0843024506078,
123.336118152477));
#119094=CARTESIAN_POINT('Ctrl Pts',(0.439734406324747,-30.0769827165876,
123.335763429683));
#119095=CARTESIAN_POINT('Ctrl Pts',(0.440628984963814,-30.0636465873523,
123.335205313235));
#119096=CARTESIAN_POINT('Ctrl Pts',(0.441034248602557,-30.057631117649,
123.334986219872));
#119097=CARTESIAN_POINT('Ctrl Pts',(0.441962986400886,-30.0439048031624,
123.334560758922));
#119098=CARTESIAN_POINT('Ctrl Pts',(0.442487565447425,-30.0361936693959,
123.334375339444));
#119099=CARTESIAN_POINT('Ctrl Pts',(0.444137173083129,-30.0120669123418,
123.333962811249));
#119100=CARTESIAN_POINT('Ctrl Pts',(0.445271670251234,-29.995649607398,
123.333924807098));
#119101=CARTESIAN_POINT('Ctrl Pts',(0.452144291417191,-29.8970892486183,
123.33515334501));
#119102=CARTESIAN_POINT('Ctrl Pts',(0.458110486290468,-29.8151390762679,
123.342251851057));
#119103=CARTESIAN_POINT('Ctrl Pts',(0.470596567811082,-29.6457821167786,
123.369637585095));
#119104=CARTESIAN_POINT('Ctrl Pts',(0.477095767494718,-29.558792907082,
123.390996844334));
#119105=CARTESIAN_POINT('Ctrl Pts',(0.485765742644005,-29.4423471582797,
123.429749246961));
#119106=CARTESIAN_POINT('Ctrl Pts',(0.488091863309416,-29.4110823230837,
123.441205483309));
#119107=CARTESIAN_POINT('Ctrl Pts',(0.492149731540387,-29.3564885356729,
123.463087365615));
#119108=CARTESIAN_POINT('Ctrl Pts',(0.493893030193381,-29.3330174631778,
123.473126766624));
#119109=CARTESIAN_POINT('Ctrl Pts',(0.496500009373458,-29.2979105507213,
123.489107340217));
#119110=CARTESIAN_POINT('Ctrl Pts',(0.49737699208755,-29.2860995412653,
123.494652074773));
#119111=CARTESIAN_POINT('Ctrl Pts',(0.498961880112305,-29.264757979387,
123.504978652865));
#119112=CARTESIAN_POINT('Ctrl Pts',(0.499671333702006,-29.255205977259,
123.509714279069));
#119113=CARTESIAN_POINT('Ctrl Pts',(0.501201638294757,-29.2346093398998,
123.520173032558));
#119114=CARTESIAN_POINT('Ctrl Pts',(0.502021295994636,-29.2235819566312,
123.525928851067));
#119115=CARTESIAN_POINT('Ctrl Pts',(0.504271013462008,-29.1933385476306,
123.542148158332));
#119116=CARTESIAN_POINT('Ctrl Pts',(0.505691989787461,-29.17426216427,123.552867735928));
#119117=CARTESIAN_POINT('Ctrl Pts',(0.515967654530167,-29.0367014191603,
123.633773281269));
#119118=CARTESIAN_POINT('Ctrl Pts',(0.524255789374191,-28.927115819782,
123.718031720228));
#119119=CARTESIAN_POINT('Ctrl Pts',(0.536044031092211,-28.7903072247371,
123.853187260546));
#119120=CARTESIAN_POINT('Ctrl Pts',(0.5394147654645,-28.7533841412355,123.893435887647));
#119121=CARTESIAN_POINT('Ctrl Pts',(0.544796753517581,-28.6992120515421,
123.958645898043));
#119122=CARTESIAN_POINT('Ctrl Pts',(0.546741615648602,-28.6805545984744,
123.982389457186));
#119123=CARTESIAN_POINT('Ctrl Pts',(0.549365902173527,-28.6567628881214,
124.01442180021));
#119124=CARTESIAN_POINT('Ctrl Pts',(0.550008823850018,-28.6510403258825,
124.022268895351));
#119125=CARTESIAN_POINT('Ctrl Pts',(0.551077882752288,-28.6417061783036,
124.03530633295));
#119126=CARTESIAN_POINT('Ctrl Pts',(0.551501372973584,-28.6380548515351,
124.040468141798));
#119127=CARTESIAN_POINT('Ctrl Pts',(0.552305889581432,-28.6312075727591,
124.050265828746));
#119128=CARTESIAN_POINT('Ctrl Pts',(0.552686482466124,-28.6280055616643,
124.054897379275));
#119129=CARTESIAN_POINT('Ctrl Pts',(0.553704843285209,-28.6195350499821,
124.06728331745));
#119130=CARTESIAN_POINT('Ctrl Pts',(0.554345304258772,-28.6143085140447,
124.075065957171));
#119131=CARTESIAN_POINT('Ctrl Pts',(0.556730305460815,-28.5952058099277,
124.104036410153));
#119132=CARTESIAN_POINT('Ctrl Pts',(0.558498628462718,-28.5817483947251,
124.125494604019));
#119133=CARTESIAN_POINT('Ctrl Pts',(0.56752911242005,-28.516294748761,124.235348758641));
#119134=CARTESIAN_POINT('Ctrl Pts',(0.575066613691092,-28.4720523084894,
124.328101890912));
#119135=CARTESIAN_POINT('Ctrl Pts',(0.588498201089292,-28.4080490681001,
124.501919031425));
#119136=CARTESIAN_POINT('Ctrl Pts',(0.594412569370975,-28.3852913269368,
124.581536584095));
#119137=CARTESIAN_POINT('Ctrl Pts',(0.602220893425202,-28.3624842367964,
124.691793209031));
#119138=CARTESIAN_POINT('Ctrl Pts',(0.604269924089063,-28.3572183076328,
124.721220855761));
#119139=CARTESIAN_POINT('Ctrl Pts',(0.607232070429548,-28.3506748515629,
124.764470014339));
#119140=CARTESIAN_POINT('Ctrl Pts',(0.608164564956312,-28.3487737789373,
124.778189706246));
#119141=CARTESIAN_POINT('Ctrl Pts',(0.60980921757349,-28.3457051817319,
124.802567569709));
#119142=CARTESIAN_POINT('Ctrl Pts',(0.61052349496063,-28.3444690548966,
124.813216142772));
#119143=CARTESIAN_POINT('Ctrl Pts',(0.612022773382726,-28.3420795381667,
124.835692521125));
#119144=CARTESIAN_POINT('Ctrl Pts',(0.612806995771749,-28.3409497416052,
124.847522271075));
#119145=CARTESIAN_POINT('Ctrl Pts',(0.614893497658181,-28.3382675101724,
124.879182921056));
#119146=CARTESIAN_POINT('Ctrl Pts',(0.616188612046181,-28.3369434543,124.899031613677));
#119147=CARTESIAN_POINT('Ctrl Pts',(0.623772420962331,-28.3312281813285,
125.016298603042));
#119148=CARTESIAN_POINT('Ctrl Pts',(0.62979586893043,-28.3350410932901,
125.113931273434));
#119149=CARTESIAN_POINT('Ctrl Pts',(0.640240300793025,-28.3566359154911,
125.283326066998));
#119150=CARTESIAN_POINT('Ctrl Pts',(0.644679613834121,-28.3706765037622,
125.355279190346));
#119151=CARTESIAN_POINT('Ctrl Pts',(0.652478488434351,-28.4027650855182,
125.476577295957));
#119152=CARTESIAN_POINT('Ctrl Pts',(0.655779574329153,-28.4184927710903,
125.52642095483));
#119153=CARTESIAN_POINT('Ctrl Pts',(0.659200637484241,-28.4365423944709,
125.575461829013));
#119154=CARTESIAN_POINT('Ctrl Pts',(0.659202304206952,-28.4365511888928,
125.575485721539));
#119155=CARTESIAN_POINT('Ctrl Pts',(0.659203971007256,-28.4365599837785,
125.575509613888));
#119156=CARTESIAN_POINT('Origin',(5.,30.,125.));
#119157=CARTESIAN_POINT('',(9.56913306840647,31.5634400114683,125.575509626801));
#119158=CARTESIAN_POINT('',(9.75970370682547,31.5634400119926,125.575509625376));
#119159=CARTESIAN_POINT('',(5.,31.5634400119422,125.575509625513));
#119160=CARTESIAN_POINT('',(10.,28.6653082844465,125.997072727755));
#119161=CARTESIAN_POINT('Ctrl Pts',(9.75970370682547,31.5634400119926,125.575509625376));
#119162=CARTESIAN_POINT('Ctrl Pts',(9.75994459139466,31.5620930770963,125.579168733439));
#119163=CARTESIAN_POINT('Ctrl Pts',(9.76018575818481,31.5607331464613,125.582823520293));
#119164=CARTESIAN_POINT('Ctrl Pts',(9.76396628152904,31.5392388666679,125.639974101608));
#119165=CARTESIAN_POINT('Ctrl Pts',(9.76756190554505,31.5163796603936,125.692397583835));
#119166=CARTESIAN_POINT('Ctrl Pts',(9.77207483843158,31.4855732267757,125.754167966873));
#119167=CARTESIAN_POINT('Ctrl Pts',(9.77285751500153,31.4801578002206,125.764741787096));
#119168=CARTESIAN_POINT('Ctrl Pts',(9.77410224807535,31.4714416077863,125.7813210223));
#119169=CARTESIAN_POINT('Ctrl Pts',(9.77455979485348,31.4682159539979,125.787365768384));
#119170=CARTESIAN_POINT('Ctrl Pts',(9.77541181945527,31.46217156249,125.798526417119));
#119171=CARTESIAN_POINT('Ctrl Pts',(9.77580564898278,31.4593629969158,125.803647783058));
#119172=CARTESIAN_POINT('Ctrl Pts',(9.77672959500891,31.4527413176242,125.815573109029));
#119173=CARTESIAN_POINT('Ctrl Pts',(9.77726105993558,31.4489073410184,125.822365090935));
#119174=CARTESIAN_POINT('Ctrl Pts',(9.77905616486145,31.4358689016285,125.845088776269));
#119175=CARTESIAN_POINT('Ctrl Pts',(9.78033302229518,31.4264486253917,125.860894178829));
#119176=CARTESIAN_POINT('Ctrl Pts',(9.78350140602102,31.4026736679402,125.899322140857));
#119177=CARTESIAN_POINT('Ctrl Pts',(9.78540715205928,31.3880315890365,125.921760200467));
#119178=CARTESIAN_POINT('Ctrl Pts',(9.79378242249019,31.3219754251849,126.017842332533));
#119179=CARTESIAN_POINT('Ctrl Pts',(9.80041817703831,31.2651954969747,126.087612861256));
#119180=CARTESIAN_POINT('Ctrl Pts',(9.81454442273501,31.1313054550444,126.227382041363));
#119181=CARTESIAN_POINT('Ctrl Pts',(9.82197011540505,31.0526882199104,126.295443454695));
#119182=CARTESIAN_POINT('Ctrl Pts',(9.83042336813809,30.9522599057718,126.36716582979));
#119183=CARTESIAN_POINT('Ctrl Pts',(9.83175674799993,30.936084486356,126.378291416433));
#119184=CARTESIAN_POINT('Ctrl Pts',(9.83385390086391,30.910120300584,126.395481804265));
#119185=CARTESIAN_POINT('Ctrl Pts',(9.83462500408079,30.900459264765,126.401735193274));
#119186=CARTESIAN_POINT('Ctrl Pts',(9.83607437031181,30.8820875978143,126.413358466382));
#119187=CARTESIAN_POINT('Ctrl Pts',(9.8367534115864,30.8733908325676,126.418749148576));
#119188=CARTESIAN_POINT('Ctrl Pts',(9.83828811921684,30.8535355246368,126.430804676216));
#119189=CARTESIAN_POINT('Ctrl Pts',(9.83914187704127,30.8423474554919,126.437419804376));
#119190=CARTESIAN_POINT('Ctrl Pts',(9.84176003815002,30.8076104740441,126.457413737022));
#119191=CARTESIAN_POINT('Ctrl Pts',(9.84350814097426,30.7838111478326,126.470350196461));
#119192=CARTESIAN_POINT('Ctrl Pts',(9.85258879217069,30.6572674520097,126.535188599539));
#119193=CARTESIAN_POINT('Ctrl Pts',(9.85955502127682,30.5496647418267,126.576919847836));
#119194=CARTESIAN_POINT('Ctrl Pts',(9.87177897248656,30.3564027375561,126.629660856546));
#119195=CARTESIAN_POINT('Ctrl Pts',(9.8770017977947,30.2726050549933,126.645752159744));
#119196=CARTESIAN_POINT('Ctrl Pts',(9.88356980597318,30.1719574979488,126.657180104862));
#119197=CARTESIAN_POINT('Ctrl Pts',(9.88462442759328,30.1559333474297,126.658764607608));
#119198=CARTESIAN_POINT('Ctrl Pts',(9.88618948312394,30.1324045698738,126.660747257134));
#119199=CARTESIAN_POINT('Ctrl Pts',(9.8866900713217,30.1249156322456,126.661327331197));
#119200=CARTESIAN_POINT('Ctrl Pts',(9.8875932127674,30.111476506953,126.662276910837));
#119201=CARTESIAN_POINT('Ctrl Pts',(9.8879946960257,30.105527839588,126.662665152759));
#119202=CARTESIAN_POINT('Ctrl Pts',(9.88889106872669,30.0923012641878,126.663457125401));
#119203=CARTESIAN_POINT('Ctrl Pts',(9.88938682424562,30.0850225581548,126.663845032129));
#119204=CARTESIAN_POINT('Ctrl Pts',(9.89084623625951,30.0636955621998,126.664841313866));
#119205=CARTESIAN_POINT('Ctrl Pts',(9.89181657197186,30.0496422441511,126.665319590807));
#119206=CARTESIAN_POINT('Ctrl Pts',(9.89407522113535,30.0171861406494,126.666012999601));
#119207=CARTESIAN_POINT('Ctrl Pts',(9.89536902846809,29.9987827042178,126.666101177692));
#119208=CARTESIAN_POINT('Ctrl Pts',(9.89988294160567,29.9351132153575,126.665351402391));
#119209=CARTESIAN_POINT('Ctrl Pts',(9.90315495945869,29.8898874761054,126.662973319785));
#119210=CARTESIAN_POINT('Ctrl Pts',(9.91521616358714,29.7250558894377,126.647552805197));
#119211=CARTESIAN_POINT('Ctrl Pts',(9.92409883915684,29.6068440151953,126.623409493784));
#119212=CARTESIAN_POINT('Ctrl Pts',(9.93686594271568,29.4360947377721,126.568771596439));
#119213=CARTESIAN_POINT('Ctrl Pts',(9.94098731420158,29.3809188867373,126.54782862083));
#119214=CARTESIAN_POINT('Ctrl Pts',(9.9463461503922,29.3092019759589,126.516156693602));
#119215=CARTESIAN_POINT('Ctrl Pts',(9.94766344887194,29.2915776404115,126.508002268485));
#119216=CARTESIAN_POINT('Ctrl Pts',(9.94982184362611,29.2627265518777,126.494035980163));
#119217=CARTESIAN_POINT('Ctrl Pts',(9.95066847590616,29.2514165912527,126.488401337476));
#119218=CARTESIAN_POINT('Ctrl Pts',(9.95232208590052,29.2293477426935,126.477091406567));
#119219=CARTESIAN_POINT('Ctrl Pts',(9.9531293103512,29.2185847635262,126.471425895264));
#119220=CARTESIAN_POINT('Ctrl Pts',(9.95505641867882,29.1929242938889,126.457557541801));
#119221=CARTESIAN_POINT('Ctrl Pts',(9.95617270637998,29.1780883064762,126.449243382604));
#119222=CARTESIAN_POINT('Ctrl Pts',(9.96020750324361,29.1246142158177,126.418190912052));
#119223=CARTESIAN_POINT('Ctrl Pts',(9.96308428783827,29.0867691561011,126.394121807055));
#119224=CARTESIAN_POINT('Ctrl Pts',(9.9707685764379,28.9872908689865,126.32506318033));
#119225=CARTESIAN_POINT('Ctrl Pts',(9.97550377578497,28.9277020871985,126.277321416801));
#119226=CARTESIAN_POINT('Ctrl Pts',(9.98509064503516,28.8146820719787,126.173269511672));
#119227=CARTESIAN_POINT('Ctrl Pts',(9.98993265788907,28.7614950083516,126.11697951251));
#119228=CARTESIAN_POINT('Ctrl Pts',(9.99589057874712,28.7033764422887,126.04619608118));
#119229=CARTESIAN_POINT('Ctrl Pts',(9.99682341121584,28.6944793874846,126.035072362502));
#119230=CARTESIAN_POINT('Ctrl Pts',(9.99817185487695,28.6819257142596,126.018957518433));
#119231=CARTESIAN_POINT('Ctrl Pts',(9.99858147442229,28.6781523448154,126.014057701144));
#119232=CARTESIAN_POINT('Ctrl Pts',(9.9993273882682,28.6713554335786,126.005129338138));
#119233=CARTESIAN_POINT('Ctrl Pts',(9.99966318296832,28.6683226971404,126.00110785131));
#119234=CARTESIAN_POINT('Ctrl Pts',(10.,28.6653082844465,125.997072727755));
#119235=CARTESIAN_POINT('',(10.,29.2076925604819,123.534460876918));
#119236=CARTESIAN_POINT('Origin',(10.,30.,125.));
#119237=CARTESIAN_POINT('Ctrl Pts',(9.99999999999989,29.2076925604819,123.534460876918));
#119238=CARTESIAN_POINT('Ctrl Pts',(9.99926836029946,29.1983407334261,123.53951671066));
#119239=CARTESIAN_POINT('Ctrl Pts',(9.99853187606714,29.1890377534795,123.544661812123));
#119240=CARTESIAN_POINT('Ctrl Pts',(9.99208084888614,29.1084579028524,123.590239774574));
#119241=CARTESIAN_POINT('Ctrl Pts',(9.98613037893974,29.0402114633257,123.635787921533));
#119242=CARTESIAN_POINT('Ctrl Pts',(9.97478930496467,28.917371786035,123.731566384957));
#119243=CARTESIAN_POINT('Ctrl Pts',(9.9694133315424,28.8622228045054,123.780790397032));
#119244=CARTESIAN_POINT('Ctrl Pts',(9.96107116435099,28.7804042760972,123.86422177828));
#119245=CARTESIAN_POINT('Ctrl Pts',(9.95803791514138,28.7514881025938,123.896086751998));
#119246=CARTESIAN_POINT('Ctrl Pts',(9.95290232109893,28.7039302985686,123.952756878366));
#119247=CARTESIAN_POINT('Ctrl Pts',(9.9507780919654,28.6846890676815,123.977027762911));
#119248=CARTESIAN_POINT('Ctrl Pts',(9.94772273497591,28.6576659677329,124.013138752683));
#119249=CARTESIAN_POINT('Ctrl Pts',(9.94677083906848,28.6493416519085,124.024562752636));
#119250=CARTESIAN_POINT('Ctrl Pts',(9.9450973829791,28.6348801425166,124.044949365195));
#119251=CARTESIAN_POINT('Ctrl Pts',(9.9443735934591,28.6286834205053,124.053868514092));
#119252=CARTESIAN_POINT('Ctrl Pts',(9.942859306635,28.6158443772112,124.07273933266));
#119253=CARTESIAN_POINT('Ctrl Pts',(9.94206954878145,28.6092211293346,124.082703276691));
#119254=CARTESIAN_POINT('Ctrl Pts',(9.93997879188096,28.5918876987556,124.109398875837));
#119255=CARTESIAN_POINT('Ctrl Pts',(9.93868476651747,28.581368262413,124.126252518104));
#119256=CARTESIAN_POINT('Ctrl Pts',(9.93125846200095,28.5222853356233,124.224792961299));
#119257=CARTESIAN_POINT('Ctrl Pts',(9.92537191052699,28.4804782994499,124.310330856594));
#119258=CARTESIAN_POINT('Ctrl Pts',(9.91507039455771,28.4199297270125,124.466865446259));
#119259=CARTESIAN_POINT('Ctrl Pts',(9.91064078618597,28.3981483822722,124.536399846889));
#119260=CARTESIAN_POINT('Ctrl Pts',(9.90298349575962,28.3692031925257,124.655683602719));
#119261=CARTESIAN_POINT('Ctrl Pts',(9.89981746831812,28.3596129071907,124.704735377485));
#119262=CARTESIAN_POINT('Ctrl Pts',(9.89579478947652,28.3505492412692,124.76547988562));
#119263=CARTESIAN_POINT('Ctrl Pts',(9.89503826657815,28.3489741982092,124.776838010076));
#119264=CARTESIAN_POINT('Ctrl Pts',(9.89382393908063,28.3466534158236,124.794945920801));
#119265=CARTESIAN_POINT('Ctrl Pts',(9.89337014896009,28.3458314540211,124.801685804175));
#119266=CARTESIAN_POINT('Ctrl Pts',(9.8924999356591,28.3443418279684,124.814554522555));
#119267=CARTESIAN_POINT('Ctrl Pts',(9.89208390114965,28.3436669549775,124.820682274528));
#119268=CARTESIAN_POINT('Ctrl Pts',(9.89115568319814,28.3422434822918,124.834301449103));
#119269=CARTESIAN_POINT('Ctrl Pts',(9.89064262202549,28.3415116295774,124.841794432531));
#119270=CARTESIAN_POINT('Ctrl Pts',(9.88911188262665,28.3394896764623,124.864054441157));
#119271=CARTESIAN_POINT('Ctrl Pts',(9.88808703414315,28.3383458870185,124.878833577842));
#119272=CARTESIAN_POINT('Ctrl Pts',(9.88134986456065,28.3321736065462,124.975304301392));
#119273=CARTESIAN_POINT('Ctrl Pts',(9.87541090078437,28.3329742887738,125.057249823764));
#119274=CARTESIAN_POINT('Ctrl Pts',(9.86410502872961,28.3459251905703,125.212161974066));
#119275=CARTESIAN_POINT('Ctrl Pts',(9.85875226363202,28.3569155002326,125.285045313465));
#119276=CARTESIAN_POINT('Ctrl Pts',(9.85053346758975,28.3816209954979,125.39767069975));
#119277=CARTESIAN_POINT('Ctrl Pts',(9.8475981786668,28.392074584836,125.438028444428));
#119278=CARTESIAN_POINT('Ctrl Pts',(9.84261362292443,28.4126897425999,125.506865836783));
#119279=CARTESIAN_POINT('Ctrl Pts',(9.84054410428431,28.4221324407004,125.535538045768));
#119280=CARTESIAN_POINT('Ctrl Pts',(9.83755478201414,28.4370715275392,125.577066020499));
#119281=CARTESIAN_POINT('Ctrl Pts',(9.83661534623579,28.4419583863854,125.590132995784));
#119282=CARTESIAN_POINT('Ctrl Pts',(9.83495917503574,28.4509138585718,125.613192034038));
#119283=CARTESIAN_POINT('Ctrl Pts',(9.83424029828365,28.4549164216817,125.623208704637));
#119284=CARTESIAN_POINT('Ctrl Pts',(9.83273196700223,28.4635569859417,125.644237234464));
#119285=CARTESIAN_POINT('Ctrl Pts',(9.83194329023348,28.4682167527892,125.655239533094));
#119286=CARTESIAN_POINT('Ctrl Pts',(9.82984608415284,28.4809846486782,125.684505383807));
#119287=CARTESIAN_POINT('Ctrl Pts',(9.82854473747946,28.4893038181359,125.70267514506));
#119288=CARTESIAN_POINT('Ctrl Pts',(9.82097238886605,28.540002793598,125.808341009415));
#119289=CARTESIAN_POINT('Ctrl Pts',(9.81496336481829,28.589650613333,125.892146335419));
#119290=CARTESIAN_POINT('Ctrl Pts',(9.80467100192769,28.68769523141,126.028808808049));
#119291=CARTESIAN_POINT('Ctrl Pts',(9.80036643622977,28.7326996666267,126.083762224968));
#119292=CARTESIAN_POINT('Ctrl Pts',(9.79365745014556,28.8063903186663,126.162855005261));
#119293=CARTESIAN_POINT('Ctrl Pts',(9.7913262553079,28.8326123663793,126.189176856684));
#119294=CARTESIAN_POINT('Ctrl Pts',(9.78744409000612,28.8767853829111,126.230648101506));
#119295=CARTESIAN_POINT('Ctrl Pts',(9.78592274972215,28.8942163341931,126.246333894596));
#119296=CARTESIAN_POINT('Ctrl Pts',(9.78379141831008,28.9186907759503,126.267440369686));
#119297=CARTESIAN_POINT('Ctrl Pts',(9.78320274610423,28.9254561537052,126.273181150679));
#119298=CARTESIAN_POINT('Ctrl Pts',(9.78219858965437,28.9369985243572,126.28281793624));
#119299=CARTESIAN_POINT('Ctrl Pts',(9.78178509695071,28.941751997332,126.286742071262));
#119300=CARTESIAN_POINT('Ctrl Pts',(9.78092290866195,28.9516618765897,126.294830919954));
#119301=CARTESIAN_POINT('Ctrl Pts',(9.78047394156271,28.9568215101036,126.298991365103));
#119302=CARTESIAN_POINT('Ctrl Pts',(9.77926024722766,28.970771235138,126.310102947866));
#119303=CARTESIAN_POINT('Ctrl Pts',(9.77849167455775,28.9796066820226,126.316996220147));
#119304=CARTESIAN_POINT('Ctrl Pts',(9.77476830526531,29.0224495855222,126.349731642557));
#119305=CARTESIAN_POINT('Ctrl Pts',(9.77174403425812,29.0573701830882,126.374346635588));
#119306=CARTESIAN_POINT('Ctrl Pts',(9.76226003425398,29.1682670325332,126.446300396185));
#119307=CARTESIAN_POINT('Ctrl Pts',(9.75568929087881,29.2471412809544,126.488881541108));
#119308=CARTESIAN_POINT('Ctrl Pts',(9.74478446278907,29.3850799915816,126.549572856507));
#119309=CARTESIAN_POINT('Ctrl Pts',(9.74040536224569,29.4424269877839,126.571119436276));
#119310=CARTESIAN_POINT('Ctrl Pts',(9.73335874784092,29.5384160479382,126.60126446523));
#119311=CARTESIAN_POINT('Ctrl Pts',(9.73063926940642,29.5764063858856,126.611730912066));
#119312=CARTESIAN_POINT('Ctrl Pts',(9.72692272228067,29.6296304519756,126.624381977367));
#119313=CARTESIAN_POINT('Ctrl Pts',(9.72588921945157,29.6445744322476,126.627717144845));
#119314=CARTESIAN_POINT('Ctrl Pts',(9.72413112226573,29.6702350317118,126.633073766658));
#119315=CARTESIAN_POINT('Ctrl Pts',(9.72340331328317,29.6809291764201,126.635196832492));
#119316=CARTESIAN_POINT('Ctrl Pts',(9.72193226891773,29.7026850433936,126.639294376947));
#119317=CARTESIAN_POINT('Ctrl Pts',(9.72118927962108,29.7137474486734,126.641262235324));
#119318=CARTESIAN_POINT('Ctrl Pts',(9.719330252277,29.741606072966,126.645927682956));
#119319=CARTESIAN_POINT('Ctrl Pts',(9.71821885658562,29.7584255282048,126.64848026034));
#119320=CARTESIAN_POINT('Ctrl Pts',(9.71392938616291,29.8239344429659,126.657397924007));
#119321=CARTESIAN_POINT('Ctrl Pts',(9.71081065952237,29.8728592425205,126.661867288073));
#119322=CARTESIAN_POINT('Ctrl Pts',(9.70023348150523,30.0417630132157,126.669792588948));
#119323=CARTESIAN_POINT('Ctrl Pts',(9.69306460946781,30.1618636872509,126.662453276365));
#119324=CARTESIAN_POINT('Ctrl Pts',(9.68314484900705,30.3200833785907,126.635464783275));
#119325=CARTESIAN_POINT('Ctrl Pts',(9.68061253924705,30.3597686874985,126.62719528075));
#119326=CARTESIAN_POINT('Ctrl Pts',(9.67643521808628,30.4232330692483,126.611535637181));
#119327=CARTESIAN_POINT('Ctrl Pts',(9.67482640763888,30.4472182085229,126.605044876782));
#119328=CARTESIAN_POINT('Ctrl Pts',(9.67259556538434,30.4796939535801,126.595472019438));
#119329=CARTESIAN_POINT('Ctrl Pts',(9.67199796926011,30.4883191676482,126.592853299981));
#119330=CARTESIAN_POINT('Ctrl Pts',(9.67098541774517,30.5027994397358,126.588328251699));
#119331=CARTESIAN_POINT('Ctrl Pts',(9.67057259587047,30.508666102462,126.586459172744));
#119332=CARTESIAN_POINT('Ctrl Pts',(9.66971506999163,30.5207731853111,126.582527877569));
#119333=CARTESIAN_POINT('Ctrl Pts',(9.6692701406393,30.5270119031628,126.580461212425));
#119334=CARTESIAN_POINT('Ctrl Pts',(9.66808395754688,30.5435348657518,126.57487903491));
#119335=CARTESIAN_POINT('Ctrl Pts',(9.66733917599276,30.5537970130761,126.571299773282));
#119336=CARTESIAN_POINT('Ctrl Pts',(9.66392967791013,30.600300566692,126.554567996119));
#119337=CARTESIAN_POINT('Ctrl Pts',(9.66120863146903,30.6361110292305,126.540261233719));
#119338=CARTESIAN_POINT('Ctrl Pts',(9.65094279156276,30.7675062283601,126.482403396383));
#119339=CARTESIAN_POINT('Ctrl Pts',(9.64321022821429,30.8594045934907,126.431086964612));
#119340=CARTESIAN_POINT('Ctrl Pts',(9.63170809265067,30.9908026570209,126.340465030825));
#119341=CARTESIAN_POINT('Ctrl Pts',(9.62782140772832,31.0341966287455,126.307277592613));
#119342=CARTESIAN_POINT('Ctrl Pts',(9.62145682970451,31.1037817760943,126.248421669904));
#119343=CARTESIAN_POINT('Ctrl Pts',(9.61893960249259,31.1308955366265,126.22391442491));
#119344=CARTESIAN_POINT('Ctrl Pts',(9.61544391609849,31.167943667768,126.188144480954));
#119345=CARTESIAN_POINT('Ctrl Pts',(9.61443490562762,31.1785639124622,126.177610652233));
#119346=CARTESIAN_POINT('Ctrl Pts',(9.61270142660526,31.1966761367847,126.159155312624));
#119347=CARTESIAN_POINT('Ctrl Pts',(9.61197406417985,31.204234727627,126.151300805881));
#119348=CARTESIAN_POINT('Ctrl Pts',(9.61057995439297,31.2186391182505,126.136035415064));
#119349=CARTESIAN_POINT('Ctrl Pts',(9.60991276077203,31.2254957346616,126.128635448981));
#119350=CARTESIAN_POINT('Ctrl Pts',(9.60815535416587,31.2434538238869,126.108897664633));
#119351=CARTESIAN_POINT('Ctrl Pts',(9.607070031325,31.2544390590741,126.09645525319));
#119352=CARTESIAN_POINT('Ctrl Pts',(9.60307316080922,31.294471345934,126.049723411253));
#119353=CARTESIAN_POINT('Ctrl Pts',(9.60020989792636,31.3223148262538,126.014425624678));
#119354=CARTESIAN_POINT('Ctrl Pts',(9.59031124964165,31.414839344165,125.886836374096));
#119355=CARTESIAN_POINT('Ctrl Pts',(9.5835370976321,31.471556489273,125.789158496023));
#119356=CARTESIAN_POINT('Ctrl Pts',(9.57414193141392,31.5344641741873,125.650058102091));
#119357=CARTESIAN_POINT('Ctrl Pts',(9.57166102470114,31.5496262471594,125.613036352373));
#119358=CARTESIAN_POINT('Ctrl Pts',(9.56913306840647,31.5634400114683,125.575509626801));
#119359=CARTESIAN_POINT('Origin',(5.,30.,125.));
#119360=CARTESIAN_POINT('',(8.86798214956472,31.5634398523358,125.575510059103));
#119361=CARTESIAN_POINT('',(9.06223782796602,31.5634400121624,125.575509624915));
#119362=CARTESIAN_POINT('',(5.,31.5634400119422,125.575509625513));
#119363=CARTESIAN_POINT('Ctrl Pts',(9.06223782796602,31.5634400121624,125.575509624915));
#119364=CARTESIAN_POINT('Ctrl Pts',(9.06389062877664,31.5546571597327,125.59936928306));
#119365=CARTESIAN_POINT('Ctrl Pts',(9.06552593039392,31.5453286920362,125.623026351691));
#119366=CARTESIAN_POINT('Ctrl Pts',(9.06986230611145,31.5189184897683,125.685755228381));
#119367=CARTESIAN_POINT('Ctrl Pts',(9.07253368351343,31.5008723940766,125.72440047704));
#119368=CARTESIAN_POINT('Ctrl Pts',(9.07974294086227,31.4476581580646,125.827808886655));
#119369=CARTESIAN_POINT('Ctrl Pts',(9.08421375479368,31.4096464454391,125.890998851454));
#119370=CARTESIAN_POINT('Ctrl Pts',(9.08959742043858,31.3593897315873,125.963234708243));
#119371=CARTESIAN_POINT('Ctrl Pts',(9.09047580983357,31.351050327314,125.974897200724));
#119372=CARTESIAN_POINT('Ctrl Pts',(9.09583349033581,31.2994172908424,126.04516988738));
#119373=CARTESIAN_POINT('Ctrl Pts',(9.100365493913,31.2524724401225,126.100988420088));
#119374=CARTESIAN_POINT('Ctrl Pts',(9.10592594088404,31.193531694105,126.162406481669));
#119375=CARTESIAN_POINT('Ctrl Pts',(9.10673421359536,31.1849334271892,126.17117013488));
#119376=CARTESIAN_POINT('Ctrl Pts',(9.10801132842461,31.1713169420958,126.184745092782));
#119377=CARTESIAN_POINT('Ctrl Pts',(9.10847529551549,31.1663639269091,126.18962157821));
#119378=CARTESIAN_POINT('Ctrl Pts',(9.10934781214595,31.1570415320287,126.198685747192));
#119379=CARTESIAN_POINT('Ctrl Pts',(9.10975578548555,31.1526796637549,126.202880798536));
#119380=CARTESIAN_POINT('Ctrl Pts',(9.11072171024584,31.1423446034807,126.212712769137));
#119381=CARTESIAN_POINT('Ctrl Pts',(9.11128114532463,31.1363524818378,126.218329382178));
#119382=CARTESIAN_POINT('Ctrl Pts',(9.11316536903013,31.1161414121232,126.236995070868));
#119383=CARTESIAN_POINT('Ctrl Pts',(9.11450371254273,31.1017378789253,126.249840799439));
#119384=CARTESIAN_POINT('Ctrl Pts',(9.11783549987676,31.0656904302382,126.280882240694));
#119385=CARTESIAN_POINT('Ctrl Pts',(9.11984353779017,31.0438005795086,126.298782344046));
#119386=CARTESIAN_POINT('Ctrl Pts',(9.12904499849737,30.9423584789533,126.37751385227));
#119387=CARTESIAN_POINT('Ctrl Pts',(9.13641089983079,30.8578758516824,126.431654074186));
#119388=CARTESIAN_POINT('Ctrl Pts',(9.14959462764769,30.6956922180221,126.516049259841));
#119389=CARTESIAN_POINT('Ctrl Pts',(9.15544338884661,30.6195940658896,126.548709116859));
#119390=CARTESIAN_POINT('Ctrl Pts',(9.16244529028004,30.5228323443837,126.581956611231));
#119391=CARTESIAN_POINT('Ctrl Pts',(9.16377633813259,30.5041790633144,126.587999971436));
#119392=CARTESIAN_POINT('Ctrl Pts',(9.16589274344447,30.4741132579814,126.597157596781));
#119393=CARTESIAN_POINT('Ctrl Pts',(9.16668488409393,30.4627671873311,126.600481900291));
#119394=CARTESIAN_POINT('Ctrl Pts',(9.16818874073528,30.4410537909091,126.606593531448));
#119395=CARTESIAN_POINT('Ctrl Pts',(9.16890110925921,30.4306930819234,126.609401969724));
#119396=CARTESIAN_POINT('Ctrl Pts',(9.17053302582577,30.4067901400571,126.615633891181));
#119397=CARTESIAN_POINT('Ctrl Pts',(9.17145028816966,30.3932304299766,126.618987627196));
#119398=CARTESIAN_POINT('Ctrl Pts',(9.17435743659877,30.3498763959247,126.629133590807));
#119399=CARTESIAN_POINT('Ctrl Pts',(9.17632671654041,30.3199356884272,126.635277068908));
#119400=CARTESIAN_POINT('Ctrl Pts',(9.18097739394434,30.2480599214561,126.647975257419));
#119401=CARTESIAN_POINT('Ctrl Pts',(9.18363630859977,30.2060098563406,126.653758292877));
#119402=CARTESIAN_POINT('Ctrl Pts',(9.19083901894009,30.0903965122107,126.665179428479));
#119403=CARTESIAN_POINT('Ctrl Pts',(9.19531489950267,30.0166084997682,126.667548675528));
#119404=CARTESIAN_POINT('Ctrl Pts',(9.200643094285,29.9295580872039,126.664563701532));
#119405=CARTESIAN_POINT('Ctrl Pts',(9.20146119573136,29.9162161335331,126.663945503343));
#119406=CARTESIAN_POINT('Ctrl Pts',(9.20683260273836,29.8288936515202,126.658846506115));
#119407=CARTESIAN_POINT('Ctrl Pts',(9.21143818011781,29.7552839386996,126.649594001097));
#119408=CARTESIAN_POINT('Ctrl Pts',(9.2170802102421,29.6704924191865,126.633135477842));
#119409=CARTESIAN_POINT('Ctrl Pts',(9.21788848552087,29.6584666233909,126.630662952818));
#119410=CARTESIAN_POINT('Ctrl Pts',(9.21916544511396,29.6396796148329,126.626583382178));
#119411=CARTESIAN_POINT('Ctrl Pts',(9.21962924929007,29.6328989837258,126.625066496676));
#119412=CARTESIAN_POINT('Ctrl Pts',(9.22050176579212,29.6202281863918,126.62214858312));
#119413=CARTESIAN_POINT('Ctrl Pts',(9.22090990482348,29.6143359115425,126.620757804946));
#119414=CARTESIAN_POINT('Ctrl Pts',(9.22187631047224,29.6004640078077,126.617403635501));
#119415=CARTESIAN_POINT('Ctrl Pts',(9.22243606340184,29.5924911772155,126.615413285033));
#119416=CARTESIAN_POINT('Ctrl Pts',(9.224320707475,29.5658428771384,126.608550932538));
#119417=CARTESIAN_POINT('Ctrl Pts',(9.2256591413514,29.5472381731496,126.603413595641));
#119418=CARTESIAN_POINT('Ctrl Pts',(9.22899069894387,29.5016129306525,126.589957704299));
#119419=CARTESIAN_POINT('Ctrl Pts',(9.23099839492724,29.4747073438418,126.581272467764));
#119420=CARTESIAN_POINT('Ctrl Pts',(9.2401935388186,29.3536292096072,126.53875685569));
#119421=CARTESIAN_POINT('Ctrl Pts',(9.2475530962725,29.2624001899776,126.497168934755));
#119422=CARTESIAN_POINT('Ctrl Pts',(9.26073813260729,29.1035208529412,126.406674816822));
#119423=CARTESIAN_POINT('Ctrl Pts',(9.26659387250964,29.034733496332,126.360394502034));
#119424=CARTESIAN_POINT('Ctrl Pts',(9.27360369517304,28.9542436488877,126.297048455659));
#119425=CARTESIAN_POINT('Ctrl Pts',(9.27493592796731,28.9390388711654,126.284641032517));
#119426=CARTESIAN_POINT('Ctrl Pts',(9.27705437023721,28.915020529009,126.264324171669));
#119427=CARTESIAN_POINT('Ctrl Pts',(9.27784736591292,28.9060662974466,126.256584708829));
#119428=CARTESIAN_POINT('Ctrl Pts',(9.27935296367374,28.8891395643087,126.241636256614));
#119429=CARTESIAN_POINT('Ctrl Pts',(9.28006621780825,28.8811529048086,126.234444283122));
#119430=CARTESIAN_POINT('Ctrl Pts',(9.28170036114069,28.8629331627562,126.217715341672));
#119431=CARTESIAN_POINT('Ctrl Pts',(9.2826189591478,28.8527493838038,126.20812569259));
#119432=CARTESIAN_POINT('Ctrl Pts',(9.28553140525843,28.8206633136011,126.17713992245));
#119433=CARTESIAN_POINT('Ctrl Pts',(9.28750458431834,28.7992287819021,126.155267106442));
#119434=CARTESIAN_POINT('Ctrl Pts',(9.29216588929718,28.7494866701461,126.101626776961));
#119435=CARTESIAN_POINT('Ctrl Pts',(9.29483143063456,28.7217688432505,126.069341214927));
#119436=CARTESIAN_POINT('Ctrl Pts',(9.30203588235172,28.6495073996171,125.978341405609));
#119437=CARTESIAN_POINT('Ctrl Pts',(9.30650751469573,28.6075745791044,125.917678581757));
#119438=CARTESIAN_POINT('Ctrl Pts',(9.31185899291285,28.5627164708772,125.842592723949));
#119439=CARTESIAN_POINT('Ctrl Pts',(9.31270451253243,28.5557863750801,125.830658438441));
#119440=CARTESIAN_POINT('Ctrl Pts',(9.31806527959504,28.5129062079765,125.754655645326));
#119441=CARTESIAN_POINT('Ctrl Pts',(9.32263291966874,28.481083144172,125.688361785598));
#119442=CARTESIAN_POINT('Ctrl Pts',(9.32823302040352,28.4491679200935,125.608791268149));
#119443=CARTESIAN_POINT('Ctrl Pts',(9.32904185726714,28.4447206732827,125.597338381785));
#119444=CARTESIAN_POINT('Ctrl Pts',(9.3303199247623,28.437954361659,125.579325314704));
#119445=CARTESIAN_POINT('Ctrl Pts',(9.33078427992747,28.4355489340645,125.572797743037));
#119446=CARTESIAN_POINT('Ctrl Pts',(9.33165839559378,28.4311213138859,125.560546622252));
#119447=CARTESIAN_POINT('Ctrl Pts',(9.33206758777648,28.4290894275987,125.554826834419));
#119448=CARTESIAN_POINT('Ctrl Pts',(9.33303720840305,28.4243698410351,125.541307362684));
#119449=CARTESIAN_POINT('Ctrl Pts',(9.33359913574653,28.4217087642537,125.533498666134));
#119450=CARTESIAN_POINT('Ctrl Pts',(9.33549401670571,28.4129787270715,125.507244085695));
#119451=CARTESIAN_POINT('Ctrl Pts',(9.3368406362249,28.407174548846,125.488712681394));
#119452=CARTESIAN_POINT('Ctrl Pts',(9.34019642174467,28.3936548256269,125.442745196853));
#119453=CARTESIAN_POINT('Ctrl Pts',(9.34222034228052,28.3863170149145,125.415204972576));
#119454=CARTESIAN_POINT('Ctrl Pts',(9.35156970863305,28.3559679050901,125.288299099347));
#119455=CARTESIAN_POINT('Ctrl Pts',(9.35907027026344,28.3414048444474,125.187138151239));
#119456=CARTESIAN_POINT('Ctrl Pts',(9.372164154986,28.3320959320033,125.005518437495));
#119457=CARTESIAN_POINT('Ctrl Pts',(9.37780521709078,28.3337478627129,124.925558053323));
#119458=CARTESIAN_POINT('Ctrl Pts',(9.38460670912955,28.3429358067847,124.826577741219));
#119459=CARTESIAN_POINT('Ctrl Pts',(9.38593173415139,28.3450814992874,124.807174087865));
#119460=CARTESIAN_POINT('Ctrl Pts',(9.38804209578857,28.3490734135898,124.776086729871));
#119461=CARTESIAN_POINT('Ctrl Pts',(9.38883410597609,28.3507038232307,124.76437767509));
#119462=CARTESIAN_POINT('Ctrl Pts',(9.39033996129603,28.3540570438136,124.742039332603));
#119463=CARTESIAN_POINT('Ctrl Pts',(9.39105443692671,28.3557585334912,124.731407501921));
#119464=CARTESIAN_POINT('Ctrl Pts',(9.39269443624668,28.3599191920535,124.706932427447));
#119465=CARTESIAN_POINT('Ctrl Pts',(9.39361762578411,28.362450788668,124.693102200754));
#119466=CARTESIAN_POINT('Ctrl Pts',(9.39655773535488,28.3711199539213,124.648908383196));
#119467=CARTESIAN_POINT('Ctrl Pts',(9.39855343876987,28.3779295651696,124.618682249049));
#119468=CARTESIAN_POINT('Ctrl Pts',(9.40992512657868,28.422011448229,124.445669455774));
#119469=CARTESIAN_POINT('Ctrl Pts',(9.41868983410944,28.4772763776186,124.308160285715));
#119470=CARTESIAN_POINT('Ctrl Pts',(9.43132946666871,28.5777254521937,124.13058726598));
#119471=CARTESIAN_POINT('Ctrl Pts',(9.43488293577421,28.607999607853,124.082897550771));
#119472=CARTESIAN_POINT('Ctrl Pts',(9.43935226483786,28.6475224960859,124.027116313338));
#119473=CARTESIAN_POINT('Ctrl Pts',(9.44013746648668,28.6545172026832,124.017465477207));
#119474=CARTESIAN_POINT('Ctrl Pts',(9.44138595240005,28.6657058712102,124.002371623125));
#119475=CARTESIAN_POINT('Ctrl Pts',(9.44184470937689,28.6698311455922,123.996877866362));
#119476=CARTESIAN_POINT('Ctrl Pts',(9.44271163534225,28.6776499829049,123.986598313697));
#119477=CARTESIAN_POINT('Ctrl Pts',(9.44311927887378,28.6813357573731,123.981806916047));
#119478=CARTESIAN_POINT('Ctrl Pts',(9.44409128401035,28.6901468744469,123.970480811052));
#119479=CARTESIAN_POINT('Ctrl Pts',(9.44465721142636,28.6952950755365,123.963964274905));
#119480=CARTESIAN_POINT('Ctrl Pts',(9.4465989478592,28.7130275268391,123.94186051072));
#119481=CARTESIAN_POINT('Ctrl Pts',(9.44798957243805,28.7258435618516,123.926462572703));
#119482=CARTESIAN_POINT('Ctrl Pts',(9.45148445529768,28.7584098351155,123.88874028656));
#119483=CARTESIAN_POINT('Ctrl Pts',(9.45360522660707,28.778487081513,123.866708214499));
#119484=CARTESIAN_POINT('Ctrl Pts',(9.46388433594104,28.8777206459923,123.763514436302));
#119485=CARTESIAN_POINT('Ctrl Pts',(9.47224652539027,28.964433988561,123.690033288061));
#119486=CARTESIAN_POINT('Ctrl Pts',(9.48533154932152,29.1150441728456,123.586775878831));
#119487=CARTESIAN_POINT('Ctrl Pts',(9.49019753131637,29.1745366771242,123.55122057893));
#119488=CARTESIAN_POINT('Ctrl Pts',(9.49621709775722,29.2527953075334,123.510840821687));
#119489=CARTESIAN_POINT('Ctrl Pts',(9.49749314487559,29.2696590066946,123.502498081818));
#119490=CARTESIAN_POINT('Ctrl Pts',(9.49954099911461,29.2971589197535,123.489468516729));
#119491=CARTESIAN_POINT('Ctrl Pts',(9.50031890924003,29.3077087797483,123.484604400071));
#119492=CARTESIAN_POINT('Ctrl Pts',(9.50180757828612,29.3280935015322,123.475463136368));
#119493=CARTESIAN_POINT('Ctrl Pts',(9.5025188638239,29.3379204390714,123.47116984087));
#119494=CARTESIAN_POINT('Ctrl Pts',(9.50416527830476,29.360865028963,123.461408293511));
#119495=CARTESIAN_POINT('Ctrl Pts',(9.505097912426,29.3740126842085,123.456012353762));
#119496=CARTESIAN_POINT('Ctrl Pts',(9.50812736701992,29.4171926113231,123.438933092395));
#119497=CARTESIAN_POINT('Ctrl Pts',(9.51020077707883,29.4474960896393,123.427952293913));
#119498=CARTESIAN_POINT('Ctrl Pts',(9.51515765977125,29.5215275542217,123.403531641257));
#119499=CARTESIAN_POINT('Ctrl Pts',(9.51801400534572,29.5655277995352,123.390999856712));
#119500=CARTESIAN_POINT('Ctrl Pts',(9.52512364974521,29.6773705502116,123.364069212202));
#119501=CARTESIAN_POINT('Ctrl Pts',(9.52932920236756,29.7456985407943,123.352064834511));
#119502=CARTESIAN_POINT('Ctrl Pts',(9.53431798473983,29.8267489886206,123.342987586275));
#119503=CARTESIAN_POINT('Ctrl Pts',(9.53506828261862,29.8389370440741,123.341758530166));
#119504=CARTESIAN_POINT('Ctrl Pts',(9.54035810917796,29.9247549024237,123.334059628491));
#119505=CARTESIAN_POINT('Ctrl Pts',(9.54495075986615,29.9987212513298,123.332362533013));
#119506=CARTESIAN_POINT('Ctrl Pts',(9.55057783631371,30.0847825397663,123.336113599624));
#119507=CARTESIAN_POINT('Ctrl Pts',(9.55138426242192,30.0970129967992,123.336781887684));
#119508=CARTESIAN_POINT('Ctrl Pts',(9.55265795879871,30.1161462260015,123.338039100329));
#119509=CARTESIAN_POINT('Ctrl Pts',(9.55312034614369,30.1230548693247,123.33853634628));
#119510=CARTESIAN_POINT('Ctrl Pts',(9.55399193859455,30.1360029627462,123.339549478472));
#119511=CARTESIAN_POINT('Ctrl Pts',(9.55440058701291,30.1420429792716,123.340055263741));
#119512=CARTESIAN_POINT('Ctrl Pts',(9.55536870442133,30.1562821750216,123.341325922979));
#119513=CARTESIAN_POINT('Ctrl Pts',(9.55592967245522,30.1644786338746,123.342118646011));
#119514=CARTESIAN_POINT('Ctrl Pts',(9.55781630920489,30.1918749689669,123.344973449155));
#119515=CARTESIAN_POINT('Ctrl Pts',(9.55915549274808,30.2110440265521,123.347308489991));
#119516=CARTESIAN_POINT('Ctrl Pts',(9.56248720925415,30.2581563689506,123.353880341232));
#119517=CARTESIAN_POINT('Ctrl Pts',(9.56449425482874,30.286040219293,123.358495977858));
#119518=CARTESIAN_POINT('Ctrl Pts',(9.57366374245559,30.4117171385766,123.382598650216));
#119519=CARTESIAN_POINT('Ctrl Pts',(9.58099718867245,30.5077582331624,123.410132053281));
#119520=CARTESIAN_POINT('Ctrl Pts',(9.59421664708468,30.6786904021136,123.476216576636));
#119521=CARTESIAN_POINT('Ctrl Pts',(9.60012880930738,30.7542517363511,123.512167781886));
#119522=CARTESIAN_POINT('Ctrl Pts',(9.60719880541295,30.8439217731816,123.563427444288));
#119523=CARTESIAN_POINT('Ctrl Pts',(9.60853753652738,30.8608628458774,123.573514849237));
#119524=CARTESIAN_POINT('Ctrl Pts',(9.61066651903751,30.8877310138302,123.590166285313));
#119525=CARTESIAN_POINT('Ctrl Pts',(9.61146358798281,30.8977733419323,123.596539813483));
#119526=CARTESIAN_POINT('Ctrl Pts',(9.61297714274904,30.9168060247153,123.608907107617));
#119527=CARTESIAN_POINT('Ctrl Pts',(9.61369428162765,30.9258079652071,123.614881830643));
#119528=CARTESIAN_POINT('Ctrl Pts',(9.61533777717813,30.9463962535605,123.628836976373));
#119529=CARTESIAN_POINT('Ctrl Pts',(9.61626182401774,30.9579410150674,123.636877504492));
#119530=CARTESIAN_POINT('Ctrl Pts',(9.61919452745109,30.9944639949957,123.663007696109));
#119531=CARTESIAN_POINT('Ctrl Pts',(9.62118231034945,31.0190432202443,123.68164566045));
#119532=CARTESIAN_POINT('Ctrl Pts',(9.62588356945235,31.0765636881982,123.727832825373));
#119533=CARTESIAN_POINT('Ctrl Pts',(9.62857411733407,31.1089854761103,123.755994254681));
#119534=CARTESIAN_POINT('Ctrl Pts',(9.63575162178631,31.1933637022315,123.835208402818));
#119535=CARTESIAN_POINT('Ctrl Pts',(9.64017532207441,31.2431200588934,123.888465363202));
#119536=CARTESIAN_POINT('Ctrl Pts',(9.64536570077535,31.2968029093329,123.954054948268));
#119537=CARTESIAN_POINT('Ctrl Pts',(9.6460984683413,31.3042728001394,123.963384692323));
#119538=CARTESIAN_POINT('Ctrl Pts',(9.65143273124897,31.3578009760821,124.031734934387));
#119539=CARTESIAN_POINT('Ctrl Pts',(9.65608514848103,31.3999293187771,124.093713176586));
#119540=CARTESIAN_POINT('Ctrl Pts',(9.66178043508395,31.4439816721087,124.168961240757));
#119541=CARTESIAN_POINT('Ctrl Pts',(9.66259330704902,31.4501015409512,124.179686652672));
#119542=CARTESIAN_POINT('Ctrl Pts',(9.66387851619824,31.4595049466089,124.196600738023));
#119543=CARTESIAN_POINT('Ctrl Pts',(9.6643459851462,31.4628697737392,124.202744028575));
#119544=CARTESIAN_POINT('Ctrl Pts',(9.66523019048358,31.4691278949307,124.214342721006));
#119545=CARTESIAN_POINT('Ctrl Pts',(9.665646393804,31.4720297484639,124.219793266977));
#119546=CARTESIAN_POINT('Ctrl Pts',(9.66663674769495,31.4788324228329,124.232743764053));
#119547=CARTESIAN_POINT('Ctrl Pts',(9.66721247383979,31.4827065626442,124.240257472547));
#119548=CARTESIAN_POINT('Ctrl Pts',(9.66917003941979,31.495614202851,124.265765995321));
#119549=CARTESIAN_POINT('Ctrl Pts',(9.67056625661295,31.5043782354683,124.283894242856));
#119550=CARTESIAN_POINT('Ctrl Pts',(9.68032333574324,31.5627377542587,124.410411688846));
#119551=CARTESIAN_POINT('Ctrl Pts',(9.68909446134691,31.600902621213,124.523688025507));
#119552=CARTESIAN_POINT('Ctrl Pts',(9.70382089364437,31.6450752332532,124.723316246679));
#119553=CARTESIAN_POINT('Ctrl Pts',(9.70985267453206,31.6570807667373,124.807870666166));
#119554=CARTESIAN_POINT('Ctrl Pts',(9.71703343871411,31.6638234915555,124.912623351592));
#119555=CARTESIAN_POINT('Ctrl Pts',(9.71836913443617,31.6647395832279,124.932283927229));
#119556=CARTESIAN_POINT('Ctrl Pts',(9.72049712123613,31.6656510753911,124.963878749423));
#119557=CARTESIAN_POINT('Ctrl Pts',(9.72129611195126,31.6658669897983,124.975804243232));
#119558=CARTESIAN_POINT('Ctrl Pts',(9.72281599628191,31.6660349028388,124.998604987353));
#119559=CARTESIAN_POINT('Ctrl Pts',(9.72353751820475,31.6660085215143,125.009479411651));
#119560=CARTESIAN_POINT('Ctrl Pts',(9.72519512144482,31.6657019362699,125.034573127701));
#119561=CARTESIAN_POINT('Ctrl Pts',(9.72612882149797,31.6653461269038,125.048790776343));
#119562=CARTESIAN_POINT('Ctrl Pts',(9.72911018517412,31.6636188199951,125.094433965659));
#119563=CARTESIAN_POINT('Ctrl Pts',(9.73113604645711,31.6615393894272,125.125826914274));
#119564=CARTESIAN_POINT('Ctrl Pts',(9.74228321099633,31.6450241359012,125.300136882798));
#119565=CARTESIAN_POINT('Ctrl Pts',(9.75083238762177,31.6130450549854,125.440751655063));
#119566=CARTESIAN_POINT('Ctrl Pts',(9.75970370682547,31.5634400119926,125.575509625376));
#119567=CARTESIAN_POINT('Ctrl Pts',(9.56913306840647,31.5634400114683,125.575509626801));
#119568=CARTESIAN_POINT('Ctrl Pts',(9.56864716996237,31.5660951549131,125.568296615402));
#119569=CARTESIAN_POINT('Ctrl Pts',(9.5681595259895,31.5687004854742,125.561064948305));
#119570=CARTESIAN_POINT('Ctrl Pts',(9.5659052451564,31.5804661087518,125.527684127776));
#119571=CARTESIAN_POINT('Ctrl Pts',(9.56411601704802,31.5890224936162,125.501329196451));
#119572=CARTESIAN_POINT('Ctrl Pts',(9.56167154232831,31.5996054289806,125.465733241958));
#119573=CARTESIAN_POINT('Ctrl Pts',(9.56104668084311,31.6022167108484,125.456669007324));
#119574=CARTESIAN_POINT('Ctrl Pts',(9.55999897001426,31.6064364641037,125.441539641122));
#119575=CARTESIAN_POINT('Ctrl Pts',(9.55957853599634,31.6080879427172,125.435486548686));
#119576=CARTESIAN_POINT('Ctrl Pts',(9.55877269141859,31.6111728577567,125.423922687406));
#119577=CARTESIAN_POINT('Ctrl Pts',(9.5583876541566,31.6126123061516,125.418413635119));
#119578=CARTESIAN_POINT('Ctrl Pts',(9.55734329597031,31.6164244484165,125.403511902199));
#119579=CARTESIAN_POINT('Ctrl Pts',(9.5566810454587,31.6187434567815,125.39410590263));
#119580=CARTESIAN_POINT('Ctrl Pts',(9.55411836420225,31.6273464125161,125.357854465012));
#119581=CARTESIAN_POINT('Ctrl Pts',(9.55218959334705,31.6330452551839,125.330876333946));
#119582=CARTESIAN_POINT('Ctrl Pts',(9.54311115963848,31.656429207402,125.204779484353));
#119583=CARTESIAN_POINT('Ctrl Pts',(9.53571324710989,31.665774868943,125.104331873209));
#119584=CARTESIAN_POINT('Ctrl Pts',(9.52128883831654,31.6662119385057,124.905333820171));
#119585=CARTESIAN_POINT('Ctrl Pts',(9.51428695032684,31.6577231140409,124.807168482993));
#119586=CARTESIAN_POINT('Ctrl Pts',(9.50620094519701,31.6371828415255,124.690841094219));
#119587=CARTESIAN_POINT('Ctrl Pts',(9.50485842021703,31.6333986035078,124.671433498286));
#119588=CARTESIAN_POINT('Ctrl Pts',(9.5027277995363,31.6267921537136,124.640494726012));
#119589=CARTESIAN_POINT('Ctrl Pts',(9.50193277656213,31.6241907427051,124.628918880407));
#119590=CARTESIAN_POINT('Ctrl Pts',(9.50042587698607,31.6190001941022,124.606922875716));
#119591=CARTESIAN_POINT('Ctrl Pts',(9.49971332206483,31.6164335627545,124.596498078643));
#119592=CARTESIAN_POINT('Ctrl Pts',(9.4980996294026,31.6103658915538,124.572840745214));
#119593=CARTESIAN_POINT('Ctrl Pts',(9.49720055568629,31.6068021622483,124.559624973969));
#119594=CARTESIAN_POINT('Ctrl Pts',(9.49436241208394,31.5949728153653,124.517813663338));
#119595=CARTESIAN_POINT('Ctrl Pts',(9.49244281698285,31.5861033002369,124.489394046141));
#119596=CARTESIAN_POINT('Ctrl Pts',(9.48147243276875,31.5304771818831,124.326629596053));
#119597=CARTESIAN_POINT('Ctrl Pts',(9.47298940546583,31.4674336864022,124.198484501313));
#119598=CARTESIAN_POINT('Ctrl Pts',(9.46154633329198,31.3650306648649,124.043908184054));
#119599=CARTESIAN_POINT('Ctrl Pts',(9.45885385407333,31.3397960104764,124.008856000932));
#119600=CARTESIAN_POINT('Ctrl Pts',(9.45444157308856,31.2972611012484,123.954369511132));
#119601=CARTESIAN_POINT('Ctrl Pts',(9.45276273588887,31.2808170251525,123.934290351413));
#119602=CARTESIAN_POINT('Ctrl Pts',(9.45044776720107,31.2579199363108,123.907627343182));
#119603=CARTESIAN_POINT('Ctrl Pts',(9.44983819582955,31.2518705100522,123.900699857198));
#119604=CARTESIAN_POINT('Ctrl Pts',(9.44880969396276,31.241636939281,123.889174923717));
#119605=CARTESIAN_POINT('Ctrl Pts',(9.4483930094494,31.2374837411765,123.884550033525));
#119606=CARTESIAN_POINT('Ctrl Pts',(9.44753430771095,31.2289126982773,123.875112334785));
#119607=CARTESIAN_POINT('Ctrl Pts',(9.44709211540075,31.2244922885013,123.87030211515));
#119608=CARTESIAN_POINT('Ctrl Pts',(9.44592027908621,31.2127573580111,123.857682143448));
#119609=CARTESIAN_POINT('Ctrl Pts',(9.44518724657377,31.2053958300472,123.849916797485));
#119610=CARTESIAN_POINT('Ctrl Pts',(9.44191820299046,31.1724530575859,123.815830667233));
#119611=CARTESIAN_POINT('Ctrl Pts',(9.43933117439354,31.146082697487,123.790290457129));
#119612=CARTESIAN_POINT('Ctrl Pts',(9.42914505173448,31.040386484491,123.694481182765));
#119613=CARTESIAN_POINT('Ctrl Pts',(9.42134133008691,30.9552712344495,123.630970914103));
#119614=CARTESIAN_POINT('Ctrl Pts',(9.40777101218967,30.7943836572881,123.533276403464));
#119615=CARTESIAN_POINT('Ctrl Pts',(9.40195322697442,30.7209928679223,123.495840284648));
#119616=CARTESIAN_POINT('Ctrl Pts',(9.39498161824195,30.6270662864124,123.456391390294));
#119617=CARTESIAN_POINT('Ctrl Pts',(9.39365183205418,30.6088740105948,123.449125355294));
#119618=CARTESIAN_POINT('Ctrl Pts',(9.39153710031163,30.5795082106172,123.437993003705));
#119619=CARTESIAN_POINT('Ctrl Pts',(9.39074538698554,30.568414804482,123.433922018177));
#119620=CARTESIAN_POINT('Ctrl Pts',(9.38924214380341,30.5471655659103,123.42637964995));
#119621=CARTESIAN_POINT('Ctrl Pts',(9.38852996381217,30.537017715169,123.422887719469));
#119622=CARTESIAN_POINT('Ctrl Pts',(9.38689820988419,30.5135855352467,123.41507697359));
#119623=CARTESIAN_POINT('Ctrl Pts',(9.38598092392063,30.5002790973745,123.410826646936));
#119624=CARTESIAN_POINT('Ctrl Pts',(9.38307265547898,30.4576810215181,123.397808102247));
#119625=CARTESIAN_POINT('Ctrl Pts',(9.38110231162277,30.4281998155988,123.389678323856));
#119626=CARTESIAN_POINT('Ctrl Pts',(9.37644856057148,30.3572809816464,123.372207232335));
#119627=CARTESIAN_POINT('Ctrl Pts',(9.37378768765131,30.3156768487121,123.36362977878));
#119628=CARTESIAN_POINT('Ctrl Pts',(9.36658170407566,30.2010217742872,123.34452781641));
#119629=CARTESIAN_POINT('Ctrl Pts',(9.36210453789624,30.1275289630816,123.33725087972));
#119630=CARTESIAN_POINT('Ctrl Pts',(9.35676858294957,30.0403413269084,123.334434094504));
#119631=CARTESIAN_POINT('Ctrl Pts',(9.35594405497878,30.0268823094354,123.334162509623));
#119632=CARTESIAN_POINT('Ctrl Pts',(9.35057193163556,29.9394012713396,123.333457724416));
#119633=CARTESIAN_POINT('Ctrl Pts',(9.34597196269281,29.8654325288746,123.337795388156));
#119634=CARTESIAN_POINT('Ctrl Pts',(9.34033627599718,29.7798291636796,123.348566844789));
#119635=CARTESIAN_POINT('Ctrl Pts',(9.33952820551658,29.7676684451976,123.350233746805));
#119636=CARTESIAN_POINT('Ctrl Pts',(9.33825164582206,29.7486573516972,123.353054004049));
#119637=CARTESIAN_POINT('Ctrl Pts',(9.33778803591536,29.7417936015258,123.354116136584));
#119638=CARTESIAN_POINT('Ctrl Pts',(9.33691592106518,29.7289624489481,123.356183931711));
#119639=CARTESIAN_POINT('Ctrl Pts',(9.33650798934424,29.7229936242695,123.357179229636));
#119640=CARTESIAN_POINT('Ctrl Pts',(9.33554217333016,29.7089375907119,123.359601842878));
#119641=CARTESIAN_POINT('Ctrl Pts',(9.3349828051974,29.7008553627503,123.361056462556));
#119642=CARTESIAN_POINT('Ctrl Pts',(9.33309999122663,29.6738350243931,123.366126036395));
#119643=CARTESIAN_POINT('Ctrl Pts',(9.33176303308278,29.6549497482706,123.37000982674));
#119644=CARTESIAN_POINT('Ctrl Pts',(9.32843566130366,29.60858602914,123.380386407281));
#119645=CARTESIAN_POINT('Ctrl Pts',(9.32643071597727,29.5811975973753,123.387251583767));
#119646=CARTESIAN_POINT('Ctrl Pts',(9.31725632910224,29.4578264844409,123.42153018603));
#119647=CARTESIAN_POINT('Ctrl Pts',(9.30991537579628,29.3642512390301,123.456839928591));
#119648=CARTESIAN_POINT('Ctrl Pts',(9.29673262182983,29.1996977010349,123.536456780961));
#119649=CARTESIAN_POINT('Ctrl Pts',(9.29086212567876,29.1277926793247,123.578134794794));
#119650=CARTESIAN_POINT('Ctrl Pts',(9.28383873261389,29.0430915215764,123.636083910724));
#119651=CARTESIAN_POINT('Ctrl Pts',(9.28250671013498,29.0270952051103,123.647447874634));
#119652=CARTESIAN_POINT('Ctrl Pts',(9.2803888262205,29.0017812781593,123.666112699913));
#119653=CARTESIAN_POINT('Ctrl Pts',(9.27959617713721,28.9923346463331,123.673234574811));
#119654=CARTESIAN_POINT('Ctrl Pts',(9.27809138274418,28.9744575708709,123.687013296674));
#119655=CARTESIAN_POINT('Ctrl Pts',(9.27737858443528,28.9660141207505,123.693652202597));
#119656=CARTESIAN_POINT('Ctrl Pts',(9.27574570214914,28.9467333340873,123.709116334068));
#119657=CARTESIAN_POINT('Ctrl Pts',(9.274827904384,28.9359415659544,123.717997278809));
#119658=CARTESIAN_POINT('Ctrl Pts',(9.27191899822293,28.9018999718918,123.74673738513));
#119659=CARTESIAN_POINT('Ctrl Pts',(9.26994850263097,28.8790837323931,123.767101884815));
#119660=CARTESIAN_POINT('Ctrl Pts',(9.26529459330476,28.8259535292162,123.817217844472));
#119661=CARTESIAN_POINT('Ctrl Pts',(9.26263367781123,28.7961909334648,123.847523165944));
#119662=CARTESIAN_POINT('Ctrl Pts',(9.25543143681679,28.7180244234719,123.933451286025));
#119663=CARTESIAN_POINT('Ctrl Pts',(9.25095773826373,28.6721028206199,123.9912002253));
#119664=CARTESIAN_POINT('Ctrl Pts',(9.24560576632945,28.6223142210004,124.063128759169));
#119665=CARTESIAN_POINT('Ctrl Pts',(9.244761677796,28.6146135150153,124.074554102582));
#119666=CARTESIAN_POINT('Ctrl Pts',(9.23939450072776,28.5666805691533,124.147610238665));
#119667=CARTESIAN_POINT('Ctrl Pts',(9.23481904443503,28.5304327596079,124.211747324718));
#119668=CARTESIAN_POINT('Ctrl Pts',(9.22921053597087,28.4932265149786,124.28912698951));
#119669=CARTESIAN_POINT('Ctrl Pts',(9.22840215686886,28.488028296534,124.300251246254));
#119670=CARTESIAN_POINT('Ctrl Pts',(9.22712490978736,28.4800807268359,124.317761242526));
#119671=CARTESIAN_POINT('Ctrl Pts',(9.22666091676075,28.4772474609219,124.324108722137));
#119672=CARTESIAN_POINT('Ctrl Pts',(9.2257882096669,28.4720208930417,124.336017691538));
#119673=CARTESIAN_POINT('Ctrl Pts',(9.225380070314,28.4696180789519,124.341574735971));
#119674=CARTESIAN_POINT('Ctrl Pts',(9.22441364065567,28.4640252335839,124.354705452181));
#119675=CARTESIAN_POINT('Ctrl Pts',(9.22385386487468,28.4608608945387,124.362289765275));
#119676=CARTESIAN_POINT('Ctrl Pts',(9.22196831925048,28.4504482161981,124.387775951836));
#119677=CARTESIAN_POINT('Ctrl Pts',(9.22062898692214,28.4434553884755,124.405779663196));
#119678=CARTESIAN_POINT('Ctrl Pts',(9.21729440188898,28.4269913757312,124.450454042056));
#119679=CARTESIAN_POINT('Ctrl Pts',(9.21528454323937,28.417884000301,124.477251805759));
#119680=CARTESIAN_POINT('Ctrl Pts',(9.20606641611484,28.3796040026176,124.600071349076));
#119681=CARTESIAN_POINT('Ctrl Pts',(9.19868545263399,28.358461040177,124.698377004531));
#119682=CARTESIAN_POINT('Ctrl Pts',(9.18551374117176,28.3363079525061,124.879727007108));
#119683=CARTESIAN_POINT('Ctrl Pts',(9.17969014083037,28.3323956444406,124.962102727797));
#119684=CARTESIAN_POINT('Ctrl Pts',(9.17271223990494,28.3351156322315,125.064032096668));
#119685=CARTESIAN_POINT('Ctrl Pts',(9.17138174775636,28.3359840624065,125.083612701075));
#119686=CARTESIAN_POINT('Ctrl Pts',(9.16926580099379,28.3379300513207,125.114975149166));
#119687=CARTESIAN_POINT('Ctrl Pts',(9.16847357751368,28.338787905789,125.126768252138));
#119688=CARTESIAN_POINT('Ctrl Pts',(9.16696929283938,28.3406643759151,125.14925353621));
#119689=CARTESIAN_POINT('Ctrl Pts',(9.16625658187803,28.3416609728578,125.159946902741));
#119690=CARTESIAN_POINT('Ctrl Pts',(9.16462348783413,28.3441927358669,125.184536565057));
#119691=CARTESIAN_POINT('Ctrl Pts',(9.16370539589856,28.3457995704,125.198424792414));
#119692=CARTESIAN_POINT('Ctrl Pts',(9.16079390380021,28.3514817222167,125.242653105299));
#119693=CARTESIAN_POINT('Ctrl Pts',(9.15882117964728,28.3562186042313,125.272902827336));
#119694=CARTESIAN_POINT('Ctrl Pts',(9.15416094092926,28.3695211461486,125.344823418261));
#119695=CARTESIAN_POINT('Ctrl Pts',(9.15149602179119,28.378854309098,125.3863308322));
#119696=CARTESIAN_POINT('Ctrl Pts',(9.14428941665975,28.4086784048964,125.498683441747));
#119697=CARTESIAN_POINT('Ctrl Pts',(9.13981526008009,28.4322986273763,125.568596838621));
#119698=CARTESIAN_POINT('Ctrl Pts',(9.13445110096442,28.4658095445839,125.649623537523));
#119699=CARTESIAN_POINT('Ctrl Pts',(9.13359540701092,28.4713097894908,125.662463076913));
#119700=CARTESIAN_POINT('Ctrl Pts',(9.12822988966241,28.5067117578528,125.742314513883));
#119701=CARTESIAN_POINT('Ctrl Pts',(9.12366752697258,28.5408486961765,125.807350829049));
#119702=CARTESIAN_POINT('Ctrl Pts',(9.11807353132014,28.585565359013,125.880387052816));
#119703=CARTESIAN_POINT('Ctrl Pts',(9.11726530298087,28.5920910319217,125.890785626423));
#119704=CARTESIAN_POINT('Ctrl Pts',(9.11598834546718,28.6024894353629,125.9069556283));
#119705=CARTESIAN_POINT('Ctrl Pts',(9.11552449194505,28.6062845311625,125.91277679502));
#119706=CARTESIAN_POINT('Ctrl Pts',(9.11465203999268,28.6134531483526,125.923623551332));
#119707=CARTESIAN_POINT('Ctrl Pts',(9.11424401607584,28.6168177826448,125.928654718023));
#119708=CARTESIAN_POINT('Ctrl Pts',(9.11327792400074,28.6248134712663,125.940470889433));
#119709=CARTESIAN_POINT('Ctrl Pts',(9.11271837148313,28.629467376369,125.947240097954));
#119710=CARTESIAN_POINT('Ctrl Pts',(9.11083404476517,28.6452219732414,125.96979634695));
#119711=CARTESIAN_POINT('Ctrl Pts',(9.10949572735296,28.656546431822,125.985424216849));
#119712=CARTESIAN_POINT('Ctrl Pts',(9.10616414897365,28.685123652693,126.023452735951));
#119713=CARTESIAN_POINT('Ctrl Pts',(9.10415631001334,28.7026797911337,126.045617237172));
#119714=CARTESIAN_POINT('Ctrl Pts',(9.09495578857043,28.7849413079796,126.144209443588));
#119715=CARTESIAN_POINT('Ctrl Pts',(9.08759085625378,28.8558928834684,126.215155230123));
#119716=CARTESIAN_POINT('Ctrl Pts',(9.07441427394306,28.9962196575627,126.332218071535));
#119717=CARTESIAN_POINT('Ctrl Pts',(9.06857145829816,29.0635082467873,126.380350268506));
#119718=CARTESIAN_POINT('Ctrl Pts',(9.0615750928155,29.1508490586062,126.433486316624));
#119719=CARTESIAN_POINT('Ctrl Pts',(9.06024411658716,29.1677768170299,126.443379704692));
#119720=CARTESIAN_POINT('Ctrl Pts',(9.05812764948606,29.1951882634531,126.458757650479));
#119721=CARTESIAN_POINT('Ctrl Pts',(9.0573353816748,29.2055621402121,126.464433103125));
#119722=CARTESIAN_POINT('Ctrl Pts',(9.05583116792962,29.2254700580637,126.475050732417));
#119723=CARTESIAN_POINT('Ctrl Pts',(9.0551185706702,29.2349931313293,126.480012092604));
#119724=CARTESIAN_POINT('Ctrl Pts',(9.05348595834825,29.2570188450594,126.491217719292));
#119725=CARTESIAN_POINT('Ctrl Pts',(9.05256823130631,29.2695535273992,126.497397493422));
#119726=CARTESIAN_POINT('Ctrl Pts',(9.04965883924049,29.3097644901472,126.516596961196));
#119727=CARTESIAN_POINT('Ctrl Pts',(9.04768781109885,29.3377230897316,126.529013042453));
#119728=CARTESIAN_POINT('Ctrl Pts',(9.04303233715148,29.4052899337179,126.556817331149));
#119729=CARTESIAN_POINT('Ctrl Pts',(9.04037042507345,29.445176324879,126.571474255084));
#119730=CARTESIAN_POINT('Ctrl Pts',(9.03316567721225,29.5557071724755,126.607356756388));
#119731=CARTESIAN_POINT('Ctrl Pts',(9.02869055674728,29.6272682001601,126.625442472419));
#119732=CARTESIAN_POINT('Ctrl Pts',(9.02333973042141,29.7133032336722,126.641203717781));
#119733=CARTESIAN_POINT('Ctrl Pts',(9.02249826232157,29.7268444278566,126.643511699627));
#119734=CARTESIAN_POINT('Ctrl Pts',(9.01712962638129,29.8131852107088,126.657131218315));
#119735=CARTESIAN_POINT('Ctrl Pts',(9.01255003678489,29.8866303794313,126.663769280485));
#119736=CARTESIAN_POINT('Ctrl Pts',(9.00693693979593,29.9725368461396,126.665818868146));
#119737=CARTESIAN_POINT('Ctrl Pts',(9.00612868875217,29.9848128368429,126.665976006613));
#119738=CARTESIAN_POINT('Ctrl Pts',(9.00485172247082,30.0040378855395,126.666009598622));
#119739=CARTESIAN_POINT('Ctrl Pts',(9.00438788383683,30.0109866260611,126.665978264232));
#119740=CARTESIAN_POINT('Ctrl Pts',(9.00351543706875,30.0239874224951,126.665838300056));
#119741=CARTESIAN_POINT('Ctrl Pts',(9.00310740324179,30.0300393444174,126.665740157251));
#119742=CARTESIAN_POINT('Ctrl Pts',(9.00214128867261,30.0443035726448,126.665431079229));
#119743=CARTESIAN_POINT('Ctrl Pts',(9.00158172344623,30.0525150018009,126.665192377392));
#119744=CARTESIAN_POINT('Ctrl Pts',(8.99969746228032,30.0800093452069,126.664189568427));
#119745=CARTESIAN_POINT('Ctrl Pts',(8.9983592260331,30.0992798941254,126.663151177217));
#119746=CARTESIAN_POINT('Ctrl Pts',(8.99502793617251,30.1467247024318,126.659767157506));
#119747=CARTESIAN_POINT('Ctrl Pts',(8.99302030917817,30.1748651079416,126.657038674591));
#119748=CARTESIAN_POINT('Ctrl Pts',(8.98382189110826,30.3022842302785,126.64140245331));
#119749=CARTESIAN_POINT('Ctrl Pts',(8.97645892392758,30.4003456884862,126.620278231699));
#119750=CARTESIAN_POINT('Ctrl Pts',(8.96327728746326,30.5748712970012,126.565860327092));
#119751=CARTESIAN_POINT('Ctrl Pts',(8.95742785122725,30.6518909001427,126.535394913637));
#119752=CARTESIAN_POINT('Ctrl Pts',(8.95042763332085,30.7439528556987,126.490796163709));
#119753=CARTESIAN_POINT('Ctrl Pts',(8.94909894063734,30.7614154818554,126.481953296802));
#119754=CARTESIAN_POINT('Ctrl Pts',(8.94698515473778,30.7891665586458,126.467280413257));
#119755=CARTESIAN_POINT('Ctrl Pts',(8.94619331698695,30.7995553735554,126.461645266639));
#119756=CARTESIAN_POINT('Ctrl Pts',(8.94468933507047,30.8192696930831,126.450678644916));
#119757=CARTESIAN_POINT('Ctrl Pts',(8.94397654563138,30.8286052749591,126.445366620738));
#119758=CARTESIAN_POINT('Ctrl Pts',(8.94234266461335,30.8499817536594,126.432928039181));
#119759=CARTESIAN_POINT('Ctrl Pts',(8.94142387195601,30.8619856604941,126.425739277675));
#119760=CARTESIAN_POINT('Ctrl Pts',(8.93850759319652,30.9000136910563,126.402309626929));
#119761=CARTESIAN_POINT('Ctrl Pts',(8.9365308818662,30.9256813247731,126.385500345896));
#119762=CARTESIAN_POINT('Ctrl Pts',(8.93185912496166,30.9858913214588,126.343649214182));
#119763=CARTESIAN_POINT('Ctrl Pts',(8.92918683350596,31.0199651149679,126.317970582259));
#119764=CARTESIAN_POINT('Ctrl Pts',(8.92200100675805,31.1097940948035,126.244701257382));
#119765=CARTESIAN_POINT('Ctrl Pts',(8.91755340833453,31.1634549148331,126.194695431589));
#119766=CARTESIAN_POINT('Ctrl Pts',(8.91226882714098,31.2226341911993,126.131765713061));
#119767=CARTESIAN_POINT('Ctrl Pts',(8.91146548971117,31.2315054209678,126.122106228499));
#119768=CARTESIAN_POINT('Ctrl Pts',(8.90609018670832,31.2899534827182,126.056936688228));
#119769=CARTESIAN_POINT('Ctrl Pts',(8.90146616531748,31.3358706493544,125.99826947128));
#119770=CARTESIAN_POINT('Ctrl Pts',(8.89580369504892,31.3846120154415,125.926583174079));
#119771=CARTESIAN_POINT('Ctrl Pts',(8.89499521700938,31.3914042262869,125.916352044299));
#119772=CARTESIAN_POINT('Ctrl Pts',(8.89371793380427,31.4018623164603,125.900214614007));
#119773=CARTESIAN_POINT('Ctrl Pts',(8.89325400766306,31.4056055446989,125.894358627129));
#119774=CARTESIAN_POINT('Ctrl Pts',(8.89238146149913,31.4125400830397,125.883359017788));
#119775=CARTESIAN_POINT('Ctrl Pts',(8.89197341652628,31.4157401430931,125.878221203947));
#119776=CARTESIAN_POINT('Ctrl Pts',(8.89100732896184,31.4232168571379,125.86607000561));
#119777=CARTESIAN_POINT('Ctrl Pts',(8.89044780258653,31.4274697158115,125.859042304214));
#119778=CARTESIAN_POINT('Ctrl Pts',(8.88856381186247,31.4415375345811,125.835402790564));
#119779=CARTESIAN_POINT('Ctrl Pts',(8.88722581229469,31.4511154455202,125.818652655633));
#119780=CARTESIAN_POINT('Ctrl Pts',(8.88389524261034,31.474000810046,125.776966143342));
#119781=CARTESIAN_POINT('Ctrl Pts',(8.88188810664293,31.4869684535879,125.751850659163));
#119782=CARTESIAN_POINT('Ctrl Pts',(8.87594098827087,31.5231584883341,125.677156349413));
#119783=CARTESIAN_POINT('Ctrl Pts',(8.87195995633795,31.5445632203393,125.626790620188));
#119784=CARTESIAN_POINT('Ctrl Pts',(8.86798214956472,31.5634398523358,125.575510059103));
#119785=CARTESIAN_POINT('Origin',(5.,30.,125.));
#119786=CARTESIAN_POINT('',(8.1662633962835,31.5634400119422,125.575509625513));
#119787=CARTESIAN_POINT('',(8.36102759409884,31.5634400156515,125.575509615436));
#119788=CARTESIAN_POINT('',(5.,31.5634400119422,125.575509625513));
#119789=CARTESIAN_POINT('Ctrl Pts',(8.36102759409884,31.5634400156515,125.575509615436));
#119790=CARTESIAN_POINT('Ctrl Pts',(8.36145852083983,31.5613892619103,125.581080730801));
#119791=CARTESIAN_POINT('Ctrl Pts',(8.36188920460623,31.5593085163546,125.586641465852));
#119792=CARTESIAN_POINT('Ctrl Pts',(8.36819296046608,31.5283939536364,125.667932879917));
#119793=CARTESIAN_POINT('Ctrl Pts',(8.37398572743088,31.4940993543677,125.741480043892));
#119794=CARTESIAN_POINT('Ctrl Pts',(8.38168335485436,31.4399870101799,125.838385140646));
#119795=CARTESIAN_POINT('Ctrl Pts',(8.38373581782508,31.4246887189983,125.864126430352));
#119796=CARTESIAN_POINT('Ctrl Pts',(8.38670231113614,31.4013023989325,125.901165799042));
#119797=CARTESIAN_POINT('Ctrl Pts',(8.38763577663898,31.3937544634111,125.912796103473));
#119798=CARTESIAN_POINT('Ctrl Pts',(8.38928192900608,31.380110235804,125.933256028303));
#119799=CARTESIAN_POINT('Ctrl Pts',(8.38999673985287,31.3740722687193,125.942123392621));
#119800=CARTESIAN_POINT('Ctrl Pts',(8.39149694279808,31.3611630417819,125.960693767205));
#119801=CARTESIAN_POINT('Ctrl Pts',(8.39228155759251,31.3542726932988,125.97038282403));
#119802=CARTESIAN_POINT('Ctrl Pts',(8.3943686850467,31.335576939568,125.996085335921));
#119803=CARTESIAN_POINT('Ctrl Pts',(8.39566403801901,31.3235872118942,126.011962798405));
#119804=CARTESIAN_POINT('Ctrl Pts',(8.40340712935528,31.2496501976135,126.106311431212));
#119805=CARTESIAN_POINT('Ctrl Pts',(8.40957462958438,31.1810242007115,126.179294727921));
#119806=CARTESIAN_POINT('Ctrl Pts',(8.42058854287345,31.0463335164611,126.298909348018));
#119807=CARTESIAN_POINT('Ctrl Pts',(8.42544480537767,30.9826488016226,126.347731155626));
#119808=CARTESIAN_POINT('Ctrl Pts',(8.43230673082812,30.8910591565401,126.407991387263));
#119809=CARTESIAN_POINT('Ctrl Pts',(8.43417388398498,30.8659911190021,126.423546749655));
#119810=CARTESIAN_POINT('Ctrl Pts',(8.43735540530436,30.8233400039988,126.448469328534));
#119811=CARTESIAN_POINT('Ctrl Pts',(8.43865182793557,30.8059774392345,126.45820178318));
#119812=CARTESIAN_POINT('Ctrl Pts',(8.4405157462498,30.7811196577645,126.471556060855));
#119813=CARTESIAN_POINT('Ctrl Pts',(8.44106821786963,30.7737644955833,126.475436768593));
#119814=CARTESIAN_POINT('Ctrl Pts',(8.44202971216977,30.7609930904826,126.482053418287));
#119815=CARTESIAN_POINT('Ctrl Pts',(8.44243713322745,30.7555904441105,126.484815105642));
#119816=CARTESIAN_POINT('Ctrl Pts',(8.44331177719675,30.744013762075,126.490653246359));
#119817=CARTESIAN_POINT('Ctrl Pts',(8.44377948213751,30.7378357644251,126.493720843886));
#119818=CARTESIAN_POINT('Ctrl Pts',(8.4450698551519,30.7208203346055,126.502038300619));
#119819=CARTESIAN_POINT('Ctrl Pts',(8.44589704809475,30.709944998219,126.507209039875));
#119820=CARTESIAN_POINT('Ctrl Pts',(8.45102186771389,30.6427096283131,126.538287353876));
#119821=CARTESIAN_POINT('Ctrl Pts',(8.45546530719541,30.5850004856562,126.56114586761));
#119822=CARTESIAN_POINT('Ctrl Pts',(8.46974306413475,30.3979455265239,126.623408521195));
#119823=CARTESIAN_POINT('Ctrl Pts',(8.47965823365812,30.2649911581475,126.65033525785));
#119824=CARTESIAN_POINT('Ctrl Pts',(8.49150673398063,30.0956673731849,126.663612348605));
#119825=CARTESIAN_POINT('Ctrl Pts',(8.49389462102906,30.0610211654159,126.66524323082));
#119826=CARTESIAN_POINT('Ctrl Pts',(8.49717171162583,30.0127639432865,126.666006490561));
#119827=CARTESIAN_POINT('Ctrl Pts',(8.49808893532242,29.9991784572749,126.666055187832));
#119828=CARTESIAN_POINT('Ctrl Pts',(8.49967286541058,29.9755860187698,126.665851168457));
#119829=CARTESIAN_POINT('Ctrl Pts',(8.50034190495544,29.9655792989757,126.665674452232));
#119830=CARTESIAN_POINT('Ctrl Pts',(8.50173627610054,29.9446403430466,126.665115897215));
#119831=CARTESIAN_POINT('Ctrl Pts',(8.50246102719351,29.9337090211443,126.664716540014));
#119832=CARTESIAN_POINT('Ctrl Pts',(8.50418758983578,29.9075588630099,126.663503196599));
#119833=CARTESIAN_POINT('Ctrl Pts',(8.5051861990846,29.8923455365339,126.662587979855));
#119834=CARTESIAN_POINT('Ctrl Pts',(8.5086872119435,29.8387266175708,126.658623240173));
#119835=CARTESIAN_POINT('Ctrl Pts',(8.51115477896851,29.8004147811303,126.654450439348));
#119836=CARTESIAN_POINT('Ctrl Pts',(8.51732449331676,29.7037939551105,126.640521149728));
#119837=CARTESIAN_POINT('Ctrl Pts',(8.52097709772414,29.6457953049644,126.628983567565));
#119838=CARTESIAN_POINT('Ctrl Pts',(8.53143350738073,29.4805246785236,126.586859849257));
#119839=CARTESIAN_POINT('Ctrl Pts',(8.53812306685359,29.3755663929442,126.548565981097));
#119840=CARTESIAN_POINT('Ctrl Pts',(8.54695407795666,29.2507034520346,126.488238069897));
#119841=CARTESIAN_POINT('Ctrl Pts',(8.54871243418737,29.2264745734536,126.47578998615));
#119842=CARTESIAN_POINT('Ctrl Pts',(8.55113802951733,29.1940995719078,126.458140399991));
#119843=CARTESIAN_POINT('Ctrl Pts',(8.55177625497132,29.185676231403,126.453453031571));
#119844=CARTESIAN_POINT('Ctrl Pts',(8.55279786232767,29.1723535360796,126.445887137549));
#119845=CARTESIAN_POINT('Ctrl Pts',(8.55317829004431,29.1674272588959,126.443056101508));
#119846=CARTESIAN_POINT('Ctrl Pts',(8.55398173673604,29.1570988645817,126.437050082402));
#119847=CARTESIAN_POINT('Ctrl Pts',(8.55440511494797,29.1517000488509,126.433869747167));
#119848=CARTESIAN_POINT('Ctrl Pts',(8.55547120913263,29.1382115516744,126.425821101955));
#119849=CARTESIAN_POINT('Ctrl Pts',(8.55611631241708,29.1301451635377,126.420914387789));
#119850=CARTESIAN_POINT('Ctrl Pts',(8.55868226675073,29.0984194010315,126.401244497095));
#119851=CARTESIAN_POINT('Ctrl Pts',(8.56063261135995,29.075091979303,126.385957665736));
#119852=CARTESIAN_POINT('Ctrl Pts',(8.56601609817774,29.0125431963903,126.342686041623));
#119853=CARTESIAN_POINT('Ctrl Pts',(8.56949265539986,28.9741353028369,126.313574434025));
#119854=CARTESIAN_POINT('Ctrl Pts',(8.58127894628778,28.8491331781839,126.209998444722));
#119855=CARTESIAN_POINT('Ctrl Pts',(8.58962918093296,28.7689299331193,126.128300983447));
#119856=CARTESIAN_POINT('Ctrl Pts',(8.60074071123726,28.6704310918054,126.004846043431));
#119857=CARTESIAN_POINT('Ctrl Pts',(8.60377126111752,28.6445077130205,125.969592862229));
#119858=CARTESIAN_POINT('Ctrl Pts',(8.60786739974862,28.6107973889234,125.919751009295));
#119859=CARTESIAN_POINT('Ctrl Pts',(8.60897803404597,28.6017963636637,125.906009072045));
#119860=CARTESIAN_POINT('Ctrl Pts',(8.61075583000625,28.5876192024087,125.883650067073));
#119861=CARTESIAN_POINT('Ctrl Pts',(8.61142768460174,28.582315423162,125.875115653316));
#119862=CARTESIAN_POINT('Ctrl Pts',(8.61282281995839,28.5714168362554,125.857219384673));
#119863=CARTESIAN_POINT('Ctrl Pts',(8.6135455627643,28.5658360758292,125.847849501632));
#119864=CARTESIAN_POINT('Ctrl Pts',(8.6152580276974,28.5527722449584,125.825417717538));
#119865=CARTESIAN_POINT('Ctrl Pts',(8.61624468624745,28.5453733237219,125.812307725258));
#119866=CARTESIAN_POINT('Ctrl Pts',(8.61965178295648,28.5202860417297,125.766413817886));
#119867=CARTESIAN_POINT('Ctrl Pts',(8.62203991211518,28.5035194603453,125.733136999518));
#119868=CARTESIAN_POINT('Ctrl Pts',(8.62795381039532,28.4642894959505,125.648311716775));
#119869=CARTESIAN_POINT('Ctrl Pts',(8.63143551930446,28.4432926685673,125.596135736531));
#119870=CARTESIAN_POINT('Ctrl Pts',(8.64146435503369,28.3900521903403,125.441704908605));
#119871=CARTESIAN_POINT('Ctrl Pts',(8.64789566207008,28.364987274512,125.337290756297));
#119872=CARTESIAN_POINT('Ctrl Pts',(8.65683244781597,28.3453429844221,125.197107740404));
#119873=CARTESIAN_POINT('Ctrl Pts',(8.65903946635646,28.3416235330142,125.162875457893));
#119874=CARTESIAN_POINT('Ctrl Pts',(8.66198687524166,28.3381580846026,125.118099256063));
#119875=CARTESIAN_POINT('Ctrl Pts',(8.66267992615894,28.3374476073891,125.107636025148));
#119876=CARTESIAN_POINT('Ctrl Pts',(8.6638104832514,28.3364574557726,125.090688064136));
#119877=CARTESIAN_POINT('Ctrl Pts',(8.66424470639012,28.3361168008911,125.084206992194));
#119878=CARTESIAN_POINT('Ctrl Pts',(8.66510137274591,28.3355224119753,125.071480283535));
#119879=CARTESIAN_POINT('Ctrl Pts',(8.66552366468333,28.3352659458463,125.065234931787));
#119880=CARTESIAN_POINT('Ctrl Pts',(8.66658338028155,28.3347130486683,125.049629352022));
#119881=CARTESIAN_POINT('Ctrl Pts',(8.66722313341433,28.3344603907533,125.040267885759));
#119882=CARTESIAN_POINT('Ctrl Pts',(8.66974027598701,28.3337809548505,125.003647822239));
#119883=CARTESIAN_POINT('Ctrl Pts',(8.67164580298702,28.3339443896708,124.976384108168));
#119884=CARTESIAN_POINT('Ctrl Pts',(8.67686456943339,28.3361968348608,124.902638029354));
#119885=CARTESIAN_POINT('Ctrl Pts',(8.68021839370413,28.3395641776208,124.856220077551));
#119886=CARTESIAN_POINT('Ctrl Pts',(8.68857530716182,28.3526988531599,124.741796847259));
#119887=CARTESIAN_POINT('Ctrl Pts',(8.6935938417762,28.3647380596105,124.67413385293));
#119888=CARTESIAN_POINT('Ctrl Pts',(8.70468506646875,28.4009513860754,124.524787742649));
#119889=CARTESIAN_POINT('Ctrl Pts',(8.71070451656663,28.4272814014683,124.443813539551));
#119890=CARTESIAN_POINT('Ctrl Pts',(8.71787095621603,28.4671793787881,124.347003861594));
#119891=CARTESIAN_POINT('Ctrl Pts',(8.71920665444058,28.4749972299187,124.328948867533));
#119892=CARTESIAN_POINT('Ctrl Pts',(8.72132899904051,28.4880305081195,124.3002539837));
#119893=CARTESIAN_POINT('Ctrl Pts',(8.72212248396117,28.493042596378,124.289524365015));
#119894=CARTESIAN_POINT('Ctrl Pts',(8.72362802353031,28.5028172631068,124.269168161197));
#119895=CARTESIAN_POINT('Ctrl Pts',(8.72434074025671,28.5075593332783,124.259532451903));
#119896=CARTESIAN_POINT('Ctrl Pts',(8.72597225366272,28.5186772664773,124.237481991774));
#119897=CARTESIAN_POINT('Ctrl Pts',(8.72688877820963,28.5251166713647,124.225100044994));
#119898=CARTESIAN_POINT('Ctrl Pts',(8.72978870234118,28.5461017498443,124.185958575804));
#119899=CARTESIAN_POINT('Ctrl Pts',(8.73175166987347,28.5612264160809,124.159515424189));
#119900=CARTESIAN_POINT('Ctrl Pts',(8.7363837636112,28.5990311677978,124.097433943471));
#119901=CARTESIAN_POINT('Ctrl Pts',(8.73903068500187,28.622358272983,124.062213883016));
#119902=CARTESIAN_POINT('Ctrl Pts',(8.74634785136885,28.6912063606978,123.966387282686));
#119903=CARTESIAN_POINT('Ctrl Pts',(8.7509438030195,28.7395586389947,123.907945064896));
#119904=CARTESIAN_POINT('Ctrl Pts',(8.75616757583938,28.7983265636739,123.846037699088));
#119905=CARTESIAN_POINT('Ctrl Pts',(8.75675531252979,28.8049915747812,123.839137001509));
#119906=CARTESIAN_POINT('Ctrl Pts',(8.76201973715487,28.8651212870059,123.777947621603));
#119907=CARTESIAN_POINT('Ctrl Pts',(8.76674784870889,28.922185654505,123.727335490899));
#119908=CARTESIAN_POINT('Ctrl Pts',(8.7725263572259,28.992235197421,123.673305934496));
#119909=CARTESIAN_POINT('Ctrl Pts',(8.77333543522115,29.0020490825062,123.665908179616));
#119910=CARTESIAN_POINT('Ctrl Pts',(8.77461353866993,29.0175421215255,123.654496054466));
#119911=CARTESIAN_POINT('Ctrl Pts',(8.77507767644332,29.0231663263354,123.650407350332));
#119912=CARTESIAN_POINT('Ctrl Pts',(8.77595051372792,29.03373504688,123.642824736743));
#119913=CARTESIAN_POINT('Ctrl Pts',(8.77635863664875,29.0386732246568,123.639322418366));
#119914=CARTESIAN_POINT('Ctrl Pts',(8.7773247879708,29.0503562823087,123.631131750977));
#119915=CARTESIAN_POINT('Ctrl Pts',(8.77788429933565,29.0571168669394,123.626466285797));
#119916=CARTESIAN_POINT('Ctrl Pts',(8.77976775712462,29.0798662433206,123.611014087461));
#119917=CARTESIAN_POINT('Ctrl Pts',(8.7811052277329,29.0960071449061,123.600455490474));
#119918=CARTESIAN_POINT('Ctrl Pts',(8.78443406955368,29.1362292528909,123.575130209165));
#119919=CARTESIAN_POINT('Ctrl Pts',(8.78643998781241,29.1605092661512,123.56069150209));
#119920=CARTESIAN_POINT('Ctrl Pts',(8.7956224088175,29.2722879488188,123.498010173361));
#119921=CARTESIAN_POINT('Ctrl Pts',(8.8029706490421,29.3636512883739,123.45708100833));
#119922=CARTESIAN_POINT('Ctrl Pts',(8.81615081259195,29.5364872015663,123.397633715322));
#119923=CARTESIAN_POINT('Ctrl Pts',(8.82201221639358,29.616752996857,123.376563123351));
#119924=CARTESIAN_POINT('Ctrl Pts',(8.82902677928226,29.717556485459,123.357999256891));
#119925=CARTESIAN_POINT('Ctrl Pts',(8.83035852964539,29.7369097947053,123.354787436159));
#119926=CARTESIAN_POINT('Ctrl Pts',(8.83247608388773,29.7680178738376,123.350187823001));
#119927=CARTESIAN_POINT('Ctrl Pts',(8.83326867365714,29.7797380415854,123.348582242919));
#119928=CARTESIAN_POINT('Ctrl Pts',(8.83477341781172,29.8021307638273,123.345757234603));
#119929=CARTESIAN_POINT('Ctrl Pts',(8.83548622473827,29.8127999031348,123.344515933498));
#119930=CARTESIAN_POINT('Ctrl Pts',(8.83711921226534,29.837378728107,123.341896964821));
#119931=CARTESIAN_POINT('Ctrl Pts',(8.838037104748,29.8512953619975,123.340590977576));
#119932=CARTESIAN_POINT('Ctrl Pts',(8.84094663978793,29.8957109544765,123.336986115787));
#119933=CARTESIAN_POINT('Ctrl Pts',(8.84291764829771,29.9262585166631,123.335351759133));
#119934=CARTESIAN_POINT('Ctrl Pts',(8.84757287809975,29.9992942154751,123.333458831552));
#119935=CARTESIAN_POINT('Ctrl Pts',(8.85023457369954,30.0417815520664,123.333982399425));
#119936=CARTESIAN_POINT('Ctrl Pts',(8.85743882329956,30.157833975101,123.339855556705));
#119937=CARTESIAN_POINT('Ctrl Pts',(8.86191367315608,30.2311362519815,123.348465096912));
#119938=CARTESIAN_POINT('Ctrl Pts',(8.86726246431578,30.317105092997,123.364399728107));
#119939=CARTESIAN_POINT('Ctrl Pts',(8.86810217116482,30.3305513612015,123.367064091462));
#119940=CARTESIAN_POINT('Ctrl Pts',(8.87347052154384,30.4160725063227,123.385109617529));
#119941=CARTESIAN_POINT('Ctrl Pts',(8.87805156770615,30.4870840567518,123.405091335915));
#119942=CARTESIAN_POINT('Ctrl Pts',(8.88366642188338,30.5681041855749,123.433805752786));
#119943=CARTESIAN_POINT('Ctrl Pts',(8.88447483126632,30.5796321475535,123.438035423761));
#119944=CARTESIAN_POINT('Ctrl Pts',(8.88575208412609,30.5976104425406,123.444858182544));
#119945=CARTESIAN_POINT('Ctrl Pts',(8.88621604948673,30.6040933575983,123.447364973871));
#119946=CARTESIAN_POINT('Ctrl Pts',(8.88708875721947,30.6161939017649,123.452131227286));
#119947=CARTESIAN_POINT('Ctrl Pts',(8.88749692517266,30.6218151443017,123.454380841298));
#119948=CARTESIAN_POINT('Ctrl Pts',(8.88846341295131,30.6350372780574,123.459756123671));
#119949=CARTESIAN_POINT('Ctrl Pts',(8.88902321885964,30.6426274407528,123.46290744963));
#119950=CARTESIAN_POINT('Ctrl Pts',(8.890908587557,30.6679729114838,123.473651060988));
#119951=CARTESIAN_POINT('Ctrl Pts',(8.89224770905777,30.6856187446232,123.481495554287));
#119952=CARTESIAN_POINT('Ctrl Pts',(8.89558153460426,30.7287721731277,123.501584984143));
#119953=CARTESIAN_POINT('Ctrl Pts',(8.89759083646413,30.754111341289,123.514176206856));
#119954=CARTESIAN_POINT('Ctrl Pts',(8.90680283125409,30.8677471659709,123.574298336104));
#119955=CARTESIAN_POINT('Ctrl Pts',(8.91417806222237,30.9519632063012,123.629096320781));
#119956=CARTESIAN_POINT('Ctrl Pts',(8.9273527113519,31.0955204788528,123.742148822495));
#119957=CARTESIAN_POINT('Ctrl Pts',(8.93318432209167,31.1564305675864,123.797907354295));
#119958=CARTESIAN_POINT('Ctrl Pts',(8.94017025098004,31.2264076446241,123.872230231214));
#119959=CARTESIAN_POINT('Ctrl Pts',(8.94150126510173,31.2395944550552,123.886740818072));
#119960=CARTESIAN_POINT('Ctrl Pts',(8.94361799687578,31.2603214122776,123.910373536095));
#119961=CARTESIAN_POINT('Ctrl Pts',(8.94441048911714,31.2680255156898,123.91934871622));
#119962=CARTESIAN_POINT('Ctrl Pts',(8.94591526328482,31.2825433366579,123.936630829599));
#119963=CARTESIAN_POINT('Ctrl Pts',(8.9466281955744,31.2893735277293,123.944923074759));
#119964=CARTESIAN_POINT('Ctrl Pts',(8.94826177652706,31.3049091038059,123.964160348231));
#119965=CARTESIAN_POINT('Ctrl Pts',(8.94918013285224,31.3135579213929,123.975150176724));
#119966=CARTESIAN_POINT('Ctrl Pts',(8.95209244659461,31.3406995704015,124.010546496219));
#119967=CARTESIAN_POINT('Ctrl Pts',(8.95406571722126,31.3586590105093,124.035355269509));
#119968=CARTESIAN_POINT('Ctrl Pts',(8.95872739653469,31.3999114568146,124.095780098686));
#119969=CARTESIAN_POINT('Ctrl Pts',(8.96139319518157,31.4225441609179,124.131821327306));
#119970=CARTESIAN_POINT('Ctrl Pts',(8.96859932375573,31.480544542999,124.232553388569));
#119971=CARTESIAN_POINT('Ctrl Pts',(8.97307224462647,31.5130386151843,124.298786083015));
#119972=CARTESIAN_POINT('Ctrl Pts',(8.97843617056716,31.5463542077416,124.379886952487));
#119973=CARTESIAN_POINT('Ctrl Pts',(8.97929283784044,31.5515044255601,124.392887540137));
#119974=CARTESIAN_POINT('Ctrl Pts',(8.98465590276752,31.5826347314577,124.474453279298));
#119975=CARTESIAN_POINT('Ctrl Pts',(8.98921483840908,31.6042252067548,124.544598179623));
#119976=CARTESIAN_POINT('Ctrl Pts',(8.99480516670045,31.6239550344586,124.627875252257));
#119977=CARTESIAN_POINT('Ctrl Pts',(8.9956135662341,31.6266535738346,124.63985432004));
#119978=CARTESIAN_POINT('Ctrl Pts',(8.99689085376639,31.6306719866406,124.658659707585));
#119979=CARTESIAN_POINT('Ctrl Pts',(8.99735486531452,31.6320820211966,124.665466601144));
#119980=CARTESIAN_POINT('Ctrl Pts',(8.99822776670442,31.6346408803267,124.678220756916));
#119981=CARTESIAN_POINT('Ctrl Pts',(8.99863608313842,31.63579992364,124.684165717449));
#119982=CARTESIAN_POINT('Ctrl Pts',(8.99960304953536,31.6384560849532,124.698196618246));
#119983=CARTESIAN_POINT('Ctrl Pts',(9.00016318771426,31.63992578075,124.706287470304));
#119984=CARTESIAN_POINT('Ctrl Pts',(9.00205015390863,31.6446491462258,124.733431445904));
#119985=CARTESIAN_POINT('Ctrl Pts',(9.00339056079286,31.6476309852622,124.752529466443));
#119986=CARTESIAN_POINT('Ctrl Pts',(9.00672818600977,31.6541620649319,124.799734374569));
#119987=CARTESIAN_POINT('Ctrl Pts',(9.00874003180645,31.6573278576865,124.827887685586));
#119988=CARTESIAN_POINT('Ctrl Pts',(9.01797562427636,31.6684601701077,124.956295872632));
#119989=CARTESIAN_POINT('Ctrl Pts',(9.02537239223562,31.6680567820779,125.057065415937));
#119990=CARTESIAN_POINT('Ctrl Pts',(9.03853426560753,31.6508295925412,125.2388418975));
#119991=CARTESIAN_POINT('Ctrl Pts',(9.04433413913181,31.6370701917772,125.31982590499));
#119992=CARTESIAN_POINT('Ctrl Pts',(9.05128943664876,31.6126993867303,125.418497945355));
#119993=CARTESIAN_POINT('Ctrl Pts',(9.05261952066453,31.6076662814296,125.437434596963));
#119994=CARTESIAN_POINT('Ctrl Pts',(9.05473523703392,31.5990611699335,125.467652901369));
#119995=CARTESIAN_POINT('Ctrl Pts',(9.05552762881655,31.5957011318969,125.478992454524));
#119996=CARTESIAN_POINT('Ctrl Pts',(9.05703250364877,31.5890581506228,125.500565344305));
#119997=CARTESIAN_POINT('Ctrl Pts',(9.05774563413572,31.5857963979551,125.510804525664));
#119998=CARTESIAN_POINT('Ctrl Pts',(9.05938008724483,31.57805922925,125.534304139384));
#119999=CARTESIAN_POINT('Ctrl Pts',(9.06029911156577,31.5735153001287,125.547541290166));
#120000=CARTESIAN_POINT('Ctrl Pts',(9.06155526888709,31.5670399249498,125.565658357052));
#120001=CARTESIAN_POINT('Ctrl Pts',(9.06189691910435,31.565251574817,125.570588300551));
#120002=CARTESIAN_POINT('Ctrl Pts',(9.06223782796602,31.5634400121624,125.575509624915));
#120003=CARTESIAN_POINT('',(8.82706654161307,31.6659995121743,124.999552917719));
#120004=CARTESIAN_POINT('Ctrl Pts',(8.86798214956472,31.5634398523358,125.575510059103));
#120005=CARTESIAN_POINT('Ctrl Pts',(8.86185959862923,31.5924943407706,125.496580170059));
#120006=CARTESIAN_POINT('Ctrl Pts',(8.85575033786931,31.6155593894588,125.41548247043));
#120007=CARTESIAN_POINT('Ctrl Pts',(8.84633162917246,31.6421958019909,125.284872744603));
#120008=CARTESIAN_POINT('Ctrl Pts',(8.84292407020463,31.6498680502033,125.236422911066));
#120009=CARTESIAN_POINT('Ctrl Pts',(8.83842236191684,31.6573105602946,125.170785025261));
#120010=CARTESIAN_POINT('Ctrl Pts',(8.83727032301696,31.6589692500531,125.153840446107));
#120011=CARTESIAN_POINT('Ctrl Pts',(8.83536837185457,31.6612948409996,125.125629325297));
#120012=CARTESIAN_POINT('Ctrl Pts',(8.83461395720211,31.6621074928471,125.114376436131));
#120013=CARTESIAN_POINT('Ctrl Pts',(8.83319042582845,31.6634313897574,125.093027807114));
#120014=CARTESIAN_POINT('Ctrl Pts',(8.83252063614475,31.6639651786523,125.082934029292));
#120015=CARTESIAN_POINT('Ctrl Pts',(8.83106750172905,31.6649279752969,125.060932692383));
#120016=CARTESIAN_POINT('Ctrl Pts',(8.83028530265433,31.6653211729731,125.04902406533));
#120017=CARTESIAN_POINT('Ctrl Pts',(8.82868898103002,31.6658655137231,125.02459404133));
#120018=CARTESIAN_POINT('Ctrl Pts',(8.827875314874,31.6660033093356,125.012073144697));
#120019=CARTESIAN_POINT('Ctrl Pts',(8.82706571805936,31.6659999396738,124.999551662012));
#120020=CARTESIAN_POINT('Ctrl Pts',(8.82706580233264,31.665999940024,124.99955296541));
#120021=CARTESIAN_POINT('Ctrl Pts',(8.82311191219987,31.6659835311962,124.938400860403));
#120022=CARTESIAN_POINT('Ctrl Pts',(8.81926106119894,31.6626002355637,124.877290397594));
#120023=CARTESIAN_POINT('Ctrl Pts',(8.80644804764151,31.6398369726596,124.671882810155));
#120024=CARTESIAN_POINT('Ctrl Pts',(8.79786135123866,31.604938388399,124.530012045354));
#120025=CARTESIAN_POINT('Ctrl Pts',(8.78706288842619,31.5437082326314,124.373062880477));
#120026=CARTESIAN_POINT('Ctrl Pts',(8.78556987258757,31.5349043321249,124.351807263532));
#120027=CARTESIAN_POINT('Ctrl Pts',(8.78347303192169,31.5221320866681,124.322691208441));
#120028=CARTESIAN_POINT('Ctrl Pts',(8.78288976210561,31.5185368793,124.314668674204));
#120029=CARTESIAN_POINT('Ctrl Pts',(8.78189262552663,31.5123229318677,124.301091524065));
#120030=CARTESIAN_POINT('Ctrl Pts',(8.78148069941551,31.5097366028299,124.295522110435));
#120031=CARTESIAN_POINT('Ctrl Pts',(8.78061676449524,31.5042736057273,124.283926323756));
#120032=CARTESIAN_POINT('Ctrl Pts',(8.78016444924453,31.5013914359647,124.277902816256));
#120033=CARTESIAN_POINT('Ctrl Pts',(8.77893744183874,31.4935117291653,124.261685978332));
#120034=CARTESIAN_POINT('Ctrl Pts',(8.77815879962782,31.4884461898224,124.251526351833));
#120035=CARTESIAN_POINT('Ctrl Pts',(8.77430621951915,31.463046613068,124.201861714845));
#120036=CARTESIAN_POINT('Ctrl Pts',(8.77115739764556,31.4412432644848,124.163132492397));
#120037=CARTESIAN_POINT('Ctrl Pts',(8.76163131245482,31.3715888915748,124.050217019742));
#120038=CARTESIAN_POINT('Ctrl Pts',(8.75515555536039,31.3193632980177,123.978910242169));
#120039=CARTESIAN_POINT('Ctrl Pts',(8.74273248152964,31.2071932368506,123.848819424931));
#120040=CARTESIAN_POINT('Ctrl Pts',(8.73679255303544,31.1479647878587,123.789746834459));
#120041=CARTESIAN_POINT('Ctrl Pts',(8.72987429344803,31.0716779565566,123.724323810785));
#120042=CARTESIAN_POINT('Ctrl Pts',(8.72871509926703,31.0586415470875,123.713484748001));
#120043=CARTESIAN_POINT('Ctrl Pts',(8.72653656167878,31.033662639708,123.693352989191));
#120044=CARTESIAN_POINT('Ctrl Pts',(8.72551569827136,31.0217546541001,123.684020396574));
#120045=CARTESIAN_POINT('Ctrl Pts',(8.72376930046346,31.0010382537288,123.668235166541));
#120046=CARTESIAN_POINT('Ctrl Pts',(8.72304073351015,30.9922906720167,123.661704670461));
#120047=CARTESIAN_POINT('Ctrl Pts',(8.72164934351712,30.975385905112,123.649341317512));
#120048=CARTESIAN_POINT('Ctrl Pts',(8.72098602904161,30.9672390377362,123.643495229719));
#120049=CARTESIAN_POINT('Ctrl Pts',(8.71925027353451,30.9456930492278,123.628326906264));
#120050=CARTESIAN_POINT('Ctrl Pts',(8.71818251493026,30.9322086308161,123.61912726183));
#120051=CARTESIAN_POINT('Ctrl Pts',(8.7143270631873,30.882710583457,123.586413157544));
#120052=CARTESIAN_POINT('Ctrl Pts',(8.71158331086487,30.8459235203386,123.564096237216));
#120053=CARTESIAN_POINT('Ctrl Pts',(8.70165305561416,30.707874526144,123.487497799325));
#120054=CARTESIAN_POINT('Ctrl Pts',(8.69475101905403,30.6019460250435,123.442305901425));
#120055=CARTESIAN_POINT('Ctrl Pts',(8.68471319411838,30.4460009885597,123.394080178988));
#120056=CARTESIAN_POINT('Ctrl Pts',(8.68171136033691,30.3991959169987,123.381810478194));
#120057=CARTESIAN_POINT('Ctrl Pts',(8.67742310757907,30.3333560991082,123.367581334883));
#120058=CARTESIAN_POINT('Ctrl Pts',(8.67620196428344,30.3147187069327,123.363885988645));
#120059=CARTESIAN_POINT('Ctrl Pts',(8.67403298271044,30.2819076000493,123.357961679316));
#120060=CARTESIAN_POINT('Ctrl Pts',(8.6730915748514,30.2677604039843,123.355595526105));
#120061=CARTESIAN_POINT('Ctrl Pts',(8.67165599586849,30.2463637083167,123.352300298216));
#120062=CARTESIAN_POINT('Ctrl Pts',(8.6711690009513,30.2391353382487,123.351235714542));
#120063=CARTESIAN_POINT('Ctrl Pts',(8.67027678372557,30.2259525935307,123.349382691082));
#120064=CARTESIAN_POINT('Ctrl Pts',(8.66987241930273,30.2200006508454,123.348578858952));
#120065=CARTESIAN_POINT('Ctrl Pts',(8.66894565782454,30.2064107093069,123.346818258179));
#120066=CARTESIAN_POINT('Ctrl Pts',(8.66842215671462,30.1987703711942,123.345882233315));
#120067=CARTESIAN_POINT('Ctrl Pts',(8.66677726855011,30.1748680301569,123.34312192567));
#120068=CARTESIAN_POINT('Ctrl Pts',(8.66564646899085,30.1585860166767,123.341484336362));
#120069=CARTESIAN_POINT('Ctrl Pts',(8.6591084614552,30.0651567378163,123.333475828782));
#120070=CARTESIAN_POINT('Ctrl Pts',(8.65349839423687,29.9876703296727,123.332248847061));
#120071=CARTESIAN_POINT('Ctrl Pts',(8.6475393364023,29.9058929549144,123.336653936853));
#120072=CARTESIAN_POINT('Ctrl Pts',(8.64721173805971,29.9013991726717,123.336914272052));
#120073=CARTESIAN_POINT('Ctrl Pts',(8.64035413409775,29.8073644820645,123.342744391764));
#120074=CARTESIAN_POINT('Ctrl Pts',(8.63383225169681,29.7184085455744,123.355520200013));
#120075=CARTESIAN_POINT('Ctrl Pts',(8.62398292990317,29.5824669872475,123.386404693268));
#120076=CARTESIAN_POINT('Ctrl Pts',(8.62053144395442,29.534538749924,123.399571827955));
#120077=CARTESIAN_POINT('Ctrl Pts',(8.61601355290141,29.4714194077108,123.419988622866));
#120078=CARTESIAN_POINT('Ctrl Pts',(8.61488705457271,29.4556499168614,123.425351970631));
#120079=CARTESIAN_POINT('Ctrl Pts',(8.6130156103648,29.4294084817164,123.434718265363));
#120080=CARTESIAN_POINT('Ctrl Pts',(8.61226646048581,29.4188920324227,123.438591939901));
#120081=CARTESIAN_POINT('Ctrl Pts',(8.61079521016866,29.3982198087819,123.446444224937));
#120082=CARTESIAN_POINT('Ctrl Pts',(8.61007296001439,29.3880624469165,123.45041702852));
#120083=CARTESIAN_POINT('Ctrl Pts',(8.60832045953376,29.3633998946243,123.460343503968));
#120084=CARTESIAN_POINT('Ctrl Pts',(8.60729380984965,29.3489381422298,123.466402821849));
#120085=CARTESIAN_POINT('Ctrl Pts',(8.6037616198176,29.2991657970233,123.488087873988));
#120086=CARTESIAN_POINT('Ctrl Pts',(8.6012906372966,29.2643128725904,123.504736923961));
#120087=CARTESIAN_POINT('Ctrl Pts',(8.59133451022103,29.1245037321512,123.57759622948));
#120088=CARTESIAN_POINT('Ctrl Pts',(8.58418159188789,29.0251415541858,123.643763196199));
#120089=CARTESIAN_POINT('Ctrl Pts',(8.5738225311856,28.8956234625868,123.75165653871));
#120090=CARTESIAN_POINT('Ctrl Pts',(8.57075175376744,28.8590051762603,123.785035363904));
#120091=CARTESIAN_POINT('Ctrl Pts',(8.56579469825905,28.8038237119711,123.840032686575));
#120092=CARTESIAN_POINT('Ctrl Pts',(8.56396288707236,28.7842337097326,123.860581735628));
#120093=CARTESIAN_POINT('Ctrl Pts',(8.56146979561538,28.7588021093787,123.888661144796));
#120094=CARTESIAN_POINT('Ctrl Pts',(8.56084060681494,28.7524851554267,123.89575683983));
#120095=CARTESIAN_POINT('Ctrl Pts',(8.55978840419957,28.7420961062591,123.907629554276));
#120096=CARTESIAN_POINT('Ctrl Pts',(8.55936787112815,28.737989585219,123.912376394481));
#120097=CARTESIAN_POINT('Ctrl Pts',(8.55851107498217,28.7297177188876,123.922047993255));
#120098=CARTESIAN_POINT('Ctrl Pts',(8.55807472113558,28.7255539862377,123.926973925302));
#120099=CARTESIAN_POINT('Ctrl Pts',(8.5569357083593,28.7148094489037,123.939836079498));
#120100=CARTESIAN_POINT('Ctrl Pts',(8.55622998620274,28.708273641222,123.947809289384));
#120101=CARTESIAN_POINT('Ctrl Pts',(8.55326073039812,28.6812619414789,123.981392583222));
#120102=CARTESIAN_POINT('Ctrl Pts',(8.55095666864024,28.6614717498443,124.007541978785));
#120103=CARTESIAN_POINT('Ctrl Pts',(8.54174628197452,28.5864429952765,124.113008823578));
#120104=CARTESIAN_POINT('Ctrl Pts',(8.53464624056418,28.5373793468705,124.196484719431));
#120105=CARTESIAN_POINT('Ctrl Pts',(8.52068717676047,28.4545344817127,124.370461919366));
#120106=CARTESIAN_POINT('Ctrl Pts',(8.51385425221636,28.4208105372209,124.460603908105));
#120107=CARTESIAN_POINT('Ctrl Pts',(8.50592953605485,28.3897566002235,124.572144459933));
#120108=CARTESIAN_POINT('Ctrl Pts',(8.50459179682329,28.3848092618782,124.591217530965));
#120109=CARTESIAN_POINT('Ctrl Pts',(8.50246718043537,28.3774309196519,124.621891685846));
#120110=CARTESIAN_POINT('Ctrl Pts',(8.5016734348206,28.3747834602172,124.633438232905));
#120111=CARTESIAN_POINT('Ctrl Pts',(8.50016799988828,28.3699722979114,124.655499066481));
#120112=CARTESIAN_POINT('Ctrl Pts',(8.49945564260801,28.3677866298647,124.666007894823));
#120113=CARTESIAN_POINT('Ctrl Pts',(8.4978411199076,28.3630420606848,124.689979862989));
#120114=CARTESIAN_POINT('Ctrl Pts',(8.4969410333358,28.3605473831199,124.703455035379));
#120115=CARTESIAN_POINT('Ctrl Pts',(8.49409439533492,28.3531425097773,124.746407162936));
#120116=CARTESIAN_POINT('Ctrl Pts',(8.49216750629334,28.3488587813619,124.77598711571));
#120117=CARTESIAN_POINT('Ctrl Pts',(8.48120701128608,28.3288096242296,124.946694203732));
#120118=CARTESIAN_POINT('Ctrl Pts',(8.47273828431608,28.3303433339884,125.08925242879));
#120119=CARTESIAN_POINT('Ctrl Pts',(8.4613123919638,28.3558905109907,125.272618818602));
#120120=CARTESIAN_POINT('Ctrl Pts',(8.4586222083635,28.3635003107159,125.315095700026));
#120121=CARTESIAN_POINT('Ctrl Pts',(8.45421341975417,28.3783099999797,125.382557350146));
#120122=CARTESIAN_POINT('Ctrl Pts',(8.4525357093555,28.3844612129153,125.407753397292));
#120123=CARTESIAN_POINT('Ctrl Pts',(8.45022211731647,28.3935859313128,125.441672241644));
#120124=CARTESIAN_POINT('Ctrl Pts',(8.44961276298937,28.3960477285878,125.450530388016));
#120125=CARTESIAN_POINT('Ctrl Pts',(8.44858453916677,28.4002963728728,125.465341739297));
#120126=CARTESIAN_POINT('Ctrl Pts',(8.44816791347502,28.4020434962221,125.47130631162));
#120127=CARTESIAN_POINT('Ctrl Pts',(8.44736324161128,28.4054659130842,125.482752419264));
#120128=CARTESIAN_POINT('Ctrl Pts',(8.44697551883245,28.4071361834842,125.488235304096));
#120129=CARTESIAN_POINT('Ctrl Pts',(8.4459134477172,28.4117699900738,125.503169500219));
#120130=CARTESIAN_POINT('Ctrl Pts',(8.44523599256275,28.4147895183836,125.512602991908));
#120131=CARTESIAN_POINT('Ctrl Pts',(8.44253625675836,28.4270803566041,125.549854138065));
#120132=CARTESIAN_POINT('Ctrl Pts',(8.44048175119273,28.4370007090071,125.577450209979));
#120133=CARTESIAN_POINT('Ctrl Pts',(8.43058845761243,28.4876378018054,125.707428689183));
#120134=CARTESIAN_POINT('Ctrl Pts',(8.42246820876931,28.5377160101224,125.805865894639));
#120135=CARTESIAN_POINT('Ctrl Pts',(8.41030548490949,28.6285524042213,125.947669838855));
#120136=CARTESIAN_POINT('Ctrl Pts',(8.40614900568784,28.6625124924165,125.995025092727));
#120137=CARTESIAN_POINT('Ctrl Pts',(8.4002581521145,28.7151123243326,126.060799068439));
#120138=CARTESIAN_POINT('Ctrl Pts',(8.39845783866359,28.7318119003453,126.080708135181));
#120139=CARTESIAN_POINT('Ctrl Pts',(8.39522817505633,28.7629090461731,126.116067833763));
#120140=CARTESIAN_POINT('Ctrl Pts',(8.39379290784193,28.7771473837845,126.13165055896));
#120141=CARTESIAN_POINT('Ctrl Pts',(8.39155153739882,28.8000380962516,126.155765923685));
#120142=CARTESIAN_POINT('Ctrl Pts',(8.39073717819677,28.8084938418462,126.164481227588));
#120143=CARTESIAN_POINT('Ctrl Pts',(8.38921444443899,28.8245634863263,126.180685831148));
#120144=CARTESIAN_POINT('Ctrl Pts',(8.38850516916867,28.8321555301534,126.188195831027));
#120145=CARTESIAN_POINT('Ctrl Pts',(8.38691145295182,28.8494532312489,126.204980635389));
#120146=CARTESIAN_POINT('Ctrl Pts',(8.38602891180433,28.8591999109625,126.214212243859));
#120147=CARTESIAN_POINT('Ctrl Pts',(8.38375575684629,28.8847306489732,126.237814961218));
#120148=CARTESIAN_POINT('Ctrl Pts',(8.38237283288687,28.9006815022897,126.25200259995));
#120149=CARTESIAN_POINT('Ctrl Pts',(8.37298877237357,29.0116577515645,126.34695489566));
#120150=CARTESIAN_POINT('Ctrl Pts',(8.36543506173788,29.1152179281998,126.417135241382));
#120151=CARTESIAN_POINT('Ctrl Pts',(8.35251044376639,29.30236585554,126.515377811488));
#120152=CARTESIAN_POINT('Ctrl Pts',(8.34718468790678,29.3820978145835,126.54959874999));
#120153=CARTESIAN_POINT('Ctrl Pts',(8.34061835408789,29.4776645857624,126.582063983745));
#120154=CARTESIAN_POINT('Ctrl Pts',(8.33967920348933,29.4912708609437,126.586491526321));
#120155=CARTESIAN_POINT('Ctrl Pts',(8.33824637861165,29.5119015835442,126.592912181252));
#120156=CARTESIAN_POINT('Ctrl Pts',(8.33775983924086,29.518885275295,126.595035390825));
#120157=CARTESIAN_POINT('Ctrl Pts',(8.33686804492697,29.5316408330934,126.598821994754));
#120158=CARTESIAN_POINT('Ctrl Pts',(8.33646364246367,29.537408038012,126.600500157221));
#120159=CARTESIAN_POINT('Ctrl Pts',(8.33553625818704,29.5505948952862,126.604260089533));
#120160=CARTESIAN_POINT('Ctrl Pts',(8.33501216603918,29.5580199711224,126.606321583988));
#120161=CARTESIAN_POINT('Ctrl Pts',(8.33336353085078,29.581300465874,126.612611538694));
#120162=CARTESIAN_POINT('Ctrl Pts',(8.33222951640808,29.597203680645,126.616657152698));
#120163=CARTESIAN_POINT('Ctrl Pts',(8.32533956440547,29.6933153841576,126.639600868683));
#120164=CARTESIAN_POINT('Ctrl Pts',(8.31935390558644,29.77476926883,126.652759826452));
#120165=CARTESIAN_POINT('Ctrl Pts',(8.3079945711629,29.9302519368262,126.666168843073));
#120166=CARTESIAN_POINT('Ctrl Pts',(8.30263490766846,30.0039942237203,126.667623701327));
#120167=CARTESIAN_POINT('Ctrl Pts',(8.29440884702313,30.1192327446014,126.662250604774));
#120168=CARTESIAN_POINT('Ctrl Pts',(8.29147213707223,30.1607861631104,126.658747059286));
#120169=CARTESIAN_POINT('Ctrl Pts',(8.2864872507338,30.2321122535858,126.650027272425));
#120170=CARTESIAN_POINT('Ctrl Pts',(8.28441859296429,30.2619537407256,126.645553566569));
#120171=CARTESIAN_POINT('Ctrl Pts',(8.28143361873136,30.3053464331246,126.637837850405));
#120172=CARTESIAN_POINT('Ctrl Pts',(8.28049751542141,30.319003189854,126.63523278271));
#120173=CARTESIAN_POINT('Ctrl Pts',(8.27884859269855,30.343139254354,126.630314867491));
#120174=CARTESIAN_POINT('Ctrl Pts',(8.27813362077775,30.353631669446,126.628071179851));
#120175=CARTESIAN_POINT('Ctrl Pts',(8.27663494226303,30.3756776942224,126.623133694604));
#120176=CARTESIAN_POINT('Ctrl Pts',(8.27585199441556,30.3872257202403,126.620417530863));
#120177=CARTESIAN_POINT('Ctrl Pts',(8.27377374505151,30.4179510307577,126.612843533235));
#120178=CARTESIAN_POINT('Ctrl Pts',(8.27248549712261,30.4370728304289,126.607766998581));
#120179=CARTESIAN_POINT('Ctrl Pts',(8.26533958107234,30.5434519017089,126.577486782053));
#120180=CARTESIAN_POINT('Ctrl Pts',(8.25970827242814,30.628629315451,126.545520215033));
#120181=CARTESIAN_POINT('Ctrl Pts',(8.24843537639549,30.7950507561807,126.467014348336));
#120182=CARTESIAN_POINT('Ctrl Pts',(8.24281535967413,30.8758276975229,126.420267759495));
#120183=CARTESIAN_POINT('Ctrl Pts',(8.23441970976056,30.9855704936985,126.34382066184));
#120184=CARTESIAN_POINT('Ctrl Pts',(8.2318302798772,31.0180106046631,126.319415394432));
#120185=CARTESIAN_POINT('Ctrl Pts',(8.22846714159822,31.0578298363242,126.287115537185));
#120186=CARTESIAN_POINT('Ctrl Pts',(8.22776072110762,31.0660699602434,126.280298868931));
#120187=CARTESIAN_POINT('Ctrl Pts',(8.22661379723479,31.0792378430255,126.26919043917));
#120188=CARTESIAN_POINT('Ctrl Pts',(8.22617675503122,31.0842071287889,126.264948058576));
#120189=CARTESIAN_POINT('Ctrl Pts',(8.22532448910126,31.0938007790999,126.256659703285));
#120190=CARTESIAN_POINT('Ctrl Pts',(8.22490951030006,31.0984279225647,126.252617199508));
#120191=CARTESIAN_POINT('Ctrl Pts',(8.22397248119027,31.1087795539742,126.243472037631));
#120192=CARTESIAN_POINT('Ctrl Pts',(8.22344942181113,31.1144913775475,126.238355268635));
#120193=CARTESIAN_POINT('Ctrl Pts',(8.22159076799756,31.1345608133872,126.220125344995));
#120194=CARTESIAN_POINT('Ctrl Pts',(8.22024110880068,31.1487233501495,126.206801011429));
#120195=CARTESIAN_POINT('Ctrl Pts',(8.21133002619227,31.2397729788634,126.118085089767));
#120196=CARTESIAN_POINT('Ctrl Pts',(8.20341418999369,31.3094250999261,126.035642196394));
#120197=CARTESIAN_POINT('Ctrl Pts',(8.18941167158819,31.4191244138898,125.876880158043));
#120198=CARTESIAN_POINT('Ctrl Pts',(8.18330322973614,31.4621608940694,125.803070376775));
#120199=CARTESIAN_POINT('Ctrl Pts',(8.17530622432523,31.5124256970906,125.69930183296));
#120200=CARTESIAN_POINT('Ctrl Pts',(8.17325105760495,31.5247635719941,125.671975292116));
#120201=CARTESIAN_POINT('Ctrl Pts',(8.17028162465115,31.5417216024768,125.63154004478));
#120202=CARTESIAN_POINT('Ctrl Pts',(8.16934786288843,31.5469254065904,125.618684195971));
#120203=CARTESIAN_POINT('Ctrl Pts',(8.16770156858408,31.5558678834473,125.595773577493));
#120204=CARTESIAN_POINT('Ctrl Pts',(8.16698690732518,31.5596710596102,125.585745014012));
#120205=CARTESIAN_POINT('Ctrl Pts',(8.1662714349765,31.5633981439605,125.57562335527));
#120206=CARTESIAN_POINT('Ctrl Pts',(8.16626741557826,31.563419079503,125.575566490962));
#120207=CARTESIAN_POINT('Ctrl Pts',(8.1662633962835,31.5634400119422,125.575509625513));
#120208=CARTESIAN_POINT('Origin',(5.,30.,125.));
#120209=CARTESIAN_POINT('',(7.46828911258472,31.5634400017109,125.575509653308));
#120210=CARTESIAN_POINT('',(7.65924497815242,31.5634400119497,125.575509625493));
#120211=CARTESIAN_POINT('',(5.,31.5634400119422,125.575509625513));
#120212=CARTESIAN_POINT('Ctrl Pts',(7.65924497815242,31.5634400119496,125.575509625493));
#120213=CARTESIAN_POINT('Ctrl Pts',(7.66017729015006,31.5584735537155,125.58900159709));
#120214=CARTESIAN_POINT('Ctrl Pts',(7.66111773020847,31.5533327778235,125.602428385792));
#120215=CARTESIAN_POINT('Ctrl Pts',(7.66261080835764,31.5449808147374,125.623424291053));
#120216=CARTESIAN_POINT('Ctrl Pts',(7.66315702419078,31.5418862215632,125.631039172576));
#120217=CARTESIAN_POINT('Ctrl Pts',(7.66411143038786,31.5364143463579,125.644223269884));
#120218=CARTESIAN_POINT('Ctrl Pts',(7.66451808945713,31.5340628459776,125.649802930435));
#120219=CARTESIAN_POINT('Ctrl Pts',(7.66539562430481,31.5289466590125,125.661760096817));
#120220=CARTESIAN_POINT('Ctrl Pts',(7.66586702566179,31.5261725065432,125.66813306138));
#120221=CARTESIAN_POINT('Ctrl Pts',(7.66717739120733,31.5183879447439,125.685714802585));
#120222=CARTESIAN_POINT('Ctrl Pts',(7.66802110248971,31.5132934994877,125.696885574195));
#120223=CARTESIAN_POINT('Ctrl Pts',(7.6739281957247,31.4770288850266,125.774131212128));
#120224=CARTESIAN_POINT('Ctrl Pts',(7.67919300440629,31.4416683139265,125.838142928507));
#120225=CARTESIAN_POINT('Ctrl Pts',(7.68553260137612,31.3945459696026,125.911591934296));
#120226=CARTESIAN_POINT('Ctrl Pts',(7.68656738638667,31.3867123306757,125.923464793082));
#120227=CARTESIAN_POINT('Ctrl Pts',(7.69296548856018,31.337364382259,125.996213697452));
#120228=CARTESIAN_POINT('Ctrl Pts',(7.69832878806617,31.2919986891319,126.054384141325));
#120229=CARTESIAN_POINT('Ctrl Pts',(7.70662546771097,31.2145866562511,126.141116477023));
#120230=CARTESIAN_POINT('Ctrl Pts',(7.70962646036876,31.1850367874528,126.171774669521));
#120231=CARTESIAN_POINT('Ctrl Pts',(7.71470711035421,31.1322561156653,126.222493505136));
#120232=CARTESIAN_POINT('Ctrl Pts',(7.7168083321998,31.1095870509708,126.243105414682));
#120233=CARTESIAN_POINT('Ctrl Pts',(7.71983094073532,31.0757577996573,126.27220154002));
#120234=CARTESIAN_POINT('Ctrl Pts',(7.72077282352162,31.0650397620834,126.281187702036));
#120235=CARTESIAN_POINT('Ctrl Pts',(7.72242843726573,31.0458912994405,126.296835683684));
#120236=CARTESIAN_POINT('Ctrl Pts',(7.72314437787457,31.0375073376343,126.303552812267));
#120237=CARTESIAN_POINT('Ctrl Pts',(7.72464168182622,31.0197584625874,126.317493276704));
#120238=CARTESIAN_POINT('Ctrl Pts',(7.72542231876526,31.0103803947095,126.32469895686));
#120239=CARTESIAN_POINT('Ctrl Pts',(7.72748645123638,30.9852585790615,126.343579420491));
#120240=CARTESIAN_POINT('Ctrl Pts',(7.72876306950882,30.9693838961959,126.355077503749));
#120241=CARTESIAN_POINT('Ctrl Pts',(7.73534829110199,30.8858172584015,126.413384802853));
#120242=CARTESIAN_POINT('Ctrl Pts',(7.74047489869333,30.8149242760387,126.455413931142));
#120243=CARTESIAN_POINT('Ctrl Pts',(7.75169815211647,30.6512876792323,126.536704684808));
#120244=CARTESIAN_POINT('Ctrl Pts',(7.75773485436627,30.5575201688452,126.573151563584));
#120245=CARTESIAN_POINT('Ctrl Pts',(7.76580292719123,30.4338471508407,126.608767836171));
#120246=CARTESIAN_POINT('Ctrl Pts',(7.76759740637812,30.4064517008403,126.615906598519));
#120247=CARTESIAN_POINT('Ctrl Pts',(7.77066742696375,30.3600776052865,126.626737010258));
#120248=CARTESIAN_POINT('Ctrl Pts',(7.77192660920649,30.3411918761311,126.630802626916));
#120249=CARTESIAN_POINT('Ctrl Pts',(7.77374607910833,30.3141761986648,126.636128625957));
#120250=CARTESIAN_POINT('Ctrl Pts',(7.77429229454883,30.3061002147552,126.637658760548));
#120251=CARTESIAN_POINT('Ctrl Pts',(7.77524670028917,30.2920559386583,126.640212179517));
#120252=CARTESIAN_POINT('Ctrl Pts',(7.77565335929858,30.2860928543941,126.641262788972));
#120253=CARTESIAN_POINT('Ctrl Pts',(7.77653089424722,30.2732722807136,126.643449595354));
#120254=CARTESIAN_POINT('Ctrl Pts',(7.77700229576726,30.2664134726515,126.644575376521));
#120255=CARTESIAN_POINT('Ctrl Pts',(7.77831266241106,30.2474202036857,126.647570934548));
#120256=CARTESIAN_POINT('Ctrl Pts',(7.77915637464264,30.2352720943578,126.649349496335));
#120257=CARTESIAN_POINT('Ctrl Pts',(7.78506373574391,30.1507022124981,126.66077778977));
#120258=CARTESIAN_POINT('Ctrl Pts',(7.79032883252951,30.077741003739,126.665787499988));
#120259=CARTESIAN_POINT('Ctrl Pts',(7.79666852811906,29.9904745394112,126.666033465635));
#120260=CARTESIAN_POINT('Ctrl Pts',(7.79770312672476,29.9762535160704,126.665891456134));
#120261=CARTESIAN_POINT('Ctrl Pts',(7.80410107461282,29.8883715695728,126.663888331602));
#120262=CARTESIAN_POINT('Ctrl Pts',(7.80946440379635,29.8148949028771,126.65732395683));
#120263=CARTESIAN_POINT('Ctrl Pts',(7.81776103740661,29.7000423700989,126.639326964603));
#120264=CARTESIAN_POINT('Ctrl Pts',(7.8207619586742,29.6582592767303,126.631128829586));
#120265=CARTESIAN_POINT('Ctrl Pts',(7.82584250257533,29.5870233032342,126.614293807885));
#120266=CARTESIAN_POINT('Ctrl Pts',(7.82794368850995,29.5574119551091,126.606427803198));
#120267=CARTESIAN_POINT('Ctrl Pts',(7.83096625567725,29.5146198444375,126.593787220432));
#120268=CARTESIAN_POINT('Ctrl Pts',(7.83190813222009,29.5012571874778,126.58965632358));
#120269=CARTESIAN_POINT('Ctrl Pts',(7.83356373882031,29.4777252986039,126.58205579444));
#120270=CARTESIAN_POINT('Ctrl Pts',(7.83427967846663,29.4675347998188,126.578655193615));
#120271=CARTESIAN_POINT('Ctrl Pts',(7.83577698413783,29.4461964307767,126.571304382951));
#120272=CARTESIAN_POINT('Ctrl Pts',(7.83655762372302,29.4350562596176,126.567333544434));
#120273=CARTESIAN_POINT('Ctrl Pts',(7.83862177191416,29.4055685634763,126.556467603902));
#120274=CARTESIAN_POINT('Ctrl Pts',(7.83989840306588,29.3872984798224,126.549366655922));
#120275=CARTESIAN_POINT('Ctrl Pts',(7.84648406016985,29.2929821945624,126.510779838452));
#120276=CARTESIAN_POINT('Ctrl Pts',(7.85161105833248,29.2192162249487,126.474011216018));
#120277=CARTESIAN_POINT('Ctrl Pts',(7.86283433713142,29.0621701508971,126.380619771661));
#120278=CARTESIAN_POINT('Ctrl Pts',(7.8688707098774,28.9806985101051,126.32161185825));
#120279=CARTESIAN_POINT('Ctrl Pts',(7.87693838655805,28.8837049712049,126.237029776872));
#120280=CARTESIAN_POINT('Ctrl Pts',(7.87873282171588,28.862849639222,126.217885929157));
#120281=CARTESIAN_POINT('Ctrl Pts',(7.88180277455025,28.8285997012969,126.184799775797));
#120282=CARTESIAN_POINT('Ctrl Pts',(7.88306193400523,28.8149413199946,126.171138341701));
#120283=CARTESIAN_POINT('Ctrl Pts',(7.88488137662834,28.7958146793757,126.151330220693));
#120284=CARTESIAN_POINT('Ctrl Pts',(7.88542758814761,28.7901490660582,126.14537516741));
#120285=CARTESIAN_POINT('Ctrl Pts',(7.88638198941899,28.7803867654472,126.134960890579));
#120286=CARTESIAN_POINT('Ctrl Pts',(7.88678864792402,28.7762699463427,126.130520862025));
#120287=CARTESIAN_POINT('Ctrl Pts',(7.88766618462007,28.7674792814555,126.120935765638));
#120288=CARTESIAN_POINT('Ctrl Pts',(7.8881375884195,28.7628134715875,126.115783940482));
#120289=CARTESIAN_POINT('Ctrl Pts',(7.88944796753677,28.74999538904,126.10145141416));
#120290=CARTESIAN_POINT('Ctrl Pts',(7.89029169010397,28.7419123498506,126.092209772709));
#120291=CARTESIAN_POINT('Ctrl Pts',(7.8962017589591,28.6864178995672,126.027327494601));
#120292=CARTESIAN_POINT('Ctrl Pts',(7.90146976693902,28.6426161805956,125.968713845724));
#120293=CARTESIAN_POINT('Ctrl Pts',(7.90781043800223,28.595077571397,125.895516871823));
#120294=CARTESIAN_POINT('Ctrl Pts',(7.90884313218526,28.5874984690762,125.883513961057));
#120295=CARTESIAN_POINT('Ctrl Pts',(7.91523948632845,28.5415306055414,125.808611735073));
#120296=CARTESIAN_POINT('Ctrl Pts',(7.92060310201217,28.5071943045998,125.743315799317));
#120297=CARTESIAN_POINT('Ctrl Pts',(7.92889927250416,28.4600279591175,125.637065747959));
#120298=CARTESIAN_POINT('Ctrl Pts',(7.93189948654414,28.4442583857804,125.59752421494));
#120299=CARTESIAN_POINT('Ctrl Pts',(7.93697898019848,28.4197722488643,125.528558601444));
#120300=CARTESIAN_POINT('Ctrl Pts',(7.93907981101,28.4103225133051,125.499419305726));
#120301=CARTESIAN_POINT('Ctrl Pts',(7.9421019700887,28.3977353790991,125.456617629355));
#120302=CARTESIAN_POINT('Ctrl Pts',(7.94304378584589,28.3939587872263,125.443151462155));
#120303=CARTESIAN_POINT('Ctrl Pts',(7.94469932392174,28.3875817959398,125.419259982886));
#120304=CARTESIAN_POINT('Ctrl Pts',(7.9454152552096,28.3849118850133,125.408854238275));
#120305=CARTESIAN_POINT('Ctrl Pts',(7.94691258078027,28.3795144366944,125.386939797216));
#120306=CARTESIAN_POINT('Ctrl Pts',(7.94769324826333,28.3768084172636,125.375426378172));
#120307=CARTESIAN_POINT('Ctrl Pts',(7.94975755769356,28.3699438593298,125.344756717018));
#120308=CARTESIAN_POINT('Ctrl Pts',(7.95103432022259,28.3660003246257,125.32555388056));
#120309=CARTESIAN_POINT('Ctrl Pts',(7.95762439611037,28.3472531151046,125.225318895443));
#120310=CARTESIAN_POINT('Ctrl Pts',(7.96275535660239,28.3381341228507,125.143335800659));
#120311=CARTESIAN_POINT('Ctrl Pts',(7.97397889053894,28.3314430746386,124.960733044532));
#120312=CARTESIAN_POINT('Ctrl Pts',(7.9800119179566,28.3368352743163,124.860340216216));
#120313=CARTESIAN_POINT('Ctrl Pts',(7.98807557233017,28.3552840326611,124.733042638468));
#120314=CARTESIAN_POINT('Ctrl Pts',(7.9898695608054,28.3600556409009,124.70514551971));
#120315=CARTESIAN_POINT('Ctrl Pts',(7.99293882661262,28.3692751412895,124.658436735692));
#120316=CARTESIAN_POINT('Ctrl Pts',(7.99419775525374,28.3733442420051,124.639555836097));
#120317=CARTESIAN_POINT('Ctrl Pts',(7.99601692213102,28.3796114167166,124.61274763689));
#120318=CARTESIAN_POINT('Ctrl Pts',(7.99656309452805,28.3815415677023,124.604758492202));
#120319=CARTESIAN_POINT('Ctrl Pts',(7.9975174518509,28.384996194286,124.590909091179));
#120320=CARTESIAN_POINT('Ctrl Pts',(7.99792410597136,28.3864936324497,124.585042333868));
#120321=CARTESIAN_POINT('Ctrl Pts',(7.99880166242837,28.3897788385109,124.57245803915));
#120322=CARTESIAN_POINT('Ctrl Pts',(7.99927309065674,28.3915766469335,124.565743589457));
#120323=CARTESIAN_POINT('Ctrl Pts',(8.00058360118448,28.3966665024585,124.547199294584));
#120324=CARTESIAN_POINT('Ctrl Pts',(8.00142743219962,28.4000473265462,124.535394571977));
#120325=CARTESIAN_POINT('Ctrl Pts',(8.007366396333,28.4245792473758,124.453181837674));
#120326=CARTESIAN_POINT('Ctrl Pts',(8.01266547828767,28.4502379979847,124.384211081478));
#120327=CARTESIAN_POINT('Ctrl Pts',(8.01901480169053,28.4860564108427,124.304497467385));
#120328=CARTESIAN_POINT('Ctrl Pts',(8.02002541510096,28.4919081042523,124.291898457524));
#120329=CARTESIAN_POINT('Ctrl Pts',(8.02640205195574,28.529804264357,124.212907130112));
#120330=CARTESIAN_POINT('Ctrl Pts',(8.0317678226661,28.5660704902492,124.148625720939));
#120331=CARTESIAN_POINT('Ctrl Pts',(8.04005974970625,28.6297525680149,124.051431814825));
#120332=CARTESIAN_POINT('Ctrl Pts',(8.04305391622489,28.6543788849495,124.016809305059));
#120333=CARTESIAN_POINT('Ctrl Pts',(8.04812442687762,28.6989693020672,123.958937842279));
#120334=CARTESIAN_POINT('Ctrl Pts',(8.05022221882604,28.7182997490558,123.935229614866));
#120335=CARTESIAN_POINT('Ctrl Pts',(8.05324088556407,28.7474005751394,123.901480066102));
#120336=CARTESIAN_POINT('Ctrl Pts',(8.05418218096618,28.7566611294397,123.891009541086));
#120337=CARTESIAN_POINT('Ctrl Pts',(8.05583713272232,28.7732694808934,123.872700744684));
#120338=CARTESIAN_POINT('Ctrl Pts',(8.05655299273948,28.7805632667765,123.864814799031));
#120339=CARTESIAN_POINT('Ctrl Pts',(8.05805048979114,28.7960494514399,123.848392847619));
#120340=CARTESIAN_POINT('Ctrl Pts',(8.05883139693659,28.8042575599505,123.839872426838));
#120341=CARTESIAN_POINT('Ctrl Pts',(8.06089709085245,28.8263171085823,123.817456393452));
#120342=CARTESIAN_POINT('Ctrl Pts',(8.06217498133404,28.8403246869818,123.803716533545));
#120343=CARTESIAN_POINT('Ctrl Pts',(8.06880434749208,28.9148163948325,123.733186887875));
#120344=CARTESIAN_POINT('Ctrl Pts',(8.07397056175925,28.9792408411131,123.680722860206));
#120345=CARTESIAN_POINT('Ctrl Pts',(8.08519649246316,29.1292056399887,123.576188905894));
#120346=CARTESIAN_POINT('Ctrl Pts',(8.09119983785487,29.216057022665,123.526584944874));
#120347=CARTESIAN_POINT('Ctrl Pts',(8.09922779230884,29.3324935823875,123.473308038464));
#120348=CARTESIAN_POINT('Ctrl Pts',(8.10101780225709,29.358460750046,123.462215758249));
#120349=CARTESIAN_POINT('Ctrl Pts',(8.10408094761068,29.402614024032,123.444667953206));
#120350=CARTESIAN_POINT('Ctrl Pts',(8.10533781904149,29.4206537265812,123.437858649841));
#120351=CARTESIAN_POINT('Ctrl Pts',(8.10715452754884,29.4465402580152,123.428597512091));
#120352=CARTESIAN_POINT('Ctrl Pts',(8.10770035047911,29.4542940961943,123.425888020323));
#120353=CARTESIAN_POINT('Ctrl Pts',(8.10865431373779,29.4677975712148,123.421281142596));
#120354=CARTESIAN_POINT('Ctrl Pts',(8.10906092718512,29.4735380290792,123.419357583844));
#120355=CARTESIAN_POINT('Ctrl Pts',(8.10993865335319,29.4858947250929,123.415291785253));
#120356=CARTESIAN_POINT('Ctrl Pts',(8.11041029446289,29.4925138288406,123.413159698885));
#120357=CARTESIAN_POINT('Ctrl Pts',(8.1117219620347,29.5108702874787,123.407373476646));
#120358=CARTESIAN_POINT('Ctrl Pts',(8.11256675023826,29.5226347608772,123.403807804541));
#120359=CARTESIAN_POINT('Ctrl Pts',(8.11874017630656,29.6082612112354,123.378886690644));
#120360=CARTESIAN_POINT('Ctrl Pts',(8.12429172306605,29.6834762305766,123.362539245164));
#120361=CARTESIAN_POINT('Ctrl Pts',(8.13680093034895,29.8537423756648,123.33770420625));
#120362=CARTESIAN_POINT('Ctrl Pts',(8.143749501351,29.9489566396222,123.332062285043));
#120363=CARTESIAN_POINT('Ctrl Pts',(8.15436594312315,30.0986156273441,123.336028553768));
#120364=CARTESIAN_POINT('Ctrl Pts',(8.15816306033289,30.1529953555493,123.340144709919));
#120365=CARTESIAN_POINT('Ctrl Pts',(8.16304867591075,30.2241139134745,123.349053717936));
#120366=CARTESIAN_POINT('Ctrl Pts',(8.1642105450047,30.2411133496201,123.35145061845));
#120367=CARTESIAN_POINT('Ctrl Pts',(8.16612441458717,30.2692499629297,123.355862400187));
#120368=CARTESIAN_POINT('Ctrl Pts',(8.16688103248263,30.280408744844,123.357728726312));
#120369=CARTESIAN_POINT('Ctrl Pts',(8.16835536296679,30.3022174807017,123.361605044283));
#120370=CARTESIAN_POINT('Ctrl Pts',(8.16907333515373,30.3128685197425,123.36360556853));
#120371=CARTESIAN_POINT('Ctrl Pts',(8.17079581853744,30.3384891189188,123.368677037219));
#120372=CARTESIAN_POINT('Ctrl Pts',(8.17179703180715,30.3534376019871,123.371850320277));
#120373=CARTESIAN_POINT('Ctrl Pts',(8.17514719167736,30.4036171077776,123.383226172473));
#120374=CARTESIAN_POINT('Ctrl Pts',(8.1774662877337,30.4386254930111,123.392370578873));
#120375=CARTESIAN_POINT('Ctrl Pts',(8.18744535598168,30.5897709479583,123.437156411244));
#120376=CARTESIAN_POINT('Ctrl Pts',(8.19474448068092,30.7021062656688,123.484296219092));
#120377=CARTESIAN_POINT('Ctrl Pts',(8.20528952279636,30.8522083280496,123.5675838564));
#120378=CARTESIAN_POINT('Ctrl Pts',(8.20839964569837,30.894969264776,123.593904569692));
#120379=CARTESIAN_POINT('Ctrl Pts',(8.21341285794739,30.9601546792472,123.638207501934));
#120380=CARTESIAN_POINT('Ctrl Pts',(8.21525998050454,30.9834150026727,123.654908733025));
#120381=CARTESIAN_POINT('Ctrl Pts',(8.21777096111479,31.0138280500334,123.67795630691));
#120382=CARTESIAN_POINT('Ctrl Pts',(8.21840214741607,31.021374548354,123.68377780645));
#120383=CARTESIAN_POINT('Ctrl Pts',(8.21945686594944,31.03381319667,123.6935445789));
#120384=CARTESIAN_POINT('Ctrl Pts',(8.21987789402631,31.038733857771,123.697453469815));
#120385=CARTESIAN_POINT('Ctrl Pts',(8.22068232362156,31.0480479374128,123.704938760973));
#120386=CARTESIAN_POINT('Ctrl Pts',(8.22106532869029,31.0524454473363,123.708509903293));
#120387=CARTESIAN_POINT('Ctrl Pts',(8.22209816859498,31.064207119915,123.718161317854));
#120388=CARTESIAN_POINT('Ctrl Pts',(8.22275082937282,31.0715372221164,123.724282487425));
#120389=CARTESIAN_POINT('Ctrl Pts',(8.22523420258614,31.0990590368401,123.747669749681));
#120390=CARTESIAN_POINT('Ctrl Pts',(8.22709117926231,31.1188882605249,123.765354021507));
#120391=CARTESIAN_POINT('Ctrl Pts',(8.23614896413271,31.2124158385421,123.852868474948));
#120392=CARTESIAN_POINT('Ctrl Pts',(8.24361003557906,31.2800479139355,123.928860971623));
#120393=CARTESIAN_POINT('Ctrl Pts',(8.25790072237452,31.3971163123766,124.087442794647));
#120394=CARTESIAN_POINT('Ctrl Pts',(8.26471553660821,31.4471754551548,124.169106930208));
#120395=CARTESIAN_POINT('Ctrl Pts',(8.27275692385634,31.4995977406789,124.273896132744));
#120396=CARTESIAN_POINT('Ctrl Pts',(8.27422280918255,31.5088629398133,124.293350925686));
#120397=CARTESIAN_POINT('Ctrl Pts',(8.27650090312042,31.5227948779878,124.324129073434));
#120398=CARTESIAN_POINT('Ctrl Pts',(8.27732182275284,31.5277183528788,124.335332866823));
#120399=CARTESIAN_POINT('Ctrl Pts',(8.27885071595576,31.5367032983413,124.35640630369));
#120400=CARTESIAN_POINT('Ctrl Pts',(8.27955965933285,31.5407942182755,124.366262626123));
#120401=CARTESIAN_POINT('Ctrl Pts',(8.28114476056929,31.5497688249438,124.388486009195));
#120402=CARTESIAN_POINT('Ctrl Pts',(8.28201911048519,31.5545997715853,124.400873686974));
#120403=CARTESIAN_POINT('Ctrl Pts',(8.28425543471283,31.5666414909333,124.432878149566));
#120404=CARTESIAN_POINT('Ctrl Pts',(8.28561014383738,31.573632506011,124.452575527924));
#120405=CARTESIAN_POINT('Ctrl Pts',(8.29662267006727,31.6278765267608,124.615045539408));
#120406=CARTESIAN_POINT('Ctrl Pts',(8.30559035061524,31.6559677911309,124.763474909878));
#120407=CARTESIAN_POINT('Ctrl Pts',(8.3176124521911,31.666073919873,124.958227368355));
#120408=CARTESIAN_POINT('Ctrl Pts',(8.32039128140837,31.6665948890141,125.002862943127));
#120409=CARTESIAN_POINT('Ctrl Pts',(8.3249288582424,31.6645681280028,125.073976470512));
#120410=CARTESIAN_POINT('Ctrl Pts',(8.32664371599238,31.6631794123358,125.100467035911));
#120411=CARTESIAN_POINT('Ctrl Pts',(8.3290007945212,31.6604527800136,125.136156282169));
#120412=CARTESIAN_POINT('Ctrl Pts',(8.3296151970263,31.6596693286104,125.145394902405));
#120413=CARTESIAN_POINT('Ctrl Pts',(8.33064959263819,31.658230427495,125.160831234165));
#120414=CARTESIAN_POINT('Ctrl Pts',(8.33106728303625,31.6576172236508,125.16703285496));
#120415=CARTESIAN_POINT('Ctrl Pts',(8.33187199221239,31.6563747934697,125.1789168169));
#120416=CARTESIAN_POINT('Ctrl Pts',(8.33225867042812,31.6557510893514,125.184599597587));
#120417=CARTESIAN_POINT('Ctrl Pts',(8.33331402068823,31.6539762632975,125.200037518568));
#120418=CARTESIAN_POINT('Ctrl Pts',(8.33398573327863,31.6527681155502,125.209785683135));
#120419=CARTESIAN_POINT('Ctrl Pts',(8.33663297112653,31.6476988166234,125.247922195983));
#120420=CARTESIAN_POINT('Ctrl Pts',(8.33863921217874,31.6431920673948,125.276218032144));
#120421=CARTESIAN_POINT('Ctrl Pts',(8.34732511271102,31.6208011871795,125.39670936142));
#120422=CARTESIAN_POINT('Ctrl Pts',(8.35421284492904,31.5958709859904,125.487407044403));
#120423=CARTESIAN_POINT('Ctrl Pts',(8.36102759409884,31.5634400156515,125.575509615436));
#120424=CARTESIAN_POINT('Ctrl Pts',(8.1662633962835,31.5634400119422,125.575509625513));
#120425=CARTESIAN_POINT('Ctrl Pts',(8.16547940338663,31.5675230376026,125.564417603061));
#120426=CARTESIAN_POINT('Ctrl Pts',(8.16469935094199,31.5714879934552,125.553282208899));
#120427=CARTESIAN_POINT('Ctrl Pts',(8.16261858217722,31.5817982102992,125.523321172272));
#120428=CARTESIAN_POINT('Ctrl Pts',(8.16132503901361,31.5879259497238,125.504422303556));
#120429=CARTESIAN_POINT('Ctrl Pts',(8.15401450562091,31.6208990948384,125.396165478388));
#120430=CARTESIAN_POINT('Ctrl Pts',(8.14823769707328,31.6405401236333,125.304782311777));
#120431=CARTESIAN_POINT('Ctrl Pts',(8.13815379187163,31.6615214357682,125.14141754525));
#120432=CARTESIAN_POINT('Ctrl Pts',(8.1338271862413,31.6660545215536,125.070101001078));
#120433=CARTESIAN_POINT('Ctrl Pts',(8.12586965586689,31.6659554899448,124.941605152703));
#120434=CARTESIAN_POINT('Ctrl Pts',(8.12227687646165,31.6629748332408,124.884540400681));
#120435=CARTESIAN_POINT('Ctrl Pts',(8.11775371755643,31.6558207837429,124.815718104112));
#120436=CARTESIAN_POINT('Ctrl Pts',(8.11695692623532,31.6544393470652,124.803702493656));
#120437=CARTESIAN_POINT('Ctrl Pts',(8.1156986941528,31.6520722827159,124.784918770768));
#120438=CARTESIAN_POINT('Ctrl Pts',(8.11524200733928,31.651175557281,124.778139599428));
#120439=CARTESIAN_POINT('Ctrl Pts',(8.11437467022709,31.6494024998621,124.765341988591));
#120440=CARTESIAN_POINT('Ctrl Pts',(8.11396450064347,31.6485349133915,124.759322574243));
#120441=CARTESIAN_POINT('Ctrl Pts',(8.11298173515628,31.6463868167796,124.744975613812));
#120442=CARTESIAN_POINT('Ctrl Pts',(8.11240750137777,31.6450760665032,124.736652860589));
#120443=CARTESIAN_POINT('Ctrl Pts',(8.11041880368796,31.6403444299506,124.708023618481));
#120444=CARTESIAN_POINT('Ctrl Pts',(8.10898876159608,31.6366103579801,124.687771722417));
#120445=CARTESIAN_POINT('Ctrl Pts',(8.10537394454592,31.6263309118788,124.637287408729));
#120446=CARTESIAN_POINT('Ctrl Pts',(8.10317148301915,31.6193172228626,124.607158853233));
#120447=CARTESIAN_POINT('Ctrl Pts',(8.09197161397868,31.5797573301492,124.456363388652));
#120448=CARTESIAN_POINT('Ctrl Pts',(8.0827492786961,31.5345391916822,124.339418226514));
#120449=CARTESIAN_POINT('Ctrl Pts',(8.06983431307662,31.4504007392126,124.178347955077));
#120450=CARTESIAN_POINT('Ctrl Pts',(8.06587361593285,31.4215804840318,124.129434323745));
#120451=CARTESIAN_POINT('Ctrl Pts',(8.06078102752913,31.3804668005706,124.067161834185));
#120452=CARTESIAN_POINT('Ctrl Pts',(8.05956981262259,31.3703765665007,124.052401065682));
#120453=CARTESIAN_POINT('Ctrl Pts',(8.05759698623261,31.3534321454635,124.028450341525));
#120454=CARTESIAN_POINT('Ctrl Pts',(8.05683015656659,31.3467174801256,124.019163952884));
#120455=CARTESIAN_POINT('Ctrl Pts',(8.05534300263878,31.3334467009033,124.001203680129));
#120456=CARTESIAN_POINT('Ctrl Pts',(8.05462234735522,31.3269004557831,123.992523259468));
#120457=CARTESIAN_POINT('Ctrl Pts',(8.05292384508931,31.3112009674688,123.97212398091));
#120458=CARTESIAN_POINT('Ctrl Pts',(8.05194892831283,31.3019747844053,123.960462231522));
#120459=CARTESIAN_POINT('Ctrl Pts',(8.04863056139839,31.2698482352999,123.920953559997));
#120460=CARTESIAN_POINT('Ctrl Pts',(8.04631713578434,31.2461998773373,123.893726107727));
#120461=CARTESIAN_POINT('Ctrl Pts',(8.04063836038355,31.1852560975805,123.827995392861));
#120462=CARTESIAN_POINT('Ctrl Pts',(8.03731240113142,31.1469511931257,123.790483397542));
#120463=CARTESIAN_POINT('Ctrl Pts',(8.03042966977431,31.0632888621334,123.716108161257));
#120464=CARTESIAN_POINT('Ctrl Pts',(8.02688373322862,31.0176680829258,123.679654143026));
#120465=CARTESIAN_POINT('Ctrl Pts',(8.01856846521728,30.9072627973995,123.600560960724));
#120466=CARTESIAN_POINT('Ctrl Pts',(8.01378953276452,30.8412350824564,123.559904125507));
#120467=CARTESIAN_POINT('Ctrl Pts',(8.00771114135584,30.7581293055201,123.51640174419));
#120468=CARTESIAN_POINT('Ctrl Pts',(8.00664023293826,30.7435197795543,123.509026453329));
#120469=CARTESIAN_POINT('Ctrl Pts',(8.00504723388949,30.721882482574,123.49850043697));
#120470=CARTESIAN_POINT('Ctrl Pts',(8.00453486656568,30.7149372173345,123.49518106542));
#120471=CARTESIAN_POINT('Ctrl Pts',(8.00361745592655,30.7025324198043,123.489357661751));
#120472=CARTESIAN_POINT('Ctrl Pts',(8.00321356364716,30.697081992667,123.486834851005));
#120473=CARTESIAN_POINT('Ctrl Pts',(8.00231425875376,30.6849709846306,123.481308414496));
#120474=CARTESIAN_POINT('Ctrl Pts',(8.00181803756103,30.6783043106643,123.478319140316));
#120475=CARTESIAN_POINT('Ctrl Pts',(8.00034036016486,30.6584927477178,123.469591879847));
#120476=CARTESIAN_POINT('Ctrl Pts',(7.99935193623896,30.6452935674306,123.463979853512));
#120477=CARTESIAN_POINT('Ctrl Pts',(7.99703551064283,30.6144464083375,123.451332013878));
#120478=CARTESIAN_POINT('Ctrl Pts',(7.99570161230325,30.5967474608037,123.444426368702));
#120479=CARTESIAN_POINT('Ctrl Pts',(7.99093377029377,30.5335897778804,123.421020408171));
#120480=CARTESIAN_POINT('Ctrl Pts',(7.98744347377121,30.4875369236231,123.406198954746));
#120481=CARTESIAN_POINT('Ctrl Pts',(7.97559565026444,30.3301799489671,123.363014573685));
#120482=CARTESIAN_POINT('Ctrl Pts',(7.96719875114672,30.2165916068098,123.344151491891));
#120483=CARTESIAN_POINT('Ctrl Pts',(7.95609761582235,30.0590035474612,123.334489079746));
#120484=CARTESIAN_POINT('Ctrl Pts',(7.95311713213314,30.0159598904829,123.333520505956));
#120485=CARTESIAN_POINT('Ctrl Pts',(7.94907638977623,29.956599414166,123.334485384452));
#120486=CARTESIAN_POINT('Ctrl Pts',(7.94797265909548,29.9402796496154,123.334990673249));
#120487=CARTESIAN_POINT('Ctrl Pts',(7.94620309146414,29.9139521404799,123.336193424277));
#120488=CARTESIAN_POINT('Ctrl Pts',(7.94553264128268,29.9039390013121,123.33674149704));
#120489=CARTESIAN_POINT('Ctrl Pts',(7.94413829492636,29.8830379102962,123.338074906346));
#120490=CARTESIAN_POINT('Ctrl Pts',(7.94341495412745,29.8721514707935,123.338876912879));
#120491=CARTESIAN_POINT('Ctrl Pts',(7.94169720050561,29.8462007216866,123.341045342342));
#120492=CARTESIAN_POINT('Ctrl Pts',(7.94070590647955,29.8311454264068,123.342510050721));
#120493=CARTESIAN_POINT('Ctrl Pts',(7.93726143839548,29.7785836839113,123.348347330616));
#120494=CARTESIAN_POINT('Ctrl Pts',(7.93484157359096,29.7412061589878,123.353789863707));
#120495=CARTESIAN_POINT('Ctrl Pts',(7.92882591070616,29.6476065425237,123.37068610308));
#120496=CARTESIAN_POINT('Ctrl Pts',(7.92527631368619,29.5917303668433,123.383781711775));
#120497=CARTESIAN_POINT('Ctrl Pts',(7.91508382551709,29.4321716469966,123.429982439392));
#120498=CARTESIAN_POINT('Ctrl Pts',(7.90855600761051,29.3309279800054,123.47038475019));
#120499=CARTESIAN_POINT('Ctrl Pts',(7.89966723044288,29.2062870285207,123.534880792568));
#120500=CARTESIAN_POINT('Ctrl Pts',(7.8976360741054,29.178642565453,123.550197862887));
#120501=CARTESIAN_POINT('Ctrl Pts',(7.89489237100837,29.1426951649625,123.571473495394));
#120502=CARTESIAN_POINT('Ctrl Pts',(7.89421944458202,29.1339857973103,123.576736516854));
#120503=CARTESIAN_POINT('Ctrl Pts',(7.89311372364442,29.1198606530076,123.585449909621));
#120504=CARTESIAN_POINT('Ctrl Pts',(7.89268395275239,29.1144154962051,123.588852484168));
#120505=CARTESIAN_POINT('Ctrl Pts',(7.89182829161612,29.103666686415,123.595655923485));
#120506=CARTESIAN_POINT('Ctrl Pts',(7.89140248040706,29.0983624082315,123.599055553105));
#120507=CARTESIAN_POINT('Ctrl Pts',(7.89032204265401,29.0850128985059,123.607718765476));
#120508=CARTESIAN_POINT('Ctrl Pts',(7.88966489768543,29.0769938146294,123.613021989139));
#120509=CARTESIAN_POINT('Ctrl Pts',(7.88698477430282,29.0446751223538,123.634799555874));
#120510=CARTESIAN_POINT('Ctrl Pts',(7.88492900238214,29.0207685383274,123.651844457387));
#120511=CARTESIAN_POINT('Ctrl Pts',(7.87914695340166,28.9556304836782,123.700933313278));
#120512=CARTESIAN_POINT('Ctrl Pts',(7.87537008386222,28.9154370496436,123.734296839081));
#120513=CARTESIAN_POINT('Ctrl Pts',(7.86219594576666,28.7815763555194,123.856475254525));
#120514=CARTESIAN_POINT('Ctrl Pts',(7.85279232132601,28.6966841254842,123.954254516698));
#120515=CARTESIAN_POINT('Ctrl Pts',(7.84182238365393,28.6074816347841,124.084959302965));
#120516=CARTESIAN_POINT('Ctrl Pts',(7.83982287605718,28.59167324514,124.109481717511));
#120517=CARTESIAN_POINT('Ctrl Pts',(7.83691392227666,28.5693587284,124.146178401709));
#120518=CARTESIAN_POINT('Ctrl Pts',(7.83598623183796,28.5623474722054,124.15803741245));
#120519=CARTESIAN_POINT('Ctrl Pts',(7.83434459552105,28.5501317531604,124.179296963083));
#120520=CARTESIAN_POINT('Ctrl Pts',(7.83362860328781,28.5448696935481,124.188663319862));
#120521=CARTESIAN_POINT('Ctrl Pts',(7.83213241674886,28.5340147828956,124.208430185137));
#120522=CARTESIAN_POINT('Ctrl Pts',(7.83135293656554,28.528441150779,124.218840609135));
#120523=CARTESIAN_POINT('Ctrl Pts',(7.82929473910204,28.513946225919,124.246620008103));
#120524=CARTESIAN_POINT('Ctrl Pts',(7.82802283033789,28.5052186200826,124.26408838172));
#120525=CARTESIAN_POINT('Ctrl Pts',(7.82089597060359,28.4576774834777,124.363579566852));
#120526=CARTESIAN_POINT('Ctrl Pts',(7.81526758462706,28.425306763893,124.44851656933));
#120527=CARTESIAN_POINT('Ctrl Pts',(7.80433881143629,28.3755953875649,124.619814571025));
#120528=CARTESIAN_POINT('Ctrl Pts',(7.79904847125346,28.3578543909645,124.705742324073));
#120529=CARTESIAN_POINT('Ctrl Pts',(7.79074311066009,28.3413084843429,124.837657812602));
#120530=CARTESIAN_POINT('Ctrl Pts',(7.78786345525984,28.3375047801776,124.882861691838));
#120531=CARTESIAN_POINT('Ctrl Pts',(7.78414759032397,28.3350575775181,124.939560393859));
#120532=CARTESIAN_POINT('Ctrl Pts',(7.78339488069868,28.3346826716383,124.950965376616));
#120533=CARTESIAN_POINT('Ctrl Pts',(7.78219093552553,28.3342738578325,124.96906165323));
#120534=CARTESIAN_POINT('Ctrl Pts',(7.78174380255814,28.3341630486648,124.975751090097));
#120535=CARTESIAN_POINT('Ctrl Pts',(7.78088226895111,28.3340278724356,124.988575816032));
#120536=CARTESIAN_POINT('Ctrl Pts',(7.78046821761287,28.3339971004304,124.994710827184));
#120537=CARTESIAN_POINT('Ctrl Pts',(7.77945854909367,28.3340046610185,125.009604853838));
#120538=CARTESIAN_POINT('Ctrl Pts',(7.77886105007367,28.3340781852903,125.018363592065));
#120539=CARTESIAN_POINT('Ctrl Pts',(7.77669705871863,28.3345916740203,125.049902096294));
#120540=CARTESIAN_POINT('Ctrl Pts',(7.77511123981863,28.3354298441543,125.072671740563));
#120541=CARTESIAN_POINT('Ctrl Pts',(7.76331096249049,28.345034490146,125.240097979747));
#120542=CARTESIAN_POINT('Ctrl Pts',(7.75253210682085,28.3721755996099,125.383078773499));
#120543=CARTESIAN_POINT('Ctrl Pts',(7.73764260775917,28.4373656924348,125.581186869983));
#120544=CARTESIAN_POINT('Ctrl Pts',(7.73318430821949,28.4607010085987,125.64044090245));
#120545=CARTESIAN_POINT('Ctrl Pts',(7.72757582582287,28.4951096077819,125.714983742574));
#120546=CARTESIAN_POINT('Ctrl Pts',(7.72632414020747,28.5031253860173,125.731616895899));
#120547=CARTESIAN_POINT('Ctrl Pts',(7.72430276290603,28.5166172616756,125.758462787412));
#120548=CARTESIAN_POINT('Ctrl Pts',(7.72352734323422,28.5219261306994,125.768757306863));
#120549=CARTESIAN_POINT('Ctrl Pts',(7.72203505804241,28.5323997074546,125.788557150542));
#120550=CARTESIAN_POINT('Ctrl Pts',(7.72131774822327,28.5375504662946,125.798069150583));
#120551=CARTESIAN_POINT('Ctrl Pts',(7.71964469751258,28.5498350382943,125.820236928453));
#120552=CARTESIAN_POINT('Ctrl Pts',(7.71869163853259,28.5570425427458,125.832851027241));
#120553=CARTESIAN_POINT('Ctrl Pts',(7.71553504002844,28.5816042387835,125.874561091506));
#120554=CARTESIAN_POINT('Ctrl Pts',(7.71335758306803,28.5996813934821,125.903222945534));
#120555=CARTESIAN_POINT('Ctrl Pts',(7.70809545278324,28.6460105336811,125.971940920347));
#120556=CARTESIAN_POINT('Ctrl Pts',(7.70504261989538,28.6751801135217,126.011340408464));
#120557=CARTESIAN_POINT('Ctrl Pts',(7.69595441545285,28.768005958698,126.125798667521));
#120558=CARTESIAN_POINT('Ctrl Pts',(7.6900402606431,28.836607764046,126.196557224185));
#120559=CARTESIAN_POINT('Ctrl Pts',(7.68066372424506,28.9508398064102,126.29521557618));
#120560=CARTESIAN_POINT('Ctrl Pts',(7.67734412115297,28.9922324149247,126.327676101586));
#120561=CARTESIAN_POINT('Ctrl Pts',(7.67313254270442,29.0447190292049,126.364966637521));
#120562=CARTESIAN_POINT('Ctrl Pts',(7.67235362444439,29.0544249119742,126.371708200758));
#120563=CARTESIAN_POINT('Ctrl Pts',(7.67111739632021,29.0698095114343,126.382153249063));
#120564=CARTESIAN_POINT('Ctrl Pts',(7.67066457148278,29.0754407375763,126.385926446496));
#120565=CARTESIAN_POINT('Ctrl Pts',(7.66979974185772,29.0861838383295,126.393030238777));
#120566=CARTESIAN_POINT('Ctrl Pts',(7.66938816571084,29.0912911931432,126.396367259283));
#120567=CARTESIAN_POINT('Ctrl Pts',(7.66839526749728,29.1036014817378,126.404314363718));
#120568=CARTESIAN_POINT('Ctrl Pts',(7.66781221520989,29.1108217379869,126.408897138234));
#120569=CARTESIAN_POINT('Ctrl Pts',(7.66575853836856,29.1362343295871,126.424753636516));
#120570=CARTESIAN_POINT('Ctrl Pts',(7.66427099435488,29.1546075098037,126.435731691455));
#120571=CARTESIAN_POINT('Ctrl Pts',(7.66047464353693,29.2015303646166,126.462555363645));
#120572=CARTESIAN_POINT('Ctrl Pts',(7.65814600305316,29.2303433361172,126.47792094369));
#120573=CARTESIAN_POINT('Ctrl Pts',(7.64516265713269,29.3919913425261,126.558116536754));
#120574=CARTESIAN_POINT('Ctrl Pts',(7.63424581479998,29.5325789428854,126.605905413153));
#120575=CARTESIAN_POINT('Ctrl Pts',(7.62134585339485,29.713652597349,126.641617849186));
#120576=CARTESIAN_POINT('Ctrl Pts',(7.61881405646138,29.7499010111748,126.647529926132));
#120577=CARTESIAN_POINT('Ctrl Pts',(7.61527680714111,29.8015385445396,126.654208148241));
#120578=CARTESIAN_POINT('Ctrl Pts',(7.61424077930881,29.8167862213805,126.655966269499));
#120579=CARTESIAN_POINT('Ctrl Pts',(7.61248389057747,29.8428473532705,126.658606850407));
#120580=CARTESIAN_POINT('Ctrl Pts',(7.61175976728051,29.8536488696803,126.659594828515));
#120581=CARTESIAN_POINT('Ctrl Pts',(7.61028862612303,29.8757120741823,126.661395791455));
#120582=CARTESIAN_POINT('Ctrl Pts',(7.6095419220133,29.8869739334423,126.662199922772));
#120583=CARTESIAN_POINT('Ctrl Pts',(7.60767544364632,29.9152762451372,126.663931817031));
#120584=CARTESIAN_POINT('Ctrl Pts',(7.60656030149541,29.9323246544792,126.664712374313));
#120585=CARTESIAN_POINT('Ctrl Pts',(7.60197943443788,30.0028814755744,126.666857064561));
#120586=CARTESIAN_POINT('Ctrl Pts',(7.59858554710241,30.05643108293,126.665904314293));
#120587=CARTESIAN_POINT('Ctrl Pts',(7.58950602481521,30.2015769896193,126.656313364939));
#120588=CARTESIAN_POINT('Ctrl Pts',(7.58394572145114,30.2926485133906,126.642670006646));
#120589=CARTESIAN_POINT('Ctrl Pts',(7.5737204231737,30.4550977610937,126.604388273474));
#120590=CARTESIAN_POINT('Ctrl Pts',(7.56908774313582,30.5268119690066,126.582290193669));
#120591=CARTESIAN_POINT('Ctrl Pts',(7.56317059711611,30.6120673691395,126.549579762324));
#120592=CARTESIAN_POINT('Ctrl Pts',(7.56209954095448,30.627261036796,126.543491965252));
#120593=CARTESIAN_POINT('Ctrl Pts',(7.56050636309539,30.6494648494323,126.534213372519));
#120594=CARTESIAN_POINT('Ctrl Pts',(7.55999396781632,30.6565470229436,126.531196023996));
#120595=CARTESIAN_POINT('Ctrl Pts',(7.55907652799532,30.6691170721733,126.525737336162));
#120596=CARTESIAN_POINT('Ctrl Pts',(7.55867263480671,30.674613021977,126.523315247564));
#120597=CARTESIAN_POINT('Ctrl Pts',(7.55777335390008,30.6867653101072,126.517881018139));
#120598=CARTESIAN_POINT('Ctrl Pts',(7.55727715788175,30.6934149093771,126.514854823003));
#120599=CARTESIAN_POINT('Ctrl Pts',(7.55579963001501,30.713057652568,126.505759092814));
#120600=CARTESIAN_POINT('Ctrl Pts',(7.55481133247162,30.7259921883703,126.499565593588));
#120601=CARTESIAN_POINT('Ctrl Pts',(7.55249525598461,30.7558692866738,126.484782281322));
#120602=CARTESIAN_POINT('Ctrl Pts',(7.55116158268466,30.7727478972863,126.476068231195));
#120603=CARTESIAN_POINT('Ctrl Pts',(7.54639489054645,30.8320464692208,126.444157899682));
#120604=CARTESIAN_POINT('Ctrl Pts',(7.54290554430773,30.873599932571,126.419406899207));
#120605=CARTESIAN_POINT('Ctrl Pts',(7.53106201613659,31.0099762168683,126.329916404571));
#120606=CARTESIAN_POINT('Ctrl Pts',(7.5226683822198,31.0991858730792,126.257189773572));
#120607=CARTESIAN_POINT('Ctrl Pts',(7.51156652673191,31.2106227338073,126.145340503689));
#120608=CARTESIAN_POINT('Ctrl Pts',(7.50858254789901,31.2398384763245,126.113648690396));
#120609=CARTESIAN_POINT('Ctrl Pts',(7.50453794722115,31.2783913784705,126.068427934785));
#120610=CARTESIAN_POINT('Ctrl Pts',(7.50343374417013,31.288804792686,126.055843268544));
#120611=CARTESIAN_POINT('Ctrl Pts',(7.50166362390539,31.3053110616948,126.035287212402));
#120612=CARTESIAN_POINT('Ctrl Pts',(7.50099308793677,31.3115197145778,126.02741064128));
#120613=CARTESIAN_POINT('Ctrl Pts',(7.49959871809119,31.3243358946151,126.010845964487));
#120614=CARTESIAN_POINT('Ctrl Pts',(7.49887543829594,31.3309299465244,126.002147999434));
#120615=CARTESIAN_POINT('Ctrl Pts',(7.49715811276073,31.3464535458631,125.981247905099));
#120616=CARTESIAN_POINT('Ctrl Pts',(7.49616718161414,31.3553034952546,125.968987648509));
#120617=CARTESIAN_POINT('Ctrl Pts',(7.49272555565311,31.3856443051889,125.92572602529));
#120618=CARTESIAN_POINT('Ctrl Pts',(7.49030809399141,31.406249144935,125.894115482181));
#120619=CARTESIAN_POINT('Ctrl Pts',(7.48276440726234,31.4679467320688,125.792046451093));
#120620=CARTESIAN_POINT('Ctrl Pts',(7.47776961305755,31.5049504781821,125.719257086047));
#120621=CARTESIAN_POINT('Ctrl Pts',(7.4712888155576,31.5459710599474,125.621395714317));
#120622=CARTESIAN_POINT('Ctrl Pts',(7.46979075119214,31.5549606711069,125.598544757198));
#120623=CARTESIAN_POINT('Ctrl Pts',(7.46828911258472,31.5634400017109,125.575509653308));
#120624=CARTESIAN_POINT('Origin',(5.,30.,125.));
#120625=CARTESIAN_POINT('',(6.76893575384937,31.5634399863339,125.575509695081));
#120626=CARTESIAN_POINT('',(6.96167312081938,31.563440026896,125.575509584889));
#120627=CARTESIAN_POINT('',(5.,31.5634400119422,125.575509625513));
#120628=CARTESIAN_POINT('Ctrl Pts',(6.96167312081939,31.563440026896,125.575509584889));
#120629=CARTESIAN_POINT('Ctrl Pts',(6.966193296855,31.5383945792393,125.643548513147));
#120630=CARTESIAN_POINT('Ctrl Pts',(6.97060998878207,31.508927581491,125.709898684935));
#120631=CARTESIAN_POINT('Ctrl Pts',(6.98041882974021,31.434304076632,125.852103848172));
#120632=CARTESIAN_POINT('Ctrl Pts',(6.98580007636323,31.3872769350315,125.926697516622));
#120633=CARTESIAN_POINT('Ctrl Pts',(6.99272052682677,31.3230206764459,126.012692190723));
#120634=CARTESIAN_POINT('Ctrl Pts',(6.99397971085297,31.3111898490752,126.027964145805));
#120635=CARTESIAN_POINT('Ctrl Pts',(6.99579918287312,31.2939506793452,126.049435659761));
#120636=CARTESIAN_POINT('Ctrl Pts',(6.99634539860296,31.2887573309838,126.055806847573));
#120637=CARTESIAN_POINT('Ctrl Pts',(6.9972998046712,31.2796567776652,126.066804197838));
#120638=CARTESIAN_POINT('Ctrl Pts',(6.99770646371591,31.2757711531439,126.071447912225));
#120639=CARTESIAN_POINT('Ctrl Pts',(6.99858399855288,31.2673707392771,126.081376771098));
#120640=CARTESIAN_POINT('Ctrl Pts',(6.99905539992462,31.2628482338718,126.086654795989));
#120641=CARTESIAN_POINT('Ctrl Pts',(7.00036576565738,31.2502460926146,126.101177301433));
#120642=CARTESIAN_POINT('Ctrl Pts',(7.00120947711509,31.2420972770347,126.110360785311));
#120643=CARTESIAN_POINT('Ctrl Pts',(7.00711662413704,31.1847569073055,126.173560669269));
#120644=CARTESIAN_POINT('Ctrl Pts',(7.01238149070013,31.132165000168,126.224374787963));
#120645=CARTESIAN_POINT('Ctrl Pts',(7.0186672546681,31.0661255139492,126.280278935297));
#120646=CARTESIAN_POINT('Ctrl Pts',(7.01964800295812,31.0557301374573,126.288864475846));
#120647=CARTESIAN_POINT('Ctrl Pts',(7.02603795929059,30.9873606527184,126.343948648749));
#120648=CARTESIAN_POINT('Ctrl Pts',(7.03144852766284,30.9264308950238,126.386652860934));
#120649=CARTESIAN_POINT('Ctrl Pts',(7.03979527649104,30.8263888625795,126.447222923726));
#120650=CARTESIAN_POINT('Ctrl Pts',(7.04280072172926,30.7890915576832,126.467892285816));
#120651=CARTESIAN_POINT('Ctrl Pts',(7.04788798330599,30.7236690833864,126.500932806407));
#120652=CARTESIAN_POINT('Ctrl Pts',(7.04999144044879,30.695920559973,126.513998355545));
#120653=CARTESIAN_POINT('Ctrl Pts',(7.05301661758845,30.655007516378,126.531899771618));
#120654=CARTESIAN_POINT('Ctrl Pts',(7.05395888293745,30.6421190293987,126.537346717438));
#120655=CARTESIAN_POINT('Ctrl Pts',(7.0556149281266,30.6192154691299,126.546687951303));
#120656=CARTESIAN_POINT('Ctrl Pts',(7.05633092151664,30.6092286283953,126.550648865331));
#120657=CARTESIAN_POINT('Ctrl Pts',(7.05782810090738,30.5881718479604,126.558765430803));
#120658=CARTESIAN_POINT('Ctrl Pts',(7.05860856276711,30.5770945408188,126.562900410803));
#120659=CARTESIAN_POINT('Ctrl Pts',(7.06067168290318,30.5475525795693,126.573571031546));
#120660=CARTESIAN_POINT('Ctrl Pts',(7.06194747625012,30.5290147495355,126.579899701239));
#120661=CARTESIAN_POINT('Ctrl Pts',(7.06853353903769,30.432005823576,126.611118781296));
#120662=CARTESIAN_POINT('Ctrl Pts',(7.07366166483805,30.3518763143641,126.630496332782));
#120663=CARTESIAN_POINT('Ctrl Pts',(7.08488643070133,30.1715630175352,126.660181672029));
#120664=CARTESIAN_POINT('Ctrl Pts',(7.09092316836261,30.0712272551629,126.667501538973));
#120665=CARTESIAN_POINT('Ctrl Pts',(7.09899128376423,29.9425468691838,126.665249663901));
#120666=CARTESIAN_POINT('Ctrl Pts',(7.1007857676625,29.9142626508337,126.664033122141));
#120667=CARTESIAN_POINT('Ctrl Pts',(7.10385579548681,29.8667521117274,126.660775175668));
#120668=CARTESIAN_POINT('Ctrl Pts',(7.10511498015536,29.8475048510824,126.659118541673));
#120669=CARTESIAN_POINT('Ctrl Pts',(7.10693445294361,29.8201157786704,126.656280541303));
#120670=CARTESIAN_POINT('Ctrl Pts',(7.1074806687826,29.8119463789569,126.655372886448));
#120671=CARTESIAN_POINT('Ctrl Pts',(7.10843507497376,29.7977712108058,126.653691682864));
#120672=CARTESIAN_POINT('Ctrl Pts',(7.10884173403102,29.7917624006745,126.652945784361));
#120673=CARTESIAN_POINT('Ctrl Pts',(7.10971926881462,29.7788646517967,126.651273287378));
#120674=CARTESIAN_POINT('Ctrl Pts',(7.11019067011921,29.7719775096223,126.650336344903));
#120675=CARTESIAN_POINT('Ctrl Pts',(7.11150103548905,29.7529415765722,126.647625223343));
#120676=CARTESIAN_POINT('Ctrl Pts',(7.11234474664724,29.7408065110413,126.645759841031));
#120677=CARTESIAN_POINT('Ctrl Pts',(7.11825181547121,29.6566112920883,126.631863231038));
#120678=CARTESIAN_POINT('Ctrl Pts',(7.12351659796537,29.5853972575236,126.615238561539));
#120679=CARTESIAN_POINT('Ctrl Pts',(7.12985618616815,29.5019033539565,126.589861017168));
#120680=CARTESIAN_POINT('Ctrl Pts',(7.13089098830388,29.4883476775932,126.585550446938));
#120681=CARTESIAN_POINT('Ctrl Pts',(7.1372891050192,29.404922107127,126.557840658739));
#120682=CARTESIAN_POINT('Ctrl Pts',(7.14265240217251,29.3366087604331,126.529999538607));
#120683=CARTESIAN_POINT('Ctrl Pts',(7.15094908680955,29.2320964648863,126.479084760424));
#120684=CARTESIAN_POINT('Ctrl Pts',(7.15395008642306,29.1945589397529,126.458983471565));
#120685=CARTESIAN_POINT('Ctrl Pts',(7.1590307467202,29.1314003294049,126.421980624633));
#120686=CARTESIAN_POINT('Ctrl Pts',(7.16113197204303,29.105401469555,126.405769528781));
#120687=CARTESIAN_POINT('Ctrl Pts',(7.16415458453434,29.0682037118246,126.381125367054));
#120688=CARTESIAN_POINT('Ctrl Pts',(7.1650964678777,29.0566419879583,126.373254267792));
#120689=CARTESIAN_POINT('Ctrl Pts',(7.16675208220771,29.0363772965739,126.359081559794));
#120690=CARTESIAN_POINT('Ctrl Pts',(7.16746802285157,29.027633736103,126.352839701833));
#120691=CARTESIAN_POINT('Ctrl Pts',(7.16896532649102,29.0093927762997,126.339549619986));
#120692=CARTESIAN_POINT('Ctrl Pts',(7.16974596308683,28.9999087909649,126.33248393679));
#120693=CARTESIAN_POINT('Ctrl Pts',(7.17181009374439,28.9749093546767,126.313441774409));
#120694=CARTESIAN_POINT('Ctrl Pts',(7.17308671056739,28.9595283480561,126.301291251019));
#120695=CARTESIAN_POINT('Ctrl Pts',(7.17967188543802,28.8806976045962,126.23672585809));
#120696=CARTESIAN_POINT('Ctrl Pts',(7.18479845117593,28.8209775130676,126.179930992096));
#120697=CARTESIAN_POINT('Ctrl Pts',(7.19602170186277,28.6982586781219,126.044560473895));
#120698=CARTESIAN_POINT('Ctrl Pts',(7.20205843940251,28.6376904265412,125.964234063907));
#120699=CARTESIAN_POINT('Ctrl Pts',(7.21012655465839,28.5697907063525,125.85490273231));
#120700=CARTESIAN_POINT('Ctrl Pts',(7.21192103853971,28.5554724320103,125.830480120127));
#120701=CARTESIAN_POINT('Ctrl Pts',(7.21499106633762,28.5324415648769,125.788797453938));
#120702=CARTESIAN_POINT('Ctrl Pts',(7.21625025099701,28.5233943524098,125.771728493233));
#120703=CARTESIAN_POINT('Ctrl Pts',(7.21806972377346,28.5109238310133,125.74717851116));
#120704=CARTESIAN_POINT('Ctrl Pts',(7.21861593961022,28.5072556024047,125.739822763249));
#120705=CARTESIAN_POINT('Ctrl Pts',(7.21957034579791,28.5009799526793,125.72700176264));
#120706=CARTESIAN_POINT('Ctrl Pts',(7.21997700485396,28.4983476516984,125.721548950972));
#120707=CARTESIAN_POINT('Ctrl Pts',(7.22085453963506,28.4927575135064,125.709805888072));
#120708=CARTESIAN_POINT('Ctrl Pts',(7.22132594093839,28.4898093411323,125.703511536007));
#120709=CARTESIAN_POINT('Ctrl Pts',(7.22263630630562,28.4817626660433,125.686048204548));
#120710=CARTESIAN_POINT('Ctrl Pts',(7.22348001746242,28.4767482312665,125.674841291059));
#120711=CARTESIAN_POINT('Ctrl Pts',(7.22938708606425,28.442758916984,125.596568200993));
#120712=CARTESIAN_POINT('Ctrl Pts',(7.23465186832113,28.418102092124,125.52772156801));
#120713=CARTESIAN_POINT('Ctrl Pts',(7.24099145646593,28.3941387776321,125.443810835012));
#120714=CARTESIAN_POINT('Ctrl Pts',(7.24202625877757,28.390408162747,125.430084220041));
#120715=CARTESIAN_POINT('Ctrl Pts',(7.24842437566815,28.3684413288612,125.344965968219));
#120716=CARTESIAN_POINT('Ctrl Pts',(7.25378767282275,28.3547811606937,125.272472926459));
#120717=CARTESIAN_POINT('Ctrl Pts',(7.26208435754627,28.3408731677075,125.157053246447));
#120718=CARTESIAN_POINT('Ctrl Pts',(7.26508535724185,28.3374021304523,125.114614118249));
#120719=CARTESIAN_POINT('Ctrl Pts',(7.27016601766141,28.3342348719602,125.041482801664));
#120720=CARTESIAN_POINT('Ctrl Pts',(7.27226724302612,28.3337536718893,125.010847710264));
#120721=CARTESIAN_POINT('Ctrl Pts',(7.27528985556495,28.3342835778378,124.966230144794));
#120722=CARTESIAN_POINT('Ctrl Pts',(7.27623173891497,28.3346257674137,124.952247635315));
#120723=CARTESIAN_POINT('Ctrl Pts',(7.27788735325175,28.3355420359784,124.927535617478));
#120724=CARTESIAN_POINT('Ctrl Pts',(7.27860329389593,28.3360438995755,124.916804411885));
#120725=CARTESIAN_POINT('Ctrl Pts',(7.28010059753142,28.3373162347825,124.894271323985));
#120726=CARTESIAN_POINT('Ctrl Pts',(7.28088123412269,28.338108649987,124.882471242065));
#120727=CARTESIAN_POINT('Ctrl Pts',(7.28294536475721,28.34054800367,124.851140342079));
#120728=CARTESIAN_POINT('Ctrl Pts',(7.28422198156203,28.342414082035,124.831628081226));
#120729=CARTESIAN_POINT('Ctrl Pts',(7.29080715586865,28.353903316031,124.730380998343));
#120730=CARTESIAN_POINT('Ctrl Pts',(7.29593372110214,28.3692291218998,124.649404060856));
#120731=CARTESIAN_POINT('Ctrl Pts',(7.30715697173942,28.4164014992063,124.472882515546));
#120732=CARTESIAN_POINT('Ctrl Pts',(7.31319370968902,28.4510371724665,124.378430322264));
#120733=CARTESIAN_POINT('Ctrl Pts',(7.32126182543699,28.5060648200421,124.262087414743));
#120734=CARTESIAN_POINT('Ctrl Pts',(7.32305630937317,28.5188176029647,124.236812060255));
#120735=CARTESIAN_POINT('Ctrl Pts',(7.32612633725581,28.5413459119135,124.194855643275));
#120736=CARTESIAN_POINT('Ctrl Pts',(7.32738552194384,28.5507794064118,124.177997094348));
#120737=CARTESIAN_POINT('Ctrl Pts',(7.32920499475501,28.5646413530681,124.154205037103));
#120738=CARTESIAN_POINT('Ctrl Pts',(7.32975121059729,28.5688317218884,124.147133704909));
#120739=CARTESIAN_POINT('Ctrl Pts',(7.33070561679346,28.5761995160184,124.134907607844));
#120740=CARTESIAN_POINT('Ctrl Pts',(7.33111227585242,28.5793529951318,124.129738687883));
#120741=CARTESIAN_POINT('Ctrl Pts',(7.33198981064104,28.5861869636679,124.118673153631));
#120742=CARTESIAN_POINT('Ctrl Pts',(7.33246121194913,28.5898761402413,124.112782435044));
#120743=CARTESIAN_POINT('Ctrl Pts',(7.33377157732532,28.6001836181937,124.096550588903));
#120744=CARTESIAN_POINT('Ctrl Pts',(7.33461528848609,28.6068793850868,124.086259516398));
#120745=CARTESIAN_POINT('Ctrl Pts',(7.34052235688253,28.6542054326214,124.015251102541));
#120746=CARTESIAN_POINT('Ctrl Pts',(7.34578713890975,28.6986735096762,123.957195891152));
#120747=CARTESIAN_POINT('Ctrl Pts',(7.35212672693545,28.7561737291237,123.891553099738));
#120748=CARTESIAN_POINT('Ctrl Pts',(7.35316152935754,28.7656827057463,123.880974023523));
#120749=CARTESIAN_POINT('Ctrl Pts',(7.35955964627689,28.8252802352485,123.816353646246));
#120750=CARTESIAN_POINT('Ctrl Pts',(7.36492294335048,28.8787760118712,123.765559522229));
#120751=CARTESIAN_POINT('Ctrl Pts',(7.37321962798843,28.9682019155929,123.691275322744));
#120752=CARTESIAN_POINT('Ctrl Pts',(7.37622062767511,29.0019743096699,123.665341694156));
#120753=CARTESIAN_POINT('Ctrl Pts',(7.38130128808386,29.0616973067255,123.623016942581));
#120754=CARTESIAN_POINT('Ctrl Pts',(7.38340251344613,29.0871741957121,123.605997292045));
#120755=CARTESIAN_POINT('Ctrl Pts',(7.38642512598808,29.1249467578543,123.582243523875));
#120756=CARTESIAN_POINT('Ctrl Pts',(7.38736700934347,29.1368796645049,123.574947401198));
#120757=CARTESIAN_POINT('Ctrl Pts',(7.38902262369281,29.1581382583909,123.562314287215));
#120758=CARTESIAN_POINT('Ctrl Pts',(7.38973856434393,29.1674262045092,123.556915704096));
#120759=CARTESIAN_POINT('Ctrl Pts',(7.39123586799713,29.1870473022802,123.545763510524));
#120760=CARTESIAN_POINT('Ctrl Pts',(7.39201650459929,29.1973908427705,123.540029312306));
#120761=CARTESIAN_POINT('Ctrl Pts',(7.39408063527072,29.2250363148598,123.525085964332));
#120762=CARTESIAN_POINT('Ctrl Pts',(7.39535725210117,29.2424415093435,123.516070988316));
#120763=CARTESIAN_POINT('Ctrl Pts',(7.40194242698856,29.3337349497125,123.470810808562));
#120764=CARTESIAN_POINT('Ctrl Pts',(7.40706899273668,29.4100793770008,123.439767700186));
#120765=CARTESIAN_POINT('Ctrl Pts',(7.41829224342091,29.5839674214316,123.383660324616));
#120766=CARTESIAN_POINT('Ctrl Pts',(7.42432898094934,29.6821059613598,123.361531787285));
#120767=CARTESIAN_POINT('Ctrl Pts',(7.43239709619095,29.809695717242,123.344662697421));
#120768=CARTESIAN_POINT('Ctrl Pts',(7.43419158007314,29.8378472940619,123.341668421405));
#120769=CARTESIAN_POINT('Ctrl Pts',(7.43726160787373,29.8853152518913,123.337839781371));
#120770=CARTESIAN_POINT('Ctrl Pts',(7.43852079253511,29.9045952413721,123.336621799531));
#120771=CARTESIAN_POINT('Ctrl Pts',(7.44034026531624,29.9321022065677,123.335363867318));
#120772=CARTESIAN_POINT('Ctrl Pts',(7.44088648115566,29.9403158462684,123.335049142056));
#120773=CARTESIAN_POINT('Ctrl Pts',(7.44184088734762,29.9545835498231,123.334608150853));
#120774=CARTESIAN_POINT('Ctrl Pts',(7.44224754640526,29.9606365184279,123.334454089457));
#120775=CARTESIAN_POINT('Ctrl Pts',(7.44312508118727,29.973639654747,123.33419405571));
#120776=CARTESIAN_POINT('Ctrl Pts',(7.44359648249007,29.9805895808218,123.334098579431));
#120777=CARTESIAN_POINT('Ctrl Pts',(7.44490684785871,29.999817067539,123.333954770206));
#120778=CARTESIAN_POINT('Ctrl Pts',(7.44575055901746,30.0120945892691,123.333998667474));
#120779=CARTESIAN_POINT('Ctrl Pts',(7.45165762904086,30.0974198227322,123.335246928159));
#120780=CARTESIAN_POINT('Ctrl Pts',(7.45692241283013,30.1703124459516,123.341119438285));
#120781=CARTESIAN_POINT('Ctrl Pts',(7.4632620014523,30.2566478753397,123.353825589296));
#120782=CARTESIAN_POINT('Ctrl Pts',(7.46429680272615,30.2706931298021,123.356076781613));
#120783=CARTESIAN_POINT('Ctrl Pts',(7.47069491871232,30.3573070701426,123.371099489073));
#120784=CARTESIAN_POINT('Ctrl Pts',(7.47605821598763,30.4289956167446,123.388494714266));
#120785=CARTESIAN_POINT('Ctrl Pts',(7.48435490041269,30.5399064039931,123.423336230416));
#120786=CARTESIAN_POINT('Ctrl Pts',(7.48735589971121,30.5800113034398,123.437644419683));
#120787=CARTESIAN_POINT('Ctrl Pts',(7.49243655953587,30.6479617717169,123.464864883197));
#120788=CARTESIAN_POINT('Ctrl Pts',(7.49453778469617,30.6760784683834,123.477038279151));
#120789=CARTESIAN_POINT('Ctrl Pts',(7.4975603969953,30.7165215215942,123.495889461756));
#120790=CARTESIAN_POINT('Ctrl Pts',(7.49850228030555,30.7291232914694,123.50195766124));
#120791=CARTESIAN_POINT('Ctrl Pts',(7.50015789459243,30.7512668178171,123.512966184254));
#120792=CARTESIAN_POINT('Ctrl Pts',(7.50087383522634,30.7608398508293,123.517841394651));
#120793=CARTESIAN_POINT('Ctrl Pts',(7.5023711388598,30.7808510729231,123.528277384162));
#120794=CARTESIAN_POINT('Ctrl Pts',(7.50315177545901,30.7912785874679,123.533857419891));
#120795=CARTESIAN_POINT('Ctrl Pts',(7.50521590615963,30.8188270566152,123.548978850164));
#120796=CARTESIAN_POINT('Ctrl Pts',(7.50649252302161,30.8358408834732,123.558712313236));
#120797=CARTESIAN_POINT('Ctrl Pts',(7.51307769939527,30.9233802351038,123.610864425048));
#120798=CARTESIAN_POINT('Ctrl Pts',(7.51820426648427,30.9908673957531,123.658168051287));
#120799=CARTESIAN_POINT('Ctrl Pts',(7.52942751729442,31.1323162742686,123.773828354633));
#120800=CARTESIAN_POINT('Ctrl Pts',(7.53546425372712,31.2041342265591,123.844277081419));
#120801=CARTESIAN_POINT('Ctrl Pts',(7.54353236765408,31.2875067704446,123.942321588919));
#120802=CARTESIAN_POINT('Ctrl Pts',(7.54532685138454,31.3052907946921,123.964348965258));
#120803=CARTESIAN_POINT('Ctrl Pts',(7.54839687894824,31.3342523150708,124.002152344534));
#120804=CARTESIAN_POINT('Ctrl Pts',(7.54965606352714,31.3457323677236,124.017689712884));
#120805=CARTESIAN_POINT('Ctrl Pts',(7.55147553620363,31.3617080004292,124.04011725396));
#120806=CARTESIAN_POINT('Ctrl Pts',(7.55202175202278,31.3664271978291,124.046847194516));
#120807=CARTESIAN_POINT('Ctrl Pts',(7.55297615818503,31.3745359834704,124.058594935591));
#120808=CARTESIAN_POINT('Ctrl Pts',(7.55338281723334,31.3779483298579,124.063596740689));
#120809=CARTESIAN_POINT('Ctrl Pts',(7.55426035200048,31.3852192295387,124.074380208753));
#120810=CARTESIAN_POINT('Ctrl Pts',(7.55473175329769,31.3890688335681,124.0801673614));
#120811=CARTESIAN_POINT('Ctrl Pts',(7.55604211865959,31.3996179521425,124.096243213456));
#120812=CARTESIAN_POINT('Ctrl Pts',(7.55688582981733,31.4062399589624,124.106581902531));
#120813=CARTESIAN_POINT('Ctrl Pts',(7.56279289993928,31.4514685836792,124.178944360683));
#120814=CARTESIAN_POINT('Ctrl Pts',(7.5680576838424,31.4860691735957,124.243369668355));
#120815=CARTESIAN_POINT('Ctrl Pts',(7.57439727268539,31.5222194197738,124.322795185727));
#120816=CARTESIAN_POINT('Ctrl Pts',(7.57543207406137,31.5279457371311,124.335816182902));
#120817=CARTESIAN_POINT('Ctrl Pts',(7.58183019034967,31.5623007978282,124.416732107576));
#120818=CARTESIAN_POINT('Ctrl Pts',(7.58719348782527,31.5865676047445,124.486395326085));
#120819=CARTESIAN_POINT('Ctrl Pts',(7.59549017257246,31.6174497571123,124.598473100837));
#120820=CARTESIAN_POINT('Ctrl Pts',(7.59849117199816,31.6271802811094,124.639927223499));
#120821=CARTESIAN_POINT('Ctrl Pts',(7.60357183201865,31.6411650772316,124.71177877631));
#120822=CARTESIAN_POINT('Ctrl Pts',(7.60567305724997,31.6461871632694,124.742003251707));
#120823=CARTESIAN_POINT('Ctrl Pts',(7.60869566962982,31.6522843227317,124.786205427981));
#120824=CARTESIAN_POINT('Ctrl Pts',(7.60963755295165,31.6540209112374,124.800083897414));
#120825=CARTESIAN_POINT('Ctrl Pts',(7.61129316725043,31.6567820246177,124.824658266149));
#120826=CARTESIAN_POINT('Ctrl Pts',(7.61200910788456,31.6578782171453,124.835345127209));
#120827=CARTESIAN_POINT('Ctrl Pts',(7.61350641150992,31.659963855613,124.857817532346));
#120828=CARTESIAN_POINT('Ctrl Pts',(7.61428704810103,31.660931333749,124.869604552378));
#120829=CARTESIAN_POINT('Ctrl Pts',(7.6163511787599,31.6631684612917,124.900950541348));
#120830=CARTESIAN_POINT('Ctrl Pts',(7.61762779558879,31.6642186433368,124.920523678669));
#120831=CARTESIAN_POINT('Ctrl Pts',(7.62421297105267,31.6678815810625,125.022354719317));
#120832=CARTESIAN_POINT('Ctrl Pts',(7.629339537333,31.6647423567958,125.104709396858));
#120833=CARTESIAN_POINT('Ctrl Pts',(7.64056278794753,31.6442878921592,125.286276751473));
#120834=CARTESIAN_POINT('Ctrl Pts',(7.6465995249291,31.6240523245838,125.384823009938));
#120835=CARTESIAN_POINT('Ctrl Pts',(7.6546676395099,31.5868991330003,125.508043745124));
#120836=CARTESIAN_POINT('Ctrl Pts',(7.65646212331654,31.5780383901506,125.534931737467));
#120837=CARTESIAN_POINT('Ctrl Pts',(7.65860526371597,31.5668323255569,125.566230402364));
#120838=CARTESIAN_POINT('Ctrl Pts',(7.65892464110724,31.5651464584609,125.570873861579));
#120839=CARTESIAN_POINT('Ctrl Pts',(7.65924497815242,31.5634400119496,125.575509625493));
#120840=CARTESIAN_POINT('',(7.4292556837088,31.665999521611,125.001262533919));
#120841=CARTESIAN_POINT('Ctrl Pts',(7.46828911258472,31.5634400017109,125.575509653308));
#120842=CARTESIAN_POINT('Ctrl Pts',(7.46528247231107,31.5804176531656,125.529387856276));
#120843=CARTESIAN_POINT('Ctrl Pts',(7.46226192838087,31.5953496106608,125.482527794622));
#120844=CARTESIAN_POINT('Ctrl Pts',(7.45662573031151,31.6188128575682,125.395797693496));
#120845=CARTESIAN_POINT('Ctrl Pts',(7.45403248721639,31.6279934835074,125.356156576094));
#120846=CARTESIAN_POINT('Ctrl Pts',(7.45064112335473,31.6378167593212,125.305344127953));
#120847=CARTESIAN_POINT('Ctrl Pts',(7.44990977216345,31.6398112597121,125.294444884129));
#120848=CARTESIAN_POINT('Ctrl Pts',(7.44873214131851,31.6428231626362,125.277005159377));
#120849=CARTESIAN_POINT('Ctrl Pts',(7.44828966293518,31.643910597604,125.270476884929));
#120850=CARTESIAN_POINT('Ctrl Pts',(7.44743040643905,31.6459364819821,125.257851038113));
#120851=CARTESIAN_POINT('Ctrl Pts',(7.44701390997584,31.6468800014469,125.251754476398));
#120852=CARTESIAN_POINT('Ctrl Pts',(7.44617153378019,31.6487115998284,125.239468491965));
#120853=CARTESIAN_POINT('Ctrl Pts',(7.44574561059107,31.649598743314,125.233278976747));
#120854=CARTESIAN_POINT('Ctrl Pts',(7.44471964986124,31.6516431637521,125.218420136887));
#120855=CARTESIAN_POINT('Ctrl Pts',(7.44411793239531,31.6527670413154,125.209746503644));
#120856=CARTESIAN_POINT('Ctrl Pts',(7.44202256058211,31.6564236033363,125.17967008459));
#120857=CARTESIAN_POINT('Ctrl Pts',(7.4405132147872,31.6586091277853,125.158228174088));
#120858=CARTESIAN_POINT('Ctrl Pts',(7.43579240609516,31.664090141318,125.091679863765));
#120859=CARTESIAN_POINT('Ctrl Pts',(7.43253489000666,31.6659652551283,125.046479492374));
#120860=CARTESIAN_POINT('Ctrl Pts',(7.4292556837088,31.665999521611,125.001262533919));
#120861=CARTESIAN_POINT('Ctrl Pts',(7.42925582289325,31.6659995201555,125.001264453133));
#120862=CARTESIAN_POINT('Ctrl Pts',(7.41937353690219,31.6661029433549,124.864997638634));
#120863=CARTESIAN_POINT('Ctrl Pts',(7.40939537630788,31.6494867121614,124.729197380578));
#120864=CARTESIAN_POINT('Ctrl Pts',(7.39773129809934,31.6088690801473,124.566304180783));
#120865=CARTESIAN_POINT('Ctrl Pts',(7.39556508607674,31.6003655312297,124.535907141989));
#120866=CARTESIAN_POINT('Ctrl Pts',(7.39246811501382,31.5868076548228,124.492262396981));
#120867=CARTESIAN_POINT('Ctrl Pts',(7.3915154034024,31.5824402979764,124.478810272853));
#120868=CARTESIAN_POINT('Ctrl Pts',(7.38984771654489,31.5744492670533,124.455223631478));
#120869=CARTESIAN_POINT('Ctrl Pts',(7.38913041941947,31.5708977536186,124.445065730701));
#120870=CARTESIAN_POINT('Ctrl Pts',(7.38763697719301,31.5632644351025,124.423893888299));
#120871=CARTESIAN_POINT('Ctrl Pts',(7.38686149381992,31.559164058377,124.412887236588));
#120872=CARTESIAN_POINT('Ctrl Pts',(7.3848264162618,31.5480445291983,124.383977361271));
#120873=CARTESIAN_POINT('Ctrl Pts',(7.38357335230851,31.5408310963366,124.36615038208));
#120874=CARTESIAN_POINT('Ctrl Pts',(7.37751431785362,31.5041856583478,124.279911452624));
#120875=CARTESIAN_POINT('Ctrl Pts',(7.37285456558696,31.4704961988646,124.213396596589));
#120876=CARTESIAN_POINT('Ctrl Pts',(7.36165097278908,31.3776634283298,124.057068934145));
#120877=CARTESIAN_POINT('Ctrl Pts',(7.35521639351726,31.3140763664132,123.970302805046));
#120878=CARTESIAN_POINT('Ctrl Pts',(7.3466654863898,31.2231005808139,123.868435979257));
#120879=CARTESIAN_POINT('Ctrl Pts',(7.34481285502146,31.2030395334059,123.847130602155));
#120880=CARTESIAN_POINT('Ctrl Pts',(7.34167298585398,31.1687020394077,123.812535792505));
#120881=CARTESIAN_POINT('Ctrl Pts',(7.34040380462425,31.1547340779628,123.798948447985));
#120882=CARTESIAN_POINT('Ctrl Pts',(7.33859560784482,31.1347733246387,123.780201692698));
#120883=CARTESIAN_POINT('Ctrl Pts',(7.33807113148018,31.1289766151009,123.774834621293));
#120884=CARTESIAN_POINT('Ctrl Pts',(7.33753987871096,31.1231009888508,123.769471588325));
#120885=CARTESIAN_POINT('Ctrl Pts',(7.33753616151487,31.1230598766707,123.769434066573));
#120886=CARTESIAN_POINT('Ctrl Pts',(7.33752865416081,31.1229768449558,123.769358293851));
#120887=CARTESIAN_POINT('Ctrl Pts',(7.33752486401972,31.1229349256002,123.769320043193));
#120888=CARTESIAN_POINT('Ctrl Pts',(7.33751720695663,31.1228502372749,123.769242774548));
#120889=CARTESIAN_POINT('Ctrl Pts',(7.33751334000804,31.1228074680027,123.769203756445));
#120890=CARTESIAN_POINT('Ctrl Pts',(7.33750552526399,31.1227210348509,123.769124912351));
#120891=CARTESIAN_POINT('Ctrl Pts',(7.33750157745753,31.1226773708409,123.769085086412));
#120892=CARTESIAN_POINT('Ctrl Pts',(7.33749359666524,31.1225891002702,123.769004583437));
#120893=CARTESIAN_POINT('Ctrl Pts',(7.3374895636713,31.1225444936103,123.768963906496));
#120894=CARTESIAN_POINT('Ctrl Pts',(7.33748140788969,31.1224542866775,123.768881655515));
#120895=CARTESIAN_POINT('Ctrl Pts',(7.33747728511051,31.1224086864881,123.768840081751));
#120896=CARTESIAN_POINT('Ctrl Pts',(7.33746894485562,31.1223164382404,123.768755988263));
#120897=CARTESIAN_POINT('Ctrl Pts',(7.33746472737942,31.1222697901659,123.768713468739));
#120898=CARTESIAN_POINT('Ctrl Pts',(7.33745619252152,31.1221753885036,123.768627431842));
#120899=CARTESIAN_POINT('Ctrl Pts',(7.33745187511125,31.1221276345881,123.768583914403));
#120900=CARTESIAN_POINT('Ctrl Pts',(7.33744313479236,31.1220309593503,123.768495825976));
#120901=CARTESIAN_POINT('Ctrl Pts',(7.33743871187758,31.1219820379475,123.768451255166));
#120902=CARTESIAN_POINT('Ctrl Pts',(7.33742975457208,31.1218829615832,123.768361000491));
#120903=CARTESIAN_POINT('Ctrl Pts',(7.33742522016576,31.1218328064357,123.768315316728));
#120904=CARTESIAN_POINT('Ctrl Pts',(7.33741603348765,31.1217311918706,123.768222772565));
#120905=CARTESIAN_POINT('Ctrl Pts',(7.33741138118688,31.1216797321178,123.768175912153));
#120906=CARTESIAN_POINT('Ctrl Pts',(7.33740195183875,31.1215754321889,123.76808094624));
#120907=CARTESIAN_POINT('Ctrl Pts',(7.33739717479071,31.1215225919898,123.768032841037));
#120908=CARTESIAN_POINT('Ctrl Pts',(7.3373874885513,31.121415449308,123.767935311988));
#120909=CARTESIAN_POINT('Ctrl Pts',(7.3373825793752,31.1213611469773,123.767885888628));
#120910=CARTESIAN_POINT('Ctrl Pts',(7.33737262096932,31.1212509924865,123.767785644642));
#120911=CARTESIAN_POINT('Ctrl Pts',(7.33736757170755,31.1211951399545,123.767734824056));
#120912=CARTESIAN_POINT('Ctrl Pts',(7.33735732457755,31.1210817904038,123.76763170064));
#120913=CARTESIAN_POINT('Ctrl Pts',(7.33735212670209,31.1210242932854,123.767579398133));
#120914=CARTESIAN_POINT('Ctrl Pts',(7.33734157312457,31.1209075525183,123.767473219309));
#120915=CARTESIAN_POINT('Ctrl Pts',(7.33733621738728,31.1208483084581,123.76741934307));
#120916=CARTESIAN_POINT('Ctrl Pts',(7.33732533810009,31.1207279632852,123.767309917648));
#120917=CARTESIAN_POINT('Ctrl Pts',(7.33731981453915,31.1206668620269,123.767254368828));
#120918=CARTESIAN_POINT('Ctrl Pts',(7.33730858880094,31.1205426828837,123.767141491046));
#120919=CARTESIAN_POINT('Ctrl Pts',(7.33730288659491,31.1204796046552,123.767084162314));
#120920=CARTESIAN_POINT('Ctrl Pts',(7.33729129183352,31.1203513417109,123.76696760834));
#120921=CARTESIAN_POINT('Ctrl Pts',(7.33728539926978,31.1202861568746,123.766908383585));
#120922=CARTESIAN_POINT('Ctrl Pts',(7.33727341106456,31.1201535398343,123.76678791139));
#120923=CARTESIAN_POINT('Ctrl Pts',(7.33726731537992,31.1200861071227,123.766726664146));
#120924=CARTESIAN_POINT('Ctrl Pts',(7.33725490705958,31.1199488407774,123.766602009512));
#120925=CARTESIAN_POINT('Ctrl Pts',(7.33724859438879,31.1198790067224,123.766538602469));
#120926=CARTESIAN_POINT('Ctrl Pts',(7.33723573693869,31.1197367699204,123.766409478129));
#120927=CARTESIAN_POINT('Ctrl Pts',(7.33722919213803,31.1196643669009,123.766343761393));
#120928=CARTESIAN_POINT('Ctrl Pts',(7.33721585387418,31.1195168089391,123.766209853824));
#120929=CARTESIAN_POINT('Ctrl Pts',(7.33720906037137,31.1194416535188,123.766141663453));
#120930=CARTESIAN_POINT('Ctrl Pts',(7.33719520656172,31.1192883899504,123.766002629159));
#120931=CARTESIAN_POINT('Ctrl Pts',(7.33718814621274,31.1192102812924,123.765931785771));
#120932=CARTESIAN_POINT('Ctrl Pts',(7.3371737387784,31.1190508906176,123.765787248386));
#120933=CARTESIAN_POINT('Ctrl Pts',(7.3371663916499,31.1189696080753,123.765713555028));
#120934=CARTESIAN_POINT('Ctrl Pts',(7.33715138871921,31.1188036268043,123.765563100958));
#120935=CARTESIAN_POINT('Ctrl Pts',(7.33714373286178,31.118718927411,123.765486340894));
#120936=CARTESIAN_POINT('Ctrl Pts',(7.3371280882549,31.1185458443574,123.765329514286));
#120937=CARTESIAN_POINT('Ctrl Pts',(7.33712009945392,31.1184574600676,123.765249448576));
#120938=CARTESIAN_POINT('Ctrl Pts',(7.33710376216209,31.1182767105816,123.765085746257));
#120939=CARTESIAN_POINT('Ctrl Pts',(7.33709541361698,31.1181843447192,123.765002110629));
#120940=CARTESIAN_POINT('Ctrl Pts',(7.33707832712759,31.1179953032151,123.764830975538));
#120941=CARTESIAN_POINT('Ctrl Pts',(7.33706958909751,31.1178986265508,123.764743476942));
#120942=CARTESIAN_POINT('Ctrl Pts',(7.3370516905616,31.117700597289,123.764564290018));
#120943=CARTESIAN_POINT('Ctrl Pts',(7.33704252998437,31.1175992438194,123.764472602937));
#120944=CARTESIAN_POINT('Ctrl Pts',(7.33663051097191,31.1130405871212,123.760349739096));
#120945=CARTESIAN_POINT('Ctrl Pts',(7.33622583397279,31.1085617479838,123.756342906941));
#120946=CARTESIAN_POINT('Ctrl Pts',(7.33529421312361,31.098247376848,123.747215512927));
#120947=CARTESIAN_POINT('Ctrl Pts',(7.33476611633774,31.0923976802799,123.742111462052));
#120948=CARTESIAN_POINT('Ctrl Pts',(7.3331321883631,31.0742834723832,123.726527872219));
#120949=CARTESIAN_POINT('Ctrl Pts',(7.33201734982392,31.0619026608961,123.716185788276));
#120950=CARTESIAN_POINT('Ctrl Pts',(7.325242972604,30.986433384442,123.654982481198));
#120951=CARTESIAN_POINT('Ctrl Pts',(7.31936056575535,30.9198580235857,123.608604409793));
#120952=CARTESIAN_POINT('Ctrl Pts',(7.30809836245104,30.7867863116177,123.529640447671));
#120953=CARTESIAN_POINT('Ctrl Pts',(7.30273291631078,30.7209613298933,123.496269310114));
#120954=CARTESIAN_POINT('Ctrl Pts',(7.29443950023808,30.6140478668175,123.450707626018));
#120955=CARTESIAN_POINT('Ctrl Pts',(7.29144360593981,30.5743311312966,123.435549330816));
#120956=CARTESIAN_POINT('Ctrl Pts',(7.28637064825851,30.505096592487,123.412117956902));
#120957=CARTESIAN_POINT('Ctrl Pts',(7.28427210425098,30.4758517140761,123.403110113347));
#120958=CARTESIAN_POINT('Ctrl Pts',(7.28125274878252,30.4329080379419,123.391167511752));
#120959=CARTESIAN_POINT('Ctrl Pts',(7.28031149801141,30.4193955435292,123.387592252779));
#120960=CARTESIAN_POINT('Ctrl Pts',(7.2786567825405,30.3954242970259,123.381571459597));
#120961=CARTESIAN_POINT('Ctrl Pts',(7.27794111295128,30.3849840506785,123.379056260978));
#120962=CARTESIAN_POINT('Ctrl Pts',(7.27644417505223,30.3629979808563,123.373983921072));
#120963=CARTESIAN_POINT('Ctrl Pts',(7.27566363458848,30.3514477443983,123.37144839869));
#120964=CARTESIAN_POINT('Ctrl Pts',(7.27359930557026,30.320679814854,123.365036770782));
#120965=CARTESIAN_POINT('Ctrl Pts',(7.2723224001043,30.3014186786258,123.361376450386));
#120966=CARTESIAN_POINT('Ctrl Pts',(7.26571999820734,30.2007296445294,123.344077405669));
#120967=CARTESIAN_POINT('Ctrl Pts',(7.26057778543781,30.1184307844295,123.336164471575));
#120968=CARTESIAN_POINT('Ctrl Pts',(7.24935294498439,29.9357146444029,123.332228951831));
#120969=CARTESIAN_POINT('Ctrl Pts',(7.24332887437045,29.8355699653185,123.339110691048));
#120970=CARTESIAN_POINT('Ctrl Pts',(7.23527606601592,29.7087343964665,123.359414741836));
#120971=CARTESIAN_POINT('Ctrl Pts',(7.23348337380518,29.6809318527754,123.364594552332));
#120972=CARTESIAN_POINT('Ctrl Pts',(7.23041617170141,29.6343966103914,123.374496158519));
#120973=CARTESIAN_POINT('Ctrl Pts',(7.22915798482784,29.6155892186855,123.378840892919));
#120974=CARTESIAN_POINT('Ctrl Pts',(7.22733980331298,29.5888910660702,123.38549916653));
#120975=CARTESIAN_POINT('Ctrl Pts',(7.22679385707214,29.5809345988379,123.387546069066));
#120976=CARTESIAN_POINT('Ctrl Pts',(7.22583986229258,29.5671429294275,123.391203121538));
#120977=CARTESIAN_POINT('Ctrl Pts',(7.22543334298627,29.5613008356146,123.39278636096));
#120978=CARTESIAN_POINT('Ctrl Pts',(7.22455605382618,29.5487701592848,123.396255655983));
#120979=CARTESIAN_POINT('Ctrl Pts',(7.22408475816362,29.5420848112174,123.398151703314));
#120980=CARTESIAN_POINT('Ctrl Pts',(7.22277458222512,29.5236222156625,123.403512944597));
#120981=CARTESIAN_POINT('Ctrl Pts',(7.22193095520257,29.5118713847495,123.407066497199));
#120982=CARTESIAN_POINT('Ctrl Pts',(7.21600299706765,29.4301802168941,123.432759364924));
#120983=CARTESIAN_POINT('Ctrl Pts',(7.21071556310233,29.3617367273716,123.459365259678));
#120984=CARTESIAN_POINT('Ctrl Pts',(7.20436849991623,29.2825747268916,123.496320015939));
#120985=CARTESIAN_POINT('Ctrl Pts',(7.20334863341958,29.2699476203082,123.502409923847));
#120986=CARTESIAN_POINT('Ctrl Pts',(7.19696312729404,29.1914119613713,123.541516098445));
#120987=CARTESIAN_POINT('Ctrl Pts',(7.19159768383466,29.1276743327996,123.578719186341));
#120988=CARTESIAN_POINT('Ctrl Pts',(7.18330426215173,29.0314098772701,123.643830826896));
#120989=CARTESIAN_POINT('Ctrl Pts',(7.18030836001311,28.9971337095694,123.668977326521));
#120990=CARTESIAN_POINT('Ctrl Pts',(7.17523539068563,28.9398975297436,123.714436035617));
#120991=CARTESIAN_POINT('Ctrl Pts',(7.17313684273824,28.9164682313566,123.734120434774));
#120992=CARTESIAN_POINT('Ctrl Pts',(7.17011748274211,28.8831435732529,123.763722091573));
#120993=CARTESIAN_POINT('Ctrl Pts',(7.16917623129671,28.8728111431952,123.773135440809));
#120994=CARTESIAN_POINT('Ctrl Pts',(7.16752151506618,28.8547516608461,123.790009274101));
#120995=CARTESIAN_POINT('Ctrl Pts',(7.16680584538502,28.8469761171536,123.797416427036));
#120996=CARTESIAN_POINT('Ctrl Pts',(7.16530890770955,28.8307901709854,123.813136823953));
#120997=CARTESIAN_POINT('Ctrl Pts',(7.16452836755698,28.8223955379555,123.821465500705));
#120998=CARTESIAN_POINT('Ctrl Pts',(7.16246404033559,28.8003214488568,123.843837521118));
#120999=CARTESIAN_POINT('Ctrl Pts',(7.16118713633342,28.7867997207624,123.858034396872));
#121000=CARTESIAN_POINT('Ctrl Pts',(7.1545847848286,28.7176564481081,123.933244677546));
#121001=CARTESIAN_POINT('Ctrl Pts',(7.14944261726476,28.6663729256509,123.998095205464));
#121002=CARTESIAN_POINT('Ctrl Pts',(7.13821777982035,28.5639676879752,124.149468279496));
#121003=CARTESIAN_POINT('Ctrl Pts',(7.13219367110133,28.5154340626107,124.237337136652));
#121004=CARTESIAN_POINT('Ctrl Pts',(7.12414081692024,28.4637009922747,124.354910080149));
#121005=CARTESIAN_POINT('Ctrl Pts',(7.12234811960874,28.4529736390788,124.381077626699));
#121006=CARTESIAN_POINT('Ctrl Pts',(7.11928090965876,28.4360533164031,124.425544301422));
#121007=CARTESIAN_POINT('Ctrl Pts',(7.11802272014844,28.4295030479053,124.443701676865));
#121008=CARTESIAN_POINT('Ctrl Pts',(7.11620453548328,28.4206168180352,124.469743211761));
#121009=CARTESIAN_POINT('Ctrl Pts',(7.11565858879512,28.4180212055672,124.477537959357));
#121010=CARTESIAN_POINT('Ctrl Pts',(7.1147045935116,28.4136135458241,124.49110840279));
#121011=CARTESIAN_POINT('Ctrl Pts',(7.11429807415367,28.411775151991,124.496875293265));
#121012=CARTESIAN_POINT('Ctrl Pts',(7.11342078521269,28.4078936697478,124.509284478302));
#121013=CARTESIAN_POINT('Ctrl Pts',(7.11294948982388,28.4058607300169,124.515929474603));
#121014=CARTESIAN_POINT('Ctrl Pts',(7.1116393153706,28.4003514992859,124.534348429388));
#121015=CARTESIAN_POINT('Ctrl Pts',(7.11079568957607,28.396963769312,124.546148116624));
#121016=CARTESIAN_POINT('Ctrl Pts',(7.10486806103463,28.3742443689039,124.628710724814));
#121017=CARTESIAN_POINT('Ctrl Pts',(7.09958098154403,28.3594764950987,124.700638441158));
#121018=CARTESIAN_POINT('Ctrl Pts',(7.09323401074213,28.3475885882259,124.787187540729));
#121019=CARTESIAN_POINT('Ctrl Pts',(7.09221388604955,28.3458559820897,124.801102586954));
#121020=CARTESIAN_POINT('Ctrl Pts',(7.08582814571166,28.3361153134979,124.888296782242));
#121021=CARTESIAN_POINT('Ctrl Pts',(7.08046272403968,28.3328020794517,124.962022821129));
#121022=CARTESIAN_POINT('Ctrl Pts',(7.07216925686224,28.3352945104118,125.078213545914));
#121023=CARTESIAN_POINT('Ctrl Pts',(7.06917329110161,28.3378309850588,125.120649879804));
#121024=CARTESIAN_POINT('Ctrl Pts',(7.06410022726345,28.3449800198226,125.193392985981));
#121025=CARTESIAN_POINT('Ctrl Pts',(7.0620016473404,28.3488105636538,125.223753526165));
#121026=CARTESIAN_POINT('Ctrl Pts',(7.05898225059248,28.3556061714426,125.26780642944));
#121027=CARTESIAN_POINT('Ctrl Pts',(7.05804099366769,28.3579108058421,125.281592695485));
#121028=CARTESIAN_POINT('Ctrl Pts',(7.05638627125911,28.3622924433477,125.305917103472));
#121029=CARTESIAN_POINT('Ctrl Pts',(7.05567060082343,28.3642983388838,125.316467060556));
#121030=CARTESIAN_POINT('Ctrl Pts',(7.05417366494116,28.368727042303,125.338591729773));
#121031=CARTESIAN_POINT('Ctrl Pts',(7.05339312730385,28.3711713676912,125.350161563697));
#121032=CARTESIAN_POINT('Ctrl Pts',(7.05132881462839,28.3779948250668,125.380840529399));
#121033=CARTESIAN_POINT('Ctrl Pts',(7.05005192247959,28.3825884864676,125.399900418676));
#121034=CARTESIAN_POINT('Ctrl Pts',(7.04344997908207,28.4082734333065,125.498775924849));
#121035=CARTESIAN_POINT('Ctrl Pts',(7.03830817762255,28.4349403681072,125.57702835479));
#121036=CARTESIAN_POINT('Ctrl Pts',(7.02708336464363,28.5065722764158,125.745162879906));
#121037=CARTESIAN_POINT('Ctrl Pts',(7.02105894741988,28.5540737781649,125.83360008448));
#121038=CARTESIAN_POINT('Ctrl Pts',(7.01300572222854,28.6247968715355,125.940835819651));
#121039=CARTESIAN_POINT('Ctrl Pts',(7.0112129836221,28.6409635887543,125.964041252593));
#121040=CARTESIAN_POINT('Ctrl Pts',(7.00814571014895,28.6691455701068,126.002374719431));
#121041=CARTESIAN_POINT('Ctrl Pts',(7.00688749929019,28.6808479366916,126.017726067114));
#121042=CARTESIAN_POINT('Ctrl Pts',(7.00506928911407,28.6979072297578,126.039316080675));
#121043=CARTESIAN_POINT('Ctrl Pts',(7.0045233387998,28.7030482034408,126.045724403592));
#121044=CARTESIAN_POINT('Ctrl Pts',(7.00356933942795,28.7120588057818,126.056787641877));
#121045=CARTESIAN_POINT('Ctrl Pts',(7.00316281964853,28.7159067466625,126.061459916897));
#121046=CARTESIAN_POINT('Ctrl Pts',(7.00228553247384,28.7242270497817,126.071451197729));
#121047=CARTESIAN_POINT('Ctrl Pts',(7.00181423929839,28.7287071857878,126.076763142828));
#121048=CARTESIAN_POINT('Ctrl Pts',(7.00050407685232,28.7411936276725,126.091381337829));
#121049=CARTESIAN_POINT('Ctrl Pts',(6.9996604609868,28.7492695796623,126.100627139911));
#121050=CARTESIAN_POINT('Ctrl Pts',(6.99373549318338,28.8062862196025,126.164465068223));
#121051=CARTESIAN_POINT('Ctrl Pts',(6.98845127521954,28.8586770632103,126.215858156313));
#121052=CARTESIAN_POINT('Ctrl Pts',(6.98210506099176,28.924931834679,126.272785079067));
#121053=CARTESIAN_POINT('Ctrl Pts',(6.98108286271784,28.9357042530065,126.281806528618));
#121054=CARTESIAN_POINT('Ctrl Pts',(6.97469524803576,29.0036959012725,126.337298620006));
#121055=CARTESIAN_POINT('Ctrl Pts',(6.96933000756723,29.0638362738374,126.380068203777));
#121056=CARTESIAN_POINT('Ctrl Pts',(6.96103616855051,29.1628073348391,126.44099645199));
#121057=CARTESIAN_POINT('Ctrl Pts',(6.9580396799083,29.1998415299242,126.461885514717));
#121058=CARTESIAN_POINT('Ctrl Pts',(6.95296583934262,29.2648429102593,126.495338177166));
#121059=CARTESIAN_POINT('Ctrl Pts',(6.95086699663923,29.2924309584427,126.508588239233));
#121060=CARTESIAN_POINT('Ctrl Pts',(6.94784729786394,29.3331313667887,126.526773588747));
#121061=CARTESIAN_POINT('Ctrl Pts',(6.94690599591197,29.3459643438783,126.532314832681));
#121062=CARTESIAN_POINT('Ctrl Pts',(6.94525122273482,29.368777439849,126.541826642866));
#121063=CARTESIAN_POINT('Ctrl Pts',(6.94453554609937,29.3787289130146,126.545863371341));
#121064=CARTESIAN_POINT('Ctrl Pts',(6.94303862495206,29.3997185398932,126.554142201648));
#121065=CARTESIAN_POINT('Ctrl Pts',(6.94225810798242,29.4107642624478,126.558363587875));
#121066=CARTESIAN_POINT('Ctrl Pts',(6.94019391482633,29.4402380281446,126.569269502409));
#121067=CARTESIAN_POINT('Ctrl Pts',(6.93891712007254,29.4587410380198,126.575747132319));
#121068=CARTESIAN_POINT('Ctrl Pts',(6.93231851969021,29.555691736407,126.60777881817));
#121069=CARTESIAN_POINT('Ctrl Pts',(6.92717971701196,29.635848047797,126.627807851358));
#121070=CARTESIAN_POINT('Ctrl Pts',(6.91595510354097,29.8159463599422,126.658833067378));
#121071=CARTESIAN_POINT('Ctrl Pts',(6.90992815877011,29.9160530124556,126.666899351068));
#121072=CARTESIAN_POINT('Ctrl Pts',(6.90187189401322,30.0445535772375,126.665644312603));
#121073=CARTESIAN_POINT('Ctrl Pts',(6.90007881719033,30.0728232683213,126.664647887263));
#121074=CARTESIAN_POINT('Ctrl Pts',(6.89701102345314,30.1203220694846,126.66176150438));
#121075=CARTESIAN_POINT('Ctrl Pts',(6.89575263775295,30.1395690963481,126.660255729475));
#121076=CARTESIAN_POINT('Ctrl Pts',(6.89393421864653,30.1669633521387,126.657632873839));
#121077=CARTESIAN_POINT('Ctrl Pts',(6.89338823863804,30.1751359997823,126.656789328783));
#121078=CARTESIAN_POINT('Ctrl Pts',(6.89243420578799,30.1893182496334,126.655219393568));
#121079=CARTESIAN_POINT('Ctrl Pts',(6.89202768255808,30.1953306744409,126.654520645615));
#121080=CARTESIAN_POINT('Ctrl Pts',(6.89115040984466,30.2082372197349,126.652949347782));
#121081=CARTESIAN_POINT('Ctrl Pts',(6.89067913479338,30.2151296248998,126.652066441189));
#121082=CARTESIAN_POINT('Ctrl Pts',(6.88936907066973,30.2341818028201,126.649504641502));
#121083=CARTESIAN_POINT('Ctrl Pts',(6.88852553610683,30.2463285675887,126.647734473086));
#121084=CARTESIAN_POINT('Ctrl Pts',(6.88262205409705,30.3305789933017,126.634504143708));
#121085=CARTESIAN_POINT('Ctrl Pts',(6.87736093849703,30.4018736043471,126.618450342471));
#121086=CARTESIAN_POINT('Ctrl Pts',(6.87107463938203,30.4848628382286,126.593940829652));
#121087=CARTESIAN_POINT('Ctrl Pts',(6.87008964816212,30.4978013753195,126.58994752353));
#121088=CARTESIAN_POINT('Ctrl Pts',(6.86362718487559,30.582321842406,126.562728569554));
#121089=CARTESIAN_POINT('Ctrl Pts',(6.85814853884835,30.6523132682235,126.534831623407));
#121090=CARTESIAN_POINT('Ctrl Pts',(6.84977679037718,30.7581409439591,126.484099163215));
#121091=CARTESIAN_POINT('Ctrl Pts',(6.84680997441759,30.7953989999941,126.464468824276));
#121092=CARTESIAN_POINT('Ctrl Pts',(6.84178024959967,30.8582018681293,126.428274759587));
#121093=CARTESIAN_POINT('Ctrl Pts',(6.8396963540326,30.8841090837144,126.41238471123));
#121094=CARTESIAN_POINT('Ctrl Pts',(6.83669384249032,30.92124792151,126.388183199477));
#121095=CARTESIAN_POINT('Ctrl Pts',(6.83575510821472,30.9328314650066,126.380425951147));
#121096=CARTESIAN_POINT('Ctrl Pts',(6.83410322754093,30.9531596381203,126.366439870816));
#121097=CARTESIAN_POINT('Ctrl Pts',(6.83338790187141,30.9619438516806,126.360270286297));
#121098=CARTESIAN_POINT('Ctrl Pts',(6.83189012725186,30.9802932433207,126.347115961736));
#121099=CARTESIAN_POINT('Ctrl Pts',(6.83110842115497,30.9898448349546,126.3401132311));
#121100=CARTESIAN_POINT('Ctrl Pts',(6.82903735147019,31.015075643772,126.321198370588));
#121101=CARTESIAN_POINT('Ctrl Pts',(6.82775495332686,31.0306200269001,126.309108899393));
#121102=CARTESIAN_POINT('Ctrl Pts',(6.82092609152769,31.1128789379639,126.242759404361));
#121103=CARTESIAN_POINT('Ctrl Pts',(6.81558017414355,31.1755349768754,126.183668323503));
#121104=CARTESIAN_POINT('Ctrl Pts',(6.80433853084959,31.29872263266,126.048012513782));
#121105=CARTESIAN_POINT('Ctrl Pts',(6.79848421968039,31.3576589359036,125.970448689836));
#121106=CARTESIAN_POINT('Ctrl Pts',(6.79063591558927,31.4243653675363,125.864591020742));
#121107=CARTESIAN_POINT('Ctrl Pts',(6.7888663935003,31.438642908284,125.840619260776));
#121108=CARTESIAN_POINT('Ctrl Pts',(6.78583486244883,31.4616762200661,125.799639888896));
#121109=CARTESIAN_POINT('Ctrl Pts',(6.78458868662136,31.4707534644218,125.782818941596));
#121110=CARTESIAN_POINT('Ctrl Pts',(6.78278486352893,31.4833010033453,125.75857834966));
#121111=CARTESIAN_POINT('Ctrl Pts',(6.78224096436679,31.487009451346,125.751282812117));
#121112=CARTESIAN_POINT('Ctrl Pts',(6.7812892735369,31.4933651826408,125.738547915569));
#121113=CARTESIAN_POINT('Ctrl Pts',(6.78088298811303,31.4960368353003,125.733120984802));
#121114=CARTESIAN_POINT('Ctrl Pts',(6.78000468412576,31.501722101558,125.721411998494));
#121115=CARTESIAN_POINT('Ctrl Pts',(6.77953212498298,31.5047258371292,125.715125648064));
#121116=CARTESIAN_POINT('Ctrl Pts',(6.77821508872227,31.5129475856079,125.697637662293));
#121117=CARTESIAN_POINT('Ctrl Pts',(6.77736578751824,31.518080407234,125.686396794351));
#121118=CARTESIAN_POINT('Ctrl Pts',(6.77402885444147,31.5376112153215,125.642333519064));
#121119=CARTESIAN_POINT('Ctrl Pts',(6.77149705255902,31.5510682071831,125.609119092788));
#121120=CARTESIAN_POINT('Ctrl Pts',(6.76893575384937,31.5634399863339,125.575509695081));
#121121=CARTESIAN_POINT('Origin',(5.,30.,125.));
#121122=CARTESIAN_POINT('',(6.06644911688889,31.5634400025946,125.575509650907));
#121123=CARTESIAN_POINT('',(6.2618827359479,31.5634400889265,125.575509416376));
#121124=CARTESIAN_POINT('',(5.,31.5634400119422,125.575509625513));
#121125=CARTESIAN_POINT('',(6.92206962423701,31.6659991809955,124.998531923256));
#121126=CARTESIAN_POINT('Ctrl Pts',(6.26188273594789,31.5634400889265,125.575509416376));
#121127=CARTESIAN_POINT('Ctrl Pts',(6.26453323098372,31.5505030333263,125.610654473577));
#121128=CARTESIAN_POINT('Ctrl Pts',(6.2671531022909,31.5363776686696,125.64537214447));
#121129=CARTESIAN_POINT('Ctrl Pts',(6.27126998919214,31.5120106847638,125.699910324414));
#121130=CARTESIAN_POINT('Ctrl Pts',(6.27278958688585,31.5025308545777,125.720036031566));
#121131=CARTESIAN_POINT('Ctrl Pts',(6.27522187622556,31.4865717375308,125.752228536729));
#121132=CARTESIAN_POINT('Ctrl Pts',(6.27614302640899,31.4803420518802,125.764415287089));
#121133=CARTESIAN_POINT('Ctrl Pts',(6.27777544030934,31.4689721799572,125.78599705788));
#121134=CARTESIAN_POINT('Ctrl Pts',(6.27848870313448,31.4638903219023,125.795421759269));
#121135=CARTESIAN_POINT('Ctrl Pts',(6.2799936941221,31.4529272351232,125.815292671185));
#121136=CARTESIAN_POINT('Ctrl Pts',(6.28078456652666,31.447023385029,125.825725757171));
#121137=CARTESIAN_POINT('Ctrl Pts',(6.28290792070682,31.4307905732418,125.853702979776));
#121138=CARTESIAN_POINT('Ctrl Pts',(6.28423278823446,31.4202515977551,125.871123355166));
#121139=CARTESIAN_POINT('Ctrl Pts',(6.28714785562688,31.3961720472937,125.909326465987));
#121140=CARTESIAN_POINT('Ctrl Pts',(6.28873250811245,31.3824812442445,125.930008984485));
#121141=CARTESIAN_POINT('Ctrl Pts',(6.29372835811387,31.3374866682258,125.994791115195));
#121142=CARTESIAN_POINT('Ctrl Pts',(6.29708363774178,31.3044947913601,126.037677183274));
#121143=CARTESIAN_POINT('Ctrl Pts',(6.30407114563171,31.2308770651783,126.124299695415));
#121144=CARTESIAN_POINT('Ctrl Pts',(6.30769132644786,31.1898716407773,126.167610234891));
#121145=CARTESIAN_POINT('Ctrl Pts',(6.31634451591232,31.0873952216886,126.264830117245));
#121146=CARTESIAN_POINT('Ctrl Pts',(6.32139183620691,31.0241127901276,126.316591446482));
#121147=CARTESIAN_POINT('Ctrl Pts',(6.32753065126077,30.9471827882536,126.370603381623));
#121148=CARTESIAN_POINT('Ctrl Pts',(6.32834449073214,30.9369855006192,126.377594647753));
#121149=CARTESIAN_POINT('Ctrl Pts',(6.32962849585779,30.9209195993999,126.388348541046));
#121150=CARTESIAN_POINT('Ctrl Pts',(6.33009370048239,30.9151033358208,126.392189089291));
#121151=CARTESIAN_POINT('Ctrl Pts',(6.33096737387406,30.9041928781788,126.399295485162));
#121152=CARTESIAN_POINT('Ctrl Pts',(6.33137525262167,30.8991047701905,126.402570220464));
#121153=CARTESIAN_POINT('Ctrl Pts',(6.33233922137343,30.8870913130234,126.410209918899));
#121154=CARTESIAN_POINT('Ctrl Pts',(6.33289677364094,30.8801515104572,126.414551633784));
#121155=CARTESIAN_POINT('Ctrl Pts',(6.33476646386004,30.8568993759404,126.428861404817));
#121156=CARTESIAN_POINT('Ctrl Pts',(6.33609186639121,30.8404481684083,126.43859940693));
#121157=CARTESIAN_POINT('Ctrl Pts',(6.33938397300423,30.7995810649746,126.46184975642));
#121158=CARTESIAN_POINT('Ctrl Pts',(6.34136484092547,30.7749866741457,126.475035616516));
#121159=CARTESIAN_POINT('Ctrl Pts',(6.35032886249905,30.6632367264032,126.531382034958));
#121160=CARTESIAN_POINT('Ctrl Pts',(6.35747773264583,30.5727331987659,126.567479107099));
#121161=CARTESIAN_POINT('Ctrl Pts',(6.37070495662873,30.3972865369762,126.620218098892));
#121162=CARTESIAN_POINT('Ctrl Pts',(6.37679326992271,30.3131741211006,126.638557104524));
#121163=CARTESIAN_POINT('Ctrl Pts',(6.38402546998996,30.2085020180894,126.653018670417));
#121164=CARTESIAN_POINT('Ctrl Pts',(6.38536258494941,30.1889473276658,126.655367868903));
#121165=CARTESIAN_POINT('Ctrl Pts',(6.38748661161821,30.1575701563187,126.658574078676));
#121166=CARTESIAN_POINT('Ctrl Pts',(6.388280381661,30.1457727188137,126.659652570755));
#121167=CARTESIAN_POINT('Ctrl Pts',(6.38978611472357,30.1232618295957,126.661468571554));
#121168=CARTESIAN_POINT('Ctrl Pts',(6.39049874344686,30.1125508419617,126.66222850718));
#121169=CARTESIAN_POINT('Ctrl Pts',(6.39212956673031,30.0879130012123,126.663737298468));
#121170=CARTESIAN_POINT('Ctrl Pts',(6.39304549550791,30.0739824717173,126.664414944528));
#121171=CARTESIAN_POINT('Ctrl Pts',(6.39594149479883,30.0296602633358,126.666013410678));
#121172=CARTESIAN_POINT('Ctrl Pts',(6.39790121280371,29.9992501158025,126.666277299375));
#121173=CARTESIAN_POINT('Ctrl Pts',(6.40252402836766,29.9267261118602,126.664920967144));
#121174=CARTESIAN_POINT('Ctrl Pts',(6.40516504666239,29.8846471549676,126.662535708677));
#121175=CARTESIAN_POINT('Ctrl Pts',(6.41245305829984,29.7676578177247,126.65144037819));
#121176=CARTESIAN_POINT('Ctrl Pts',(6.41702657266004,29.6931832877958,126.639238265844));
#121177=CARTESIAN_POINT('Ctrl Pts',(6.42242697299816,29.6072559608185,126.619096614067));
#121178=CARTESIAN_POINT('Ctrl Pts',(6.42321578123079,29.5947567912209,126.616013509519));
#121179=CARTESIAN_POINT('Ctrl Pts',(6.42852037429965,29.5111563866242,126.594361328546));
#121180=CARTESIAN_POINT('Ctrl Pts',(6.43308895516093,29.4413236799063,126.571252417981));
#121181=CARTESIAN_POINT('Ctrl Pts',(6.43868997878531,29.3618765073843,126.53899486264));
#121182=CARTESIAN_POINT('Ctrl Pts',(6.43949837093124,29.3505511643521,126.534249968932));
#121183=CARTESIAN_POINT('Ctrl Pts',(6.44077562084146,29.3328987137899,126.52662378816));
#121184=CARTESIAN_POINT('Ctrl Pts',(6.44123960134599,29.3265351710516,126.523827233131));
#121185=CARTESIAN_POINT('Ctrl Pts',(6.44211234169883,29.3146613139832,126.518520184515));
#121186=CARTESIAN_POINT('Ctrl Pts',(6.44252052717498,29.3091469461265,126.51601936617));
#121187=CARTESIAN_POINT('Ctrl Pts',(6.44348707937824,29.2961796725674,126.510053145173));
#121188=CARTESIAN_POINT('Ctrl Pts',(6.44404693248017,29.2887386444359,126.506562587998));
#121189=CARTESIAN_POINT('Ctrl Pts',(6.4459326113132,29.2638991334082,126.494685437374));
#121190=CARTESIAN_POINT('Ctrl Pts',(6.44727200104214,29.2466214371786,126.486051716484));
#121191=CARTESIAN_POINT('Ctrl Pts',(6.45060665406564,29.2044072083047,126.464031760517));
#121192=CARTESIAN_POINT('Ctrl Pts',(6.45261652320512,29.1796546718011,126.450306949463));
#121193=CARTESIAN_POINT('Ctrl Pts',(6.46183393868985,29.0687809783488,126.385083042454));
#121194=CARTESIAN_POINT('Ctrl Pts',(6.4692141542084,28.9870703369412,126.326498349653));
#121195=CARTESIAN_POINT('Ctrl Pts',(6.48238623938157,28.8487927532436,126.207087800662));
#121196=CARTESIAN_POINT('Ctrl Pts',(6.48821088004376,28.7905285921975,126.148704342915));
#121197=CARTESIAN_POINT('Ctrl Pts',(6.49519001018681,28.7240349991667,126.071379266078));
#121198=CARTESIAN_POINT('Ctrl Pts',(6.49652076142678,28.7115176079655,126.056292287906));
#121199=CARTESIAN_POINT('Ctrl Pts',(6.49863715773475,28.6918791743119,126.031753736607));
#121200=CARTESIAN_POINT('Ctrl Pts',(6.49942957417504,28.6845878073523,126.02244151105));
#121201=CARTESIAN_POINT('Ctrl Pts',(6.50093425479178,28.6708639055627,126.004524086572));
#121202=CARTESIAN_POINT('Ctrl Pts',(6.50164716877997,28.6644142669889,125.99593280749));
#121203=CARTESIAN_POINT('Ctrl Pts',(6.50328077809434,28.6497605818281,125.976014901765));
#121204=CARTESIAN_POINT('Ctrl Pts',(6.50419918025611,28.6416150822143,125.964646054125));
#121205=CARTESIAN_POINT('Ctrl Pts',(6.5071119256167,28.6160913479543,125.928057536032));
#121206=CARTESIAN_POINT('Ctrl Pts',(6.50908557121767,28.5992643440476,125.90245983752));
#121207=CARTESIAN_POINT('Ctrl Pts',(6.51374832126198,28.5607667677671,125.840222830019));
#121208=CARTESIAN_POINT('Ctrl Pts',(6.51641479894631,28.5397754581317,125.803188252582));
#121209=CARTESIAN_POINT('Ctrl Pts',(6.52362148459172,28.4863692014257,125.699934417149));
#121210=CARTESIAN_POINT('Ctrl Pts',(6.52809430880673,28.4568936053249,125.632304831701));
#121211=CARTESIAN_POINT('Ctrl Pts',(6.5334621940821,28.4272451267642,125.549723098583));
#121212=CARTESIAN_POINT('Ctrl Pts',(6.53432290077695,28.4226653916835,125.536440960096));
#121213=CARTESIAN_POINT('Ctrl Pts',(6.53968555690888,28.3952555125483,125.453559589253));
#121214=CARTESIAN_POINT('Ctrl Pts',(6.54424008350693,28.376870929878,125.382583954629));
#121215=CARTESIAN_POINT('Ctrl Pts',(6.54982550579754,28.3609274233676,125.298576364644));
#121216=CARTESIAN_POINT('Ctrl Pts',(6.55063384008586,28.3587715387297,125.286488870896));
#121217=CARTESIAN_POINT('Ctrl Pts',(6.55191101823856,28.3556047751723,125.267523192279));
#121218=CARTESIAN_POINT('Ctrl Pts',(6.55237498572978,28.3545029651142,125.260660349208));
#121219=CARTESIAN_POINT('Ctrl Pts',(6.55324771624495,28.3525217295595,125.247806404879));
#121220=CARTESIAN_POINT('Ctrl Pts',(6.55365590506358,28.351631979949,125.241817145095));
#121221=CARTESIAN_POINT('Ctrl Pts',(6.55462248509758,28.3496114358677,125.227686512057));
#121222=CARTESIAN_POINT('Ctrl Pts',(6.55518236294708,28.3485082214955,125.219541474079));
#121223=CARTESIAN_POINT('Ctrl Pts',(6.55706821431895,28.3450144030586,125.192228506631));
#121224=CARTESIAN_POINT('Ctrl Pts',(6.55840775508845,28.3428970003459,125.173028014631));
#121225=CARTESIAN_POINT('Ctrl Pts',(6.56174286848806,28.3385011081693,125.125612744714));
#121226=CARTESIAN_POINT('Ctrl Pts',(6.56375305178258,28.3366070086541,125.09736890993));
#121227=CARTESIAN_POINT('Ctrl Pts',(6.5729732626186,28.3312706460676,124.968805515804));
#121228=CARTESIAN_POINT('Ctrl Pts',(6.5803560357767,28.3361793615962,124.868348519008));
#121229=CARTESIAN_POINT('Ctrl Pts',(6.59352754570157,28.3615173680557,124.687418324636));
#121230=CARTESIAN_POINT('Ctrl Pts',(6.59934931514316,28.3789623229815,124.606842074978));
#121231=CARTESIAN_POINT('Ctrl Pts',(6.60632566981298,28.4078517187159,124.50907839942));
#121232=CARTESIAN_POINT('Ctrl Pts',(6.60765633670465,28.4137376553053,124.490380535847));
#121233=CARTESIAN_POINT('Ctrl Pts',(6.60977263186832,28.4237019717756,124.460574020175));
#121234=CARTESIAN_POINT('Ctrl Pts',(6.61056503036285,28.4275709375132,124.449397859226));
#121235=CARTESIAN_POINT('Ctrl Pts',(6.61206969710485,28.4351807621224,124.428150236314));
#121236=CARTESIAN_POINT('Ctrl Pts',(6.61278261495284,28.4389006562751,124.418071956595));
#121237=CARTESIAN_POINT('Ctrl Pts',(6.61441626159378,28.4476871690297,124.394957469147));
#121238=CARTESIAN_POINT('Ctrl Pts',(6.61533469685582,28.4528210240405,124.381947554457));
#121239=CARTESIAN_POINT('Ctrl Pts',(6.61824766681568,28.4697189036466,124.340656466048));
#121240=CARTESIAN_POINT('Ctrl Pts',(6.62022149926635,28.4820996323642,124.312633436655));
#121241=CARTESIAN_POINT('Ctrl Pts',(6.62488478589524,28.5135121920068,124.24652725224));
#121242=CARTESIAN_POINT('Ctrl Pts',(6.62755160590334,28.5332447520683,124.208800525387));
#121243=CARTESIAN_POINT('Ctrl Pts',(6.63475845347621,28.5910305894367,124.107928692374));
#121244=CARTESIAN_POINT('Ctrl Pts',(6.6392311204136,28.6318622486393,124.046487822005));
#121245=CARTESIAN_POINT('Ctrl Pts',(6.64460000274253,28.6851732601604,123.976777372913));
#121246=CARTESIAN_POINT('Ctrl Pts',(6.64546185461863,28.6938601246875,123.965711587453));
#121247=CARTESIAN_POINT('Ctrl Pts',(6.65082410561159,28.7486247698257,123.897739875715));
#121248=CARTESIAN_POINT('Ctrl Pts',(6.65537709208036,28.7982669053413,123.843819992595));
#121249=CARTESIAN_POINT('Ctrl Pts',(6.66096080497191,28.8601792063967,123.784880535494));
#121250=CARTESIAN_POINT('Ctrl Pts',(6.66176913286139,28.8691650911879,123.776513530192));
#121251=CARTESIAN_POINT('Ctrl Pts',(6.66304630307807,28.8833813569835,123.763566775114));
#121252=CARTESIAN_POINT('Ctrl Pts',(6.66351026912993,28.8885495321933,123.758918952376));
#121253=CARTESIAN_POINT('Ctrl Pts',(6.6643829985571,28.8982741276389,123.750282924777));
#121254=CARTESIAN_POINT('Ctrl Pts',(6.66479118774555,28.9028234015672,123.746287045173));
#121255=CARTESIAN_POINT('Ctrl Pts',(6.66575777085838,28.9135993257459,123.736925522379));
#121256=CARTESIAN_POINT('Ctrl Pts',(6.66631765144547,28.9198440136909,123.731581063215));
#121257=CARTESIAN_POINT('Ctrl Pts',(6.66820352190422,28.9408961192109,123.713832007997));
#121258=CARTESIAN_POINT('Ctrl Pts',(6.66954307938242,28.9558790734049,123.701639285459));
#121259=CARTESIAN_POINT('Ctrl Pts',(6.67287824371164,28.9933311099518,123.672229348907));
#121260=CARTESIAN_POINT('Ctrl Pts',(6.67488846176037,29.0160330930262,123.655319331158));
#121261=CARTESIAN_POINT('Ctrl Pts',(6.68410898190789,29.1211541314611,123.58110555354));
#121262=CARTESIAN_POINT('Ctrl Pts',(6.69149203808143,29.208218275861,123.5307438313));
#121263=CARTESIAN_POINT('Ctrl Pts',(6.70466348439964,29.373968172544,123.453902953511));
#121264=CARTESIAN_POINT('Ctrl Pts',(6.71048493618625,29.4511213636809,123.424859424188));
#121265=CARTESIAN_POINT('Ctrl Pts',(6.71746098376527,29.5489211848458,123.396108462286));
#121266=CARTESIAN_POINT('Ctrl Pts',(6.71879164130262,29.5678222669254,123.390912486472));
#121267=CARTESIAN_POINT('Ctrl Pts',(6.72090792524934,29.5982681498962,123.383118006338));
#121268=CARTESIAN_POINT('Ctrl Pts',(6.72170032175374,29.6097560903192,123.380306953692));
#121269=CARTESIAN_POINT('Ctrl Pts',(6.72320498695728,29.6317344195238,123.375176359769));
#121270=CARTESIAN_POINT('Ctrl Pts',(6.72391790523362,29.6422191658679,123.372835508142));
#121271=CARTESIAN_POINT('Ctrl Pts',(6.72555155601529,29.6664042068442,123.367680963252));
#121272=CARTESIAN_POINT('Ctrl Pts',(6.72646999494893,29.6801188784146,123.364938019905));
#121273=CARTESIAN_POINT('Ctrl Pts',(6.72938298982267,29.7239745065552,123.356739802464));
#121274=CARTESIAN_POINT('Ctrl Pts',(6.73135684299987,29.7542330657226,123.351942673112));
#121275=CARTESIAN_POINT('Ctrl Pts',(6.7360201891513,29.8268097561523,123.342480051985));
#121276=CARTESIAN_POINT('Ctrl Pts',(6.73868704713319,29.8692084892348,123.338596617197));
#121277=CARTESIAN_POINT('Ctrl Pts',(6.74589391255398,29.9852966392249,123.332435971777));
#121278=CARTESIAN_POINT('Ctrl Pts',(6.75036656193504,30.059061136963,123.333417232298));
#121279=CARTESIAN_POINT('Ctrl Pts',(6.75573555229408,30.1465436339659,123.340397963137));
#121280=CARTESIAN_POINT('Ctrl Pts',(6.75659752874064,30.1605539400058,123.341694725452));
#121281=CARTESIAN_POINT('Ctrl Pts',(6.76195973481106,30.2473614434156,123.350839835931));
#121282=CARTESIAN_POINT('Ctrl Pts',(6.76651255289934,30.3195831444888,123.363301849301));
#121283=CARTESIAN_POINT('Ctrl Pts',(6.77209607890747,30.4026769742861,123.383349756854));
#121284=CARTESIAN_POINT('Ctrl Pts',(6.77290440609658,30.4145800704601,123.38636122453));
#121285=CARTESIAN_POINT('Ctrl Pts',(6.77418157544481,30.4331675823993,123.391283070563));
#121286=CARTESIAN_POINT('Ctrl Pts',(6.77464554133918,30.4398754509814,123.393104266996));
#121287=CARTESIAN_POINT('Ctrl Pts',(6.77551827064704,30.4524052233899,123.396590451635));
#121288=CARTESIAN_POINT('Ctrl Pts',(6.77592645987569,30.4582296991918,123.398245273447));
#121289=CARTESIAN_POINT('Ctrl Pts',(6.7768930433258,30.4719392011326,123.402221244495));
#121290=CARTESIAN_POINT('Ctrl Pts',(6.77745292421245,30.479816212621,123.404569037491));
#121291=CARTESIAN_POINT('Ctrl Pts',(6.7793387967593,30.5061459016077,123.41262938756));
#121292=CARTESIAN_POINT('Ctrl Pts',(6.78067835606566,30.5245157794411,123.418604333972));
#121293=CARTESIAN_POINT('Ctrl Pts',(6.78401352596746,30.569537060273,123.434118556207));
#121294=CARTESIAN_POINT('Ctrl Pts',(6.78602374781892,30.596056690669,123.44402011593));
#121295=CARTESIAN_POINT('Ctrl Pts',(6.79524430181211,30.7154212177369,123.49208618448));
#121296=CARTESIAN_POINT('Ctrl Pts',(6.80262738895412,30.8049531052218,123.537918412208));
#121297=CARTESIAN_POINT('Ctrl Pts',(6.81581202222102,30.9595618433797,123.635594239608));
#121298=CARTESIAN_POINT('Ctrl Pts',(6.82164607199979,31.0259469056759,123.684781900821));
#121299=CARTESIAN_POINT('Ctrl Pts',(6.8286270269019,31.1031886744835,123.751436361586));
#121300=CARTESIAN_POINT('Ctrl Pts',(6.82995102338177,31.11773059282,123.764437460648));
#121301=CARTESIAN_POINT('Ctrl Pts',(6.83205931931205,31.1407031295016,123.785713481385));
#121302=CARTESIAN_POINT('Ctrl Pts',(6.83285029829913,31.1492795270704,123.793827557926));
#121303=CARTESIAN_POINT('Ctrl Pts',(6.83435387418819,31.1654975062067,123.809501332601));
#121304=CARTESIAN_POINT('Ctrl Pts',(6.83506710392819,31.1731535618737,123.81704512193));
#121305=CARTESIAN_POINT('Ctrl Pts',(6.8358099347739,31.1810865677337,123.825014567701));
#121306=CARTESIAN_POINT('Ctrl Pts',(6.8358427323928,31.1814367437494,123.825366666948));
#121307=CARTESIAN_POINT('Ctrl Pts',(6.83590340358551,31.1820843671655,123.826018429797));
#121308=CARTESIAN_POINT('Ctrl Pts',(6.8359312790547,31.182381858045,123.826318049879));
#121309=CARTESIAN_POINT('Ctrl Pts',(6.83598319034381,31.1829357493136,123.826876329775));
#121310=CARTESIAN_POINT('Ctrl Pts',(6.83600722742855,31.1831921787587,123.827134960547));
#121311=CARTESIAN_POINT('Ctrl Pts',(6.83605224364996,31.1836723303381,123.827619551723));
#121312=CARTESIAN_POINT('Ctrl Pts',(6.83607322366717,31.1838960726408,123.82784549214));
#121313=CARTESIAN_POINT('Ctrl Pts',(6.83611270482746,31.184317056052,123.828270854925));
#121314=CARTESIAN_POINT('Ctrl Pts',(6.83613120659242,31.1845143114719,123.828470263036));
#121315=CARTESIAN_POINT('Ctrl Pts',(6.83616617017156,31.1848870225307,123.828847231933));
#121316=CARTESIAN_POINT('Ctrl Pts',(6.83618263243793,31.1850624885993,123.829024782317));
#121317=CARTESIAN_POINT('Ctrl Pts',(6.83621385628806,31.1853952531242,123.829361651066));
#121318=CARTESIAN_POINT('Ctrl Pts',(6.83622861821685,31.1855525594419,123.829520961774));
#121319=CARTESIAN_POINT('Ctrl Pts',(6.83625670813026,31.1858518588694,123.8298241971));
#121320=CARTESIAN_POINT('Ctrl Pts',(6.83627003636292,31.1859938578017,123.829968115762));
#121321=CARTESIAN_POINT('Ctrl Pts',(6.83629547171104,31.1862648190436,123.830242840227));
#121322=CARTESIAN_POINT('Ctrl Pts',(6.83630757902373,31.1863937859098,123.830373641501));
#121323=CARTESIAN_POINT('Ctrl Pts',(6.83633074456984,31.1866405226297,123.830623970568));
#121324=CARTESIAN_POINT('Ctrl Pts',(6.83634180296788,31.1867582961606,123.830743494929));
#121325=CARTESIAN_POINT('Ctrl Pts',(6.83636301139702,31.1869841503641,123.830972775975));
#121326=CARTESIAN_POINT('Ctrl Pts',(6.83637316154242,31.1870922337808,123.831082529763));
#121327=CARTESIAN_POINT('Ctrl Pts',(6.83639266973831,31.187299950285,123.831293514937));
#121328=CARTESIAN_POINT('Ctrl Pts',(6.83640202788553,31.1873995856289,123.831394744055));
#121329=CARTESIAN_POINT('Ctrl Pts',(6.83644599565934,31.1878676737873,123.831870441451));
#121330=CARTESIAN_POINT('Ctrl Pts',(6.83648059819211,31.1882359627286,123.832245071574));
#121331=CARTESIAN_POINT('Ctrl Pts',(6.83654978594269,31.1889721651694,123.832994658793));
#121332=CARTESIAN_POINT('Ctrl Pts',(6.83658437116217,31.1893400786978,123.833369615878));
#121333=CARTESIAN_POINT('Ctrl Pts',(6.83769552992994,31.2011573758218,123.84542455043));
#121334=CARTESIAN_POINT('Ctrl Pts',(6.83876463532282,31.2124346360422,123.857272650799));
#121335=CARTESIAN_POINT('Ctrl Pts',(6.84307431199839,31.257482519891,123.906018547587));
#121336=CARTESIAN_POINT('Ctrl Pts',(6.8462526482211,31.2897598023664,123.944264195551));
#121337=CARTESIAN_POINT('Ctrl Pts',(6.85509057777599,31.3758971638434,124.05618760401));
#121338=CARTESIAN_POINT('Ctrl Pts',(6.86061604731787,31.4254956588701,124.132914148576));
#121339=CARTESIAN_POINT('Ctrl Pts',(6.86695878713564,31.4744411549266,124.224284794228));
#121340=CARTESIAN_POINT('Ctrl Pts',(6.86772113622544,31.4801930975265,124.235317589096));
#121341=CARTESIAN_POINT('Ctrl Pts',(6.87301921800923,31.5192130050196,124.312251833965));
#121342=CARTESIAN_POINT('Ctrl Pts',(6.87760764457699,31.5481880979843,124.380228636115));
#121343=CARTESIAN_POINT('Ctrl Pts',(6.88323070623185,31.5766126688508,124.461484167233));
#121344=CARTESIAN_POINT('Ctrl Pts',(6.88403917876402,31.58053919779,124.473119907191));
#121345=CARTESIAN_POINT('Ctrl Pts',(6.88531652837233,31.5864862515534,124.49140812614));
#121346=CARTESIAN_POINT('Ctrl Pts',(6.88578052695712,31.5885944632874,124.498031925956));
#121347=CARTESIAN_POINT('Ctrl Pts',(6.88665328098075,31.5924614110914,124.510449881254));
#121348=CARTESIAN_POINT('Ctrl Pts',(6.88706146181564,31.5942300905237,124.516240681366));
#121349=CARTESIAN_POINT('Ctrl Pts',(6.88802797536398,31.598324991112,124.529914083135));
#121350=CARTESIAN_POINT('Ctrl Pts',(6.88858779409208,31.6006244922968,124.537804398521));
#121351=CARTESIAN_POINT('Ctrl Pts',(6.89047323329542,31.6081313233629,124.564290721975));
#121352=CARTESIAN_POINT('Ctrl Pts',(6.89181241325579,31.61307346818,124.582959432531));
#121353=CARTESIAN_POINT('Ctrl Pts',(6.90253161359105,31.6496630424049,124.731570746258));
#121354=CARTESIAN_POINT('Ctrl Pts',(6.91244836012507,31.6658815080754,124.86480119885));
#121355=CARTESIAN_POINT('Ctrl Pts',(6.92206992138496,31.6659993531474,124.998531901728));
#121356=CARTESIAN_POINT('Ctrl Pts',(6.92206982081665,31.665999351915,124.998530503923));
#121357=CARTESIAN_POINT('Ctrl Pts',(6.92753181140456,31.6660663141654,125.074447049386));
#121358=CARTESIAN_POINT('Ctrl Pts',(6.93289219990884,31.6609442423801,125.150289871046));
#121359=CARTESIAN_POINT('Ctrl Pts',(6.93911166202533,31.6486554136217,125.240232187486));
#121360=CARTESIAN_POINT('Ctrl Pts',(6.94012221746603,31.6464503321999,125.254906855563));
#121361=CARTESIAN_POINT('Ctrl Pts',(6.94186362685613,31.6422878030681,125.280295059211));
#121362=CARTESIAN_POINT('Ctrl Pts',(6.94259726897818,31.6404208576317,125.291022280846));
#121363=CARTESIAN_POINT('Ctrl Pts',(6.94406287339542,31.6364634093353,125.312511899126));
#121364=CARTESIAN_POINT('Ctrl Pts',(6.94479475356403,31.634371570694,125.323273500301));
#121365=CARTESIAN_POINT('Ctrl Pts',(6.94618655018325,31.6301725158045,125.343792367028));
#121366=CARTESIAN_POINT('Ctrl Pts',(6.94684701262364,31.6280835433912,125.353552833388));
#121367=CARTESIAN_POINT('Ctrl Pts',(6.9485622804204,31.6224071119003,125.378957454216));
#121368=CARTESIAN_POINT('Ctrl Pts',(6.94961262412396,31.6186810281943,125.394569825618));
#121369=CARTESIAN_POINT('Ctrl Pts',(6.95332701362548,31.6046166342835,125.44994348004));
#121370=CARTESIAN_POINT('Ctrl Pts',(6.95595137220481,31.5930336159903,125.489375114406));
#121371=CARTESIAN_POINT('Ctrl Pts',(6.95959038684336,31.5747174825424,125.544149528908));
#121372=CARTESIAN_POINT('Ctrl Pts',(6.96063437872422,31.5691955020297,125.559874154248));
#121373=CARTESIAN_POINT('Ctrl Pts',(6.96167312081939,31.563440026896,125.575509584889));
#121374=CARTESIAN_POINT('Ctrl Pts',(6.76893575384937,31.5634399863339,125.575509695081));
#121375=CARTESIAN_POINT('Ctrl Pts',(6.76566846517258,31.5792218917318,125.532636287091));
#121376=CARTESIAN_POINT('Ctrl Pts',(6.7623534844689,31.5932378790754,125.48912013638));
#121377=CARTESIAN_POINT('Ctrl Pts',(6.7546987721579,31.6213480053,125.38772196693));
#121378=CARTESIAN_POINT('Ctrl Pts',(6.75035979235393,31.6341628180893,125.329560310083));
#121379=CARTESIAN_POINT('Ctrl Pts',(6.74216811017329,31.6526476961366,125.217366558126));
#121380=CARTESIAN_POINT('Ctrl Pts',(6.7383111165396,31.6588438782114,125.163494847297));
#121381=CARTESIAN_POINT('Ctrl Pts',(6.73198981774126,31.6647895384476,125.073156983302));
#121382=CARTESIAN_POINT('Ctrl Pts',(6.72948680256719,31.6659891926143,125.036830939512));
#121383=CARTESIAN_POINT('Ctrl Pts',(6.72610898150434,31.6660038935743,124.987066426564));
#121384=CARTESIAN_POINT('Ctrl Pts',(6.72520276065366,31.6658455695417,124.973640808191));
#121385=CARTESIAN_POINT('Ctrl Pts',(6.72363257222695,31.665286952603,124.950253454733));
#121386=CARTESIAN_POINT('Ctrl Pts',(6.7229663684906,31.6649595121106,124.94029084021));
#121387=CARTESIAN_POINT('Ctrl Pts',(6.72157290120123,31.6640839746543,124.919372189542));
#121388=CARTESIAN_POINT('Ctrl Pts',(6.72084625972782,31.663517043225,124.908417385948));
#121389=CARTESIAN_POINT('Ctrl Pts',(6.71910583299487,31.6618926436736,124.882073029297));
#121390=CARTESIAN_POINT('Ctrl Pts',(6.71809539010171,31.6607295443041,124.86669082381));
#121391=CARTESIAN_POINT('Ctrl Pts',(6.71449763569955,31.6557971289075,124.811639849404));
#121392=CARTESIAN_POINT('Ctrl Pts',(6.71194788150291,31.6508184933732,124.772091302045));
#121393=CARTESIAN_POINT('Ctrl Pts',(6.70550673554532,31.6344501884969,124.671372335618));
#121394=CARTESIAN_POINT('Ctrl Pts',(6.70167115063231,31.6210445612681,124.610591568612));
#121395=CARTESIAN_POINT('Ctrl Pts',(6.69223213099618,31.5794709929212,124.46214906716));
#121396=CARTESIAN_POINT('Ctrl Pts',(6.68668138531257,31.5473838265913,124.375809808904));
#121397=CARTESIAN_POINT('Ctrl Pts',(6.67844007291379,31.4916773452116,124.25703659814));
#121398=CARTESIAN_POINT('Ctrl Pts',(6.6759352462958,31.4737654155543,124.222111267959));
#121399=CARTESIAN_POINT('Ctrl Pts',(6.67264686331178,31.4493120621227,124.178312736655));
#121400=CARTESIAN_POINT('Ctrl Pts',(6.67192537503852,31.4438914832879,124.1688244584));
#121401=CARTESIAN_POINT('Ctrl Pts',(6.6707598943962,31.4350555901827,124.153705243666));
#121402=CARTESIAN_POINT('Ctrl Pts',(6.67031956726799,31.4316994348043,124.148039856491));
#121403=CARTESIAN_POINT('Ctrl Pts',(6.66946121476285,31.4251248692273,124.137090161889));
#121404=CARTESIAN_POINT('Ctrl Pts',(6.6690434387682,31.4219104733702,124.1318036614));
#121405=CARTESIAN_POINT('Ctrl Pts',(6.66801018811353,31.4139235946949,124.118831505665));
#121406=CARTESIAN_POINT('Ctrl Pts',(6.66739261973903,31.4091178510767,124.111166652563));
#121407=CARTESIAN_POINT('Ctrl Pts',(6.66506667823885,31.3908903058785,124.082614262726));
#121408=CARTESIAN_POINT('Ctrl Pts',(6.66333514601541,31.3770652496449,124.061989566856));
#121409=CARTESIAN_POINT('Ctrl Pts',(6.65873186824812,31.3395275833869,124.008608714111));
#121410=CARTESIAN_POINT('Ctrl Pts',(6.65582933936729,31.3150747499944,123.976394205894));
#121411=CARTESIAN_POINT('Ctrl Pts',(6.64422777868077,31.2135366659428,123.852276918859));
#121412=CARTESIAN_POINT('Ctrl Pts',(6.63541839725036,31.1277847013632,123.767909466563));
#121413=CARTESIAN_POINT('Ctrl Pts',(6.62352641523548,30.995741565389,123.663437604996));
#121414=CARTESIAN_POINT('Ctrl Pts',(6.62016210801722,30.9564764107155,123.635062642549));
#121415=CARTESIAN_POINT('Ctrl Pts',(6.61570431649433,30.9018347339696,123.599093571785));
#121416=CARTESIAN_POINT('Ctrl Pts',(6.61455453767669,30.887499746302,123.589968459404));
#121417=CARTESIAN_POINT('Ctrl Pts',(6.61273097368413,30.8643836653132,123.575745854207));
#121418=CARTESIAN_POINT('Ctrl Pts',(6.61205202666465,30.8556915649227,123.570506751934));
#121419=CARTESIAN_POINT('Ctrl Pts',(6.6106544320865,30.8376245748689,123.559840844616));
#121420=CARTESIAN_POINT('Ctrl Pts',(6.60993622013046,30.8282435240922,123.554425375328));
#121421=CARTESIAN_POINT('Ctrl Pts',(6.60825610543794,30.8060757000681,123.541915030134));
#121422=CARTESIAN_POINT('Ctrl Pts',(6.60729695346035,30.793246881779,123.534896174114));
#121423=CARTESIAN_POINT('Ctrl Pts',(6.60409597356454,30.7498700496152,123.511900799454));
#121424=CARTESIAN_POINT('Ctrl Pts',(6.60188127962806,30.7189178113786,123.496703034692));
#121425=CARTESIAN_POINT('Ctrl Pts',(6.59650648304181,30.6417635497319,123.461748290888));
#121426=CARTESIAN_POINT('Ctrl Pts',(6.59338016661069,30.5950965893341,123.443099432007));
#121427=CARTESIAN_POINT('Ctrl Pts',(6.58628694986402,30.486375883835,123.405257187973));
#121428=CARTESIAN_POINT('Ctrl Pts',(6.58234800923876,30.423902590394,123.38752586745));
#121429=CARTESIAN_POINT('Ctrl Pts',(6.57368827061504,30.2858500804228,123.356923422177));
#121430=CARTESIAN_POINT('Ctrl Pts',(6.56896426463972,30.2101023782979,123.345531757429));
#121431=CARTESIAN_POINT('Ctrl Pts',(6.56296074054861,30.117757664634,123.338088515151));
#121432=CARTESIAN_POINT('Ctrl Pts',(6.5619043733652,30.1016478830074,123.337025462653));
#121433=CARTESIAN_POINT('Ctrl Pts',(6.5603218933115,30.0777701608207,123.335798055202));
#121434=CARTESIAN_POINT('Ctrl Pts',(6.55980510393975,30.0700118852934,123.335453623076));
#121435=CARTESIAN_POINT('Ctrl Pts',(6.55888304769967,30.0562459456892,123.334938886153));
#121436=CARTESIAN_POINT('Ctrl Pts',(6.55847898200649,30.0502393549644,123.33474682877));
#121437=CARTESIAN_POINT('Ctrl Pts',(6.55758333846138,30.036983600381,123.33439476896));
#121438=CARTESIAN_POINT('Ctrl Pts',(6.55709099500868,30.0297344664941,123.334249589853));
#121439=CARTESIAN_POINT('Ctrl Pts',(6.55563626598367,30.0084189860264,123.333961884132));
#121440=CARTESIAN_POINT('Ctrl Pts',(6.55466722071023,29.994351914211,123.33395019601));
#121441=CARTESIAN_POINT('Ctrl Pts',(6.54798466243464,29.8981306186771,123.335088818889));
#121442=CARTESIAN_POINT('Ctrl Pts',(6.54202798855866,29.8161669707849,123.342137143349));
#121443=CARTESIAN_POINT('Ctrl Pts',(6.52654041030243,29.6060487682507,123.375981521745));
#121444=CARTESIAN_POINT('Ctrl Pts',(6.51706505609792,29.4798978137246,123.411875382835));
#121445=CARTESIAN_POINT('Ctrl Pts',(6.5066473226768,29.3400669615481,123.47013884988));
#121446=CARTESIAN_POINT('Ctrl Pts',(6.50523177199624,29.3210590203445,123.47847906116));
#121447=CARTESIAN_POINT('Ctrl Pts',(6.50293214807661,29.2901783428614,123.492722717465));
#121448=CARTESIAN_POINT('Ctrl Pts',(6.50204104992566,29.2782119164071,123.498416312229));
#121449=CARTESIAN_POINT('Ctrl Pts',(6.50044168657876,29.2567393890003,123.508948893068));
#121450=CARTESIAN_POINT('Ctrl Pts',(6.49973172434151,29.2472095236347,123.51373749051));
#121451=CARTESIAN_POINT('Ctrl Pts',(6.49821230823,29.2268227148164,123.52422791467));
#121452=CARTESIAN_POINT('Ctrl Pts',(6.49740392325962,29.2159813637002,123.529958791876));
#121453=CARTESIAN_POINT('Ctrl Pts',(6.49517794678016,29.1861533133621,123.546150131607));
#121454=CARTESIAN_POINT('Ctrl Pts',(6.49376932510773,29.1673055684959,123.556862472511));
#121455=CARTESIAN_POINT('Ctrl Pts',(6.49063998672077,29.1255549961917,123.581682278525));
#121456=CARTESIAN_POINT('Ctrl Pts',(6.48892621597124,29.1027737337512,123.595982774814));
#121457=CARTESIAN_POINT('Ctrl Pts',(6.48334081515579,29.0290107900213,123.644814968658));
#121458=CARTESIAN_POINT('Ctrl Pts',(6.47954193904515,28.9795946482407,123.681622112195));
#121459=CARTESIAN_POINT('Ctrl Pts',(6.47023368799811,28.862923746602,123.779021946069));
#121460=CARTESIAN_POINT('Ctrl Pts',(6.46477578823116,28.7983563015707,123.842511196219));
#121461=CARTESIAN_POINT('Ctrl Pts',(6.45651536395954,28.7122196526121,123.942224488467));
#121462=CARTESIAN_POINT('Ctrl Pts',(6.45387986474419,28.6863551673293,123.974522604075));
#121463=CARTESIAN_POINT('Ctrl Pts',(6.45044039445048,28.6550899515346,124.016690820631));
#121464=CARTESIAN_POINT('Ctrl Pts',(6.44970553512465,28.6485483109278,124.025701125809));
#121465=CARTESIAN_POINT('Ctrl Pts',(6.44852358223024,28.6382563994411,124.040180055691));
#121466=CARTESIAN_POINT('Ctrl Pts',(6.44808033878806,28.6344474811615,124.045606855845));
#121467=CARTESIAN_POINT('Ctrl Pts',(6.44722073702929,28.6271605547018,124.056121912629));
#121468=CARTESIAN_POINT('Ctrl Pts',(6.44680467167672,28.6236782416112,124.061206945738));
#121469=CARTESIAN_POINT('Ctrl Pts',(6.4457820581066,28.6152265756055,124.073696547416));
#121470=CARTESIAN_POINT('Ctrl Pts',(6.44517351164284,28.6102883488275,124.081121857456));
#121471=CARTESIAN_POINT('Ctrl Pts',(6.44292169165269,28.5923405043771,124.10858455724));
#121472=CARTESIAN_POINT('Ctrl Pts',(6.44125705738956,28.5797033742168,124.12886045977));
#121473=CARTESIAN_POINT('Ctrl Pts',(6.43688123202123,28.5479958749019,124.182258936347));
#121474=CARTESIAN_POINT('Ctrl Pts',(6.43414257082114,28.5296219412697,124.215777819422));
#121475=CARTESIAN_POINT('Ctrl Pts',(6.42636297470662,28.481141548104,124.311922639527));
#121476=CARTESIAN_POINT('Ctrl Pts',(6.42128110692228,28.4537753625509,124.375843885437));
#121477=CARTESIAN_POINT('Ctrl Pts',(6.40925762727111,28.3981261400603,124.532172052491));
#121478=CARTESIAN_POINT('Ctrl Pts',(6.40239179061435,28.3737237958675,124.625708328326));
#121479=CARTESIAN_POINT('Ctrl Pts',(6.394422281649,28.3542194874083,124.740464765179));
#121480=CARTESIAN_POINT('Ctrl Pts',(6.39307075153351,28.351236628781,124.760142877868));
#121481=CARTESIAN_POINT('Ctrl Pts',(6.39092960348249,28.3470362176849,124.791654006149));
#121482=CARTESIAN_POINT('Ctrl Pts',(6.39013292706237,28.3455916144051,124.803454267017));
#121483=CARTESIAN_POINT('Ctrl Pts',(6.3886251703804,28.3430843749332,124.825926449132));
#121484=CARTESIAN_POINT('Ctrl Pts',(6.38791338807996,28.3419982408849,124.836595086831));
#121485=CARTESIAN_POINT('Ctrl Pts',(6.38628936633682,28.3397451370627,124.861069356698));
#121486=CARTESIAN_POINT('Ctrl Pts',(6.38537932927415,28.3386472062693,124.8748806668));
#121487=CARTESIAN_POINT('Ctrl Pts',(6.38252197281539,28.3357245210372,124.918533041298));
#121488=CARTESIAN_POINT('Ctrl Pts',(6.38059422659175,28.334530539402,124.948411363841));
#121489=CARTESIAN_POINT('Ctrl Pts',(6.37342718024813,28.3330670685648,125.060795833283));
#121490=CARTESIAN_POINT('Ctrl Pts',(6.36834527609445,28.3381210360748,125.143254217431));
#121491=CARTESIAN_POINT('Ctrl Pts',(6.35704814479076,28.3630714757776,125.326301131831));
#121492=CARTESIAN_POINT('Ctrl Pts',(6.35087833401576,28.3861717177644,125.426100341294));
#121493=CARTESIAN_POINT('Ctrl Pts',(6.3427150414444,28.4263419848175,125.547556112928));
#121494=CARTESIAN_POINT('Ctrl Pts',(6.34105231593054,28.4349803240993,125.571778355805));
#121495=CARTESIAN_POINT('Ctrl Pts',(6.33873921413658,28.4475477194582,125.60459643992));
#121496=CARTESIAN_POINT('Ctrl Pts',(6.33811452722373,28.4509949253843,125.613374442734));
#121497=CARTESIAN_POINT('Ctrl Pts',(6.33710919758382,28.4566230793419,125.627355966506));
#121498=CARTESIAN_POINT('Ctrl Pts',(6.33673134286049,28.4587563212774,125.632578649919));
#121499=CARTESIAN_POINT('Ctrl Pts',(6.33592756514873,28.463330752225,125.643617440336));
#121500=CARTESIAN_POINT('Ctrl Pts',(6.33550123657487,28.4657785085624,125.649430672004));
#121501=CARTESIAN_POINT('Ctrl Pts',(6.33441786867087,28.4720540980336,125.664101216503));
#121502=CARTESIAN_POINT('Ctrl Pts',(6.33375828435987,28.4759259296848,125.672939315327));
#121503=CARTESIAN_POINT('Ctrl Pts',(6.33105459344575,28.4920120766179,125.708807621319));
#121504=CARTESIAN_POINT('Ctrl Pts',(6.328976990741,28.5048697243589,125.735541311528));
#121505=CARTESIAN_POINT('Ctrl Pts',(6.32311048891109,28.5427047417038,125.809112607265));
#121506=CARTESIAN_POINT('Ctrl Pts',(6.31926942004885,28.569216484543,125.855120189009));
#121507=CARTESIAN_POINT('Ctrl Pts',(6.30578385549763,28.6693921821795,126.011223354872));
#121508=CARTESIAN_POINT('Ctrl Pts',(6.29614326225557,28.7539536768138,126.113764170959));
#121509=CARTESIAN_POINT('Ctrl Pts',(6.28518173627638,28.8687449970032,126.223317399741));
#121510=CARTESIAN_POINT('Ctrl Pts',(6.28338919329618,28.8881365293536,126.240968613648));
#121511=CARTESIAN_POINT('Ctrl Pts',(6.28071304786774,28.9180165719773,126.266904093456));
#121512=CARTESIAN_POINT('Ctrl Pts',(6.27981537483889,28.9282005529466,126.275531294723));
#121513=CARTESIAN_POINT('Ctrl Pts',(6.27820891482175,28.9467125941445,126.290835207247));
#121514=CARTESIAN_POINT('Ctrl Pts',(6.27749836434077,28.9550031269339,126.297555947149));
#121515=CARTESIAN_POINT('Ctrl Pts',(6.27598269763902,28.9729044143073,126.311784804919));
#121516=CARTESIAN_POINT('Ctrl Pts',(6.27517859971786,28.9825342277472,126.31926802892));
#121517=CARTESIAN_POINT('Ctrl Pts',(6.27297765691045,29.00925064968,126.339562525642));
#121518=CARTESIAN_POINT('Ctrl Pts',(6.27158944310107,29.026503126198,126.352152335843));
#121519=CARTESIAN_POINT('Ctrl Pts',(6.26328593824872,29.1320038354848,126.426074065688));
#121520=CARTESIAN_POINT('Ctrl Pts',(6.25669533492763,29.2257775596631,126.479083512348));
#121521=CARTESIAN_POINT('Ctrl Pts',(6.24364533706041,29.4210792246415,126.56578579227));
#121522=CARTESIAN_POINT('Ctrl Pts',(6.23720834210651,29.522028794827,126.59949108886));
#121523=CARTESIAN_POINT('Ctrl Pts',(6.22931655961956,29.6404821282031,126.626818944679));
#121524=CARTESIAN_POINT('Ctrl Pts',(6.22830780916112,29.6555288243556,126.630071331798));
#121525=CARTESIAN_POINT('Ctrl Pts',(6.22679019075446,29.6779828867365,126.634600082726));
#121526=CARTESIAN_POINT('Ctrl Pts',(6.22628977852532,29.6853577986835,126.636035675464));
#121527=CARTESIAN_POINT('Ctrl Pts',(6.22538458333702,29.6986403021103,126.638528103996));
#121528=CARTESIAN_POINT('Ctrl Pts',(6.22498081470885,29.7045442391213,126.639602971935));
#121529=CARTESIAN_POINT('Ctrl Pts',(6.22407009415916,29.7178137820148,126.6419448203));
#121530=CARTESIAN_POINT('Ctrl Pts',(6.22356220601175,29.7251821135943,126.643194138997));
#121531=CARTESIAN_POINT('Ctrl Pts',(6.22201430603384,29.7475501934873,126.646832047732));
#121532=CARTESIAN_POINT('Ctrl Pts',(6.22096634294683,29.7625739607222,126.64906504833));
#121533=CARTESIAN_POINT('Ctrl Pts',(6.214239988704,29.8583733281886,126.661967621428));
#121534=CARTESIAN_POINT('Ctrl Pts',(6.20832952025617,29.9398024230305,126.666903753681));
#121535=CARTESIAN_POINT('Ctrl Pts',(6.19299247442665,30.1505254695771,126.664214898999));
#121536=CARTESIAN_POINT('Ctrl Pts',(6.18362314896035,30.2791884326212,126.647523921862));
#121537=CARTESIAN_POINT('Ctrl Pts',(6.17328928026487,30.4249206014095,126.61103553132));
#121538=CARTESIAN_POINT('Ctrl Pts',(6.17186325968043,30.4451025863081,126.605576767734));
#121539=CARTESIAN_POINT('Ctrl Pts',(6.1695502604646,30.4779436504929,126.596027138637));
#121540=CARTESIAN_POINT('Ctrl Pts',(6.1686561176047,30.4906654123736,126.592162124659));
#121541=CARTESIAN_POINT('Ctrl Pts',(6.16705347505006,30.5135093931105,126.584922051913));
#121542=CARTESIAN_POINT('Ctrl Pts',(6.16634324753615,30.5236479197711,126.581601300156));
#121543=CARTESIAN_POINT('Ctrl Pts',(6.16482560319896,30.5453399946238,126.574264869246));
#121544=CARTESIAN_POINT('Ctrl Pts',(6.16401923158058,30.5568826830236,126.57021886341));
#121545=CARTESIAN_POINT('Ctrl Pts',(6.16180502113609,30.5886139269804,126.558702340121));
#121546=CARTESIAN_POINT('Ctrl Pts',(6.16040599219921,30.6087043053468,126.550966949264));
#121547=CARTESIAN_POINT('Ctrl Pts',(6.15303681439696,30.7146044578148,126.507817377358));
#121548=CARTESIAN_POINT('Ctrl Pts',(6.14729965965831,30.7974960563683,126.465665662885));
#121549=CARTESIAN_POINT('Ctrl Pts',(6.13569639994598,30.9587634419109,126.365904948752));
#121550=CARTESIAN_POINT('Ctrl Pts',(6.12985525162857,31.0364735784667,126.307915587103));
#121551=CARTESIAN_POINT('Ctrl Pts',(6.12167168058232,31.1330236320952,126.221832648336));
#121552=CARTESIAN_POINT('Ctrl Pts',(6.11957939928412,31.1566997671829,126.199442742693));
#121553=CARTESIAN_POINT('Ctrl Pts',(6.11676481224766,31.1869660424645,126.169090857237));
#121554=CARTESIAN_POINT('Ctrl Pts',(6.11608473173688,31.1941617878221,126.161739828757));
#121555=CARTESIAN_POINT('Ctrl Pts',(6.1149702181184,31.205754326921,126.149675624323));
#121556=CARTESIAN_POINT('Ctrl Pts',(6.11453890025574,31.2101927808608,126.145002605959));
#121557=CARTESIAN_POINT('Ctrl Pts',(6.11368305905451,31.2189027413773,126.135725122369));
#121558=CARTESIAN_POINT('Ctrl Pts',(6.11325864120831,31.2231755214743,126.131122047296));
#121559=CARTESIAN_POINT('Ctrl Pts',(6.11218614603746,31.2338586912055,126.119481731413));
#121560=CARTESIAN_POINT('Ctrl Pts',(6.11153562212534,31.2402349066889,126.112413584198));
#121561=CARTESIAN_POINT('Ctrl Pts',(6.108999354549,31.2647084935015,126.084812220464));
#121562=CARTESIAN_POINT('Ctrl Pts',(6.10708545722772,31.2823583280782,126.063890049858));
#121563=CARTESIAN_POINT('Ctrl Pts',(6.10179136357219,31.3291770104192,126.005532707082));
#121564=CARTESIAN_POINT('Ctrl Pts',(6.09836858901783,31.3572738784761,125.967271735084));
#121565=CARTESIAN_POINT('Ctrl Pts',(6.08793005323057,31.437368953623,125.847828505974));
#121566=CARTESIAN_POINT('Ctrl Pts',(6.08087903640557,31.4839989688586,125.763277419907));
#121567=CARTESIAN_POINT('Ctrl Pts',(6.07146606012556,31.5375894141665,125.642386490861));
#121568=CARTESIAN_POINT('Ctrl Pts',(6.06894107617486,31.5510566138041,125.609150590502));
#121569=CARTESIAN_POINT('Ctrl Pts',(6.06644911688889,31.5634400025946,125.575509650907));
#121570=CARTESIAN_POINT('Origin',(5.,30.,125.));
#121571=CARTESIAN_POINT('',(5.36787244251734,31.5634400119422,125.575509625513));
#121572=CARTESIAN_POINT('',(5.55934605048515,31.5634400125327,125.575509623909));
#121573=CARTESIAN_POINT('',(5.,31.5634400119422,125.575509625513));
#121574=CARTESIAN_POINT('Ctrl Pts',(5.55934605048515,31.5634400125327,125.575509623909));
#121575=CARTESIAN_POINT('Ctrl Pts',(5.56457325969903,31.5376336036079,125.645615788283));
#121576=CARTESIAN_POINT('Ctrl Pts',(5.56999012258899,31.507141899839,125.713904230111));
#121577=CARTESIAN_POINT('Ctrl Pts',(5.5821568579232,31.4288705775657,125.861650140254));
#121578=CARTESIAN_POINT('Ctrl Pts',(5.58889024925279,31.3788321131222,125.939647398461));
#121579=CARTESIAN_POINT('Ctrl Pts',(5.59899374878281,31.2919283036445,126.053098701067));
#121580=CARTESIAN_POINT('Ctrl Pts',(5.60249704164566,31.2594815404164,126.09169720192));
#121581=CARTESIAN_POINT('Ctrl Pts',(5.60704747128831,31.2142220122951,126.140828541928));
#121582=CARTESIAN_POINT('Ctrl Pts',(5.60815689890244,31.2029348422995,126.152724015447));
#121583=CARTESIAN_POINT('Ctrl Pts',(5.60929411181592,31.191106268656,126.16482708282));
#121584=CARTESIAN_POINT('Ctrl Pts',(5.60932941348466,31.1907388238759,126.165202698855));
#121585=CARTESIAN_POINT('Ctrl Pts',(5.60939999170995,31.1900036779194,126.165953482131));
#121586=CARTESIAN_POINT('Ctrl Pts',(5.60943526826434,31.1896359769058,126.166328649398));
#121587=CARTESIAN_POINT('Ctrl Pts',(5.60947983086635,31.1891711569369,126.166802459147));
#121588=CARTESIAN_POINT('Ctrl Pts',(5.60948912415662,31.1890742032685,126.166901263297));
#121589=CARTESIAN_POINT('Ctrl Pts',(5.60950848156975,31.1888722166713,126.167107053747));
#121590=CARTESIAN_POINT('Ctrl Pts',(5.60951854560201,31.1887671815783,126.16721403799));
#121591=CARTESIAN_POINT('Ctrl Pts',(5.6095395554274,31.1885478647307,126.167437364418));
#121592=CARTESIAN_POINT('Ctrl Pts',(5.6095505010958,31.1884335804163,126.167553703919));
#121593=CARTESIAN_POINT('Ctrl Pts',(5.60957340793005,31.1881943567315,126.167797158071));
#121594=CARTESIAN_POINT('Ctrl Pts',(5.60958536894441,31.1880694140929,126.167924269405));
#121595=CARTESIAN_POINT('Ctrl Pts',(5.609610469325,31.1878071574507,126.168190992542));
#121596=CARTESIAN_POINT('Ctrl Pts',(5.6096236085078,31.1876698391951,126.168330600221));
#121597=CARTESIAN_POINT('Ctrl Pts',(5.60965126576703,31.1873807161161,126.168624440027));
#121598=CARTESIAN_POINT('Ctrl Pts',(5.60966578360975,31.1872289057797,126.168778666863));
#121599=CARTESIAN_POINT('Ctrl Pts',(5.60969644824963,31.1869081586972,126.169104392588));
#121600=CARTESIAN_POINT('Ctrl Pts',(5.60971259472704,31.1867392148708,126.1692758844));
#121601=CARTESIAN_POINT('Ctrl Pts',(5.60974683284431,31.1863808593938,126.169639486871));
#121602=CARTESIAN_POINT('Ctrl Pts',(5.60976492407513,31.1861914381201,126.16983158827));
#121603=CARTESIAN_POINT('Ctrl Pts',(5.60980345807131,31.1857878288947,126.17024070935));
#121604=CARTESIAN_POINT('Ctrl Pts',(5.60982390026522,31.1855736280023,126.170457716263));
#121605=CARTESIAN_POINT('Ctrl Pts',(5.60986766819247,31.185114824843,126.170922274555));
#121606=CARTESIAN_POINT('Ctrl Pts',(5.60989099313652,31.184870204477,126.171169808207));
#121607=CARTESIAN_POINT('Ctrl Pts',(5.60994123826933,31.1843430141136,126.171702942872));
#121608=CARTESIAN_POINT('Ctrl Pts',(5.609968157316,31.1840604183304,126.171988518356));
#121609=CARTESIAN_POINT('Ctrl Pts',(5.61002656736855,31.1834469022115,126.172608055014));
#121610=CARTESIAN_POINT('Ctrl Pts',(5.61005805669007,31.1831159436978,126.172941978449));
#121611=CARTESIAN_POINT('Ctrl Pts',(5.61012698942341,31.1823909947736,126.173672802887));
#121612=CARTESIAN_POINT('Ctrl Pts',(5.61016443024702,31.1819969456538,126.174069645815));
#121613=CARTESIAN_POINT('Ctrl Pts',(5.61024729666775,31.1811241626173,126.17494773214));
#121614=CARTESIAN_POINT('Ctrl Pts',(5.61029271808654,31.1806453340635,126.175428881701));
#121615=CARTESIAN_POINT('Ctrl Pts',(5.61056165950892,31.1778076227556,126.178276864748));
#121616=CARTESIAN_POINT('Ctrl Pts',(5.61078487736116,31.1754419033654,126.180636903674));
#121617=CARTESIAN_POINT('Ctrl Pts',(5.61172144478894,31.1654721204463,126.190523078419));
#121618=CARTESIAN_POINT('Ctrl Pts',(5.61243186680322,31.1578026198435,126.197983124417));
#121619=CARTESIAN_POINT('Ctrl Pts',(5.61403858074731,31.1402166881517,126.214762141136));
#121620=CARTESIAN_POINT('Ctrl Pts',(5.61493284580725,31.1302567997614,126.224034615652));
#121621=CARTESIAN_POINT('Ctrl Pts',(5.61725783755841,31.1039217845292,126.247956480633));
#121622=CARTESIAN_POINT('Ctrl Pts',(5.61868026565278,31.0873682083727,126.262406089641));
#121623=CARTESIAN_POINT('Ctrl Pts',(5.62747313631323,30.9824138034119,126.350424100891));
#121624=CARTESIAN_POINT('Ctrl Pts',(5.63447378993395,30.8868779082634,126.415002938947));
#121625=CARTESIAN_POINT('Ctrl Pts',(5.64731086811544,30.7015324742168,126.514087601024));
#121626=CARTESIAN_POINT('Ctrl Pts',(5.65312596698492,30.6139450501004,126.551668663773));
#121627=CARTESIAN_POINT('Ctrl Pts',(5.66024628090668,30.5100417646885,126.586070206986));
#121628=CARTESIAN_POINT('Ctrl Pts',(5.66118670807923,30.4963825505974,126.590397947976));
#121629=CARTESIAN_POINT('Ctrl Pts',(5.66262118188542,30.475678312678,126.596665119041));
#121630=CARTESIAN_POINT('Ctrl Pts',(5.66310807124715,30.4686731600006,126.598735382602));
#121631=CARTESIAN_POINT('Ctrl Pts',(5.6640003324627,30.4558816505424,126.602424420016));
#121632=CARTESIAN_POINT('Ctrl Pts',(5.66440484899187,30.4500998541532,126.604058047231));
#121633=CARTESIAN_POINT('Ctrl Pts',(5.66533228546413,30.4368832366709,126.607715275486));
#121634=CARTESIAN_POINT('Ctrl Pts',(5.66585631394989,30.4294431594788,126.609718589194));
#121635=CARTESIAN_POINT('Ctrl Pts',(5.66750403563471,30.4061270759994,126.615823526705));
#121636=CARTESIAN_POINT('Ctrl Pts',(5.66863718330682,30.3902047867189,126.619742277491));
#121637=CARTESIAN_POINT('Ctrl Pts',(5.67562178609053,30.2925929659798,126.642243516335));
#121638=CARTESIAN_POINT('Ctrl Pts',(5.68171073253202,30.2096622307838,126.654875692006));
#121639=CARTESIAN_POINT('Ctrl Pts',(5.69423683596305,30.0380747589092,126.667904948228));
#121640=CARTESIAN_POINT('Ctrl Pts',(5.70065309217485,29.9496065178747,126.667579077431));
#121641=CARTESIAN_POINT('Ctrl Pts',(5.71037123417081,29.8124878954803,126.656146572711));
#121642=CARTESIAN_POINT('Ctrl Pts',(5.71379282929853,29.7636029262947,126.64987864419));
#121643=CARTESIAN_POINT('Ctrl Pts',(5.71827889062258,29.6986963837706,126.638611628788));
#121644=CARTESIAN_POINT('Ctrl Pts',(5.71940235811241,29.682372639126,126.635525858399));
#121645=CARTESIAN_POINT('Ctrl Pts',(5.72127034752949,29.6551242288974,126.629951578646));
#121646=CARTESIAN_POINT('Ctrl Pts',(5.72201903697238,29.644173899557,126.627596154777));
#121647=CARTESIAN_POINT('Ctrl Pts',(5.72349054832347,29.622598328577,126.622727077587));
#121648=CARTESIAN_POINT('Ctrl Pts',(5.72421350898735,29.6119724082001,126.620219055424));
#121649=CARTESIAN_POINT('Ctrl Pts',(5.72596978311197,29.5861024843057,126.613843906288));
#121650=CARTESIAN_POINT('Ctrl Pts',(5.72699946111895,29.5708869104211,126.609864991698));
#121651=CARTESIAN_POINT('Ctrl Pts',(5.73055307472606,29.5182397148198,126.595298126329));
#121652=CARTESIAN_POINT('Ctrl Pts',(5.73304187817072,29.4811226802842,126.583614782041));
#121653=CARTESIAN_POINT('Ctrl Pts',(5.74372333143259,29.3216196833483,126.527196780995));
#121654=CARTESIAN_POINT('Ctrl Pts',(5.75150405627262,29.2043184327592,126.469496694858));
#121655=CARTESIAN_POINT('Ctrl Pts',(5.76213358570567,29.059874621473,126.376032109371));
#121656=CARTESIAN_POINT('Ctrl Pts',(5.76474133504684,29.0256800414665,126.352035594465));
#121657=CARTESIAN_POINT('Ctrl Pts',(5.76902996662426,28.9722147815773,126.311433408143));
#121658=CARTESIAN_POINT('Ctrl Pts',(5.77067265823775,28.9523587442249,126.295626362772));
#121659=CARTESIAN_POINT('Ctrl Pts',(5.7729454084626,28.9258673488297,126.273529845309));
#121660=CARTESIAN_POINT('Ctrl Pts',(5.77355013204621,28.9189102414311,126.267629340032));
#121661=CARTESIAN_POINT('Ctrl Pts',(5.77457289000334,28.9073047204626,126.257621366232));
#121662=CARTESIAN_POINT('Ctrl Pts',(5.77498873591552,28.9026300221485,126.253544416811));
#121663=CARTESIAN_POINT('Ctrl Pts',(5.77584867806959,28.8930560434106,126.245100057384));
#121664=CARTESIAN_POINT('Ctrl Pts',(5.77629297421402,28.888159659177,126.240729675914));
#121665=CARTESIAN_POINT('Ctrl Pts',(5.77747532839682,28.8752581774155,126.229076463896));
#121666=CARTESIAN_POINT('Ctrl Pts',(5.77821687431527,28.8672981585801,126.221744508696));
#121667=CARTESIAN_POINT('Ctrl Pts',(5.78158509077229,28.8317070770929,126.188314860766));
#121668=CARTESIAN_POINT('Ctrl Pts',(5.78426648446888,28.8049046033917,126.161355698573));
#121669=CARTESIAN_POINT('Ctrl Pts',(5.7936175718252,28.7158896607248,126.065473724263));
#121670=CARTESIAN_POINT('Ctrl Pts',(5.80043429861472,28.658527688714,125.992282870422));
#121671=CARTESIAN_POINT('Ctrl Pts',(5.81168160693744,28.5732219271696,125.862422226442));
#121672=CARTESIAN_POINT('Ctrl Pts',(5.81615920509418,28.5418510314233,125.808251634476));
#121673=CARTESIAN_POINT('Ctrl Pts',(5.82334481840903,28.4955342557765,125.716755562493));
#121674=CARTESIAN_POINT('Ctrl Pts',(5.82610706460244,28.478759785408,125.68042956269));
#121675=CARTESIAN_POINT('Ctrl Pts',(5.82987492082888,28.4573404512171,125.629282278208));
#121676=CARTESIAN_POINT('Ctrl Pts',(5.83091795629424,28.4515712688815,125.6149497229));
#121677=CARTESIAN_POINT('Ctrl Pts',(5.83269055460315,28.442045658395,125.590300550476));
#121678=CARTESIAN_POINT('Ctrl Pts',(5.83342338647556,28.4381903965146,125.580023484712));
#121679=CARTESIAN_POINT('Ctrl Pts',(5.83490328386405,28.4305755164743,125.559097751976));
#121680=CARTESIAN_POINT('Ctrl Pts',(5.83565011344544,28.4268220354759,125.548447452646));
#121681=CARTESIAN_POINT('Ctrl Pts',(5.8375165322432,28.417669726288,125.52161097868));
#121682=CARTESIAN_POINT('Ctrl Pts',(5.83863149320454,28.4124106436824,125.50537825348));
#121683=CARTESIAN_POINT('Ctrl Pts',(5.84292260665953,28.3929994513573,125.442167638477));
#121684=CARTESIAN_POINT('Ctrl Pts',(5.84603996684777,28.3806750011564,125.394652025608));
#121685=CARTESIAN_POINT('Ctrl Pts',(5.85596082405347,28.3476928012931,125.239612611489));
#121686=CARTESIAN_POINT('Ctrl Pts',(5.8625386665665,28.3355238834389,125.130586327015));
#121687=CARTESIAN_POINT('Ctrl Pts',(5.87317034740403,28.3333308227973,124.95787782252));
#121688=CARTESIAN_POINT('Ctrl Pts',(5.87711492428867,28.3361332355556,124.894614577595));
#121689=CARTESIAN_POINT('Ctrl Pts',(5.88222741517975,28.3440918674147,124.816248607254));
#121690=CARTESIAN_POINT('Ctrl Pts',(5.88324308642268,28.3458732912283,124.800849034407));
#121691=CARTESIAN_POINT('Ctrl Pts',(5.88476920586318,28.3488395895283,124.778004312739));
#121692=CARTESIAN_POINT('Ctrl Pts',(5.88527106230205,28.3498605886854,124.77053822974));
#121693=CARTESIAN_POINT('Ctrl Pts',(5.88617783273807,28.3517859057663,124.757137200296));
#121694=CARTESIAN_POINT('Ctrl Pts',(5.88658171696137,28.3526716999606,124.751199861386));
#121695=CARTESIAN_POINT('Ctrl Pts',(5.88749140192732,28.3547297454272,124.737898120819));
#121696=CARTESIAN_POINT('Ctrl Pts',(5.88799812504275,28.3559193502293,124.730536797822));
#121697=CARTESIAN_POINT('Ctrl Pts',(5.88953845833747,28.3596666390805,124.708297476768));
#121698=CARTESIAN_POINT('Ctrl Pts',(5.89057990850622,28.362377088442,124.693446486329));
#121699=CARTESIAN_POINT('Ctrl Pts',(5.89927507152819,28.3864848932785,124.570815513254));
#121700=CARTESIAN_POINT('Ctrl Pts',(5.90734487442019,28.4182941018893,124.465366209693));
#121701=CARTESIAN_POINT('Ctrl Pts',(5.92284609007664,28.4997823262785,124.268138138674));
#121702=CARTESIAN_POINT('Ctrl Pts',(5.930253221389,28.5481559517931,124.176331084483));
#121703=CARTESIAN_POINT('Ctrl Pts',(5.93885599461161,28.6166351377654,124.071382371052));
#121704=CARTESIAN_POINT('Ctrl Pts',(5.94033607771004,28.6288764127222,124.053401231306));
#121705=CARTESIAN_POINT('Ctrl Pts',(5.94263110922004,28.648574791763,124.02565062655));
#121706=CARTESIAN_POINT('Ctrl Pts',(5.94345498385429,28.6557934362825,124.015715730568));
#121707=CARTESIAN_POINT('Ctrl Pts',(5.94498659138499,28.6694866247886,123.997301669683));
#121708=CARTESIAN_POINT('Ctrl Pts',(5.94569532590523,28.6759339946595,123.988803181479));
#121709=CARTESIAN_POINT('Ctrl Pts',(5.94727640487547,28.6905637486762,123.969899078162));
#121710=CARTESIAN_POINT('Ctrl Pts',(5.94814698287283,28.6987894773204,123.959527800489));
#121711=CARTESIAN_POINT('Ctrl Pts',(5.95036663735369,28.7201921856478,123.93319338448));
#121712=CARTESIAN_POINT('Ctrl Pts',(5.9517086357629,28.7335448560628,123.9173754919));
#121713=CARTESIAN_POINT('Ctrl Pts',(5.96277271526625,28.8469472964873,123.78800645423));
#121714=CARTESIAN_POINT('Ctrl Pts',(5.97179323522894,28.9617397211405,123.688330864023));
#121715=CARTESIAN_POINT('Ctrl Pts',(5.98482514095229,29.1386333198886,123.572693847425));
#121716=CARTESIAN_POINT('Ctrl Pts',(5.98857484555124,29.1905820295968,123.542606284667));
#121717=CARTESIAN_POINT('Ctrl Pts',(5.99345340023804,29.2575146114485,123.508524119668));
#121718=CARTESIAN_POINT('Ctrl Pts',(5.99444509664196,29.2710877446885,123.501843887122));
#121719=CARTESIAN_POINT('Ctrl Pts',(5.99594206689023,29.291489682272,123.492145621225));
#121720=CARTESIAN_POINT('Ctrl Pts',(5.99643921922003,29.2982512873055,123.488986950152));
#121721=CARTESIAN_POINT('Ctrl Pts',(5.99734131504561,29.3104897315577,123.48336964656));
#121722=CARTESIAN_POINT('Ctrl Pts',(5.9977452830855,29.3159589462932,123.48089504212));
#121723=CARTESIAN_POINT('Ctrl Pts',(5.9986600419308,29.3283179270791,123.475383365257));
#121724=CARTESIAN_POINT('Ctrl Pts',(5.99917180976277,29.3352149243644,123.472363430751));
#121725=CARTESIAN_POINT('Ctrl Pts',(6.00074299328435,29.3563438963562,123.463282032669));
#121726=CARTESIAN_POINT('Ctrl Pts',(6.00181069771191,29.3706395712153,123.457372145034));
#121727=CARTESIAN_POINT('Ctrl Pts',(6.01017667108098,29.4823217640223,123.413013023175));
#121728=CARTESIAN_POINT('Ctrl Pts',(6.01785091234201,29.5830472697835,123.383625836273));
#121729=CARTESIAN_POINT('Ctrl Pts',(6.03333780873458,29.7922555946841,123.343456370911));
#121730=CARTESIAN_POINT('Ctrl Pts',(6.04110419612859,29.9004123296194,123.333451318377));
#121731=CARTESIAN_POINT('Ctrl Pts',(6.05002753583856,30.0304167987172,123.334137305565));
#121732=CARTESIAN_POINT('Ctrl Pts',(6.05149904397454,30.0520393938018,123.334672501828));
#121733=CARTESIAN_POINT('Ctrl Pts',(6.05378384717539,30.0858885010986,123.336170282431));
#121734=CARTESIAN_POINT('Ctrl Pts',(6.05460593822486,30.0981245764871,123.336847046999));
#121735=CARTESIAN_POINT('Ctrl Pts',(6.05613590370432,30.1209983339723,123.338365491635));
#121736=CARTESIAN_POINT('Ctrl Pts',(6.05684476057622,30.1316374790162,123.339174476537));
#121737=CARTESIAN_POINT('Ctrl Pts',(6.05842824886481,30.1554917767242,123.341218986328));
#121738=CARTESIAN_POINT('Ctrl Pts',(6.05930108894348,30.1687015118014,123.342510343673));
#121739=CARTESIAN_POINT('Ctrl Pts',(6.06153073589555,30.2025884449256,123.346232386923));
#121740=CARTESIAN_POINT('Ctrl Pts',(6.06288035280219,30.2232384314512,123.348893080274));
#121741=CARTESIAN_POINT('Ctrl Pts',(6.07258663013868,30.3725637997045,123.370986079972));
#121742=CARTESIAN_POINT('Ctrl Pts',(6.08044769594742,30.4986189752606,123.405047667186));
#121743=CARTESIAN_POINT('Ctrl Pts',(6.0934687629512,30.6961172590375,123.484150280772));
#121744=CARTESIAN_POINT('Ctrl Pts',(6.09856140046476,30.7704004292598,123.520520603427));
#121745=CARTESIAN_POINT('Ctrl Pts',(6.10485266390874,30.8538143567022,123.56935152415));
#121746=CARTESIAN_POINT('Ctrl Pts',(6.10577662360586,30.8658673172546,123.576613975761));
#121747=CARTESIAN_POINT('Ctrl Pts',(6.10719097789564,30.8839908355671,123.587849580047));
#121748=CARTESIAN_POINT('Ctrl Pts',(6.10767451300823,30.8901301578181,123.591711356592));
#121749=CARTESIAN_POINT('Ctrl Pts',(6.10856368367182,30.9013117728976,123.59884717786));
#121750=CARTESIAN_POINT('Ctrl Pts',(6.10896850376115,30.9063618147695,123.602108587929));
#121751=CARTESIAN_POINT('Ctrl Pts',(6.10990063128414,30.9178973185441,123.609647215044));
#121752=CARTESIAN_POINT('Ctrl Pts',(6.11042909445382,30.9243705732351,123.613942500713));
#121753=CARTESIAN_POINT('Ctrl Pts',(6.11206475935497,30.9442089845233,123.62730692776));
#121754=CARTESIAN_POINT('Ctrl Pts',(6.11318099227888,30.9574720354773,123.636524979944));
#121755=CARTESIAN_POINT('Ctrl Pts',(6.12028434315648,31.0402784231018,123.69588083174));
#121756=CARTESIAN_POINT('Ctrl Pts',(6.12652065243238,31.1059928106279,123.751127226154));
#121757=CARTESIAN_POINT('Ctrl Pts',(6.13647511919247,31.2035733040398,123.846929520133));
#121758=CARTESIAN_POINT('Ctrl Pts',(6.14018772461461,31.2383276964915,123.884336482728));
#121759=CARTESIAN_POINT('Ctrl Pts',(6.1476774249638,31.3055715319364,123.963733076918));
#121760=CARTESIAN_POINT('Ctrl Pts',(6.15144714540973,31.3378842210959,124.005800387596));
#121761=CARTESIAN_POINT('Ctrl Pts',(6.15764476412742,31.3885612194047,124.078732019532));
#121762=CARTESIAN_POINT('Ctrl Pts',(6.16010939106544,31.4080328899557,124.108775745907));
#121763=CARTESIAN_POINT('Ctrl Pts',(6.1635451467901,31.4341841530298,124.152125133234));
#121764=CARTESIAN_POINT('Ctrl Pts',(6.1645454930962,31.4416756813994,124.164926812268));
#121765=CARTESIAN_POINT('Ctrl Pts',(6.16626814032352,31.4543588649423,124.187279625948));
#121766=CARTESIAN_POINT('Ctrl Pts',(6.16699325507513,31.4596297421235,124.196784499662));
#121767=CARTESIAN_POINT('Ctrl Pts',(6.16838580266179,31.4696185112332,124.215220140819));
#121768=CARTESIAN_POINT('Ctrl Pts',(6.16905365650199,31.4743489257356,124.224143538587));
#121769=CARTESIAN_POINT('Ctrl Pts',(6.17081907703487,31.4866903515453,124.247944779643));
#121770=CARTESIAN_POINT('Ctrl Pts',(6.17191164392309,31.4941592832044,124.262895309067));
#121771=CARTESIAN_POINT('Ctrl Pts',(6.17597888409622,31.5213053355789,124.319342217589));
#121772=CARTESIAN_POINT('Ctrl Pts',(6.17890276317572,31.5394899186674,124.361535977443));
#121773=CARTESIAN_POINT('Ctrl Pts',(6.18882379509985,31.5960154523824,124.509207360837));
#121774=CARTESIAN_POINT('Ctrl Pts',(6.19556590220482,31.6254352413948,124.617765168342));
#121775=CARTESIAN_POINT('Ctrl Pts',(6.20539765587632,31.6514821995445,124.775434604708));
#121776=CARTESIAN_POINT('Ctrl Pts',(6.20835469298737,31.657224828524,124.822719665012));
#121777=CARTESIAN_POINT('Ctrl Pts',(6.21314914560204,31.66309109616,124.897774725197));
#121778=CARTESIAN_POINT('Ctrl Pts',(6.21493634287029,31.6645596559382,124.925414871101));
#121779=CARTESIAN_POINT('Ctrl Pts',(6.21737769447918,31.6656042696135,124.962488980599));
#121780=CARTESIAN_POINT('Ctrl Pts',(6.21800142458465,31.6657896644415,124.9719029703));
#121781=CARTESIAN_POINT('Ctrl Pts',(6.21904709398241,31.6659654539585,124.987578112864));
#121782=CARTESIAN_POINT('Ctrl Pts',(6.21946661914249,31.6660003702729,124.993838730766));
#121783=CARTESIAN_POINT('Ctrl Pts',(6.22032418092333,31.6659996109844,125.006574978272));
#121784=CARTESIAN_POINT('Ctrl Pts',(6.22076233223928,31.6659614691076,125.013050439539));
#121785=CARTESIAN_POINT('Ctrl Pts',(6.2219108566375,31.6657634396951,125.029946113778));
#121786=CARTESIAN_POINT('Ctrl Pts',(6.22262438321931,31.665543529189,125.040365148543));
#121787=CARTESIAN_POINT('Ctrl Pts',(6.22591362540958,31.6640886812597,125.088072871787));
#121788=CARTESIAN_POINT('Ctrl Pts',(6.2285427766786,31.6616991854907,125.125312846353));
#121789=CARTESIAN_POINT('Ctrl Pts',(6.2368304743083,31.650382157143,125.240829879691));
#121790=CARTESIAN_POINT('Ctrl Pts',(6.24259339957814,31.6371527188931,125.318575718898));
#121791=CARTESIAN_POINT('Ctrl Pts',(6.25289100296512,31.6035456758948,125.456245515323));
#121792=CARTESIAN_POINT('Ctrl Pts',(6.25743099835426,31.5851690022004,125.516480227392));
#121793=CARTESIAN_POINT('Ctrl Pts',(6.26188273594789,31.5634400889265,125.575509416376));
#121794=CARTESIAN_POINT('',(6.02851963656823,31.6659993037066,124.998476829273));
#121795=CARTESIAN_POINT('Ctrl Pts',(6.06644911688889,31.5634400025946,125.575509650907));
#121796=CARTESIAN_POINT('Ctrl Pts',(6.06485626759794,31.571355409626,125.554006511958));
#121797=CARTESIAN_POINT('Ctrl Pts',(6.06327683483192,31.578827998692,125.532337889805));
#121798=CARTESIAN_POINT('Ctrl Pts',(6.06046683788409,31.5914378618506,125.493167072324));
#121799=CARTESIAN_POINT('Ctrl Pts',(6.05923143504398,31.5967383372352,125.475725716762));
#121800=CARTESIAN_POINT('Ctrl Pts',(6.057229595139,31.6049235121702,125.447112425146));
#121801=CARTESIAN_POINT('Ctrl Pts',(6.05645763721405,31.6079801734448,125.435991713235));
#121802=CARTESIAN_POINT('Ctrl Pts',(6.0549675145839,31.6136847571051,125.41436089562));
#121803=CARTESIAN_POINT('Ctrl Pts',(6.05424895043071,31.6163460733296,125.40385495888));
#121804=CARTESIAN_POINT('Ctrl Pts',(6.05282974809935,31.6214225497731,125.382960377269));
#121805=CARTESIAN_POINT('Ctrl Pts',(6.05212904065077,31.6238408409157,125.37257303663));
#121806=CARTESIAN_POINT('Ctrl Pts',(6.05050106010127,31.629251148826,125.348280045128));
#121807=CARTESIAN_POINT('Ctrl Pts',(6.04957626062148,31.6321651911645,125.334357749262));
#121808=CARTESIAN_POINT('Ctrl Pts',(6.04651039208248,31.6412854194013,125.287820012642));
#121809=CARTESIAN_POINT('Ctrl Pts',(6.04439352764609,31.6466952091796,125.255055479839));
#121810=CARTESIAN_POINT('Ctrl Pts',(6.03758378161774,31.6610970214292,125.148014208556));
#121811=CARTESIAN_POINT('Ctrl Pts',(6.03299866726444,31.6660674538522,125.073289477035));
#121812=CARTESIAN_POINT('Ctrl Pts',(6.02842896873232,31.6659993087612,124.998482367842));
#121813=CARTESIAN_POINT('Ctrl Pts',(6.02851963656823,31.6659993037066,124.998476829273));
#121814=CARTESIAN_POINT('Ctrl Pts',(6.02319560875282,31.6659265050813,124.91885183581));
#121815=CARTESIAN_POINT('Ctrl Pts',(6.0178715809374,31.6601415384358,124.839481023796));
#121816=CARTESIAN_POINT('Ctrl Pts',(6.01254755312199,31.6487752900045,124.761052216854));
#121817=CARTESIAN_POINT('Ctrl Pts',(6.00879991050873,31.6407744608483,124.705845304119));
#121818=CARTESIAN_POINT('Ctrl Pts',(6.00505226789547,31.6300091693845,124.651104499699));
#121819=CARTESIAN_POINT('Ctrl Pts',(6.00130462528221,31.6165387634105,124.597062751298));
#121820=CARTESIAN_POINT('Ctrl Pts',(5.99722727558211,31.6018832688967,124.538266561433));
#121821=CARTESIAN_POINT('Ctrl Pts',(5.99314992588201,31.5839855577696,124.480149579525));
#121822=CARTESIAN_POINT('Ctrl Pts',(5.9890725761819,31.5629257672559,124.42309528859));
#121823=CARTESIAN_POINT('Ctrl Pts',(5.98495160860948,31.5416406874437,124.365430653445));
#121824=CARTESIAN_POINT('Ctrl Pts',(5.98083064103705,31.5171255131338,124.308852114332));
#121825=CARTESIAN_POINT('Ctrl Pts',(5.97670967346462,31.4895158984512,124.25374375161));
#121826=CARTESIAN_POINT('Ctrl Pts',(5.97264355643923,31.4622737708798,124.199368887463));
#121827=CARTESIAN_POINT('Ctrl Pts',(5.96857743941384,31.4320193111668,124.146425773321));
#121828=CARTESIAN_POINT('Ctrl Pts',(5.96451132238844,31.3989316336102,124.095264522369));
#121829=CARTESIAN_POINT('Ctrl Pts',(5.96044769316908,31.3658642003612,124.044134573828));
#121830=CARTESIAN_POINT('Ctrl Pts',(5.95638406394971,31.3299672636843,123.994784755909));
#121831=CARTESIAN_POINT('Ctrl Pts',(5.95232043473035,31.2914648767174,123.947538850026));
#121832=CARTESIAN_POINT('Ctrl Pts',(5.94825778211368,31.2529717429409,123.900304298643));
#121833=CARTESIAN_POINT('Ctrl Pts',(5.94419512949701,31.2118747251711,123.855173052237));
#121834=CARTESIAN_POINT('Ctrl Pts',(5.94013247688035,31.1684387532848,123.812436578611));
#121835=CARTESIAN_POINT('Ctrl Pts',(5.93596888334396,31.1239235685381,123.7686382719));
#121836=CARTESIAN_POINT('Ctrl Pts',(5.93180528980757,31.0769520072842,123.727355765411));
#121837=CARTESIAN_POINT('Ctrl Pts',(5.92764169627117,31.0278483005135,123.688861612517));
#121838=CARTESIAN_POINT('Ctrl Pts',(5.92357385644521,30.979873873553,123.651252742477));
#121839=CARTESIAN_POINT('Ctrl Pts',(5.91950601661925,30.9298648035679,123.616305575443));
#121840=CARTESIAN_POINT('Ctrl Pts',(5.91543817679328,30.8781537565013,123.584230958121));
#121841=CARTESIAN_POINT('Ctrl Pts',(5.91122670640168,30.8246168541263,123.551023824372));
#121842=CARTESIAN_POINT('Ctrl Pts',(5.90701523601007,30.769256040787,123.520896213992));
#121843=CARTESIAN_POINT('Ctrl Pts',(5.90280376561847,30.712466588119,123.494029428968));
#121844=CARTESIAN_POINT('Ctrl Pts',(5.89859229522686,30.655677135451,123.467162643945));
#121845=CARTESIAN_POINT('Ctrl Pts',(5.89438082483526,30.5974596275333,123.443556842907));
#121846=CARTESIAN_POINT('Ctrl Pts',(5.89016935444365,30.5382274340245,123.423336678532));
#121847=CARTESIAN_POINT('Ctrl Pts',(5.88609200474354,30.4808815799681,123.4037604561));
#121848=CARTESIAN_POINT('Ctrl Pts',(5.88201465504342,30.4223478962537,123.387276539074));
#121849=CARTESIAN_POINT('Ctrl Pts',(5.87793730534331,30.3629920272199,123.374025588093));
#121850=CARTESIAN_POINT('Ctrl Pts',(5.87381633777088,30.3030011926064,123.360632883687));
#121851=CARTESIAN_POINT('Ctrl Pts',(5.86969537019845,30.2421709473292,123.350542981847));
#121852=CARTESIAN_POINT('Ctrl Pts',(5.86557440262603,30.1808975479542,123.343850225027));
#121853=CARTESIAN_POINT('Ctrl Pts',(5.86150828560062,30.1204397044928,123.337246549561));
#121854=CARTESIAN_POINT('Ctrl Pts',(5.85744216857521,30.0595509558089,123.333950195322));
#121855=CARTESIAN_POINT('Ctrl Pts',(5.85337605154981,29.9986225924009,123.334000569403));
#121856=CARTESIAN_POINT('Ctrl Pts',(5.84931242233043,29.9377315072977,123.334050912664));
#121857=CARTESIAN_POINT('Ctrl Pts',(5.84524879311105,29.8768013664308,123.33744392392));
#121858=CARTESIAN_POINT('Ctrl Pts',(5.84118516389167,29.8162257110445,123.344166973781));
#121859=CARTESIAN_POINT('Ctrl Pts',(5.83712251127499,29.7556646136666,123.350888407906));
#121860=CARTESIAN_POINT('Ctrl Pts',(5.83305985865831,29.6954583412569,123.360938235477));
#121861=CARTESIAN_POINT('Ctrl Pts',(5.82899720604163,29.6359954570605,123.37425195903));
#121862=CARTESIAN_POINT('Ctrl Pts',(5.82483361250525,29.5750551543435,123.387896476186));
#121863=CARTESIAN_POINT('Ctrl Pts',(5.82067001896887,29.5148962345785,123.404969181928));
#121864=CARTESIAN_POINT('Ctrl Pts',(5.81650642543249,29.4559235329719,123.425345498839));
#121865=CARTESIAN_POINT('Ctrl Pts',(5.81243858560652,29.3983070768638,123.445253204218));
#121866=CARTESIAN_POINT('Ctrl Pts',(5.80837074578054,29.3418233160874,123.468313913944));
#121867=CARTESIAN_POINT('Ctrl Pts',(5.80430290595456,29.2868298182051,123.494362496549));
#121868=CARTESIAN_POINT('Ctrl Pts',(5.80009143556298,29.2298945655971,123.521330823493));
#121869=CARTESIAN_POINT('Ctrl Pts',(5.7958799651714,29.174557330909,123.551501720362));
#121870=CARTESIAN_POINT('Ctrl Pts',(5.79166849477982,29.1211848149767,123.584641433921));
#121871=CARTESIAN_POINT('Ctrl Pts',(5.78745702438825,29.0678122990443,123.617781147481));
#121872=CARTESIAN_POINT('Ctrl Pts',(5.78324555399667,29.016404951922,123.653889273057));
#121873=CARTESIAN_POINT('Ctrl Pts',(5.77903408360509,28.967291696611,123.692686127928));
#121874=CARTESIAN_POINT('Ctrl Pts',(5.77495673390497,28.9197425277472,123.730247437843));
#121875=CARTESIAN_POINT('Ctrl Pts',(5.77087938420486,28.8741471032045,123.770483850587));
#121876=CARTESIAN_POINT('Ctrl Pts',(5.76680203450474,28.8308219104709,123.813164461703));
#121877=CARTESIAN_POINT('Ctrl Pts',(5.76268106693231,28.7870332419838,123.856301653093));
#121878=CARTESIAN_POINT('Ctrl Pts',(5.75856009935989,28.7455641356007,123.901935391439));
#121879=CARTESIAN_POINT('Ctrl Pts',(5.75443913178746,28.7067087678563,123.949783932298));
#121880=CARTESIAN_POINT('Ctrl Pts',(5.75037301476205,28.6683705694751,123.996995603636));
#121881=CARTESIAN_POINT('Ctrl Pts',(5.74630689773664,28.6325772882018,124.046363069474));
#121882=CARTESIAN_POINT('Ctrl Pts',(5.74224078071123,28.5995742535649,124.097578962611));
#121883=CARTESIAN_POINT('Ctrl Pts',(5.73817715149185,28.5665914114478,124.148763519905));
#121884=CARTESIAN_POINT('Ctrl Pts',(5.73411352227247,28.5363957078714,124.201793832718));
#121885=CARTESIAN_POINT('Ctrl Pts',(5.73004989305309,28.5091899749721,124.256332420179));
#121886=CARTESIAN_POINT('Ctrl Pts',(5.72598724043641,28.4819907803642,124.310857900507));
#121887=CARTESIAN_POINT('Ctrl Pts',(5.72192458781972,28.4577803583883,124.366890477991));
#121888=CARTESIAN_POINT('Ctrl Pts',(5.71786193520304,28.4367152646657,124.424068722615));
#121889=CARTESIAN_POINT('Ctrl Pts',(5.71369834166666,28.4151267863139,124.482667621462));
#121890=CARTESIAN_POINT('Ctrl Pts',(5.70953474813029,28.3968422725696,124.542469372822));
#121891=CARTESIAN_POINT('Ctrl Pts',(5.70537115459391,28.3819766285952,124.603066290688));
#121892=CARTESIAN_POINT('Ctrl Pts',(5.70130331476793,28.3674528625097,124.66226960957));
#121893=CARTESIAN_POINT('Ctrl Pts',(5.69723547494195,28.3561924059842,124.722231378084));
#121894=CARTESIAN_POINT('Ctrl Pts',(5.69316763511597,28.3482504566834,124.782561626769));
#121895=CARTESIAN_POINT('Ctrl Pts',(5.68895616472439,28.3400280866387,124.845022064476));
#121896=CARTESIAN_POINT('Ctrl Pts',(5.68474469433282,28.3353630426135,124.907876896629));
#121897=CARTESIAN_POINT('Ctrl Pts',(5.68053322394125,28.3342578236991,124.970691262525));
#121898=CARTESIAN_POINT('Ctrl Pts',(5.67632175354967,28.3331526047847,125.033505628421));
#121899=CARTESIAN_POINT('Ctrl Pts',(5.6721102831581,28.3356071150888,125.096278930468));
#121900=CARTESIAN_POINT('Ctrl Pts',(5.66789881276653,28.3415647769982,125.158583136263));
#121901=CARTESIAN_POINT('Ctrl Pts',(5.66382146306642,28.3473327080867,125.218903169694));
#121902=CARTESIAN_POINT('Ctrl Pts',(5.6597441133663,28.3564077503369,125.279032657118));
#121903=CARTESIAN_POINT('Ctrl Pts',(5.65566676366619,28.3687675623041,125.338580469326));
#121904=CARTESIAN_POINT('Ctrl Pts',(5.65154579609376,28.3812595946448,125.398765300446));
#121905=CARTESIAN_POINT('Ctrl Pts',(5.64742482852134,28.3971071320074,125.458355403812));
#121906=CARTESIAN_POINT('Ctrl Pts',(5.64330386094891,28.4162330194005,125.516950820836));
#121907=CARTESIAN_POINT('Ctrl Pts',(5.63923774392351,28.4351043390575,125.574766326196));
#121908=CARTESIAN_POINT('Ctrl Pts',(5.6351716268981,28.4571671072163,125.631612961354));
#121909=CARTESIAN_POINT('Ctrl Pts',(5.63110550987269,28.4822961492294,125.687117909355));
#121910=CARTESIAN_POINT('Ctrl Pts',(5.62704188065332,28.5074098163328,125.742588897304));
#121911=CARTESIAN_POINT('Ctrl Pts',(5.62297825143394,28.5355858268912,125.796719360266));
#121912=CARTESIAN_POINT('Ctrl Pts',(5.61891462221457,28.5666506573924,125.849155852624));
#121913=CARTESIAN_POINT('Ctrl Pts',(5.61485196959789,28.5977080221541,125.901579743041));
#121914=CARTESIAN_POINT('Ctrl Pts',(5.61078931698121,28.6316525678179,125.952310030753));
#121915=CARTESIAN_POINT('Ctrl Pts',(5.60672666436453,28.6682655514314,126.001019159904));
#121916=CARTESIAN_POINT('Ctrl Pts',(5.60256307082815,28.7057882235139,126.05093851911));
#121917=CARTESIAN_POINT('Ctrl Pts',(5.59839947729177,28.7461134161297,126.098734457736));
#121918=CARTESIAN_POINT('Ctrl Pts',(5.59423588375539,28.7889609349392,126.144089324702));
#121919=CARTESIAN_POINT('Ctrl Pts',(5.59016804392941,28.8308230528271,126.188401127123));
#121920=CARTESIAN_POINT('Ctrl Pts',(5.58610020410344,28.8750922791935,126.23038263688));
#121921=CARTESIAN_POINT('Ctrl Pts',(5.58203236427746,28.9214709209375,126.269775974578));
#121922=CARTESIAN_POINT('Ctrl Pts',(5.57782089388588,28.9694871371266,126.31056024398));
#121923=CARTESIAN_POINT('Ctrl Pts',(5.5736094234943,29.0197640671423,126.348569754223));
#121924=CARTESIAN_POINT('Ctrl Pts',(5.56939795310271,29.0719377209833,126.383566552887));
#121925=CARTESIAN_POINT('Ctrl Pts',(5.56518648271113,29.1241113748242,126.41856335155));
#121926=CARTESIAN_POINT('Ctrl Pts',(5.56097501231955,29.1781811984191,126.450547195083));
#121927=CARTESIAN_POINT('Ctrl Pts',(5.55676354192797,29.2337568974358,126.479333467401));
#121928=CARTESIAN_POINT('Ctrl Pts',(5.55268619222785,29.2875627036389,126.507202997017));
#121929=CARTESIAN_POINT('Ctrl Pts',(5.54860884252774,29.3430020821622,126.532190733182));
#121930=CARTESIAN_POINT('Ctrl Pts',(5.54453149282762,29.3997343111234,126.554103311481));
#121931=CARTESIAN_POINT('Ctrl Pts',(5.54041052525519,29.4570734390019,126.576250301866));
#121932=CARTESIAN_POINT('Ctrl Pts',(5.53628955768277,29.5157328156011,126.595255627346));
#121933=CARTESIAN_POINT('Ctrl Pts',(5.53216859011034,29.5753345721938,126.610967186018));
#121934=CARTESIAN_POINT('Ctrl Pts',(5.52810247308494,29.6341430226284,126.626469622057));
#121935=CARTESIAN_POINT('Ctrl Pts',(5.52403635605953,29.693868410051,126.638765302794));
#121936=CARTESIAN_POINT('Ctrl Pts',(5.51997023903412,29.7541296244665,126.647757190376));
#121937=CARTESIAN_POINT('Ctrl Pts',(5.51590660981474,29.8143539687645,126.656743576377));
#121938=CARTESIAN_POINT('Ctrl Pts',(5.51184298059536,29.8751129847364,126.662430101641));
#121939=CARTESIAN_POINT('Ctrl Pts',(5.50777935137598,29.9360156144037,126.664770854622));
#121940=CARTESIAN_POINT('Ctrl Pts',(5.5037166987593,29.9969036074816,126.667111045055));
#121941=CARTESIAN_POINT('Ctrl Pts',(5.49965404614262,30.0579346343865,126.66610703977));
#121942=CARTESIAN_POINT('Ctrl Pts',(5.49559139352594,30.1187148628542,126.661764959715));
#121943=CARTESIAN_POINT('Ctrl Pts',(5.49142779998956,30.1810052406603,126.65731499607));
#121944=CARTESIAN_POINT('Ctrl Pts',(5.48726420645318,30.2430316268307,126.64935884579));
#121945=CARTESIAN_POINT('Ctrl Pts',(5.4831006129168,30.3043751815096,126.637959629808));
#121946=CARTESIAN_POINT('Ctrl Pts',(5.47903277309083,30.3643079661606,126.626822571315));
#121947=CARTESIAN_POINT('Ctrl Pts',(5.47496493326485,30.4235884996283,126.612399329089));
#121948=CARTESIAN_POINT('Ctrl Pts',(5.47089709343887,30.4818386681556,126.594800143551));
#121949=CARTESIAN_POINT('Ctrl Pts',(5.46668562304729,30.5421455805592,126.576579551792));
#121950=CARTESIAN_POINT('Ctrl Pts',(5.46247415265571,30.6013474269172,126.554954706161));
#121951=CARTESIAN_POINT('Ctrl Pts',(5.45826268226414,30.6590468779301,126.530102353665));
#121952=CARTESIAN_POINT('Ctrl Pts',(5.45405121187256,30.7167463289429,126.505250001169));
#121953=CARTESIAN_POINT('Ctrl Pts',(5.44983974148098,30.7729428794861,126.477170475215));
#121954=CARTESIAN_POINT('Ctrl Pts',(5.44562827108941,30.8272697439158,126.446091549938));
#121955=CARTESIAN_POINT('Ctrl Pts',(5.44155183031641,30.8798547616506,126.416009087899));
#121956=CARTESIAN_POINT('Ctrl Pts',(5.43747538954341,30.9309053353052,126.382992519671));
#121957=CARTESIAN_POINT('Ctrl Pts',(5.43339894877041,30.9800744454229,126.347223100095));
#121958=CARTESIAN_POINT('Ctrl Pts',(5.42932840898418,31.0291723791678,126.311505459725));
#121959=CARTESIAN_POINT('Ctrl Pts',(5.42525786919795,31.0763938380124,126.273043165971));
#121960=CARTESIAN_POINT('Ctrl Pts',(5.42118732941172,31.1214179736454,126.232062388187));
#121961=CARTESIAN_POINT('Ctrl Pts',(5.41712116917604,31.1663936671829,126.191125702193));
#121962=CARTESIAN_POINT('Ctrl Pts',(5.41305500894035,31.2091763496132,126.147676249284));
#121963=CARTESIAN_POINT('Ctrl Pts',(5.40898884870466,31.2494773534112,126.101981099345));
#121964=CARTESIAN_POINT('Ctrl Pts',(5.40492500380731,31.2897554091565,126.056311968973));
#121965=CARTESIAN_POINT('Ctrl Pts',(5.40086115890996,31.3275542478635,126.008400058138));
#121966=CARTESIAN_POINT('Ctrl Pts',(5.39679731401261,31.36262266187,125.958548632756));
#121967=CARTESIAN_POINT('Ctrl Pts',(5.392734798567,31.3976796035479,125.908713515837));
#121968=CARTESIAN_POINT('Ctrl Pts',(5.3886722831214,31.430007603046,125.856940565119));
#121969=CARTESIAN_POINT('Ctrl Pts',(5.38460976767579,31.4593976670292,125.803563593918));
#121970=CARTESIAN_POINT('Ctrl Pts',(5.38054576390159,31.4887984982509,125.75016706772));
#121971=CARTESIAN_POINT('Ctrl Pts',(5.37648176012739,31.5152590011302,125.695165798204));
#121972=CARTESIAN_POINT('Ctrl Pts',(5.37241775635318,31.538616049042,125.638918346606));
#121973=CARTESIAN_POINT('Ctrl Pts',(5.37090265174123,31.5473238094131,125.617948687605));
#121974=CARTESIAN_POINT('Ctrl Pts',(5.36938754712929,31.5556007043374,125.59680603244));
#121975=CARTESIAN_POINT('Ctrl Pts',(5.36787244251734,31.5634400119422,125.575509625513));
#121976=CARTESIAN_POINT('Origin',(5.,30.,125.));
#121977=CARTESIAN_POINT('',(4.66781556978768,31.5660436956742,125.576468401513));
#121978=CARTESIAN_POINT('',(4.86075489241547,31.5634400172546,125.575509611081));
#121979=CARTESIAN_POINT('',(5.,31.5634400119422,125.575509625513));
#121980=CARTESIAN_POINT('',(5.52205786626619,31.6659992468011,125.001394788999));
#121981=CARTESIAN_POINT('Ctrl Pts',(4.86075489241547,31.5634400172546,125.575509611081));
#121982=CARTESIAN_POINT('Ctrl Pts',(4.86238037643612,31.554247439111,125.600482338304));
#121983=CARTESIAN_POINT('Ctrl Pts',(4.86400395132135,31.5444563766197,125.625235228954));
#121984=CARTESIAN_POINT('Ctrl Pts',(4.86651208868844,31.5284682148076,125.662983839313));
#121985=CARTESIAN_POINT('Ctrl Pts',(4.86739290510976,31.5226906633799,125.676147758858));
#121986=CARTESIAN_POINT('Ctrl Pts',(4.87273741189656,31.4867068185035,125.755334469012));
#121987=CARTESIAN_POINT('Ctrl Pts',(4.87725395371479,31.4523849452009,125.819391630691));
#121988=CARTESIAN_POINT('Ctrl Pts',(4.88279721873322,31.4075094565573,125.891416748726));
#121989=CARTESIAN_POINT('Ctrl Pts',(4.88360537788959,31.4009032748706,125.901763096892));
#121990=CARTESIAN_POINT('Ctrl Pts',(4.88488233883513,31.3903787862481,125.917851369303));
#121991=CARTESIAN_POINT('Ctrl Pts',(4.88534626693394,31.3865376916344,125.923643616706));
#121992=CARTESIAN_POINT('Ctrl Pts',(4.88621896768022,31.3792824446093,125.934437052726));
#121993=CARTESIAN_POINT('Ctrl Pts',(4.88662716662745,31.3758771236352,125.939443879902));
#121994=CARTESIAN_POINT('Ctrl Pts',(4.88759383095554,31.3677845027958,125.951204043296));
#121995=CARTESIAN_POINT('Ctrl Pts',(4.88815378375568,31.3630744285798,125.957941372494));
#121996=CARTESIAN_POINT('Ctrl Pts',(4.89004015775076,31.3471265142947,125.980397638121));
#121997=CARTESIAN_POINT('Ctrl Pts',(4.8913801560382,31.3356655614814,125.995955221188));
#121998=CARTESIAN_POINT('Ctrl Pts',(4.89471666408884,31.3067479010221,126.033812260193));
#121999=CARTESIAN_POINT('Ctrl Pts',(4.89672779912124,31.288988532416,126.05587226895));
#122000=CARTESIAN_POINT('Ctrl Pts',(4.90595648533575,31.2056945727883,126.15410230925));
#122001=CARTESIAN_POINT('Ctrl Pts',(4.91334701386877,31.1339135416843,126.224700824916));
#122002=CARTESIAN_POINT('Ctrl Pts',(4.92651678449591,30.9926372350616,126.340516485883));
#122003=CARTESIAN_POINT('Ctrl Pts',(4.93232985392164,30.9252890744389,126.387860550889));
#122004=CARTESIAN_POINT('Ctrl Pts',(4.93929779582167,30.8378894863385,126.440097646218));
#122005=CARTESIAN_POINT('Ctrl Pts',(4.94062820487365,30.8208917951965,126.449854040734));
#122006=CARTESIAN_POINT('Ctrl Pts',(4.94274419085391,30.7933668817169,126.465013595099));
#122007=CARTESIAN_POINT('Ctrl Pts',(4.94353653449039,30.7829478195366,126.470608230357));
#122008=CARTESIAN_POINT('Ctrl Pts',(4.94504115883189,30.76295177568,126.481072581541));
#122009=CARTESIAN_POINT('Ctrl Pts',(4.9457540884917,30.7533855777773,126.485961501595));
#122010=CARTESIAN_POINT('Ctrl Pts',(4.94738784930017,30.7312569046288,126.497001995012));
#122011=CARTESIAN_POINT('Ctrl Pts',(4.94830638579662,30.7186627985128,126.503088631929));
#122012=CARTESIAN_POINT('Ctrl Pts',(4.95122004275614,30.6782421650691,126.521999425974));
#122013=CARTESIAN_POINT('Ctrl Pts',(4.95319444674746,30.6501369790614,126.534215364481));
#122014=CARTESIAN_POINT('Ctrl Pts',(4.95785937483207,30.5822095607378,126.561537925775));
#122015=CARTESIAN_POINT('Ctrl Pts',(4.96052724207514,30.5421134216512,126.575906750325));
#122016=CARTESIAN_POINT('Ctrl Pts',(4.96773457354951,30.4312452615663,126.610904217683));
#122017=CARTESIAN_POINT('Ctrl Pts',(4.97220674837597,30.3595863944731,126.62839886413));
#122018=CARTESIAN_POINT('Ctrl Pts',(4.97757842588871,30.2730950261339,126.643525023215));
#122019=CARTESIAN_POINT('Ctrl Pts',(4.97844353696784,30.2591551426606,126.645780666132));
#122020=CARTESIAN_POINT('Ctrl Pts',(4.98380455056035,30.1728393402246,126.658623776316));
#122021=CARTESIAN_POINT('Ctrl Pts',(4.9883530698556,30.0998686316507,126.664611012936));
#122022=CARTESIAN_POINT('Ctrl Pts',(4.99393182489342,30.0144746497704,126.66598236244));
#122023=CARTESIAN_POINT('Ctrl Pts',(4.99474013415032,30.0021969454228,126.666043786675));
#122024=CARTESIAN_POINT('Ctrl Pts',(4.99601728125774,29.9829695293546,126.665927452113));
#122025=CARTESIAN_POINT('Ctrl Pts',(4.99648124311894,29.9760194162668,126.66584190122));
#122026=CARTESIAN_POINT('Ctrl Pts',(4.99735396937867,29.9630159890462,126.665600446998));
#122027=CARTESIAN_POINT('Ctrl Pts',(4.99776215964407,29.9569627274974,126.665455029293));
#122028=CARTESIAN_POINT('Ctrl Pts',(4.99872875172116,29.942694391322,126.665034423107));
#122029=CARTESIAN_POINT('Ctrl Pts',(4.9992886402795,29.934480412536,126.664731431641));
#122030=CARTESIAN_POINT('Ctrl Pts',(5.00117456631664,29.906970794567,126.663512767436));
#122031=CARTESIAN_POINT('Ctrl Pts',(5.00251417244876,29.8876896962,126.662322314294));
#122032=CARTESIAN_POINT('Ctrl Pts',(5.00584948508166,29.8402170328163,126.658561617138));
#122033=CARTESIAN_POINT('Ctrl Pts',(5.00785980433287,29.8120624432313,126.655607600932));
#122034=CARTESIAN_POINT('Ctrl Pts',(5.01708122525734,29.6844579294815,126.638922487842));
#122035=CARTESIAN_POINT('Ctrl Pts',(5.02446510563703,29.5862982109609,126.616936927469));
#122036=CARTESIAN_POINT('Ctrl Pts',(5.03763636678413,29.4123501603004,126.56108856782));
#122037=CARTESIAN_POINT('Ctrl Pts',(5.04345689356615,29.3359493383585,126.530153663104));
#122038=CARTESIAN_POINT('Ctrl Pts',(5.05043204686999,29.2445657553768,126.485011531568));
#122039=CARTESIAN_POINT('Ctrl Pts',(5.05176267714154,29.2271471418306,126.47602122728));
#122040=CARTESIAN_POINT('Ctrl Pts',(5.05387892839298,29.1994789367576,126.461116657269));
#122041=CARTESIAN_POINT('Ctrl Pts',(5.05467131909631,29.1891270959937,126.455397198319));
#122042=CARTESIAN_POINT('Ctrl Pts',(5.05617597981531,29.169489920522,126.444272968646));
#122043=CARTESIAN_POINT('Ctrl Pts',(5.0568888993397,29.1601942917123,126.438887689023));
#122044=CARTESIAN_POINT('Ctrl Pts',(5.05852256218956,29.1389181594045,126.426285265794));
#122045=CARTESIAN_POINT('Ctrl Pts',(5.05944101182486,29.1269750402998,126.419006354857));
#122046=CARTESIAN_POINT('Ctrl Pts',(5.06235407931748,29.0891721664285,126.395308878475));
#122047=CARTESIAN_POINT('Ctrl Pts',(5.06432799290853,29.063672050337,126.378326655157));
#122048=CARTESIAN_POINT('Ctrl Pts',(5.06899151255869,29.003893478202,126.336091012022));
#122049=CARTESIAN_POINT('Ctrl Pts',(5.07165848122883,28.9700858794517,126.310207876848));
#122050=CARTESIAN_POINT('Ctrl Pts',(5.07886539854358,28.8805548991423,126.236053608914));
#122051=CARTESIAN_POINT('Ctrl Pts',(5.08333799662581,28.826984711163,126.185335966073));
#122052=CARTESIAN_POINT('Ctrl Pts',(5.08870729896525,28.7673905716162,126.120905044818));
#122053=CARTESIAN_POINT('Ctrl Pts',(5.08956963572815,28.7579644472012,126.110451170399));
#122054=CARTESIAN_POINT('Ctrl Pts',(5.09493171087788,28.7003393052001,126.044891285209));
#122055=CARTESIAN_POINT('Ctrl Pts',(5.09948404095198,28.6556895946933,125.986783941282));
#122056=CARTESIAN_POINT('Ctrl Pts',(5.10506702532268,28.6081867669985,125.915730679814));
#122057=CARTESIAN_POINT('Ctrl Pts',(5.10587535048109,28.6014760351014,125.90544875689));
#122058=CARTESIAN_POINT('Ctrl Pts',(5.1071525173104,28.5911453449174,125.889231620139));
#122059=CARTESIAN_POINT('Ctrl Pts',(5.10761648274811,28.5874476970702,125.88334608196));
#122060=CARTESIAN_POINT('Ctrl Pts',(5.10848921171111,28.5805979360069,125.872290345407));
#122061=CARTESIAN_POINT('Ctrl Pts',(5.10889740105742,28.5774370411825,125.867125878679));
#122062=CARTESIAN_POINT('Ctrl Pts',(5.1098639854839,28.5700518312273,125.854910402286));
#122063=CARTESIAN_POINT('Ctrl Pts',(5.11042386723923,28.5658514678204,125.847845234625));
#122064=CARTESIAN_POINT('Ctrl Pts',(5.11230974584357,28.5519554263393,125.824072842979));
#122065=CARTESIAN_POINT('Ctrl Pts',(5.11364931045251,28.5424984731596,125.807228813635));
#122066=CARTESIAN_POINT('Ctrl Pts',(5.11698449651718,28.5199113062932,125.765306883766));
#122067=CARTESIAN_POINT('Ctrl Pts',(5.11899472939815,28.5071235348106,125.740051921382));
#122068=CARTESIAN_POINT('Ctrl Pts',(5.12821538155622,28.451937431038,125.623806153446));
#122069=CARTESIAN_POINT('Ctrl Pts',(5.13559855851799,28.4171722790135,125.529423004262));
#122070=CARTESIAN_POINT('Ctrl Pts',(5.14876997769516,28.3697457712846,125.352991177952));
#122071=CARTESIAN_POINT('Ctrl Pts',(5.15459129391607,28.3542955681113,125.272015090418));
#122072=CARTESIAN_POINT('Ctrl Pts',(5.16156721043594,28.342656882081,125.170745276547));
#122073=CARTESIAN_POINT('Ctrl Pts',(5.16289786397962,28.340762749002,125.151234790322));
#122074=CARTESIAN_POINT('Ctrl Pts',(5.16501414313744,28.3382784375587,125.119905418752));
#122075=CARTESIAN_POINT('Ctrl Pts',(5.16580653879206,28.3374691269613,125.10810628661));
#122076=CARTESIAN_POINT('Ctrl Pts',(5.1673112033387,28.3361645657059,125.085574805121));
#122077=CARTESIAN_POINT('Ctrl Pts',(5.16802412179771,28.3356473547087,125.07484437865));
#122078=CARTESIAN_POINT('Ctrl Pts',(5.16965777434659,28.3346957844673,125.05013443285));
#122079=CARTESIAN_POINT('Ctrl Pts',(5.17057621484759,28.334333591356,125.036152821475));
#122080=CARTESIAN_POINT('Ctrl Pts',(5.17348922035691,28.3337399336835,124.99154128465));
#122081=CARTESIAN_POINT('Ctrl Pts',(5.17546308238214,28.3341770360683,124.960907799184));
#122082=CARTESIAN_POINT('Ctrl Pts',(5.18012645394362,28.3372390291876,124.887780503026));
#122083=CARTESIAN_POINT('Ctrl Pts',(5.18279332813655,28.3406482725798,124.845340738013));
#122084=CARTESIAN_POINT('Ctrl Pts',(5.19000020116968,28.3543894324385,124.729904054905));
#122085=CARTESIAN_POINT('Ctrl Pts',(5.19447284304928,28.367944796246,124.657389238388));
#122086=CARTESIAN_POINT('Ctrl Pts',(5.19984187937073,28.3897529073344,124.572380680672));
#122087=CARTESIAN_POINT('Ctrl Pts',(5.2007039088472,28.3934218549189,124.558796374364));
#122088=CARTESIAN_POINT('Ctrl Pts',(5.20606609574129,28.4172472508609,124.47482337492));
#122089=CARTESIAN_POINT('Ctrl Pts',(5.21061884209723,28.4418512940101,124.405789048505));
#122090=CARTESIAN_POINT('Ctrl Pts',(5.21620228849069,28.475785209564,124.327336617031));
#122091=CARTESIAN_POINT('Ctrl Pts',(5.21701061538136,28.4807838511674,124.316122068249));
#122092=CARTESIAN_POINT('Ctrl Pts',(5.21828778435916,28.4888055918879,124.29864718267));
#122093=CARTESIAN_POINT('Ctrl Pts',(5.21875175018648,28.4917448198266,124.292348517567));
#122094=CARTESIAN_POINT('Ctrl Pts',(5.21962447944393,28.4973181629705,124.280597496109));
#122095=CARTESIAN_POINT('Ctrl Pts',(5.22003266869008,28.49994269986,124.275140870545));
#122096=CARTESIAN_POINT('Ctrl Pts',(5.2209992522832,28.5061999753993,124.262311008866));
#122097=CARTESIAN_POINT('Ctrl Pts',(5.22155913329749,28.5098575992237,124.254950216788));
#122098=CARTESIAN_POINT('Ctrl Pts',(5.22344500673452,28.5222930722812,124.230382321442));
#122099=CARTESIAN_POINT('Ctrl Pts',(5.22478456682007,28.5313153316397,124.213301582077));
#122100=CARTESIAN_POINT('Ctrl Pts',(5.22811973909698,28.5542852032068,124.171588335049));
#122101=CARTESIAN_POINT('Ctrl Pts',(5.23012996256916,28.5685672974179,124.147147493787));
#122102=CARTESIAN_POINT('Ctrl Pts',(5.23935053098661,28.636298820608,124.037736666752));
#122103=CARTESIAN_POINT('Ctrl Pts',(5.24673363132664,28.6967381215495,123.957339660999));
#122104=CARTESIAN_POINT('Ctrl Pts',(5.25990506772165,28.8192435466228,123.82180391584));
#122105=CARTESIAN_POINT('Ctrl Pts',(5.2657264699393,28.8788962343529,123.764904122622));
#122106=CARTESIAN_POINT('Ctrl Pts',(5.27270246959723,28.9576659371131,123.700200068183));
#122107=CARTESIAN_POINT('Ctrl Pts',(5.2740331256744,28.9730302641684,123.688026913378));
#122108=CARTESIAN_POINT('Ctrl Pts',(5.27614940787022,28.99800406661,123.668947780821));
#122109=CARTESIAN_POINT('Ctrl Pts',(5.27694180406383,29.0074780963142,123.661868413085));
#122110=CARTESIAN_POINT('Ctrl Pts',(5.27844646902708,29.0257002322304,123.64855212377));
#122111=CARTESIAN_POINT('Ctrl Pts',(5.27915938737013,29.0344348123309,123.642297795088));
#122112=CARTESIAN_POINT('Ctrl Pts',(5.28079303879772,29.0546786015462,123.628096561409));
#122113=CARTESIAN_POINT('Ctrl Pts',(5.28171147830432,29.0662287083991,123.620209151381));
#122114=CARTESIAN_POINT('Ctrl Pts',(5.28462447706611,29.1033867358027,123.595514753564));
#122115=CARTESIAN_POINT('Ctrl Pts',(5.28659833347796,29.1293602515496,123.579267523329));
#122116=CARTESIAN_POINT('Ctrl Pts',(5.29126168891873,29.1924581602637,123.542178534906));
#122117=CARTESIAN_POINT('Ctrl Pts',(5.29392855282703,29.2299625480471,123.522025050736));
#122118=CARTESIAN_POINT('Ctrl Pts',(5.30113542103113,29.3343985313334,123.470960871794));
#122119=CARTESIAN_POINT('Ctrl Pts',(5.30560806767021,29.402673386095,123.443019830104));
#122120=CARTESIAN_POINT('Ctrl Pts',(5.31097707484294,29.4859202551149,123.415236300833));
#122121=CARTESIAN_POINT('Ctrl Pts',(5.31183907068656,29.4993224027386,123.410951258228));
#122122=CARTESIAN_POINT('Ctrl Pts',(5.31720126974645,29.5827939947003,123.385423890155));
#122123=CARTESIAN_POINT('Ctrl Pts',(5.32175406160045,29.6541378297784,123.368652852121));
#122124=CARTESIAN_POINT('Ctrl Pts',(5.32733755849163,29.7384544348061,123.354612303568));
#122125=CARTESIAN_POINT('Ctrl Pts',(5.32814588557151,29.7505873522995,123.352729511085));
#122126=CARTESIAN_POINT('Ctrl Pts',(5.32942305478397,29.7696194724705,123.349991173954));
#122127=CARTESIAN_POINT('Ctrl Pts',(5.32988702065385,29.7765053877053,123.349044377521));
#122128=CARTESIAN_POINT('Ctrl Pts',(5.33075974994338,29.789400714346,123.347353453753));
#122129=CARTESIAN_POINT('Ctrl Pts',(5.33116793917849,29.7954085175658,123.34659896378));
#122130=CARTESIAN_POINT('Ctrl Pts',(5.33213452268102,29.8095811634394,123.344897517432));
#122131=CARTESIAN_POINT('Ctrl Pts',(5.33269440361449,29.8177490481325,123.34397821736));
#122132=CARTESIAN_POINT('Ctrl Pts',(5.33458027648687,29.8451341530161,123.34110105656));
#122133=CARTESIAN_POINT('Ctrl Pts',(5.33591983607837,29.8643777686456,123.339417070444));
#122134=CARTESIAN_POINT('Ctrl Pts',(5.33925500684945,29.9118808967923,123.336091293626));
#122135=CARTESIAN_POINT('Ctrl Pts',(5.34126522929403,29.9401607930236,123.334834468322));
#122136=CARTESIAN_POINT('Ctrl Pts',(5.35048578856561,30.0688166143859,123.332398164924));
#122137=CARTESIAN_POINT('Ctrl Pts',(5.35786888053724,30.1691416359921,123.339571383381));
#122138=CARTESIAN_POINT('Ctrl Pts',(5.37104207867903,30.3494777771977,123.368987695162));
#122139=CARTESIAN_POINT('Ctrl Pts',(5.37686517540465,30.4296587910167,123.388251617995));
#122140=CARTESIAN_POINT('Ctrl Pts',(5.38384184190729,30.5267511615722,123.419344163597));
#122141=CARTESIAN_POINT('Ctrl Pts',(5.38517160844966,30.5452990806009,123.425646599748));
#122142=CARTESIAN_POINT('Ctrl Pts',(5.38728682396925,30.5748583436767,123.436275701722));
#122143=CARTESIAN_POINT('Ctrl Pts',(5.38807903090096,30.5859417741661,123.440394907009));
#122144=CARTESIAN_POINT('Ctrl Pts',(5.3895835496665,30.6070103828556,123.448481450394));
#122145=CARTESIAN_POINT('Ctrl Pts',(5.39029650884441,30.6170028244621,123.452428050625));
#122146=CARTESIAN_POINT('Ctrl Pts',(5.39193055457517,30.6399189587419,123.461736215586));
#122147=CARTESIAN_POINT('Ctrl Pts',(5.39284934367759,30.6528148002263,123.467164522663));
#122148=CARTESIAN_POINT('Ctrl Pts',(5.39576471541366,30.6937481665943,123.485005095427));
#122149=CARTESIAN_POINT('Ctrl Pts',(5.39774054604783,30.7215130309643,123.498029555853));
#122150=CARTESIAN_POINT('Ctrl Pts',(5.40240957233133,30.7869741797879,123.530971746993));
#122151=CARTESIAN_POINT('Ctrl Pts',(5.40508005444592,30.8242968849747,123.551584522475));
#122152=CARTESIAN_POINT('Ctrl Pts',(5.4123368675085,30.9245241718314,123.612069020306));
#122153=CARTESIAN_POINT('Ctrl Pts',(5.41685383658555,30.9856091454516,123.654759383831));
#122154=CARTESIAN_POINT('Ctrl Pts',(5.42221449123898,31.0538976593136,123.709639950839));
#122155=CARTESIAN_POINT('Ctrl Pts',(5.42302120683429,31.0640617267757,123.718008592365));
#122156=CARTESIAN_POINT('Ctrl Pts',(5.42833063752569,31.1301297359296,123.773733091716));
#122157=CARTESIAN_POINT('Ctrl Pts',(5.4328862029799,31.1829502843929,123.824606592241));
#122158=CARTESIAN_POINT('Ctrl Pts',(5.43847277833247,31.2405084362413,123.887864406536));
#122159=CARTESIAN_POINT('Ctrl Pts',(5.43928111693002,31.2486708336146,123.897036770262));
#122160=CARTESIAN_POINT('Ctrl Pts',(5.44055830042732,31.2612939157065,123.911541469668));
#122161=CARTESIAN_POINT('Ctrl Pts',(5.44102226888773,31.2658240609743,123.916813148005));
#122162=CARTESIAN_POINT('Ctrl Pts',(5.44189500013556,31.2742386636389,123.926729999525));
#122163=CARTESIAN_POINT('Ctrl Pts',(5.44230318870524,31.2781309553681,123.931368200886));
#122164=CARTESIAN_POINT('Ctrl Pts',(5.44326976666608,31.2872470999813,123.942352391604));
#122165=CARTESIAN_POINT('Ctrl Pts',(5.44382964267218,31.2924493682281,123.948715935895));
#122166=CARTESIAN_POINT('Ctrl Pts',(5.44571548119146,31.3097189900807,123.970162495472));
#122167=CARTESIAN_POINT('Ctrl Pts',(5.44705501070969,31.3215705764539,123.985416218034));
#122168=CARTESIAN_POINT('Ctrl Pts',(5.4545075053824,31.3853843042896,124.070563944558));
#122169=CARTESIAN_POINT('Ctrl Pts',(5.46085769394969,31.4320654938738,124.144238899093));
#122170=CARTESIAN_POINT('Ctrl Pts',(5.47370805071857,31.514594526569,124.300311182841));
#122171=CARTESIAN_POINT('Ctrl Pts',(5.4801850450461,31.5499832386887,124.382653766623));
#122172=CARTESIAN_POINT('Ctrl Pts',(5.48939019275632,31.5918863134997,124.506862815249));
#122173=CARTESIAN_POINT('Ctrl Pts',(5.49226837628911,31.6037032851654,124.546764283238));
#122174=CARTESIAN_POINT('Ctrl Pts',(5.49619602346351,31.6180116664799,124.602691229674));
#122175=CARTESIAN_POINT('Ctrl Pts',(5.49728581892356,31.6217814459432,124.618370618012));
#122176=CARTESIAN_POINT('Ctrl Pts',(5.49903924546741,31.6275181243303,124.643853061928));
#122177=CARTESIAN_POINT('Ctrl Pts',(5.49970732654887,31.6296253975822,124.653623098934));
#122178=CARTESIAN_POINT('Ctrl Pts',(5.5011015085536,31.6338570064753,124.674136236065));
#122179=CARTESIAN_POINT('Ctrl Pts',(5.50182701382798,31.6359636018971,124.684882540548));
#122180=CARTESIAN_POINT('Ctrl Pts',(5.50326585811388,31.6399493304295,124.706333042058));
#122181=CARTESIAN_POINT('Ctrl Pts',(5.50397921216962,31.6418299846005,124.717036399002));
#122182=CARTESIAN_POINT('Ctrl Pts',(5.50565528089859,31.6460211659661,124.742339769015));
#122183=CARTESIAN_POINT('Ctrl Pts',(5.50661520089376,31.6482424077205,124.756953788149));
#122184=CARTESIAN_POINT('Ctrl Pts',(5.5125320454875,31.6608072246128,124.847737268346));
#122185=CARTESIAN_POINT('Ctrl Pts',(5.51732912507926,31.6660638404818,124.924519570155));
#122186=CARTESIAN_POINT('Ctrl Pts',(5.52205824491057,31.6659994149782,125.001396170626));
#122187=CARTESIAN_POINT('Ctrl Pts',(5.52205815882027,31.6659994161504,125.001394771142));
#122188=CARTESIAN_POINT('Ctrl Pts',(5.52952817550204,31.6658977530252,125.12282738621));
#122189=CARTESIAN_POINT('Ctrl Pts',(5.53677883282065,31.6525201216262,125.243875523706));
#122190=CARTESIAN_POINT('Ctrl Pts',(5.54571783249626,31.6219777811608,125.380926412135));
#122191=CARTESIAN_POINT('Ctrl Pts',(5.54693875696725,31.617529138693,125.399394886252));
#122192=CARTESIAN_POINT('Ctrl Pts',(5.549107440675,31.6091692314404,125.43166664503));
#122193=CARTESIAN_POINT('Ctrl Pts',(5.55004877350797,31.6053935658685,125.445503280201));
#122194=CARTESIAN_POINT('Ctrl Pts',(5.55148435318858,31.5994253101844,125.466313283183));
#122195=CARTESIAN_POINT('Ctrl Pts',(5.55197142621871,31.5973645787756,125.473324200069));
#122196=CARTESIAN_POINT('Ctrl Pts',(5.55286385855791,31.5935256100598,125.486074304289));
#122197=CARTESIAN_POINT('Ctrl Pts',(5.55326836036909,31.5917623625524,125.491817727222));
#122198=CARTESIAN_POINT('Ctrl Pts',(5.55419554837357,31.5876679445464,125.504901787628));
#122199=CARTESIAN_POINT('Ctrl Pts',(5.55471934058999,31.5853169223576,125.512235851038));
#122200=CARTESIAN_POINT('Ctrl Pts',(5.5563655655747,31.5778072627781,125.535115423373));
#122201=CARTESIAN_POINT('Ctrl Pts',(5.55749742930064,31.5724703467732,125.550600792995));
#122202=CARTESIAN_POINT('Ctrl Pts',(5.55887450521995,31.565760403058,125.569176366074));
#122203=CARTESIAN_POINT('Ctrl Pts',(5.55911008052214,31.5646049816606,125.572344847383));
#122204=CARTESIAN_POINT('Ctrl Pts',(5.55934605048515,31.5634400125327,125.575509623909));
#122205=CARTESIAN_POINT('',(5.32851907198357,31.6679764309607,125.000530942783));
#122206=CARTESIAN_POINT('Ctrl Pts',(5.36787244251734,31.5634400119422,125.575509625513));
#122207=CARTESIAN_POINT('Ctrl Pts',(5.36380377202413,31.5844917329173,125.518320133915));
#122208=CARTESIAN_POINT('Ctrl Pts',(5.35973510153093,31.6023841697817,125.460021086487));
#122209=CARTESIAN_POINT('Ctrl Pts',(5.35566643103772,31.6170218318539,125.400994258448));
#122210=CARTESIAN_POINT('Ctrl Pts',(5.35159020376397,31.6316866805955,125.341857799317));
#122211=CARTESIAN_POINT('Ctrl Pts',(5.34751397649022,31.6430845848598,125.281991363721));
#122212=CARTESIAN_POINT('Ctrl Pts',(5.34343774921647,31.6511713932636,125.221786000613));
#122213=CARTESIAN_POINT('Ctrl Pts',(5.34045616622793,31.6570865419413,125.17774839564));
#122214=CARTESIAN_POINT('Ctrl Pts',(5.33747458323939,31.6612312483094,125.133529634148));
#122215=CARTESIAN_POINT('Ctrl Pts',(5.33449300025085,31.6636058986978,125.089282774474));
#122216=CARTESIAN_POINT('Ctrl Pts',(5.33250187903717,31.6651917062308,125.059734423388));
#122217=CARTESIAN_POINT('Ctrl Pts',(5.33051075782348,31.6659903400224,125.030143448948));
#122218=CARTESIAN_POINT('Ctrl Pts',(5.3285196366098,31.6659999129021,125.000538711647));
#122219=CARTESIAN_POINT('Ctrl Pts',(5.32851890484269,31.6685615206205,125.00052864304));
#122220=CARTESIAN_POINT('Ctrl Pts',(5.29346517969922,31.6663498316797,124.478534520954));
#122221=CARTESIAN_POINT('Ctrl Pts',(5.22136636427624,31.1216475883581,123.40092281885));
#122222=CARTESIAN_POINT('Ctrl Pts',(5.11222245857374,29.2866679733565,123.164583862537));
#122223=CARTESIAN_POINT('Ctrl Pts',(5.00108718773517,28.0711012827654,124.603837512444));
#122224=CARTESIAN_POINT('Ctrl Pts',(4.88995191689663,28.6210012493043,126.405687526968));
#122225=CARTESIAN_POINT('Ctrl Pts',(4.77886137758078,30.4323305780535,126.920743955777));
#122226=CARTESIAN_POINT('Ctrl Pts',(4.70481592854447,31.3757142918801,126.093332246506));
#122227=CARTESIAN_POINT('Ctrl Pts',(4.66781556978768,31.5660436956742,125.576468401513));
#122228=CARTESIAN_POINT('Origin',(5.,30.,125.));
#122229=CARTESIAN_POINT('',(3.96713561979274,31.5634400104587,125.575509629543));
#122230=CARTESIAN_POINT('',(4.16231120066723,31.5634400119557,125.575509625476));
#122231=CARTESIAN_POINT('',(5.,31.5634400119422,125.575509625513));
#122232=CARTESIAN_POINT('Ctrl Pts',(4.16231120066723,31.5634400119558,125.575509625476));
#122233=CARTESIAN_POINT('Ctrl Pts',(4.16319058703546,31.5589599896281,125.587680136362));
#122234=CARTESIAN_POINT('Ctrl Pts',(4.16406524665906,31.554337873318,125.59979828981));
#122235=CARTESIAN_POINT('Ctrl Pts',(4.16567097839286,31.5455459090605,125.62206444262));
#122236=CARTESIAN_POINT('Ctrl Pts',(4.16640334762147,31.5414164942572,125.632227434503));
#122237=CARTESIAN_POINT('Ctrl Pts',(4.16779517503746,31.5333413397352,125.651551851126));
#122238=CARTESIAN_POINT('Ctrl Pts',(4.16845518751511,31.5294131298379,125.660720034854));
#122239=CARTESIAN_POINT('Ctrl Pts',(4.17016732897336,31.5189663013785,125.684509778734));
#122240=CARTESIAN_POINT('Ctrl Pts',(4.17121502931073,31.5123187561079,125.699073866687));
#122241=CARTESIAN_POINT('Ctrl Pts',(4.17490877765944,31.4879873140498,125.750409529617));
#122242=CARTESIAN_POINT('Ctrl Pts',(4.17751573861791,31.4691630315169,125.786626413127));
#122243=CARTESIAN_POINT('Ctrl Pts',(4.18745721451471,31.3913217619973,125.923825785018));
#122244=CARTESIAN_POINT('Ctrl Pts',(4.19448379154936,31.3230706609143,126.019173786773));
#122245=CARTESIAN_POINT('Ctrl Pts',(4.20468121314224,31.21288702587,126.143178243967));
#122246=CARTESIAN_POINT('Ctrl Pts',(4.20771729517768,31.1787836554665,126.178312296051));
#122247=CARTESIAN_POINT('Ctrl Pts',(4.21205002789272,31.1292622752695,126.22502616147));
#122248=CARTESIAN_POINT('Ctrl Pts',(4.21327996640977,31.1151138180846,126.237919015802));
#122249=CARTESIAN_POINT('Ctrl Pts',(4.21519394755994,31.093025012955,126.257361582333));
#122250=CARTESIAN_POINT('Ctrl Pts',(4.21586732731321,31.0852404281857,126.264086638059));
#122251=CARTESIAN_POINT('Ctrl Pts',(4.21709875135551,31.0709930528768,126.276166255583));
#122252=CARTESIAN_POINT('Ctrl Pts',(4.21765518008878,31.0645510649365,126.281544948101));
#122253=CARTESIAN_POINT('Ctrl Pts',(4.2186246014314,31.0533269192791,126.290773445787));
#122254=CARTESIAN_POINT('Ctrl Pts',(4.21903599390885,31.0485635082625,126.294645995778));
#122255=CARTESIAN_POINT('Ctrl Pts',(4.21983196103034,31.0393495033326,126.302052574293));
#122256=CARTESIAN_POINT('Ctrl Pts',(4.22021623946143,31.0349020409072,126.305590310768));
#122257=CARTESIAN_POINT('Ctrl Pts',(4.22125694631312,31.0228574639984,126.315070965117));
#122258=CARTESIAN_POINT('Ctrl Pts',(4.22191627524253,31.0152268362459,126.32097066385));
#122259=CARTESIAN_POINT('Ctrl Pts',(4.22445583620608,30.9858202384963,126.343301391327));
#122260=CARTESIAN_POINT('Ctrl Pts',(4.22636381832533,30.9636943533992,126.359261990562));
#122261=CARTESIAN_POINT('Ctrl Pts',(4.23828066895123,30.8247539430314,126.454389530815));
#122262=CARTESIAN_POINT('Ctrl Pts',(4.24875982908233,30.6986629412363,126.518993915378));
#122263=CARTESIAN_POINT('Ctrl Pts',(4.26177503365491,30.5269491191074,126.581011789793));
#122264=CARTESIAN_POINT('Ctrl Pts',(4.26469428421219,30.487454794372,126.593631684596));
#122265=CARTESIAN_POINT('Ctrl Pts',(4.26965324794239,30.4185891917061,126.612836531113));
#122266=CARTESIAN_POINT('Ctrl Pts',(4.27171314914196,30.3894358271902,126.620122997255));
#122267=CARTESIAN_POINT('Ctrl Pts',(4.27468821168877,30.3465451244102,126.629618116513));
#122268=CARTESIAN_POINT('Ctrl Pts',(4.27562296846786,30.3329532924104,126.632449342017));
#122269=CARTESIAN_POINT('Ctrl Pts',(4.27727056627474,30.3087966052571,126.637166998658));
#122270=CARTESIAN_POINT('Ctrl Pts',(4.27798554443899,30.2982460896326,126.639121839336));
#122271=CARTESIAN_POINT('Ctrl Pts',(4.27948527629863,30.2759768807872,126.643025826409));
#122272=CARTESIAN_POINT('Ctrl Pts',(4.28026926066304,30.2642547028447,126.644951844067));
#122273=CARTESIAN_POINT('Ctrl Pts',(4.28235275218274,30.232894844977,126.649760558191));
#122274=CARTESIAN_POINT('Ctrl Pts',(4.28364514455263,30.2132241916118,126.652418048444));
#122275=CARTESIAN_POINT('Ctrl Pts',(4.29092516026438,30.1012955810992,126.665507431881));
#122276=CARTESIAN_POINT('Ctrl Pts',(4.29667517862958,30.008335689306,126.668565096381));
#122277=CARTESIAN_POINT('Ctrl Pts',(4.30674853932338,29.8440315204372,126.660230209088));
#122278=CARTESIAN_POINT('Ctrl Pts',(4.31109083183077,29.7727790608835,126.651986857076));
#122279=CARTESIAN_POINT('Ctrl Pts',(4.31795495956892,29.6637088657278,126.632176816563));
#122280=CARTESIAN_POINT('Ctrl Pts',(4.32040918598953,29.6253984908349,126.62381224196));
#122281=CARTESIAN_POINT('Ctrl Pts',(4.32447237417068,29.5638658489251,126.608083990391));
#122282=CARTESIAN_POINT('Ctrl Pts',(4.32604793989103,29.5404463517141,126.601548442702));
#122283=CARTESIAN_POINT('Ctrl Pts',(4.32824200481638,29.5085869564058,126.591901324369));
#122284=CARTESIAN_POINT('Ctrl Pts',(4.32883737485338,29.5000155841861,126.589230059145));
#122285=CARTESIAN_POINT('Ctrl Pts',(4.32984895519503,29.4855855493209,126.58460465465));
#122286=CARTESIAN_POINT('Ctrl Pts',(4.3302630862102,29.4797152426027,126.582686926873));
#122287=CARTESIAN_POINT('Ctrl Pts',(4.3311246768605,29.4675822858722,126.57864850247));
#122288=CARTESIAN_POINT('Ctrl Pts',(4.33157238172558,29.4613214357542,126.576523110283));
#122289=CARTESIAN_POINT('Ctrl Pts',(4.33277352031084,29.4446362270969,126.570747932771));
#122290=CARTESIAN_POINT('Ctrl Pts',(4.33353063290721,29.4342354436852,126.567031728767));
#122291=CARTESIAN_POINT('Ctrl Pts',(4.33706867090928,29.3861340105069,126.549303782684));
#122292=CARTESIAN_POINT('Ctrl Pts',(4.33991086584414,29.3489145563841,126.534034169986));
#122293=CARTESIAN_POINT('Ctrl Pts',(4.3493206248095,29.2292066346742,126.479781658319));
#122294=CARTESIAN_POINT('Ctrl Pts',(4.35601718698825,29.1493599045371,126.43537011905));
#122295=CARTESIAN_POINT('Ctrl Pts',(4.36709643973142,29.0221146494648,126.350231925024));
#122296=CARTESIAN_POINT('Ctrl Pts',(4.37152507249643,28.9726325240827,126.312975018402));
#122297=CARTESIAN_POINT('Ctrl Pts',(4.37864351690706,28.894982183219,126.247425100924));
#122298=CARTESIAN_POINT('Ctrl Pts',(4.3813862397343,28.8655540471636,126.220723800427));
#122299=CARTESIAN_POINT('Ctrl Pts',(4.38513247215379,28.826071308131,126.182237245629));
#122300=CARTESIAN_POINT('Ctrl Pts',(4.3861728394732,28.8151856987691,126.171327698753));
#122301=CARTESIAN_POINT('Ctrl Pts',(4.38794229809535,28.7968135455444,126.152396924661));
#122302=CARTESIAN_POINT('Ctrl Pts',(4.38867462956843,28.7892521599083,126.144450083571));
#122303=CARTESIAN_POINT('Ctrl Pts',(4.39015468248037,28.7740601524281,126.128164539176));
#122304=CARTESIAN_POINT('Ctrl Pts',(4.39090215712362,28.7664347948603,126.119821696806));
#122305=CARTESIAN_POINT('Ctrl Pts',(4.39277244530255,28.7474793569807,126.098654109383));
#122306=CARTESIAN_POINT('Ctrl Pts',(4.39389058943712,28.7362606958482,126.085731007152));
#122307=CARTESIAN_POINT('Ctrl Pts',(4.39821587929387,28.6933446490841,126.034728158176));
#122308=CARTESIAN_POINT('Ctrl Pts',(4.40136294724094,28.6631514106822,125.99541304205));
#122309=CARTESIAN_POINT('Ctrl Pts',(4.41189628154717,28.5666641679311,125.857449200472));
#122310=CARTESIAN_POINT('Ctrl Pts',(4.41900492270334,28.5091870388347,125.753091473105));
#122311=CARTESIAN_POINT('Ctrl Pts',(4.42884562177325,28.4477416979857,125.606359832775));
#122312=CARTESIAN_POINT('Ctrl Pts',(4.43136421206043,28.4335382621367,125.568660954391));
#122313=CARTESIAN_POINT('Ctrl Pts',(4.4355221579014,28.4128303397632,125.507012530812));
#122314=CARTESIAN_POINT('Ctrl Pts',(4.43712614451108,28.4054699875807,125.483366445528));
#122315=CARTESIAN_POINT('Ctrl Pts',(4.43935355468554,28.3961461537136,125.45087754303));
#122316=CARTESIAN_POINT('Ctrl Pts',(4.4399529273415,28.3937233385711,125.442168516331));
#122317=CARTESIAN_POINT('Ctrl Pts',(4.44096928204918,28.3897618869612,125.427466372996));
#122318=CARTESIAN_POINT('Ctrl Pts',(4.44138413823894,28.3881855015162,125.421483453766));
#122319=CARTESIAN_POINT('Ctrl Pts',(4.44218977871404,28.3852031845383,125.409903099919));
#122320=CARTESIAN_POINT('Ctrl Pts',(4.44258027642,28.3837929585358,125.404306941705));
#122321=CARTESIAN_POINT('Ctrl Pts',(4.44365865606108,28.3799944816574,125.388896070233));
#122322=CARTESIAN_POINT('Ctrl Pts',(4.44434980275872,28.3776664207772,125.379066983391));
#122323=CARTESIAN_POINT('Ctrl Pts',(4.44717556007952,28.368571834471,125.339050448907));
#122324=CARTESIAN_POINT('Ctrl Pts',(4.44934614872122,28.3625578221788,125.308700328386));
#122325=CARTESIAN_POINT('Ctrl Pts',(4.4593000480868,28.33915876353,125.170544040238));
#122326=CARTESIAN_POINT('Ctrl Pts',(4.46734653090748,28.3315534069206,125.061356211219));
#122327=CARTESIAN_POINT('Ctrl Pts',(4.47938671832493,28.3363372292898,124.894655331219));
#122328=CARTESIAN_POINT('Ctrl Pts',(4.48349491064335,28.3409716220761,124.837220208576));
#122329=CARTESIAN_POINT('Ctrl Pts',(4.49016954584143,28.3535684389535,124.742604002876));
#122330=CARTESIAN_POINT('Ctrl Pts',(4.49278066319695,28.3598435421195,124.705251332033));
#122331=CARTESIAN_POINT('Ctrl Pts',(4.49638054881835,28.3704031023441,124.653302332234));
#122332=CARTESIAN_POINT('Ctrl Pts',(4.49740245511979,28.3736218531016,124.638503843338));
#122333=CARTESIAN_POINT('Ctrl Pts',(4.49915025000755,28.3795084708342,124.613111803149));
#122334=CARTESIAN_POINT('Ctrl Pts',(4.49987918061958,28.3820795198762,124.602497040587));
#122335=CARTESIAN_POINT('Ctrl Pts',(4.50127101140126,28.3872112272003,124.582185523349));
#122336=CARTESIAN_POINT('Ctrl Pts',(4.50193440561334,28.3897554171307,124.572485142534));
#122337=CARTESIAN_POINT('Ctrl Pts',(4.50366981427321,28.396668662493,124.547064215024));
#122338=CARTESIAN_POINT('Ctrl Pts',(4.50473715294574,28.4011814047808,124.531383596488));
#122339=CARTESIAN_POINT('Ctrl Pts',(4.50858775156105,28.4184044451597,124.47468551383));
#122340=CARTESIAN_POINT('Ctrl Pts',(4.51132723006017,28.4324694376922,124.434095215161));
#122341=CARTESIAN_POINT('Ctrl Pts',(4.52125756321136,28.4898846005365,124.287038054555));
#122342=CARTESIAN_POINT('Ctrl Pts',(4.52816326411835,28.5426443521346,124.18459921125));
#122343=CARTESIAN_POINT('Ctrl Pts',(4.5382056402252,28.632002177851,124.047908238331));
#122344=CARTESIAN_POINT('Ctrl Pts',(4.54120833510575,28.6602250770414,124.008587232885));
#122345=CARTESIAN_POINT('Ctrl Pts',(4.54549778742929,28.7018598538428,123.955610543496));
#122346=CARTESIAN_POINT('Ctrl Pts',(4.54671923867236,28.7138574075062,123.94087095061));
#122347=CARTESIAN_POINT('Ctrl Pts',(4.54888876933783,28.7353501460472,123.915369835031));
#122348=CARTESIAN_POINT('Ctrl Pts',(4.54983041535226,28.7447373294063,123.904519538375));
#122349=CARTESIAN_POINT('Ctrl Pts',(4.55126637743371,28.759115900008,123.8883273568));
#122350=CARTESIAN_POINT('Ctrl Pts',(4.55175351395751,28.764004515797,123.882894555896));
#122351=CARTESIAN_POINT('Ctrl Pts',(4.55264600549826,28.7729767699733,123.873054530373));
#122352=CARTESIAN_POINT('Ctrl Pts',(4.55305050226626,28.777048710634,123.868636999535));
#122353=CARTESIAN_POINT('Ctrl Pts',(4.55397760457306,28.7863941837865,123.858607770252));
#122354=CARTESIAN_POINT('Ctrl Pts',(4.55450131526568,28.791682766488,123.853010568232));
#122355=CARTESIAN_POINT('Ctrl Pts',(4.55614702402541,28.8083366521187,123.83562783675));
#122356=CARTESIAN_POINT('Ctrl Pts',(4.5572784449458,28.8198366214168,123.823973461583));
#122357=CARTESIAN_POINT('Ctrl Pts',(4.56384081447224,28.886924392363,123.757959929136));
#122358=CARTESIAN_POINT('Ctrl Pts',(4.56947637030779,28.9460870302979,123.707380181069));
#122359=CARTESIAN_POINT('Ctrl Pts',(4.57997711671616,29.062060175513,123.621501892103));
#122360=CARTESIAN_POINT('Ctrl Pts',(4.58482823244832,29.117891823969,123.585123999372));
#122361=CARTESIAN_POINT('Ctrl Pts',(4.59482948120842,29.2390456792669,123.516150641602));
#122362=CARTESIAN_POINT('Ctrl Pts',(4.5999533195312,29.3046403192063,123.48430282542));
#122363=CARTESIAN_POINT('Ctrl Pts',(4.60620495545551,29.3893839370133,123.449822107671));
#122364=CARTESIAN_POINT('Ctrl Pts',(4.60746903192942,29.406767345019,123.443086855244));
#122365=CARTESIAN_POINT('Ctrl Pts',(4.60950543731256,29.4351671576774,123.432628014138));
#122366=CARTESIAN_POINT('Ctrl Pts',(4.61028365211428,29.4461155158327,123.428725653531));
#122367=CARTESIAN_POINT('Ctrl Pts',(4.6117780754605,29.4673201051505,123.421416807166));
#122368=CARTESIAN_POINT('Ctrl Pts',(4.61249476099101,29.4775703675198,123.41799492556));
#122369=CARTESIAN_POINT('Ctrl Pts',(4.61414500163495,29.5013554597621,123.410311051165));
#122370=CARTESIAN_POINT('Ctrl Pts',(4.61507614156788,29.5149130180437,123.406121719806));
#122371=CARTESIAN_POINT('Ctrl Pts',(4.61805143589898,29.5586547473912,123.393215214038));
#122372=CARTESIAN_POINT('Ctrl Pts',(4.62007372595736,29.5890335590473,123.385178100508));
#122373=CARTESIAN_POINT('Ctrl Pts',(4.63095222128706,29.7554788903902,123.346144728701));
#122374=CARTESIAN_POINT('Ctrl Pts',(4.63927654918687,29.8947923300856,123.331479819019));
#122375=CARTESIAN_POINT('Ctrl Pts',(4.65053615341447,30.077157536108,123.33523582151));
#122376=CARTESIAN_POINT('Ctrl Pts',(4.65320965586474,30.1199565405167,123.337771678674));
#122377=CARTESIAN_POINT('Ctrl Pts',(4.65759424598209,30.1883074183726,123.344474954379));
#122378=CARTESIAN_POINT('Ctrl Pts',(4.65926499660684,30.2139440209308,123.347592471049));
#122379=CARTESIAN_POINT('Ctrl Pts',(4.66157056615668,30.2485819808267,123.352624118736));
#122380=CARTESIAN_POINT('Ctrl Pts',(4.66217909830849,30.257656544573,123.354019018695));
#122381=CARTESIAN_POINT('Ctrl Pts',(4.66320642732542,30.2728528374561,123.356483664653));
#122382=CARTESIAN_POINT('Ctrl Pts',(4.6636229909301,30.278981123993,123.357512817004));
#122383=CARTESIAN_POINT('Ctrl Pts',(4.6644823574858,30.2915514491688,123.359696191749));
#122384=CARTESIAN_POINT('Ctrl Pts',(4.66492534256169,30.2979926420563,123.360854121065));
#122385=CARTESIAN_POINT('Ctrl Pts',(4.66610047765069,30.314982676704,123.36401186097));
#122386=CARTESIAN_POINT('Ctrl Pts',(4.66683604316334,30.3255190936232,123.366075710992));
#122387=CARTESIAN_POINT('Ctrl Pts',(4.67013139659234,30.37231933019,123.375713466757));
#122388=CARTESIAN_POINT('Ctrl Pts',(4.67274313869128,30.4083418970573,123.384393347198));
#122389=CARTESIAN_POINT('Ctrl Pts',(4.68206764426872,30.5341780830882,123.419191478542));
#122390=CARTESIAN_POINT('Ctrl Pts',(4.68893548139201,30.6220531464908,123.451661775286));
#122391=CARTESIAN_POINT('Ctrl Pts',(4.70025454787673,30.7636319255206,123.517984655344));
#122392=CARTESIAN_POINT('Ctrl Pts',(4.70475321673696,30.8189768571155,123.547835589487));
#122393=CARTESIAN_POINT('Ctrl Pts',(4.71196768202377,30.9066809251967,123.601752936437));
#122394=CARTESIAN_POINT('Ctrl Pts',(4.71473828244273,30.9400863584744,123.623990093825));
#122395=CARTESIAN_POINT('Ctrl Pts',(4.71851538498551,30.9852148999651,123.656442491769));
#122396=CARTESIAN_POINT('Ctrl Pts',(4.71955955672165,30.9976448768381,123.665646259504));
#122397=CARTESIAN_POINT('Ctrl Pts',(4.72133349273079,31.018676842668,123.681677571086));
#122398=CARTESIAN_POINT('Ctrl Pts',(4.72206653833957,31.0273425919794,123.688419371514));
#122399=CARTESIAN_POINT('Ctrl Pts',(4.72354637324233,31.0447812465562,123.702265221575));
#122400=CARTESIAN_POINT('Ctrl Pts',(4.72429293120188,31.0535498676956,123.709373758527));
#122401=CARTESIAN_POINT('Ctrl Pts',(4.72615771856068,31.0753734365306,123.727436303128));
#122402=CARTESIAN_POINT('Ctrl Pts',(4.72727133702211,31.0883340213392,123.738502681865));
#122403=CARTESIAN_POINT('Ctrl Pts',(4.73154812285012,31.1377885901312,123.782058986931));
#122404=CARTESIAN_POINT('Ctrl Pts',(4.73465303227406,31.1730181807384,123.815950923078));
#122405=CARTESIAN_POINT('Ctrl Pts',(4.74606657253298,31.2987288526957,123.94801521169));
#122406=CARTESIAN_POINT('Ctrl Pts',(4.75399665507499,31.3787918609511,124.055384382602));
#122407=CARTESIAN_POINT('Ctrl Pts',(4.76430157832991,31.4609278659618,124.198596883284));
#122408=CARTESIAN_POINT('Ctrl Pts',(4.76629909704706,31.4758837534199,124.226485880613));
#122409=CARTESIAN_POINT('Ctrl Pts',(4.76967926044928,31.4993984699941,124.273502681005));
#122410=CARTESIAN_POINT('Ctrl Pts',(4.77104093140285,31.5084071619223,124.292397101091));
#122411=CARTESIAN_POINT('Ctrl Pts',(4.77298248210799,31.5205618972558,124.319177384393));
#122412=CARTESIAN_POINT('Ctrl Pts',(4.7735455967691,31.5240076767844,124.326926073336));
#122413=CARTESIAN_POINT('Ctrl Pts',(4.77451929883274,31.5298266163881,124.340285190678));
#122414=CARTESIAN_POINT('Ctrl Pts',(4.77492816469663,31.5322284201851,124.345882905679));
#122415=CARTESIAN_POINT('Ctrl Pts',(4.77579856550045,31.537252493166,124.357771674774));
#122416=CARTESIAN_POINT('Ctrl Pts',(4.77626051349565,31.5398668388154,124.364065597711));
#122417=CARTESIAN_POINT('Ctrl Pts',(4.7775406683905,31.5469708172924,124.381468785417));
#122418=CARTESIAN_POINT('Ctrl Pts',(4.77836340090532,31.5513792266664,124.392610464904));
#122419=CARTESIAN_POINT('Ctrl Pts',(4.7829834856537,31.5752859376067,124.454990159955));
#122420=CARTESIAN_POINT('Ctrl Pts',(4.78689460982024,31.5923642217666,124.507114158395));
#122421=CARTESIAN_POINT('Ctrl Pts',(4.80156358365905,31.6460146750772,124.703031503824));
#122422=CARTESIAN_POINT('Ctrl Pts',(4.81248206114835,31.6659177012127,124.850709225393));
#122423=CARTESIAN_POINT('Ctrl Pts',(4.82498053605921,31.6660171786085,125.030605074771));
#122424=CARTESIAN_POINT('Ctrl Pts',(4.82714466607129,31.6651397379159,125.062127259757));
#122425=CARTESIAN_POINT('Ctrl Pts',(4.83022912265091,31.6625822283161,125.107573197646));
#122426=CARTESIAN_POINT('Ctrl Pts',(4.83117147356669,31.6616204221105,125.121528812696));
#122427=CARTESIAN_POINT('Ctrl Pts',(4.83283001099022,31.6596067401981,125.146210726491));
#122428=CARTESIAN_POINT('Ctrl Pts',(4.83354838862347,31.6586263492754,125.156941873076));
#122429=CARTESIAN_POINT('Ctrl Pts',(4.83504072795697,31.6563633201379,125.179314526542));
#122430=CARTESIAN_POINT('Ctrl Pts',(4.83581405944858,31.6550619000457,125.190953571702));
#122431=CARTESIAN_POINT('Ctrl Pts',(4.83783592342047,31.651320493612,125.22149452715));
#122432=CARTESIAN_POINT('Ctrl Pts',(4.83907808604678,31.6486786702876,125.240370316004));
#122433=CARTESIAN_POINT('Ctrl Pts',(4.84549041615057,31.6332546043597,125.33830187556));
#122434=CARTESIAN_POINT('Ctrl Pts',(4.85048819649043,31.6151078641715,125.4164104943));
#122435=CARTESIAN_POINT('Ctrl Pts',(4.85720161207947,31.5828077818136,125.520692724916));
#122436=CARTESIAN_POINT('Ctrl Pts',(4.85897940275955,31.5734809202704,125.548232308875));
#122437=CARTESIAN_POINT('Ctrl Pts',(4.86075489241547,31.5634400172546,125.575509611081));
#122438=CARTESIAN_POINT('',(4.62852042921073,31.6642502403512,125.001193954075));
#122439=CARTESIAN_POINT('Ctrl Pts',(4.66781556978768,31.5660436956742,125.576468401513));
#122440=CARTESIAN_POINT('Ctrl Pts',(4.66777083826495,31.5662737940932,125.575843539819));
#122441=CARTESIAN_POINT('Ctrl Pts',(4.65467245807264,31.633531411034,125.392825945703));
#122442=CARTESIAN_POINT('Ctrl Pts',(4.64157407788033,31.6655315577241,125.196877806597));
#122443=CARTESIAN_POINT('Ctrl Pts',(4.62852042921073,31.6642502403512,125.001193954075));
#122444=CARTESIAN_POINT('Ctrl Pts',(4.62751359642243,31.665999527619,125.001254580872));
#122445=CARTESIAN_POINT('Ctrl Pts',(4.6239375376834,31.6660375432059,124.950772422952));
#122446=CARTESIAN_POINT('Ctrl Pts',(4.620419739526,31.6637810501156,124.900309733779));
#122447=CARTESIAN_POINT('Ctrl Pts',(4.61604551457903,31.6580148301263,124.836516989429));
#122448=CARTESIAN_POINT('Ctrl Pts',(4.61512459863438,31.6566292630902,124.823027190808));
#122449=CARTESIAN_POINT('Ctrl Pts',(4.61350374798853,31.6538856469017,124.799183494231));
#122450=CARTESIAN_POINT('Ctrl Pts',(4.61280175823768,31.6525946846149,124.788822778187));
#122451=CARTESIAN_POINT('Ctrl Pts',(4.61141209549366,31.649834377863,124.768247992353));
#122452=CARTESIAN_POINT('Ctrl Pts',(4.61072438195141,31.6483673655148,124.75803408511));
#122453=CARTESIAN_POINT('Ctrl Pts',(4.60926074568572,31.6450289347522,124.736231970565));
#122454=CARTESIAN_POINT('Ctrl Pts',(4.60848573929539,31.6431297425108,124.724648532455));
#122455=CARTESIAN_POINT('Ctrl Pts',(4.6064534220572,31.6378027646385,124.69417897145));
#122456=CARTESIAN_POINT('Ctrl Pts',(4.60520260852067,31.634170687524,124.675329996917));
#122457=CARTESIAN_POINT('Ctrl Pts',(4.59880830461285,31.6137859097119,124.578572727055));
#122458=CARTESIAN_POINT('Ctrl Pts',(4.59383502211434,31.5917841448493,124.501872042224));
#122459=CARTESIAN_POINT('Ctrl Pts',(4.58254820986431,31.5286644162865,124.329536060907));
#122460=CARTESIAN_POINT('Ctrl Pts',(4.57631401501912,31.4839215685967,124.235597580406));
#122461=CARTESIAN_POINT('Ctrl Pts',(4.56803212861921,31.4162381294626,124.122147074781));
#122462=CARTESIAN_POINT('Ctrl Pts',(4.56623883557412,31.4011295787923,124.098228454284));
#122463=CARTESIAN_POINT('Ctrl Pts',(4.56317070923784,31.3746972486314,124.058651902695));
#122464=CARTESIAN_POINT('Ctrl Pts',(4.56191221176865,31.3636963750407,124.042784828558));
#122465=CARTESIAN_POINT('Ctrl Pts',(4.56009365910278,31.3476247189508,124.020443402823));
#122466=CARTESIAN_POINT('Ctrl Pts',(4.55954766011369,31.3427774369491,124.013809218244));
#122467=CARTESIAN_POINT('Ctrl Pts',(4.55859360586352,31.3342742505681,124.002350329422));
#122468=CARTESIAN_POINT('Ctrl Pts',(4.55818708042727,31.3306408025923,123.997509254872));
#122469=CARTESIAN_POINT('Ctrl Pts',(4.55730981695369,31.322779588904,123.987153297438));
#122470=CARTESIAN_POINT('Ctrl Pts',(4.55683855348448,31.3185437440771,123.981645113792));
#122471=CARTESIAN_POINT('Ctrl Pts',(4.55552855219161,31.3067304602129,123.966480689454));
#122472=CARTESIAN_POINT('Ctrl Pts',(4.55468506958303,31.2990807494605,123.956881672482));
#122473=CARTESIAN_POINT('Ctrl Pts',(4.54879413520227,31.2453107467731,123.890918802521));
#122474=CARTESIAN_POINT('Ctrl Pts',(4.54354650317086,31.1956484151725,123.83755323724));
#122475=CARTESIAN_POINT('Ctrl Pts',(4.53721259282661,31.1321971526107,123.777751100028));
#122476=CARTESIAN_POINT('Ctrl Pts',(4.53616650612087,31.1216057700827,123.768024651911));
#122477=CARTESIAN_POINT('Ctrl Pts',(4.52975899118879,31.0559976953666,123.709321774576));
#122478=CARTESIAN_POINT('Ctrl Pts',(4.52439743288553,30.9979052861488,123.663898298047));
#122479=CARTESIAN_POINT('Ctrl Pts',(4.51609773864597,30.901750659307,123.598494185376));
#122480=CARTESIAN_POINT('Ctrl Pts',(4.51309225307635,30.8655977837028,123.575881401399));
#122481=CARTESIAN_POINT('Ctrl Pts',(4.50800505152788,30.8020142829812,123.539428454368));
#122482=CARTESIAN_POINT('Ctrl Pts',(4.50590169074892,30.774996552601,123.524914677643));
#122483=CARTESIAN_POINT('Ctrl Pts',(4.50287679986803,30.7350909498831,123.504876936965));
#122484=CARTESIAN_POINT('Ctrl Pts',(4.5019347243888,30.7225110323898,123.498757345723));
#122485=CARTESIAN_POINT('Ctrl Pts',(4.50027907880937,30.7001388763902,123.488220617423));
#122486=CARTESIAN_POINT('Ctrl Pts',(4.49956329541892,30.6903783494703,123.483738448787));
#122487=CARTESIAN_POINT('Ctrl Pts',(4.49806662613094,30.6697873561553,123.474522835288));
#122488=CARTESIAN_POINT('Ctrl Pts',(4.4972864632009,30.6589484537709,123.469809609913));
#122489=CARTESIAN_POINT('Ctrl Pts',(4.49522431741981,30.6300261086534,123.457597227897));
#122490=CARTESIAN_POINT('Ctrl Pts',(4.49394919106735,30.6118587484649,123.450300631313));
#122491=CARTESIAN_POINT('Ctrl Pts',(4.48734481868632,30.5163742815439,123.413892008877));
#122492=CARTESIAN_POINT('Ctrl Pts',(4.48219918854202,30.4370949166804,123.39023868696));
#122493=CARTESIAN_POINT('Ctrl Pts',(4.47097106952106,30.258514571176,123.351132824828));
#122494=CARTESIAN_POINT('Ctrl Pts',(4.4649470365792,30.1589230178527,123.33857474555));
#122495=CARTESIAN_POINT('Ctrl Pts',(4.45689427352911,30.0305533785609,123.334040178307));
#122496=CARTESIAN_POINT('Ctrl Pts',(4.4551015863614,30.0022738875131,123.333761636019));
#122497=CARTESIAN_POINT('Ctrl Pts',(4.45203439201522,29.9547028075906,123.334504055862));
#122498=CARTESIAN_POINT('Ctrl Pts',(4.45077620774895,29.9354106359493,123.335140633047));
#122499=CARTESIAN_POINT('Ctrl Pts',(4.44895802935054,29.9079296833214,123.336525758087));
#122500=CARTESIAN_POINT('Ctrl Pts',(4.44841208355267,29.8997278445778,123.337000004639));
#122501=CARTESIAN_POINT('Ctrl Pts',(4.44745808927257,29.8854898336433,123.337928984224));
#122502=CARTESIAN_POINT('Ctrl Pts',(4.44705157001777,29.8794520882996,123.338355982972));
#122503=CARTESIAN_POINT('Ctrl Pts',(4.44617428064305,29.8664875990031,123.339343886004));
#122504=CARTESIAN_POINT('Ctrl Pts',(4.44570298471046,29.8595621020924,123.339915218249));
#122505=CARTESIAN_POINT('Ctrl Pts',(4.44439280730621,29.8404121811999,123.341615714017));
#122506=CARTESIAN_POINT('Ctrl Pts',(4.44354917907181,29.8281966399155,123.342836672123));
#122507=CARTESIAN_POINT('Ctrl Pts',(4.43762089560038,29.7430796205433,123.352295415229));
#122508=CARTESIAN_POINT('Ctrl Pts',(4.4323331117368,29.6707856942883,123.365205200804));
#122509=CARTESIAN_POINT('Ctrl Pts',(4.42598595763153,29.5859824652277,123.386202646103));
#122510=CARTESIAN_POINT('Ctrl Pts',(4.42496634626789,29.5724214434115,123.389742569395));
#122511=CARTESIAN_POINT('Ctrl Pts',(4.41858107174438,29.4878220241583,123.412970171694));
#122512=CARTESIAN_POINT('Ctrl Pts',(4.41321560691376,29.4181065104412,123.437184836468));
#122513=CARTESIAN_POINT('Ctrl Pts',(4.40492223001949,29.3110938963762,123.482511957329));
#122514=CARTESIAN_POINT('Ctrl Pts',(4.40192639044384,29.2726128410122,123.500576776877));
#122515=CARTESIAN_POINT('Ctrl Pts',(4.39685351405384,29.2076862771862,123.534144996522));
#122516=CARTESIAN_POINT('Ctrl Pts',(4.39475499754981,29.1809013668893,123.548941913927));
#122517=CARTESIAN_POINT('Ctrl Pts',(4.39173567369348,29.142494529767,123.571561793016));
#122518=CARTESIAN_POINT('Ctrl Pts',(4.39079442763599,29.1305409147393,123.578806043363));
#122519=CARTESIAN_POINT('Ctrl Pts',(4.38913971748014,29.1095666750761,123.591880754784));
#122520=CARTESIAN_POINT('Ctrl Pts',(4.38842404854045,29.1005087538223,123.597649536594));
#122521=CARTESIAN_POINT('Ctrl Pts',(4.38692710910026,29.0815952054365,123.609953793155));
#122522=CARTESIAN_POINT('Ctrl Pts',(4.38614656647374,29.0717520764694,123.616507452699));
#122523=CARTESIAN_POINT('Ctrl Pts',(4.38408222494615,29.0457781071075,123.63420320327));
#122524=CARTESIAN_POINT('Ctrl Pts',(4.38280530928595,29.0297724322667,123.64552636413));
#122525=CARTESIAN_POINT('Ctrl Pts',(4.37620255613942,28.9474190767965,123.705996018596));
#122526=CARTESIAN_POINT('Ctrl Pts',(4.37106002826708,28.8845886462763,123.75974482309));
#122527=CARTESIAN_POINT('Ctrl Pts',(4.35983516673441,28.7549170786552,123.888532289982));
#122528=CARTESIAN_POINT('Ctrl Pts',(4.35381136163362,28.6903545612229,123.965389719219));
#122529=CARTESIAN_POINT('Ctrl Pts',(4.34575887258919,28.6169245027203,124.070775712212));
#122530=CARTESIAN_POINT('Ctrl Pts',(4.34396621592166,28.6013530076224,124.094383072906));
#122531=CARTESIAN_POINT('Ctrl Pts',(4.34089906849349,28.5761763226775,124.134751653046));
#122532=CARTESIAN_POINT('Ctrl Pts',(4.33964089999516,28.5662478922055,124.151304894849));
#122533=CARTESIAN_POINT('Ctrl Pts',(4.33782274043886,28.5525070632302,124.17514383433));
#122534=CARTESIAN_POINT('Ctrl Pts',(4.33727679731929,28.5484571370885,124.18229173529));
#122535=CARTESIAN_POINT('Ctrl Pts',(4.33632280605877,28.5415154515645,124.194757513792));
#122536=CARTESIAN_POINT('Ctrl Pts',(4.33591628711518,28.5385995386652,124.200061671198));
#122537=CARTESIAN_POINT('Ctrl Pts',(4.33503899643536,28.5323980381598,124.211489523151));
#122538=CARTESIAN_POINT('Ctrl Pts',(4.33456769886762,28.5291218881997,124.217617825919));
#122539=CARTESIAN_POINT('Ctrl Pts',(4.33325751259384,28.5201642622918,124.234628911002));
#122540=CARTESIAN_POINT('Ctrl Pts',(4.33241387702492,28.5145647264256,124.245554017583));
#122541=CARTESIAN_POINT('Ctrl Pts',(4.32648362199371,28.4763343381828,124.322220099976));
#122542=CARTESIAN_POINT('Ctrl Pts',(4.32119371768404,28.4479615462381,124.389986153815));
#122543=CARTESIAN_POINT('Ctrl Pts',(4.31484601842944,28.4196101608446,124.47262937442));
#122544=CARTESIAN_POINT('Ctrl Pts',(4.31382795901488,28.4152362960595,124.485922360479));
#122545=CARTESIAN_POINT('Ctrl Pts',(4.30744409686147,28.3888740511055,124.569577633223));
#122546=CARTESIAN_POINT('Ctrl Pts',(4.30207850537624,28.3714072476193,124.641283959141));
#122547=CARTESIAN_POINT('Ctrl Pts',(4.29378539742429,28.3514511564899,124.755770895924));
#122548=CARTESIAN_POINT('Ctrl Pts',(4.29078993197952,28.3457586356449,124.797893209285));
#122549=CARTESIAN_POINT('Ctrl Pts',(4.28571761137024,28.3387481885042,124.870639335085));
#122550=CARTESIAN_POINT('Ctrl Pts',(4.28361928290735,28.3366528773597,124.901165159404));
#122551=CARTESIAN_POINT('Ctrl Pts',(4.28060017518036,28.3348265654864,124.945697489825));
#122552=CARTESIAN_POINT('Ctrl Pts',(4.27965896134667,28.3344296038693,124.95966879837));
#122553=CARTESIAN_POINT('Ctrl Pts',(4.27800428752195,28.3340386086976,124.984380899615));
#122554=CARTESIAN_POINT('Ctrl Pts',(4.27728862301793,28.3339725379405,124.995119574565));
#122555=CARTESIAN_POINT('Ctrl Pts',(4.27579167302631,28.3340518817492,125.017683230656));
#122556=CARTESIAN_POINT('Ctrl Pts',(4.27501111560342,28.334219358815,125.029507574273));
#122557=CARTESIAN_POINT('Ctrl Pts',(4.27294668851087,28.3349990703969,125.060928303955));
#122558=CARTESIAN_POINT('Ctrl Pts',(4.27166970312514,28.3358313485668,125.080517737309));
#122559=CARTESIAN_POINT('Ctrl Pts',(4.26506454224581,28.34197166826,125.182540285609));
#122560=CARTESIAN_POINT('Ctrl Pts',(4.25991985433236,28.3530592852464,125.264514039844));
#122561=CARTESIAN_POINT('Ctrl Pts',(4.24869484790847,28.3909433744583,125.443308460205));
#122562=CARTESIAN_POINT('Ctrl Pts',(4.24267286268373,28.4204927891004,125.539203341651));
#122563=CARTESIAN_POINT('Ctrl Pts',(4.23462256229896,28.4691942727592,125.658019154722));
#122564=CARTESIAN_POINT('Ctrl Pts',(4.23283014930831,28.4805810417531,125.683901478033));
#122565=CARTESIAN_POINT('Ctrl Pts',(4.22976337672776,28.5008391903916,125.726942471238));
#122566=CARTESIAN_POINT('Ctrl Pts',(4.22850533420944,28.5093606480927,125.744259856653));
#122567=CARTESIAN_POINT('Ctrl Pts',(4.22668732519725,28.5219352283501,125.768731436477));
#122568=CARTESIAN_POINT('Ctrl Pts',(4.22614140347588,28.5257438126068,125.776010423612));
#122569=CARTESIAN_POINT('Ctrl Pts',(4.22518743633911,28.5324517720066,125.788603092583));
#122570=CARTESIAN_POINT('Ctrl Pts',(4.22478091988075,28.5353265241769,125.793929623452));
#122571=CARTESIAN_POINT('Ctrl Pts',(4.22390361877397,28.541564168575,125.805337953106));
#122572=CARTESIAN_POINT('Ctrl Pts',(4.22343230814111,28.544936053455,125.811414320898));
#122573=CARTESIAN_POINT('Ctrl Pts',(4.22212205098766,28.5543700339596,125.828167094421));
#122574=CARTESIAN_POINT('Ctrl Pts',(4.22127835680807,28.5605121433436,125.838797605755));
#122575=CARTESIAN_POINT('Ctrl Pts',(4.21533221368887,28.6043050045739,125.912694757357));
#122576=CARTESIAN_POINT('Ctrl Pts',(4.21002521897172,28.6459921360164,125.973466251084));
#122577=CARTESIAN_POINT('Ctrl Pts',(4.19736356040869,28.7538672361296,126.110334323629));
#122578=CARTESIAN_POINT('Ctrl Pts',(4.19000833253669,28.8232231628061,126.183591601516));
#122579=CARTESIAN_POINT('Ctrl Pts',(4.17914469474326,28.9383328515318,126.284989557615));
#122580=CARTESIAN_POINT('Ctrl Pts',(4.17547523752923,28.979527497469,126.317942415896));
#122581=CARTESIAN_POINT('Ctrl Pts',(4.17072495952773,29.035969628908,126.358856077292));
#122582=CARTESIAN_POINT('Ctrl Pts',(4.1695758183336,29.0498714072905,126.368612468738));
#122583=CARTESIAN_POINT('Ctrl Pts',(4.16767733256486,29.0732457618727,126.384488954336));
#122584=CARTESIAN_POINT('Ctrl Pts',(4.16692351974461,29.0826353721918,126.390728310275));
#122585=CARTESIAN_POINT('Ctrl Pts',(4.16545069464834,29.1011913482187,126.402788969361));
#122586=CARTESIAN_POINT('Ctrl Pts',(4.16473146085928,29.1103527058597,126.408616905545));
#122587=CARTESIAN_POINT('Ctrl Pts',(4.16315787876189,29.1306118786374,126.421228146816));
#122588=CARTESIAN_POINT('Ctrl Pts',(4.16230500461638,29.1417335416142,126.427971937081));
#122589=CARTESIAN_POINT('Ctrl Pts',(4.15936955957198,29.1804875647951,126.450854682549));
#122590=CARTESIAN_POINT('Ctrl Pts',(4.1573107349061,29.2085061529089,126.466327945709));
#122591=CARTESIAN_POINT('Ctrl Pts',(4.14726467295489,29.3489411795435,126.538684028992));
#122592=CARTESIAN_POINT('Ctrl Pts',(4.13969282258815,29.4671084462327,126.58349440859));
#122593=CARTESIAN_POINT('Ctrl Pts',(4.12880290138125,29.6390212026807,126.627234737882));
#122594=CARTESIAN_POINT('Ctrl Pts',(4.12562065060112,29.6893966584587,126.637596840689));
#122595=CARTESIAN_POINT('Ctrl Pts',(4.1205050544084,29.7688813713826,126.650147046079));
#122596=CARTESIAN_POINT('Ctrl Pts',(4.11863048822673,29.7977078628706,126.653928276468));
#122597=CARTESIAN_POINT('Ctrl Pts',(4.1160877883894,29.836145151061,126.657950355198));
#122598=CARTESIAN_POINT('Ctrl Pts',(4.11545338462258,29.8456820735412,126.658865202054));
#122599=CARTESIAN_POINT('Ctrl Pts',(4.11439484146624,29.8614955879011,126.660244600571));
#122600=CARTESIAN_POINT('Ctrl Pts',(4.11397324615907,29.8677680493433,126.660755946739));
#122601=CARTESIAN_POINT('Ctrl Pts',(4.1131168247805,29.8804540146102,126.661717813797));
#122602=CARTESIAN_POINT('Ctrl Pts',(4.11268192929386,29.886867491127,126.66216676877));
#122603=CARTESIAN_POINT('Ctrl Pts',(4.11155095500766,29.9034767576726,126.663232875771));
#122604=CARTESIAN_POINT('Ctrl Pts',(4.11085188987724,29.9136757323124,126.663793389524));
#122605=CARTESIAN_POINT('Ctrl Pts',(4.10794864798838,29.9557818777473,126.665719270336));
#122606=CARTESIAN_POINT('Ctrl Pts',(4.10570606803766,29.9877178581445,126.666260713563));
#122607=CARTESIAN_POINT('Ctrl Pts',(4.09571356291661,30.1282417104813,126.664603405995));
#122608=CARTESIAN_POINT('Ctrl Pts',(4.08771134013885,30.2364484263436,126.652707605576));
#122609=CARTESIAN_POINT('Ctrl Pts',(4.07574525631691,30.3986852341966,126.618603031214));
#122610=CARTESIAN_POINT('Ctrl Pts',(4.07166659013704,30.4540049130392,126.603965808263));
#122611=CARTESIAN_POINT('Ctrl Pts',(4.06503337067012,30.54435346129,126.575009662619));
#122612=CARTESIAN_POINT('Ctrl Pts',(4.06243486137301,30.579841721536,126.562293218225));
#122613=CARTESIAN_POINT('Ctrl Pts',(4.05884924057299,30.6289180251403,126.542804771297));
#122614=CARTESIAN_POINT('Ctrl Pts',(4.05782933492302,30.6428891846669,126.537035447567));
#122615=CARTESIAN_POINT('Ctrl Pts',(4.05608405283442,30.6668100182096,126.526774215611));
#122616=CARTESIAN_POINT('Ctrl Pts',(4.05535565411528,30.6767974115517,126.522373272007));
#122617=CARTESIAN_POINT('Ctrl Pts',(4.05396423560397,30.6958793388433,126.51373992092));
#122618=CARTESIAN_POINT('Ctrl Pts',(4.05330072757054,30.7049802722395,126.509522913247));
#122619=CARTESIAN_POINT('Ctrl Pts',(4.05156368060672,30.7288052574025,126.498220901817));
#122620=CARTESIAN_POINT('Ctrl Pts',(4.05049483779986,30.7434643651665,126.491000919728));
#122621=CARTESIAN_POINT('Ctrl Pts',(4.04663050152185,30.796422525431,126.463942406264));
#122622=CARTESIAN_POINT('Ctrl Pts',(4.0438792239805,30.8340554032095,126.442833420357));
#122623=CARTESIAN_POINT('Ctrl Pts',(4.03394950825957,30.9686536103306,126.360306350369));
#122624=CARTESIAN_POINT('Ctrl Pts',(4.02705426726375,31.0600178031161,126.290382153097));
#122625=CARTESIAN_POINT('Ctrl Pts',(4.01702518417021,31.1786245043795,126.178446666427));
#122626=CARTESIAN_POINT('Ctrl Pts',(4.01402524486027,31.212314042209,126.143759715701));
#122627=CARTESIAN_POINT('Ctrl Pts',(4.0091694058192,31.2630259181156,126.086785401346));
#122628=CARTESIAN_POINT('Ctrl Pts',(4.00736531167835,31.2810766905238,126.065447921962));
#122629=CARTESIAN_POINT('Ctrl Pts',(4.00490442570335,31.3044991452293,126.036304600822));
#122630=CARTESIAN_POINT('Ctrl Pts',(4.00427868555851,31.3103543137012,126.028891057287));
#122631=CARTESIAN_POINT('Ctrl Pts',(4.00323067058586,31.3199874785417,126.016478389267));
#122632=CARTESIAN_POINT('Ctrl Pts',(4.00281083489726,31.3238009989842,126.011506881978));
#122633=CARTESIAN_POINT('Ctrl Pts',(4.00195375515965,31.3314916654427,126.001362936387));
#122634=CARTESIAN_POINT('Ctrl Pts',(4.00151640593082,31.3353668986533,125.996189253052));
#122635=CARTESIAN_POINT('Ctrl Pts',(4.00037190791011,31.3453831017511,125.982653522468));
#122636=CARTESIAN_POINT('Ctrl Pts',(3.99966164302565,31.3514761307239,125.974256583269));
#122637=CARTESIAN_POINT('Ctrl Pts',(3.99664635284777,31.3768441487848,125.938600435456));
#122638=CARTESIAN_POINT('Ctrl Pts',(3.99429928234992,31.3953746043831,125.910823774527));
#122639=CARTESIAN_POINT('Ctrl Pts',(3.98424972008916,31.4701434628719,125.791105649042));
#122640=CARTESIAN_POINT('Ctrl Pts',(3.97631017450905,31.5182255724779,125.694378192039));
#122641=CARTESIAN_POINT('Ctrl Pts',(3.96806744683423,31.5589348157813,125.587639434157));
#122642=CARTESIAN_POINT('Ctrl Pts',(3.9676011994398,31.5612051496513,125.581580893384));
#122643=CARTESIAN_POINT('Ctrl Pts',(3.96713561979274,31.5634400104587,125.575509629543));
#122644=CARTESIAN_POINT('Origin',(5.,30.,125.));
#122645=CARTESIAN_POINT('',(3.26654942290125,31.5634400114153,125.575509626944));
#122646=CARTESIAN_POINT('',(3.46014891354655,31.5634400625338,125.575509488075));
#122647=CARTESIAN_POINT('',(5.,31.5634400119422,125.575509625513));
#122648=CARTESIAN_POINT('',(4.12030994055874,31.6659997586642,124.99910326656));
#122649=CARTESIAN_POINT('Ctrl Pts',(3.46014891354656,31.5634400625339,125.575509488075));
#122650=CARTESIAN_POINT('Ctrl Pts',(3.46532993227505,31.5387713160517,125.642525075727));
#122651=CARTESIAN_POINT('Ctrl Pts',(3.47055309778454,31.509808822216,125.707913585587));
#122652=CARTESIAN_POINT('Ctrl Pts',(3.4816738125574,31.4384123201443,125.844614441927));
#122653=CARTESIAN_POINT('Ctrl Pts',(3.48752710731656,31.3946875940775,125.915015733321));
#122654=CARTESIAN_POINT('Ctrl Pts',(3.49453391055907,31.3343448909579,125.997729618313));
#122655=CARTESIAN_POINT('Ctrl Pts',(3.495865483649,31.3225061918041,126.013369680307));
#122656=CARTESIAN_POINT('Ctrl Pts',(3.49798286544945,31.3030888557521,126.038101806722));
#122657=CARTESIAN_POINT('Ctrl Pts',(3.49877545673878,31.2956850527535,126.047328116527));
#122658=CARTESIAN_POINT('Ctrl Pts',(3.5002802726476,31.2813717111757,126.06478069199));
#122659=CARTESIAN_POINT('Ctrl Pts',(3.50099314913645,31.2744796800137,126.073020474495));
#122660=CARTESIAN_POINT('Ctrl Pts',(3.50262639530776,31.2584357699984,126.091829128911));
#122661=CARTESIAN_POINT('Ctrl Pts',(3.50354447539312,31.2492295085491,126.10235071037));
#122662=CARTESIAN_POINT('Ctrl Pts',(3.50645503601106,31.2194553085823,126.135526717517));
#122663=CARTESIAN_POINT('Ctrl Pts',(3.50842686414188,31.1983945853018,126.157731740102));
#122664=CARTESIAN_POINT('Ctrl Pts',(3.51308439602941,31.1466498608286,126.209361854017));
#122665=CARTESIAN_POINT('Ctrl Pts',(3.51574754502253,31.1154277634125,126.238217784413));
#122666=CARTESIAN_POINT('Ctrl Pts',(3.52295255650722,31.0271259394368,126.313773952552));
#122667=CARTESIAN_POINT('Ctrl Pts',(3.52742681479081,30.9679971312345,126.357929163602));
#122668=CARTESIAN_POINT('Ctrl Pts',(3.53278268226031,30.8945315865238,126.405546353547));
#122669=CARTESIAN_POINT('Ctrl Pts',(3.53363002501478,30.8828317117301,126.412924440375));
#122670=CARTESIAN_POINT('Ctrl Pts',(3.53899663482922,30.808354329522,126.458604554307));
#122671=CARTESIAN_POINT('Ctrl Pts',(3.54356836259951,30.7431978780145,126.492855701118));
#122672=CARTESIAN_POINT('Ctrl Pts',(3.54917288014986,30.6647788454937,126.527670079088));
#122673=CARTESIAN_POINT('Ctrl Pts',(3.54998128513186,30.6535013926619,126.532528202669));
#122674=CARTESIAN_POINT('Ctrl Pts',(3.55125855096193,30.6357577579263,126.539940385371));
#122675=CARTESIAN_POINT('Ctrl Pts',(3.55172253435364,30.6293272740659,126.5425794939));
#122676=CARTESIAN_POINT('Ctrl Pts',(3.55259527688928,30.6172645634356,126.547442122969));
#122677=CARTESIAN_POINT('Ctrl Pts',(3.55300346162404,30.6116364871698,126.549675278273));
#122678=CARTESIAN_POINT('Ctrl Pts',(3.55397000765372,30.5983403860437,126.554867304849));
#122679=CARTESIAN_POINT('Ctrl Pts',(3.55452985526582,30.5906625008217,126.557800165715));
#122680=CARTESIAN_POINT('Ctrl Pts',(3.55641549582653,30.5648706121503,126.567434277971));
#122681=CARTESIAN_POINT('Ctrl Pts',(3.55775485205199,30.546662582218,126.573877049177));
#122682=CARTESIAN_POINT('Ctrl Pts',(3.5610894029587,30.5015094841628,126.588976107234));
#122683=CARTESIAN_POINT('Ctrl Pts',(3.56309920241594,30.4744484490152,126.597264949989));
#122684=CARTESIAN_POINT('Ctrl Pts',(3.57231599801876,30.3505417418867,126.631791306795));
#122685=CARTESIAN_POINT('Ctrl Pts',(3.57969564638525,30.251657931563,126.649936707753));
#122686=CARTESIAN_POINT('Ctrl Pts',(3.59286785922977,30.0697154667537,126.66657741103));
#122687=CARTESIAN_POINT('Ctrl Pts',(3.59869313671815,29.9872364316415,126.667987192966));
#122688=CARTESIAN_POINT('Ctrl Pts',(3.60567288238736,29.8854103400715,126.662170098247));
#122689=CARTESIAN_POINT('Ctrl Pts',(3.60700365228553,29.8658611389089,126.660706791867));
#122690=CARTESIAN_POINT('Ctrl Pts',(3.60912007096686,29.8345653586577,126.657807964873));
#122691=CARTESIAN_POINT('Ctrl Pts',(3.60991249137689,29.8228008428132,126.656591784396));
#122692=CARTESIAN_POINT('Ctrl Pts',(3.61141717506324,29.8003769871737,126.654032058479));
#122693=CARTESIAN_POINT('Ctrl Pts',(3.61213008819787,29.7897157933807,126.652710488679));
#122694=CARTESIAN_POINT('Ctrl Pts',(3.61376368925664,29.7652067307976,126.649431323938));
#122695=CARTESIAN_POINT('Ctrl Pts',(3.61468208409774,29.7513691139675,126.647402280536));
#122696=CARTESIAN_POINT('Ctrl Pts',(3.61759477978564,29.7073154311185,126.640374850524));
#122697=CARTESIAN_POINT('Ctrl Pts',(3.61956838406271,29.677209916018,126.634717302033));
#122698=CARTESIAN_POINT('Ctrl Pts',(3.62423101543838,29.6056894296176,126.619223816489));
#122699=CARTESIAN_POINT('Ctrl Pts',(3.62689741741674,29.5644614683956,126.608624618168));
#122700=CARTESIAN_POINT('Ctrl Pts',(3.63410406699923,29.4530666415299,126.575388956479));
#122701=CARTESIAN_POINT('Ctrl Pts',(3.63857692575548,29.3839251354062,126.549657570839));
#122702=CARTESIAN_POINT('Ctrl Pts',(3.64394458484375,29.3039050115591,126.513672694208));
#122703=CARTESIAN_POINT('Ctrl Pts',(3.64480503283153,29.29116920407,126.507750693825));
#122704=CARTESIAN_POINT('Ctrl Pts',(3.65016777860263,29.2124822883973,126.46994485749));
#122705=CARTESIAN_POINT('Ctrl Pts',(3.65472265125325,29.1486268732331,126.433904849781));
#122706=CARTESIAN_POINT('Ctrl Pts',(3.66030845763685,29.077086115248,126.387060459703));
#122707=CARTESIAN_POINT('Ctrl Pts',(3.66111679336123,29.0668890189016,126.380221226011));
#122708=CARTESIAN_POINT('Ctrl Pts',(3.66239397329506,29.0510393125109,126.369334848572));
#122709=CARTESIAN_POINT('Ctrl Pts',(3.66285794110926,29.0453346216952,126.365363806831));
#122710=CARTESIAN_POINT('Ctrl Pts',(3.66373067186867,29.0347070952065,126.357866810042));
#122711=CARTESIAN_POINT('Ctrl Pts',(3.66413886060442,29.0297784180783,126.354349564606));
#122712=CARTESIAN_POINT('Ctrl Pts',(3.66510543994742,29.0182046644932,126.345994606016));
#122713=CARTESIAN_POINT('Ctrl Pts',(3.66566531718262,29.0115760959378,126.341134497));
#122714=CARTESIAN_POINT('Ctrl Pts',(3.66755116427151,28.9894911088743,126.324688983783));
#122715=CARTESIAN_POINT('Ctrl Pts',(3.66889070129161,28.9742009045673,126.31288432814));
#122716=CARTESIAN_POINT('Ctrl Pts',(3.67222580326294,28.9370202963898,126.283133380777));
#122717=CARTESIAN_POINT('Ctrl Pts',(3.67423597875879,28.9153758147292,126.26489023989));
#122718=CARTESIAN_POINT('Ctrl Pts',(3.68345612018844,28.8191331113837,126.179484622085));
#122719=CARTESIAN_POINT('Ctrl Pts',(3.69083882984096,28.7502330208457,126.106215872603));
#122720=CARTESIAN_POINT('Ctrl Pts',(3.70401035403832,28.6375898934945,125.962378044533));
#122721=CARTESIAN_POINT('Ctrl Pts',(3.7098321947585,28.5917012227628,125.89388534971));
#122722=CARTESIAN_POINT('Ctrl Pts',(3.7168086183357,28.5413858916655,125.805223603519));
#122723=CARTESIAN_POINT('Ctrl Pts',(3.71813928732583,28.5320132527416,125.78800706564));
#122724=CARTESIAN_POINT('Ctrl Pts',(3.72025558500587,28.5174758573163,125.760143425944));
#122725=CARTESIAN_POINT('Ctrl Pts',(3.72104798394689,28.5121171345539,125.749600195332));
#122726=CARTESIAN_POINT('Ctrl Pts',(3.72255265103414,28.5021059162805,125.729372821938));
#122727=CARTESIAN_POINT('Ctrl Pts',(3.7232655687861,28.4974339597639,125.719699036662));
#122728=CARTESIAN_POINT('Ctrl Pts',(3.72489921449837,28.4868958394483,125.69732875195));
#122729=CARTESIAN_POINT('Ctrl Pts',(3.72581764893689,28.4810952757181,125.684602108737));
#122730=CARTESIAN_POINT('Ctrl Pts',(3.72873061330856,28.4631046304957,125.643775386516));
#122731=CARTESIAN_POINT('Ctrl Pts',(3.73070444111024,28.4515284653459,125.61541061114));
#122732=CARTESIAN_POINT('Ctrl Pts',(3.73536771438811,28.4257520729958,125.546910081464));
#122733=CARTESIAN_POINT('Ctrl Pts',(3.73803452587861,28.4122948323951,125.506517378453));
#122734=CARTESIAN_POINT('Ctrl Pts',(3.74524136944499,28.3798023548413,125.3948995031));
#122735=CARTESIAN_POINT('Ctrl Pts',(3.74971404031728,28.3639225551281,125.322857528649));
#122736=CARTESIAN_POINT('Ctrl Pts',(3.75508289834654,28.3507534828001,125.236092806036));
#122737=CARTESIAN_POINT('Ctrl Pts',(3.75594472221589,28.3488187977033,125.222158768837));
#122738=CARTESIAN_POINT('Ctrl Pts',(3.76130698328557,28.3379101990462,125.135554180075));
#122739=CARTESIAN_POINT('Ctrl Pts',(3.76586000758779,28.3335600490799,125.062390897778));
#122740=CARTESIAN_POINT('Ctrl Pts',(3.77144376247034,28.3341147525847,124.976911105354));
#122741=CARTESIAN_POINT('Ctrl Pts',(3.7722520905171,28.3343301531606,124.964634845102));
#122742=CARTESIAN_POINT('Ctrl Pts',(3.77352926092877,28.3348799605726,124.945414582176));
#122743=CARTESIAN_POINT('Ctrl Pts',(3.77399322701611,28.3351221863597,124.938468099218));
#122744=CARTESIAN_POINT('Ctrl Pts',(3.77486595647011,28.3356567519304,124.925473370286));
#122745=CARTESIAN_POINT('Ctrl Pts',(3.77527414564945,28.3359386065939,124.919424940444));
#122746=CARTESIAN_POINT('Ctrl Pts',(3.77624072868633,28.3366807875664,124.905169843559));
#122747=CARTESIAN_POINT('Ctrl Pts',(3.77680060920601,28.3371688835396,124.896964898848));
#122748=CARTESIAN_POINT('Ctrl Pts',(3.77868647919485,28.3390073996597,124.869490554571));
#122749=CARTESIAN_POINT('Ctrl Pts',(3.78002603626177,28.3406321802209,124.850241885446));
#122750=CARTESIAN_POINT('Ctrl Pts',(3.78336119933753,28.3454619412868,124.802868146404));
#122751=CARTESIAN_POINT('Ctrl Pts',(3.7853714165309,28.3490497161394,124.774788688702));
#122752=CARTESIAN_POINT('Ctrl Pts',(3.79459192906553,28.3686051080659,124.647605052887));
#122753=CARTESIAN_POINT('Ctrl Pts',(3.80197497827345,28.392794106492,124.549976461569));
#122754=CARTESIAN_POINT('Ctrl Pts',(3.81514642615884,28.45254643723,124.377328806859));
#122755=CARTESIAN_POINT('Ctrl Pts',(3.82096788576526,28.4852000959407,124.30163271898));
#122756=CARTESIAN_POINT('Ctrl Pts',(3.82794394090392,28.5323970313496,124.211278446618));
#122757=CARTESIAN_POINT('Ctrl Pts',(3.82927459867152,28.5417779416629,124.194066598367));
#122758=CARTESIAN_POINT('Ctrl Pts',(3.83139088289436,28.55730274825,124.166741036276));
#122759=CARTESIAN_POINT('Ctrl Pts',(3.83218327944765,28.5632541818446,124.156520701303));
#122760=CARTESIAN_POINT('Ctrl Pts',(3.83368794468906,28.5748183448608,124.137139264152));
#122761=CARTESIAN_POINT('Ctrl Pts',(3.83440086295466,28.5804118183179,124.127967429931));
#122762=CARTESIAN_POINT('Ctrl Pts',(3.83603451363388,28.5934906165754,124.106980993908));
#122763=CARTESIAN_POINT('Ctrl Pts',(3.83695295247706,28.6010368469153,124.095205157524));
#122764=CARTESIAN_POINT('Ctrl Pts',(3.83986594673684,28.6255799431405,124.057947105179));
#122765=CARTESIAN_POINT('Ctrl Pts',(3.84183979940321,28.6431321746941,124.032837116693));
#122766=CARTESIAN_POINT('Ctrl Pts',(3.84650314408774,28.6867030122478,123.974028139143));
#122767=CARTESIAN_POINT('Ctrl Pts',(3.84917000113386,28.7133404892142,123.940814028766));
#122768=CARTESIAN_POINT('Ctrl Pts',(3.85637686611507,28.7894932661763,123.852978018775));
#122769=CARTESIAN_POINT('Ctrl Pts',(3.86084951592899,28.8414061106628,123.800564074202));
#122770=CARTESIAN_POINT('Ctrl Pts',(3.86621850363203,28.9071601815433,123.742440821587));
#122771=CARTESIAN_POINT('Ctrl Pts',(3.86708047701465,28.9178193495902,123.733256541473));
#122772=CARTESIAN_POINT('Ctrl Pts',(3.87244268419204,28.9846627937088,123.677121585994));
#122773=CARTESIAN_POINT('Ctrl Pts',(3.87699550642383,29.0437684540843,123.633787914116));
#122774=CARTESIAN_POINT('Ctrl Pts',(3.88257903703063,29.1158817054854,123.587894623055));
#122775=CARTESIAN_POINT('Ctrl Pts',(3.88338736423698,29.1263123411007,123.581417394997));
#122776=CARTESIAN_POINT('Ctrl Pts',(3.88466453360653,29.1427583035081,123.571454940404));
#122777=CARTESIAN_POINT('Ctrl Pts',(3.88512849950472,29.1487257185332,123.567890923554));
#122778=CARTESIAN_POINT('Ctrl Pts',(3.88600122881559,29.159933083632,123.561292162403));
#122779=CARTESIAN_POINT('Ctrl Pts',(3.88640941804338,29.1651675014516,123.558248509409));
#122780=CARTESIAN_POINT('Ctrl Pts',(3.88737600148491,29.1775463667203,123.551140592669));
#122781=CARTESIAN_POINT('Ctrl Pts',(3.88793588236415,29.1847044284616,123.547100593622));
#122782=CARTESIAN_POINT('Ctrl Pts',(3.88982175485984,29.2087839988527,123.533744096531));
#122783=CARTESIAN_POINT('Ctrl Pts',(3.89116131412128,29.225836894663,123.524669344952));
#122784=CARTESIAN_POINT('Ctrl Pts',(3.89449648388623,29.2682572102138,123.503033183881));
#122785=CARTESIAN_POINT('Ctrl Pts',(3.89650670564428,29.2937939239464,123.490818116928));
#122786=CARTESIAN_POINT('Ctrl Pts',(3.90572725880528,29.4112530985108,123.438267411568));
#122787=CARTESIAN_POINT('Ctrl Pts',(3.91311034518584,29.5063948676848,123.40563929982));
#122788=CARTESIAN_POINT('Ctrl Pts',(3.92628178471754,29.6838511777597,123.36220215769));
#122789=CARTESIAN_POINT('Ctrl Pts',(3.93210320260243,29.7651563746571,123.348581220137));
#122790=CARTESIAN_POINT('Ctrl Pts',(3.93907921740668,29.8666642736799,123.339228569082));
#122791=CARTESIAN_POINT('Ctrl Pts',(3.94040987394538,29.8862125483689,123.337774794306));
#122792=CARTESIAN_POINT('Ctrl Pts',(3.94252615669465,29.9175900194915,123.335997459179));
#122793=CARTESIAN_POINT('Ctrl Pts',(3.94331855298645,29.9294044081779,123.33545437562));
#122794=CARTESIAN_POINT('Ctrl Pts',(3.94482321802553,29.9519595816701,123.334658137847));
#122795=CARTESIAN_POINT('Ctrl Pts',(3.94553613634749,29.9626989391974,123.334382985283));
#122796=CARTESIAN_POINT('Ctrl Pts',(3.94716978757093,29.9874240372146,123.333988764662));
#122797=CARTESIAN_POINT('Ctrl Pts',(3.94808822689634,30.0014102421621,123.333941891143));
#122798=CARTESIAN_POINT('Ctrl Pts',(3.951001224429,30.0460236996587,123.334354187991));
#122799=CARTESIAN_POINT('Ctrl Pts',(3.95297507981826,30.0766394380173,123.33548183026));
#122800=CARTESIAN_POINT('Ctrl Pts',(3.95763843232247,30.1496788045913,123.340191727994));
#122801=CARTESIAN_POINT('Ctrl Pts',(3.96030529435738,30.1920307180263,123.344556908635));
#122802=CARTESIAN_POINT('Ctrl Pts',(3.96751216168179,30.3071281490144,123.360897113427));
#122803=CARTESIAN_POINT('Ctrl Pts',(3.97198480918777,30.3793190101193,123.376083923441));
#122804=CARTESIAN_POINT('Ctrl Pts',(3.98144491979491,30.5281976279092,123.417876441958));
#122805=CARTESIAN_POINT('Ctrl Pts',(3.98642787460068,30.6044209573295,123.445400420983));
#122806=CARTESIAN_POINT('Ctrl Pts',(3.99271757909824,30.6930702159501,123.484919131293));
#122807=CARTESIAN_POINT('Ctrl Pts',(3.9937733753815,30.7077110244348,123.491702475682));
#122808=CARTESIAN_POINT('Ctrl Pts',(3.99535524999535,30.7292482770566,123.502063667725));
#122809=CARTESIAN_POINT('Ctrl Pts',(3.99587201757454,30.7362224240439,123.50547905953));
#122810=CARTESIAN_POINT('Ctrl Pts',(3.99679417070097,30.7485526618185,123.511624693621));
#122811=CARTESIAN_POINT('Ctrl Pts',(3.99719835641313,30.753918223606,123.514335350732));
#122812=CARTESIAN_POINT('Ctrl Pts',(3.99809445022717,30.7657273082469,123.520381693954));
#122813=CARTESIAN_POINT('Ctrl Pts',(3.9985871263319,30.7721636812068,123.523730415327));
#122814=CARTESIAN_POINT('Ctrl Pts',(4.00004337210746,30.7910293853934,123.533703005599));
#122815=CARTESIAN_POINT('Ctrl Pts',(4.0010136195239,30.8033964762513,123.54044238429));
#122816=CARTESIAN_POINT('Ctrl Pts',(4.00788436451526,30.889662299283,123.588881006176));
#122817=CARTESIAN_POINT('Ctrl Pts',(4.01404389374448,30.9603591773377,123.636012044499));
#122818=CARTESIAN_POINT('Ctrl Pts',(4.0294834768799,31.1273731969797,123.766797102822));
#122819=CARTESIAN_POINT('Ctrl Pts',(4.03870273966068,31.21828908597,123.856521539238));
#122820=CARTESIAN_POINT('Ctrl Pts',(4.04891694059792,31.3113362887856,123.97218744119));
#122821=CARTESIAN_POINT('Ctrl Pts',(4.05035712062509,31.3242532299976,123.988884293505));
#122822=CARTESIAN_POINT('Ctrl Pts',(4.0526883412668,31.3448204354563,124.016540597177));
#122823=CARTESIAN_POINT('Ctrl Pts',(4.0535867346915,31.3526619775464,124.027354127569));
#122824=CARTESIAN_POINT('Ctrl Pts',(4.0551941741983,31.3665357289057,124.046978449541));
#122825=CARTESIAN_POINT('Ctrl Pts',(4.0559049892657,31.3726148137569,124.055755033809));
#122826=CARTESIAN_POINT('Ctrl Pts',(4.05742089899463,31.3854561162687,124.074680565043));
#122827=CARTESIAN_POINT('Ctrl Pts',(4.05822497791378,31.3921921430221,124.084846593739));
#122828=CARTESIAN_POINT('Ctrl Pts',(4.06042504878695,31.4104082186223,124.113005000897));
#122829=CARTESIAN_POINT('Ctrl Pts',(4.06181242502166,31.4216553553276,124.131145818043));
#122830=CARTESIAN_POINT('Ctrl Pts',(4.06801589487877,31.4707858618911,124.213899302527));
#122831=CARTESIAN_POINT('Ctrl Pts',(4.07268825199925,31.5046367602592,124.280809140658));
#122832=CARTESIAN_POINT('Ctrl Pts',(4.08218333822555,31.5648784907217,124.422919019021));
#122833=CARTESIAN_POINT('Ctrl Pts',(4.08698583571402,31.5906121945652,124.498183682773));
#122834=CARTESIAN_POINT('Ctrl Pts',(4.09532081336199,31.6250886016307,124.628858288635));
#122835=CARTESIAN_POINT('Ctrl Pts',(4.09880030409581,31.636587655521,124.683394880651));
#122836=CARTESIAN_POINT('Ctrl Pts',(4.10354695190264,31.648118216037,124.755916109427));
#122837=CARTESIAN_POINT('Ctrl Pts',(4.10470543907957,31.6506232793526,124.773475546927));
#122838=CARTESIAN_POINT('Ctrl Pts',(4.10639860834429,31.6538336108501,124.798872604941));
#122839=CARTESIAN_POINT('Ctrl Pts',(4.10692157933837,31.6547645315561,124.806681143307));
#122840=CARTESIAN_POINT('Ctrl Pts',(4.10785101762972,31.6563115799768,124.820488675419));
#122841=CARTESIAN_POINT('Ctrl Pts',(4.10825622073179,31.6569504706871,124.826484866271));
#122842=CARTESIAN_POINT('Ctrl Pts',(4.10904749108155,31.6581290706816,124.838147053464));
#122843=CARTESIAN_POINT('Ctrl Pts',(4.10943330429272,31.6586723014105,124.843812338997));
#122844=CARTESIAN_POINT('Ctrl Pts',(4.11030145769451,31.6598247453823,124.85651577955));
#122845=CARTESIAN_POINT('Ctrl Pts',(4.11078461615754,31.6604182365978,124.863555204913));
#122846=CARTESIAN_POINT('Ctrl Pts',(4.11237846316793,31.6622201424697,124.886683957907));
#122847=CARTESIAN_POINT('Ctrl Pts',(4.11349824869852,31.6632395571304,124.902786538608));
#122848=CARTESIAN_POINT('Ctrl Pts',(4.11649927525144,31.6653269690255,124.945616789931));
#122849=CARTESIAN_POINT('Ctrl Pts',(4.11839632409284,31.6659853632973,124.972358777486));
#122850=CARTESIAN_POINT('Ctrl Pts',(4.12030994055874,31.6659997586642,124.99910326656));
#122851=CARTESIAN_POINT('Ctrl Pts',(4.12030976540797,31.6659997573448,124.999100818672));
#122852=CARTESIAN_POINT('Ctrl Pts',(4.12690058450125,31.6660494727944,125.091213415329));
#122853=CARTESIAN_POINT('Ctrl Pts',(4.13366432505074,31.6584599294103,125.183173080206));
#122854=CARTESIAN_POINT('Ctrl Pts',(4.144812852646,31.6331199009412,125.335129094415));
#122855=CARTESIAN_POINT('Ctrl Pts',(4.14924516230143,31.6195324395953,125.39561107137));
#122856=CARTESIAN_POINT('Ctrl Pts',(4.15636865642105,31.5917480049583,125.493430538165));
#122857=CARTESIAN_POINT('Ctrl Pts',(4.15911285061266,31.5795242165704,125.531261815179));
#122858=CARTESIAN_POINT('Ctrl Pts',(4.1619795480403,31.565123709874,125.570920088539));
#122859=CARTESIAN_POINT('Ctrl Pts',(4.16214545821458,31.5642843847085,125.573215786958));
#122860=CARTESIAN_POINT('Ctrl Pts',(4.16231120066723,31.5634400119558,125.575509625476));
#122861=CARTESIAN_POINT('Ctrl Pts',(3.96713561979274,31.5634400104587,125.575509629543));
#122862=CARTESIAN_POINT('Ctrl Pts',(3.96352862299315,31.5807542032736,125.52847357592));
#122863=CARTESIAN_POINT('Ctrl Pts',(3.95996288128871,31.5959393093763,125.480673796253));
#122864=CARTESIAN_POINT('Ctrl Pts',(3.95384263844318,31.6186573985309,125.396112138332));
#122865=CARTESIAN_POINT('Ctrl Pts',(3.95126252080062,31.6271474673079,125.359649976059));
#122866=CARTESIAN_POINT('Ctrl Pts',(3.94769744747633,31.6373249383762,125.308140114473));
#122867=CARTESIAN_POINT('Ctrl Pts',(3.94668020010676,31.6400463819926,125.293310713825));
#122868=CARTESIAN_POINT('Ctrl Pts',(3.94493802658564,31.6443891496727,125.267692518425));
#122869=CARTESIAN_POINT('Ctrl Pts',(3.94421010642985,31.6461064567215,125.256921199726));
#122870=CARTESIAN_POINT('Ctrl Pts',(3.94272865504895,31.6494010741873,125.234865694673));
#122871=CARTESIAN_POINT('Ctrl Pts',(3.94197546677462,31.6509686593607,125.223580622533));
#122872=CARTESIAN_POINT('Ctrl Pts',(3.94007038614763,31.6546581000016,125.194861461032));
#122873=CARTESIAN_POINT('Ctrl Pts',(3.93892354119861,31.6566203118629,125.177407997258));
#122874=CARTESIAN_POINT('Ctrl Pts',(3.93429798673835,31.6634684630543,125.106398175224));
#122875=CARTESIAN_POINT('Ctrl Pts',(3.93089119182993,31.6660362988545,125.052648178121));
#122876=CARTESIAN_POINT('Ctrl Pts',(3.92157740828373,31.6659344406967,124.90331771581));
#122877=CARTESIAN_POINT('Ctrl Pts',(3.91580905976596,31.6576502345239,124.807955195007));
#122878=CARTESIAN_POINT('Ctrl Pts',(3.9052557548619,31.6281069486617,124.638520840064));
#122879=CARTESIAN_POINT('Ctrl Pts',(3.90051311998408,31.6098104463343,124.564217107924));
#122880=CARTESIAN_POINT('Ctrl Pts',(3.89471855049518,31.5827307707288,124.479740144298));
#122881=CARTESIAN_POINT('Ctrl Pts',(3.89390955363458,31.5788503638266,124.468080347329));
#122882=CARTESIAN_POINT('Ctrl Pts',(3.89263163983194,31.5725734289611,124.449893520797));
#122883=CARTESIAN_POINT('Ctrl Pts',(3.89216761024834,31.5702643258904,124.443336483687));
#122884=CARTESIAN_POINT('Ctrl Pts',(3.89129500109225,31.5658681845837,124.431098020723));
#122885=CARTESIAN_POINT('Ctrl Pts',(3.89088699806223,31.5637911362241,124.425413269286));
#122886=CARTESIAN_POINT('Ctrl Pts',(3.88992119971945,31.5588233897662,124.412043319928));
#122887=CARTESIAN_POINT('Ctrl Pts',(3.88936192310935,31.5559068016037,124.404368036632));
#122888=CARTESIAN_POINT('Ctrl Pts',(3.88747965125037,31.5459544279629,124.378749345957));
#122889=CARTESIAN_POINT('Ctrl Pts',(3.88614315287176,31.5386643118929,124.360907264358));
#122890=CARTESIAN_POINT('Ctrl Pts',(3.88281715100822,31.5199412845325,124.317262231384));
#122891=CARTESIAN_POINT('Ctrl Pts',(3.88081312916866,31.5081592900544,124.291616103136));
#122892=CARTESIAN_POINT('Ctrl Pts',(3.8716465746977,31.4518151281689,124.176754653832));
#122893=CARTESIAN_POINT('Ctrl Pts',(3.86431273633819,31.3999489014488,124.091350700761));
#122894=CARTESIAN_POINT('Ctrl Pts',(3.85112931772382,31.2914405212585,123.944234913046));
#122895=CARTESIAN_POINT('Ctrl Pts',(3.84525171206695,31.2371868009904,123.88114740955));
#122896=CARTESIAN_POINT('Ctrl Pts',(3.83822171472868,31.1645751794945,123.80848601697));
#122897=CARTESIAN_POINT('Ctrl Pts',(3.83688971346384,31.1504623802431,123.794853830778));
#122898=CARTESIAN_POINT('Ctrl Pts',(3.83477197690267,31.127460415763,123.773407601132));
#122899=CARTESIAN_POINT('Ctrl Pts',(3.83397945161786,31.1187234616638,123.765433788375));
#122900=CARTESIAN_POINT('Ctrl Pts',(3.83247496762936,31.1018943643616,123.750400021365));
#122901=CARTESIAN_POINT('Ctrl Pts',(3.83176235527004,31.0938174725448,123.743323970636));
#122902=CARTESIAN_POINT('Ctrl Pts',(3.83013001388486,31.0750762976567,123.727222677686));
#122903=CARTESIAN_POINT('Ctrl Pts',(3.82921256912457,31.0643656824223,123.718252414961));
#122904=CARTESIAN_POINT('Ctrl Pts',(3.82630533554839,31.0298734357762,123.690095300974));
#122905=CARTESIAN_POINT('Ctrl Pts',(3.82433613581767,31.0056754681708,123.671426835084));
#122906=CARTESIAN_POINT('Ctrl Pts',(3.81968594490355,30.9466897183713,123.628455595871));
#122907=CARTESIAN_POINT('Ctrl Pts',(3.81702741162792,30.9114599692911,123.60479514842));
#122908=CARTESIAN_POINT('Ctrl Pts',(3.80982481102461,30.8126199804357,123.543757294105));
#122909=CARTESIAN_POINT('Ctrl Pts',(3.80534865352413,30.7473717042517,123.509218340482));
#122910=CARTESIAN_POINT('Ctrl Pts',(3.8000161615178,30.6677968601917,123.473637166322));
#122911=CARTESIAN_POINT('Ctrl Pts',(3.79919397425709,30.6554784237595,123.468306761371));
#122912=CARTESIAN_POINT('Ctrl Pts',(3.79382154719974,30.5747769618755,123.43453765363));
#122913=CARTESIAN_POINT('Ctrl Pts',(3.78921906755502,30.5046349627858,123.410540443666));
#122914=CARTESIAN_POINT('Ctrl Pts',(3.78358053704357,30.4212829808363,123.388098196648));
#122915=CARTESIAN_POINT('Ctrl Pts',(3.78277215993997,30.4093917381067,123.385037103647));
#122916=CARTESIAN_POINT('Ctrl Pts',(3.78149501476816,30.3907191849761,123.380449810446));
#122917=CARTESIAN_POINT('Ctrl Pts',(3.78103112455801,30.3839600340956,123.378834065915));
#122918=CARTESIAN_POINT('Ctrl Pts',(3.78015862096159,30.371295264862,123.375890254456));
#122919=CARTESIAN_POINT('Ctrl Pts',(3.77975058233277,30.3653922631154,123.374552022162));
#122920=CARTESIAN_POINT('Ctrl Pts',(3.77878448681502,30.3514610590279,123.371473486735));
#122921=CARTESIAN_POINT('Ctrl Pts',(3.77822494585976,30.3434271335287,123.369760362));
#122922=CARTESIAN_POINT('Ctrl Pts',(3.7763408325478,30.3164798522999,123.364222249514));
#122923=CARTESIAN_POINT('Ctrl Pts',(3.77500272243682,30.2975135489668,123.360666612683));
#122924=CARTESIAN_POINT('Ctrl Pts',(3.77167181072081,30.250622706819,123.35271641315));
#122925=CARTESIAN_POINT('Ctrl Pts',(3.76966443947044,30.2226403846133,123.348701712137));
#122926=CARTESIAN_POINT('Ctrl Pts',(3.76046823954153,30.0951743223672,123.333712449522));
#122927=CARTESIAN_POINT('Ctrl Pts',(3.7531072933845,29.9949271986037,123.331004174576));
#122928=CARTESIAN_POINT('Ctrl Pts',(3.73993008640346,29.8125413417562,123.34251734815));
#122929=CARTESIAN_POINT('Ctrl Pts',(3.73408305538641,29.730532733163,123.353858878976));
#122930=CARTESIAN_POINT('Ctrl Pts',(3.72708254649382,29.6305250923967,123.37536812323));
#122931=CARTESIAN_POINT('Ctrl Pts',(3.72575139149734,29.6114298326118,123.379829106431));
#122932=CARTESIAN_POINT('Ctrl Pts',(3.72363466969997,29.5809509642906,123.387519381053));
#122933=CARTESIAN_POINT('Ctrl Pts',(3.72284232445438,29.5695157642461,123.3905345061));
#122934=CARTESIAN_POINT('Ctrl Pts',(3.72133797998545,29.547759697168,123.396519404718));
#122935=CARTESIAN_POINT('Ctrl Pts',(3.7206253292228,29.5374335959599,123.399467700415));
#122936=CARTESIAN_POINT('Ctrl Pts',(3.7189926149693,29.5137361790457,123.406482256444));
#122937=CARTESIAN_POINT('Ctrl Pts',(3.71807483940607,29.5003859600017,123.410617373523));
#122938=CARTESIAN_POINT('Ctrl Pts',(3.71516536342022,29.4579897593647,123.424336225931));
#122939=CARTESIAN_POINT('Ctrl Pts',(3.71319429839723,29.4291539840933,123.43455231832));
#122940=CARTESIAN_POINT('Ctrl Pts',(3.70853875481299,29.3609816719742,123.460839233088));
#122941=CARTESIAN_POINT('Ctrl Pts',(3.70587680782465,29.3219461760718,123.477632212263));
#122942=CARTESIAN_POINT('Ctrl Pts',(3.69867222710805,29.2170331484494,123.527602570088));
#122943=CARTESIAN_POINT('Ctrl Pts',(3.69419728862964,29.152649516931,123.563689167423));
#122944=CARTESIAN_POINT('Ctrl Pts',(3.68884537306649,29.0793398752456,123.611428726712));
#122945=CARTESIAN_POINT('Ctrl Pts',(3.68800262886321,29.067905529692,123.619078156074));
#122946=CARTESIAN_POINT('Ctrl Pts',(3.682634262437,28.9958678630912,123.668572816012));
#122947=CARTESIAN_POINT('Ctrl Pts',(3.67805621923547,28.9380079202976,123.714251280594));
#122948=CARTESIAN_POINT('Ctrl Pts',(3.6724448316176,28.8742549761992,123.771828644879));
#122949=CARTESIAN_POINT('Ctrl Pts',(3.67163655268575,28.865234985076,123.780157766226));
#122950=CARTESIAN_POINT('Ctrl Pts',(3.6703595292693,28.8512550628881,123.793356157472));
#122951=CARTESIAN_POINT('Ctrl Pts',(3.66989566113923,28.8462319402818,123.798158266138));
#122952=CARTESIAN_POINT('Ctrl Pts',(3.66902317424784,28.8368900046065,123.807201702377));
#122953=CARTESIAN_POINT('Ctrl Pts',(3.66861512996107,28.8325640738332,123.81143532199));
#122954=CARTESIAN_POINT('Ctrl Pts',(3.66764898728223,28.8224214124804,123.821470339566));
#122955=CARTESIAN_POINT('Ctrl Pts',(3.6670894043844,28.8166244172952,123.827291292139));
#122956=CARTESIAN_POINT('Ctrl Pts',(3.66520499876969,28.7973534733861,123.846930263471));
#122957=CARTESIAN_POINT('Ctrl Pts',(3.66386663279833,28.7840771857697,123.860938932381));
#122958=CARTESIAN_POINT('Ctrl Pts',(3.66053494143929,28.751958942969,123.896030395364));
#122959=CARTESIAN_POINT('Ctrl Pts',(3.65852703825346,28.7334049725675,123.917367918429));
#122960=CARTESIAN_POINT('Ctrl Pts',(3.64932611865575,28.6516397177456,124.016379932212));
#122961=CARTESIAN_POINT('Ctrl Pts',(3.64196085559383,28.5949673266824,124.099185075933));
#122962=CARTESIAN_POINT('Ctrl Pts',(3.62878462957162,28.5057447685608,124.258663469944));
#122963=CARTESIAN_POINT('Ctrl Pts',(3.62294245721442,28.4708278105737,124.333655747558));
#122964=CARTESIAN_POINT('Ctrl Pts',(3.61594663911569,28.4346828885717,124.429278785217));
#122965=CARTESIAN_POINT('Ctrl Pts',(3.61461562229018,28.4280749353141,124.447739180896));
#122966=CARTESIAN_POINT('Ctrl Pts',(3.61249906617595,28.4180060956667,124.477514481102));
#122967=CARTESIAN_POINT('Ctrl Pts',(3.61170675032658,28.4143373549911,124.488756594655));
#122968=CARTESIAN_POINT('Ctrl Pts',(3.61020242861816,28.4075659673028,124.510280524408));
#122969=CARTESIAN_POINT('Ctrl Pts',(3.60948977156561,28.4044424475102,124.520555092666));
#122970=CARTESIAN_POINT('Ctrl Pts',(3.60785699633333,28.397482848226,124.544269701998));
#122971=CARTESIAN_POINT('Ctrl Pts',(3.60693916668006,28.3937160788647,124.557729369427));
#122972=CARTESIAN_POINT('Ctrl Pts',(3.6040293239106,28.3822464200609,124.600794436882));
#122973=CARTESIAN_POINT('Ctrl Pts',(3.60205795377475,28.3751890489907,124.630566259418));
#122974=CARTESIAN_POINT('Ctrl Pts',(3.59740153442503,28.3602976614656,124.702111901186));
#122975=CARTESIAN_POINT('Ctrl Pts',(3.59473902885037,28.3532340716015,124.744024542191));
#122976=CARTESIAN_POINT('Ctrl Pts',(3.58753414385141,28.3383179472313,124.859274957168));
#122977=CARTESIAN_POINT('Ctrl Pts',(3.58305942369869,28.3337186709136,124.932935249666));
#122978=CARTESIAN_POINT('Ctrl Pts',(3.57770486474803,28.3340684680187,125.020461058019));
#122979=CARTESIAN_POINT('Ctrl Pts',(3.57685927315372,28.33429516796,125.034262674931));
#122980=CARTESIAN_POINT('Ctrl Pts',(3.57149157056634,28.336816126696,125.121615763974));
#122981=CARTESIAN_POINT('Ctrl Pts',(3.56691701409882,28.3438097601599,125.194941369759));
#122982=CARTESIAN_POINT('Ctrl Pts',(3.56130949820639,28.3575962384021,125.279672334438));
#122983=CARTESIAN_POINT('Ctrl Pts',(3.56050123340875,28.3597017452784,125.291767620826));
#122984=CARTESIAN_POINT('Ctrl Pts',(3.55922422752216,28.3632080377829,125.310670830606));
#122985=CARTESIAN_POINT('Ctrl Pts',(3.55876036257101,28.3645181296845,125.317495417391));
#122986=CARTESIAN_POINT('Ctrl Pts',(3.55788787808429,28.367049179345,125.330248781452));
#122987=CARTESIAN_POINT('Ctrl Pts',(3.55747983298255,28.3682598016447,125.336179357965));
#122988=CARTESIAN_POINT('Ctrl Pts',(3.55651368351164,28.3711896651417,125.350143377474));
#122989=CARTESIAN_POINT('Ctrl Pts',(3.55595409457362,28.3729360399246,125.358170845382));
#122990=CARTESIAN_POINT('Ctrl Pts',(3.55406964686146,28.37898387128,125.385013267021));
#122991=CARTESIAN_POINT('Ctrl Pts',(3.55273124404052,28.3835527219579,125.403765554884));
#122992=CARTESIAN_POINT('Ctrl Pts',(3.54939944039085,28.395615265959,125.449783339423));
#122993=CARTESIAN_POINT('Ctrl Pts',(3.54739146058956,28.4034791946279,125.476945033324));
#122994=CARTESIAN_POINT('Ctrl Pts',(3.5381898609488,28.4423201843109,125.599348932699));
#122995=CARTESIAN_POINT('Ctrl Pts',(3.53082397584887,28.481155543515,125.691879701384));
#122996=CARTESIAN_POINT('Ctrl Pts',(3.5176478909884,28.5667515299219,125.853332171553));
#122997=CARTESIAN_POINT('Ctrl Pts',(3.5118064184972,28.6108136717573,125.923332018516));
#122998=CARTESIAN_POINT('Ctrl Pts',(3.50481127619276,28.6715412842545,126.005553476254));
#122999=CARTESIAN_POINT('Ctrl Pts',(3.5034802793548,28.6834665864198,126.021117124008));
#123000=CARTESIAN_POINT('Ctrl Pts',(3.50136374720814,28.7030209304076,126.045725165805));
#123001=CARTESIAN_POINT('Ctrl Pts',(3.50057143561116,28.7104760917228,126.054904702719));
#123002=CARTESIAN_POINT('Ctrl Pts',(3.4990671171947,28.7248867022551,126.072267406721));
#123003=CARTESIAN_POINT('Ctrl Pts',(3.49835445923184,28.7318247427581,126.080464177902));
#123004=CARTESIAN_POINT('Ctrl Pts',(3.4967216751761,28.7479738797309,126.099173291085));
#123005=CARTESIAN_POINT('Ctrl Pts',(3.49580383769647,28.7572390585602,126.109638045409));
#123006=CARTESIAN_POINT('Ctrl Pts',(3.4928939418534,28.7871997414039,126.142631744169));
#123007=CARTESIAN_POINT('Ctrl Pts',(3.49092252756731,28.8083851960636,126.164708597571));
#123008=CARTESIAN_POINT('Ctrl Pts',(3.48626598148828,28.8604188050897,126.216024626695));
#123009=CARTESIAN_POINT('Ctrl Pts',(3.48360339508098,28.8918014839276,126.24469177753));
#123010=CARTESIAN_POINT('Ctrl Pts',(3.47639846649747,28.9805393746336,126.319731314348));
#123011=CARTESIAN_POINT('Ctrl Pts',(3.47192377836683,29.0399298786321,126.363545539011));
#123012=CARTESIAN_POINT('Ctrl Pts',(3.46656884846885,29.1136590786099,126.410725513862));
#123013=CARTESIAN_POINT('Ctrl Pts',(3.46572285598404,29.1253829818725,126.418023896207));
#123014=CARTESIAN_POINT('Ctrl Pts',(3.46035524942957,29.2001385065439,126.463281022382));
#123015=CARTESIAN_POINT('Ctrl Pts',(3.45578118644328,29.2655284443782,126.497170181264));
#123016=CARTESIAN_POINT('Ctrl Pts',(3.45017421849734,29.3441842203121,126.531539223497));
#123017=CARTESIAN_POINT('Ctrl Pts',(3.44936595570352,29.3554879202592,126.536330331442));
#123018=CARTESIAN_POINT('Ctrl Pts',(3.44808895230225,29.3732709824101,126.543636949215));
#123019=CARTESIAN_POINT('Ctrl Pts',(3.44762508780179,29.3797151554707,126.546237691865));
#123020=CARTESIAN_POINT('Ctrl Pts',(3.44675260365591,29.3918025576823,126.55102821106));
#123021=CARTESIAN_POINT('Ctrl Pts',(3.44634455843855,29.397441692908,126.55322764662));
#123022=CARTESIAN_POINT('Ctrl Pts',(3.44537840800485,29.4107625397687,126.558339727849));
#123023=CARTESIAN_POINT('Ctrl Pts',(3.44481881821046,29.418453947817,126.561226336586));
#123024=CARTESIAN_POINT('Ctrl Pts',(3.44293436452967,29.4442856432646,126.570703683677));
#123025=CARTESIAN_POINT('Ctrl Pts',(3.44159595648408,29.4625183080825,126.577035782631));
#123026=CARTESIAN_POINT('Ctrl Pts',(3.43826413691347,29.5077223580024,126.59185996835));
#123027=CARTESIAN_POINT('Ctrl Pts',(3.43625614624933,29.5348073376272,126.599984700574));
#123028=CARTESIAN_POINT('Ctrl Pts',(3.42705445018405,29.658711437572,126.633740464172));
#123029=CARTESIAN_POINT('Ctrl Pts',(3.41968847688366,29.7575146637356,126.651298610726));
#123030=CARTESIAN_POINT('Ctrl Pts',(3.40651241203323,29.9395819718255,126.666951232189));
#123031=CARTESIAN_POINT('Ctrl Pts',(3.40067103877146,30.0222882588045,126.667897982785));
#123032=CARTESIAN_POINT('Ctrl Pts',(3.39367599228565,30.1243011709922,126.661472109407));
#123033=CARTESIAN_POINT('Ctrl Pts',(3.39234499828336,30.14384468412,126.659894308462));
#123034=CARTESIAN_POINT('Ctrl Pts',(3.39022846953704,30.1751244963244,126.656812373186));
#123035=CARTESIAN_POINT('Ctrl Pts',(3.38943615854334,30.1868800281768,126.655527618828));
#123036=CARTESIAN_POINT('Ctrl Pts',(3.38793184059409,30.2092829831432,126.652837543927));
#123037=CARTESIAN_POINT('Ctrl Pts',(3.38721918250205,30.2199323937662,126.65145422735));
#123038=CARTESIAN_POINT('Ctrl Pts',(3.38558639719452,30.2444094658033,126.648033780959));
#123039=CARTESIAN_POINT('Ctrl Pts',(3.38466855860457,30.2582264790076,126.645925403964));
#123040=CARTESIAN_POINT('Ctrl Pts',(3.38175865523192,30.3021956357366,126.63864870362));
#123041=CARTESIAN_POINT('Ctrl Pts',(3.37978723468221,30.3322336885918,126.632823548484));
#123042=CARTESIAN_POINT('Ctrl Pts',(3.3751306706239,30.403567959783,126.616939736214));
#123043=CARTESIAN_POINT('Ctrl Pts',(3.3724680727487,30.4446734995351,126.606121747278));
#123044=CARTESIAN_POINT('Ctrl Pts',(3.36526313799108,30.5558458219071,126.572267827239));
#123045=CARTESIAN_POINT('Ctrl Pts',(3.36078845441238,30.6248672562079,126.54613452732));
#123046=CARTESIAN_POINT('Ctrl Pts',(3.35133282169985,30.7654693231246,126.481940579878));
#123047=CARTESIAN_POINT('Ctrl Pts',(3.34635651373472,30.8364578959568,126.443061410053));
#123048=CARTESIAN_POINT('Ctrl Pts',(3.34005345722458,30.9181656501343,126.390251421584));
#123049=CARTESIAN_POINT('Ctrl Pts',(3.3389760302868,30.9318618972197,126.381108442841));
#123050=CARTESIAN_POINT('Ctrl Pts',(3.33737514500823,30.951773644525,126.367385270653));
#123051=CARTESIAN_POINT('Ctrl Pts',(3.33686154773424,30.9580968960103,126.362962171449));
#123052=CARTESIAN_POINT('Ctrl Pts',(3.33594285128177,30.9692874299057,126.355018067934));
#123053=CARTESIAN_POINT('Ctrl Pts',(3.3355389171035,30.9741667253314,126.351514437642));
#123054=CARTESIAN_POINT('Ctrl Pts',(3.33464065845415,30.9849259124668,126.343700151946));
#123055=CARTESIAN_POINT('Ctrl Pts',(3.33414553756842,30.9907964352877,126.339377306873));
#123056=CARTESIAN_POINT('Ctrl Pts',(3.33267439078484,31.0080686087668,126.326482999535));
#123057=CARTESIAN_POINT('Ctrl Pts',(3.33169148548803,31.0193884292462,126.317803727587));
#123058=CARTESIAN_POINT('Ctrl Pts',(3.3293902934715,31.0454147347688,126.297312530433));
#123059=CARTESIAN_POINT('Ctrl Pts',(3.32806621059145,31.0600346613704,126.285394189197));
#123060=CARTESIAN_POINT('Ctrl Pts',(3.32334838674721,31.1109818241644,126.242401120407));
#123061=CARTESIAN_POINT('Ctrl Pts',(3.31989939648284,31.1461692123785,126.210015176482));
#123062=CARTESIAN_POINT('Ctrl Pts',(3.30823788005546,31.2595782867348,126.096244548077));
#123063=CARTESIAN_POINT('Ctrl Pts',(3.2999826709812,31.3309278840731,126.008427549007));
#123064=CARTESIAN_POINT('Ctrl Pts',(3.2888487604919,31.4176463946644,125.87628570116));
#123065=CARTESIAN_POINT('Ctrl Pts',(3.28571494723918,31.4408935347018,125.837510846481));
#123066=CARTESIAN_POINT('Ctrl Pts',(3.28150575909692,31.4704942474655,125.783248841607));
#123067=CARTESIAN_POINT('Ctrl Pts',(3.28038199612462,31.4782329403291,125.768543745391));
#123068=CARTESIAN_POINT('Ctrl Pts',(3.27858896626285,31.490310851459,125.744735636403));
#123069=CARTESIAN_POINT('Ctrl Pts',(3.27791485001578,31.4947895164398,125.735705043725));
#123070=CARTESIAN_POINT('Ctrl Pts',(3.2765193161326,31.5039296161606,125.716847260663));
#123071=CARTESIAN_POINT('Ctrl Pts',(3.27579840024908,31.5085773430972,125.707013928379));
#123072=CARTESIAN_POINT('Ctrl Pts',(3.27409799123439,31.5193611164379,125.683607814098));
#123073=CARTESIAN_POINT('Ctrl Pts',(3.27312144694752,31.5254121613228,125.669996721972));
#123074=CARTESIAN_POINT('Ctrl Pts',(3.27026164857302,31.5427011961233,125.629658288214));
#123075=CARTESIAN_POINT('Ctrl Pts',(3.26839562934732,31.5534248189975,125.602717082415));
#123076=CARTESIAN_POINT('Ctrl Pts',(3.26654942290125,31.5634400114153,125.575509626944));
#123077=CARTESIAN_POINT('Origin',(5.,30.,125.));
#123078=CARTESIAN_POINT('',(2.56904933390813,31.5634400118358,125.575509625802));
#123079=CARTESIAN_POINT('',(2.75979332369797,31.5634400150579,125.575509617049));
#123080=CARTESIAN_POINT('',(5.,31.5634400119422,125.575509625513));
#123081=CARTESIAN_POINT('Ctrl Pts',(2.75979332369797,31.5634400150579,125.575509617049));
#123082=CARTESIAN_POINT('Ctrl Pts',(2.76041358651822,31.559981406667,125.584905336242));
#123083=CARTESIAN_POINT('Ctrl Pts',(2.76103576549018,31.5564377314933,125.594270881401));
#123084=CARTESIAN_POINT('Ctrl Pts',(2.76368036814329,31.5410732388471,125.633796936527));
#123085=CARTESIAN_POINT('Ctrl Pts',(2.76572347926925,31.528459758398,125.663638303974));
#123086=CARTESIAN_POINT('Ctrl Pts',(2.76917271010146,31.5061307195007,125.712445975781));
#123087=CARTESIAN_POINT('Ctrl Pts',(2.77055674212779,31.4969064936737,125.731628224946));
#123088=CARTESIAN_POINT('Ctrl Pts',(2.77252482942317,31.4834722581688,125.758247261965));
#123089=CARTESIAN_POINT('Ctrl Pts',(2.7730915014663,31.4795682324861,125.765837246845));
#123090=CARTESIAN_POINT('Ctrl Pts',(2.77406932080167,31.4727744530551,125.778799472925));
#123091=CARTESIAN_POINT('Ctrl Pts',(2.77447870635722,31.4699132169148,125.784186420574));
#123092=CARTESIAN_POINT('Ctrl Pts',(2.77534785585793,31.4638045537374,125.795536503927));
#123093=CARTESIAN_POINT('Ctrl Pts',(2.77580801108254,31.4605502817986,125.801495459022));
#123094=CARTESIAN_POINT('Ctrl Pts',(2.77707815531717,31.4515101517744,125.817811113318));
#123095=CARTESIAN_POINT('Ctrl Pts',(2.77789255871442,31.4456500826764,125.828125930106));
#123096=CARTESIAN_POINT('Ctrl Pts',(2.78241420296411,31.4127404635743,125.884639102952));
#123097=CARTESIAN_POINT('Ctrl Pts',(2.78623016575027,31.3835887736318,125.929571346781));
#123098=CARTESIAN_POINT('Ctrl Pts',(2.79713444714875,31.2953414870224,126.052220020763));
#123099=CARTESIAN_POINT('Ctrl Pts',(2.80430021625587,31.231502617139,126.12626787655));
#123100=CARTESIAN_POINT('Ctrl Pts',(2.81480762648961,31.1265367979438,126.228355150878));
#123101=CARTESIAN_POINT('Ctrl Pts',(2.81826965337511,31.0900406162061,126.260854359214));
#123102=CARTESIAN_POINT('Ctrl Pts',(2.82402596645811,31.0259569398931,126.313054091823));
#123103=CARTESIAN_POINT('Ctrl Pts',(2.82635043076461,30.9991026078242,126.333601498122));
#123104=CARTESIAN_POINT('Ctrl Pts',(2.8296278782315,30.9598467161995,126.361785978704));
#123105=CARTESIAN_POINT('Ctrl Pts',(2.83060654518557,30.9479430783254,126.370098797103));
#123106=CARTESIAN_POINT('Ctrl Pts',(2.83230410870678,30.9269825194263,126.384332487089));
#123107=CARTESIAN_POINT('Ctrl Pts',(2.83302559281953,30.9179739184319,126.390322595914));
#123108=CARTESIAN_POINT('Ctrl Pts',(2.83451334342174,30.8991931297128,126.40254842091));
#123109=CARTESIAN_POINT('Ctrl Pts',(2.83527908410116,30.8894129016869,126.408770761795));
#123110=CARTESIAN_POINT('Ctrl Pts',(2.83725690595954,30.8638623342852,126.424654299822));
#123111=CARTESIAN_POINT('Ctrl Pts',(2.83846313004437,30.847994383697,126.434156050182));
#123112=CARTESIAN_POINT('Ctrl Pts',(2.84373836423414,30.7773972657187,126.474848222531));
#123113=CARTESIAN_POINT('Ctrl Pts',(2.8477059680593,30.7210798780603,126.503186253981));
#123114=CARTESIAN_POINT('Ctrl Pts',(2.86062048426853,30.5299717219439,126.586129537178));
#123115=CARTESIAN_POINT('Ctrl Pts',(2.8691980346961,30.3896780366754,126.626289545261));
#123116=CARTESIAN_POINT('Ctrl Pts',(2.87998171472577,30.2233020437298,126.651126200779));
#123117=CARTESIAN_POINT('Ctrl Pts',(2.88146959984958,30.2005626630594,126.654042328997));
#123118=CARTESIAN_POINT('Ctrl Pts',(2.8835604985241,30.169040636722,126.657425224111));
#123119=CARTESIAN_POINT('Ctrl Pts',(2.88414311380086,30.1603024875565,126.658293162989));
#123120=CARTESIAN_POINT('Ctrl Pts',(2.88513957805721,30.1454431902161,126.659650560478));
#123121=CARTESIAN_POINT('Ctrl Pts',(2.88555149478189,30.1393253024884,126.660175341159));
#123122=CARTESIAN_POINT('Ctrl Pts',(2.8864159330681,30.1265409799594,126.661200791808));
#123123=CARTESIAN_POINT('Ctrl Pts',(2.88686876590961,30.119874290692,126.66169517084));
#123124=CARTESIAN_POINT('Ctrl Pts',(2.88809823298623,30.1018506238574,126.662922718974));
#123125=CARTESIAN_POINT('Ctrl Pts',(2.88887884151984,30.0904890540283,126.663579644047));
#123126=CARTESIAN_POINT('Ctrl Pts',(2.89276124346385,30.0343413814461,126.666249234226));
#123127=CARTESIAN_POINT('Ctrl Pts',(2.89593927887881,29.9894970689316,126.666569761793));
#123128=CARTESIAN_POINT('Ctrl Pts',(2.90547612845563,29.8567830012224,126.662162036695));
#123129=CARTESIAN_POINT('Ctrl Pts',(2.91193072300331,29.7692373708531,126.652283989316));
#123130=CARTESIAN_POINT('Ctrl Pts',(2.92267577694516,29.623374918835,126.624002354429));
#123131=CARTESIAN_POINT('Ctrl Pts',(2.92700963160559,29.5645381565499,126.609224762518));
#123132=CARTESIAN_POINT('Ctrl Pts',(2.933119339431,29.4811896525542,126.583382899251));
#123133=CARTESIAN_POINT('Ctrl Pts',(2.93496670580938,29.4559382285905,126.574884918794));
#123134=CARTESIAN_POINT('Ctrl Pts',(2.93827174992921,29.4106758654013,126.558433868167));
#123135=CARTESIAN_POINT('Ctrl Pts',(2.93973577249966,29.3905950687023,126.550691704362));
#123136=CARTESIAN_POINT('Ctrl Pts',(2.94201164346743,29.3593437024263,126.537941845825));
#123137=CARTESIAN_POINT('Ctrl Pts',(2.94283217480837,29.3480693167826,126.533196664119));
#123138=CARTESIAN_POINT('Ctrl Pts',(2.94436071387478,29.3270580963708,126.524079748587));
#123139=CARTESIAN_POINT('Ctrl Pts',(2.94506968721008,29.3173090972797,126.519737814926));
#123140=CARTESIAN_POINT('Ctrl Pts',(2.94665532922495,29.2955021949079,126.509773434883));
#123141=CARTESIAN_POINT('Ctrl Pts',(2.94753018440601,29.2834684735075,126.504099588021));
#123142=CARTESIAN_POINT('Ctrl Pts',(2.94976874416363,29.252684687574,126.48913186307));
#123143=CARTESIAN_POINT('Ctrl Pts',(2.95112515828914,29.2340390986472,126.479627602431));
#123144=CARTESIAN_POINT('Ctrl Pts',(2.9607714366619,29.1016695867877,126.40898157404));
#123145=CARTESIAN_POINT('Ctrl Pts',(2.96857500373158,28.9952149178294,126.335154390318));
#123146=CARTESIAN_POINT('Ctrl Pts',(2.98158070008948,28.8357769450745,126.194611997377));
#123147=CARTESIAN_POINT('Ctrl Pts',(2.98672011951199,28.7774446259738,126.134842683276));
#123148=CARTESIAN_POINT('Ctrl Pts',(2.99306394893745,28.7147909360834,126.060184796897));
#123149=CARTESIAN_POINT('Ctrl Pts',(2.99398819234034,28.7058795610027,126.04928852029));
#123150=CARTESIAN_POINT('Ctrl Pts',(2.99540289343865,28.6925869292023,126.032608193478));
#123151=CARTESIAN_POINT('Ctrl Pts',(2.99588648657258,28.6881033788603,126.026905969133));
#123152=CARTESIAN_POINT('Ctrl Pts',(2.9967757101234,28.6799723613746,126.016424702276));
#123153=CARTESIAN_POINT('Ctrl Pts',(2.99718052438614,28.6763133376372,126.011654960091));
#123154=CARTESIAN_POINT('Ctrl Pts',(2.99811256822277,28.6679857390021,126.000676943365));
#123155=CARTESIAN_POINT('Ctrl Pts',(2.99864095269692,28.6633347249646,125.994455767225));
#123156=CARTESIAN_POINT('Ctrl Pts',(3.00027614303048,28.6491503753529,125.975203560358));
#123157=CARTESIAN_POINT('Ctrl Pts',(3.00139197289242,28.6397631554656,125.962066718775));
#123158=CARTESIAN_POINT('Ctrl Pts',(3.00785170084655,28.5869974212952,125.88590805824));
#123159=CARTESIAN_POINT('Ctrl Pts',(3.01339405136169,28.5478138613454,125.820099113123));
#123160=CARTESIAN_POINT('Ctrl Pts',(3.02367981821342,28.4840154051156,125.693942296414));
#123161=CARTESIAN_POINT('Ctrl Pts',(3.0284089031753,28.4581425546146,125.634382764511));
#123162=CARTESIAN_POINT('Ctrl Pts',(3.03667846597153,28.4185187260463,125.526304092791));
#123163=CARTESIAN_POINT('Ctrl Pts',(3.04024277763164,28.403369279339,125.478382839419));
#123164=CARTESIAN_POINT('Ctrl Pts',(3.04614662244591,28.3815124549162,125.396538289062));
#123165=CARTESIAN_POINT('Ctrl Pts',(3.04851844013303,28.3736529454115,125.362960203776));
#123166=CARTESIAN_POINT('Ctrl Pts',(3.05184951356238,28.3639509549359,125.314822855414));
#123167=CARTESIAN_POINT('Ctrl Pts',(3.05283562313009,28.3612501464017,125.300447747825));
#123168=CARTESIAN_POINT('Ctrl Pts',(3.05454177222463,28.3568786869573,125.275364741452));
#123169=CARTESIAN_POINT('Ctrl Pts',(3.05526447664666,28.3551225933755,125.264672848878));
#123170=CARTESIAN_POINT('Ctrl Pts',(3.05665798183441,28.3519233047215,125.243930876256));
#123171=CARTESIAN_POINT('Ctrl Pts',(3.05732915303646,28.3504674328856,125.233883269289));
#123172=CARTESIAN_POINT('Ctrl Pts',(3.05911652231163,28.3468196776442,125.206977758677));
#123173=CARTESIAN_POINT('Ctrl Pts',(3.0602274796093,28.3447937737002,125.190098274724));
#123174=CARTESIAN_POINT('Ctrl Pts',(3.06447609585473,28.3379886392869,125.124991090773));
#123175=CARTESIAN_POINT('Ctrl Pts',(3.06755653922172,28.3350559042702,125.076592173165));
#123176=CARTESIAN_POINT('Ctrl Pts',(3.07809925085577,28.3322130159441,124.908249071328));
#123177=CARTESIAN_POINT('Ctrl Pts',(3.0852718322245,28.3431352879358,124.788504523533));
#123178=CARTESIAN_POINT('Ctrl Pts',(3.09518818485887,28.3747983060623,124.631340674317));
#123179=CARTESIAN_POINT('Ctrl Pts',(3.09771581674007,28.3842215499221,124.592017383705));
#123180=CARTESIAN_POINT('Ctrl Pts',(3.10188704564452,28.4017247032338,124.529161993919));
#123181=CARTESIAN_POINT('Ctrl Pts',(3.10349499226149,28.4089179978693,124.505398889994));
#123182=CARTESIAN_POINT('Ctrl Pts',(3.10572704502167,28.4194534531143,124.473207359104));
#123183=CARTESIAN_POINT('Ctrl Pts',(3.10632697040285,28.4223378002467,124.464631110683));
#123184=CARTESIAN_POINT('Ctrl Pts',(3.10734398546722,28.4273123026022,124.450229405107));
#123185=CARTESIAN_POINT('Ctrl Pts',(3.10775894284056,28.4293653758128,124.444391165977));
#123186=CARTESIAN_POINT('Ctrl Pts',(3.10856453673155,28.4333950685419,124.43313293382));
#123187=CARTESIAN_POINT('Ctrl Pts',(3.1089548846171,28.4353673799386,124.427711573005));
#123188=CARTESIAN_POINT('Ctrl Pts',(3.1100323637874,28.4408666520327,124.412836465196));
#123189=CARTESIAN_POINT('Ctrl Pts',(3.11072275096625,28.444451334304,124.403404534625));
#123190=CARTESIAN_POINT('Ctrl Pts',(3.11354129899314,28.459340532903,124.365275062926));
#123191=CARTESIAN_POINT('Ctrl Pts',(3.11570521700883,28.4713546087149,124.336863270827));
#123192=CARTESIAN_POINT('Ctrl Pts',(3.12486595233927,28.524862083711,124.219516980018));
#123193=CARTESIAN_POINT('Ctrl Pts',(3.13207592402463,28.5733823403823,124.134005360044));
#123194=CARTESIAN_POINT('Ctrl Pts',(3.14387363295889,28.6659059948645,124.000032957676));
#123195=CARTESIAN_POINT('Ctrl Pts',(3.14851138548278,28.7057399331862,123.948984659089));
#123196=CARTESIAN_POINT('Ctrl Pts',(3.15591551809863,28.775429196581,123.869666570163));
#123197=CARTESIAN_POINT('Ctrl Pts',(3.15874055968381,28.8035357619547,123.839956405336));
#123198=CARTESIAN_POINT('Ctrl Pts',(3.16257781918233,28.8438193544095,123.800398074729));
#123199=CARTESIAN_POINT('Ctrl Pts',(3.16362931632742,28.8550821858649,123.789643981373));
#123200=CARTESIAN_POINT('Ctrl Pts',(3.16541188485943,28.8745548122119,123.771565999191));
#123201=CARTESIAN_POINT('Ctrl Pts',(3.16614631717641,28.8826892142886,123.764162800692));
#123202=CARTESIAN_POINT('Ctrl Pts',(3.16753837535789,28.8983174211389,123.750219859778));
#123203=CARTESIAN_POINT('Ctrl Pts',(3.16819658966974,28.9057976044839,123.743665638305));
#123204=CARTESIAN_POINT('Ctrl Pts',(3.1698961300391,28.9253436652138,123.726846159011));
#123205=CARTESIAN_POINT('Ctrl Pts',(3.17093315991077,28.9374982456451,123.716685155119));
#123206=CARTESIAN_POINT('Ctrl Pts',(3.1745449639437,28.9806072719259,123.681679187845));
#123207=CARTESIAN_POINT('Ctrl Pts',(3.17708298180775,29.0123042012483,123.657767272609));
#123208=CARTESIAN_POINT('Ctrl Pts',(3.18703174815099,29.1415090216432,123.567354274854));
#123209=CARTESIAN_POINT('Ctrl Pts',(3.19412232044589,29.2451029463337,123.510163791845));
#123210=CARTESIAN_POINT('Ctrl Pts',(3.20545085458583,29.4149925939744,123.438680266656));
#123211=CARTESIAN_POINT('Ctrl Pts',(3.20957435327357,29.4775866670924,123.416637958818));
#123212=CARTESIAN_POINT('Ctrl Pts',(3.21490157245063,29.5565419525,123.394026251145));
#123213=CARTESIAN_POINT('Ctrl Pts',(3.21593849753998,29.5718249111311,123.389884236938));
#123214=CARTESIAN_POINT('Ctrl Pts',(3.21749041712337,29.5945260788391,123.384077771955));
#123215=CARTESIAN_POINT('Ctrl Pts',(3.21799639264703,29.6019008857442,123.382245124426));
#123216=CARTESIAN_POINT('Ctrl Pts',(3.21890733157072,29.6151247944122,123.379054865311));
#123217=CARTESIAN_POINT('Ctrl Pts',(3.21931121793574,29.6209690585979,123.377678331411));
#123218=CARTESIAN_POINT('Ctrl Pts',(3.2202167918883,29.6340300445327,123.374676428692));
#123219=CARTESIAN_POINT('Ctrl Pts',(3.22071935650986,29.6412501421166,123.37306753245));
#123220=CARTESIAN_POINT('Ctrl Pts',(3.22223452539326,29.6629402830115,123.368385592928));
#123221=CARTESIAN_POINT('Ctrl Pts',(3.22325461251871,29.6774403443719,123.365457232998));
#123222=CARTESIAN_POINT('Ctrl Pts',(3.23212030405779,29.8027395069395,123.341884537806));
#123223=CARTESIAN_POINT('Ctrl Pts',(3.24040579483127,29.9153219494606,123.332341553944));
#123224=CARTESIAN_POINT('Ctrl Pts',(3.25502125559649,30.1165959031958,123.335724323828));
#123225=CARTESIAN_POINT('Ctrl Pts',(3.26137212387327,30.2049461765468,123.344279852133));
#123226=CARTESIAN_POINT('Ctrl Pts',(3.26956240925985,30.3212642648536,123.365002632665));
#123227=CARTESIAN_POINT('Ctrl Pts',(3.27158521968818,30.3501802488817,123.370950858853));
#123228=CARTESIAN_POINT('Ctrl Pts',(3.27451750064764,30.3923520757415,123.380800820732));
#123229=CARTESIAN_POINT('Ctrl Pts',(3.27544577401502,30.4057404534445,123.384103704513));
#123230=CARTESIAN_POINT('Ctrl Pts',(3.27708611589577,30.4294604993485,123.390268790646));
#123231=CARTESIAN_POINT('Ctrl Pts',(3.27780025571393,30.4398082998792,123.39306516764));
#123232=CARTESIAN_POINT('Ctrl Pts',(3.27930238687223,30.4616139979326,123.399184326891));
#123233=CARTESIAN_POINT('Ctrl Pts',(3.28008956846626,30.473064686975,123.402530714929));
#123234=CARTESIAN_POINT('Ctrl Pts',(3.28219155590904,30.5036947891746,123.411840395599));
#123235=CARTESIAN_POINT('Ctrl Pts',(3.28349901697462,30.5228043285662,123.418028110187));
#123236=CARTESIAN_POINT('Ctrl Pts',(3.29110887254802,30.6342382453536,123.456350531951));
#123237=CARTESIAN_POINT('Ctrl Pts',(3.29714530477315,30.7237062879604,123.496216604328));
#123238=CARTESIAN_POINT('Ctrl Pts',(3.30753549303479,30.872203427531,123.578727027031));
#123239=CARTESIAN_POINT('Ctrl Pts',(3.31190841014993,30.9328928924409,123.617804008825));
#123240=CARTESIAN_POINT('Ctrl Pts',(3.31965997291716,31.0331691807712,123.69199097212));
#123241=CARTESIAN_POINT('Ctrl Pts',(3.32298482121273,31.0739693307999,123.725278511882));
#123242=CARTESIAN_POINT('Ctrl Pts',(3.32718175520478,31.1216700648778,123.768113529545));
#123243=CARTESIAN_POINT('Ctrl Pts',(3.32793952126156,31.1301387885983,123.775878147016));
#123244=CARTESIAN_POINT('Ctrl Pts',(3.32914978264526,31.1434240067198,123.788314170853));
#123245=CARTESIAN_POINT('Ctrl Pts',(3.32959810350882,31.1482939332931,123.792928317583));
#123246=CARTESIAN_POINT('Ctrl Pts',(3.33046048098246,31.1575603673239,123.801814881478));
#123247=CARTESIAN_POINT('Ctrl Pts',(3.33087417325538,31.1619613457941,123.806082327778));
#123248=CARTESIAN_POINT('Ctrl Pts',(3.33188093263697,31.1725667468185,123.816480122207));
#123249=CARTESIAN_POINT('Ctrl Pts',(3.3324758536315,31.1787467169499,123.822635041387));
#123250=CARTESIAN_POINT('Ctrl Pts',(3.33450972238414,31.199589608525,123.843722032137));
#123251=CARTESIAN_POINT('Ctrl Pts',(3.33596450408592,31.2140187469185,123.858881096811));
#123252=CARTESIAN_POINT('Ctrl Pts',(3.34490408043666,31.3000213075562,123.95271192715));
#123253=CARTESIAN_POINT('Ctrl Pts',(3.35272216199712,31.3642076253796,124.037813402579));
#123254=CARTESIAN_POINT('Ctrl Pts',(3.36756474752012,31.4712346299523,124.212170329023));
#123255=CARTESIAN_POINT('Ctrl Pts',(3.37457589674533,31.5151288015248,124.300287548376));
#123256=CARTESIAN_POINT('Ctrl Pts',(3.38280007253362,31.5588768919739,124.41184717088));
#123257=CARTESIAN_POINT('Ctrl Pts',(3.38426709555954,31.5663586084554,124.432072451718));
#123258=CARTESIAN_POINT('Ctrl Pts',(3.38654654722683,31.5774690161018,124.463998752982));
#123259=CARTESIAN_POINT('Ctrl Pts',(3.38736770404948,31.5813646923647,124.475603625904));
#123260=CARTESIAN_POINT('Ctrl Pts',(3.3888968140588,31.5884163796476,124.497403471591));
#123261=CARTESIAN_POINT('Ctrl Pts',(3.38960573961199,31.5916029980613,124.507587803644));
#123262=CARTESIAN_POINT('Ctrl Pts',(3.39119051260019,31.5985384111118,124.530524130365));
#123263=CARTESIAN_POINT('Ctrl Pts',(3.39206455546905,31.6022329270157,124.543291878118));
#123264=CARTESIAN_POINT('Ctrl Pts',(3.39429952106896,31.6113383287057,124.576230180002));
#123265=CARTESIAN_POINT('Ctrl Pts',(3.39565319394755,31.616523576891,124.596461083212));
#123266=CARTESIAN_POINT('Ctrl Pts',(3.40532392051984,31.651121597653,124.742840260298));
#123267=CARTESIAN_POINT('Ctrl Pts',(3.41315090634434,31.6661146386835,124.871939976784));
#123268=CARTESIAN_POINT('Ctrl Pts',(3.42169053587817,31.6659904387919,125.011483828701));
#123269=CARTESIAN_POINT('Ctrl Pts',(3.42230324180335,31.6658914832599,125.021484514393));
#123270=CARTESIAN_POINT('Ctrl Pts',(3.42757187605949,31.6642691668115,125.107316267364));
#123271=CARTESIAN_POINT('Ctrl Pts',(3.43227947183841,31.6576591413254,125.182953145629));
#123272=CARTESIAN_POINT('Ctrl Pts',(3.43803510316227,31.6440205893638,125.270006114265));
#123273=CARTESIAN_POINT('Ctrl Pts',(3.43884407433654,31.6419844131629,125.282124378797));
#123274=CARTESIAN_POINT('Ctrl Pts',(3.44012204237294,31.6385865334908,125.301062313955));
#123275=CARTESIAN_POINT('Ctrl Pts',(3.44058615310007,31.6373158124992,125.307898149363));
#123276=CARTESIAN_POINT('Ctrl Pts',(3.44145899199215,31.6348585608187,125.320671398859));
#123277=CARTESIAN_POINT('Ctrl Pts',(3.44186714411603,31.6336824047121,125.326610556756));
#123278=CARTESIAN_POINT('Ctrl Pts',(3.44283341824922,31.6308340380017,125.340593359794));
#123279=CARTESIAN_POINT('Ctrl Pts',(3.44339302404201,31.629134672667,125.348631191206));
#123280=CARTESIAN_POINT('Ctrl Pts',(3.44527697932228,31.6232457411608,125.375501643422));
#123281=CARTESIAN_POINT('Ctrl Pts',(3.44661486036773,31.6187886723666,125.39427322425));
#123282=CARTESIAN_POINT('Ctrl Pts',(3.44994491598246,31.6070026459566,125.440337320279));
#123283=CARTESIAN_POINT('Ctrl Pts',(3.45195164831175,31.599303442617,125.467528371332));
#123284=CARTESIAN_POINT('Ctrl Pts',(3.45602017567125,31.5824492453355,125.52175111791));
#123285=CARTESIAN_POINT('Ctrl Pts',(3.45808088852165,31.5732866945828,125.548759939466));
#123286=CARTESIAN_POINT('Ctrl Pts',(3.46014891354656,31.5634400625339,125.575509488075));
#123287=CARTESIAN_POINT('',(3.23000355491767,31.6660003196933,124.999395783345));
#123288=CARTESIAN_POINT('Ctrl Pts',(3.26654942290125,31.5634400114153,125.575509626944));
#123289=CARTESIAN_POINT('Ctrl Pts',(3.26608923191792,31.5659364284638,125.568727814589));
#123290=CARTESIAN_POINT('Ctrl Pts',(3.26563026442176,31.5683888288847,125.561929459962));
#123291=CARTESIAN_POINT('Ctrl Pts',(3.26175567718783,31.5887702507647,125.504256584977));
#123292=CARTESIAN_POINT('Ctrl Pts',(3.25840827363323,31.6042637027712,125.452553012212));
#123293=CARTESIAN_POINT('Ctrl Pts',(3.25136312741718,31.6317934377905,125.341300417692));
#123294=CARTESIAN_POINT('Ctrl Pts',(3.24767930295061,31.6431377050807,125.28166345445));
#123295=CARTESIAN_POINT('Ctrl Pts',(3.23940935061001,31.6610854010454,125.147894277671));
#123296=CARTESIAN_POINT('Ctrl Pts',(3.23481638988841,31.6660268335795,125.073679945117));
#123297=CARTESIAN_POINT('Ctrl Pts',(3.23000429551471,31.6659998904155,124.999395735533));
#123298=CARTESIAN_POINT('Ctrl Pts',(3.23000440964381,31.6659998910536,124.999397497343));
#123299=CARTESIAN_POINT('Ctrl Pts',(3.22944762951936,31.6659967827001,124.990802487001));
#123300=CARTESIAN_POINT('Ctrl Pts',(3.22888796913527,31.6659271610561,124.982207798573));
#123301=CARTESIAN_POINT('Ctrl Pts',(3.22781267407205,31.665667102016,124.965789721261));
#123302=CARTESIAN_POINT('Ctrl Pts',(3.22729759777495,31.6654880388823,124.957966386865));
#123303=CARTESIAN_POINT('Ctrl Pts',(3.22636902803633,31.6650681990382,124.943942980828));
#123304=CARTESIAN_POINT('Ctrl Pts',(3.2259565956253,31.664847885872,124.937742384129));
#123305=CARTESIAN_POINT('Ctrl Pts',(3.22516379738237,31.664360059699,124.925880406756));
#123306=CARTESIAN_POINT('Ctrl Pts',(3.2247837449481,31.664098279809,124.920218822269));
#123307=CARTESIAN_POINT('Ctrl Pts',(3.22396279904964,31.6634731437093,124.908045476223));
#123308=CARTESIAN_POINT('Ctrl Pts',(3.22352140189257,31.6631004340768,124.901534387878));
#123309=CARTESIAN_POINT('Ctrl Pts',(3.2223546176247,31.6620191634388,124.884408110011));
#123310=CARTESIAN_POINT('Ctrl Pts',(3.22162589643186,31.6612471462891,124.873797429269));
#123311=CARTESIAN_POINT('Ctrl Pts',(3.21840445398554,31.6574105836397,124.827233797765));
#123312=CARTESIAN_POINT('Ctrl Pts',(3.21586246647544,31.6532802809791,124.791381010853));
#123313=CARTESIAN_POINT('Ctrl Pts',(3.20562451751908,31.6322425991551,124.649469437146));
#123314=CARTESIAN_POINT('Ctrl Pts',(3.19771370889377,31.6062624843367,124.545017802866));
#123315=CARTESIAN_POINT('Ctrl Pts',(3.18602107104068,31.5521000669193,124.392094302889));
#123316=CARTESIAN_POINT('Ctrl Pts',(3.18211563770412,31.5312466637038,124.341328163862));
#123317=CARTESIAN_POINT('Ctrl Pts',(3.17653687767181,31.4972867537276,124.269031843283));
#123318=CARTESIAN_POINT('Ctrl Pts',(3.17480516696833,31.4861392970172,124.246626140132));
#123319=CARTESIAN_POINT('Ctrl Pts',(3.17168572395223,31.464948942663,124.206337117742));
#123320=CARTESIAN_POINT('Ctrl Pts',(3.17029267393445,31.4550727073158,124.188372217841));
#123321=CARTESIAN_POINT('Ctrl Pts',(3.16810179449721,31.4388857413205,124.160173726339));
#123322=CARTESIAN_POINT('Ctrl Pts',(3.16729632224105,31.432791771423,124.149818784408));
#123323=CARTESIAN_POINT('Ctrl Pts',(3.16578130769558,31.421060772584,124.130369774933));
#123324=CARTESIAN_POINT('Ctrl Pts',(3.16507096320784,31.4154471529324,124.121262374711));
#123325=CARTESIAN_POINT('Ctrl Pts',(3.16346296610323,31.4024837405915,124.100677428543));
#123326=CARTESIAN_POINT('Ctrl Pts',(3.16256735690727,31.3950799966663,124.089234634286));
#123327=CARTESIAN_POINT('Ctrl Pts',(3.160235832714,31.3753315034283,124.059518475247));
#123328=CARTESIAN_POINT('Ctrl Pts',(3.15880829835496,31.3627626754443,124.04139674227));
#123329=CARTESIAN_POINT('Ctrl Pts',(3.15024218807943,31.2845397643885,123.933264271455));
#123330=CARTESIAN_POINT('Ctrl Pts',(3.14344738531115,31.2103514671904,123.849773771238));
#123331=CARTESIAN_POINT('Ctrl Pts',(3.13062264146857,31.0558443368599,123.707534003338));
#123332=CARTESIAN_POINT('Ctrl Pts',(3.12461113188037,30.977537802283,123.647339615485));
#123333=CARTESIAN_POINT('Ctrl Pts',(3.11726684994839,30.8822912276902,123.586732995289));
#123334=CARTESIAN_POINT('Ctrl Pts',(3.1163261232019,30.8701003858477,123.579195044409));
#123335=CARTESIAN_POINT('Ctrl Pts',(3.11489137340451,30.8515526415955,123.568054661646));
#123336=CARTESIAN_POINT('Ctrl Pts',(3.11440451401603,30.8452664480177,123.564335004163));
#123337=CARTESIAN_POINT('Ctrl Pts',(3.11351242163061,30.8337669183006,123.55763222351));
#123338=CARTESIAN_POINT('Ctrl Pts',(3.11310804489819,30.8285616433028,123.554635798009));
#123339=CARTESIAN_POINT('Ctrl Pts',(3.11218109392786,30.8166461798106,123.547862159107));
#123340=CARTESIAN_POINT('Ctrl Pts',(3.11165741374762,30.8099259591167,123.544103291158));
#123341=CARTESIAN_POINT('Ctrl Pts',(3.11001138861411,30.7888311998346,123.532495460942));
#123342=CARTESIAN_POINT('Ctrl Pts',(3.10887961328207,30.7743673156416,123.524812064725));
#123343=CARTESIAN_POINT('Ctrl Pts',(3.10209237642772,30.6877357982926,123.480417399505));
#123344=CARTESIAN_POINT('Ctrl Pts',(3.09621494572295,30.6130889694828,123.448796836085));
#123345=CARTESIAN_POINT('Ctrl Pts',(3.08495771413926,30.4666583254375,123.39899407243));
#123346=CARTESIAN_POINT('Ctrl Pts',(3.07959224124605,30.3953660309375,123.3799145121));
#123347=CARTESIAN_POINT('Ctrl Pts',(3.07129888128102,30.2813555298315,123.357379953355));
#123348=CARTESIAN_POINT('Ctrl Pts',(3.06830306533877,30.2393676024499,123.350737981842));
#123349=CARTESIAN_POINT('Ctrl Pts',(3.06323022405642,30.1667908351939,123.342087839018));
#123350=CARTESIAN_POINT('Ctrl Pts',(3.06113171943038,30.1363175246406,123.339304464373));
#123351=CARTESIAN_POINT('Ctrl Pts',(3.05811240922627,30.0918347572182,123.336474310629));
#123352=CARTESIAN_POINT('Ctrl Pts',(3.05717116520443,30.0778755149462,123.335762406784));
#123353=CARTESIAN_POINT('Ctrl Pts',(3.0555164573438,30.0531780198984,123.334814300745));
#123354=CARTESIAN_POINT('Ctrl Pts',(3.05480078868459,30.0424435090379,123.334506117506));
#123355=CARTESIAN_POINT('Ctrl Pts',(3.05330384857882,30.0198839626366,123.334076696778));
#123356=CARTESIAN_POINT('Ctrl Pts',(3.052523305018,30.0080590671158,123.333977524833));
#123357=CARTESIAN_POINT('Ctrl Pts',(3.05045895808728,29.9766299898239,123.334048573286));
#123358=CARTESIAN_POINT('Ctrl Pts',(3.04918203802404,29.9570277972582,123.334438906566));
#123359=CARTESIAN_POINT('Ctrl Pts',(3.04257913310749,29.8549277744348,123.338275795651));
#123360=CARTESIAN_POINT('Ctrl Pts',(3.03743646908265,29.7727585324845,123.34750579861));
#123361=CARTESIAN_POINT('Ctrl Pts',(3.02621159844141,29.5931575752951,123.381336726373));
#123362=CARTESIAN_POINT('Ctrl Pts',(3.02018790806716,29.4965911241707,123.408721044981));
#123363=CARTESIAN_POINT('Ctrl Pts',(3.01213555699536,29.3766758060392,123.454741916964));
#123364=CARTESIAN_POINT('Ctrl Pts',(3.01034291568652,29.3505397920609,123.465543466888));
#123365=CARTESIAN_POINT('Ctrl Pts',(3.00727579188438,29.3070477952539,123.484828127528));
#123366=CARTESIAN_POINT('Ctrl Pts',(3.00601763132619,29.2895409791455,123.492957710288));
#123367=CARTESIAN_POINT('Ctrl Pts',(3.00419948125809,29.2647901500576,123.504978270309));
#123368=CARTESIAN_POINT('Ctrl Pts',(3.00365353948722,29.2574268638396,123.508621903689));
#123369=CARTESIAN_POINT('Ctrl Pts',(3.00269954974722,29.2446858423245,123.515044390292));
#123370=CARTESIAN_POINT('Ctrl Pts',(3.00229303096033,29.2392958145425,123.5177983334));
#123371=CARTESIAN_POINT('Ctrl Pts',(3.00141573962227,29.2277498676595,123.523777109051));
#123372=CARTESIAN_POINT('Ctrl Pts',(3.00094444123053,29.2215991742195,123.527011052084));
#123373=CARTESIAN_POINT('Ctrl Pts',(2.9996342504882,29.2046387967321,123.536064457668));
#123374=CARTESIAN_POINT('Ctrl Pts',(2.99879061122449,29.1938731841119,123.541964935139));
#123375=CARTESIAN_POINT('Ctrl Pts',(2.99285936166074,29.1191947573507,123.583974976772));
#123376=CARTESIAN_POINT('Ctrl Pts',(2.9875683876885,29.0576709083589,123.624151811937));
#123377=CARTESIAN_POINT('Ctrl Pts',(2.98122041712203,28.9878262569549,123.676649769886));
#123378=CARTESIAN_POINT('Ctrl Pts',(2.98020314425414,28.9767551095666,123.685191493708));
#123379=CARTESIAN_POINT('Ctrl Pts',(2.97382000014652,28.9079984609273,123.739633777752));
#123380=CARTESIAN_POINT('Ctrl Pts',(2.96845434657568,28.8533015165863,123.789184457528));
#123381=CARTESIAN_POINT('Ctrl Pts',(2.96016137272527,28.7725391977684,123.872746298215));
#123382=CARTESIAN_POINT('Ctrl Pts',(2.95716609284884,28.7441916692102,123.904414828906));
#123383=CARTESIAN_POINT('Ctrl Pts',(2.95209404791017,28.6975689721157,123.9606900851));
#123384=CARTESIAN_POINT('Ctrl Pts',(2.94999581271927,28.6787054374135,123.984779544265));
#123385=CARTESIAN_POINT('Ctrl Pts',(2.94697681219696,28.6522046429645,124.020612947446));
#123386=CARTESIAN_POINT('Ctrl Pts',(2.94603561434711,28.64403597099,124.031954083807));
#123387=CARTESIAN_POINT('Ctrl Pts',(2.94438095854266,28.6298448664701,124.052188719715));
#123388=CARTESIAN_POINT('Ctrl Pts',(2.9436652962379,28.6237640012545,124.06104004451));
#123389=CARTESIAN_POINT('Ctrl Pts',(2.9421683410089,28.6111676360915,124.079760630573));
#123390=CARTESIAN_POINT('Ctrl Pts',(2.94138777624414,28.6046707575993,124.089641746607));
#123391=CARTESIAN_POINT('Ctrl Pts',(2.93932330669706,28.5876834839577,124.11608686307));
#123392=CARTESIAN_POINT('Ctrl Pts',(2.9380462867162,28.5773791352406,124.132768598983));
#123393=CARTESIAN_POINT('Ctrl Pts',(2.93143992771044,28.525200352599,124.22067471995));
#123394=CARTESIAN_POINT('Ctrl Pts',(2.92629416486954,28.4883698025541,124.294763493629));
#123395=CARTESIAN_POINT('Ctrl Pts',(2.91506908605419,28.4193977524785,124.464015859961));
#123396=CARTESIAN_POINT('Ctrl Pts',(2.90904800629896,28.390049289096,124.559955877235));
#123397=CARTESIAN_POINT('Ctrl Pts',(2.90099879489973,28.3636883673267,124.685612482727));
#123398=CARTESIAN_POINT('Ctrl Pts',(2.89920650318679,28.3585893630659,124.713423289447));
#123399=CARTESIAN_POINT('Ctrl Pts',(2.89613991716965,28.3512044210566,124.760413709986));
#123400=CARTESIAN_POINT('Ctrl Pts',(2.89488193735399,28.3485398518485,124.77952834035));
#123401=CARTESIAN_POINT('Ctrl Pts',(2.89306400327071,28.3452153465866,124.806838827014));
#123402=CARTESIAN_POINT('Ctrl Pts',(2.89251809219995,28.3442830075713,124.815000751605));
#123403=CARTESIAN_POINT('Ctrl Pts',(2.89156413706995,28.3427686209241,124.829187836868));
#123404=CARTESIAN_POINT('Ctrl Pts',(2.89115762184814,28.3421589845353,124.835209815321));
#123405=CARTESIAN_POINT('Ctrl Pts',(2.89028031554994,28.340919903072,124.84815295074));
#123406=CARTESIAN_POINT('Ctrl Pts',(2.88980899841296,28.3403009503174,124.855074658979));
#123407=CARTESIAN_POINT('Ctrl Pts',(2.88849870597299,28.3387083217207,124.874235518156));
#123408=CARTESIAN_POINT('Ctrl Pts',(2.88765498261459,28.3378266359041,124.886481583925));
#123409=CARTESIAN_POINT('Ctrl Pts',(2.88170085173004,28.3325984551041,124.972336661931));
#123410=CARTESIAN_POINT('Ctrl Pts',(2.87638526315512,28.3330083071948,125.046146050823));
#123411=CARTESIAN_POINT('Ctrl Pts',(2.87011512066167,28.3392074572243,125.132220663024));
#123412=CARTESIAN_POINT('Ctrl Pts',(2.86920022172322,28.3402529134883,125.144754205294));
#123413=CARTESIAN_POINT('Ctrl Pts',(2.86279641950432,28.3485594398537,125.232351735376));
#123414=CARTESIAN_POINT('Ctrl Pts',(2.85730583372106,28.3607686736817,125.30686367938));
#123415=CARTESIAN_POINT('Ctrl Pts',(2.84891951398021,28.3876037615196,125.42131913763));
#123416=CARTESIAN_POINT('Ctrl Pts',(2.84594972126466,28.3987755656737,125.46196563411));
#123417=CARTESIAN_POINT('Ctrl Pts',(2.84091556729559,28.4206422099122,125.531139818426));
#123418=CARTESIAN_POINT('Ctrl Pts',(2.83883016903536,28.4305993735213,125.559877146311));
#123419=CARTESIAN_POINT('Ctrl Pts',(2.8358259288854,28.4462622815148,125.601373041239));
#123420=CARTESIAN_POINT('Ctrl Pts',(2.8348869358725,28.451350113537,125.614356559547));
#123421=CARTESIAN_POINT('Ctrl Pts',(2.83323476396836,28.4606421420797,125.637219437581));
#123422=CARTESIAN_POINT('Ctrl Pts',(2.83251940317294,28.4647798894719,125.647124754489));
#123423=CARTESIAN_POINT('Ctrl Pts',(2.83102171578353,28.473682733824,125.667871106731));
#123424=CARTESIAN_POINT('Ctrl Pts',(2.83024013049114,28.4784682753279,125.678702759118));
#123425=CARTESIAN_POINT('Ctrl Pts',(2.82816975939818,28.4915141137239,125.70739923356));
#123426=CARTESIAN_POINT('Ctrl Pts',(2.82688793048867,28.4999763349493,125.725170602168));
#123427=CARTESIAN_POINT('Ctrl Pts',(2.82008673483577,28.5469034763966,125.819383178545));
#123428=CARTESIAN_POINT('Ctrl Pts',(2.81476574922657,28.5909018149036,125.892929611599));
#123429=CARTESIAN_POINT('Ctrl Pts',(2.80352647892542,28.6967605444655,126.042423763495));
#123430=CARTESIAN_POINT('Ctrl Pts',(2.79765157040846,28.7600447450523,126.116955270718));
#123431=CARTESIAN_POINT('Ctrl Pts',(2.78977841579008,28.849368766442,126.20514924836));
#123432=CARTESIAN_POINT('Ctrl Pts',(2.78800603449176,28.8697443248551,126.224278922585));
#123433=CARTESIAN_POINT('Ctrl Pts',(2.78497009847331,28.9048667440436,126.255629471254));
#123434=CARTESIAN_POINT('Ctrl Pts',(2.7837224369373,28.9193611498396,126.268125315913));
#123435=CARTESIAN_POINT('Ctrl Pts',(2.78191683718211,28.9403595034149,126.285606884402));
#123436=CARTESIAN_POINT('Ctrl Pts',(2.78137268404044,28.9466905802202,126.290799094551));
#123437=CARTESIAN_POINT('Ctrl Pts',(2.78042070779235,28.9577653864412,126.299745978419));
#123438=CARTESIAN_POINT('Ctrl Pts',(2.78001439378176,28.9624917079205,126.303521822067));
#123439=CARTESIAN_POINT('Ctrl Pts',(2.77913621763289,28.972703854175,126.311589546725));
#123440=CARTESIAN_POINT('Ctrl Pts',(2.77866381676206,28.9781959755135,126.315872729946));
#123441=CARTESIAN_POINT('Ctrl Pts',(2.77734764052124,28.9934984812606,126.327653247953));
#123442=CARTESIAN_POINT('Ctrl Pts',(2.77649905079012,29.0033653714899,126.335075971174));
#123443=CARTESIAN_POINT('Ctrl Pts',(2.77002521186004,29.0787102163956,126.390456188607));
#123444=CARTESIAN_POINT('Ctrl Pts',(2.76415222016676,29.1475251621098,126.433676055205));
#123445=CARTESIAN_POINT('Ctrl Pts',(2.75366050534591,29.2749321145779,126.501270138842));
#123446=CARTESIAN_POINT('Ctrl Pts',(2.7490606523328,29.332294547713,126.527647032274));
#123447=CARTESIAN_POINT('Ctrl Pts',(2.73887014809178,29.4641319206823,126.579421344778));
#123448=CARTESIAN_POINT('Ctrl Pts',(2.73332826459998,29.5391952837345,126.602931260864));
#123449=CARTESIAN_POINT('Ctrl Pts',(2.72665930936424,29.6341094845195,126.625435361452));
#123450=CARTESIAN_POINT('Ctrl Pts',(2.72537215889611,29.6526449550512,126.629497010733));
#123451=CARTESIAN_POINT('Ctrl Pts',(2.72330822395127,29.6827072610619,126.635548223058));
#123452=CARTESIAN_POINT('Ctrl Pts',(2.72252525086594,29.6941922814834,126.637734509461));
#123453=CARTESIAN_POINT('Ctrl Pts',(2.7210278618457,29.7163074629667,126.641703595438));
#123454=CARTESIAN_POINT('Ctrl Pts',(2.72031290691692,29.7269337344024,126.643504479683));
#123455=CARTESIAN_POINT('Ctrl Pts',(2.71867534903226,29.7514215874654,126.647410490299));
#123456=CARTESIAN_POINT('Ctrl Pts',(2.71775504441344,29.7652938856565,126.649444030723));
#123457=CARTESIAN_POINT('Ctrl Pts',(2.71476910960261,29.8106422456316,126.655507939296));
#123458=CARTESIAN_POINT('Ctrl Pts',(2.71272605736257,29.842209151933,126.658814381774));
#123459=CARTESIAN_POINT('Ctrl Pts',(2.70264383453606,30.0001853716208,126.670810543705));
#123460=CARTESIAN_POINT('Ctrl Pts',(2.69502837993978,30.1271975408264,126.665962365335));
#123461=CARTESIAN_POINT('Ctrl Pts',(2.6840836703434,30.3034387242932,126.63894573199));
#123462=CARTESIAN_POINT('Ctrl Pts',(2.68089014888625,30.3540450708383,126.628763186564));
#123463=CARTESIAN_POINT('Ctrl Pts',(2.67575857260075,30.4323620649775,126.609182433477));
#123464=CARTESIAN_POINT('Ctrl Pts',(2.67387974124537,30.4604382687125,126.601374852077));
#123465=CARTESIAN_POINT('Ctrl Pts',(2.67133209660001,30.4974608902823,126.590025347803));
#123466=CARTESIAN_POINT('Ctrl Pts',(2.67069717887378,30.5066038302762,126.587135940091));
#123467=CARTESIAN_POINT('Ctrl Pts',(2.6696380099088,30.5217068213611,126.582219207083));
#123468=CARTESIAN_POINT('Ctrl Pts',(2.66921630901507,30.5276814041959,126.580236678435));
#123469=CARTESIAN_POINT('Ctrl Pts',(2.66835992027973,30.5397331294258,126.576161621997));
#123470=CARTESIAN_POINT('Ctrl Pts',(2.66792516509816,30.5458096487933,126.574067702927));
#123471=CARTESIAN_POINT('Ctrl Pts',(2.66679496470894,30.5615028776378,126.568558148879));
#123472=CARTESIAN_POINT('Ctrl Pts',(2.66609654053953,30.5711004209757,126.565089276706));
#123473=CARTESIAN_POINT('Ctrl Pts',(2.66319956791773,30.610523130223,126.550429707478));
#123474=CARTESIAN_POINT('Ctrl Pts',(2.66096281499383,30.6400542742139,126.538473589378));
#123475=CARTESIAN_POINT('Ctrl Pts',(2.65097345311355,30.7687205971854,126.482035546318));
#123476=CARTESIAN_POINT('Ctrl Pts',(2.64296767709374,30.8637088123153,126.428764377939));
#123477=CARTESIAN_POINT('Ctrl Pts',(2.63099559960946,30.999766338879,126.333902798652));
#123478=CARTESIAN_POINT('Ctrl Pts',(2.62691451983526,31.0449857240352,126.29878225012));
#123479=CARTESIAN_POINT('Ctrl Pts',(2.62027792440761,31.1168554941155,126.23677444253));
#123480=CARTESIAN_POINT('Ctrl Pts',(2.61767839377811,31.1445567531923,126.211184316766));
#123481=CARTESIAN_POINT('Ctrl Pts',(2.614091632524,31.1821170212712,126.174045934805));
#123482=CARTESIAN_POINT('Ctrl Pts',(2.61307157974278,31.1927213509525,126.16327138457));
#123483=CARTESIAN_POINT('Ctrl Pts',(2.61132612552146,31.210726921053,126.144471684482));
#123484=CARTESIAN_POINT('Ctrl Pts',(2.61059770023467,31.2181984833588,126.136515542723));
#123485=CARTESIAN_POINT('Ctrl Pts',(2.60911653368624,31.2333002529586,126.12011428141));
#123486=CARTESIAN_POINT('Ctrl Pts',(2.60836412313826,31.2409231959974,126.111663235817));
#123487=CARTESIAN_POINT('Ctrl Pts',(2.60646364308394,31.2600484018051,126.090018517044));
#123488=CARTESIAN_POINT('Ctrl Pts',(2.60532057092064,31.2714306282132,126.076720269119));
#123489=CARTESIAN_POINT('Ctrl Pts',(2.60073648248559,31.3165468031565,126.022296225832));
#123490=CARTESIAN_POINT('Ctrl Pts',(2.59736567137769,31.3485137854623,125.97974306972));
#123491=CARTESIAN_POINT('Ctrl Pts',(2.58601116936331,31.4507215337578,125.829184216894));
#123492=CARTESIAN_POINT('Ctrl Pts',(2.57834874049672,31.51044843214,125.714620214557));
#123493=CARTESIAN_POINT('Ctrl Pts',(2.56988925421428,31.5587739581986,125.588068557324));
#123494=CARTESIAN_POINT('Ctrl Pts',(2.56946987217007,31.5611259847506,125.581795954251));
#123495=CARTESIAN_POINT('Ctrl Pts',(2.56904933390813,31.5634400118358,125.575509625802));
#123496=CARTESIAN_POINT('Origin',(5.,30.,125.));
#123497=CARTESIAN_POINT('',(1.86811695019056,31.5634399562749,125.57550977674));
#123498=CARTESIAN_POINT('',(2.06219312175648,31.563440011958,125.57550962547));
#123499=CARTESIAN_POINT('',(5.,31.5634400119422,125.575509625513));
#123500=CARTESIAN_POINT('',(2.72302676052858,31.665999544352,124.999966471175));
#123501=CARTESIAN_POINT('Ctrl Pts',(2.06219312175648,31.563440011958,125.57550962547));
#123502=CARTESIAN_POINT('Ctrl Pts',(2.06231484708762,31.5627891862177,125.577277670622));
#123503=CARTESIAN_POINT('Ctrl Pts',(2.06243648101149,31.5621353548853,125.579044629305));
#123504=CARTESIAN_POINT('Ctrl Pts',(2.06925164381925,31.5253054375802,125.67805992843));
#123505=CARTESIAN_POINT('Ctrl Pts',(2.0756324149288,31.4801251938429,125.771722157109));
#123506=CARTESIAN_POINT('Ctrl Pts',(2.0887983756326,31.3688101572776,125.956240348087));
#123507=CARTESIAN_POINT('Ctrl Pts',(2.09554812002998,31.3016343222387,126.045838354362));
#123508=CARTESIAN_POINT('Ctrl Pts',(2.10377396890585,31.215922015026,126.138995948441));
#123509=CARTESIAN_POINT('Ctrl Pts',(2.1047512882903,31.2056846823302,126.149827172351));
#123510=CARTESIAN_POINT('Ctrl Pts',(2.10623075533151,31.1901357690531,126.165842139739));
#123511=CARTESIAN_POINT('Ctrl Pts',(2.10672505754805,31.184932296468,126.171130433003));
#123512=CARTESIAN_POINT('Ctrl Pts',(2.10762436945739,31.1754543445013,126.180635054225));
#123513=CARTESIAN_POINT('Ctrl Pts',(2.10802843681176,31.1711921621607,126.184863267796));
#123514=CARTESIAN_POINT('Ctrl Pts',(2.10894648309864,31.1615003415256,126.194374457592));
#123515=CARTESIAN_POINT('Ctrl Pts',(2.10946147379547,31.156057504266,126.199643459335));
#123516=CARTESIAN_POINT('Ctrl Pts',(2.11105255777801,31.1392174230616,126.21572466635));
#123517=CARTESIAN_POINT('Ctrl Pts',(2.11213723569339,31.1277033981437,126.226412574405));
#123518=CARTESIAN_POINT('Ctrl Pts',(2.11776959276997,31.0676605524709,126.280586978131));
#123519=CARTESIAN_POINT('Ctrl Pts',(2.12246258437263,31.0167657922176,126.321358290381));
#123520=CARTESIAN_POINT('Ctrl Pts',(2.1355219105744,30.8700428474146,126.425391383337));
#123521=CARTESIAN_POINT('Ctrl Pts',(2.14391103957429,30.7698494470602,126.481908590973));
#123522=CARTESIAN_POINT('Ctrl Pts',(2.15501367498537,30.6250688167146,126.544897028975));
#123523=CARTESIAN_POINT('Ctrl Pts',(2.15800227012495,30.5848453769678,126.560568589754));
#123524=CARTESIAN_POINT('Ctrl Pts',(2.1620521663546,30.5286065892752,126.579999440152));
#123525=CARTESIAN_POINT('Ctrl Pts',(2.16315718987412,30.5130795851568,126.585109626958));
#123526=CARTESIAN_POINT('Ctrl Pts',(2.16492841791662,30.487903858439,126.592986657812));
#123527=CARTESIAN_POINT('Ctrl Pts',(2.16559924956397,30.4783012738165,126.595896163953));
#123528=CARTESIAN_POINT('Ctrl Pts',(2.16699408313781,30.4581967224745,126.601789918692));
#123529=CARTESIAN_POINT('Ctrl Pts',(2.16771753186965,30.4476904990334,126.604758052427));
#123530=CARTESIAN_POINT('Ctrl Pts',(2.16943499196601,30.4225663754263,126.611589973862));
#123531=CARTESIAN_POINT('Ctrl Pts',(2.17042589069407,30.407923400741,126.615358508011));
#123532=CARTESIAN_POINT('Ctrl Pts',(2.173866020572,30.356598324263,126.627825156942));
#123533=CARTESIAN_POINT('Ctrl Pts',(2.17628206571861,30.3196725064753,126.635477585654));
#123534=CARTESIAN_POINT('Ctrl Pts',(2.18228518652278,30.2261383791953,126.651571989087));
#123535=CARTESIAN_POINT('Ctrl Pts',(2.18582633457376,30.1692951335907,126.658363193327));
#123536=CARTESIAN_POINT('Ctrl Pts',(2.19599832498569,30.003904166691,126.669528323762));
#123537=CARTESIAN_POINT('Ctrl Pts',(2.20251400819836,29.8951508506819,126.666236113557));
#123538=CARTESIAN_POINT('Ctrl Pts',(2.21140813023452,29.7558176380258,126.648317752978));
#123539=CARTESIAN_POINT('Ctrl Pts',(2.21346072168204,29.7242603312846,126.643333126849));
#123540=CARTESIAN_POINT('Ctrl Pts',(2.21622941755561,29.6828261808594,126.635561420476));
#123541=CARTESIAN_POINT('Ctrl Pts',(2.2169050000686,29.6728019286809,126.633585565818));
#123542=CARTESIAN_POINT('Ctrl Pts',(2.2180140722637,29.6564987501744,126.630216013647));
#123543=CARTESIAN_POINT('Ctrl Pts',(2.21844450520571,29.6502084273531,126.628877899647));
#123544=CARTESIAN_POINT('Ctrl Pts',(2.21930049520768,29.6377760348753,126.6261578747));
#123545=CARTESIAN_POINT('Ctrl Pts',(2.2197259641605,29.6316337664497,126.624777507278));
#123546=CARTESIAN_POINT('Ctrl Pts',(2.22080404156066,29.6161600013267,126.621207798638));
#123547=CARTESIAN_POINT('Ctrl Pts',(2.22145914551838,29.6068394175093,126.618972704018));
#123548=CARTESIAN_POINT('Ctrl Pts',(2.2241186656368,29.5693100586655,126.60962990419));
#123549=CARTESIAN_POINT('Ctrl Pts',(2.22615526131399,29.5412720904004,126.601864761229));
#123550=CARTESIAN_POINT('Ctrl Pts',(2.23186336714723,29.4642406198312,126.57834269446));
#123551=CARTESIAN_POINT('Ctrl Pts',(2.23558409626776,29.4157528725329,126.561044017813));
#123552=CARTESIAN_POINT('Ctrl Pts',(2.24849224655666,29.2514118472204,126.493682762023));
#123553=CARTESIAN_POINT('Ctrl Pts',(2.25769400967526,29.1404691927851,126.432720832713));
#123554=CARTESIAN_POINT('Ctrl Pts',(2.26870870646079,29.0111645325439,126.341192991018));
#123555=CARTESIAN_POINT('Ctrl Pts',(2.27092173493167,28.9854091633001,126.321816894845));
#123556=CARTESIAN_POINT('Ctrl Pts',(2.27406198197868,28.9492106248379,126.292902395978));
#123557=CARTESIAN_POINT('Ctrl Pts',(2.27501235043641,28.9383027832521,126.283960263277));
#123558=CARTESIAN_POINT('Ctrl Pts',(2.27668009619661,28.9192505697169,126.267932628841));
#123559=CARTESIAN_POINT('Ctrl Pts',(2.27739974508893,28.9110591727596,126.260904582646));
#123560=CARTESIAN_POINT('Ctrl Pts',(2.27889001156984,28.8941621673948,126.246119825689));
#123561=CARTESIAN_POINT('Ctrl Pts',(2.27966004370379,28.885468505363,126.238350310336));
#123562=CARTESIAN_POINT('Ctrl Pts',(2.28166278776605,28.8629619861222,126.217807241287));
#123563=CARTESIAN_POINT('Ctrl Pts',(2.28288935440913,28.8492824267927,126.204889636175));
#123564=CARTESIAN_POINT('Ctrl Pts',(2.2890017913848,28.7817082453176,126.138878546755));
#123565=CARTESIAN_POINT('Ctrl Pts',(2.29373535362855,28.7312522112861,126.082386373105));
#123566=CARTESIAN_POINT('Ctrl Pts',(2.30239056060592,28.6450207047523,125.971487511175));
#123567=CARTESIAN_POINT('Ctrl Pts',(2.3063251398579,28.6082550963964,125.918043077578));
#123568=CARTESIAN_POINT('Ctrl Pts',(2.31497358055427,28.5351393486953,125.797230345943));
#123569=CARTESIAN_POINT('Ctrl Pts',(2.31969069810125,28.5001297080804,125.729232017946));
#123570=CARTESIAN_POINT('Ctrl Pts',(2.32568657328166,28.4635257513297,125.644254228056));
#123571=CARTESIAN_POINT('Ctrl Pts',(2.32674289278498,28.4573552313602,125.629335918189));
#123572=CARTESIAN_POINT('Ctrl Pts',(2.32832540632171,28.448538604023,125.607111082976));
#123573=CARTESIAN_POINT('Ctrl Pts',(2.32884227884974,28.4457250555176,125.599871420605));
#123574=CARTESIAN_POINT('Ctrl Pts',(2.32976454291645,28.4408238590203,125.586993954589));
#123575=CARTESIAN_POINT('Ctrl Pts',(2.33016873343164,28.4387159526978,125.581364139575));
#123576=CARTESIAN_POINT('Ctrl Pts',(2.33106474337751,28.4341316668017,125.568915623458));
#123577=CARTESIAN_POINT('Ctrl Pts',(2.33155732981303,28.4316693626588,125.562092190422));
#123578=CARTESIAN_POINT('Ctrl Pts',(2.33301304691124,28.4245598212857,125.541980100141));
#123579=CARTESIAN_POINT('Ctrl Pts',(2.33398284829192,28.4200365011293,125.528648744649));
#123580=CARTESIAN_POINT('Ctrl Pts',(2.3407725054562,28.3897986134358,125.435673942654));
#123581=CARTESIAN_POINT('Ctrl Pts',(2.34684448950259,28.3699509518981,125.354256299569));
#123582=CARTESIAN_POINT('Ctrl Pts',(2.36230371302771,28.3353092941659,125.144687285004));
#123583=CARTESIAN_POINT('Ctrl Pts',(2.37163215567612,28.3291029829872,125.015642098542));
#123584=CARTESIAN_POINT('Ctrl Pts',(2.38193366428839,28.3392461574188,124.866238622592));
#123585=CARTESIAN_POINT('Ctrl Pts',(2.38336373979404,28.3410607293745,124.845352020939));
#123586=CARTESIAN_POINT('Ctrl Pts',(2.38568206348581,28.3446716199138,124.811264139324));
#123587=CARTESIAN_POINT('Ctrl Pts',(2.38657752852385,28.3462328467409,124.798040866294));
#123588=CARTESIAN_POINT('Ctrl Pts',(2.38818179854772,28.3493308181814,124.774254223855));
#123589=CARTESIAN_POINT('Ctrl Pts',(2.38889234291897,28.3508108592451,124.763684341683));
#123590=CARTESIAN_POINT('Ctrl Pts',(2.39040987926162,28.3542037689673,124.741040174056));
#123591=CARTESIAN_POINT('Ctrl Pts',(2.39121583326844,28.3561481745557,124.72897119179));
#123592=CARTESIAN_POINT('Ctrl Pts',(2.39342684271795,28.3618753986251,124.695754578958));
#123593=CARTESIAN_POINT('Ctrl Pts',(2.39482313524652,28.3659347605844,124.674656569582));
#123594=CARTESIAN_POINT('Ctrl Pts',(2.40352072320405,28.3939924887682,124.542646159419));
#123595=CARTESIAN_POINT('Ctrl Pts',(2.41045532144491,28.4288623700194,124.43434704776));
#123596=CARTESIAN_POINT('Ctrl Pts',(2.42343326398717,28.5142820621516,124.23973181976));
#123597=CARTESIAN_POINT('Ctrl Pts',(2.42946142027302,28.5620910209305,124.152782142219));
#123598=CARTESIAN_POINT('Ctrl Pts',(2.4369187935266,28.626246403007,124.05733749447));
#123599=CARTESIAN_POINT('Ctrl Pts',(2.43796541666402,28.6353543180777,124.044199988772));
#123600=CARTESIAN_POINT('Ctrl Pts',(2.43952909600102,28.6490852029212,124.024990565933));
#123601=CARTESIAN_POINT('Ctrl Pts',(2.44003693506263,28.6535634232798,124.018815652042));
#123602=CARTESIAN_POINT('Ctrl Pts',(2.44094978134239,28.6616427152804,124.007834770874));
#123603=CARTESIAN_POINT('Ctrl Pts',(2.44135369022403,28.6652275899375,124.003017214677));
#123604=CARTESIAN_POINT('Ctrl Pts',(2.44225749895012,28.6732709598002,123.992329224982));
#123605=CARTESIAN_POINT('Ctrl Pts',(2.44275825603309,28.6777423609436,123.98646901));
#123606=CARTESIAN_POINT('Ctrl Pts',(2.4442625596831,28.6912234478525,123.969041752596));
#123607=CARTESIAN_POINT('Ctrl Pts',(2.44527343738382,28.7003468249733,123.957564122197));
#123608=CARTESIAN_POINT('Ctrl Pts',(2.44765198017155,28.7219879545002,123.931064298304));
#123609=CARTESIAN_POINT('Ctrl Pts',(2.44902595940349,28.7346209170494,123.916139294703));
#123610=CARTESIAN_POINT('Ctrl Pts',(2.45400059784178,28.7809200023238,123.86335288));
#123611=CARTESIAN_POINT('Ctrl Pts',(2.4576622429291,28.8160450206779,123.826810886431));
#123612=CARTESIAN_POINT('Ctrl Pts',(2.47029424685196,28.9421087011361,123.707096917967));
#123613=CARTESIAN_POINT('Ctrl Pts',(2.47928650658561,29.0405886223175,123.632421515674));
#123614=CARTESIAN_POINT('Ctrl Pts',(2.49027513645961,29.1759058271934,123.551689187209));
#123615=CARTESIAN_POINT('Ctrl Pts',(2.49263963166935,29.2059370662376,123.535008610103));
#123616=CARTESIAN_POINT('Ctrl Pts',(2.49589057643095,29.248495607888,123.513063423203));
#123617=CARTESIAN_POINT('Ctrl Pts',(2.49680445631832,29.2606021770034,123.507006325224));
#123618=CARTESIAN_POINT('Ctrl Pts',(2.49838425131612,29.2817751986499,123.496733869181));
#123619=CARTESIAN_POINT('Ctrl Pts',(2.49905246958652,29.2908081090442,123.492451395588));
#123620=CARTESIAN_POINT('Ctrl Pts',(2.50044667841361,29.3098140892484,123.483649354386));
#123621=CARTESIAN_POINT('Ctrl Pts',(2.50117207549156,29.3197942986351,123.479146264294));
#123622=CARTESIAN_POINT('Ctrl Pts',(2.50290305226282,29.3438240237021,123.46858786835));
#123623=CARTESIAN_POINT('Ctrl Pts',(2.50390538625201,29.3579141327025,123.462626982969));
#123624=CARTESIAN_POINT('Ctrl Pts',(2.50743613085758,29.4081432165906,123.442188380183));
#123625=CARTESIAN_POINT('Ctrl Pts',(2.50992888344628,29.4447068368197,123.428783475297));
#123626=CARTESIAN_POINT('Ctrl Pts',(2.51618095379018,29.5387567160002,123.397996939118));
#123627=CARTESIAN_POINT('Ctrl Pts',(2.51988887958108,29.5967749617278,123.382418617265));
#123628=CARTESIAN_POINT('Ctrl Pts',(2.52702891407718,29.7107654582403,123.358327421136));
#123629=CARTESIAN_POINT('Ctrl Pts',(2.53046000823088,29.7665778892013,123.349466901731));
#123630=CARTESIAN_POINT('Ctrl Pts',(2.5385518614802,29.897655105699,123.335440214263));
#123631=CARTESIAN_POINT('Ctrl Pts',(2.54323033156511,29.973026660294,123.332515881254));
#123632=CARTESIAN_POINT('Ctrl Pts',(2.54895351809678,30.060607536818,123.335057455553));
#123633=CARTESIAN_POINT('Ctrl Pts',(2.5497623578414,30.0728837701607,123.335549675095));
#123634=CARTESIAN_POINT('Ctrl Pts',(2.55104016287578,30.0920964744503,123.33653296466));
#123635=CARTESIAN_POINT('Ctrl Pts',(2.55150424404567,30.0990375098509,123.336931779652));
#123636=CARTESIAN_POINT('Ctrl Pts',(2.55237706055531,30.1120182708224,123.337759172637));
#123637=CARTESIAN_POINT('Ctrl Pts',(2.55278522023267,30.1180584180493,123.338177245793));
#123638=CARTESIAN_POINT('Ctrl Pts',(2.55375155740589,30.1322896458728,123.339240246437));
#123639=CARTESIAN_POINT('Ctrl Pts',(2.55431121927308,30.1404783815892,123.339912855694));
#123640=CARTESIAN_POINT('Ctrl Pts',(2.55619556524564,30.1678824483649,123.342367987097));
#123641=CARTESIAN_POINT('Ctrl Pts',(2.557533788259,30.18707093269,123.344423727673));
#123642=CARTESIAN_POINT('Ctrl Pts',(2.56086488577724,30.2342676960707,123.350311042706));
#123643=CARTESIAN_POINT('Ctrl Pts',(2.56287232893253,30.2622219442267,123.354523023291));
#123644=CARTESIAN_POINT('Ctrl Pts',(2.57206819547035,30.3886012888545,123.376867161957));
#123645=CARTESIAN_POINT('Ctrl Pts',(2.57942869852923,30.485377674129,123.403134278938));
#123646=CARTESIAN_POINT('Ctrl Pts',(2.59260681628881,30.6567380705163,123.466674320744));
#123647=CARTESIAN_POINT('Ctrl Pts',(2.59845512517556,30.7320252577369,123.501155356578));
#123648=CARTESIAN_POINT('Ctrl Pts',(2.60545625046126,30.8216132380106,123.550554652936));
#123649=CARTESIAN_POINT('Ctrl Pts',(2.60678684558914,30.8386084050745,123.560320825025));
#123650=CARTESIAN_POINT('Ctrl Pts',(2.60890305469828,30.8655760375088,123.576457243498));
#123651=CARTESIAN_POINT('Ctrl Pts',(2.60969543792399,30.8756594224334,123.582637504135));
#123652=CARTESIAN_POINT('Ctrl Pts',(2.61120009286179,30.8947750738458,123.594635645858));
#123653=CARTESIAN_POINT('Ctrl Pts',(2.61191301399459,30.9038185011594,123.600434522128));
#123654=CARTESIAN_POINT('Ctrl Pts',(2.61354669239935,30.9245050753181,123.613983417353));
#123655=CARTESIAN_POINT('Ctrl Pts',(2.6144651558284,30.9361080885384,123.621793459603));
#123656=CARTESIAN_POINT('Ctrl Pts',(2.61737831692675,30.9728054088336,123.64717188037));
#123657=CARTESIAN_POINT('Ctrl Pts',(2.61935230839179,30.9975149960066,123.665287182066));
#123658=CARTESIAN_POINT('Ctrl Pts',(2.62401605168759,31.0553314988408,123.710177134437));
#123659=CARTESIAN_POINT('Ctrl Pts',(2.62668316303981,31.0879395739724,123.737559719633));
#123660=CARTESIAN_POINT('Ctrl Pts',(2.63389014695948,31.1740370188715,123.815676234277));
#123661=CARTESIAN_POINT('Ctrl Pts',(2.6383626786391,31.225265292257,123.868756865402));
#123662=CARTESIAN_POINT('Ctrl Pts',(2.6437323767735,31.2818980296044,123.935814032153));
#123663=CARTESIAN_POINT('Ctrl Pts',(2.64459517191213,31.2908479117433,123.94668808275));
#123664=CARTESIAN_POINT('Ctrl Pts',(2.64995707834337,31.3454557633846,124.014777709002));
#123665=CARTESIAN_POINT('Ctrl Pts',(2.65450878543387,31.3874339340077,124.074830530808));
#123666=CARTESIAN_POINT('Ctrl Pts',(2.66009107837441,31.4316798645555,124.14794394671));
#123667=CARTESIAN_POINT('Ctrl Pts',(2.66089940093836,31.437920239317,124.158517905049));
#123668=CARTESIAN_POINT('Ctrl Pts',(2.66217656454987,31.4475093262418,124.175184224375));
#123669=CARTESIAN_POINT('Ctrl Pts',(2.66264052940382,31.4509378877096,124.181230462884));
#123670=CARTESIAN_POINT('Ctrl Pts',(2.66351325792558,31.4572822840432,124.192583743911));
#123671=CARTESIAN_POINT('Ctrl Pts',(2.66392144742188,31.4602071498572,124.197885456556));
#123672=CARTESIAN_POINT('Ctrl Pts',(2.66488803309729,31.467034181087,124.210421458564));
#123673=CARTESIAN_POINT('Ctrl Pts',(2.66544791596296,31.4709117806914,124.217668811874));
#123674=CARTESIAN_POINT('Ctrl Pts',(2.66733380230659,31.4837220759187,124.242043574492));
#123675=CARTESIAN_POINT('Ctrl Pts',(2.66867337369049,31.4924101193453,124.259296889656));
#123676=CARTESIAN_POINT('Ctrl Pts',(2.67200858040578,31.5130845801798,124.302194703582));
#123677=CARTESIAN_POINT('Ctrl Pts',(2.67401882737852,31.5247209155569,124.328000649385));
#123678=CARTESIAN_POINT('Ctrl Pts',(2.68179150686038,31.5667759875388,124.427989187578));
#123679=CARTESIAN_POINT('Ctrl Pts',(2.68766344128463,31.5924827800888,124.504034784201));
#123680=CARTESIAN_POINT('Ctrl Pts',(2.70088063835712,31.6382248331295,124.680349949422));
#123681=CARTESIAN_POINT('Ctrl Pts',(2.70815570515403,31.6547206185765,124.78122367749));
#123682=CARTESIAN_POINT('Ctrl Pts',(2.71647465747929,31.6632548411833,124.902433088291));
#123683=CARTESIAN_POINT('Ctrl Pts',(2.71779867745289,31.6642825973897,124.921900954));
#123684=CARTESIAN_POINT('Ctrl Pts',(2.71988334606309,31.6653712535199,124.95282341065));
#123685=CARTESIAN_POINT('Ctrl Pts',(2.72065089605411,31.6656561060218,124.964267795548));
#123686=CARTESIAN_POINT('Ctrl Pts',(2.7219542101763,31.6659408291883,124.983797869167));
#123687=CARTESIAN_POINT('Ctrl Pts',(2.7224917965327,31.6659998375613,124.991882126584));
#123688=CARTESIAN_POINT('Ctrl Pts',(2.72302755883131,31.6659999996651,124.999966594594));
#123689=CARTESIAN_POINT('Ctrl Pts',(2.72302754719672,31.6659999996616,124.999966419032));
#123690=CARTESIAN_POINT('Ctrl Pts',(2.72339558096022,31.6660001116015,125.005519921113));
#123691=CARTESIAN_POINT('Ctrl Pts',(2.72376274997295,31.6659724551936,125.011073458905));
#123692=CARTESIAN_POINT('Ctrl Pts',(2.72472346752639,31.6658270924562,125.025638010347));
#123693=CARTESIAN_POINT('Ctrl Pts',(2.72531560230014,31.6656640414659,125.034648460313));
#123694=CARTESIAN_POINT('Ctrl Pts',(2.7272324465681,31.6648967006198,125.063920793919));
#123695=CARTESIAN_POINT('Ctrl Pts',(2.72854800141681,31.6639957203849,125.084173578587));
#123696=CARTESIAN_POINT('Ctrl Pts',(2.73600252008977,31.6567396460939,125.199731153278));
#123697=CARTESIAN_POINT('Ctrl Pts',(2.74189284273147,31.6425675085602,125.294370330194));
#123698=CARTESIAN_POINT('Ctrl Pts',(2.75174615151661,31.605106952336,125.451102252216));
#123699=CARTESIAN_POINT('Ctrl Pts',(2.75572966382173,31.5860991325912,125.51395344143));
#123700=CARTESIAN_POINT('Ctrl Pts',(2.75979332369797,31.5634400150579,125.575509617049));
#123701=CARTESIAN_POINT('Ctrl Pts',(2.56904933390813,31.5634400118358,125.575509625802));
#123702=CARTESIAN_POINT('Ctrl Pts',(2.56750768440673,31.5719229943011,125.552464599948));
#123703=CARTESIAN_POINT('Ctrl Pts',(2.56595051571147,31.5798953096122,125.529235120265));
#123704=CARTESIAN_POINT('Ctrl Pts',(2.56303659776313,31.5936510056218,125.486068913008));
#123705=CARTESIAN_POINT('Ctrl Pts',(2.56168650874348,31.5995806545989,125.466184673763));
#123706=CARTESIAN_POINT('Ctrl Pts',(2.55975881801057,31.6074002625116,125.438054564161));
#123707=CARTESIAN_POINT('Ctrl Pts',(2.55919766684648,31.6096013883969,125.429896229335));
#123708=CARTESIAN_POINT('Ctrl Pts',(2.55822633255545,31.6132807220529,125.4158345151));
#123709=CARTESIAN_POINT('Ctrl Pts',(2.55781784972441,31.6147888095325,125.409939180308));
#123710=CARTESIAN_POINT('Ctrl Pts',(2.55694707943159,31.6179200985488,125.397413075285));
#123711=CARTESIAN_POINT('Ctrl Pts',(2.5564843681348,31.619534834569,125.390780645791));
#123712=CARTESIAN_POINT('Ctrl Pts',(2.55519954180064,31.6238845656322,125.372424285793));
#123713=CARTESIAN_POINT('Ctrl Pts',(2.55437284706231,31.62653324698,125.360680615845));
#123714=CARTESIAN_POINT('Ctrl Pts',(2.54965622493531,31.6408145640836,125.294001354521));
#123715=CARTESIAN_POINT('Ctrl Pts',(2.54564696591654,31.6497900057805,125.238538991999));
#123716=CARTESIAN_POINT('Ctrl Pts',(2.53092411806609,31.6721389246965,125.036013588231));
#123717=CARTESIAN_POINT('Ctrl Pts',(2.52006485417299,31.6687604919269,124.887755290083));
#123718=CARTESIAN_POINT('Ctrl Pts',(2.50765667614603,31.6410743164775,124.711219905917));
#123719=CARTESIAN_POINT('Ctrl Pts',(2.50552745157347,31.6354108782717,124.680703372049));
#123720=CARTESIAN_POINT('Ctrl Pts',(2.50247286587228,31.625948858238,124.636621718354));
#123721=CARTESIAN_POINT('Ctrl Pts',(2.50152638550819,31.6228259662935,124.622919943099));
#123722=CARTESIAN_POINT('Ctrl Pts',(2.49986576324301,31.6170091144835,124.598810456889));
#123723=CARTESIAN_POINT('Ctrl Pts',(2.49914936313765,31.6143871225168,124.588386402332));
#123724=CARTESIAN_POINT('Ctrl Pts',(2.49765408285465,31.6086784916746,124.566585121346));
#123725=CARTESIAN_POINT('Ctrl Pts',(2.49687589991155,31.6055716032335,124.555213775471));
#123726=CARTESIAN_POINT('Ctrl Pts',(2.49482520500147,31.5970248560212,124.525189408577));
#123727=CARTESIAN_POINT('Ctrl Pts',(2.49355941074421,31.5913788398077,124.506596586992));
#123728=CARTESIAN_POINT('Ctrl Pts',(2.48725774246659,31.5614258265708,124.413827811878));
#123729=CARTESIAN_POINT('Ctrl Pts',(2.48238388449402,31.5322511863651,124.341321819731));
#123730=CARTESIAN_POINT('Ctrl Pts',(2.47117051387643,31.4525132725897,124.177432953324));
#123731=CARTESIAN_POINT('Ctrl Pts',(2.46491618176057,31.398245417011,124.08823322209));
#123732=CARTESIAN_POINT('Ctrl Pts',(2.45571450168454,31.3104986927239,123.970450451187));
#123733=CARTESIAN_POINT('Ctrl Pts',(2.4529952182635,31.2836854524679,123.937206475624));
#123734=CARTESIAN_POINT('Ctrl Pts',(2.44948437292046,31.2484924018074,123.896849697564));
#123735=CARTESIAN_POINT('Ctrl Pts',(2.4487674654407,31.2412773500014,123.888737478313));
#123736=CARTESIAN_POINT('Ctrl Pts',(2.44760762717081,31.2295700819844,123.875830719551));
#123737=CARTESIAN_POINT('Ctrl Pts',(2.44716829910654,31.2251277480399,123.870991074058));
#123738=CARTESIAN_POINT('Ctrl Pts',(2.44631517630151,31.2164892592834,123.861690997691));
#123739=CARTESIAN_POINT('Ctrl Pts',(2.4459016611756,31.2122969525896,123.857227233143));
#123740=CARTESIAN_POINT('Ctrl Pts',(2.44497164910762,31.2028548791652,123.847284196805));
#123741=CARTESIAN_POINT('Ctrl Pts',(2.44445418919199,31.1975920966534,123.841817480805));
#123742=CARTESIAN_POINT('Ctrl Pts',(2.44261357240089,31.1788336112256,123.822596658982));
#123743=CARTESIAN_POINT('Ctrl Pts',(2.44127656029826,31.165137397526,123.809041530215));
#123744=CARTESIAN_POINT('Ctrl Pts',(2.43236282805903,31.0731820713852,123.721137917035));
#123745=CARTESIAN_POINT('Ctrl Pts',(2.42442760407517,30.9880948382047,123.654312788474));
#123746=CARTESIAN_POINT('Ctrl Pts',(2.41039467056622,30.8251416040873,123.550172440081));
#123747=CARTESIAN_POINT('Ctrl Pts',(2.40427516634134,30.7496928316227,123.509757438197));
#123748=CARTESIAN_POINT('Ctrl Pts',(2.39626880572495,30.644045787585,123.46323107403));
#123749=CARTESIAN_POINT('Ctrl Pts',(2.39421461651924,30.6163031175517,123.451896522758));
#123750=CARTESIAN_POINT('Ctrl Pts',(2.39124631007734,30.5752955991356,123.436419738837));
#123751=CARTESIAN_POINT('Ctrl Pts',(2.39031271834411,30.5622620535688,123.43168572576));
#123752=CARTESIAN_POINT('Ctrl Pts',(2.38866661466185,30.539045255487,123.423579614265));
#123753=CARTESIAN_POINT('Ctrl Pts',(2.38795197572336,30.5288858375409,123.420142158257));
#123754=CARTESIAN_POINT('Ctrl Pts',(2.38645240894849,30.5074027180524,123.413103767499));
#123755=CARTESIAN_POINT('Ctrl Pts',(2.38566825521845,30.4960722215795,123.40952537452));
#123756=CARTESIAN_POINT('Ctrl Pts',(2.38358303030669,30.4656924247426,123.400287077126));
#123757=CARTESIAN_POINT('Ctrl Pts',(2.38228909880272,30.4465781508587,123.394846150684));
#123758=CARTESIAN_POINT('Ctrl Pts',(2.37459420560437,30.3314461354506,123.364289425666));
#123759=CARTESIAN_POINT('Ctrl Pts',(2.36846900019063,30.2334337937581,123.347451100979));
#123760=CARTESIAN_POINT('Ctrl Pts',(2.35712166498238,30.0484735090973,123.332470549024));
#123761=CARTESIAN_POINT('Ctrl Pts',(2.35189847504009,29.9620469648778,123.332198513648));
#123762=CARTESIAN_POINT('Ctrl Pts',(2.34401577394342,29.8370031962186,123.341531774075));
#123763=CARTESIAN_POINT('Ctrl Pts',(2.34151788091398,29.7981295065047,123.345813620046));
#123764=CARTESIAN_POINT('Ctrl Pts',(2.33825905284894,29.748983465588,123.352984974295));
#123765=CARTESIAN_POINT('Ctrl Pts',(2.3375604506864,29.7385360336302,123.354611178036));
#123766=CARTESIAN_POINT('Ctrl Pts',(2.33642315192652,29.7216848517864,123.357398701416));
#123767=CARTESIAN_POINT('Ctrl Pts',(2.33598781240839,29.7152709951856,123.358498328358));
#123768=CARTESIAN_POINT('Ctrl Pts',(2.33513609963773,29.7027977306627,123.360712115441));
#123769=CARTESIAN_POINT('Ctrl Pts',(2.33471994490285,29.6967377882096,123.361822358923));
#123770=CARTESIAN_POINT('Ctrl Pts',(2.33367560794991,29.6816132159569,123.364680129679));
#123771=CARTESIAN_POINT('Ctrl Pts',(2.3330451577626,29.6725567810803,123.366469421453));
#123772=CARTESIAN_POINT('Ctrl Pts',(2.33074381425698,29.6397485077054,123.373235180857));
#123773=CARTESIAN_POINT('Ctrl Pts',(2.32905120321328,29.6160924583892,123.378654951812));
#123774=CARTESIAN_POINT('Ctrl Pts',(2.32004493578621,29.4922764882314,123.409883530933));
#123775=CARTESIAN_POINT('Ctrl Pts',(2.31244298822751,29.3945667624941,123.444460727571));
#123776=CARTESIAN_POINT('Ctrl Pts',(2.29890959143051,29.2251886175557,123.522791682623));
#123777=CARTESIAN_POINT('Ctrl Pts',(2.29295775707005,29.1523924535725,123.563322617609));
#123778=CARTESIAN_POINT('Ctrl Pts',(2.28511457005254,29.0579737618701,123.62557811282));
#123779=CARTESIAN_POINT('Ctrl Pts',(2.28306595474137,29.033472041509,123.642696473962));
#123780=CARTESIAN_POINT('Ctrl Pts',(2.28010407320749,28.9983052906521,123.668701543796));
#123781=CARTESIAN_POINT('Ctrl Pts',(2.27917145221545,28.9872707862423,123.677076181351));
#123782=CARTESIAN_POINT('Ctrl Pts',(2.27752643649752,28.9678816254554,123.692176370919));
#123783=CARTESIAN_POINT('Ctrl Pts',(2.2768119246418,28.9594851772492,123.698846705138));
#123784=CARTESIAN_POINT('Ctrl Pts',(2.27531200665376,28.9419163829581,123.71308259512));
#123785=CARTESIAN_POINT('Ctrl Pts',(2.27452738061961,28.932759411369,123.720666233565));
#123786=CARTESIAN_POINT('Ctrl Pts',(2.27243942412201,28.9084897629472,123.741207854997));
#123787=CARTESIAN_POINT('Ctrl Pts',(2.27114326715865,28.8935265417639,123.754340013031));
#123788=CARTESIAN_POINT('Ctrl Pts',(2.2637871406152,28.8092949159083,123.830979824061));
#123789=CARTESIAN_POINT('Ctrl Pts',(2.25797112631215,28.7452592899401,123.899992839493));
#123790=CARTESIAN_POINT('Ctrl Pts',(2.24787115203191,28.6436509421557,124.029992093533));
#123791=CARTESIAN_POINT('Ctrl Pts',(2.24356696978252,28.6035459355214,124.088674833431));
#123792=CARTESIAN_POINT('Ctrl Pts',(2.23676400379598,28.5474935141545,124.183122848311));
#123793=CARTESIAN_POINT('Ctrl Pts',(2.23433250431504,28.5288531415018,124.217191017946));
#123794=CARTESIAN_POINT('Ctrl Pts',(2.23030294485382,28.5005759158235,124.273455658855));
#123795=CARTESIAN_POINT('Ctrl Pts',(2.22873760062581,28.4902020608207,124.295266503208));
#123796=CARTESIAN_POINT('Ctrl Pts',(2.22655564749562,28.4766373461281,124.325461344167));
#123797=CARTESIAN_POINT('Ctrl Pts',(2.225961842205,28.4730341304597,124.333658197502));
#123798=CARTESIAN_POINT('Ctrl Pts',(2.22495222010856,28.4670600209088,124.34755146802));
#123799=CARTESIAN_POINT('Ctrl Pts',(2.22453846530128,28.4646543164811,124.353232887994));
#123800=CARTESIAN_POINT('Ctrl Pts',(2.22367688566946,28.4597339908895,124.365035113364));
#123801=CARTESIAN_POINT('Ctrl Pts',(2.22322880898844,28.4572242117579,124.371157691105));
#123802=CARTESIAN_POINT('Ctrl Pts',(2.22202522766242,28.4506115663153,124.387567037897));
#123803=CARTESIAN_POINT('Ctrl Pts',(2.22126601736054,28.4465747724071,124.397879831561));
#123804=CARTESIAN_POINT('Ctrl Pts',(2.21769862511443,28.4282157522584,124.446195335171));
#123805=CARTESIAN_POINT('Ctrl Pts',(2.2148279607198,28.4151844929541,124.484670447427));
#123806=CARTESIAN_POINT('Ctrl Pts',(2.20540719597188,28.3775671166334,124.61072168151));
#123807=CARTESIAN_POINT('Ctrl Pts',(2.19873109221899,28.3587404135626,124.699845296651));
#123808=CARTESIAN_POINT('Ctrl Pts',(2.18768018724387,28.339495724135,124.851345490244));
#123809=CARTESIAN_POINT('Ctrl Pts',(2.18325963961434,28.3351249939939,124.913022177084));
#123810=CARTESIAN_POINT('Ctrl Pts',(2.17615245495413,28.3335905372008,125.014473291492));
#123811=CARTESIAN_POINT('Ctrl Pts',(2.17341311675692,28.3344076633956,125.054153481255));
#123812=CARTESIAN_POINT('Ctrl Pts',(2.16967082987506,28.3375077988401,125.109146075771));
#123813=CARTESIAN_POINT('Ctrl Pts',(2.16863111864284,28.338587818163,125.124510138092));
#123814=CARTESIAN_POINT('Ctrl Pts',(2.16686260137528,28.3408012169422,125.150783355902));
#123815=CARTESIAN_POINT('Ctrl Pts',(2.16613056069923,28.3418295296182,125.161700102593));
#123816=CARTESIAN_POINT('Ctrl Pts',(2.16473917933094,28.3439987313666,125.182524635184));
#123817=CARTESIAN_POINT('Ctrl Pts',(2.16407928631761,28.345120950561,125.19243384115));
#123818=CARTESIAN_POINT('Ctrl Pts',(2.1625361847491,28.3479649431131,125.215677847066));
#123819=CARTESIAN_POINT('Ctrl Pts',(2.16165528268827,28.3497593147327,125.22900318993));
#123820=CARTESIAN_POINT('Ctrl Pts',(2.15857813177452,28.3566280414943,125.275727725687));
#123821=CARTESIAN_POINT('Ctrl Pts',(2.15640851826147,28.3625568781979,125.308994244319));
#123822=CARTESIAN_POINT('Ctrl Pts',(2.14465579092078,28.4005873918265,125.490275631819));
#123823=CARTESIAN_POINT('Ctrl Pts',(2.1357002042975,28.4517410493955,125.633547186988));
#123824=CARTESIAN_POINT('Ctrl Pts',(2.12421330619666,28.5366927651692,125.797099847025));
#123825=CARTESIAN_POINT('Ctrl Pts',(2.12214143477398,28.5527014418604,125.825810420963));
#123826=CARTESIAN_POINT('Ctrl Pts',(2.11864881717407,28.5805707774142,125.872490161107));
#123827=CARTESIAN_POINT('Ctrl Pts',(2.11725087847344,28.5919497196416,125.890737167683));
#123828=CARTESIAN_POINT('Ctrl Pts',(2.11526640810246,28.6083512703442,125.915938434034));
#123829=CARTESIAN_POINT('Ctrl Pts',(2.11469765099059,28.6130797928288,125.923082733429));
#123830=CARTESIAN_POINT('Ctrl Pts',(2.11371751494314,28.62127083578,125.935253518153));
#123831=CARTESIAN_POINT('Ctrl Pts',(2.11330791156008,28.6247063311271,125.940298130768));
#123832=CARTESIAN_POINT('Ctrl Pts',(2.11243980955811,28.6320117988284,125.950899645255));
#123833=CARTESIAN_POINT('Ctrl Pts',(2.11198092285726,28.6358879942933,125.956451925442));
#123834=CARTESIAN_POINT('Ctrl Pts',(2.11071744974352,28.6466027983288,125.971602235303));
#123835=CARTESIAN_POINT('Ctrl Pts',(2.10990852067194,28.6535094207371,125.981151359045));
#123836=CARTESIAN_POINT('Ctrl Pts',(2.10550818269214,28.6913585325467,126.032329358542));
#123837=CARTESIAN_POINT('Ctrl Pts',(2.10181469510058,28.7241283320169,126.072565518666));
#123838=CARTESIAN_POINT('Ctrl Pts',(2.09095331498943,28.8245942356333,126.18479209712));
#123839=CARTESIAN_POINT('Ctrl Pts',(2.08369699422513,28.8968890502394,126.252381214588));
#123840=CARTESIAN_POINT('Ctrl Pts',(2.073074585622,29.0135313207396,126.343449647559));
#123841=CARTESIAN_POINT('Ctrl Pts',(2.0695856132006,29.0536429993486,126.372000939735));
#123842=CARTESIAN_POINT('Ctrl Pts',(2.06379048581444,29.1234919579681,126.417195925477));
#123843=CARTESIAN_POINT('Ctrl Pts',(2.06145360046727,29.1525805068665,126.434779123136));
#123844=CARTESIAN_POINT('Ctrl Pts',(2.05816225498934,29.1948592769611,126.458600676972));
#123845=CARTESIAN_POINT('Ctrl Pts',(2.05718180413031,29.2076233811371,126.465573893032));
#123846=CARTESIAN_POINT('Ctrl Pts',(2.05548236302441,29.2300392874922,126.477441557332));
#123847=CARTESIAN_POINT('Ctrl Pts',(2.05476076510907,29.2396503269645,126.482410684783));
#123848=CARTESIAN_POINT('Ctrl Pts',(2.05327389914097,29.2596433464019,126.492501934617));
#123849=CARTESIAN_POINT('Ctrl Pts',(2.05250914598858,29.2700316987983,126.497610192945));
#123850=CARTESIAN_POINT('Ctrl Pts',(2.05053630372098,29.2970966500618,126.51057029147));
#123851=CARTESIAN_POINT('Ctrl Pts',(2.04933401803458,29.3138520959994,126.518254531589));
#123852=CARTESIAN_POINT('Ctrl Pts',(2.04405306145618,29.3885465246893,126.551021070744));
#123853=CARTESIAN_POINT('Ctrl Pts',(2.04007641786547,29.4477595579309,126.573077726668));
#123854=CARTESIAN_POINT('Ctrl Pts',(2.02715479675985,29.6469140094264,126.634625291418));
#123855=CARTESIAN_POINT('Ctrl Pts',(2.01857863180699,29.7907363503682,126.659176908244));
#123856=CARTESIAN_POINT('Ctrl Pts',(2.00779634488768,29.9588105245502,126.66564857244));
#123857=CARTESIAN_POINT('Ctrl Pts',(2.00630817305725,29.9817369738419,126.666057644819));
#123858=CARTESIAN_POINT('Ctrl Pts',(2.00421704216577,30.013443408266,126.665968897727));
#123859=CARTESIAN_POINT('Ctrl Pts',(2.00363449149764,30.0222230877966,126.665874911073));
#123860=CARTESIAN_POINT('Ctrl Pts',(2.00263820106578,30.0371390944546,126.665597301974));
#123861=CARTESIAN_POINT('Ctrl Pts',(2.00222639368994,30.0432760482853,126.665449148775));
#123862=CARTESIAN_POINT('Ctrl Pts',(2.0013622704175,30.0560911705319,126.665068896678));
#123863=CARTESIAN_POINT('Ctrl Pts',(2.00090964418383,30.0627689041207,126.664830535167));
#123864=CARTESIAN_POINT('Ctrl Pts',(1.99968092741465,30.0808077533322,126.664077956934));
#123865=CARTESIAN_POINT('Ctrl Pts',(1.99890086883427,30.0921650928268,126.663487576623));
#123866=CARTESIAN_POINT('Ctrl Pts',(1.99502521720697,30.1481709589136,126.660000976265));
#123867=CARTESIAN_POINT('Ctrl Pts',(1.99185368136524,30.1926926728845,126.655423406051));
#123868=CARTESIAN_POINT('Ctrl Pts',(1.98231906174619,30.3241066326442,126.636539083468));
#123869=CARTESIAN_POINT('Ctrl Pts',(1.97585958504778,30.410111074259,126.61713147611));
#123870=CARTESIAN_POINT('Ctrl Pts',(1.96510770015513,30.5520915004783,126.573031583146));
#123871=CARTESIAN_POINT('Ctrl Pts',(1.9607718416773,30.6089829306542,126.551893821281));
#123872=CARTESIAN_POINT('Ctrl Pts',(1.95378127910273,30.7005374787702,126.512064543252));
#123873=CARTESIAN_POINT('Ctrl Pts',(1.95107611390662,30.7359146575836,126.495166211577));
#123874=CARTESIAN_POINT('Ctrl Pts',(1.94737173507689,30.7842589981586,126.469941805635));
#123875=CARTESIAN_POINT('Ctrl Pts',(1.94633674152783,30.7977543074398,126.462661676674));
#123876=CARTESIAN_POINT('Ctrl Pts',(1.94457376980897,30.8207140226308,126.449863595264));
#123877=CARTESIAN_POINT('Ctrl Pts',(1.94384260786403,30.8302278284621,126.444436815694));
#123878=CARTESIAN_POINT('Ctrl Pts',(1.94245127042418,30.8483118999807,126.433883756422));
#123879=CARTESIAN_POINT('Ctrl Pts',(1.94179055761511,30.8568909075131,126.428773490291));
#123880=CARTESIAN_POINT('Ctrl Pts',(1.94024309949947,30.8769590042724,126.416573734841));
#123881=CARTESIAN_POINT('Ctrl Pts',(1.93935869460053,30.8884090038081,126.409421051704));
#123882=CARTESIAN_POINT('Ctrl Pts',(1.93625622460555,30.9284877438922,126.383701827216));
#123883=CARTESIAN_POINT('Ctrl Pts',(1.93406539022289,30.9566329224646,126.364395083296));
#123884=CARTESIAN_POINT('Ctrl Pts',(1.92328624366364,31.0937548245079,126.264002893837));
#123885=CARTESIAN_POINT('Ctrl Pts',(1.91518068298333,31.1931157191803,126.170674153587));
#123886=CARTESIAN_POINT('Ctrl Pts',(1.90417378267724,31.3072035363218,126.033719077966));
#123887=CARTESIAN_POINT('Ctrl Pts',(1.90152611468047,31.3331030636473,126.00009597486));
#123888=CARTESIAN_POINT('Ctrl Pts',(1.89717927392726,31.3725533538331,125.94462219776));
#123889=CARTESIAN_POINT('Ctrl Pts',(1.89551959231258,31.3869317882335,125.923381746079));
#123890=CARTESIAN_POINT('Ctrl Pts',(1.89322707557086,31.4057697631156,125.894120357556));
#123891=CARTESIAN_POINT('Ctrl Pts',(1.89262015135067,31.4106625312169,125.886380874228));
#123892=CARTESIAN_POINT('Ctrl Pts',(1.89159484689329,31.418765014924,125.873327184444));
#123893=CARTESIAN_POINT('Ctrl Pts',(1.89117868182008,31.4220093648947,125.868034505788));
#123894=CARTESIAN_POINT('Ctrl Pts',(1.89031938970207,31.4286154701201,125.857121187626));
#123895=CARTESIAN_POINT('Ctrl Pts',(1.88987607418007,31.4319737667784,125.851498690118));
#123896=CARTESIAN_POINT('Ctrl Pts',(1.88869872797906,31.4407638003234,125.836583250243));
#123897=CARTESIAN_POINT('Ctrl Pts',(1.88796125805969,31.4461386692578,125.827257394608));
#123898=CARTESIAN_POINT('Ctrl Pts',(1.88464135417116,31.4697693782988,125.785321991227));
#123899=CARTESIAN_POINT('Ctrl Pts',(1.88200603188418,31.4870139095433,125.752158103781));
#123900=CARTESIAN_POINT('Ctrl Pts',(1.87563875356216,31.5254502461663,125.671741835603));
#123901=CARTESIAN_POINT('Ctrl Pts',(1.87188086914729,31.5455741574153,125.624044319361));
#123902=CARTESIAN_POINT('Ctrl Pts',(1.86811695019056,31.5634399562749,125.57550977674));
#123903=CARTESIAN_POINT('Origin',(5.,30.,125.));
#123904=CARTESIAN_POINT('',(1.16625576032278,31.5634400119388,125.575509625522));
#123905=CARTESIAN_POINT('',(1.36115613275098,31.5634400145948,125.575509618307));
#123906=CARTESIAN_POINT('',(5.,31.5634400119422,125.575509625513));
#123907=CARTESIAN_POINT('Ctrl Pts',(1.36115613275098,31.5634400145948,125.575509618307));
#123908=CARTESIAN_POINT('Ctrl Pts',(1.36788843714252,31.5313390004694,125.662715823723));
#123909=CARTESIAN_POINT('Ctrl Pts',(1.37450631330542,31.4919908242762,125.747102957969));
#123910=CARTESIAN_POINT('Ctrl Pts',(1.38236650476969,31.4350852948616,125.846493320159));
#123911=CARTESIAN_POINT('Ctrl Pts',(1.3838332531891,31.4240112791323,125.864992888475));
#123912=CARTESIAN_POINT('Ctrl Pts',(1.38611237940914,31.4060915723659,125.893651108808));
#123913=CARTESIAN_POINT('Ctrl Pts',(1.38693348118945,31.3994879769824,125.903957537879));
#123914=CARTESIAN_POINT('Ctrl Pts',(1.38846254431071,31.3869157521616,125.923111350145));
#123915=CARTESIAN_POINT('Ctrl Pts',(1.38917147738888,31.3809745757465,125.931975910933));
#123916=CARTESIAN_POINT('Ctrl Pts',(1.39075633862594,31.3674425867808,125.951752829778));
#123917=CARTESIAN_POINT('Ctrl Pts',(1.391630461375,31.3598054665056,125.962632737567));
#123918=CARTESIAN_POINT('Ctrl Pts',(1.39386577366159,31.3398351135063,125.99037069423));
#123919=CARTESIAN_POINT('Ctrl Pts',(1.39521970951885,31.3273133741414,126.007090617742));
#123920=CARTESIAN_POINT('Ctrl Pts',(1.40488805332882,31.2349239505862,126.125738004368));
#123921=CARTESIAN_POINT('Ctrl Pts',(1.41271276384103,31.1437288724805,126.21828206136));
#123922=CARTESIAN_POINT('Ctrl Pts',(1.42572400376261,30.9779077990288,126.351354860294));
#123923=CARTESIAN_POINT('Ctrl Pts',(1.43084613520645,30.909293792728,126.398443729326));
#123924=CARTESIAN_POINT('Ctrl Pts',(1.43717053171415,30.8252969675018,126.447286775893));
#123925=CARTESIAN_POINT('Ctrl Pts',(1.43809467192393,30.8130411236341,126.454207067591));
#123926=CARTESIAN_POINT('Ctrl Pts',(1.43950924853964,30.7943386632721,126.464457135803));
#123927=CARTESIAN_POINT('Ctrl Pts',(1.43999282229543,30.7879551971601,126.467901637342));
#123928=CARTESIAN_POINT('Ctrl Pts',(1.44088202979343,30.7762402861211,126.474124540496));
#123929=CARTESIAN_POINT('Ctrl Pts',(1.44128684763122,30.7709160307832,126.476915912445));
#123930=CARTESIAN_POINT('Ctrl Pts',(1.44221892605108,30.7586774434982,126.483248084509));
#123931=CARTESIAN_POINT('Ctrl Pts',(1.44274734184737,30.7517533934417,126.486769374479));
#123932=CARTESIAN_POINT('Ctrl Pts',(1.44438271947967,30.7303605083595,126.497461282664));
#123933=CARTESIAN_POINT('Ctrl Pts',(1.44549870813941,30.715812324722,126.504469817929));
#123934=CARTESIAN_POINT('Ctrl Pts',(1.45226606876418,30.6277635487778,126.545320842738));
#123935=CARTESIAN_POINT('Ctrl Pts',(1.45813955116446,30.5519850555145,126.573980181122));
#123936=CARTESIAN_POINT('Ctrl Pts',(1.46939071625332,30.4038000201976,126.618002116637));
#123937=CARTESIAN_POINT('Ctrl Pts',(1.47475405342166,30.3318483728441,126.634277599297));
#123938=CARTESIAN_POINT('Ctrl Pts',(1.4830506607513,30.2170086743266,126.652354282216));
#123939=CARTESIAN_POINT('Ctrl Pts',(1.48605154938794,30.1747245185688,126.657359129859));
#123940=CARTESIAN_POINT('Ctrl Pts',(1.49113204457282,30.1017581020467,126.663171525842));
#123941=CARTESIAN_POINT('Ctrl Pts',(1.49323321385457,30.0711613095641,126.664761399673));
#123942=CARTESIAN_POINT('Ctrl Pts',(1.49625576184964,30.0265547467054,126.665847064912));
#123943=CARTESIAN_POINT('Ctrl Pts',(1.49719763550133,30.0125691555328,126.666011295067));
#123944=CARTESIAN_POINT('Ctrl Pts',(1.49885323880198,29.9878403260271,126.665990258866));
#123945=CARTESIAN_POINT('Ctrl Pts',(1.49956917801096,29.9770980059061,126.665877218845));
#123946=CARTESIAN_POINT('Ctrl Pts',(1.50106648449706,29.9545335804967,126.665421466873));
#123947=CARTESIAN_POINT('Ctrl Pts',(1.50184712531767,29.9427124800443,126.665056758738));
#123948=CARTESIAN_POINT('Ctrl Pts',(1.50391128077752,29.911313423008,126.66375323574));
#123949=CARTESIAN_POINT('Ctrl Pts',(1.5051879178707,29.8917460785984,126.662594743005));
#123950=CARTESIAN_POINT('Ctrl Pts',(1.51177375811627,29.7901391093795,126.654777555307));
#123951=CARTESIAN_POINT('Ctrl Pts',(1.51690091992469,29.7086505813626,126.64239104304));
#123952=CARTESIAN_POINT('Ctrl Pts',(1.52812422821807,29.5305361858221,126.601636379029));
#123953=CARTESIAN_POINT('Ctrl Pts',(1.53416048059969,29.434900417567,126.57044435649));
#123954=CARTESIAN_POINT('Ctrl Pts',(1.54222801375701,29.316650531387,126.519667973499));
#123955=CARTESIAN_POINT('Ctrl Pts',(1.54402243346827,29.2909310511884,126.507838947316));
#123956=CARTESIAN_POINT('Ctrl Pts',(1.54709236254215,29.2481880080668,126.486844945667));
#123957=CARTESIAN_POINT('Ctrl Pts',(1.54835151398663,29.2309994718478,126.478028170672));
#123958=CARTESIAN_POINT('Ctrl Pts',(1.5501709467685,29.2067217280122,126.465036909522));
#123959=CARTESIAN_POINT('Ctrl Pts',(1.55071715664052,29.1995034137108,126.461105325225));
#123960=CARTESIAN_POINT('Ctrl Pts',(1.55167155573971,29.1870186995625,126.454185019206));
#123961=CARTESIAN_POINT('Ctrl Pts',(1.55207821373416,29.1817390213714,126.451220739397));
#123962=CARTESIAN_POINT('Ctrl Pts',(1.55295575010206,29.1704333208859,126.44479183181));
#123963=CARTESIAN_POINT('Ctrl Pts',(1.55342715409083,29.1644128762686,126.441318308567));
#123964=CARTESIAN_POINT('Ctrl Pts',(1.55473753527695,29.1478183259475,126.43160509228));
#123965=CARTESIAN_POINT('Ctrl Pts',(1.55558125975455,29.137291439999,126.425286169237));
#123966=CARTESIAN_POINT('Ctrl Pts',(1.56149195184508,29.0645717552314,126.38053432621));
#123967=CARTESIAN_POINT('Ctrl Pts',(1.5667606305462,29.0049041505482,126.338164006801));
#123968=CARTESIAN_POINT('Ctrl Pts',(1.57310152214887,28.9372147896413,126.283060763051));
#123969=CARTESIAN_POINT('Ctrl Pts',(1.57413377338813,28.9263259284823,126.273962836714));
#123970=CARTESIAN_POINT('Ctrl Pts',(1.5805297536356,28.8596145021991,126.216760850669));
#123971=CARTESIAN_POINT('Ctrl Pts',(1.5858934328867,28.8069148305002,126.165133099205));
#123972=CARTESIAN_POINT('Ctrl Pts',(1.59418949790209,28.7294503436004,126.078457249508));
#123973=CARTESIAN_POINT('Ctrl Pts',(1.59718955248034,28.7023203053945,126.045655001549));
#123974=CARTESIAN_POINT('Ctrl Pts',(1.60226880889453,28.6578742134838,125.987518224455));
#123975=CARTESIAN_POINT('Ctrl Pts',(1.60436955922799,28.6399476634801,125.962679451522));
#123976=CARTESIAN_POINT('Ctrl Pts',(1.60739162529151,28.614846714531,125.92579800432));
#123977=CARTESIAN_POINT('Ctrl Pts',(1.60833342676447,28.6071240905643,125.914138004172));
#123978=CARTESIAN_POINT('Ctrl Pts',(1.60998894819264,28.59373046158,125.893351768683));
#123979=CARTESIAN_POINT('Ctrl Pts',(1.61070487697827,28.5879992936424,125.884265464572));
#123980=CARTESIAN_POINT('Ctrl Pts',(1.61220220555134,28.5761439384451,125.865060567569));
#123981=CARTESIAN_POINT('Ctrl Pts',(1.61298287846048,28.5700387876429,125.854930881935));
#123982=CARTESIAN_POINT('Ctrl Pts',(1.61504722145929,28.5541028643732,125.827841594732));
#123983=CARTESIAN_POINT('Ctrl Pts',(1.61632401170468,28.5444624732624,125.810771727214));
#123984=CARTESIAN_POINT('Ctrl Pts',(1.62291504384544,28.495884428535,125.721096107323));
#123985=CARTESIAN_POINT('Ctrl Pts',(1.62804686221697,28.4620681710365,125.645841632242));
#123986=CARTESIAN_POINT('Ctrl Pts',(1.63927045501971,28.3997275171634,125.474077605111));
#123987=CARTESIAN_POINT('Ctrl Pts',(1.64530276138104,28.3740900755344,125.376876857683));
#123988=CARTESIAN_POINT('Ctrl Pts',(1.6533655489414,28.3526313051633,125.250066271206));
#123989=CARTESIAN_POINT('Ctrl Pts',(1.65515944087159,28.3486218171002,125.222051059855));
#123990=CARTESIAN_POINT('Ctrl Pts',(1.65822855801079,28.343079531499,125.17476715656));
#123991=CARTESIAN_POINT('Ctrl Pts',(1.65948743656081,28.3411650080246,125.155548671883));
#123992=CARTESIAN_POINT('Ctrl Pts',(1.66130654328476,28.3389126581761,125.128110866713));
#123993=CARTESIAN_POINT('Ctrl Pts',(1.66185270685914,28.338300874547,125.11991480642));
#123994=CARTESIAN_POINT('Ctrl Pts',(1.66280705396003,28.337343748033,125.105673325348));
#123995=CARTESIAN_POINT('Ctrl Pts',(1.66321370677633,28.3369706783309,125.099630004616));
#123996=CARTESIAN_POINT('Ctrl Pts',(1.66409126664441,28.3362400844329,125.086644454505));
#123997=CARTESIAN_POINT('Ctrl Pts',(1.66456269964768,28.3358930649802,125.079702086268));
#123998=CARTESIAN_POINT('Ctrl Pts',(1.66587323662131,28.3350532264047,125.060489932643));
#123999=CARTESIAN_POINT('Ctrl Pts',(1.66671708960978,28.3346526174751,125.04821684611));
#124000=CARTESIAN_POINT('Ctrl Pts',(1.67266204871686,28.3327998838993,124.962355479993));
#124001=CARTESIAN_POINT('Ctrl Pts',(1.67796757987229,28.3360904001255,124.888753519978));
#124002=CARTESIAN_POINT('Ctrl Pts',(1.68431842629328,28.3457643669062,124.801879876537));
#124003=CARTESIAN_POINT('Ctrl Pts',(1.68532418592172,28.3474652940615,124.788160071502));
#124004=CARTESIAN_POINT('Ctrl Pts',(1.69169632094496,28.3593174067707,124.701416633705));
#124005=CARTESIAN_POINT('Ctrl Pts',(1.69706240822283,28.374136446682,124.629108613771));
#124006=CARTESIAN_POINT('Ctrl Pts',(1.70535358077061,28.4049610309634,124.517082680831));
#124007=CARTESIAN_POINT('Ctrl Pts',(1.70834673343382,28.417785537069,124.476591608923));
#124008=CARTESIAN_POINT('Ctrl Pts',(1.71341573792905,28.4424832714218,124.407857711538));
#124009=CARTESIAN_POINT('Ctrl Pts',(1.7155130202741,28.4536131983008,124.379372154915));
#124010=CARTESIAN_POINT('Ctrl Pts',(1.71853110124874,28.4709642368116,124.338334704028));
#124011=CARTESIAN_POINT('Ctrl Pts',(1.71947230929001,28.4765688409329,124.325530687684));
#124012=CARTESIAN_POINT('Ctrl Pts',(1.72112716257105,28.4867646642519,124.303013491713));
#124013=CARTESIAN_POINT('Ctrl Pts',(1.72184301058404,28.4912898845768,124.293271501212));
#124014=CARTESIAN_POINT('Ctrl Pts',(1.72334053634561,28.500996742821,124.272892575523));
#124015=CARTESIAN_POINT('Ctrl Pts',(1.72412148368649,28.506198126562,124.262265666496));
#124016=CARTESIAN_POINT('Ctrl Pts',(1.72618741005727,28.5203259151761,124.234163443987));
#124017=CARTESIAN_POINT('Ctrl Pts',(1.72746548996388,28.529448767495,124.216788564199));
#124018=CARTESIAN_POINT('Ctrl Pts',(1.73410172018248,28.5787859400112,124.126726427666));
#124019=CARTESIAN_POINT('Ctrl Pts',(1.73927409767307,28.624090176007,124.056956621597));
#124020=CARTESIAN_POINT('Ctrl Pts',(1.75050046146239,28.7348278079584,123.911495430027));
#124021=CARTESIAN_POINT('Ctrl Pts',(1.756498624146,28.8022395048367,123.837730521627));
#124022=CARTESIAN_POINT('Ctrl Pts',(1.76452034257048,28.8966668096847,123.751397425456));
#124023=CARTESIAN_POINT('Ctrl Pts',(1.76630965489659,28.9179753863162,123.732887110786));
#124024=CARTESIAN_POINT('Ctrl Pts',(1.76937172689543,28.9546110445973,123.702660609856));
#124025=CARTESIAN_POINT('Ctrl Pts',(1.7706282374366,28.9696905753923,123.690652844637));
#124026=CARTESIAN_POINT('Ctrl Pts',(1.7724445147675,28.9914867171358,123.673906335216));
#124027=CARTESIAN_POINT('Ctrl Pts',(1.77299027647761,28.9980359440086,123.668950987754));
#124028=CARTESIAN_POINT('Ctrl Pts',(1.77394417097862,29.0094762765465,123.66042715472));
#124029=CARTESIAN_POINT('Ctrl Pts',(1.77435077757914,29.0143506296302,123.656836580355));
#124030=CARTESIAN_POINT('Ctrl Pts',(1.77522853465085,29.0248664523636,123.649178423531));
#124031=CARTESIAN_POINT('Ctrl Pts',(1.77570021395467,29.0305137668903,123.64511963385));
#124032=CARTESIAN_POINT('Ctrl Pts',(1.77701208757998,29.046215212826,123.633983251205));
#124033=CARTESIAN_POINT('Ctrl Pts',(1.77785704595068,29.0563223017492,123.62698158867));
#124034=CARTESIAN_POINT('Ctrl Pts',(1.78405869542625,29.1305246831192,123.576784369876));
#124035=CARTESIAN_POINT('Ctrl Pts',(1.78964061639427,29.197473222275,123.537988310393));
#124036=CARTESIAN_POINT('Ctrl Pts',(1.79586696042007,29.27437487689,123.500301981295));
#124037=CARTESIAN_POINT('Ctrl Pts',(1.7964754996018,29.2819136316209,123.496677701413));
#124038=CARTESIAN_POINT('Ctrl Pts',(1.80260370465787,29.3580788605175,123.460764674209));
#124039=CARTESIAN_POINT('Ctrl Pts',(1.80812653922023,29.4288115508352,123.43313902632));
#124040=CARTESIAN_POINT('Ctrl Pts',(1.8165523485444,29.5414934588872,123.39777885141));
#124041=CARTESIAN_POINT('Ctrl Pts',(1.81953030723498,29.582272023511,123.386666590883));
#124042=CARTESIAN_POINT('Ctrl Pts',(1.82457672658104,29.6531098765742,123.370229634247));
#124043=CARTESIAN_POINT('Ctrl Pts',(1.82666635927882,29.6829726992655,123.364158288784));
#124044=CARTESIAN_POINT('Ctrl Pts',(1.82967564470528,29.7267353441532,123.356504570745));
#124045=CARTESIAN_POINT('Ctrl Pts',(1.83061553904464,29.7405136992961,123.354272902803));
#124046=CARTESIAN_POINT('Ctrl Pts',(1.83226891182424,29.7649402578377,123.350630957027));
#124047=CARTESIAN_POINT('Ctrl Pts',(1.83298457966375,29.7755769423046,123.349150030209));
#124048=CARTESIAN_POINT('Ctrl Pts',(1.83448253969067,29.7979700554958,123.346252709959));
#124049=CARTESIAN_POINT('Ctrl Pts',(1.83526409364735,29.8097288009486,123.344858591905));
#124050=CARTESIAN_POINT('Ctrl Pts',(1.83733352958761,29.8410555440159,123.341482754373));
#124051=CARTESIAN_POINT('Ctrl Pts',(1.83861446956224,29.8606458325574,123.339721931946));
#124052=CARTESIAN_POINT('Ctrl Pts',(1.84536496575442,29.9648415987415,123.332213892433));
#124053=CARTESIAN_POINT('Ctrl Pts',(1.85064009096393,30.0497669918163,123.332585086059));
#124054=CARTESIAN_POINT('Ctrl Pts',(1.86006566838607,30.202848239972,123.344965970038));
#124055=CARTESIAN_POINT('Ctrl Pts',(1.86423332221204,30.2709823084041,123.354748225466));
#124056=CARTESIAN_POINT('Ctrl Pts',(1.87133630242154,30.3839564865597,123.378178160646));
#124057=CARTESIAN_POINT('Ctrl Pts',(1.87423369101479,30.429176750271,123.389554289904));
#124058=CARTESIAN_POINT('Ctrl Pts',(1.8789424342582,30.5000258497311,123.410573933885));
#124059=CARTESIAN_POINT('Ctrl Pts',(1.88070573276224,30.525997903815,123.418979104566));
#124060=CARTESIAN_POINT('Ctrl Pts',(1.88311927028536,30.5605901873607,123.431120648662));
#124061=CARTESIAN_POINT('Ctrl Pts',(1.88373995892311,30.5694038303257,123.434297906662));
#124062=CARTESIAN_POINT('Ctrl Pts',(1.88478194609291,30.5840526673782,123.439718756127));
#124063=CARTESIAN_POINT('Ctrl Pts',(1.88520086696497,30.589903044506,123.441921223312));
#124064=CARTESIAN_POINT('Ctrl Pts',(1.88600538029486,30.601060629361,123.446193522512));
#124065=CARTESIAN_POINT('Ctrl Pts',(1.88639061072643,30.6063698538341,123.448257738043));
#124066=CARTESIAN_POINT('Ctrl Pts',(1.8874371555427,30.6207059806807,123.453916402289));
#124067=CARTESIAN_POINT('Ctrl Pts',(1.88810142608172,30.6297120248546,123.457562591248));
#124068=CARTESIAN_POINT('Ctrl Pts',(1.89068342876682,30.6643786924457,123.471951952564));
#124069=CARTESIAN_POINT('Ctrl Pts',(1.89263006146988,30.6897991089644,123.483257815077));
#124070=CARTESIAN_POINT('Ctrl Pts',(1.90246864897745,30.8152952126032,123.542880125558));
#124071=CARTESIAN_POINT('Ctrl Pts',(1.91065987168029,30.910641652665,123.600487322182));
#124072=CARTESIAN_POINT('Ctrl Pts',(1.92293820138425,31.0466027330274,123.702448832827));
#124073=CARTESIAN_POINT('Ctrl Pts',(1.9271389265445,31.0917652175097,123.740211848135));
#124074=CARTESIAN_POINT('Ctrl Pts',(1.93308461304396,31.1539823375902,123.798099640762));
#124075=CARTESIAN_POINT('Ctrl Pts',(1.93489688160465,31.1727045570917,123.816359911119));
#124076=CARTESIAN_POINT('Ctrl Pts',(1.93814578362795,31.2058222630889,123.850218019044));
#124077=CARTESIAN_POINT('Ctrl Pts',(1.93958844032543,31.2203640556432,123.865664257095));
#124078=CARTESIAN_POINT('Ctrl Pts',(1.94183879943864,31.2427770329806,123.890401294279));
#124079=CARTESIAN_POINT('Ctrl Pts',(1.94265486548425,31.250847730041,123.899507377898));
#124080=CARTESIAN_POINT('Ctrl Pts',(1.94417937218529,31.2658134254406,123.916770376831));
#124081=CARTESIAN_POINT('Ctrl Pts',(1.94488872994252,31.2727311065784,123.924906709183));
#124082=CARTESIAN_POINT('Ctrl Pts',(1.94648079036711,31.2881494403024,123.943398610948));
#124083=CARTESIAN_POINT('Ctrl Pts',(1.94736161392708,31.2966044428568,123.953791410809));
#124084=CARTESIAN_POINT('Ctrl Pts',(1.94962663647813,31.3181408757305,123.980925920629));
#124085=CARTESIAN_POINT('Ctrl Pts',(1.95100324286549,31.331029316296,123.997818194174));
#124086=CARTESIAN_POINT('Ctrl Pts',(1.96045600370541,31.4180051242381,124.116452092594));
#124087=CARTESIAN_POINT('Ctrl Pts',(1.96807484248614,31.4806790616155,124.226056417331));
#124088=CARTESIAN_POINT('Ctrl Pts',(1.98103498906011,31.5644150982949,124.420720799116));
#124089=CARTESIAN_POINT('Ctrl Pts',(1.98632707210239,31.5922356404503,124.502264339919));
#124090=CARTESIAN_POINT('Ctrl Pts',(1.99284283712311,31.6171379296576,124.599226419919));
#124091=CARTESIAN_POINT('Ctrl Pts',(1.99376800248439,31.6204695809314,124.612917513817));
#124092=CARTESIAN_POINT('Ctrl Pts',(1.99518383053812,31.6252532947745,124.633720886531));
#124093=CARTESIAN_POINT('Ctrl Pts',(1.995667612143,31.6268332832375,124.640803501195));
#124094=CARTESIAN_POINT('Ctrl Pts',(1.99655700762109,31.6296374492197,124.653771861941));
#124095=CARTESIAN_POINT('Ctrl Pts',(1.9969618030914,31.6308761069571,124.659654205974));
#124096=CARTESIAN_POINT('Ctrl Pts',(1.99789357567764,31.6336415589165,124.673149060572));
#124097=CARTESIAN_POINT('Ctrl Pts',(1.99842170498291,31.6351469891592,124.68076560736));
#124098=CARTESIAN_POINT('Ctrl Pts',(2.00005535704772,31.6396155626593,124.704235056647));
#124099=CARTESIAN_POINT('Ctrl Pts',(2.00116988052132,31.6424016928945,124.720120157181));
#124100=CARTESIAN_POINT('Ctrl Pts',(2.00842381528541,31.6588865784798,124.822852290617));
#124101=CARTESIAN_POINT('Ctrl Pts',(2.01482532547526,31.6659215294908,124.910620757329));
#124102=CARTESIAN_POINT('Ctrl Pts',(2.02992531169939,31.6661051617482,125.118055341483));
#124103=CARTESIAN_POINT('Ctrl Pts',(2.03855843505277,31.6533468393091,125.237270699926));
#124104=CARTESIAN_POINT('Ctrl Pts',(2.04828927217212,31.6233145648734,125.375336857162));
#124105=CARTESIAN_POINT('Ctrl Pts',(2.04977254501389,31.618282177548,125.396472954639));
#124106=CARTESIAN_POINT('Ctrl Pts',(2.05215867252703,31.6094454212157,125.430609640405));
#124107=CARTESIAN_POINT('Ctrl Pts',(2.05306947180075,31.6058935612211,125.443672305969));
#124108=CARTESIAN_POINT('Ctrl Pts',(2.05469045494552,31.5992519380296,125.466972752801));
#124109=CARTESIAN_POINT('Ctrl Pts',(2.05540253319247,31.5962221080516,125.477226679963));
#124110=CARTESIAN_POINT('Ctrl Pts',(2.05691213317322,31.589560125953,125.498999459493));
#124111=CARTESIAN_POINT('Ctrl Pts',(2.05770872900135,31.5859009915848,125.510509463561));
#124112=CARTESIAN_POINT('Ctrl Pts',(2.05974163396675,31.576195531666,125.539926690842));
#124113=CARTESIAN_POINT('Ctrl Pts',(2.0609719891437,31.5699690107231,125.557772827586));
#124114=CARTESIAN_POINT('Ctrl Pts',(2.06219312175648,31.563440011958,125.57550962547));
#124115=CARTESIAN_POINT('Ctrl Pts',(1.86811695019056,31.5634399562749,125.57550977674));
#124116=CARTESIAN_POINT('Ctrl Pts',(1.8650975957568,31.5777716089006,125.536576157781));
#124117=CARTESIAN_POINT('Ctrl Pts',(1.86207416272325,31.5906501488235,125.497103921108));
#124118=CARTESIAN_POINT('Ctrl Pts',(1.85225960628685,31.6278521720039,125.366739431899));
#124119=CARTESIAN_POINT('Ctrl Pts',(1.84557562255184,31.645959334402,125.274269386285));
#124120=CARTESIAN_POINT('Ctrl Pts',(1.83779330177858,31.6582965364205,125.161227512936));
#124121=CARTESIAN_POINT('Ctrl Pts',(1.83645989763197,31.6600819946652,125.141667010593));
#124122=CARTESIAN_POINT('Ctrl Pts',(1.83434047940836,31.6623882543454,125.110278263081));
#124123=CARTESIAN_POINT('Ctrl Pts',(1.83354765617931,31.6631295647758,125.098468608018));
#124124=CARTESIAN_POINT('Ctrl Pts',(1.83204294171875,31.6643034403869,125.075929780786));
#124125=CARTESIAN_POINT('Ctrl Pts',(1.83133039332371,31.664758218864,125.065202417317));
#124126=CARTESIAN_POINT('Ctrl Pts',(1.82971404962073,31.6655581377755,125.040749997231));
#124127=CARTESIAN_POINT('Ctrl Pts',(1.82881235060955,31.6658373942977,125.027023453554));
#124128=CARTESIAN_POINT('Ctrl Pts',(1.82595478419034,31.6661865645428,124.983269170221));
#124129=CARTESIAN_POINT('Ctrl Pts',(1.82401880020484,31.6656144187612,124.953241310217));
#124130=CARTESIAN_POINT('Ctrl Pts',(1.81306268485349,31.6576973888719,124.781584047833));
#124131=CARTESIAN_POINT('Ctrl Pts',(1.80460487138785,31.6331054437484,124.641345075194));
#124132=CARTESIAN_POINT('Ctrl Pts',(1.79319152746903,31.578260222233,124.46473380145));
#124133=CARTESIAN_POINT('Ctrl Pts',(1.79050259143215,31.5638794088472,124.424069510597));
#124134=CARTESIAN_POINT('Ctrl Pts',(1.78609561888315,31.5383529214723,124.359923100736));
#124135=CARTESIAN_POINT('Ctrl Pts',(1.78441843546376,31.5282067261145,124.336063125251));
#124136=CARTESIAN_POINT('Ctrl Pts',(1.78210545923976,31.5137148434697,124.304077675527));
#124137=CARTESIAN_POINT('Ctrl Pts',(1.78149617563148,31.5098518598556,124.2957359439));
#124138=CARTESIAN_POINT('Ctrl Pts',(1.78046803682817,31.5032618987868,124.281809015657));
#124139=CARTESIAN_POINT('Ctrl Pts',(1.78005142460269,31.5005722663843,124.276206177107));
#124140=CARTESIAN_POINT('Ctrl Pts',(1.77924674889782,31.4953418884016,124.265465118399));
#124141=CARTESIAN_POINT('Ctrl Pts',(1.77885900856078,31.4928058767948,124.26032475559));
#124142=CARTESIAN_POINT('Ctrl Pts',(1.77779683150709,31.4858147039284,124.246336413686));
#124143=CARTESIAN_POINT('Ctrl Pts',(1.77711928694477,31.4813071561139,124.2375150933));
#124144=CARTESIAN_POINT('Ctrl Pts',(1.77441874119394,31.4631421169201,124.202734968191));
#124145=CARTESIAN_POINT('Ctrl Pts',(1.77236349159094,31.4488795584703,124.177100151305));
#124146=CARTESIAN_POINT('Ctrl Pts',(1.76323993688256,31.3833906809416,124.066378591908));
#124147=CARTESIAN_POINT('Ctrl Pts',(1.75594251866082,31.3252927288633,123.985595354362));
#124148=CARTESIAN_POINT('Ctrl Pts',(1.74289423580892,31.2075504571697,123.849393260035));
#124149=CARTESIAN_POINT('Ctrl Pts',(1.73712361616642,31.1503766023283,123.792229017934));
#124150=CARTESIAN_POINT('Ctrl Pts',(1.72944786058439,31.0666339856568,123.719865891249));
#124151=CARTESIAN_POINT('Ctrl Pts',(1.72739638262212,31.0434686329461,123.700913856721));
#124152=CARTESIAN_POINT('Ctrl Pts',(1.7244312011817,31.0088448891291,123.674111596015));
#124153=CARTESIAN_POINT('Ctrl Pts',(1.72349808147628,30.9977800988859,123.66576502648));
#124154=CARTESIAN_POINT('Ctrl Pts',(1.72185250703582,30.9779709465843,123.651206528042));
#124155=CARTESIAN_POINT('Ctrl Pts',(1.72113793010426,30.9692684587398,123.644939238819));
#124156=CARTESIAN_POINT('Ctrl Pts',(1.71963819342284,30.9507948539696,123.631904096089));
#124157=CARTESIAN_POINT('Ctrl Pts',(1.71885381068788,30.9410105719847,123.62515587343));
#124158=CARTESIAN_POINT('Ctrl Pts',(1.71676726088378,30.9146628316728,123.607396880218));
#124159=CARTESIAN_POINT('Ctrl Pts',(1.71547224989026,30.8979727006939,123.596576817728));
#124160=CARTESIAN_POINT('Ctrl Pts',(1.70786660590026,30.7980466847075,123.534308333818));
#124161=CARTESIAN_POINT('Ctrl Pts',(1.70182307785615,30.7105991765247,123.489972560508));
#124162=CARTESIAN_POINT('Ctrl Pts',(1.69131998367277,30.5512051637506,123.426093160997));
#124163=CARTESIAN_POINT('Ctrl Pts',(1.68684289026914,30.4809069952529,123.403210261657));
#124164=CARTESIAN_POINT('Ctrl Pts',(1.68009636241854,30.375774821969,123.376563125523));
#124165=CARTESIAN_POINT('Ctrl Pts',(1.6779188293992,30.3419687636271,123.369107278227));
#124166=CARTESIAN_POINT('Ctrl Pts',(1.67426721690907,30.2860391290879,123.358587493148));
#124167=CARTESIAN_POINT('Ctrl Pts',(1.67281867641262,30.2640416777576,123.354905693599));
#124168=CARTESIAN_POINT('Ctrl Pts',(1.67077432723228,30.2333822537574,123.350404835233));
#124169=CARTESIAN_POINT('Ctrl Pts',(1.67019774800596,30.224776726699,123.349210219644));
#124170=CARTESIAN_POINT('Ctrl Pts',(1.6692084775017,30.2100911535124,123.347288531093));
#124171=CARTESIAN_POINT('Ctrl Pts',(1.66879765044966,30.2040155840612,123.346527553127));
#124172=CARTESIAN_POINT('Ctrl Pts',(1.66793192650467,30.191264125538,123.345001756826));
#124173=CARTESIAN_POINT('Ctrl Pts',(1.6674766864847,30.184587675353,123.344243817247));
#124174=CARTESIAN_POINT('Ctrl Pts',(1.6662334926318,30.1664285366477,123.342293507142));
#124175=CARTESIAN_POINT('Ctrl Pts',(1.66544141644789,30.154937993463,123.34118009602));
#124176=CARTESIAN_POINT('Ctrl Pts',(1.66137117460098,30.0962474934186,123.336108200566));
#124177=CARTESIAN_POINT('Ctrl Pts',(1.65800789036152,30.0489097016657,123.334044877448));
#124178=CARTESIAN_POINT('Ctrl Pts',(1.64734993075662,29.9007418367087,123.333906731279));
#124179=CARTESIAN_POINT('Ctrl Pts',(1.6399375326435,29.8001291518946,123.342962945291));
#124180=CARTESIAN_POINT('Ctrl Pts',(1.62718881121054,29.6256408696133,123.374801116256));
#124181=CARTESIAN_POINT('Ctrl Pts',(1.62179331615814,29.5513606417542,123.393717987868));
#124182=CARTESIAN_POINT('Ctrl Pts',(1.61526993533219,29.4607210070736,123.423583198583));
#124183=CARTESIAN_POINT('Ctrl Pts',(1.61399052298572,29.4429076180026,123.429789857158));
#124184=CARTESIAN_POINT('Ctrl Pts',(1.61193587120959,29.4142521813549,123.44032323458));
#124185=CARTESIAN_POINT('Ctrl Pts',(1.61115454483907,29.4033438962492,123.444463557008));
#124186=CARTESIAN_POINT('Ctrl Pts',(1.60965830588906,29.382437114595,123.452651168812));
#124187=CARTESIAN_POINT('Ctrl Pts',(1.60894287466394,29.3724327019125,123.456681621149));
#124188=CARTESIAN_POINT('Ctrl Pts',(1.60728518219,29.3492392910392,123.466288319388));
#124189=CARTESIAN_POINT('Ctrl Pts',(1.60634545309903,29.3360815113137,123.47193806372));
#124190=CARTESIAN_POINT('Ctrl Pts',(1.60328414981054,29.2932083170981,123.491005480833));
#124191=CARTESIAN_POINT('Ctrl Pts',(1.60118647626245,29.2638126631903,123.505126302234));
#124192=CARTESIAN_POINT('Ctrl Pts',(1.59616231346269,29.1936169490497,123.54141956238));
#124193=CARTESIAN_POINT('Ctrl Pts',(1.59326378160945,29.1532921971898,123.56445241086));
#124194=CARTESIAN_POINT('Ctrl Pts',(1.58617262825909,29.0561065167093,123.625485063611));
#124195=CARTESIAN_POINT('Ctrl Pts',(1.58202370498385,29.0005242168353,123.665356005313));
#124196=CARTESIAN_POINT('Ctrl Pts',(1.57720950396108,28.9395410898399,123.715052700657));
#124197=CARTESIAN_POINT('Ctrl Pts',(1.5765767667947,28.9315959817358,123.721651255095));
#124198=CARTESIAN_POINT('Ctrl Pts',(1.57130488719242,28.866034153506,123.777139692381));
#124199=CARTESIAN_POINT('Ctrl Pts',(1.56661388582035,28.8117506658058,123.829817765646));
#124200=CARTESIAN_POINT('Ctrl Pts',(1.56087688616262,28.7530217076119,123.895123512882));
#124201=CARTESIAN_POINT('Ctrl Pts',(1.56006814239335,28.7449088378722,123.904348108919));
#124202=CARTESIAN_POINT('Ctrl Pts',(1.55879054196527,28.7323665446149,123.918931205423));
#124203=CARTESIAN_POINT('Ctrl Pts',(1.5583265687682,28.7278672028904,123.924229365542));
#124204=CARTESIAN_POINT('Ctrl Pts',(1.55745400450032,28.7195122309835,123.934193399882));
#124205=CARTESIAN_POINT('Ctrl Pts',(1.55704598926925,28.7156487037191,123.938852329539));
#124206=CARTESIAN_POINT('Ctrl Pts',(1.55608007680387,28.7066029877078,123.949882096635));
#124207=CARTESIAN_POINT('Ctrl Pts',(1.55552069717715,28.7014424251636,123.956270312704));
#124208=CARTESIAN_POINT('Ctrl Pts',(1.55363769079733,28.6843234727806,123.977785200966));
#124209=CARTESIAN_POINT('Ctrl Pts',(1.55230054690105,28.6725810021383,123.993080666286));
#124210=CARTESIAN_POINT('Ctrl Pts',(1.54897257481461,28.6443028078553,124.031269629524));
#124211=CARTESIAN_POINT('Ctrl Pts',(1.54696720749342,28.628078964157,124.054385967221));
#124212=CARTESIAN_POINT('Ctrl Pts',(1.53778874825973,28.5571779386006,124.16107595635));
#124213=CARTESIAN_POINT('Ctrl Pts',(1.5304440219652,28.5094952621727,124.249050532757));
#124214=CARTESIAN_POINT('Ctrl Pts',(1.51726303597941,28.4371686474596,124.416914197472));
#124215=CARTESIAN_POINT('Ctrl Pts',(1.51139765433763,28.410085701166,124.495413880593));
#124216=CARTESIAN_POINT('Ctrl Pts',(1.50437944812438,28.3839623571727,124.594582849902));
#124217=CARTESIAN_POINT('Ctrl Pts',(1.50304778634159,28.3793010836614,124.613637724073));
#124218=CARTESIAN_POINT('Ctrl Pts',(1.50093046138679,28.3723702746541,124.644307220874));
#124219=CARTESIAN_POINT('Ctrl Pts',(1.50013801275799,28.3698861798404,124.655870922818));
#124220=CARTESIAN_POINT('Ctrl Pts',(1.49863359616269,28.365382076191,124.677982075944));
#124221=CARTESIAN_POINT('Ctrl Pts',(1.49792097536365,28.3633405044518,124.68852447112));
#124222=CARTESIAN_POINT('Ctrl Pts',(1.49628850487941,28.3588773709665,124.71282805367));
#124223=CARTESIAN_POINT('Ctrl Pts',(1.49537094084789,28.3565266891281,124.726601561018));
#124224=CARTESIAN_POINT('Ctrl Pts',(1.49246287112248,28.3495866520175,124.770596259197));
#124225=CARTESIAN_POINT('Ctrl Pts',(1.49049297210273,28.3456554157299,124.800915897787));
#124226=CARTESIAN_POINT('Ctrl Pts',(1.48584076938843,28.3382635276247,124.873551651356));
#124227=CARTESIAN_POINT('Ctrl Pts',(1.48318095157678,28.3355814206046,124.915925868181));
#124228=CARTESIAN_POINT('Ctrl Pts',(1.47597757567576,28.332677457431,125.032072244088));
#124229=CARTESIAN_POINT('Ctrl Pts',(1.47150184865063,28.3357302567508,125.105828540613));
#124230=CARTESIAN_POINT('Ctrl Pts',(1.46616139066561,28.3451170752842,125.192619646064));
#124231=CARTESIAN_POINT('Ctrl Pts',(1.46533083939547,28.3467394223706,125.206080759893));
#124232=CARTESIAN_POINT('Ctrl Pts',(1.45995993592433,28.3582624962417,125.292769981152));
#124233=CARTESIAN_POINT('Ctrl Pts',(1.45536726811178,28.3728605335367,125.365281642797));
#124234=CARTESIAN_POINT('Ctrl Pts',(1.44973963917309,28.395437009501,125.44842431533));
#124235=CARTESIAN_POINT('Ctrl Pts',(1.44893130543299,28.3987853187646,125.460237199597));
#124236=CARTESIAN_POINT('Ctrl Pts',(1.4476542163264,28.4042326947301,125.478676302766));
#124237=CARTESIAN_POINT('Ctrl Pts',(1.44719033822738,28.4062432634974,125.485328503054));
#124238=CARTESIAN_POINT('Ctrl Pts',(1.4463178475217,28.4100827970753,125.497750868358));
#124239=CARTESIAN_POINT('Ctrl Pts',(1.44590980955758,28.4119016651429,125.503523895415));
#124240=CARTESIAN_POINT('Ctrl Pts',(1.44494370365468,28.4162631416855,125.517108350949));
#124241=CARTESIAN_POINT('Ctrl Pts',(1.44438415149831,28.4188321117056,125.524911025757));
#124242=CARTESIAN_POINT('Ctrl Pts',(1.44249995071792,28.4276288343304,125.550978498169));
#124243=CARTESIAN_POINT('Ctrl Pts',(1.44116176253548,28.4341159518442,125.56915328031));
#124244=CARTESIAN_POINT('Ctrl Pts',(1.43783061264571,28.4508804641549,125.613664195643));
#124245=CARTESIAN_POINT('Ctrl Pts',(1.43582307863503,28.4615151483336,125.639858783005));
#124246=CARTESIAN_POINT('Ctrl Pts',(1.42662548102339,28.5128118807922,125.757527049544));
#124247=CARTESIAN_POINT('Ctrl Pts',(1.41926325833615,28.5610011663348,125.845493073363));
#124248=CARTESIAN_POINT('Ctrl Pts',(1.40608611756473,28.6628626288872,125.997221328557));
#124249=CARTESIAN_POINT('Ctrl Pts',(1.40024031005497,28.7139771662845,126.062325611546));
#124250=CARTESIAN_POINT('Ctrl Pts',(1.39324097673362,28.7829422723837,126.137853643252));
#124251=CARTESIAN_POINT('Ctrl Pts',(1.39190985071197,28.7964180500025,126.152098508131));
#124252=CARTESIAN_POINT('Ctrl Pts',(1.38979316274644,28.8184197241252,126.174548377303));
#124253=CARTESIAN_POINT('Ctrl Pts',(1.38900082276235,28.8267866462151,126.182905861826));
#124254=CARTESIAN_POINT('Ctrl Pts',(1.38749648085482,28.8429198387189,126.19868128048));
#124255=CARTESIAN_POINT('Ctrl Pts',(1.38678382746859,28.8506701973549,126.20611455748));
#124256=CARTESIAN_POINT('Ctrl Pts',(1.38515109674147,28.8686712850179,126.223048096816));
#124257=CARTESIAN_POINT('Ctrl Pts',(1.38423330746454,28.8789708596368,126.232495433923));
#124258=CARTESIAN_POINT('Ctrl Pts',(1.38132374359486,28.9121866748853,126.26220191311));
#124259=CARTESIAN_POINT('Ctrl Pts',(1.37935260609621,28.9355432106215,126.281960776079));
#124260=CARTESIAN_POINT('Ctrl Pts',(1.37469685152446,28.992605965859,126.327598485688));
#124261=CARTESIAN_POINT('Ctrl Pts',(1.37203476879308,29.0267842935368,126.352853298509));
#124262=CARTESIAN_POINT('Ctrl Pts',(1.36483014220288,29.1228169789706,126.41828806364));
#124263=CARTESIAN_POINT('Ctrl Pts',(1.36035528249527,29.18643107814,126.455711873894));
#124264=CARTESIAN_POINT('Ctrl Pts',(1.35500293105549,29.2646158106712,126.494976778658));
#124265=CARTESIAN_POINT('Ctrl Pts',(1.35415967602753,29.2769927027013,126.501001637901));
#124266=CARTESIAN_POINT('Ctrl Pts',(1.3487915211988,29.356043150369,126.538277435509));
#124267=CARTESIAN_POINT('Ctrl Pts',(1.3442141964137,29.424644275302,126.5652287169));
#124268=CARTESIAN_POINT('Ctrl Pts',(1.33860360548016,29.5064921560772,126.591275194559));
#124269=CARTESIAN_POINT('Ctrl Pts',(1.33779532474864,29.5182319085358,126.594868715952));
#124270=CARTESIAN_POINT('Ctrl Pts',(1.33651829617363,29.5366769996734,126.60029250181));
#124271=CARTESIAN_POINT('Ctrl Pts',(1.33605442461696,29.543356173537,126.602211192496));
#124272=CARTESIAN_POINT('Ctrl Pts',(1.33518191808346,29.5558754060376,126.605722886482));
#124273=CARTESIAN_POINT('Ctrl Pts',(1.33477385745745,29.5617123945586,126.607325920083));
#124274=CARTESIAN_POINT('Ctrl Pts',(1.33380766348178,29.5754920640902,126.611029643168));
#124275=CARTESIAN_POINT('Ctrl Pts',(1.3332480453986,29.5834416911668,126.613103427274));
#124276=CARTESIAN_POINT('Ctrl Pts',(1.33136348526455,29.6101182453291,126.619852082733));
#124277=CARTESIAN_POINT('Ctrl Pts',(1.33002499825152,29.6289102465318,126.624260098651));
#124278=CARTESIAN_POINT('Ctrl Pts',(1.32669295527103,29.6754107403253,126.634318624314));
#124279=CARTESIAN_POINT('Ctrl Pts',(1.32468481904022,29.7031941431251,126.639591917562));
#124280=CARTESIAN_POINT('Ctrl Pts',(1.31548177421981,29.8299490429691,126.660322818526));
#124281=CARTESIAN_POINT('Ctrl Pts',(1.30811457890264,29.9300573564844,126.667542404684));
#124282=CARTESIAN_POINT('Ctrl Pts',(1.29493958186778,30.1127543627972,126.664229081732));
#124283=CARTESIAN_POINT('Ctrl Pts',(1.28910033775239,30.1950842061433,126.656598270649));
#124284=CARTESIAN_POINT('Ctrl Pts',(1.28210732868493,30.2958523550384,126.639637675855));
#124285=CARTESIAN_POINT('Ctrl Pts',(1.28077638392426,30.3151263585623,126.636042713124));
#124286=CARTESIAN_POINT('Ctrl Pts',(1.27865989763603,30.3459176275524,126.629735201287));
#124287=CARTESIAN_POINT('Ctrl Pts',(1.27786758091951,30.3574767568382,126.627238830709));
#124288=CARTESIAN_POINT('Ctrl Pts',(1.27636322918002,30.3794807020006,126.622240956089));
#124289=CARTESIAN_POINT('Ctrl Pts',(1.27565054324009,30.3899297740913,126.61976112538));
#124290=CARTESIAN_POINT('Ctrl Pts',(1.27401766079166,30.4139218890745,126.613821560628));
#124291=CARTESIAN_POINT('Ctrl Pts',(1.27309975342713,30.4274469513864,126.610292049063));
#124292=CARTESIAN_POINT('Ctrl Pts',(1.27018948650855,30.4704303860945,126.598495325958));
#124293=CARTESIAN_POINT('Ctrl Pts',(1.26821777763292,30.4997071350736,126.589586431336));
#124294=CARTESIAN_POINT('Ctrl Pts',(1.26356041448887,30.5690226336343,126.566389208934));
#124295=CARTESIAN_POINT('Ctrl Pts',(1.26089731591647,30.6087928832071,126.551365049412));
#124296=CARTESIAN_POINT('Ctrl Pts',(1.25369207243897,30.7158613383938,126.506164953304));
#124297=CARTESIAN_POINT('Ctrl Pts',(1.2492175499748,30.7817990681317,126.473017618766));
#124298=CARTESIAN_POINT('Ctrl Pts',(1.24385975445351,30.8572670334666,126.428580168892));
#124299=CARTESIAN_POINT('Ctrl Pts',(1.2430107406695,30.8691210068066,126.421399569191));
#124300=CARTESIAN_POINT('Ctrl Pts',(1.23764365312306,30.9432852055279,126.375199622325));
#124301=CARTESIAN_POINT('Ctrl Pts',(1.23307310763841,31.0030373928751,126.332244059039));
#124302=CARTESIAN_POINT('Ctrl Pts',(1.22747004235412,31.0692232147379,126.277680885065));
#124303=CARTESIAN_POINT('Ctrl Pts',(1.22666178740936,31.078609299087,126.269767177542));
#124304=CARTESIAN_POINT('Ctrl Pts',(1.22538479080401,31.0931697994912,126.25721282296));
#124305=CARTESIAN_POINT('Ctrl Pts',(1.22492092503705,31.0984043095,126.25264211219));
#124306=CARTESIAN_POINT('Ctrl Pts',(1.22404846207362,31.1081442385341,126.24402933362));
#124307=CARTESIAN_POINT('Ctrl Pts',(1.22364043952439,31.1126564223152,126.23999528931));
#124308=CARTESIAN_POINT('Ctrl Pts',(1.22267435703036,31.1232405855415,126.230428408292));
#124309=CARTESIAN_POINT('Ctrl Pts',(1.22211481281497,31.1292937342623,126.224875151036));
#124310=CARTESIAN_POINT('Ctrl Pts',(1.22023051617607,31.1494294461739,126.206126193112));
#124311=CARTESIAN_POINT('Ctrl Pts',(1.21889222056169,31.1633231647867,126.192731143373));
#124312=CARTESIAN_POINT('Ctrl Pts',(1.21556070692504,31.1969892648387,126.159125523245));
#124313=CARTESIAN_POINT('Ctrl Pts',(1.21355291098837,31.216485472978,126.138647527719));
#124314=CARTESIAN_POINT('Ctrl Pts',(1.20435287778152,31.3026239646651,126.043433009063));
#124315=CARTESIAN_POINT('Ctrl Pts',(1.19698839218701,31.3629668656202,125.963277432235));
#124316=CARTESIAN_POINT('Ctrl Pts',(1.18381117140529,31.4592994560645,125.807977316129));
#124317=CARTESIAN_POINT('Ctrl Pts',(1.17796734212128,31.4975731280804,125.734616005332));
#124318=CARTESIAN_POINT('Ctrl Pts',(1.17096998784353,31.5380004281088,125.640698873322));
#124319=CARTESIAN_POINT('Ctrl Pts',(1.16963897284778,31.5454337686396,125.622555127569));
#124320=CARTESIAN_POINT('Ctrl Pts',(1.16762808093418,31.556265365759,125.594726235129));
#124321=CARTESIAN_POINT('Ctrl Pts',(1.16694044491676,31.5598970610783,125.585134470859));
#124322=CARTESIAN_POINT('Ctrl Pts',(1.16625576032278,31.5634400119388,125.575509625522));
#124323=CARTESIAN_POINT('Origin',(5.,30.,125.));
#124324=CARTESIAN_POINT('',(0.46813995976768,31.5634400089539,125.575509633631));
#124325=CARTESIAN_POINT('',(0.659204001356836,31.5634400119422,125.575509625513));
#124326=CARTESIAN_POINT('',(5.,31.5634400119422,125.575509625513));
#124327=CARTESIAN_POINT('',(0.,28.7309291201476,126.079358653049));
#124328=CARTESIAN_POINT('Ctrl Pts',(0.468139959767684,31.5634400089539,
125.575509633631));
#124329=CARTESIAN_POINT('Ctrl Pts',(0.467368770690193,31.567802085591,125.563659536364));
#124330=CARTESIAN_POINT('Ctrl Pts',(0.466596956162903,31.5720298178673,
125.551758806788));
#124331=CARTESIAN_POINT('Ctrl Pts',(0.461141010456295,31.6009067962447,
125.46744456039));
#124332=CARTESIAN_POINT('Ctrl Pts',(0.456419879107899,31.6206752627371,
125.393466556818));
#124333=CARTESIAN_POINT('Ctrl Pts',(0.450407011445989,31.638409104359,125.302386884556));
#124334=CARTESIAN_POINT('Ctrl Pts',(0.449339268556211,31.6412918510075,
125.286327141761));
#124335=CARTESIAN_POINT('Ctrl Pts',(0.447751287487431,31.6451821308189,
125.262660571821));
#124336=CARTESIAN_POINT('Ctrl Pts',(0.447240769391864,31.6463738178038,
125.255084428795));
#124337=CARTESIAN_POINT('Ctrl Pts',(0.446325458016176,31.648404789134,125.241565055238));
#124338=CARTESIAN_POINT('Ctrl Pts',(0.445921798641823,31.6492643262127,
125.235625134549));
#124339=CARTESIAN_POINT('Ctrl Pts',(0.445021426772412,31.651101607034,125.222425580418));
#124340=CARTESIAN_POINT('Ctrl Pts',(0.44452388505581,31.6520635739916,125.215164118675));
#124341=CARTESIAN_POINT('Ctrl Pts',(0.443043352510583,31.6547700134784,
125.193645338723));
#124342=CARTESIAN_POINT('Ctrl Pts',(0.442053395789655,31.656377970519,125.179371957054));
#124343=CARTESIAN_POINT('Ctrl Pts',(0.434513415275642,31.6671300724779,
125.071395054618));
#124344=CARTESIAN_POINT('Ctrl Pts',(0.42764868542884,31.6684999275946,124.977096703258));
#124345=CARTESIAN_POINT('Ctrl Pts',(0.412304827135571,31.653722402769,124.766837295084));
#124346=CARTESIAN_POINT('Ctrl Pts',(0.403889262908525,31.6333448864033,
124.651637932408));
#124347=CARTESIAN_POINT('Ctrl Pts',(0.394336279461322,31.595018794061,124.518384267772));
#124348=CARTESIAN_POINT('Ctrl Pts',(0.392835702202461,31.588528832241,124.497391906723));
#124349=CARTESIAN_POINT('Ctrl Pts',(0.390424858204483,31.5773379130571,
124.463579180904));
#124350=CARTESIAN_POINT('Ctrl Pts',(0.389506471943513,31.5728914726194,
124.450678034635));
#124351=CARTESIAN_POINT('Ctrl Pts',(0.387873691290787,31.5646585834181,
124.427710617482));
#124352=CARTESIAN_POINT('Ctrl Pts',(0.387157366668118,31.5609322709169,
124.417623768616));
#124353=CARTESIAN_POINT('Ctrl Pts',(0.385640417512856,31.5527982994039,
124.396244785696));
#124354=CARTESIAN_POINT('Ctrl Pts',(0.384840708010599,31.5483645157232,
124.384963206909));
#124355=CARTESIAN_POINT('Ctrl Pts',(0.382679527278756,31.5359886582273,
124.354455646217));
#124356=CARTESIAN_POINT('Ctrl Pts',(0.381326043245242,31.5278088458072,
124.335328002947));
#124357=CARTESIAN_POINT('Ctrl Pts',(0.372816736258931,31.4737024844142,
124.215086270981));
#124358=CARTESIAN_POINT('Ctrl Pts',(0.366010330351707,31.4181195833027,
124.118620703354));
#124359=CARTESIAN_POINT('Ctrl Pts',(0.352940332421378,31.2934163691235,
123.944922250076));
#124360=CARTESIAN_POINT('Ctrl Pts',(0.346693658205991,31.2259025825912,
123.867183949264));
#124361=CARTESIAN_POINT('Ctrl Pts',(0.339013873587773,31.1403992568927,
123.785385291027));
#124362=CARTESIAN_POINT('Ctrl Pts',(0.33799191278734,31.1289765556816,123.77476073737));
#124363=CARTESIAN_POINT('Ctrl Pts',(0.336455722723449,31.1117743934971,
123.759205349809));
#124364=CARTESIAN_POINT('Ctrl Pts',(0.335950087347881,31.1061073081551,
123.754150778275));
#124365=CARTESIAN_POINT('Ctrl Pts',(0.335033168053102,31.0958263971097,
123.745106494143));
#124366=CARTESIAN_POINT('Ctrl Pts',(0.334622882564975,31.0912249366391,
123.74110312682));
#124367=CARTESIAN_POINT('Ctrl Pts',(0.333693765673588,31.0808016304986,
123.73213471557));
#124368=CARTESIAN_POINT('Ctrl Pts',(0.333173937905942,31.0749674812954,
123.727184438947));
#124369=CARTESIAN_POINT('Ctrl Pts',(0.331584096848049,31.0571107958942,
123.712243376026));
#124370=CARTESIAN_POINT('Ctrl Pts',(0.330505870857499,31.0449819336647,
123.702381769159));
#124371=CARTESIAN_POINT('Ctrl Pts',(0.32499257597472,30.9827861411625,123.653249761813));
#124372=CARTESIAN_POINT('Ctrl Pts',(0.320423120177883,30.9306413534343,
123.616703221994));
#124373=CARTESIAN_POINT('Ctrl Pts',(0.307698517681965,30.7811244703153,
123.52419866703));
#124374=CARTESIAN_POINT('Ctrl Pts',(0.299521308008059,30.67997659713,123.474948408541));
#124375=CARTESIAN_POINT('Ctrl Pts',(0.288679174945068,30.534995564185,123.421671925826));
#124376=CARTESIAN_POINT('Ctrl Pts',(0.28575732732078,30.494810505844,123.408616054369));
#124377=CARTESIAN_POINT('Ctrl Pts',(0.28177491245182,30.4384865965643,123.392657098812));
#124378=CARTESIAN_POINT('Ctrl Pts',(0.280673378841057,30.4227389239297,
123.388443754657));
#124379=CARTESIAN_POINT('Ctrl Pts',(0.278901027352942,30.3971341915459,
123.381994279869));
#124380=CARTESIAN_POINT('Ctrl Pts',(0.278225719759276,30.387314498595,123.379615612478));
#124381=CARTESIAN_POINT('Ctrl Pts',(0.276816168551184,30.3666874725309,
123.374817261534));
#124382=CARTESIAN_POINT('Ctrl Pts',(0.276082530698485,30.355876395902,123.372415705186));
#124383=CARTESIAN_POINT('Ctrl Pts',(0.274330374375297,30.3298812737826,
123.366912588925));
#124384=CARTESIAN_POINT('Ctrl Pts',(0.273315169406157,30.3146761516838,
123.363914704848));
#124385=CARTESIAN_POINT('Ctrl Pts',(0.269726970706268,30.2604530153548,
123.354007829728));
#124386=CARTESIAN_POINT('Ctrl Pts',(0.26719076948498,30.221231264432,123.348278742434));
#124387=CARTESIAN_POINT('Ctrl Pts',(0.260817490673064,30.1208997243022,
123.337261974428));
#124388=CARTESIAN_POINT('Ctrl Pts',(0.257034128238834,30.0596335023462,
123.333939030875));
#124389=CARTESIAN_POINT('Ctrl Pts',(0.247839320171625,29.9094801953683,
123.334090415222));
#124390=CARTESIAN_POINT('Ctrl Pts',(0.242477938268877,29.8207947027282,
123.341285927766));
#124391=CARTESIAN_POINT('Ctrl Pts',(0.234159662091679,29.6894615256933,
123.362600436931));
#124392=CARTESIAN_POINT('Ctrl Pts',(0.231349311652282,29.6461152983617,
123.371418915673));
#124393=CARTESIAN_POINT('Ctrl Pts',(0.227712284229607,29.5921767632879,
123.38464726608));
#124394=CARTESIAN_POINT('Ctrl Pts',(0.226965162534283,29.581206228346,123.387456665141));
#124395=CARTESIAN_POINT('Ctrl Pts',(0.225768717193004,29.563829096667,123.392095984191));
#124396=CARTESIAN_POINT('Ctrl Pts',(0.225323434430909,29.5574031382573,
123.393852934802));
#124397=CARTESIAN_POINT('Ctrl Pts',(0.224477673033089,29.545279881108,123.397245886415));
#124398=CARTESIAN_POINT('Ctrl Pts',(0.224077670321568,29.5395805739931,
123.398873806956));
#124399=CARTESIAN_POINT('Ctrl Pts',(0.223118448933726,29.5259975931469,
123.402832101328));
#124400=CARTESIAN_POINT('Ctrl Pts',(0.222557613118673,29.5181226345996,
123.405190363881));
#124401=CARTESIAN_POINT('Ctrl Pts',(0.220548127685299,29.490131162165,123.413799031918));
#124402=CARTESIAN_POINT('Ctrl Pts',(0.219081790091245,29.4701171161197,
123.42037227058));
#124403=CARTESIAN_POINT('Ctrl Pts',(0.215326067188745,29.4197529847743,
123.437978216238));
#124404=CARTESIAN_POINT('Ctrl Pts',(0.213015409762782,29.3895897780316,
123.44951693326));
#124405=CARTESIAN_POINT('Ctrl Pts',(0.200529610501357,29.2300646652659,
123.515918521441));
#124406=CARTESIAN_POINT('Ctrl Pts',(0.190064542815158,29.1076728703631,
123.58611876236));
#124407=CARTESIAN_POINT('Ctrl Pts',(0.176589423172343,28.9559563764781,
123.700772690116));
#124408=CARTESIAN_POINT('Ctrl Pts',(0.173134986376414,28.9177180680903,
123.732449039431));
#124409=CARTESIAN_POINT('Ctrl Pts',(0.168612282644377,28.8685655253681,
123.777015381181));
#124410=CARTESIAN_POINT('Ctrl Pts',(0.167481173164388,28.8563528711332,
123.788428033549));
#124411=CARTESIAN_POINT('Ctrl Pts',(0.165626985887512,28.8364739180026,
123.807573262244));
#124412=CARTESIAN_POINT('Ctrl Pts',(0.164899249616014,28.8287082396161,
123.815200400668));
#124413=CARTESIAN_POINT('Ctrl Pts',(0.163480579706886,28.8136446596442,
123.830288110655));
#124414=CARTESIAN_POINT('Ctrl Pts',(0.162789399244573,28.8063410261192,
123.83774221427));
#124415=CARTESIAN_POINT('Ctrl Pts',(0.161149985660963,28.7891064289632,
123.855665709101));
#124416=CARTESIAN_POINT('Ctrl Pts',(0.160204680457111,28.779240386751,123.866196578458));
#124417=CARTESIAN_POINT('Ctrl Pts',(0.156942374811789,28.7454615307051,
123.903203783401));
#124418=CARTESIAN_POINT('Ctrl Pts',(0.154655988771575,28.7222622101635,
123.930320071177));
#124419=CARTESIAN_POINT('Ctrl Pts',(0.14901271229703,28.6664752093685,123.999933478309));
#124420=CARTESIAN_POINT('Ctrl Pts',(0.145696720407851,28.6350312584555,
124.043296079065));
#124421=CARTESIAN_POINT('Ctrl Pts',(0.136010305398242,28.5486172949571,
124.175420816695));
#124422=CARTESIAN_POINT('Ctrl Pts',(0.129760520647114,28.4998402846621,
124.267906791714));
#124423=CARTESIAN_POINT('Ctrl Pts',(0.120761037950463,28.445148887449,124.400403266088));
#124424=CARTESIAN_POINT('Ctrl Pts',(0.118270580114547,28.4315352623153,
124.436975987133));
#124425=CARTESIAN_POINT('Ctrl Pts',(0.115008671259818,28.4158399621266,
124.484143906482));
#124426=CARTESIAN_POINT('Ctrl Pts',(0.114301287857148,28.4125589999163,
124.494330551949));
#124427=CARTESIAN_POINT('Ctrl Pts',(0.113160173153524,28.4074664239155,
124.510680000478));
#124428=CARTESIAN_POINT('Ctrl Pts',(0.112730107672887,28.4055918425637,
124.516823138953));
#124429=CARTESIAN_POINT('Ctrl Pts',(0.111880549185385,28.4019773047899,
124.528918352972));
#124430=CARTESIAN_POINT('Ctrl Pts',(0.111461248669659,28.4002350013568,
124.534869482342));
#124431=CARTESIAN_POINT('Ctrl Pts',(0.110430701722022,28.3960533375199,
124.549454117648));
#124432=CARTESIAN_POINT('Ctrl Pts',(0.109817422587184,28.3936504488922,
124.558097749877));
#124433=CARTESIAN_POINT('Ctrl Pts',(0.10755902290542,28.3851094317105,124.589811783972));
#124434=CARTESIAN_POINT('Ctrl Pts',(0.105892391064636,28.3793978953718,
124.612992775244));
#124435=CARTESIAN_POINT('Ctrl Pts',(0.0953374774786414,28.346769127222,
124.758844787492));
#124436=CARTESIAN_POINT('Ctrl Pts',(0.0860039510206011,28.3332983044055,
124.884103984439));
#124437=CARTESIAN_POINT('Ctrl Pts',(0.0697063715490643,28.3346008157314,
125.108220445731));
#124438=CARTESIAN_POINT('Ctrl Pts',(0.0626898594723843,28.343914664283,
125.206527192335));
#124439=CARTESIAN_POINT('Ctrl Pts',(0.054437159096772,28.3658285735266,
125.324826806449));
#124440=CARTESIAN_POINT('Ctrl Pts',(0.0529582260633922,28.3702069174437,
125.346126113057));
#124441=CARTESIAN_POINT('Ctrl Pts',(0.0506065414160396,28.3778936493717,
125.380130358099));
#124442=CARTESIAN_POINT('Ctrl Pts',(0.0497261093003398,28.3809372930433,
125.392891929786));
#124443=CARTESIAN_POINT('Ctrl Pts',(0.0480517958143798,28.3870419178504,
125.417211135297));
#124444=CARTESIAN_POINT('Ctrl Pts',(0.0472572206844655,28.3900771757282,
125.428774320061));
#124445=CARTESIAN_POINT('Ctrl Pts',(0.0454282488283537,28.397382327402,
125.455432374105));
#124446=CARTESIAN_POINT('Ctrl Pts',(0.044396501792675,28.4017415133624,
125.470501738964));
#124447=CARTESIAN_POINT('Ctrl Pts',(0.0410412543902908,28.4166910837999,
125.519573952442));
#124448=CARTESIAN_POINT('Ctrl Pts',(0.0387426856803513,28.4281592505517,
125.553300207085));
#124449=CARTESIAN_POINT('Ctrl Pts',(0.0310769026755918,28.4704076382907,
125.66559821414));
#124450=CARTESIAN_POINT('Ctrl Pts',(0.0258331118161244,28.5060708126985,
125.742192994397));
#124451=CARTESIAN_POINT('Ctrl Pts',(0.0154827819627932,28.5873200683497,
125.8868727954));
#124452=CARTESIAN_POINT('Ctrl Pts',(0.010389205693264,28.6324204876046,
125.954951236689));
#124453=CARTESIAN_POINT('Ctrl Pts',(0.00414832869307692,28.6911391688753,
126.030847754724));
#124454=CARTESIAN_POINT('Ctrl Pts',(0.00320452041853181,28.700106702341,
126.042132984382));
#124455=CARTESIAN_POINT('Ctrl Pts',(0.00184158482903431,28.7131616496016,
126.05813134517));
#124456=CARTESIAN_POINT('Ctrl Pts',(0.00142859836214397,28.7171310837055,
126.062940367519));
#124457=CARTESIAN_POINT('Ctrl Pts',(0.000677079262193936,28.724376940454,
126.07161911092));
#124458=CARTESIAN_POINT('Ctrl Pts',(0.000339057602576914,28.7276442281703,
126.075496395827));
#124459=CARTESIAN_POINT('Ctrl Pts',(1.87192926090485E-13,28.7309291201478,
126.079358653049));
#124460=CARTESIAN_POINT('',(0.,31.2524897196664,126.098556098763));
#124461=CARTESIAN_POINT('Origin',(0.,30.,125.));
#124462=CARTESIAN_POINT('Ctrl Pts',(1.19418364086243E-13,31.2524897196665,
126.098556098763));
#124463=CARTESIAN_POINT('Ctrl Pts',(0.000120419872249425,31.2513359446956,
126.099871544821));
#124464=CARTESIAN_POINT('Ctrl Pts',(0.000240971468816246,31.2501801021712,
126.101185167756));
#124465=CARTESIAN_POINT('Ctrl Pts',(0.00193646291216417,31.233912230833,
126.119615089179));
#124466=CARTESIAN_POINT('Ctrl Pts',(0.0035330494313661,31.2184528025057,
126.136419811813));
#124467=CARTESIAN_POINT('Ctrl Pts',(0.0132700945587604,31.1230711888905,
126.235917611428));
#124468=CARTESIAN_POINT('Ctrl Pts',(0.021756819076212,31.0351097558255,
126.310468700313));
#124469=CARTESIAN_POINT('Ctrl Pts',(0.0343332838466417,30.8914286708614,
126.408686373077));
#124470=CARTESIAN_POINT('Ctrl Pts',(0.0385499468194289,30.8409429808811,
126.439395170051));
#124471=CARTESIAN_POINT('Ctrl Pts',(0.0445224030564696,30.7657573349109,
126.479818848122));
#124472=CARTESIAN_POINT('Ctrl Pts',(0.0463457463768341,30.7422930627286,
126.491726938576));
#124473=CARTESIAN_POINT('Ctrl Pts',(0.0496166659792298,30.6992723961174,
126.512293268752));
#124474=CARTESIAN_POINT('Ctrl Pts',(0.0510702612592213,30.6798130112003,
126.521140084812));
#124475=CARTESIAN_POINT('Ctrl Pts',(0.0533394920189012,30.6489075855109,
126.534479030971));
#124476=CARTESIAN_POINT('Ctrl Pts',(0.0541635202143546,30.6375734396752,
126.539222879867));
#124477=CARTESIAN_POINT('Ctrl Pts',(0.0557042291348595,30.6161764593036,
126.547901573664));
#124478=CARTESIAN_POINT('Ctrl Pts',(0.0564218214363469,30.6061258787205,
126.551864729663));
#124479=CARTESIAN_POINT('Ctrl Pts',(0.0580345429839894,30.5833511871357,
126.560590257455));
#124480=CARTESIAN_POINT('Ctrl Pts',(0.0589277495074523,30.570605847082,
126.565295353718));
#124481=CARTESIAN_POINT('Ctrl Pts',(0.061230862686238,30.5374144326067,
126.577089076055));
#124482=CARTESIAN_POINT('Ctrl Pts',(0.0626329784772223,30.516884895882,
126.58393633018));
#124483=CARTESIAN_POINT('Ctrl Pts',(0.0713881304400068,30.3868326848086,
126.624514897965));
#124484=CARTESIAN_POINT('Ctrl Pts',(0.0783802403871928,30.2742065579199,
126.647271164091));
#124485=CARTESIAN_POINT('Ctrl Pts',(0.0909542344985003,30.0700614129422,
126.666983748548));
#124486=CARTESIAN_POINT('Ctrl Pts',(0.0965118220669303,29.9794482348121,
126.668327567464));
#124487=CARTESIAN_POINT('Ctrl Pts',(0.103345836149256,29.87463576077,126.661340571532));
#124488=CARTESIAN_POINT('Ctrl Pts',(0.104302962662541,29.8600982165223,
126.660179551556));
#124489=CARTESIAN_POINT('Ctrl Pts',(0.105763581129966,29.8381641540326,
126.658137692169));
#124490=CARTESIAN_POINT('Ctrl Pts',(0.106259834300462,29.8307548053142,
126.65739781166));
#124491=CARTESIAN_POINT('Ctrl Pts',(0.107167817586604,29.8172817915208,
126.655961143403));
#124492=CARTESIAN_POINT('Ctrl Pts',(0.107578659519283,29.8112166647196,
126.655280671597));
#124493=CARTESIAN_POINT('Ctrl Pts',(0.108520526137026,29.797383769729,126.653651685739));
#124494=CARTESIAN_POINT('Ctrl Pts',(0.109052671483722,29.7896189599143,
126.65268177408));
#124495=CARTESIAN_POINT('Ctrl Pts',(0.110697137358969,29.7657699975256,
126.649531981497));
#124496=CARTESIAN_POINT('Ctrl Pts',(0.111818488437504,29.749711170695,126.647171789978));
#124497=CARTESIAN_POINT('Ctrl Pts',(0.118574861806228,29.6540160048456,
126.631675672434));
#124498=CARTESIAN_POINT('Ctrl Pts',(0.124428652658414,29.5753920586676,
126.613002196761));
#124499=CARTESIAN_POINT('Ctrl Pts',(0.135603602004164,29.4288597830144,
126.566741408986));
#124500=CARTESIAN_POINT('Ctrl Pts',(0.140910586278219,29.3607945398787,
126.540226416423));
#124501=CARTESIAN_POINT('Ctrl Pts',(0.149161203294748,29.2560298529204,
126.491269538329));
#124502=CARTESIAN_POINT('Ctrl Pts',(0.152169158710906,29.2180815027312,
126.47172700641));
#124503=CARTESIAN_POINT('Ctrl Pts',(0.157261953427681,29.1541860318168,
126.435652271797));
#124504=CARTESIAN_POINT('Ctrl Pts',(0.15936825883863,29.1278703901019,126.419820013881));
#124505=CARTESIAN_POINT('Ctrl Pts',(0.162400090719225,29.0901763019751,
126.395698420953));
#124506=CARTESIAN_POINT('Ctrl Pts',(0.16334604576855,29.0784426697601,126.387978872917));
#124507=CARTESIAN_POINT('Ctrl Pts',(0.165009732633383,29.0578603643131,
126.374061703277));
#124508=CARTESIAN_POINT('Ctrl Pts',(0.165729670330972,29.048971859355,126.367924757666));
#124509=CARTESIAN_POINT('Ctrl Pts',(0.167236333917631,29.0304126867199,
126.354842492236));
#124510=CARTESIAN_POINT('Ctrl Pts',(0.168022319148125,29.0207554900144,
126.347879052001));
#124511=CARTESIAN_POINT('Ctrl Pts',(0.170103192254091,28.9952622904181,
126.329078250773));
#124512=CARTESIAN_POINT('Ctrl Pts',(0.171391102004005,28.9795606446763,
126.317061288452));
#124513=CARTESIAN_POINT('Ctrl Pts',(0.178216470464427,28.8968543440787,
126.25139636933));
#124514=CARTESIAN_POINT('Ctrl Pts',(0.183555173863248,28.8338532511722,
126.192907235631));
#124515=CARTESIAN_POINT('Ctrl Pts',(0.194824144986091,28.7093355564115,
126.057969197731));
#124516=CARTESIAN_POINT('Ctrl Pts',(0.200711153308162,28.6494938617959,
125.980430737206));
#124517=CARTESIAN_POINT('Ctrl Pts',(0.208600682002403,28.5817001482742,
125.874509002213));
#124518=CARTESIAN_POINT('Ctrl Pts',(0.210377412201224,28.5671996919254,
125.850543100639));
#124519=CARTESIAN_POINT('Ctrl Pts',(0.21342102665041,28.5437966293544,125.809565191917));
#124520=CARTESIAN_POINT('Ctrl Pts',(0.214672012808006,28.5345712120699,
125.79274362048));
#124521=CARTESIAN_POINT('Ctrl Pts',(0.216482736540219,28.5218140695251,
125.768498419952));
#124522=CARTESIAN_POINT('Ctrl Pts',(0.217028676566177,28.5180432482695,
125.761201448732));
#124523=CARTESIAN_POINT('Ctrl Pts',(0.217983088824172,28.5115851404496,
125.748474388849));
#124524=CARTESIAN_POINT('Ctrl Pts',(0.218390039097989,28.5088732564213,
125.743057022276));
#124525=CARTESIAN_POINT('Ctrl Pts',(0.219267141160128,28.5031188319966,
125.731403385843));
#124526=CARTESIAN_POINT('Ctrl Pts',(0.219737812071764,28.5000857266515,
125.725162955584));
#124527=CARTESIAN_POINT('Ctrl Pts',(0.221049293472486,28.4917831141627,
125.707805886538));
#124528=CARTESIAN_POINT('Ctrl Pts',(0.22189490322558,28.4865977515219,125.696649811398));
#124529=CARTESIAN_POINT('Ctrl Pts',(0.228299151452013,28.4485442980768,
125.612349266656));
#124530=CARTESIAN_POINT('Ctrl Pts',(0.234100851802819,28.4208755617529,
125.536981920421));
#124531=CARTESIAN_POINT('Ctrl Pts',(0.240293458575491,28.3973795694616,
125.45517923896));
#124532=CARTESIAN_POINT('Ctrl Pts',(0.2406528604165,28.396037463859,125.450427093416));
#124533=CARTESIAN_POINT('Ctrl Pts',(0.245962791381931,28.3765250131813,
125.380143966479));
#124534=CARTESIAN_POINT('Ctrl Pts',(0.250918207616037,28.3623616103307,
125.313563174657));
#124535=CARTESIAN_POINT('Ctrl Pts',(0.25916348053512,28.3453536468021,125.199783868053));
#124536=CARTESIAN_POINT('Ctrl Pts',(0.262492976182862,28.3403727147697,
125.15299046966));
#124537=CARTESIAN_POINT('Ctrl Pts',(0.268053993240698,28.335285751493,125.073235019719));
#124538=CARTESIAN_POINT('Ctrl Pts',(0.27031327992051,28.3341645998031,125.040368080396));
#124539=CARTESIAN_POINT('Ctrl Pts',(0.273513266818834,28.333952470457,124.993168119654));
#124540=CARTESIAN_POINT('Ctrl Pts',(0.274478252745838,28.3340727293236,
124.978848251524));
#124541=CARTESIAN_POINT('Ctrl Pts',(0.276156810082106,28.3346062390976,
124.953794438435));
#124542=CARTESIAN_POINT('Ctrl Pts',(0.27687287180603,28.3349386926446,124.943059813253));
#124543=CARTESIAN_POINT('Ctrl Pts',(0.27835368746437,28.3358449289516,124.920767514385));
#124544=CARTESIAN_POINT('Ctrl Pts',(0.279117878664363,28.3364353729257,
124.909211067412));
#124545=CARTESIAN_POINT('Ctrl Pts',(0.281100629030457,28.3382885882748,
124.879098988909));
#124546=CARTESIAN_POINT('Ctrl Pts',(0.28231317409968,28.3397417700217,124.860556371253));
#124547=CARTESIAN_POINT('Ctrl Pts',(0.287731413302196,28.3476808759991,
124.777199329844));
#124548=CARTESIAN_POINT('Ctrl Pts',(0.291827206387565,28.3576542608388,
124.712770921812));
#124549=CARTESIAN_POINT('Ctrl Pts',(0.304762928305831,28.4016909800989,
124.508392544346));
#124550=CARTESIAN_POINT('Ctrl Pts',(0.313254178368665,28.4501038627908,
124.372240989306));
#124551=CARTESIAN_POINT('Ctrl Pts',(0.323941609087643,28.5257761912828,
124.223634412228));
#124552=CARTESIAN_POINT('Ctrl Pts',(0.325426153653166,28.53657532494,124.203465343797));
#124553=CARTESIAN_POINT('Ctrl Pts',(0.327511038110602,28.552069024776,124.17590760082));
#124554=CARTESIAN_POINT('Ctrl Pts',(0.328090890717785,28.5564122027791,
124.168322986537));
#124555=CARTESIAN_POINT('Ctrl Pts',(0.329082585095573,28.5638929812083,
124.155494243625));
#124556=CARTESIAN_POINT('Ctrl Pts',(0.329492489877153,28.5670001060839,
124.150232593667));
#124557=CARTESIAN_POINT('Ctrl Pts',(0.330354170156425,28.573561568467,124.139259651117));
#124558=CARTESIAN_POINT('Ctrl Pts',(0.330806252477442,28.5770212534269,
124.133552061565));
#124559=CARTESIAN_POINT('Ctrl Pts',(0.332031517224733,28.5864465606485,
124.118211443503));
#124560=CARTESIAN_POINT('Ctrl Pts',(0.332808629225396,28.5924761903665,
124.108618436396));
#124561=CARTESIAN_POINT('Ctrl Pts',(0.336633882415379,28.6224290199547,
124.062025865209));
#124562=CARTESIAN_POINT('Ctrl Pts',(0.339755647276421,28.6477138004997,
124.02592680392));
#124563=CARTESIAN_POINT('Ctrl Pts',(0.349274887476877,28.7280359353408,
123.920414244656));
#124564=CARTESIAN_POINT('Ctrl Pts',(0.355773539922679,28.7872069940285,
123.854342503203));
#124565=CARTESIAN_POINT('Ctrl Pts',(0.366581855952751,28.8954451058935,
123.751312360873));
#124566=CARTESIAN_POINT('Ctrl Pts',(0.370935350416607,28.9418123787886,
123.711783185823));
#124567=CARTESIAN_POINT('Ctrl Pts',(0.377951826521861,29.0215140838698,
123.651049694617));
#124568=CARTESIAN_POINT('Ctrl Pts',(0.380665657124409,29.0536200283644,
123.628334221189));
#124569=CARTESIAN_POINT('Ctrl Pts',(0.38438091751618,29.0993537831104,123.59834791684));
#124570=CARTESIAN_POINT('Ctrl Pts',(0.385418315944144,29.1123217737337,
123.590099448794));
#124571=CARTESIAN_POINT('Ctrl Pts',(0.387185185521635,29.1347431347277,
123.57627004013));
#124572=CARTESIAN_POINT('Ctrl Pts',(0.387917851668388,29.1441407287606,
123.570601049642));
#124573=CARTESIAN_POINT('Ctrl Pts',(0.389311960667801,29.1622108778907,
123.559942545048));
#124574=CARTESIAN_POINT('Ctrl Pts',(0.38997394269656,29.1708736664756,123.554937504075));
#124575=CARTESIAN_POINT('Ctrl Pts',(0.391695021873892,29.1936069158011,
123.542074798301));
#124576=CARTESIAN_POINT('Ctrl Pts',(0.392749620275369,29.2077474471295,
123.534342597254));
#124577=CARTESIAN_POINT('Ctrl Pts',(0.396491474681653,29.2586429840492,
123.507464199005));
#124578=CARTESIAN_POINT('Ctrl Pts',(0.399138377662074,29.2959989525964,
123.489484755959));
#124579=CARTESIAN_POINT('Ctrl Pts',(0.409051233442797,29.4402334131195,
123.426579428819));
#124580=CARTESIAN_POINT('Ctrl Pts',(0.416019982644108,29.5510209455288,
123.391457331225));
#124581=CARTESIAN_POINT('Ctrl Pts',(0.426138251613408,29.7121565240423,
123.358335198261));
#124582=CARTESIAN_POINT('Ctrl Pts',(0.429154233192449,29.7601555452664,
123.350639160858));
#124583=CARTESIAN_POINT('Ctrl Pts',(0.433460935383947,29.8273545219931,
123.342860020302));
#124584=CARTESIAN_POINT('Ctrl Pts',(0.434686112669329,29.8463258125067,
123.340993202916));
#124585=CARTESIAN_POINT('Ctrl Pts',(0.436861932572467,29.8796633116692,
123.338289421349));
#124586=CARTESIAN_POINT('Ctrl Pts',(0.437806122271101,29.8940164080375,
123.337312293315));
#124587=CARTESIAN_POINT('Ctrl Pts',(0.439245961409634,29.9156971251417,
123.336118173804));
#124588=CARTESIAN_POINT('Ctrl Pts',(0.439734414844805,29.9230168970012,
123.33576344739));
#124589=CARTESIAN_POINT('Ctrl Pts',(0.440628995988438,29.9363530647816,
123.335205326532));
#124590=CARTESIAN_POINT('Ctrl Pts',(0.441034259632286,29.9423685351658,
123.334986231886));
#124591=CARTESIAN_POINT('Ctrl Pts',(0.441962994899013,29.9560948135542,
123.334560769196));
#124592=CARTESIAN_POINT('Ctrl Pts',(0.442487571378068,29.9638059105064,
123.334375348743));
#124593=CARTESIAN_POINT('Ctrl Pts',(0.444137162823976,29.9879324341714,
123.333962817919));
#124594=CARTESIAN_POINT('Ctrl Pts',(0.445271646113914,30.0043495425571,
123.333924806814));
#124595=CARTESIAN_POINT('Ctrl Pts',(0.452149199731338,30.1029806714545,
123.335154164901));
#124596=CARTESIAN_POINT('Ctrl Pts',(0.458120736128249,30.1850013857375,
123.342264002874));
#124597=CARTESIAN_POINT('Ctrl Pts',(0.470608274499982,30.3543741164985,
123.369674358478));
#124598=CARTESIAN_POINT('Ctrl Pts',(0.477103570605014,30.4413113746485,
123.391028303444));
#124599=CARTESIAN_POINT('Ctrl Pts',(0.485769101215786,30.5576975206259,
123.429765325448));
#124600=CARTESIAN_POINT('Ctrl Pts',(0.488094502943807,30.5889527240976,
123.441218936991));
#124601=CARTESIAN_POINT('Ctrl Pts',(0.492151258319918,30.6435315700449,
123.463095879849));
#124602=CARTESIAN_POINT('Ctrl Pts',(0.493894154064312,30.6669972250208,
123.473133279331));
#124603=CARTESIAN_POINT('Ctrl Pts',(0.496500659639892,30.7020977641217,
123.489111213766));
#124604=CARTESIAN_POINT('Ctrl Pts',(0.497377564370255,30.7139077240488,
123.494655530092));
#124605=CARTESIAN_POINT('Ctrl Pts',(0.498962370100576,30.7352481782841,
123.504981681577));
#124606=CARTESIAN_POINT('Ctrl Pts',(0.499671818589518,30.7448001115646,
123.509717322466));
#124607=CARTESIAN_POINT('Ctrl Pts',(0.501202177328026,30.7653974762926,
123.520176550304));
#124608=CARTESIAN_POINT('Ctrl Pts',(0.502021893598458,30.7764256458123,
123.525932847675));
#124609=CARTESIAN_POINT('Ctrl Pts',(0.504271941509844,30.8066734874212,
123.542154754372));
#124610=CARTESIAN_POINT('Ctrl Pts',(0.505693185222492,30.8257534459316,
123.552876579499));
#124611=CARTESIAN_POINT('Ctrl Pts',(0.51596710352404,30.9632905553324,123.633770685432));
#124612=CARTESIAN_POINT('Ctrl Pts',(0.524253532652145,31.0728529698589,
123.718008864406));
#124613=CARTESIAN_POINT('Ctrl Pts',(0.536040815112307,31.209656949812,123.853148707026));
#124614=CARTESIAN_POINT('Ctrl Pts',(0.539412498956275,31.2465919908856,
123.893408206995));
#124615=CARTESIAN_POINT('Ctrl Pts',(0.544795821256298,31.3007786776399,
123.958634157515));
#124616=CARTESIAN_POINT('Ctrl Pts',(0.546741028654071,31.3194397187668,
123.982381925061));
#124617=CARTESIAN_POINT('Ctrl Pts',(0.549365714333144,31.3432351649281,
124.014419140651));
#124618=CARTESIAN_POINT('Ctrl Pts',(0.55000867594225,31.3489581047971,124.022266724061));
#124619=CARTESIAN_POINT('Ctrl Pts',(0.551077783483638,31.3582927024894,
124.03530475626));
#124620=CARTESIAN_POINT('Ctrl Pts',(0.551501281917573,31.3619441092458,
124.040466665902));
#124621=CARTESIAN_POINT('Ctrl Pts',(0.552305799385169,31.368791410968,124.050264364683));
#124622=CARTESIAN_POINT('Ctrl Pts',(0.552686384795243,31.3719933671395,
124.054895824862));
#124623=CARTESIAN_POINT('Ctrl Pts',(0.553704699010479,31.3804635139322,
124.067281197679));
#124624=CARTESIAN_POINT('Ctrl Pts',(0.554345120421671,31.3856897469891,
124.075063357688));
#124625=CARTESIAN_POINT('Ctrl Pts',(0.556729805589084,31.4047900136592,
124.104029974355));
#124626=CARTESIAN_POINT('Ctrl Pts',(0.558497844305222,31.418245439427,124.125484719619));
#124627=CARTESIAN_POINT('Ctrl Pts',(0.567528240818528,31.4836997811928,
124.235337699133));
#124628=CARTESIAN_POINT('Ctrl Pts',(0.575065987911613,31.5279442536527,
124.328093566176));
#124629=CARTESIAN_POINT('Ctrl Pts',(0.588497965147215,31.591949911208,124.501915443828));
#124630=CARTESIAN_POINT('Ctrl Pts',(0.594412477961797,31.6147083244348,
124.581534851399));
#124631=CARTESIAN_POINT('Ctrl Pts',(0.602220934874307,31.6375157908092,
124.691793359584));
#124632=CARTESIAN_POINT('Ctrl Pts',(0.604269962726265,31.642781710564,124.721220967286));
#124633=CARTESIAN_POINT('Ctrl Pts',(0.607232105492085,31.6493251569751,
124.764470074825));
#124634=CARTESIAN_POINT('Ctrl Pts',(0.608164599205063,31.6512262275195,
124.778189755053));
#124635=CARTESIAN_POINT('Ctrl Pts',(0.609809250555115,31.6542948218558,
124.802567600137));
#124636=CARTESIAN_POINT('Ctrl Pts',(0.610523527484548,31.6555309477397,
124.813216166525));
#124637=CARTESIAN_POINT('Ctrl Pts',(0.612022805099943,31.6579204629778,
124.835692533048));
#124638=CARTESIAN_POINT('Ctrl Pts',(0.612807027139203,31.6590502589798,
124.847522277845));
#124639=CARTESIAN_POINT('Ctrl Pts',(0.614893528427083,31.6617324896373,
124.879182919037));
#124640=CARTESIAN_POINT('Ctrl Pts',(0.616188642564974,31.6630565453131,
124.899031608022));
#124641=CARTESIAN_POINT('Ctrl Pts',(0.623772434758818,31.6687718064019,
125.016298340099));
#124642=CARTESIAN_POINT('Ctrl Pts',(0.629795867719878,31.6649589272272,
125.113930756203));
#124643=CARTESIAN_POINT('Ctrl Pts',(0.640240285887603,31.6433642118955,
125.283325335272));
#124644=CARTESIAN_POINT('Ctrl Pts',(0.64467960019994,31.6293236497559,125.355278492019));
#124645=CARTESIAN_POINT('Ctrl Pts',(0.652478489251387,31.5972350524001,
125.476576858804));
#124646=CARTESIAN_POINT('Ctrl Pts',(0.655779588951016,31.5815073081684,
125.526420739406));
#124647=CARTESIAN_POINT('Ctrl Pts',(0.659200667255647,31.5634576043012,
125.57546183235));
#124648=CARTESIAN_POINT('Ctrl Pts',(0.659202334267445,31.5634488083536,
125.57548572902));
#124649=CARTESIAN_POINT('Ctrl Pts',(0.659204001356838,31.5634400119422,
125.575509625513));
#124650=CARTESIAN_POINT('Origin',(5.,30.,125.));
#124651=CARTESIAN_POINT('',(1.3202051089041,31.6659997343953,125.000940741602));
#124652=CARTESIAN_POINT('Ctrl Pts',(0.659204001356838,31.5634400119422,
125.575509625513));
#124653=CARTESIAN_POINT('Ctrl Pts',(0.659952818579036,31.5594888714704,
125.58624336624));
#124654=CARTESIAN_POINT('Ctrl Pts',(0.660707209088037,31.5554274335712,
125.59693576341));
#124655=CARTESIAN_POINT('Ctrl Pts',(0.661913462714968,31.5488129268718,
125.613823595541));
#124656=CARTESIAN_POINT('Ctrl Pts',(0.662361198565082,31.5463319310609,
125.620047130398));
#124657=CARTESIAN_POINT('Ctrl Pts',(0.663223043581735,31.5415087804316,
125.631936920441));
#124658=CARTESIAN_POINT('Ctrl Pts',(0.663636794203542,31.5391727896203,
125.637605450252));
#124659=CARTESIAN_POINT('Ctrl Pts',(0.664644208306056,31.5334345380658,
125.651314628873));
#124660=CARTESIAN_POINT('Ctrl Pts',(0.665239732984002,31.5300002824465,
125.659341607683));
#124661=CARTESIAN_POINT('Ctrl Pts',(0.667387495713215,31.5174590041267,
125.688029042452));
#124662=CARTESIAN_POINT('Ctrl Pts',(0.668958690484256,31.5079957187007,
125.708529873833));
#124663=CARTESIAN_POINT('Ctrl Pts',(0.68070975642583,31.4349176589108,125.858742594515));
#124664=CARTESIAN_POINT('Ctrl Pts',(0.69145408655341,31.3550877098455,125.979881810146));
#124665=CARTESIAN_POINT('Ctrl Pts',(0.706353123477042,31.2187010461449,
126.137732923072));
#124666=CARTESIAN_POINT('Ctrl Pts',(0.710848360648883,31.1740040118202,
126.183801013888));
#124667=CARTESIAN_POINT('Ctrl Pts',(0.716500696364889,31.1130668513934,
126.239751416371));
#124668=CARTESIAN_POINT('Ctrl Pts',(0.717760885644108,31.0991674888283,
126.252091158872));
#124669=CARTESIAN_POINT('Ctrl Pts',(0.7197927482922,31.0762523264584,126.271759323671));
#124670=CARTESIAN_POINT('Ctrl Pts',(0.720570254941475,31.0673615787215,
126.279230284049));
#124671=CARTESIAN_POINT('Ctrl Pts',(0.722064445742197,31.050042414074,126.293477427806));
#124672=CARTESIAN_POINT('Ctrl Pts',(0.722781595637464,31.0416247365479,
126.300265682542));
#124673=CARTESIAN_POINT('Ctrl Pts',(0.724451127881559,31.0217858453109,
126.315948027207));
#124674=CARTESIAN_POINT('Ctrl Pts',(0.725400869349282,31.0103135106441,
126.324776266404));
#124675=CARTESIAN_POINT('Ctrl Pts',(0.728531657477741,30.9718925022953,
126.353552741498));
#124676=CARTESIAN_POINT('Ctrl Pts',(0.730687241748473,30.9444558325748,
126.372837748582));
#124677=CARTESIAN_POINT('Ctrl Pts',(0.735883479201286,30.8761378346528,
126.417839617048));
#124678=CARTESIAN_POINT('Ctrl Pts',(0.738893417719294,30.8346842554547,
126.442632797124));
#124679=CARTESIAN_POINT('Ctrl Pts',(0.745995230933175,30.7334358222402,
126.497361544146));
#124680=CARTESIAN_POINT('Ctrl Pts',(0.750051128482708,30.6728038918927,
126.525567033434));
#124681=CARTESIAN_POINT('Ctrl Pts',(0.758902128955931,30.5382987635135,
126.578555078483));
#124682=CARTESIAN_POINT('Ctrl Pts',(0.763698665792319,30.4640577037242,
126.601951716197));
#124683=CARTESIAN_POINT('Ctrl Pts',(0.769796878259095,30.3725425064711,
126.623895369703));
#124684=CARTESIAN_POINT('Ctrl Pts',(0.770868306932346,30.35656566161,126.627478101455));
#124685=CARTESIAN_POINT('Ctrl Pts',(0.772462133810009,30.3329995914776,
126.632399031748));
#124686=CARTESIAN_POINT('Ctrl Pts',(0.772974803978947,30.325449187111,126.633921095877));
#124687=CARTESIAN_POINT('Ctrl Pts',(0.773892751723442,30.3119893872091,
126.636537423632));
#124688=CARTESIAN_POINT('Ctrl Pts',(0.774296877163166,30.3060842358617,
126.6376521471));
#124689=CARTESIAN_POINT('Ctrl Pts',(0.775196718014226,30.2929819943888,
126.640052132557));
#124690=CARTESIAN_POINT('Ctrl Pts',(0.775693242797695,30.2857825020341,
126.641321968107));
#124691=CARTESIAN_POINT('Ctrl Pts',(0.777172121290137,30.264421454863,126.644944795683));
#124692=CARTESIAN_POINT('Ctrl Pts',(0.778161455541685,30.2502380004913,
126.647162103504));
#124693=CARTESIAN_POINT('Ctrl Pts',(0.780480263962006,30.217201524402,126.651890191334));
#124694=CARTESIAN_POINT('Ctrl Pts',(0.781815648233726,30.1983308546577,
126.654261923864));
#124695=CARTESIAN_POINT('Ctrl Pts',(0.786590563466671,30.1312698577639,
126.661526501931));
#124696=CARTESIAN_POINT('Ctrl Pts',(0.790086589152524,30.082913377996,126.664640166428));
#124697=CARTESIAN_POINT('Ctrl Pts',(0.801961065874912,29.919409229959,126.668026122323));
#124698=CARTESIAN_POINT('Ctrl Pts',(0.810378374963458,29.8043718472874,
126.658475759223));
#124699=CARTESIAN_POINT('Ctrl Pts',(0.821474117974972,29.6492547775654,
126.629220199659));
#124700=CARTESIAN_POINT('Ctrl Pts',(0.824431891531851,29.607595737263,126.619691368837));
#124701=CARTESIAN_POINT('Ctrl Pts',(0.828447769148284,29.5506222132914,
126.604331885885));
#124702=CARTESIAN_POINT('Ctrl Pts',(0.829548632789009,29.5349612879075,
126.599862564166));
#124703=CARTESIAN_POINT('Ctrl Pts',(0.831315013146628,29.509771220983,126.592272653086));
#124704=CARTESIAN_POINT('Ctrl Pts',(0.831985108009481,29.5002006393613,
126.589294517775));
#124705=CARTESIAN_POINT('Ctrl Pts',(0.833379791687525,29.480254229731,126.582889673207));
#124706=CARTESIAN_POINT('Ctrl Pts',(0.834103815727575,29.4698840356168,
126.579446883321));
#124707=CARTESIAN_POINT('Ctrl Pts',(0.835825175608085,29.4451982358715,
126.570980949779));
#124708=CARTESIAN_POINT('Ctrl Pts',(0.836819360979899,29.4309157381964,
126.565863745683));
#124709=CARTESIAN_POINT('Ctrl Pts',(0.840285127572467,29.3810676016894,
126.547231760538));
#124710=CARTESIAN_POINT('Ctrl Pts',(0.842722834844815,29.3458952993867,
126.532693975326));
#124711=CARTESIAN_POINT('Ctrl Pts',(0.848795560938966,29.2584458742504,
126.492989105741));
#124712=CARTESIAN_POINT('Ctrl Pts',(0.852383163650852,29.2069274277764,
126.466272698576));
#124713=CARTESIAN_POINT('Ctrl Pts',(0.862670243545594,29.0622800374831,
126.381402728523));
#124714=CARTESIAN_POINT('Ctrl Pts',(0.869255011291786,28.9733801675694,
126.316677504005));
#124715=CARTESIAN_POINT('Ctrl Pts',(0.878120473650786,28.869088274024,126.223722013611));
#124716=CARTESIAN_POINT('Ctrl Pts',(0.880052719187994,28.8472270646883,
126.203150529413));
#124717=CARTESIAN_POINT('Ctrl Pts',(0.882681529434413,28.8188461883467,
126.174960213398));
#124718=CARTESIAN_POINT('Ctrl Pts',(0.883342512649087,28.811821082035,126.167855588923));
#124719=CARTESIAN_POINT('Ctrl Pts',(0.884391506669561,28.8008547513549,
126.15656376032));
#124720=CARTESIAN_POINT('Ctrl Pts',(0.884776275815562,28.7968704397023,
126.152418464643));
#124721=CARTESIAN_POINT('Ctrl Pts',(0.885579694648213,28.7886321161988,
126.143757987326));
#124722=CARTESIAN_POINT('Ctrl Pts',(0.885998628644832,28.7843817779742,
126.139239578341));
#124723=CARTESIAN_POINT('Ctrl Pts',(0.887038553534329,28.7739406751601,
126.128014996122));
#124724=CARTESIAN_POINT('Ctrl Pts',(0.887661696806021,28.767779651318,126.121281544598));
#124725=CARTESIAN_POINT('Ctrl Pts',(0.890033896506755,28.7446733891965,
126.095608035311));
#124726=CARTESIAN_POINT('Ctrl Pts',(0.891807269866931,28.728107887861,126.076332732886));
#124727=CARTESIAN_POINT('Ctrl Pts',(0.896555147256173,28.6854461416704,
126.02433181204));
#124728=CARTESIAN_POINT('Ctrl Pts',(0.899562627305037,28.6601316737754,
125.990989372923));
#124729=CARTESIAN_POINT('Ctrl Pts',(0.912076439066468,28.5608792446586,
125.849496931349));
#124730=CARTESIAN_POINT('Ctrl Pts',(0.921691452239241,28.4985538138432,
125.733745386815));
#124731=CARTESIAN_POINT('Ctrl Pts',(0.933543598717862,28.4363725259767,
125.576273050132));
#124732=CARTESIAN_POINT('Ctrl Pts',(0.936186469382574,28.4235430828048,
125.540190249118));
#124733=CARTESIAN_POINT('Ctrl Pts',(0.939850840103563,28.4072440800358,
125.488803278875));
#124734=CARTESIAN_POINT('Ctrl Pts',(0.940905888925251,28.4027303364164,
125.473845667598));
#124735=CARTESIAN_POINT('Ctrl Pts',(0.942685251681564,28.3954262235344,
125.448350037626));
#124736=CARTESIAN_POINT('Ctrl Pts',(0.943413034264247,28.3925277302467,
125.437844346847));
#124737=CARTESIAN_POINT('Ctrl Pts',(0.944883589146057,28.3868537524629,
125.416462665857));
#124738=CARTESIAN_POINT('Ctrl Pts',(0.945626121342268,28.3840846737134,
125.405585547953));
#124739=CARTESIAN_POINT('Ctrl Pts',(0.947466774148661,28.3774623333828,
125.378427542424));
#124740=CARTESIAN_POINT('Ctrl Pts',(0.948560536708781,28.3737439347172,
125.362114799254));
#124741=CARTESIAN_POINT('Ctrl Pts',(0.952914978220962,28.3598267199175,
125.296514254568));
#124742=CARTESIAN_POINT('Ctrl Pts',(0.956112837826936,28.351617389738,125.24682910196));
#124743=CARTESIAN_POINT('Ctrl Pts',(0.965014141073731,28.3348077580783,
125.10555676311));
#124744=CARTESIAN_POINT('Ctrl Pts',(0.97058122621504,28.3315200463238,125.01352615613));
#124745=CARTESIAN_POINT('Ctrl Pts',(0.97651601084138,28.3360778930133,124.916666153156));
#124746=CARTESIAN_POINT('Ctrl Pts',(0.976824089541183,28.3363371165403,
124.911642102236));
#124747=CARTESIAN_POINT('Ctrl Pts',(0.982046211373305,28.3411132169989,
124.826565896748));
#124748=CARTESIAN_POINT('Ctrl Pts',(0.987007554900982,28.3513800315247,
124.746951485922));
#124749=CARTESIAN_POINT('Ctrl Pts',(0.993048223344464,28.3697888909617,
124.656314457611));
#124750=CARTESIAN_POINT('Ctrl Pts',(0.993859839462372,28.3723768980549,
124.644259886892));
#124751=CARTESIAN_POINT('Ctrl Pts',(0.995141065074082,28.3766351740338,
124.625445451774));
#124752=CARTESIAN_POINT('Ctrl Pts',(0.995605747122006,28.3782144998812,
124.618665166829));
#124753=CARTESIAN_POINT('Ctrl Pts',(0.996479002658836,28.3812462210789,
124.60600909048));
#124754=CARTESIAN_POINT('Ctrl Pts',(0.996886992587754,28.3826881998646,
124.60013105892));
#124755=CARTESIAN_POINT('Ctrl Pts',(0.997851965809552,28.3861589690541,
124.586308868633));
#124756=CARTESIAN_POINT('Ctrl Pts',(0.998410420994445,28.3882144110028,
124.57837168809));
#124757=CARTESIAN_POINT('Ctrl Pts',(1.00028635216151,28.3952771152164,124.551905291348));
#124758=CARTESIAN_POINT('Ctrl Pts',(1.00161720896866,28.4005457857632,124.533448241567));
#124759=CARTESIAN_POINT('Ctrl Pts',(1.00492587989113,28.4142983909995,124.488244555675));
#124760=CARTESIAN_POINT('Ctrl Pts',(1.00691802891608,28.4231412964133,124.461613819438));
#124761=CARTESIAN_POINT('Ctrl Pts',(1.01597949388326,28.4660223570574,124.342612389942));
#124762=CARTESIAN_POINT('Ctrl Pts',(1.02321720301547,28.5075344275784,124.253144807469));
#124763=CARTESIAN_POINT('Ctrl Pts',(1.03642265546007,28.5989391316009,124.094607835047));
#124764=CARTESIAN_POINT('Ctrl Pts',(1.04240890848009,28.6466968307238,124.024663641592));
#124765=CARTESIAN_POINT('Ctrl Pts',(1.04954358140924,28.711857745256,123.943291839808));
#124766=CARTESIAN_POINT('Ctrl Pts',(1.05087855734872,28.7244191307929,123.928162275411));
#124767=CARTESIAN_POINT('Ctrl Pts',(1.05300003611701,28.7449690258938,123.904284054407));
#124768=CARTESIAN_POINT('Ctrl Pts',(1.05379336763362,28.7527877697174,123.895392447721));
#124769=CARTESIAN_POINT('Ctrl Pts',(1.05529878780915,28.7678781759838,123.878595903846));
#124770=CARTESIAN_POINT('Ctrl Pts',(1.05601153674331,28.7751327553615,123.87067649528));
#124771=CARTESIAN_POINT('Ctrl Pts',(1.05764336520534,28.7919921784295,123.852625615239));
#124772=CARTESIAN_POINT('Ctrl Pts',(1.05856016952897,28.8016488856344,123.842543520416));
#124773=CARTESIAN_POINT('Ctrl Pts',(1.06146198922086,28.8327903696453,123.810837786707));
#124774=CARTESIAN_POINT('Ctrl Pts',(1.06342653393592,28.8547430612517,123.789681107625));
#124775=CARTESIAN_POINT('Ctrl Pts',(1.06806317226052,28.9084988238109,123.740647623599));
#124776=CARTESIAN_POINT('Ctrl Pts',(1.07071299943881,28.9408070988456,123.713355527454));
#124777=CARTESIAN_POINT('Ctrl Pts',(1.0779091005603,29.0322434778389,123.641896566375));
#124778=CARTESIAN_POINT('Ctrl Pts',(1.08238699243441,29.0933205750657,123.600382045042));
#124779=CARTESIAN_POINT('Ctrl Pts',(1.08763840827616,29.1673634778397,123.55694135908));
#124780=CARTESIAN_POINT('Ctrl Pts',(1.08837798832119,29.1778448805665,123.550944178062));
#124781=CARTESIAN_POINT('Ctrl Pts',(1.09376010146922,29.2544242382338,123.508225852885));
#124782=CARTESIAN_POINT('Ctrl Pts',(1.09845400542489,29.322881007457,123.475932988059));
#124783=CARTESIAN_POINT('Ctrl Pts',(1.10419437901174,29.4047272492038,123.443928879114));
#124784=CARTESIAN_POINT('Ctrl Pts',(1.10500330146222,29.4162196539468,123.439580996383));
#124785=CARTESIAN_POINT('Ctrl Pts',(1.10628122189851,29.4342887051178,123.432972535078));
#124786=CARTESIAN_POINT('Ctrl Pts',(1.10674533487703,29.4408334698775,123.430625241637));
#124787=CARTESIAN_POINT('Ctrl Pts',(1.10761819081847,29.4531047513464,123.426310624824));
#124788=CARTESIAN_POINT('Ctrl Pts',(1.10802635787912,29.4588275466715,123.424333463698));
#124789=CARTESIAN_POINT('Ctrl Pts',(1.10899269581838,29.4723413166809,123.419746912091));
#124790=CARTESIAN_POINT('Ctrl Pts',(1.10955235086725,29.480140956618,123.417163913771));
#124791=CARTESIAN_POINT('Ctrl Pts',(1.11143662837365,29.5063221126128,123.408707909851));
#124792=CARTESIAN_POINT('Ctrl Pts',(1.11277478822223,29.5247857488185,123.403096837993));
#124793=CARTESIAN_POINT('Ctrl Pts',(1.11610568808141,29.5705240079117,123.390060474166));
#124794=CARTESIAN_POINT('Ctrl Pts',(1.11811299445784,29.5978976384193,123.383006365152));
#124795=CARTESIAN_POINT('Ctrl Pts',(1.12730763320554,29.7229349798826,123.354155791651));
#124796=CARTESIAN_POINT('Ctrl Pts',(1.13466700934437,29.8222618537179,123.340488692602));
#124797=CARTESIAN_POINT('Ctrl Pts',(1.14784369775615,30.004803028561,123.331956693205));
#124798=CARTESIAN_POINT('Ctrl Pts',(1.15369166135275,30.0875729025551,123.334249046508));
#124799=CARTESIAN_POINT('Ctrl Pts',(1.16069331953902,30.1893506945456,123.344679212863));
#124800=CARTESIAN_POINT('Ctrl Pts',(1.16202474155987,30.2088234492544,123.347022862252));
#124801=CARTESIAN_POINT('Ctrl Pts',(1.16414194306474,30.2399681137035,123.351330469495));
#124802=CARTESIAN_POINT('Ctrl Pts',(1.16493450303635,30.2516678618541,123.353075831675));
#124803=CARTESIAN_POINT('Ctrl Pts',(1.16643929615208,30.2739550846055,123.3566436787));
#124804=CARTESIAN_POINT('Ctrl Pts',(1.1671521807826,30.2845454096222,123.358444242123));
#124805=CARTESIAN_POINT('Ctrl Pts',(1.1687854972134,30.3088774222517,123.362823711763));
#124806=CARTESIAN_POINT('Ctrl Pts',(1.16970363874614,30.322605665053,123.365473443055));
#124807=CARTESIAN_POINT('Ctrl Pts',(1.17261460969725,30.3662717155549,123.374473150756));
#124808=CARTESIAN_POINT('Ctrl Pts',(1.17458677823152,30.3960696321055,123.381475504621));
#124809=CARTESIAN_POINT('Ctrl Pts',(1.17924528002188,30.466755745292,123.40015565067));
#124810=CARTESIAN_POINT('Ctrl Pts',(1.18190904512399,30.5074233584667,123.412585503692));
#124811=CARTESIAN_POINT('Ctrl Pts',(1.18911444875213,30.6171889142565,123.450784996727));
#124812=CARTESIAN_POINT('Ctrl Pts',(1.19358851883807,30.6851215217037,123.479605923504));
#124813=CARTESIAN_POINT('Ctrl Pts',(1.20304788111868,30.823147536297,123.549299960639));
#124814=CARTESIAN_POINT('Ctrl Pts',(1.20802859471426,30.8926117881279,123.590977809746));
#124815=CARTESIAN_POINT('Ctrl Pts',(1.21433279756274,30.9721804331959,123.64696995769));
#124816=CARTESIAN_POINT('Ctrl Pts',(1.21540616685556,30.9854549760152,123.656607454636));
#124817=CARTESIAN_POINT('Ctrl Pts',(1.21700223551545,31.0047530616942,123.671058062475));
#124818=CARTESIAN_POINT('Ctrl Pts',(1.2175151606351,31.0108894104195,123.675719824828));
#124819=CARTESIAN_POINT('Ctrl Pts',(1.2184173343787,31.0215635000866,123.683946311164));
#124820=CARTESIAN_POINT('Ctrl Pts',(1.21880528522261,31.0261153966085,123.687492290473));
#124821=CARTESIAN_POINT('Ctrl Pts',(1.21920080715234,31.0307171248432,123.69111565977));
#124822=CARTESIAN_POINT('Ctrl Pts',(1.21920667341311,31.0307853676731,123.691169402353));
#124823=CARTESIAN_POINT('Ctrl Pts',(1.21922183236524,31.0309616911448,123.691308282932));
#124824=CARTESIAN_POINT('Ctrl Pts',(1.21923112559518,31.0310697650798,123.691393428693));
#124825=CARTESIAN_POINT('Ctrl Pts',(1.21924929405809,31.0312810097945,123.691559899692));
#124826=CARTESIAN_POINT('Ctrl Pts',(1.21925816922612,31.0313841817224,123.691641223918));
#124827=CARTESIAN_POINT('Ctrl Pts',(1.21927553586896,31.0315860268068,123.691800364971));
#124828=CARTESIAN_POINT('Ctrl Pts',(1.2192840272588,31.0316847006437,123.691878180654));
#124829=CARTESIAN_POINT('Ctrl Pts',(1.21930065697599,31.0318779104089,123.69203058426));
#124830=CARTESIAN_POINT('Ctrl Pts',(1.21930879523635,31.031972447027,123.692105171248));
#124831=CARTESIAN_POINT('Ctrl Pts',(1.21932474616484,31.0321577057908,123.692251368292));
#124832=CARTESIAN_POINT('Ctrl Pts',(1.21933255878525,31.0322484286796,123.692322977625));
#124833=CARTESIAN_POINT('Ctrl Pts',(1.21934788320445,31.0324263514604,123.692463445576));
#124834=CARTESIAN_POINT('Ctrl Pts',(1.21935539494409,31.032513551816,123.692532303396));
#124835=CARTESIAN_POINT('Ctrl Pts',(1.21937013993988,31.0326846922427,123.69266747235));
#124836=CARTESIAN_POINT('Ctrl Pts',(1.21937737314511,31.0327686327463,123.69273378279));
#124837=CARTESIAN_POINT('Ctrl Pts',(1.21939158129738,31.0329334912076,123.692864041739));
#124838=CARTESIAN_POINT('Ctrl Pts',(1.21939855620023,31.0330144095663,123.69292798964));
#124839=CARTESIAN_POINT('Ctrl Pts',(1.21941226611225,31.0331734394942,123.693053691295));
#124840=CARTESIAN_POINT('Ctrl Pts',(1.21941900108266,31.0332515514322,123.69311544451));
#124841=CARTESIAN_POINT('Ctrl Pts',(1.21943224784002,31.0334051647447,123.69323690948));
#124842=CARTESIAN_POINT('Ctrl Pts',(1.21943875959904,31.0334806665304,123.693296620815));
#124843=CARTESIAN_POINT('Ctrl Pts',(1.21945157515994,31.0336292382594,123.693414141169));
#124844=CARTESIAN_POINT('Ctrl Pts',(1.21945787895093,31.0337023087384,123.693471949941));
#124845=CARTESIAN_POINT('Ctrl Pts',(1.21947029255831,31.0338461818934,123.693585792967));
#124846=CARTESIAN_POINT('Ctrl Pts',(1.21947640234328,31.0339169848029,123.693641826799));
#124847=CARTESIAN_POINT('Ctrl Pts',(1.21948844072825,31.0340564728022,123.693752236852));
#124848=CARTESIAN_POINT('Ctrl Pts',(1.21949436929992,31.0341251581047,123.693806612691));
#124849=CARTESIAN_POINT('Ctrl Pts',(1.21950605700752,31.0342605486142,123.693913814168));
#124850=CARTESIAN_POINT('Ctrl Pts',(1.21951181611796,31.0343272540166,123.693966639462));
#124851=CARTESIAN_POINT('Ctrl Pts',(1.21952317574618,31.0344588117726,123.694070838984));
#124852=CARTESIAN_POINT('Ctrl Pts',(1.21952877623557,31.0345236642437,123.694122212853));
#124853=CARTESIAN_POINT('Ctrl Pts',(1.21953982852408,31.0346516321283,123.694223600068));
#124854=CARTESIAN_POINT('Ctrl Pts',(1.21954528034411,31.0347147481906,123.694273613515));
#124855=CARTESIAN_POINT('Ctrl Pts',(1.21955604459482,31.0348393521421,123.694372364947));
#124856=CARTESIAN_POINT('Ctrl Pts',(1.21956135699385,31.0349008400361,123.694421102557));
#124857=CARTESIAN_POINT('Ctrl Pts',(1.21957185096577,31.035022287867,123.694517380631));
#124858=CARTESIAN_POINT('Ctrl Pts',(1.21957703250395,31.0350822477416,123.694564920701));
#124859=CARTESIAN_POINT('Ctrl Pts',(1.21958727266399,31.0352007320731,123.694658876042));
#124860=CARTESIAN_POINT('Ctrl Pts',(1.21959233127398,31.0352592567035,123.694705291136));
#124861=CARTESIAN_POINT('Ctrl Pts',(1.21960233292773,31.0353749565056,123.694797063761));
#124862=CARTESIAN_POINT('Ctrl Pts',(1.21960727597216,31.0354321319706,123.694842421234));
#124863=CARTESIAN_POINT('Ctrl Pts',(1.21961705343487,31.0355452145648,123.694932142115));
#124864=CARTESIAN_POINT('Ctrl Pts',(1.21962188781855,31.035601121556,123.694976505144));
#124865=CARTESIAN_POINT('Ctrl Pts',(1.21963145426949,31.0357117409508,123.695064294865));
#124866=CARTESIAN_POINT('Ctrl Pts',(1.21963618636369,31.0357664539071,123.695107721749));
#124867=CARTESIAN_POINT('Ctrl Pts',(1.21964555432574,31.0358747563637,123.695193694907));
#124868=CARTESIAN_POINT('Ctrl Pts',(1.21965019015896,31.035928345686,123.695236240814));
#124869=CARTESIAN_POINT('Ctrl Pts',(1.21965937114814,31.0360344656818,123.695320502798));
#124870=CARTESIAN_POINT('Ctrl Pts',(1.21966391631347,31.0360869966688,123.695362218915));
#124871=CARTESIAN_POINT('Ctrl Pts',(1.21967292122972,31.0361910614302,123.695444869489));
#124872=CARTESIAN_POINT('Ctrl Pts',(1.21967738098021,31.036242595389,123.695485803898));
#124873=CARTESIAN_POINT('Ctrl Pts',(1.21968622007376,31.036344724515,123.695566936886));
#124874=CARTESIAN_POINT('Ctrl Pts',(1.21969059938012,31.0363953194332,123.695607135088));
#124875=CARTESIAN_POINT('Ctrl Pts',(1.21969928215642,31.0364956238086,123.695686837505));
#124876=CARTESIAN_POINT('Ctrl Pts',(1.21970358563773,31.0365453335592,123.695726341787));
#124877=CARTESIAN_POINT('Ctrl Pts',(1.21971212122168,31.0366439195734,123.695804697175));
#124878=CARTESIAN_POINT('Ctrl Pts',(1.21971635329085,31.0366927956005,123.695843547941));
#124879=CARTESIAN_POINT('Ctrl Pts',(1.21972475011958,31.0367897616077,123.69592063355));
#124880=CARTESIAN_POINT('Ctrl Pts',(1.21972891489335,31.0368378518908,123.695958868493));
#124881=CARTESIAN_POINT('Ctrl Pts',(1.21973718105,31.036933292073,123.696034758343));
#124882=CARTESIAN_POINT('Ctrl Pts',(1.21974128243751,31.0369806421544,123.696072413262));
#124883=CARTESIAN_POINT('Ctrl Pts',(1.22028397769698,31.0432454572721,123.701055033715));
#124884=CARTESIAN_POINT('Ctrl Pts',(1.22082562537764,31.0494273201492,123.706044280924));
#124885=CARTESIAN_POINT('Ctrl Pts',(1.22202868314172,31.063007270087,123.717165685881));
#124886=CARTESIAN_POINT('Ctrl Pts',(1.2226913751114,31.0703884151777,123.723317986299));
#124887=CARTESIAN_POINT('Ctrl Pts',(1.22455787967135,31.0909123956658,123.740728141102));
#124888=CARTESIAN_POINT('Ctrl Pts',(1.22576982250827,31.1039332970036,123.752127132211));
#124889=CARTESIAN_POINT('Ctrl Pts',(1.22993490269307,31.1477219639052,123.791683125796));
#124890=CARTESIAN_POINT('Ctrl Pts',(1.23293161995211,31.1776076635566,123.820790463895));
#124891=CARTESIAN_POINT('Ctrl Pts',(1.24534838092547,31.2958928554335,123.944979981985));
#124892=CARTESIAN_POINT('Ctrl Pts',(1.25487755850006,31.3741410617327,124.049131547035));
#124893=CARTESIAN_POINT('Ctrl Pts',(1.26673032546307,31.4592919610593,124.195283835595));
#124894=CARTESIAN_POINT('Ctrl Pts',(1.26944596021835,31.4778731338379,124.229939887222));
#124895=CARTESIAN_POINT('Ctrl Pts',(1.2731921198376,31.502172933079,124.279388061748));
#124896=CARTESIAN_POINT('Ctrl Pts',(1.27425822595668,31.5089322424796,124.293651216599));
#124897=CARTESIAN_POINT('Ctrl Pts',(1.27605066006876,31.5200270579677,124.317949297389));
#124898=CARTESIAN_POINT('Ctrl Pts',(1.27678057790763,31.5244682347428,124.327934505453));
#124899=CARTESIAN_POINT('Ctrl Pts',(1.27825095082319,31.5332565239658,124.348228885664));
#124900=CARTESIAN_POINT('Ctrl Pts',(1.27899120722439,31.537598684842,124.358539597106));
#124901=CARTESIAN_POINT('Ctrl Pts',(1.28081775627551,31.5481048919435,124.384206985614));
#124902=CARTESIAN_POINT('Ctrl Pts',(1.28189983863684,31.5541447227466,124.399613452858));
#124903=CARTESIAN_POINT('Ctrl Pts',(1.28613710096058,31.5770468556965,124.460695271514));
#124904=CARTESIAN_POINT('Ctrl Pts',(1.289233864174,31.5921340232231,124.50701287269));
#124905=CARTESIAN_POINT('Ctrl Pts',(1.30175015240752,31.6456276915849,124.699507841544));
#124906=CARTESIAN_POINT('Ctrl Pts',(1.31064630109017,31.6660850299523,124.849887173953));
#124907=CARTESIAN_POINT('Ctrl Pts',(1.3202051089041,31.6659997343953,125.000940741602));
#124908=CARTESIAN_POINT('Ctrl Pts',(1.32020526047221,31.6659997330411,125.000943136764));
#124909=CARTESIAN_POINT('Ctrl Pts',(1.32219893801785,31.6659818976929,125.032448308161));
#124910=CARTESIAN_POINT('Ctrl Pts',(1.32422173835897,31.6650703897071,125.063944775686));
#124911=CARTESIAN_POINT('Ctrl Pts',(1.32680936405944,31.6628115005492,125.103330023435));
#124912=CARTESIAN_POINT('Ctrl Pts',(1.32733346424632,31.6622995925459,125.111262027454));
#124913=CARTESIAN_POINT('Ctrl Pts',(1.3282558745491,31.6613044281163,125.125136490565));
#124914=CARTESIAN_POINT('Ctrl Pts',(1.32865288126487,31.6608459899292,125.131080659028));
#124915=CARTESIAN_POINT('Ctrl Pts',(1.32944779578682,31.6598685577877,125.142924622143));
#124916=CARTESIAN_POINT('Ctrl Pts',(1.32984567753739,31.6593500037223,125.148824193138));
#124917=CARTESIAN_POINT('Ctrl Pts',(1.3307184216827,31.6581490151828,125.16170026855));
#124918=CARTESIAN_POINT('Ctrl Pts',(1.33119393266027,31.6574540172209,125.168675160255));
#124919=CARTESIAN_POINT('Ctrl Pts',(1.33252665365269,31.6553928067528,125.188116833037));
#124920=CARTESIAN_POINT('Ctrl Pts',(1.33338886477738,31.6539298363843,125.200572581251));
#124921=CARTESIAN_POINT('Ctrl Pts',(1.33795703000348,31.6454968392836,125.265987604827));
#124922=CARTESIAN_POINT('Ctrl Pts',(1.34176854934652,31.6361239516461,125.318600890097));
#124923=CARTESIAN_POINT('Ctrl Pts',(1.3504369306267,31.6094152752173,125.435636654983));
#124924=CARTESIAN_POINT('Ctrl Pts',(1.35530991971809,31.5907040896157,125.499657140944));
#124925=CARTESIAN_POINT('Ctrl Pts',(1.36048146718461,31.5666375771793,125.566766595078));
#124926=CARTESIAN_POINT('Ctrl Pts',(1.36081892588276,31.5650478864037,125.571141644177));
#124927=CARTESIAN_POINT('Ctrl Pts',(1.36115613275098,31.5634400145948,125.575509618307));
#124928=CARTESIAN_POINT('Ctrl Pts',(1.16625576032278,31.5634400119388,125.575509625522));
#124929=CARTESIAN_POINT('Ctrl Pts',(1.16615104541434,31.5639818669451,125.574037612267));
#124930=CARTESIAN_POINT('Ctrl Pts',(1.16604639949232,31.5645216461886,125.572564825237));
#124931=CARTESIAN_POINT('Ctrl Pts',(1.1652259625993,31.5687400693189,125.561004356859));
#124932=CARTESIAN_POINT('Ctrl Pts',(1.16451336704287,31.5723232598739,125.55088190129));
#124933=CARTESIAN_POINT('Ctrl Pts',(1.16288077169874,31.5803439224431,125.527507690019));
#124934=CARTESIAN_POINT('Ctrl Pts',(1.16196305973342,31.5847130653475,125.514233212133));
#124935=CARTESIAN_POINT('Ctrl Pts',(1.15905376820061,31.5981099678571,125.471737056413));
#124936=CARTESIAN_POINT('Ctrl Pts',(1.15708282306876,31.606500675845,125.442320117487));
#124937=CARTESIAN_POINT('Ctrl Pts',(1.15242757306978,31.624598565457,125.371536763432));
#124938=CARTESIAN_POINT('Ctrl Pts',(1.14976579838331,31.6335428965921,125.329997045072));
#124939=CARTESIAN_POINT('Ctrl Pts',(1.14256128485893,31.6536422265335,125.215543399428));
#124940=CARTESIAN_POINT('Ctrl Pts',(1.13808625857221,31.6615602323168,125.14216023227));
#124941=CARTESIAN_POINT('Ctrl Pts',(1.13273557453383,31.6651561164103,125.054770113502));
#124942=CARTESIAN_POINT('Ctrl Pts',(1.13189415096574,31.6655510682859,125.04104010977));
#124943=CARTESIAN_POINT('Ctrl Pts',(1.12652557143184,31.6669837310359,124.953644787307));
#124944=CARTESIAN_POINT('Ctrl Pts',(1.121945997636,31.6633036550011,124.87999264205));
#124945=CARTESIAN_POINT('Ctrl Pts',(1.11633292104252,31.6533404778681,124.79464180066));
#124946=CARTESIAN_POINT('Ctrl Pts',(1.11552466937479,31.651782321632,124.782464104157));
#124947=CARTESIAN_POINT('Ctrl Pts',(1.11424769822748,31.6491317170624,124.763422596876));
#124948=CARTESIAN_POINT('Ctrl Pts',(1.11378385527769,31.6481306211017,124.756546227583));
#124949=CARTESIAN_POINT('Ctrl Pts',(1.11291140865508,31.646177088406,124.743692311869));
#124950=CARTESIAN_POINT('Ctrl Pts',(1.11250337937553,31.6452350561548,124.737713433993));
#124951=CARTESIAN_POINT('Ctrl Pts',(1.11153727988101,31.6429377259955,124.723632288774));
#124952=CARTESIAN_POINT('Ctrl Pts',(1.11097772525339,31.6415550575652,124.71553476624));
#124953=CARTESIAN_POINT('Ctrl Pts',(1.1090934975894,31.6367239002156,124.688450205421));
#124954=CARTESIAN_POINT('Ctrl Pts',(1.10775528409002,31.6330055499766,124.669513700042));
#124955=CARTESIAN_POINT('Ctrl Pts',(1.10442406724899,31.6230315611231,124.623007081869));
#124956=CARTESIAN_POINT('Ctrl Pts',(1.10241649043974,31.6164015710208,124.595523932047));
#124957=CARTESIAN_POINT('Ctrl Pts',(1.0932188414337,31.5831337189889,124.471546332358));
#124958=CARTESIAN_POINT('Ctrl Pts',(1.08585659497729,31.5485315442009,124.377403698515));
#124959=CARTESIAN_POINT('Ctrl Pts',(1.07267823814797,31.4703067631554,124.212226378259));
#124960=CARTESIAN_POINT('Ctrl Pts',(1.06683129443048,31.4294105282845,124.140245089017));
#124961=CARTESIAN_POINT('Ctrl Pts',(1.05983080640134,31.3724051956386,124.055307217959));
#124962=CARTESIAN_POINT('Ctrl Pts',(1.05849959388575,31.3611912868546,124.039219686378));
#124963=CARTESIAN_POINT('Ctrl Pts',(1.05638278288682,31.3427628122987,124.013752626706));
#124964=CARTESIAN_POINT('Ctrl Pts',(1.05559040554109,31.3357281098834,124.004245873536));
#124965=CARTESIAN_POINT('Ctrl Pts',(1.05408600133388,31.3221134044702,123.986250787895));
#124966=CARTESIAN_POINT('Ctrl Pts',(1.05337332289603,31.3155514170519,123.977749640437));
#124967=CARTESIAN_POINT('Ctrl Pts',(1.05174054621389,31.3002614353206,123.958332338911));
#124968=CARTESIAN_POINT('Ctrl Pts',(1.05082273596291,31.2914772837104,123.947461277807));
#124969=CARTESIAN_POINT('Ctrl Pts',(1.04791314522152,31.2630361558175,123.913155407181));
#124970=CARTESIAN_POINT('Ctrl Pts',(1.04594200063166,31.2428695406762,123.890150013382));
#124971=CARTESIAN_POINT('Ctrl Pts',(1.04128622263145,31.1932091019712,123.836551452902));
#124972=CARTESIAN_POINT('Ctrl Pts',(1.03862412209428,31.1631558104998,123.806505373867));
#124973=CARTESIAN_POINT('Ctrl Pts',(1.03141968496264,31.0778966978345,123.727549917461));
#124974=CARTESIAN_POINT('Ctrl Pts',(1.0269450135002,31.020542054095,123.68110470999));
#124975=CARTESIAN_POINT('Ctrl Pts',(1.02159392370077,30.9490659496804,123.630686737188));
#124976=CARTESIAN_POINT('Ctrl Pts',(1.02075174300647,30.9377346247631,123.622902052726));
#124977=CARTESIAN_POINT('Ctrl Pts',(1.01538394693864,30.8650963458796,123.574311433637));
#124978=CARTESIAN_POINT('Ctrl Pts',(1.01080592116414,30.8012440445017,123.537473142206));
#124979=CARTESIAN_POINT('Ctrl Pts',(1.00519454109444,30.7241560373828,123.499565133853));
#124980=CARTESIAN_POINT('Ctrl Pts',(1.0043862151566,30.7130788047338,123.494269163991));
#124981=CARTESIAN_POINT('Ctrl Pts',(1.00310910495451,30.6956415117699,123.486168044705));
#124982=CARTESIAN_POINT('Ctrl Pts',(1.00264519684143,30.6893204507745,123.483279322505));
#124983=CARTESIAN_POINT('Ctrl Pts',(1.00177254203339,30.6774588086583,123.477948021258));
#124984=CARTESIAN_POINT('Ctrl Pts',(1.00136436896197,30.6719227467918,123.475495988502));
#124985=CARTESIAN_POINT('Ctrl Pts',(1.0003978307594,30.6588404471331,123.469786674817));
#124986=CARTESIAN_POINT('Ctrl Pts',(0.999837979457446,30.6512833337974,
123.466555000208));
#124987=CARTESIAN_POINT('Ctrl Pts',(0.997952403917785,30.6258895824725,
123.455917351632));
#124988=CARTESIAN_POINT('Ctrl Pts',(0.996613123784626,30.6079488668393,
123.448765946));
#124989=CARTESIAN_POINT('Ctrl Pts',(0.993278775046426,30.5634241947271,
123.43190882006));
#124990=CARTESIAN_POINT('Ctrl Pts',(0.991269110342212,30.5367099625444,
123.422565688461));
#124991=CARTESIAN_POINT('Ctrl Pts',(0.982051976004868,30.414243428537,123.383204761397));
#124992=CARTESIAN_POINT('Ctrl Pts',(0.974671960578939,30.3161367357605,
123.361194794368));
#124993=CARTESIAN_POINT('Ctrl Pts',(0.961505591149596,30.1350541980818,
123.337445376626));
#124994=CARTESIAN_POINT('Ctrl Pts',(0.955686222244953,30.0527732855876,
123.332802905411));
#124995=CARTESIAN_POINT('Ctrl Pts',(0.948712314266306,29.950881064108,123.334608945481));
#124996=CARTESIAN_POINT('Ctrl Pts',(0.947381888523307,29.9312943118038,
123.335301943406));
#124997=CARTESIAN_POINT('Ctrl Pts',(0.945265920871936,29.899915231188,123.336966966903));
#124998=CARTESIAN_POINT('Ctrl Pts',(0.944473613316821,29.8881136146423,
123.337719253745));
#124999=CARTESIAN_POINT('Ctrl Pts',(0.942969084660503,29.8656086898683,
123.33939458038));
#125000=CARTESIAN_POINT('Ctrl Pts',(0.942256214547882,29.8549043950995,
123.340295611091));
#125001=CARTESIAN_POINT('Ctrl Pts',(0.94062262953714,29.8302855494874,123.342607895621));
#125002=CARTESIAN_POINT('Ctrl Pts',(0.939704207962742,29.8163784335405,
123.344090967942));
#125003=CARTESIAN_POINT('Ctrl Pts',(0.936791097864563,29.772076179508,123.349380420096));
#125004=CARTESIAN_POINT('Ctrl Pts',(0.934817112327998,29.7417656123787,
123.353850111493));
#125005=CARTESIAN_POINT('Ctrl Pts',(0.930153404728529,29.6696745211926,
123.366521318667));
#125006=CARTESIAN_POINT('Ctrl Pts',(0.927486320210308,29.6280509444095,
123.375493365516));
#125007=CARTESIAN_POINT('Ctrl Pts',(0.920278729470461,29.5154207041526,
123.404327720658));
#125008=CARTESIAN_POINT('Ctrl Pts',(0.915805598831463,29.445316897942,123.427322621771));
#125009=CARTESIAN_POINT('Ctrl Pts',(0.910429136892259,29.3638109894641,
123.460188086302));
#125010=CARTESIAN_POINT('Ctrl Pts',(0.90956014794745,29.3507245215536,123.465660228814));
#125011=CARTESIAN_POINT('Ctrl Pts',(0.904197065286935,29.2706206185653,
123.500364225849));
#125012=CARTESIAN_POINT('Ctrl Pts',(0.899650350216493,29.2055258592992,
123.533811103953));
#125013=CARTESIAN_POINT('Ctrl Pts',(0.894073721140564,29.1323200037801,
123.577734861494));
#125014=CARTESIAN_POINT('Ctrl Pts',(0.893265536754654,29.1218639504466,
123.584166762371));
#125015=CARTESIAN_POINT('Ctrl Pts',(0.891988617515621,29.1056018994423,
123.594419575672));
#125016=CARTESIAN_POINT('Ctrl Pts',(0.891524757164687,29.0997468694983,
123.598162424464));
#125017=CARTESIAN_POINT('Ctrl Pts',(0.890652489745682,29.0888386116333,
123.605232088714));
#125018=CARTESIAN_POINT('Ctrl Pts',(0.890244659052364,29.0837798704517,
123.608549939243));
#125019=CARTESIAN_POINT('Ctrl Pts',(0.889279155980788,29.0718997256016,
123.616434581438));
#125020=CARTESIAN_POINT('Ctrl Pts',(0.888720001926843,29.0650938859424,
123.6210243158));
#125021=CARTESIAN_POINT('Ctrl Pts',(0.886837125733698,29.0424146041814,
123.636563872111));
#125022=CARTESIAN_POINT('Ctrl Pts',(0.885499870838667,29.0266980624203,
123.647738514862));
#125023=CARTESIAN_POINT('Ctrl Pts',(0.882171241948214,28.9884478451966,
123.675947121282));
#125024=CARTESIAN_POINT('Ctrl Pts',(0.880165303956652,28.9661470653072,
123.693285908564));
#125025=CARTESIAN_POINT('Ctrl Pts',(0.870981480686386,28.8669962839387,
123.774502633823));
#125026=CARTESIAN_POINT('Ctrl Pts',(0.863631571630988,28.7955475808231,
123.844648966041));
#125027=CARTESIAN_POINT('Ctrl Pts',(0.850443421795366,28.6770853776692,
123.983962454178));
#125028=CARTESIAN_POINT('Ctrl Pts',(0.84457590690708,28.628143072863,124.051080766918));
#125029=CARTESIAN_POINT('Ctrl Pts',(0.837556162480866,28.5740591741384,
124.138238258094));
#125030=CARTESIAN_POINT('Ctrl Pts',(0.836224832608533,28.5640143082487,
124.15508243668));
#125031=CARTESIAN_POINT('Ctrl Pts',(0.834108248050821,28.5483945145437,
124.182358728252));
#125032=CARTESIAN_POINT('Ctrl Pts',(0.833316204751512,28.5426294515965,
124.19267922621));
#125033=CARTESIAN_POINT('Ctrl Pts',(0.83181270470213,28.5318417559076,124.212483329035));
#125034=CARTESIAN_POINT('Ctrl Pts',(0.831100593998624,28.5267999751587,
124.221955764274));
#125035=CARTESIAN_POINT('Ctrl Pts',(0.829469518582781,28.5154109610429,
124.243860976518));
#125036=CARTESIAN_POINT('Ctrl Pts',(0.828552834871153,28.5091277034344,
124.256326245983));
#125037=CARTESIAN_POINT('Ctrl Pts',(0.82564862643093,28.4896076228686,124.296293831737));
#125038=CARTESIAN_POINT('Ctrl Pts',(0.823681652593458,28.4769690788082,
124.324082472258));
#125039=CARTESIAN_POINT('Ctrl Pts',(0.819037388497101,28.4486289372169,
124.391232127994));
#125040=CARTESIAN_POINT('Ctrl Pts',(0.816382497106407,28.4336511640838,
124.4308759382));
#125041=CARTESIAN_POINT('Ctrl Pts',(0.80918211559994,28.3967798458641,124.540998420847));
#125042=CARTESIAN_POINT('Ctrl Pts',(0.804704797706259,28.3780306001838,
124.612426844358));
#125043=CARTESIAN_POINT('Ctrl Pts',(0.799406715139897,28.361647415525,124.697474363291));
#125044=CARTESIAN_POINT('Ctrl Pts',(0.798620069040916,28.3593639243095,
124.710113445385));
#125045=CARTESIAN_POINT('Ctrl Pts',(0.793243648806473,28.3447918609733,
124.796465027007));
#125046=CARTESIAN_POINT('Ctrl Pts',(0.78860190390421,28.3373304790088,124.870896631371));
#125047=CARTESIAN_POINT('Ctrl Pts',(0.782919806619903,28.3344883440115,
124.957837733997));
#125048=CARTESIAN_POINT('Ctrl Pts',(0.782111537013232,28.3342228761568,
124.970112129245));
#125049=CARTESIAN_POINT('Ctrl Pts',(0.780834670687406,28.3340196555056,
124.989334509761));
#125050=CARTESIAN_POINT('Ctrl Pts',(0.78037095485496,28.3339896674098,124.996281363847));
#125051=CARTESIAN_POINT('Ctrl Pts',(0.779498674049345,28.3340148542163,
125.009280299266));
#125052=CARTESIAN_POINT('Ctrl Pts',(0.779090682784958,28.3340595598204,
125.015332155614));
#125053=CARTESIAN_POINT('Ctrl Pts',(0.778124739261436,28.3342426536421,
125.029595895695));
#125054=CARTESIAN_POINT('Ctrl Pts',(0.777565303041478,28.3344087937849,
125.037807151429));
#125055=CARTESIAN_POINT('Ctrl Pts',(0.775682254334744,28.3351682259923,
125.065291377494));
#125056=CARTESIAN_POINT('Ctrl Pts',(0.774345125880129,28.3360353760421,
125.084554424996));
#125057=CARTESIAN_POINT('Ctrl Pts',(0.771017386764214,28.3389957014857,
125.131976986764));
#125058=CARTESIAN_POINT('Ctrl Pts',(0.769012240783627,28.3414708173332,
125.160106136882));
#125059=CARTESIAN_POINT('Ctrl Pts',(0.759838698169651,28.3559303565895,
125.287316109779));
#125060=CARTESIAN_POINT('Ctrl Pts',(0.752498754756179,28.3760880869748,
125.385261015734));
#125061=CARTESIAN_POINT('Ctrl Pts',(0.739308435077516,28.4288719284735,
125.560372404515));
#125062=CARTESIAN_POINT('Ctrl Pts',(0.733429820491881,28.4587745338714,
125.638034853079));
#125063=CARTESIAN_POINT('Ctrl Pts',(0.726398187296024,28.5027557609034,
125.730890518723));
#125064=CARTESIAN_POINT('Ctrl Pts',(0.725065564549435,28.5114709305134,
125.748480145571));
#125065=CARTESIAN_POINT('Ctrl Pts',(0.722946813425933,28.5259355536561,
125.776421305557));
#125066=CARTESIAN_POINT('Ctrl Pts',(0.722153891958588,28.5314877927967,
125.786872254876));
#125067=CARTESIAN_POINT('Ctrl Pts',(0.720648632632085,28.5422921512439,
125.806696499387));
#125068=CARTESIAN_POINT('Ctrl Pts',(0.719935641032287,28.547524484198,125.816079836574));
#125069=CARTESIAN_POINT('Ctrl Pts',(0.718302386126289,28.5597725077789,
125.837553667904));
#125070=CARTESIAN_POINT('Ctrl Pts',(0.717384408841334,28.5668503880867,
125.849607901068));
#125071=CARTESIAN_POINT('Ctrl Pts',(0.714475190960476,28.5898920516393,
125.88774236557));
#125072=CARTESIAN_POINT('Ctrl Pts',(0.712504558122011,28.606422982935,125.913473710069));
#125073=CARTESIAN_POINT('Ctrl Pts',(0.70785036019596,28.647578339997,125.973814396864));
#125074=CARTESIAN_POINT('Ctrl Pts',(0.705189286004692,28.6728363165386,
126.007966151164));
#125075=CARTESIAN_POINT('Ctrl Pts',(0.697986956610556,28.7454262638781,
126.09864991108));
#125076=CARTESIAN_POINT('Ctrl Pts',(0.693513284049057,28.7952471826995,
126.153064569791));
#125077=CARTESIAN_POINT('Ctrl Pts',(0.688176206903143,28.858288579375,126.213356590394));
#125078=CARTESIAN_POINT('Ctrl Pts',(0.6873470021138,28.8681834119047,126.222591668937));
#125079=CARTESIAN_POINT('Ctrl Pts',(0.681980499194111,28.9327778016449,
126.28142284487));
#125080=CARTESIAN_POINT('Ctrl Pts',(0.677390966578049,28.99060419533,126.327450592712));
#125081=CARTESIAN_POINT('Ctrl Pts',(0.671766700678755,29.0613820205161,
126.376482187741));
#125082=CARTESIAN_POINT('Ctrl Pts',(0.670957926524988,29.0715573650559,
126.38336588668));
#125083=CARTESIAN_POINT('Ctrl Pts',(0.669680022733904,29.0876111068642,
126.393969469991));
#125084=CARTESIAN_POINT('Ctrl Pts',(0.66921576842484,29.0934384966343,126.397766293706));
#125085=CARTESIAN_POINT('Ctrl Pts',(0.668341896917066,29.104394164388,126.404807107438));
#125086=CARTESIAN_POINT('Ctrl Pts',(0.66793284828064,29.1095166161575,126.408059714717));
#125087=CARTESIAN_POINT('Ctrl Pts',(0.666963659612877,29.1216415317055,
126.415666059009));
#125088=CARTESIAN_POINT('Ctrl Pts',(0.666402022771516,29.1286586857989,
126.419995879042));
#125089=CARTESIAN_POINT('Ctrl Pts',(0.664508563905053,29.1522946861015,
126.434338925018));
#125090=CARTESIAN_POINT('Ctrl Pts',(0.663163099641827,29.1690555728924,
126.444113475416));
#125091=CARTESIAN_POINT('Ctrl Pts',(0.659810683398703,29.2108201689025,
126.467501814608));
#125092=CARTESIAN_POINT('Ctrl Pts',(0.657789009349254,29.2360090062294,
126.480771407286));
#125093=CARTESIAN_POINT('Ctrl Pts',(0.6484590393188,29.3527353388503,126.538492228506));
#125094=CARTESIAN_POINT('Ctrl Pts',(0.640976122976484,29.4478866494741,
126.575144875196));
#125095=CARTESIAN_POINT('Ctrl Pts',(0.627877905708863,29.6228926231761,
126.624736398472));
#125096=CARTESIAN_POINT('Ctrl Pts',(0.622216764615846,29.7014811773404,
126.640996111611));
#125097=CARTESIAN_POINT('Ctrl Pts',(0.615395910433173,29.8003033203065,
126.654103545578));
#125098=CARTESIAN_POINT('Ctrl Pts',(0.614070380700639,29.819705101918,126.656330615932));
#125099=CARTESIAN_POINT('Ctrl Pts',(0.611959571554278,29.8509076833447,
126.659357468475));
#125100=CARTESIAN_POINT('Ctrl Pts',(0.611167610191796,29.8626851432515,
126.660373563277));
#125101=CARTESIAN_POINT('Ctrl Pts',(0.609662074371933,29.8852046054757,
126.662075163477));
#125102=CARTESIAN_POINT('Ctrl Pts',(0.608947867417984,29.8959443377139,
126.662782084356));
#125103=CARTESIAN_POINT('Ctrl Pts',(0.607308815025502,29.9207169894568,
126.66417173663));
#125104=CARTESIAN_POINT('Ctrl Pts',(0.606386297959672,29.9347533275941,
126.664781143722));
#125105=CARTESIAN_POINT('Ctrl Pts',(0.603449792534127,29.9797120701522,
126.666163588421));
#125106=CARTESIAN_POINT('Ctrl Pts',(0.601456950722025,30.0106499918481,
126.666253124582));
#125107=CARTESIAN_POINT('Ctrl Pts',(0.596740447039811,30.0846742076842,
126.664405315339));
#125108=CARTESIAN_POINT('Ctrl Pts',(0.594040121294101,30.1277182675217,
126.661656767285));
#125109=CARTESIAN_POINT('Ctrl Pts',(0.586842660233912,30.2432627289797,
126.649761697095));
#125110=CARTESIAN_POINT('Ctrl Pts',(0.58240957196995,30.3153468908837,126.637512470602));
#125111=CARTESIAN_POINT('Ctrl Pts',(0.577016471332671,30.4010959915034,
126.617067228247));
#125112=CARTESIAN_POINT('Ctrl Pts',(0.576090424704046,30.4157487919857,
126.613362125855));
#125113=CARTESIAN_POINT('Ctrl Pts',(0.570735612060012,30.4999191911044,
126.59085601265));
#125114=CARTESIAN_POINT('Ctrl Pts',(0.566253895149197,30.5682016592702,
126.567764755207));
#125115=CARTESIAN_POINT('Ctrl Pts',(0.560749370323946,30.6461126659113,
126.535657840446));
#125116=CARTESIAN_POINT('Ctrl Pts',(0.559941500548798,30.6574057464283,
126.530857355476));
#125117=CARTESIAN_POINT('Ctrl Pts',(0.558664973549813,30.6750082834363,
126.523144147176));
#125118=CARTESIAN_POINT('Ctrl Pts',(0.558201186201658,30.6813545573832,
126.52031583513));
#125119=CARTESIAN_POINT('Ctrl Pts',(0.557371232117855,30.6926199447267,
126.515210544299));
#125120=CARTESIAN_POINT('Ctrl Pts',(0.557006011680592,30.6975458987382,
126.512949139164));
#125121=CARTESIAN_POINT('Ctrl Pts',(0.556112857223938,30.7095166972507,
126.507382701346));
#125122=CARTESIAN_POINT('Ctrl Pts',(0.555583406191478,30.7165494215158,
126.504052350291));
#125123=CARTESIAN_POINT('Ctrl Pts',(0.553889413758413,30.7388581186891,
126.49329607934));
#125124=CARTESIAN_POINT('Ctrl Pts',(0.552714545376632,30.7540434219739,
126.485686024027));
#125125=CARTESIAN_POINT('Ctrl Pts',(0.549867236056007,30.7902234496698,
126.466857003386));
#125126=CARTESIAN_POINT('Ctrl Pts',(0.548184731357374,30.8110989331917,
126.455417799357));
#125127=CARTESIAN_POINT('Ctrl Pts',(0.541418138772753,30.893316645787,126.40804648008));
#125128=CARTESIAN_POINT('Ctrl Pts',(0.536227271511378,30.9525747682982,
126.36865260101));
#125129=CARTESIAN_POINT('Ctrl Pts',(0.522908170011819,31.0981049568245,
126.257865285868));
#125130=CARTESIAN_POINT('Ctrl Pts',(0.514852835877638,31.1800462963872,
126.181337565979));
#125131=CARTESIAN_POINT('Ctrl Pts',(0.505625127887404,31.2682350069771,
126.080565781917));
#125132=CARTESIAN_POINT('Ctrl Pts',(0.504118606412817,31.2824294126384,
126.063681025808));
#125133=CARTESIAN_POINT('Ctrl Pts',(0.501705780468279,31.3048223410172,
126.035943712146));
#125134=CARTESIAN_POINT('Ctrl Pts',(0.500791124888508,31.3132302114156,
126.025264427983));
#125135=CARTESIAN_POINT('Ctrl Pts',(0.499169604700596,31.3279868665607,
126.006041814014));
#125136=CARTESIAN_POINT('Ctrl Pts',(0.498460762918687,31.3343861512601,
125.997538399112));
#125137=CARTESIAN_POINT('Ctrl Pts',(0.496964616802881,31.3477804158328,
125.979380451607));
#125138=CARTESIAN_POINT('Ctrl Pts',(0.496178166579844,31.3547541564008,
125.969710939655));
#125139=CARTESIAN_POINT('Ctrl Pts',(0.494065885852746,31.3732967140546,
125.943410056116));
#125140=CARTESIAN_POINT('Ctrl Pts',(0.49274763566798,31.384667188492,125.926640833353));
#125141=CARTESIAN_POINT('Ctrl Pts',(0.489846976954011,31.4092054278564,
125.888991108142));
#125142=CARTESIAN_POINT('Ctrl Pts',(0.488270089023461,31.4222208209061,
125.868016796208));
#125143=CARTESIAN_POINT('Ctrl Pts',(0.483300369326884,31.462104782962,125.800436684676));
#125144=CARTESIAN_POINT('Ctrl Pts',(0.479963116353044,31.4871856101745,
125.752813978256));
#125145=CARTESIAN_POINT('Ctrl Pts',(0.473803296962714,31.5295458105348,
125.661968556735));
#125146=CARTESIAN_POINT('Ctrl Pts',(0.470975552750166,31.5474010448887,
125.619081377102));
#125147=CARTESIAN_POINT('Ctrl Pts',(0.468139959767684,31.5634400089539,
125.575509633631));
#125148=CARTESIAN_POINT('Origin',(5.,-30.,125.));
#125149=CARTESIAN_POINT('',(1.32020507860662,-28.3340002656058,125.000940743489));
#125150=CARTESIAN_POINT('Ctrl Pts',(0.659203971007256,-28.4365599837785,
125.575509613888));
#125151=CARTESIAN_POINT('Ctrl Pts',(0.659952788000284,-28.4405111228567,
125.586243351075));
#125152=CARTESIAN_POINT('Ctrl Pts',(0.660707178275404,-28.4445725592891,
125.596935744733));
#125153=CARTESIAN_POINT('Ctrl Pts',(0.661913431714573,-28.4511870645999,
125.613823574029));
#125154=CARTESIAN_POINT('Ctrl Pts',(0.662361167616503,-28.4536680605702,
125.620047109534));
#125155=CARTESIAN_POINT('Ctrl Pts',(0.663223012937918,-28.4584912126697,
125.631936903649));
#125156=CARTESIAN_POINT('Ctrl Pts',(0.663636763814656,-28.4608272048218,
125.63760543687));
#125157=CARTESIAN_POINT('Ctrl Pts',(0.664644178966683,-28.4665654621471,
125.651314629528));
#125158=CARTESIAN_POINT('Ctrl Pts',(0.665239704446657,-28.4699997223272,
125.659341618913));
#125159=CARTESIAN_POINT('Ctrl Pts',(0.66738747270351,-28.4825410329116,
125.688029126372));
#125160=CARTESIAN_POINT('Ctrl Pts',(0.668958672319821,-28.4920043483959,
125.708530018805));
#125161=CARTESIAN_POINT('Ctrl Pts',(0.680709757870277,-28.5650825441696,
125.858742966811));
#125162=CARTESIAN_POINT('Ctrl Pts',(0.691454103024878,-28.6449126402584,
125.979882323236));
#125163=CARTESIAN_POINT('Ctrl Pts',(0.70635313264515,-28.7812993357348,
126.137733317166));
#125164=CARTESIAN_POINT('Ctrl Pts',(0.710848350620454,-28.8259961962093,
126.183801205807));
#125165=CARTESIAN_POINT('Ctrl Pts',(0.716500666851209,-28.8869331488791,
126.239751416357));
#125166=CARTESIAN_POINT('Ctrl Pts',(0.717760854930286,-28.9008324984542,
126.252091147451));
#125167=CARTESIAN_POINT('Ctrl Pts',(0.71979271624179,-28.9237476457165,
126.271759300105));
#125168=CARTESIAN_POINT('Ctrl Pts',(0.720570222738542,-28.9326383916829,
126.279230259336));
#125169=CARTESIAN_POINT('Ctrl Pts',(0.722064413641303,-28.9499575574367,
126.293477404711));
#125170=CARTESIAN_POINT('Ctrl Pts',(0.72278156378737,-28.9583752379163,
126.300265662119));
#125171=CARTESIAN_POINT('Ctrl Pts',(0.724451097211425,-28.9782141433035,
126.315948018525));
#125172=CARTESIAN_POINT('Ctrl Pts',(0.725400839598706,-28.9896864893521,
126.324776266559));
#125173=CARTESIAN_POINT('Ctrl Pts',(0.728531633613869,-29.0281075714805,
126.35355279639));
#125174=CARTESIAN_POINT('Ctrl Pts',(0.730687222715632,-29.0555443061314,
126.372837845898));
#125175=CARTESIAN_POINT('Ctrl Pts',(0.735883474388284,-29.1238625039574,
126.417839831529));
#125176=CARTESIAN_POINT('Ctrl Pts',(0.738893422057637,-29.1653162225518,
126.442633078843));
#125177=CARTESIAN_POINT('Ctrl Pts',(0.745995229778165,-29.2665646144079,
126.497361747878));
#125178=CARTESIAN_POINT('Ctrl Pts',(0.750051113498307,-29.3271963442272,
126.525567127607));
#125179=CARTESIAN_POINT('Ctrl Pts',(0.758902099603246,-29.4617012585901,
126.578555085847));
#125180=CARTESIAN_POINT('Ctrl Pts',(0.7636986361377,-29.5359423153221,126.601951721544));
#125181=CARTESIAN_POINT('Ctrl Pts',(0.769796848439415,-29.6274575112708,
126.623895373793));
#125182=CARTESIAN_POINT('Ctrl Pts',(0.770868277232152,-29.6434343580739,
126.627478105787));
#125183=CARTESIAN_POINT('Ctrl Pts',(0.772462104297826,-29.6670004311443,
126.632399036367));
#125184=CARTESIAN_POINT('Ctrl Pts',(0.772974774531412,-29.6745508365018,
126.633921100585));
#125185=CARTESIAN_POINT('Ctrl Pts',(0.773892722424834,-29.6880106386339,
126.636537428563));
#125186=CARTESIAN_POINT('Ctrl Pts',(0.774296847948697,-29.6939157912203,
126.637652152166));
#125187=CARTESIAN_POINT('Ctrl Pts',(0.775196689044128,-29.7070180362633,
126.640052138043));
#125188=CARTESIAN_POINT('Ctrl Pts',(0.775693213989008,-29.7142175309546,
126.641321973861));
#125189=CARTESIAN_POINT('Ctrl Pts',(0.777172093011416,-29.7355785857425,
126.644944802257));
#125190=CARTESIAN_POINT('Ctrl Pts',(0.778161427636895,-29.7497620454105,
126.647162110524));
#125191=CARTESIAN_POINT('Ctrl Pts',(0.780480236995961,-29.7827985346632,
126.65189019919));
#125192=CARTESIAN_POINT('Ctrl Pts',(0.781815621837031,-29.8016692122806,
126.65426193198));
#125193=CARTESIAN_POINT('Ctrl Pts',(0.786590539582907,-29.8687302437716,
126.661526510729));
#125194=CARTESIAN_POINT('Ctrl Pts',(0.790086567261338,-29.9170867503672,
126.664640173597));
#125195=CARTESIAN_POINT('Ctrl Pts',(0.801961053567282,-30.0805910286992,
126.66802611696));
#125196=CARTESIAN_POINT('Ctrl Pts',(0.810378370068741,-30.1956285135019,
126.658475723849));
#125197=CARTESIAN_POINT('Ctrl Pts',(0.821474111727933,-30.3507455707969,
126.629220121835));
#125198=CARTESIAN_POINT('Ctrl Pts',(0.824431877616766,-30.392404504127,
126.61969130751));
#125199=CARTESIAN_POINT('Ctrl Pts',(0.828447746977999,-30.4493779111564,
126.604331850906));
#125200=CARTESIAN_POINT('Ctrl Pts',(0.829548609789823,-30.4650388247494,
126.599862531299));
#125201=CARTESIAN_POINT('Ctrl Pts',(0.831314989341577,-30.4902288801112,
126.592272621963));
#125202=CARTESIAN_POINT('Ctrl Pts',(0.831985084216166,-30.4997994618681,
126.589294485942));
#125203=CARTESIAN_POINT('Ctrl Pts',(0.8333797683235,-30.5197458775554,126.582889638024));
#125204=CARTESIAN_POINT('Ctrl Pts',(0.834103792777535,-30.5301160775566,
126.579446845381));
#125205=CARTESIAN_POINT('Ctrl Pts',(0.835825154396519,-30.5548019021225,
126.570980901244));
#125206=CARTESIAN_POINT('Ctrl Pts',(0.836819341079492,-30.5690844185817,
126.565863688903));
#125207=CARTESIAN_POINT('Ctrl Pts',(0.840285116630252,-30.6189326836981,
126.547231649304));
#125208=CARTESIAN_POINT('Ctrl Pts',(0.842722831317173,-30.6541050929578,
126.532693810843));
#125209=CARTESIAN_POINT('Ctrl Pts',(0.84879558111837,-30.7415548564192,
126.492988753184));
#125210=CARTESIAN_POINT('Ctrl Pts',(0.852383199621562,-30.7930735250193,
126.466272193781));
#125211=CARTESIAN_POINT('Ctrl Pts',(0.862670320436195,-30.9377214396954,
126.381401759193));
#125212=CARTESIAN_POINT('Ctrl Pts',(0.869255113445024,-31.0266215752484,
126.316676180117));
#125213=CARTESIAN_POINT('Ctrl Pts',(0.878120565810813,-31.1309131168693,
126.223720711109));
#125214=CARTESIAN_POINT('Ctrl Pts',(0.880052767804596,-31.1527737991446,
126.203149684368));
#125215=CARTESIAN_POINT('Ctrl Pts',(0.882681527470541,-31.1811541142419,
126.174959908517));
#125216=CARTESIAN_POINT('Ctrl Pts',(0.883342505382893,-31.1881791612443,
126.167855340709));
#125217=CARTESIAN_POINT('Ctrl Pts',(0.884391493103859,-31.1991454228612,
126.156563579617));
#125218=CARTESIAN_POINT('Ctrl Pts',(0.884776261322163,-31.2031297238217,
126.152418293851));
#125219=CARTESIAN_POINT('Ctrl Pts',(0.885579680345145,-31.2113680472079,
126.143757814347));
#125220=CARTESIAN_POINT('Ctrl Pts',(0.885998615477635,-31.2156183957721,
126.139239393033));
#125221=CARTESIAN_POINT('Ctrl Pts',(0.887038546669201,-31.2260595587147,
126.128014742525));
#125222=CARTESIAN_POINT('Ctrl Pts',(0.887661695162183,-31.2322206315728,
126.121281234328));
#125223=CARTESIAN_POINT('Ctrl Pts',(0.890033938164367,-31.2553273030339,
126.095607254887));
#125224=CARTESIAN_POINT('Ctrl Pts',(0.891807350696535,-31.2718931466652,
126.076331523339));
#125225=CARTESIAN_POINT('Ctrl Pts',(0.896555364268742,-31.314556022892,
126.024329088885));
#125226=CARTESIAN_POINT('Ctrl Pts',(0.899562943419358,-31.3398712180821,
125.990985519493));
#125227=CARTESIAN_POINT('Ctrl Pts',(0.912077654603941,-31.4391301885819,
125.849482640872));
#125228=CARTESIAN_POINT('Ctrl Pts',(0.921693463471601,-31.5014593082718,
125.733720494547));
#125229=CARTESIAN_POINT('Ctrl Pts',(0.933545634833785,-31.5636376122723,
125.576244937981));
#125230=CARTESIAN_POINT('Ctrl Pts',(0.936187861162518,-31.5764634633483,
125.5401705015));
#125231=CARTESIAN_POINT('Ctrl Pts',(0.939851490197423,-31.5927588579299,
125.488793652399));
#125232=CARTESIAN_POINT('Ctrl Pts',(0.94090642416339,-31.5972720388305,
125.473837606134));
#125233=CARTESIAN_POINT('Ctrl Pts',(0.942685651888065,-31.6045755080865,
125.448343833051));
#125234=CARTESIAN_POINT('Ctrl Pts',(0.943413413033034,-31.6074738814749,
125.43783842213));
#125235=CARTESIAN_POINT('Ctrl Pts',(0.94488397245525,-31.6131478112168,
125.416456619934));
#125236=CARTESIAN_POINT('Ctrl Pts',(0.945626530187649,-31.6159169481621,
125.405579097346));
#125237=CARTESIAN_POINT('Ctrl Pts',(0.947467337420167,-31.6225397421857,
125.378418731322));
#125238=CARTESIAN_POINT('Ctrl Pts',(0.948561227260991,-31.6262584857579,
125.362104020899));
#125239=CARTESIAN_POINT('Ctrl Pts',(0.952916961696848,-31.6401793689172,
125.29648365487));
#125240=CARTESIAN_POINT('Ctrl Pts',(0.956115937444605,-31.6483904627062,
125.246780360908));
#125241=CARTESIAN_POINT('Ctrl Pts',(0.965022166420443,-31.6652039047736,
125.105427193662));
#125242=CARTESIAN_POINT('Ctrl Pts',(0.970592851241548,-31.6684849518826,
125.013333446826));
#125243=CARTESIAN_POINT('Ctrl Pts',(0.976476273650288,-31.6639519553479,
124.917314311575));
#125244=CARTESIAN_POINT('Ctrl Pts',(0.976728993283109,-31.6637420180873,
124.913192570066));
#125245=CARTESIAN_POINT('Ctrl Pts',(0.981942939262595,-31.6590975300757,
124.828222541442));
#125246=CARTESIAN_POINT('Ctrl Pts',(0.986950336421848,-31.648790639554,
124.747813445692));
#125247=CARTESIAN_POINT('Ctrl Pts',(0.993043460817581,-31.6302260786282,
124.656384872667));
#125248=CARTESIAN_POINT('Ctrl Pts',(0.993856149516315,-31.627635035567,
124.644313913594));
#125249=CARTESIAN_POINT('Ctrl Pts',(0.995138705276603,-31.6233726973217,
124.62547949956));
#125250=CARTESIAN_POINT('Ctrl Pts',(0.99560362837449,-31.6217926611739,
124.618695555468));
#125251=CARTESIAN_POINT('Ctrl Pts',(0.996477068376249,-31.6187604666437,
124.606036580946));
#125252=CARTESIAN_POINT('Ctrl Pts',(0.996884998644199,-31.6173187788029,
124.600159297963));
#125253=CARTESIAN_POINT('Ctrl Pts',(0.997849466516603,-31.613850024864,
124.586344084224));
#125254=CARTESIAN_POINT('Ctrl Pts',(0.998407471292178,-31.6117963913303,
124.578413110631));
#125255=CARTESIAN_POINT('Ctrl Pts',(1.00028027613092,-31.604746086708,124.55199004273));
#125256=CARTESIAN_POINT('Ctrl Pts',(1.00160839860681,-31.599489197655,124.533569776379));
#125257=CARTESIAN_POINT('Ctrl Pts',(1.00490875905489,-31.585774838564,124.488475759881));
#125258=CARTESIAN_POINT('Ctrl Pts',(1.0068952458719,-31.576960836835,124.461917078837));
#125259=CARTESIAN_POINT('Ctrl Pts',(1.01590761029936,-31.53433686381,124.34354058279));
#125260=CARTESIAN_POINT('Ctrl Pts',(1.02310053201971,-31.4931467962678,
124.254586388757));
#125261=CARTESIAN_POINT('Ctrl Pts',(1.03631690639912,-31.4018999306265,
124.095841930695));
#125262=CARTESIAN_POINT('Ctrl Pts',(1.04235452313837,-31.35379455986,124.025284881628));
#125263=CARTESIAN_POINT('Ctrl Pts',(1.04953835166265,-31.2881908987373,
123.943350836977));
#125264=CARTESIAN_POINT('Ctrl Pts',(1.05087445908436,-31.2756197223439,
123.928208216638));
#125265=CARTESIAN_POINT('Ctrl Pts',(1.05299729466008,-31.2550575658085,
123.904314475793));
#125266=CARTESIAN_POINT('Ctrl Pts',(1.05379086698088,-31.2472367401788,
123.895420085311));
#125267=CARTESIAN_POINT('Ctrl Pts',(1.05529647517862,-31.2321449294111,
123.878621299215));
#125268=CARTESIAN_POINT('Ctrl Pts',(1.05600917415139,-31.2248910952324,
123.87070237241));
#125269=CARTESIAN_POINT('Ctrl Pts',(1.05764051056466,-31.208037317787,123.852656754201));
#125270=CARTESIAN_POINT('Ctrl Pts',(1.05855687764223,-31.1983856230341,
123.842579331887));
#125271=CARTESIAN_POINT('Ctrl Pts',(1.06145573908754,-31.1672774503254,
123.810905361708));
#125272=CARTESIAN_POINT('Ctrl Pts',(1.06341782363415,-31.1453544374955,
123.789774358659));
#125273=CARTESIAN_POINT('Ctrl Pts',(1.06804741290466,-31.0916878542415,
123.740811947588));
#125274=CARTESIAN_POINT('Ctrl Pts',(1.07069274749435,-31.059441319136,123.713562521073));
#125275=CARTESIAN_POINT('Ctrl Pts',(1.07800220401919,-30.9665882968917,
123.640960710175));
#125276=CARTESIAN_POINT('Ctrl Pts',(1.08259225305527,-30.9038778200993,
123.598470128191));
#125277=CARTESIAN_POINT('Ctrl Pts',(1.08786899299986,-30.829368119352,123.555072289489));
#125278=CARTESIAN_POINT('Ctrl Pts',(1.08851612439677,-30.8201906482293,
123.549843158828));
#125279=CARTESIAN_POINT('Ctrl Pts',(1.09379079653486,-30.7451279522311,
123.508014515775));
#125280=CARTESIAN_POINT('Ctrl Pts',(1.09847029713675,-30.6768861982096,
123.475841703367));
#125281=CARTESIAN_POINT('Ctrl Pts',(1.10419462993725,-30.5952687498334,
123.443927356345));
#125282=CARTESIAN_POINT('Ctrl Pts',(1.10500348888736,-30.583777257668,123.439579848731));
#125283=CARTESIAN_POINT('Ctrl Pts',(1.10628133065542,-30.5657093295162,
123.432971826538));
#125284=CARTESIAN_POINT('Ctrl Pts',(1.10674542943947,-30.5591647685032,
123.430624614947));
#125285=CARTESIAN_POINT('Ctrl Pts',(1.10761827480739,-30.5468936415534,
123.426310066122));
#125286=CARTESIAN_POINT('Ctrl Pts',(1.10802644567243,-30.5411707958751,
123.42433289424));
#125287=CARTESIAN_POINT('Ctrl Pts',(1.10899281456034,-30.5276565998648,
123.419746214365));
#125288=CARTESIAN_POINT('Ctrl Pts',(1.10955249703968,-30.5198565825867,
123.417163103519));
#125289=CARTESIAN_POINT('Ctrl Pts',(1.11143696502406,-30.493672798988,123.408706302729));
#125290=CARTESIAN_POINT('Ctrl Pts',(1.11277529150004,-30.4752068903733,
123.403094619134));
#125291=CARTESIAN_POINT('Ctrl Pts',(1.11610669889285,-30.4294617379501,
123.39005658859));
#125292=CARTESIAN_POINT('Ctrl Pts',(1.11811435147819,-30.4020834479405,
123.383001579213));
#125293=CARTESIAN_POINT('Ctrl Pts',(1.12731205982333,-30.2770045639129,
123.354143337078));
#125294=CARTESIAN_POINT('Ctrl Pts',(1.13467424331126,-30.177639681118,123.340475888893));
#125295=CARTESIAN_POINT('Ctrl Pts',(1.14785029236992,-29.9951033935346,
123.331959099954));
#125296=CARTESIAN_POINT('Ctrl Pts',(1.15369509473113,-29.912376869125,123.334253827135));
#125297=CARTESIAN_POINT('Ctrl Pts',(1.16069370150931,-29.8106432788171,
123.344679917503));
#125298=CARTESIAN_POINT('Ctrl Pts',(1.16202503416068,-29.7911718099492,
123.347023476445));
#125299=CARTESIAN_POINT('Ctrl Pts',(1.16414212867657,-29.760028697994,123.351330935507));
#125300=CARTESIAN_POINT('Ctrl Pts',(1.16493466980795,-29.748329221065,123.353076279386));
#125301=CARTESIAN_POINT('Ctrl Pts',(1.16643944864941,-29.7260421986319,
123.356644131116));
#125302=CARTESIAN_POINT('Ctrl Pts',(1.16715233762151,-29.71545180378,123.358444724667));
#125303=CARTESIAN_POINT('Ctrl Pts',(1.16878569430159,-29.6911191792949,
123.36282434819));
#125304=CARTESIAN_POINT('Ctrl Pts',(1.1697038713505,-29.6773903968712,123.365474215564));
#125305=CARTESIAN_POINT('Ctrl Pts',(1.17261508210444,-29.6337207185938,
123.374474795799));
#125306=CARTESIAN_POINT('Ctrl Pts',(1.1745874499727,-29.6039197497773,123.381478042994));
#125307=CARTESIAN_POINT('Ctrl Pts',(1.17924652379521,-29.5332248658153,
123.400161146468));
#125308=CARTESIAN_POINT('Ctrl Pts',(1.18191065371257,-29.4925516225319,
123.412593338978));
#125309=CARTESIAN_POINT('Ctrl Pts',(1.18911624590242,-29.3827833289793,
123.450796168208));
#125310=CARTESIAN_POINT('Ctrl Pts',(1.19359016368393,-29.3148534168532,
123.479617332439));
#125311=CARTESIAN_POINT('Ctrl Pts',(1.20304885159216,-29.1768385354342,
123.549308360876));
#125312=CARTESIAN_POINT('Ctrl Pts',(1.20802904347214,-29.1073822496287,
123.590982098273));
#125313=CARTESIAN_POINT('Ctrl Pts',(1.21433268730004,-29.0278205573635,
123.646969241793));
#125314=CARTESIAN_POINT('Ctrl Pts',(1.2154060785304,-29.0145457307697,123.65660693198));
#125315=CARTESIAN_POINT('Ctrl Pts',(1.21700217383662,-28.995247313429,123.671057778482));
#125316=CARTESIAN_POINT('Ctrl Pts',(1.21751510320364,-28.9891109113589,
123.675719578817));
#125317=CARTESIAN_POINT('Ctrl Pts',(1.21841728125938,-28.9784367671974,
123.683946103684));
#125318=CARTESIAN_POINT('Ctrl Pts',(1.2188052321189,-28.9738848689808,123.687492082831));
#125319=CARTESIAN_POINT('Ctrl Pts',(1.21920075568198,-28.9692831202466,
123.691115466765));
#125320=CARTESIAN_POINT('Ctrl Pts',(1.21920662355708,-28.9692148586174,
123.691169224134));
#125321=CARTESIAN_POINT('Ctrl Pts',(1.21922178435846,-28.9690385135907,
123.691308121645));
#125322=CARTESIAN_POINT('Ctrl Pts',(1.2192310778624,-28.9689304364423,123.69139326991));
#125323=CARTESIAN_POINT('Ctrl Pts',(1.21924924690886,-28.9687191848912,
123.691559746245));
#125324=CARTESIAN_POINT('Ctrl Pts',(1.21925812235001,-28.9686160097637,
123.691641072968));
#125325=CARTESIAN_POINT('Ctrl Pts',(1.21927548947839,-28.9684141589893,
123.691800218461));
#125326=CARTESIAN_POINT('Ctrl Pts',(1.21928398111029,-28.9683154823172,
123.691878036357));
#125327=CARTESIAN_POINT('Ctrl Pts',(1.21930061129616,-28.9681222670639,
123.692030444249));
#125328=CARTESIAN_POINT('Ctrl Pts',(1.2193087497812,-28.9680277278153,123.692105033291));
#125329=CARTESIAN_POINT('Ctrl Pts',(1.21932470114206,-28.9678424639905,
123.692251234289));
#125330=CARTESIAN_POINT('Ctrl Pts',(1.21933251397122,-28.9677517386588,
123.692322845532));
#125331=CARTESIAN_POINT('Ctrl Pts',(1.21934783878755,-28.9675738112311,
123.692463317115));
#125332=CARTESIAN_POINT('Ctrl Pts',(1.2193553507183,-28.9674866086396,123.692532176684));
#125333=CARTESIAN_POINT('Ctrl Pts',(1.21937009609573,-28.9673154637501,
123.692667349129));
#125334=CARTESIAN_POINT('Ctrl Pts',(1.21937732948593,-28.9672315210839,
123.692733661261));
#125335=CARTESIAN_POINT('Ctrl Pts',(1.21939153797072,-28.9670666587335,
123.692863923251));
#125336=CARTESIAN_POINT('Ctrl Pts',(1.21939851303747,-28.9669857384585,
123.692927872652));
#125337=CARTESIAN_POINT('Ctrl Pts',(1.21941222328814,-28.9668267045739,
123.693053577405));
#125338=CARTESIAN_POINT('Ctrl Pts',(1.21941895842297,-28.9667485907153,
123.693115332125));
#125339=CARTESIAN_POINT('Ctrl Pts',(1.21943220545572,-28.9665949741827,
123.693236799614));
#125340=CARTESIAN_POINT('Ctrl Pts',(1.21943871735016,-28.966519470814,123.693296512188));
#125341=CARTESIAN_POINT('Ctrl Pts',(1.21945153321689,-28.9663708955148,
123.693414035341));
#125342=CARTESIAN_POINT('Ctrl Pts',(1.2194578371461,-28.9662978234217,123.693471845378));
#125343=CARTESIAN_POINT('Ctrl Pts',(1.21947025101568,-28.9661539472047,
123.693585690804));
#125344=CARTESIAN_POINT('Ctrl Pts',(1.21947636092835,-28.9660831428042,
123.693641725804));
#125345=CARTESIAN_POINT('Ctrl Pts',(1.21948839957223,-28.9659436517833,
123.693752138227));
#125346=CARTESIAN_POINT('Ctrl Pts',(1.2194943282726,-28.9658749649792,123.693806515244));
#125347=CARTESIAN_POINT('Ctrl Pts',(1.2195060161932,-28.9657395719821,123.693913718671));
#125348=CARTESIAN_POINT('Ctrl Pts',(1.21951177541156,-28.9656728653199,
123.693966544952));
#125349=CARTESIAN_POINT('Ctrl Pts',(1.21952313526533,-28.9655413049327,
123.694070746539));
#125350=CARTESIAN_POINT('Ctrl Pts',(1.21952873585499,-28.9654764512913,
123.694122121325));
#125351=CARTESIAN_POINT('Ctrl Pts',(1.21953978836484,-28.965348480826,123.694223510567));
#125352=CARTESIAN_POINT('Ctrl Pts',(1.21954524028525,-28.9652853635928,
123.694273524933));
#125353=CARTESIAN_POINT('Ctrl Pts',(1.21955600474592,-28.965160757194,123.694372278287));
#125354=CARTESIAN_POINT('Ctrl Pts',(1.21956131725224,-28.9650992680499,
123.69442101688));
#125355=CARTESIAN_POINT('Ctrl Pts',(1.21957181139231,-28.9649778182569,
123.694517296493));
#125356=CARTESIAN_POINT('Ctrl Pts',(1.21957699302637,-28.9649178572651,
123.694564837441));
#125357=CARTESIAN_POINT('Ctrl Pts',(1.21958723333976,-28.9647993711441,
123.694658794186));
#125358=CARTESIAN_POINT('Ctrl Pts',(1.21959229202362,-28.9647408456518,
123.694705209955));
#125359=CARTESIAN_POINT('Ctrl Pts',(1.21960229387362,-28.964625143565,123.694796984378));
#125360=CARTESIAN_POINT('Ctrl Pts',(1.21960723700523,-28.9645679670848,
123.69484234265));
#125361=CARTESIAN_POINT('Ctrl Pts',(1.21961701460404,-28.9644548829029,
123.694932064776));
#125362=CARTESIAN_POINT('Ctrl Pts',(1.2196218490546,-28.9643989751315,123.694976428418));
#125363=CARTESIAN_POINT('Ctrl Pts',(1.21963141568774,-28.9642883536169,
123.695064219808));
#125364=CARTESIAN_POINT('Ctrl Pts',(1.21963614786677,-28.9642336396734,
123.695107647468));
#125365=CARTESIAN_POINT('Ctrl Pts',(1.21964551593236,-28.9641253360074,
123.695193621574));
#125366=CARTESIAN_POINT('Ctrl Pts',(1.21965015181907,-28.9640717460609,
123.69523616797));
#125367=CARTESIAN_POINT('Ctrl Pts',(1.21965933297478,-28.9639656241284,
123.69532043148));
#125368=CARTESIAN_POINT('Ctrl Pts',(1.21966387820487,-28.9639130923872,
123.695362148191));
#125369=CARTESIAN_POINT('Ctrl Pts',(1.21967288326782,-28.9638090259192,
123.695444800108));
#125370=CARTESIAN_POINT('Ctrl Pts',(1.21967734309576,-28.9637574910599,
123.695485735227));
#125371=CARTESIAN_POINT('Ctrl Pts',(1.21968618227514,-28.9636553609314,
123.695566869));
#125372=CARTESIAN_POINT('Ctrl Pts',(1.21969056163286,-28.9636047654146,
123.695607067673));
#125373=CARTESIAN_POINT('Ctrl Pts',(1.21969924454946,-28.963504459408,123.695686771376));
#125374=CARTESIAN_POINT('Ctrl Pts',(1.2197035480933,-28.9634547489301,123.69572627623));
#125375=CARTESIAN_POINT('Ctrl Pts',(1.21971208379459,-28.9633561615505,
123.695804632694));
#125376=CARTESIAN_POINT('Ctrl Pts',(1.21971631593383,-28.9633072847094,
123.695843484101));
#125377=CARTESIAN_POINT('Ctrl Pts',(1.21972471282815,-28.9632103179353,
123.695920570311));
#125378=CARTESIAN_POINT('Ctrl Pts',(1.21972887764312,-28.9631622271718,
123.695958805631));
#125379=CARTESIAN_POINT('Ctrl Pts',(1.21973714391899,-28.9630667856039,
123.696034696573));
#125380=CARTESIAN_POINT('Ctrl Pts',(1.21974124535099,-28.9630194350046,
123.696072351899));
#125381=CARTESIAN_POINT('Ctrl Pts',(1.22028393924562,-28.9567546350548,
123.701054959689));
#125382=CARTESIAN_POINT('Ctrl Pts',(1.22082558548529,-28.9505727878688,
123.706044193446));
#125383=CARTESIAN_POINT('Ctrl Pts',(1.22202863962478,-28.9369928768266,
123.717165564375));
#125384=CARTESIAN_POINT('Ctrl Pts',(1.22269132940012,-28.9296117547805,
123.723317844037));
#125385=CARTESIAN_POINT('Ctrl Pts',(1.22455782570845,-28.9090878603758,
123.740727920465));
#125386=CARTESIAN_POINT('Ctrl Pts',(1.22576976240379,-28.8960670206688,
123.752126852365));
#125387=CARTESIAN_POINT('Ctrl Pts',(1.22993481286726,-28.8522786474751,
123.791682556353));
#125388=CARTESIAN_POINT('Ctrl Pts',(1.2329315059388,-28.8223931646664,123.82078964835));
#125389=CARTESIAN_POINT('Ctrl Pts',(1.24534804968517,-28.7041099104753,
123.944976909866));
#125390=CARTESIAN_POINT('Ctrl Pts',(1.25487703514157,-28.6258629693803,
124.049126082904));
#125391=CARTESIAN_POINT('Ctrl Pts',(1.26672980387923,-28.5407114183588,
124.195277594783));
#125392=CARTESIAN_POINT('Ctrl Pts',(1.26944560205847,-28.5221290323072,
124.229935612407));
#125393=CARTESIAN_POINT('Ctrl Pts',(1.27319194526195,-28.4978279849176,
124.279386140264));
#125394=CARTESIAN_POINT('Ctrl Pts',(1.27425807616971,-28.491068505303,124.293649611147));
#125395=CARTESIAN_POINT('Ctrl Pts',(1.27605053971841,-28.4799734914073,
124.31794807193));
#125396=CARTESIAN_POINT('Ctrl Pts',(1.27678046247768,-28.4755322784921,
124.327933340134));
#125397=CARTESIAN_POINT('Ctrl Pts',(1.27825083547488,-28.4667439771098,
124.348227708216));
#125398=CARTESIAN_POINT('Ctrl Pts',(1.27899108712776,-28.4624018375552,
124.358538346231));
#125399=CARTESIAN_POINT('Ctrl Pts',(1.28081760606239,-28.4518957858664,
124.384205292149));
#125400=CARTESIAN_POINT('Ctrl Pts',(1.28189966337131,-28.4458560796823,
124.399611386536));
#125401=CARTESIAN_POINT('Ctrl Pts',(1.28613667752862,-28.4229552088,124.460689548178));
#125402=CARTESIAN_POINT('Ctrl Pts',(1.28923322675697,-28.4078689017657,
124.507003769619));
#125403=CARTESIAN_POINT('Ctrl Pts',(1.30174960511128,-28.3543734897741,
124.699499177115));
#125404=CARTESIAN_POINT('Ctrl Pts',(1.31064599465137,-28.3339149674139,
124.849882812604));
#125405=CARTESIAN_POINT('Ctrl Pts',(1.32020507860662,-28.3340002656058,
125.000940743489));
#125406=CARTESIAN_POINT('Ctrl Pts',(1.32020523017832,-28.33400026696,125.000943138708));
#125407=CARTESIAN_POINT('Ctrl Pts',(1.32219890698379,-28.3340181023383,
125.032448298303));
#125408=CARTESIAN_POINT('Ctrl Pts',(1.32422170656257,-28.3349296096847,
125.063944754036));
#125409=CARTESIAN_POINT('Ctrl Pts',(1.32680933174148,-28.3371884976266,
125.103329994415));
#125410=CARTESIAN_POINT('Ctrl Pts',(1.32733343221065,-28.3377004057832,
125.111262002803));
#125411=CARTESIAN_POINT('Ctrl Pts',(1.32825584296946,-28.3386955705439,
125.125136472903));
#125412=CARTESIAN_POINT('Ctrl Pts',(1.32865284985722,-28.3391540088743,
125.131080643988));
#125413=CARTESIAN_POINT('Ctrl Pts',(1.329447764642,-28.3401314412556,125.142924611089));
#125414=CARTESIAN_POINT('Ctrl Pts',(1.32984564648262,-28.3406499954039,
125.148824183451));
#125415=CARTESIAN_POINT('Ctrl Pts',(1.33071839080185,-28.3418509841225,
125.161700261481));
#125416=CARTESIAN_POINT('Ctrl Pts',(1.33119390186315,-28.3425459821816,
125.168675154436));
#125417=CARTESIAN_POINT('Ctrl Pts',(1.33252662288963,-28.3446071926527,
125.188116827758));
#125418=CARTESIAN_POINT('Ctrl Pts',(1.33338883396304,-28.3460701628955,
125.200572575268));
#125419=CARTESIAN_POINT('Ctrl Pts',(1.3379570008922,-28.3545031629007,125.26598762346));
#125420=CARTESIAN_POINT('Ctrl Pts',(1.34176852209445,-28.3638760560123,
125.318600933699));
#125421=CARTESIAN_POINT('Ctrl Pts',(1.35044146688248,-28.3905987980285,
125.43569831053));
#125422=CARTESIAN_POINT('Ctrl Pts',(1.35531912301383,-28.4093313976143,
125.499778532008));
#125423=CARTESIAN_POINT('Ctrl Pts',(1.36049059062027,-28.4334055482443,
125.566885271663));
#125424=CARTESIAN_POINT('Ctrl Pts',(1.36082346855069,-28.4349739191953,
125.571200881571));
#125425=CARTESIAN_POINT('Ctrl Pts',(1.36115610141822,-28.4365599811973,
125.575509606876));
#125426=CARTESIAN_POINT('Ctrl Pts',(1.16625578224439,-28.4365599837819,
125.575509613897));
#125427=CARTESIAN_POINT('Ctrl Pts',(1.16615106715064,-28.4360181278264,
125.574037598029));
#125428=CARTESIAN_POINT('Ctrl Pts',(1.16604642104355,-28.4354783476409,
125.572564808384));
#125429=CARTESIAN_POINT('Ctrl Pts',(1.16522598371781,-28.4312599224099,
125.561004333803));
#125430=CARTESIAN_POINT('Ctrl Pts',(1.16451338791583,-28.4276767307586,
125.550881874627));
#125431=CARTESIAN_POINT('Ctrl Pts',(1.16288079176412,-28.419656064612,125.527507651467));
#125432=CARTESIAN_POINT('Ctrl Pts',(1.16196307924118,-28.4152869193639,
125.514233165253));
#125433=CARTESIAN_POINT('Ctrl Pts',(1.15905378485932,-28.4018900050275,
125.471736966863));
#125434=CARTESIAN_POINT('Ctrl Pts',(1.15708283748867,-28.393499289232,125.44231999311));
#125435=CARTESIAN_POINT('Ctrl Pts',(1.15242758125335,-28.3754013816926,
125.371536539769));
#125436=CARTESIAN_POINT('Ctrl Pts',(1.14976580265002,-28.3664570433951,
125.329996756368));
#125437=CARTESIAN_POINT('Ctrl Pts',(1.14256128716452,-28.346357731558,125.215543068738));
#125438=CARTESIAN_POINT('Ctrl Pts',(1.13808626256621,-28.3384397427388,
125.142159926808));
#125439=CARTESIAN_POINT('Ctrl Pts',(1.13273556033149,-28.3348438611616,
125.054769512405));
#125440=CARTESIAN_POINT('Ctrl Pts',(1.13189411697792,-28.334448906308,125.041039186489));
#125441=CARTESIAN_POINT('Ctrl Pts',(1.1265255423805,-28.3330163104506,124.953643957334));
#125442=CARTESIAN_POINT('Ctrl Pts',(1.12194599314035,-28.3366963931124,
124.879992230711));
#125443=CARTESIAN_POINT('Ctrl Pts',(1.11633294369522,-28.346659521943,124.79464180214));
#125444=CARTESIAN_POINT('Ctrl Pts',(1.11552469198212,-28.3482176782578,
124.782464104954));
#125445=CARTESIAN_POINT('Ctrl Pts',(1.11424772069684,-28.3508682831121,
124.763422595618));
#125446=CARTESIAN_POINT('Ctrl Pts',(1.113783877654,-28.3518693792809,124.756546224953));
#125447=CARTESIAN_POINT('Ctrl Pts',(1.11291143080005,-28.3538229125227,
124.743692305856));
#125448=CARTESIAN_POINT('Ctrl Pts',(1.11250340138189,-28.3547649451166,
124.737713425971));
#125449=CARTESIAN_POINT('Ctrl Pts',(1.1115373014639,-28.3570622763596,124.72363227465));
#125450=CARTESIAN_POINT('Ctrl Pts',(1.11097774654946,-28.3584449455696,
124.71553474803));
#125451=CARTESIAN_POINT('Ctrl Pts',(1.10909351746417,-28.3632761068919,
124.688450167068));
#125452=CARTESIAN_POINT('Ctrl Pts',(1.10775530280762,-28.3669944608212,
124.669513645733));
#125453=CARTESIAN_POINT('Ctrl Pts',(1.10442408258247,-28.3769684616018,
124.623006981712));
#125454=CARTESIAN_POINT('Ctrl Pts',(1.10241650351457,-28.3835984609188,
124.595523802243));
#125455=CARTESIAN_POINT('Ctrl Pts',(1.09321883513799,-28.4168663943231,
124.471545948245));
#125456=CARTESIAN_POINT('Ctrl Pts',(1.08585657108412,-28.4514686801848,
124.377403102497));
#125457=CARTESIAN_POINT('Ctrl Pts',(1.07267821986524,-28.5296935240147,
124.212225872802));
#125458=CARTESIAN_POINT('Ctrl Pts',(1.06683129749109,-28.5705896333804,
124.140244848222));
#125459=CARTESIAN_POINT('Ctrl Pts',(1.05983082986308,-28.6275948005129,
124.055307223673));
#125460=CARTESIAN_POINT('Ctrl Pts',(1.05849961776267,-28.6388087058061,
124.039219696898));
#125461=CARTESIAN_POINT('Ctrl Pts',(1.0563828071248,-28.6572371770517,124.013752641196));
#125462=CARTESIAN_POINT('Ctrl Pts',(1.05559042973218,-28.6642718798303,
124.004245887325));
#125463=CARTESIAN_POINT('Ctrl Pts',(1.05408602524642,-28.6778865876812,
123.986250798093));
#125464=CARTESIAN_POINT('Ctrl Pts',(1.05337334657858,-28.6844485772155,
123.977749647777));
#125465=CARTESIAN_POINT('Ctrl Pts',(1.05174056909496,-28.6997385665339,
123.958332336478));
#125466=CARTESIAN_POINT('Ctrl Pts',(1.05082275827726,-28.7085227237348,
123.947461268555));
#125467=CARTESIAN_POINT('Ctrl Pts',(1.04791316454007,-28.736963881813,123.913155362386));
#125468=CARTESIAN_POINT('Ctrl Pts',(1.04594201757812,-28.7571305229629,
123.890149941074));
#125469=CARTESIAN_POINT('Ctrl Pts',(1.04128623296005,-28.806791038723,123.836551306082));
#125470=CARTESIAN_POINT('Ctrl Pts',(1.03862412826436,-28.8368443834861,
123.806505182348));
#125471=CARTESIAN_POINT('Ctrl Pts',(1.03141968890869,-28.9221035442637,
123.727549713869));
#125472=CARTESIAN_POINT('Ctrl Pts',(1.0269450191103,-28.9794581763953,123.681104533079));
#125473=CARTESIAN_POINT('Ctrl Pts',(1.02159391043209,-29.0509345397209,
123.630686394644));
#125474=CARTESIAN_POINT('Ctrl Pts',(1.02075170930233,-29.0622661425251,
123.62290152692));
#125475=CARTESIAN_POINT('Ctrl Pts',(1.01538391823107,-29.1349043791237,
123.574311015818));
#125476=CARTESIAN_POINT('Ctrl Pts',(1.01080591771019,-29.1987563224001,
123.537472962735));
#125477=CARTESIAN_POINT('Ctrl Pts',(1.00519456556864,-29.2758439453853,
123.499565142168));
#125478=CARTESIAN_POINT('Ctrl Pts',(1.004386239616,-29.2869211781704,123.494269172085));
#125479=CARTESIAN_POINT('Ctrl Pts',(1.00310912933111,-29.3043584721581,
123.486168052086));
#125480=CARTESIAN_POINT('Ctrl Pts',(1.00264522114973,-29.3106795340434,
123.4832793294));
#125481=CARTESIAN_POINT('Ctrl Pts',(1.00177256620039,-29.3225411779991,
123.477948027192));
#125482=CARTESIAN_POINT('Ctrl Pts',(1.00136439305603,-29.3280772408143,
123.475495993961));
#125483=CARTESIAN_POINT('Ctrl Pts',(1.00039785463017,-29.3411595433869,
123.469786678887));
#125484=CARTESIAN_POINT('Ctrl Pts',(0.99983800317666,-29.3487166586959,
123.466555003385));
#125485=CARTESIAN_POINT('Ctrl Pts',(0.997952426810626,-29.3741104208787,
123.455917350153));
#125486=CARTESIAN_POINT('Ctrl Pts',(0.996613145986367,-29.3920511455114,
123.448765941039));
#125487=CARTESIAN_POINT('Ctrl Pts',(0.993278795220195,-29.4365758439961,
123.431908805816));
#125488=CARTESIAN_POINT('Ctrl Pts',(0.991269129156873,-29.4632900937476,
123.42256566898));
#125489=CARTESIAN_POINT('Ctrl Pts',(0.982051983685102,-29.5857567736997,
123.383204701323));
#125490=CARTESIAN_POINT('Ctrl Pts',(0.974671958152577,-29.6838636007809,
123.361194721295));
#125491=CARTESIAN_POINT('Ctrl Pts',(0.961505589281053,-29.8649461454338,
123.337445355301));
#125492=CARTESIAN_POINT('Ctrl Pts',(0.955686230085221,-29.9472269253968,
123.332802905299));
#125493=CARTESIAN_POINT('Ctrl Pts',(0.948712331337758,-30.0491190120977,
123.334608947749));
#125494=CARTESIAN_POINT('Ctrl Pts',(0.947381905713893,-30.0687057626552,
123.3353019465));
#125495=CARTESIAN_POINT('Ctrl Pts',(0.945265938121997,-30.1000848423782,
123.336966971324));
#125496=CARTESIAN_POINT('Ctrl Pts',(0.944473630508666,-30.1118864597902,
123.337719258749));
#125497=CARTESIAN_POINT('Ctrl Pts',(0.942969101659076,-30.1343913874589,
123.339394586624));
#125498=CARTESIAN_POINT('Ctrl Pts',(0.942256231412057,-30.1450956842545,
123.340295618014));
#125499=CARTESIAN_POINT('Ctrl Pts',(0.940622645972129,-30.1697145363664,
123.342607904374));
#125500=CARTESIAN_POINT('Ctrl Pts',(0.93970422410551,-30.1836216567743,
123.344090977918));
#125501=CARTESIAN_POINT('Ctrl Pts',(0.936791112539374,-30.2279239332839,
123.349380435329));
#125502=CARTESIAN_POINT('Ctrl Pts',(0.934817125855642,-30.2582345182754,
123.353850131647));
#125503=CARTESIAN_POINT('Ctrl Pts',(0.93015341504093,-30.3303256597539,
123.366521354377));
#125504=CARTESIAN_POINT('Ctrl Pts',(0.927486328497796,-30.371949268577,
123.375493413394));
#125505=CARTESIAN_POINT('Ctrl Pts',(0.920278737169879,-30.4845795175345,
123.404327788921));
#125506=CARTESIAN_POINT('Ctrl Pts',(0.915805607809372,-30.5546833012663,
123.427322692987));
#125507=CARTESIAN_POINT('Ctrl Pts',(0.910429142862871,-30.6361892506851,
123.46018818489));
#125508=CARTESIAN_POINT('Ctrl Pts',(0.90956014969723,-30.649275780915,123.465660356173));
#125509=CARTESIAN_POINT('Ctrl Pts',(0.904197070038578,-30.7293796271543,
123.50036435128));
#125510=CARTESIAN_POINT('Ctrl Pts',(0.899650362145599,-30.7944742737766,
123.533811182113));
#125511=CARTESIAN_POINT('Ctrl Pts',(0.894073740930451,-30.8676800253446,
123.577734879252));
#125512=CARTESIAN_POINT('Ctrl Pts',(0.893265556468678,-30.8781360795331,
123.584166780955));
#125513=CARTESIAN_POINT('Ctrl Pts',(0.891988637072149,-30.8943981323138,
123.594419595873));
#125514=CARTESIAN_POINT('Ctrl Pts',(0.891524776639683,-30.9002531631936,
123.598162445453));
#125515=CARTESIAN_POINT('Ctrl Pts',(0.890652508969474,-30.9111614240045,
123.605232111984));
#125516=CARTESIAN_POINT('Ctrl Pts',(0.890244678105772,-30.9162201671904,
123.608549964018));
#125517=CARTESIAN_POINT('Ctrl Pts',(0.889279174523455,-30.9281003180437,
123.616434610686));
#125518=CARTESIAN_POINT('Ctrl Pts',(0.888720020126513,-30.9349061616793,
123.621024348056));
#125519=CARTESIAN_POINT('Ctrl Pts',(0.886837142423207,-30.9575854608541,
123.63656391755));
#125520=CARTESIAN_POINT('Ctrl Pts',(0.885499886339679,-30.973302015754,
123.647738570888));
#125521=CARTESIAN_POINT('Ctrl Pts',(0.882171254050822,-31.0115522694112,
123.675947208183));
#125522=CARTESIAN_POINT('Ctrl Pts',(0.880165313821002,-31.0338530719746,
123.693286016514));
#125523=CARTESIAN_POINT('Ctrl Pts',(0.870981471847521,-31.1330040430234,
123.774502917571));
#125524=CARTESIAN_POINT('Ctrl Pts',(0.863631545894803,-31.2044528863925,
123.844649433441));
#125525=CARTESIAN_POINT('Ctrl Pts',(0.850443401970882,-31.3229149775003,
123.983962939969));
#125526=CARTESIAN_POINT('Ctrl Pts',(0.844575908090151,-31.3718570945992,
124.051081034038));
#125527=CARTESIAN_POINT('Ctrl Pts',(0.83755618354263,-31.4259408390617,
124.138238280016));
#125528=CARTESIAN_POINT('Ctrl Pts',(0.836224853915574,-31.4359857029084,
124.155082455724));
#125529=CARTESIAN_POINT('Ctrl Pts',(0.834108269421008,-31.4516054958727,
124.182358746707));
#125530=CARTESIAN_POINT('Ctrl Pts',(0.833316225946469,-31.4573705599678,
124.192679247047));
#125531=CARTESIAN_POINT('Ctrl Pts',(0.831812725354296,-31.4681582592602,
124.212483357237));
#125532=CARTESIAN_POINT('Ctrl Pts',(0.831100614285069,-31.4732000424193,
124.221955797481));
#125533=CARTESIAN_POINT('Ctrl Pts',(0.829469537723204,-31.4845890640284,
124.243861025522));
#125534=CARTESIAN_POINT('Ctrl Pts',(0.828552853236997,-31.4908723265472,
124.256326305864));
#125535=CARTESIAN_POINT('Ctrl Pts',(0.825648640970225,-31.5103924311854,
124.296293945706));
#125536=CARTESIAN_POINT('Ctrl Pts',(0.823681664147706,-31.5230309923198,
124.324082630396));
#125537=CARTESIAN_POINT('Ctrl Pts',(0.819037391774664,-31.5513711766943,
124.391232412323));
#125538=CARTESIAN_POINT('Ctrl Pts',(0.816382495195395,-31.566348971826,
124.430876305876));
#125539=CARTESIAN_POINT('Ctrl Pts',(0.809182110492082,-31.6032202771721,
124.540998854901));
#125540=CARTESIAN_POINT('Ctrl Pts',(0.804704794253211,-31.6219694972719,
124.612427257312));
#125541=CARTESIAN_POINT('Ctrl Pts',(0.799406664717733,-31.6383528061114,
124.697475530023));
#125542=CARTESIAN_POINT('Ctrl Pts',(0.798619970096382,-31.6406364258722,
124.710115392251));
#125543=CARTESIAN_POINT('Ctrl Pts',(0.79324355618884,-31.655208323417,124.796466865955));
#125544=CARTESIAN_POINT('Ctrl Pts',(0.788601865667353,-31.6626695510857,
124.870897553711));
#125545=CARTESIAN_POINT('Ctrl Pts',(0.782919828727749,-31.6655116559534,
124.957837732638));
#125546=CARTESIAN_POINT('Ctrl Pts',(0.782111559124968,-31.6657771238166,
124.970112127799));
#125547=CARTESIAN_POINT('Ctrl Pts',(0.780834692681443,-31.6659803445043,
124.989334510083));
#125548=CARTESIAN_POINT('Ctrl Pts',(0.780370976724859,-31.6660103326028,
124.996281366027));
#125549=CARTESIAN_POINT('Ctrl Pts',(0.779498695584072,-31.6659851457551,
125.009280306434));
#125550=CARTESIAN_POINT('Ctrl Pts',(0.779090704107883,-31.6659404400962,
125.015332165912));
#125551=CARTESIAN_POINT('Ctrl Pts',(0.77812475990824,-31.6657573460318,
125.029595915936));
#125552=CARTESIAN_POINT('Ctrl Pts',(0.777565323220713,-31.6655912056346,
125.037807178484));
#125553=CARTESIAN_POINT('Ctrl Pts',(0.775682272090778,-31.6648317718971,
125.065291439682));
#125554=CARTESIAN_POINT('Ctrl Pts',(0.774345141642842,-31.6639646196891,
125.084554515466));
#125555=CARTESIAN_POINT('Ctrl Pts',(0.771017396621862,-31.661004285685,
125.131977159938));
#125556=CARTESIAN_POINT('Ctrl Pts',(0.769012246675701,-31.6585291616439,
125.160106364307));
#125557=CARTESIAN_POINT('Ctrl Pts',(0.7598386688879,-31.6440695458233,125.287316818176));
#125558=CARTESIAN_POINT('Ctrl Pts',(0.752498693421345,-31.6239116732194,
125.385262138454));
#125559=CARTESIAN_POINT('Ctrl Pts',(0.739308387318392,-31.5711277066871,
125.560373342479));
#125560=CARTESIAN_POINT('Ctrl Pts',(0.733429814837493,-31.5412252745476,
125.638035241197));
#125561=CARTESIAN_POINT('Ctrl Pts',(0.726398222103071,-31.4972443070696,
125.730890379078));
#125562=CARTESIAN_POINT('Ctrl Pts',(0.725065600402682,-31.4885291458107,
125.748479993391));
#125563=CARTESIAN_POINT('Ctrl Pts',(0.722946850400739,-31.4740645331745,
125.776421140688));
#125564=CARTESIAN_POINT('Ctrl Pts',(0.72215392902457,-31.4685122957506,
125.786872089606));
#125565=CARTESIAN_POINT('Ctrl Pts',(0.720648669531772,-31.4577079381769,
125.806696337857));
#125566=CARTESIAN_POINT('Ctrl Pts',(0.719935677677714,-31.4524756042906,
125.816079679133));
#125567=CARTESIAN_POINT('Ctrl Pts',(0.718302421703189,-31.4402275747301,
125.837553526235));
#125568=CARTESIAN_POINT('Ctrl Pts',(0.717384443611637,-31.4331496891641,
125.849607770966));
#125569=CARTESIAN_POINT('Ctrl Pts',(0.714475221098579,-31.4101079913955,
125.887742299267));
#125570=CARTESIAN_POINT('Ctrl Pts',(0.712504584526768,-31.3935770285898,
125.913473694485));
#125571=CARTESIAN_POINT('Ctrl Pts',(0.707850376161537,-31.3524215746607,
125.973814520167));
#125572=CARTESIAN_POINT('Ctrl Pts',(0.705189295406144,-31.3271635286492,
126.007966359622));
#125573=CARTESIAN_POINT('Ctrl Pts',(0.697986961690473,-31.2545735091527,
126.098650168494));
#125574=CARTESIAN_POINT('Ctrl Pts',(0.69351329100442,-31.2047525974259,
126.153064797835));
#125575=CARTESIAN_POINT('Ctrl Pts',(0.688176181758693,-31.1417108112333,
126.213357169947));
#125576=CARTESIAN_POINT('Ctrl Pts',(0.687346943166105,-31.1318155697849,
126.222592617736));
#125577=CARTESIAN_POINT('Ctrl Pts',(0.681980447100824,-31.0672212088951,
126.2814236296));
#125578=CARTESIAN_POINT('Ctrl Pts',(0.67739095481364,-31.0093953255646,
126.32745091908));
#125579=CARTESIAN_POINT('Ctrl Pts',(0.671766733598932,-30.9386180658002,
126.376482128867));
#125580=CARTESIAN_POINT('Ctrl Pts',(0.670957959561977,-30.9284427231868,
126.38336582744));
#125581=CARTESIAN_POINT('Ctrl Pts',(0.669680055901379,-30.9123889837533,
126.393969410678));
#125582=CARTESIAN_POINT('Ctrl Pts',(0.669215801605281,-30.9065615944165,
126.397766234651));
#125583=CARTESIAN_POINT('Ctrl Pts',(0.668341930295656,-30.8956059296626,
126.404807047466));
#125584=CARTESIAN_POINT('Ctrl Pts',(0.667932881846171,-30.8904834804768,
126.408059653592));
#125585=CARTESIAN_POINT('Ctrl Pts',(0.666963693731415,-30.878358572475,
126.415665994338));
#125586=CARTESIAN_POINT('Ctrl Pts',(0.666402057257771,-30.8713414233687,
126.419995812023));
#125587=CARTESIAN_POINT('Ctrl Pts',(0.664508599745873,-30.8477054414036,
126.434338849463));
#125588=CARTESIAN_POINT('Ctrl Pts',(0.663163136475742,-30.8309445681685,
126.444113394053));
#125589=CARTESIAN_POINT('Ctrl Pts',(0.659810723061453,-30.7891800108563,
126.467501717418));
#125590=CARTESIAN_POINT('Ctrl Pts',(0.657789050857232,-30.7639911990428,
126.480771300861));
#125591=CARTESIAN_POINT('Ctrl Pts',(0.648459099339785,-30.6472651122729,
126.538492023009));
#125592=CARTESIAN_POINT('Ctrl Pts',(0.640976199854946,-30.5521140381387,
126.575144618829));
#125593=CARTESIAN_POINT('Ctrl Pts',(0.627877965661515,-30.377107912237,
126.624736295201));
#125594=CARTESIAN_POINT('Ctrl Pts',(0.622216793183016,-30.298518942658,
126.64099611059));
#125595=CARTESIAN_POINT('Ctrl Pts',(0.615395908507051,-30.1996963591046,
126.654103584471));
#125596=CARTESIAN_POINT('Ctrl Pts',(0.614070377653021,-30.1802945611189,
126.656330652801));
#125597=CARTESIAN_POINT('Ctrl Pts',(0.611959567323206,-30.1490919619853,
126.65935750035));
#125598=CARTESIAN_POINT('Ctrl Pts',(0.611167605878462,-30.1373145007617,
126.660373592725));
#125599=CARTESIAN_POINT('Ctrl Pts',(0.609662070284355,-30.1147950417186,
126.662075187814));
#125600=CARTESIAN_POINT('Ctrl Pts',(0.608947863634468,-30.1040553139814,
126.662782106122));
#125601=CARTESIAN_POINT('Ctrl Pts',(0.607308812492061,-30.0792826810204,
126.664171752207));
#125602=CARTESIAN_POINT('Ctrl Pts',(0.606386296364463,-30.0652463571903,
126.664781155955));
#125603=CARTESIAN_POINT('Ctrl Pts',(0.603449796313902,-30.0202876973036,
126.66616358998));
#125604=CARTESIAN_POINT('Ctrl Pts',(0.601456958839757,-29.9893498441647,
126.666253122262));
#125605=CARTESIAN_POINT('Ctrl Pts',(0.596740467267545,-29.91532582262,126.664405313624));
#125606=CARTESIAN_POINT('Ctrl Pts',(0.594040149136078,-29.8722818882341,
126.661656775995));
#125607=CARTESIAN_POINT('Ctrl Pts',(0.586842690992665,-29.7567374825711,
126.649761731282));
#125608=CARTESIAN_POINT('Ctrl Pts',(0.582409598552956,-29.6846532524469,
126.637512501222));
#125609=CARTESIAN_POINT('Ctrl Pts',(0.577016503721894,-29.5989042411632,
126.617067284458));
#125610=CARTESIAN_POINT('Ctrl Pts',(0.57609046697172,-29.5842515955794,
126.613362224224));
#125611=CARTESIAN_POINT('Ctrl Pts',(0.57073564931471,-29.5000811012224,
126.590856115885));
#125612=CARTESIAN_POINT('Ctrl Pts',(0.566253917592269,-29.4317983918142,
126.567764785254));
#125613=CARTESIAN_POINT('Ctrl Pts',(0.560749376253956,-29.3538871549404,
126.535657765087));
#125614=CARTESIAN_POINT('Ctrl Pts',(0.559941506354228,-29.3425940732412,
126.53085727805));
#125615=CARTESIAN_POINT('Ctrl Pts',(0.558664979174158,-29.3249915347029,
126.523144066585));
#125616=CARTESIAN_POINT('Ctrl Pts',(0.558201191772277,-29.3186452603866,
126.520315753464));
#125617=CARTESIAN_POINT('Ctrl Pts',(0.557371237326707,-29.3073798688148,
126.515210459083));
#125618=CARTESIAN_POINT('Ctrl Pts',(0.557006016579308,-29.3024539109558,
126.512949051439));
#125619=CARTESIAN_POINT('Ctrl Pts',(0.556112861077067,-29.2904830992487,
126.507382605615));
#125620=CARTESIAN_POINT('Ctrl Pts',(0.555583409303405,-29.2834503656735,
126.504052248961));
#125621=CARTESIAN_POINT('Ctrl Pts',(0.553889414205153,-29.2611416352582,
126.493295957914));
#125622=CARTESIAN_POINT('Ctrl Pts',(0.552714543876437,-29.2459563083808,
126.48568588749));
#125623=CARTESIAN_POINT('Ctrl Pts',(0.549867229395235,-29.2097762194701,
126.466856825882));
#125624=CARTESIAN_POINT('Ctrl Pts',(0.548184721456098,-29.1889006988942,
126.455417595061));
#125625=CARTESIAN_POINT('Ctrl Pts',(0.541418110010879,-29.1066827715153,
126.408046121392));
#125626=CARTESIAN_POINT('Ctrl Pts',(0.536227226792752,-29.0474244857738,
126.368652093163));
#125627=CARTESIAN_POINT('Ctrl Pts',(0.522908139521502,-28.9018945116724,
126.25786478686));
#125628=CARTESIAN_POINT('Ctrl Pts',(0.514852835373573,-28.8199534865787,
126.181337311866));
#125629=CARTESIAN_POINT('Ctrl Pts',(0.50562515322859,-28.7317650209868,
126.080565815076));
#125630=CARTESIAN_POINT('Ctrl Pts',(0.50411863058937,-28.7175706042957,
126.063681046568));
#125631=CARTESIAN_POINT('Ctrl Pts',(0.501705802567479,-28.6951776569899,
126.03594370981));
#125632=CARTESIAN_POINT('Ctrl Pts',(0.500791146072882,-28.6867697784389,
126.025264415164));
#125633=CARTESIAN_POINT('Ctrl Pts',(0.499169624106025,-28.6720131077862,
126.006041780287));
#125634=CARTESIAN_POINT('Ctrl Pts',(0.498460781459573,-28.6656138156697,
125.99753835501));
#125635=CARTESIAN_POINT('Ctrl Pts',(0.496964633333417,-28.6522195341151,
125.979380382936));
#125636=CARTESIAN_POINT('Ctrl Pts',(0.496178181967775,-28.6452457840825,
125.969710856716));
#125637=CARTESIAN_POINT('Ctrl Pts',(0.494065897637493,-28.626703196969,
125.943409927396));
#125638=CARTESIAN_POINT('Ctrl Pts',(0.492747645016592,-28.6153327033637,
125.92664067257));
#125639=CARTESIAN_POINT('Ctrl Pts',(0.489846980583185,-28.5907944208838,
125.888990869792));
#125640=CARTESIAN_POINT('Ctrl Pts',(0.488270089392217,-28.5777790046832,
125.868016511898));
#125641=CARTESIAN_POINT('Ctrl Pts',(0.483300356898985,-28.5378949550602,
125.800436216336));
#125642=CARTESIAN_POINT('Ctrl Pts',(0.479963094649077,-28.5128140745072,
125.752813366189));
#125643=CARTESIAN_POINT('Ctrl Pts',(0.473803282860917,-28.4704539722927,
125.661968035598));
#125644=CARTESIAN_POINT('Ctrl Pts',(0.470975555099976,-28.4525988551096,
125.619081106435));
#125645=CARTESIAN_POINT('Ctrl Pts',(0.468139978699828,-28.4365599867671,
125.575509622007));
#125646=CARTESIAN_POINT('Origin',(5.,-30.,55.));
#125647=CARTESIAN_POINT('',(1.32021575923829,-28.3340002652327,55.0009400825958));
#125648=CARTESIAN_POINT('Ctrl Pts',(0.659214745210768,-28.4365623102018,
55.5755159338528));
#125649=CARTESIAN_POINT('Ctrl Pts',(0.659963641292018,-28.4405139534956,
55.5862509069418));
#125650=CARTESIAN_POINT('Ctrl Pts',(0.660718112395066,-28.4445759197288,
55.5969445264719));
#125651=CARTESIAN_POINT('Ctrl Pts',(0.661924434192335,-28.4511909595541,
55.6138333999505));
#125652=CARTESIAN_POINT('Ctrl Pts',(0.662372155669629,-28.4536719329351,
55.6200567649136));
#125653=CARTESIAN_POINT('Ctrl Pts',(0.663233890173186,-28.4584945714238,
55.6319450832073));
#125654=CARTESIAN_POINT('Ctrl Pts',(0.663647543837139,-28.4608300603191,
55.6376123165684));
#125655=CARTESIAN_POINT('Ctrl Pts',(0.664654545452568,-28.4665660606024,
55.6513159771192));
#125656=CARTESIAN_POINT('Ctrl Pts',(0.665249751707099,-28.4699985149372,
55.6593387565258));
#125657=CARTESIAN_POINT('Ctrl Pts',(0.667395281146444,-28.4825267915646,
55.687996809844));
#125658=CARTESIAN_POINT('Ctrl Pts',(0.668964512435956,-28.4919779215533,
55.7084728909968));
#125659=CARTESIAN_POINT('Ctrl Pts',(0.680707788462809,-28.5650020372384,
55.8585954186811));
#125660=CARTESIAN_POINT('Ctrl Pts',(0.691446198038116,-28.6447740481354,
55.9796792143553));
#125661=CARTESIAN_POINT('Ctrl Pts',(0.706348215234274,-28.7811489998703,
56.1375782492685));
#125662=CARTESIAN_POINT('Ctrl Pts',(0.710851108539443,-28.825915457073,
56.1837268875902));
#125663=CARTESIAN_POINT('Ctrl Pts',(0.716511229173992,-28.8869357299301,
56.2397538400991));
#125664=CARTESIAN_POINT('Ctrl Pts',(0.717771910094331,-28.9008404423981,
56.2520982265341));
#125665=CARTESIAN_POINT('Ctrl Pts',(0.719804332451236,-28.9237619754479,
56.2717714362838));
#125666=CARTESIAN_POINT('Ctrl Pts',(0.720581913525034,-28.9326536036333,
56.2792429611344));
#125667=CARTESIAN_POINT('Ctrl Pts',(0.722076094015,-28.9499727184326,56.2934897010616));
#125668=CARTESIAN_POINT('Ctrl Pts',(0.72279316063993,-28.9583894354873,
56.3002770243558));
#125669=CARTESIAN_POINT('Ctrl Pts',(0.724462268379914,-28.9782232838014,
56.3159550573192));
#125670=CARTESIAN_POINT('Ctrl Pts',(0.72541167226813,-28.9896914662681,
56.3247800040469));
#125671=CARTESIAN_POINT('Ctrl Pts',(0.728540249029682,-29.0280848532284,
56.3535357580327));
#125672=CARTESIAN_POINT('Ctrl Pts',(0.730694011293115,-29.0554970934145,
56.3728046485986));
#125673=CARTESIAN_POINT('Ctrl Pts',(0.735884881361671,-29.1237397587507,
56.4177619905098));
#125674=CARTESIAN_POINT('Ctrl Pts',(0.738891364809314,-29.1651407596486,
56.442529593517));
#125675=CARTESIAN_POINT('Ctrl Pts',(0.745995233323475,-29.266404573629,
56.4972871703079));
#125676=CARTESIAN_POINT('Ctrl Pts',(0.750056334966432,-29.3271119036571,
56.5255336385376));
#125677=CARTESIAN_POINT('Ctrl Pts',(0.758912614853314,-29.4616954151474,
56.5785530440077));
#125678=CARTESIAN_POINT('Ctrl Pts',(0.763709136771604,-29.5359354234534,
56.6019496767449));
#125679=CARTESIAN_POINT('Ctrl Pts',(0.76980726565648,-29.6274488471113,
56.6238933788813));
#125680=CARTESIAN_POINT('Ctrl Pts',(0.770878651015154,-29.6434249755122,
56.6274760429261));
#125681=CARTESIAN_POINT('Ctrl Pts',(0.772472415436527,-29.6669900525349,
56.6323969178816));
#125682=CARTESIAN_POINT('Ctrl Pts',(0.772985068171922,-29.6745401826819,
56.6339189772137));
#125683=CARTESIAN_POINT('Ctrl Pts',(0.773902973631897,-29.6879993405186,
56.6365352733002));
#125684=CARTESIAN_POINT('Ctrl Pts',(0.774307074264652,-29.6939041239484,
56.637649970112));
#125685=CARTESIAN_POINT('Ctrl Pts',(0.775206840638491,-29.707005271969,
56.6400498545001));
#125686=CARTESIAN_POINT('Ctrl Pts',(0.775703315393402,-29.7142040375561,
56.6413196211194));
#125687=CARTESIAN_POINT('Ctrl Pts',(0.777182043165073,-29.7355629128225,
56.6449422701476));
#125688=CARTESIAN_POINT('Ctrl Pts',(0.778171275327273,-29.7497449188664,
56.6471594959333));
#125689=CARTESIAN_POINT('Ctrl Pts',(0.780489834331059,-29.7827778964682,
56.6518874618695));
#125690=CARTESIAN_POINT('Ctrl Pts',(0.781825070041427,-29.8016465136671,
56.6542591869629));
#125691=CARTESIAN_POINT('Ctrl Pts',(0.786599363794931,-29.8686989762837,
56.6615238516719));
#125692=CARTESIAN_POINT('Ctrl Pts',(0.790094904868642,-29.9170489575495,
56.6646381026969));
#125693=CARTESIAN_POINT('Ctrl Pts',(0.801966995933811,-30.0805207792727,
56.6680277218472));
#125694=CARTESIAN_POINT('Ctrl Pts',(0.810382446848105,-30.1955326990349,
56.6584852228168));
#125695=CARTESIAN_POINT('Ctrl Pts',(0.821478443120727,-30.3506519603713,
56.6292409537629));
#125696=CARTESIAN_POINT('Ctrl Pts',(0.824438057573833,-30.3923367446291,
56.619708408388));
#125697=CARTESIAN_POINT('Ctrl Pts',(0.828455890430732,-30.4493380675934,
56.6043430359028));
#125698=CARTESIAN_POINT('Ctrl Pts',(0.829556926894114,-30.4650014798904,
56.5998734113248));
#125699=CARTESIAN_POINT('Ctrl Pts',(0.831323450748539,-30.4901936579209,
56.5922834629587));
#125700=CARTESIAN_POINT('Ctrl Pts',(0.831993518833882,-30.4997638833363,
56.5893056714085));
#125701=CARTESIAN_POINT('Ctrl Pts',(0.833388042719641,-30.5197080667199,
56.5829020386295));
#125702=CARTESIAN_POINT('Ctrl Pts',(0.83411193475826,-30.530076401145,56.5794601473679));
#125703=CARTESIAN_POINT('Ctrl Pts',(0.835832785829586,-30.5547549817536,
56.5709974143047));
#125704=CARTESIAN_POINT('Ctrl Pts',(0.836826598044922,-30.5690321616613,
56.5658826231637));
#125705=CARTESIAN_POINT('Ctrl Pts',(0.840289916299863,-30.6188452550762,
56.5472658228053));
#125706=CARTESIAN_POINT('Ctrl Pts',(0.842725610946042,-30.6539886139836,
56.5327427099798));
#125707=CARTESIAN_POINT('Ctrl Pts',(0.848791916699208,-30.7413466796475,
56.4930893241426));
#125708=CARTESIAN_POINT('Ctrl Pts',(0.852375246155066,-30.792805214712,
56.466414422777));
#125709=CARTESIAN_POINT('Ctrl Pts',(0.862651125810953,-30.9373096076258,
56.3816720105806));
#125710=CARTESIAN_POINT('Ctrl Pts',(0.869228930686582,-31.0261365411004,
56.3170445643393));
#125711=CARTESIAN_POINT('Ctrl Pts',(0.878097227136037,-31.1305267278775,
56.2240824572584));
#125712=CARTESIAN_POINT('Ctrl Pts',(0.88004155115911,-31.1525341799814,
56.2033840792647));
#125713=CARTESIAN_POINT('Ctrl Pts',(0.88268437638759,-31.18107055971,56.1750440895643));
#125714=CARTESIAN_POINT('Ctrl Pts',(0.883346812629502,-31.1881119242406,
56.1679239370166));
#125715=CARTESIAN_POINT('Ctrl Pts',(0.884397523809826,-31.199097091447,
56.1566137076135));
#125716=CARTESIAN_POINT('Ctrl Pts',(0.884782538026635,-31.2030842410492,
56.1524657954881));
#125717=CARTESIAN_POINT('Ctrl Pts',(0.885585877276413,-31.211322322205,
56.143806214921));
#125718=CARTESIAN_POINT('Ctrl Pts',(0.886004481639483,-31.2155696457618,
56.1392913836904));
#125719=CARTESIAN_POINT('Ctrl Pts',(0.887042618707048,-31.2259936761341,
56.1280861758301));
#125720=CARTESIAN_POINT('Ctrl Pts',(0.887664288533123,-31.2321408607672,
56.121368718919));
#125721=CARTESIAN_POINT('Ctrl Pts',(0.890024387995303,-31.2551327325838,
56.0958265989553));
#125722=CARTESIAN_POINT('Ctrl Pts',(0.891786831028371,-31.2716026938486,
56.0766710422131));
#125723=CARTESIAN_POINT('Ctrl Pts',(0.896496804446941,-31.3139498103398,
56.0250914029554));
#125724=CARTESIAN_POINT('Ctrl Pts',(0.899476732144382,-31.3390618911845,
55.9920631579025));
#125725=CARTESIAN_POINT('Ctrl Pts',(0.911742955187062,-31.436512417141,
55.8534431135917));
#125726=CARTESIAN_POINT('Ctrl Pts',(0.921138969129262,-31.4978151011057,
55.7406019954244));
#125727=CARTESIAN_POINT('Ctrl Pts',(0.932994445367097,-31.5608703064797,
55.5838791540793));
#125728=CARTESIAN_POINT('Ctrl Pts',(0.935824974923883,-31.574743222478,
55.545357921975));
#125729=CARTESIAN_POINT('Ctrl Pts',(0.939699465085544,-31.5920548005865,
55.4910950090183));
#125730=CARTESIAN_POINT('Ctrl Pts',(0.940782341143438,-31.5967049905873,
55.4757583421885));
#125731=CARTESIAN_POINT('Ctrl Pts',(0.942527586162851,-31.6038897272558,
55.4507696182194));
#125732=CARTESIAN_POINT('Ctrl Pts',(0.943194326698031,-31.6065600285174,
55.4411580081438));
#125733=CARTESIAN_POINT('Ctrl Pts',(0.944587994716938,-31.6119836600457,
55.4209333448612));
#125734=CARTESIAN_POINT('Ctrl Pts',(0.945314307638591,-31.61471888452,55.4103158963638));
#125735=CARTESIAN_POINT('Ctrl Pts',(0.947052218707638,-31.6210414861569,
55.3847302801767));
#125736=CARTESIAN_POINT('Ctrl Pts',(0.948060499974413,-31.6245266806757,
55.3697377154156));
#125737=CARTESIAN_POINT('Ctrl Pts',(0.951640215251125,-31.6362344790149,
55.3160075949944));
#125738=CARTESIAN_POINT('Ctrl Pts',(0.954174604394025,-31.6432835844108,
55.2770262066794));
#125739=CARTESIAN_POINT('Ctrl Pts',(0.960564404724356,-31.6577309517901,
55.1768580372996));
#125740=CARTESIAN_POINT('Ctrl Pts',(0.964365223745703,-31.6631368409799,
55.1154441197577));
#125741=CARTESIAN_POINT('Ctrl Pts',(0.973680422779509,-31.6680548877707,
54.9634230593059));
#125742=CARTESIAN_POINT('Ctrl Pts',(0.979143253785267,-31.6636067451724,
54.8728950791873));
#125743=CARTESIAN_POINT('Ctrl Pts',(0.987402570717024,-31.6464623037035,
54.7422797707631));
#125744=CARTESIAN_POINT('Ctrl Pts',(0.990031037836238,-31.6395765784195,
54.7015944670879));
#125745=CARTESIAN_POINT('Ctrl Pts',(0.993462558443658,-31.6289264133717,
54.6503165183594));
#125746=CARTESIAN_POINT('Ctrl Pts',(0.994196884827876,-31.6265547956662,
54.6394458741157));
#125747=CARTESIAN_POINT('Ctrl Pts',(0.995378206655547,-31.6225968145929,
54.6221382295046));
#125748=CARTESIAN_POINT('Ctrl Pts',(0.995821359168282,-31.6210805523774,
54.6156853122823));
#125749=CARTESIAN_POINT('Ctrl Pts',(0.996681022140957,-31.6180797379266,
54.6032482193401));
#125750=CARTESIAN_POINT('Ctrl Pts',(0.997097241816606,-31.6166004158405,
54.5972629838045));
#125751=CARTESIAN_POINT('Ctrl Pts',(0.998120537342818,-31.6128983525958,
54.582633777008));
#125752=CARTESIAN_POINT('Ctrl Pts',(0.998729616657382,-31.61063932153,54.5739992642144));
#125753=CARTESIAN_POINT('Ctrl Pts',(1.00098522511608,-31.6020664926277,
54.5422752550403));
#125754=CARTESIAN_POINT('Ctrl Pts',(1.0026532021352,-31.5953249728398,54.5193056316508));
#125755=CARTESIAN_POINT('Ctrl Pts',(1.00704012273649,-31.5765093364595,
54.4599602500243));
#125756=CARTESIAN_POINT('Ctrl Pts',(1.00978669059544,-31.5636709241073,
54.4238424729003));
#125757=CARTESIAN_POINT('Ctrl Pts',(1.0175652224386,-31.5241375833952,54.3237100179675));
#125758=CARTESIAN_POINT('Ctrl Pts',(1.0226375406149,-31.4946744638198,54.2608709199988));
#125759=CARTESIAN_POINT('Ctrl Pts',(1.03464843330274,-31.4150800113469,
54.1154644229076));
#125760=CARTESIAN_POINT('Ctrl Pts',(1.04151112617786,-31.361515594002,54.0350463214709));
#125761=CARTESIAN_POINT('Ctrl Pts',(1.04947794848679,-31.2888556764999,
53.9441575882492));
#125762=CARTESIAN_POINT('Ctrl Pts',(1.05082968622706,-31.2761492812382,
53.9288346416686));
#125763=CARTESIAN_POINT('Ctrl Pts',(1.05297120198867,-31.2554182870267,
53.9047272940103));
#125764=CARTESIAN_POINT('Ctrl Pts',(1.05376803998593,-31.2475692633859,
53.8957951631918));
#125765=CARTESIAN_POINT('Ctrl Pts',(1.0552761313253,-31.2324591194727,53.878966742388));
#125766=CARTESIAN_POINT('Ctrl Pts',(1.05598808668145,-31.2252160867848,
53.8710550962479));
#125767=CARTESIAN_POINT('Ctrl Pts',(1.05761255005021,-31.2084409905437,
53.8530830806558));
#125768=CARTESIAN_POINT('Ctrl Pts',(1.05852285411219,-31.1988587122944,
53.843070505736));
#125769=CARTESIAN_POINT('Ctrl Pts',(1.06138128369846,-31.1682056598785,
53.8118308114439));
#125770=CARTESIAN_POINT('Ctrl Pts',(1.06330981930706,-31.1466869563556,
53.7910501726467));
#125771=CARTESIAN_POINT('Ctrl Pts',(1.07043446628666,-31.0642544911494,
53.715627459757));
#125772=CARTESIAN_POINT('Ctrl Pts',(1.07547632256952,-30.9999001979576,
53.6649150074561));
#125773=CARTESIAN_POINT('Ctrl Pts',(1.08666462366743,-30.8482724542223,
53.5625674788946));
#125774=CARTESIAN_POINT('Ctrl Pts',(1.09276640156089,-30.75950366134,53.5137534967374));
#125775=CARTESIAN_POINT('Ctrl Pts',(1.10093007852872,-30.6420524393445,
53.4624506456449));
#125776=CARTESIAN_POINT('Ctrl Pts',(1.10267860066395,-30.6169771469631,
53.4522182471399));
#125777=CARTESIAN_POINT('Ctrl Pts',(1.1050926392708,-30.5826737458718,53.439186165975));
#125778=CARTESIAN_POINT('Ctrl Pts',(1.10572949521159,-30.5736529521352,
53.4358482176635));
#125779=CARTESIAN_POINT('Ctrl Pts',(1.10674944642822,-30.5592623409872,
53.4306645132565));
#125780=CARTESIAN_POINT('Ctrl Pts',(1.10712960461376,-30.5539109522798,
53.4287677159289));
#125781=CARTESIAN_POINT('Ctrl Pts',(1.10793302524484,-30.542630143941,53.4248340297426));
#125782=CARTESIAN_POINT('Ctrl Pts',(1.10835665129977,-30.5366987801322,
53.4228032076037));
#125783=CARTESIAN_POINT('Ctrl Pts',(1.10942431157411,-30.5217884717841,
53.4177919554728));
#125784=CARTESIAN_POINT('Ctrl Pts',(1.11007074770082,-30.5127954371229,
53.414854475276));
#125785=CARTESIAN_POINT('Ctrl Pts',(1.11264930593903,-30.4770414154817,
53.4035118904902));
#125786=CARTESIAN_POINT('Ctrl Pts',(1.11461127806468,-30.4500965777982,
53.3957071202711));
#125787=CARTESIAN_POINT('Ctrl Pts',(1.12003804526655,-30.3759520788193,
53.3762454035932));
#125788=CARTESIAN_POINT('Ctrl Pts',(1.12354701370819,-30.3284197424937,
53.3659685303982));
#125789=CARTESIAN_POINT('Ctrl Pts',(1.13547970136026,-30.1664360243814,
53.3382998293558));
#125790=CARTESIAN_POINT('Ctrl Pts',(1.14394117757766,-30.0506264895923,
53.3307511443493));
#125791=CARTESIAN_POINT('Ctrl Pts',(1.15502814538573,-29.8929283312015,
53.3369121636872));
#125792=CARTESIAN_POINT('Ctrl Pts',(1.15793962131046,-29.850969421449,53.3401458132592));
#125793=CARTESIAN_POINT('Ctrl Pts',(1.16190413889962,-29.7930899355848,
53.346819314464));
#125794=CARTESIAN_POINT('Ctrl Pts',(1.16299852222704,-29.777032751387,53.3489083029754));
#125795=CARTESIAN_POINT('Ctrl Pts',(1.16475725076074,-29.7511064147828,
53.3526663707886));
#125796=CARTESIAN_POINT('Ctrl Pts',(1.16542609961355,-29.741217711071,53.3541908260158));
#125797=CARTESIAN_POINT('Ctrl Pts',(1.16682028678175,-29.7205480095359,
53.357568195804));
#125798=CARTESIAN_POINT('Ctrl Pts',(1.16754504294498,-29.7097702888344,
53.3594383977234));
#125799=CARTESIAN_POINT('Ctrl Pts',(1.16927200883321,-29.6840165445165,
53.3641690513153));
#125800=CARTESIAN_POINT('Ctrl Pts',(1.17027101109583,-29.6690596652992,
53.3671292283001));
#125801=CARTESIAN_POINT('Ctrl Pts',(1.17377560962581,-29.6164110960138,
53.3783022677858));
#125802=CARTESIAN_POINT('Ctrl Pts',(1.1762462678384,-29.5789645509273,53.3876186887177));
#125803=CARTESIAN_POINT('Ctrl Pts',(1.18242614099913,-29.4849493492021,
53.4145082238645));
#125804=CARTESIAN_POINT('Ctrl Pts',(1.18608558387259,-29.4289313316328,
53.4338126901721));
#125805=CARTESIAN_POINT('Ctrl Pts',(1.19655994573354,-29.2705929944841,
53.4980060801958));
#125806=CARTESIAN_POINT('Ctrl Pts',(1.20326065921172,-29.1716182010739,
53.5502417494761));
#125807=CARTESIAN_POINT('Ctrl Pts',(1.21208881541147,-29.0561632499323,
53.6268813743853));
#125808=CARTESIAN_POINT('Ctrl Pts',(1.21382945801558,-29.0340723299868,
53.6423306323007));
#125809=CARTESIAN_POINT('Ctrl Pts',(1.21623422885395,-29.0046349399247,
53.6639997806444));
#125810=CARTESIAN_POINT('Ctrl Pts',(1.21686997369886,-28.9969520651439,
53.6697582857092));
#125811=CARTESIAN_POINT('Ctrl Pts',(1.21788857533824,-28.9848088374216,
53.6790249436114));
#125812=CARTESIAN_POINT('Ctrl Pts',(1.21826850845923,-28.9803157540354,
53.6824901395899));
#125813=CARTESIAN_POINT('Ctrl Pts',(1.21905930458946,-28.9710411111115,
53.6897188727172));
#125814=CARTESIAN_POINT('Ctrl Pts',(1.21947041646921,-28.9662623424226,
53.6934857525445));
#125815=CARTESIAN_POINT('Ctrl Pts',(1.22045299713856,-28.9549398472241,
53.7025117508851));
#125816=CARTESIAN_POINT('Ctrl Pts',(1.2210260689708,-28.9484150728044,53.7077942838033));
#125817=CARTESIAN_POINT('Ctrl Pts',(1.2223077814754,-28.9339903933139,53.7196542701509));
#125818=CARTESIAN_POINT('Ctrl Pts',(1.22301794647307,-28.9261109354356,
53.7262559385422));
#125819=CARTESIAN_POINT('Ctrl Pts',(1.22506093262138,-28.9037508370259,
53.7453449124877));
#125820=CARTESIAN_POINT('Ctrl Pts',(1.22640372360606,-28.8894238278728,
53.7580088103662));
#125821=CARTESIAN_POINT('Ctrl Pts',(1.23121688973683,-28.8392705232512,
53.8039019162475));
#125822=CARTESIAN_POINT('Ctrl Pts',(1.23474462079593,-28.804693204456,53.8384559331168));
#125823=CARTESIAN_POINT('Ctrl Pts',(1.24676234642063,-28.6928931196582,
53.9604663629038));
#125824=CARTESIAN_POINT('Ctrl Pts',(1.25528841883712,-28.6233358799653,
54.0545048294473));
#125825=CARTESIAN_POINT('Ctrl Pts',(1.26636223392244,-28.5433199730105,
54.1904758995821));
#125826=CARTESIAN_POINT('Ctrl Pts',(1.26920574386274,-28.523787467326,54.226667578192));
#125827=CARTESIAN_POINT('Ctrl Pts',(1.27309474604692,-28.4985164994813,
54.2779466913659));
#125828=CARTESIAN_POINT('Ctrl Pts',(1.27417953476662,-28.4916287921005,
54.292447872342));
#125829=CARTESIAN_POINT('Ctrl Pts',(1.27592705245948,-28.4808001858974,
54.3161231551476));
#125830=CARTESIAN_POINT('Ctrl Pts',(1.27659417429594,-28.4767304062588,
54.3252368071961));
#125831=CARTESIAN_POINT('Ctrl Pts',(1.27798801302688,-28.4683637848074,
54.3444341142369));
#125832=CARTESIAN_POINT('Ctrl Pts',(1.27871412054514,-28.464084044836,54.3545247373503));
#125833=CARTESIAN_POINT('Ctrl Pts',(1.28045036987591,-28.4540431656761,
54.3788642176465));
#125834=CARTESIAN_POINT('Ctrl Pts',(1.28145721243702,-28.448378938272,54.3931521603375));
#125835=CARTESIAN_POINT('Ctrl Pts',(1.2850248863174,-28.4288891562718,54.444372662124));
#125836=CARTESIAN_POINT('Ctrl Pts',(1.28754901973547,-28.4161774351021,
54.4817167879635));
#125837=CARTESIAN_POINT('Ctrl Pts',(1.2939047253306,-28.3871475977008,54.5780879430202));
#125838=CARTESIAN_POINT('Ctrl Pts',(1.29768251325451,-28.3727354337739,
54.6376279524458));
#125839=CARTESIAN_POINT('Ctrl Pts',(1.30766056230485,-28.3431899516063,
54.7978233223371));
#125840=CARTESIAN_POINT('Ctrl Pts',(1.31378284441053,-28.3339429029157,
54.8992834777778));
#125841=CARTESIAN_POINT('Ctrl Pts',(1.32021575923829,-28.3340002652327,
55.0009400825958));
#125842=CARTESIAN_POINT('Ctrl Pts',(1.32021590954351,-28.3340002665747,
55.000942457804));
#125843=CARTESIAN_POINT('Ctrl Pts',(1.32220985562038,-28.3340180915062,
55.0324519122196));
#125844=CARTESIAN_POINT('Ctrl Pts',(1.32423293252513,-28.3349298320778,
55.0639526592521));
#125845=CARTESIAN_POINT('Ctrl Pts',(1.32682074830839,-28.3371891639739,
55.1033405957195));
#125846=CARTESIAN_POINT('Ctrl Pts',(1.32734474700025,-28.3377010174839,
55.1112710289715));
#125847=CARTESIAN_POINT('Ctrl Pts',(1.32826699345549,-28.3386960641558,
55.1251429808795));
#125848=CARTESIAN_POINT('Ctrl Pts',(1.32866393842213,-28.3391544514235,
55.1310862081801));
#125849=CARTESIAN_POINT('Ctrl Pts',(1.32945875925557,-28.3401317993643,
55.1429287499632));
#125850=CARTESIAN_POINT('Ctrl Pts',(1.3298566093499,-28.340650325113,55.1488278403667));
#125851=CARTESIAN_POINT('Ctrl Pts',(1.33072929281893,-28.3418512531499,
55.1617030012841));
#125852=CARTESIAN_POINT('Ctrl Pts',(1.331204774772,-28.3425462185789,55.1686774592109));
#125853=CARTESIAN_POINT('Ctrl Pts',(1.3325374877822,-28.3446074371047,55.1881189991655));
#125854=CARTESIAN_POINT('Ctrl Pts',(1.33339972061422,-28.3460704603213,
55.2005750468619));
#125855=CARTESIAN_POINT('Ctrl Pts',(1.33796728344874,-28.3545024450872,
55.2659813549176));
#125856=CARTESIAN_POINT('Ctrl Pts',(1.34177814116433,-28.363873396488,55.3185857505541));
#125857=CARTESIAN_POINT('Ctrl Pts',(1.35078342266844,-28.391618412814,55.4401709101938));
#125858=CARTESIAN_POINT('Ctrl Pts',(1.35600155264901,-28.4119305928387,
55.5086017904495));
#125859=CARTESIAN_POINT('Ctrl Pts',(1.36116732170967,-28.4365623080758,
55.5755159280775));
#125860=CARTESIAN_POINT('Ctrl Pts',(1.16624546596859,-28.4365623102019,
55.575515933853));
#125861=CARTESIAN_POINT('Ctrl Pts',(1.16623406145781,-28.4365032961389,
55.5753556171617));
#125862=CARTESIAN_POINT('Ctrl Pts',(1.16622265776398,-28.4364443066904,
55.5751952912736));
#125863=CARTESIAN_POINT('Ctrl Pts',(1.16549980768447,-28.4327064137748,
55.5650313454292));
#125864=CARTESIAN_POINT('Ctrl Pts',(1.16479157876853,-28.4291235001549,
55.5549924666191));
#125865=CARTESIAN_POINT('Ctrl Pts',(1.16321390103826,-28.4213222899542,
55.5324534831877));
#125866=CARTESIAN_POINT('Ctrl Pts',(1.16234619052926,-28.4171555947951,
55.5199361783316));
#125867=CARTESIAN_POINT('Ctrl Pts',(1.16013833760378,-28.406876906967,55.4877883429162));
#125868=CARTESIAN_POINT('Ctrl Pts',(1.15880514823918,-28.4009786949724,
55.4680914253662));
#125869=CARTESIAN_POINT('Ctrl Pts',(1.14770621329044,-28.3545505755323,
55.3019122474401));
#125870=CARTESIAN_POINT('Ctrl Pts',(1.13864993213321,-28.3338772243859,
55.1506356236224));
#125871=CARTESIAN_POINT('Ctrl Pts',(1.12530416485984,-28.334052803967,54.9342472504104));
#125872=CARTESIAN_POINT('Ctrl Pts',(1.12127417411137,-28.3378392579978,
54.869910826422));
#125873=CARTESIAN_POINT('Ctrl Pts',(1.11627530334294,-28.3467489465006,
54.7939328377005));
#125874=CARTESIAN_POINT('Ctrl Pts',(1.11547762566429,-28.3482908250023,
54.7819185896074));
#125875=CARTESIAN_POINT('Ctrl Pts',(1.11421381289345,-28.3509180014544,
54.7630773733838));
#125876=CARTESIAN_POINT('Ctrl Pts',(1.11375239404336,-28.351915058325,54.756238252291));
#125877=CARTESIAN_POINT('Ctrl Pts',(1.11288183398201,-28.3538662063784,
54.7434142206414));
#125878=CARTESIAN_POINT('Ctrl Pts',(1.11247323670157,-28.3548104370481,
54.737428055846));
#125879=CARTESIAN_POINT('Ctrl Pts',(1.1115021446493,-28.3571218253109,54.72327659247));
#125880=CARTESIAN_POINT('Ctrl Pts',(1.11093811813268,-28.3585172123379,
54.7151161785498));
#125881=CARTESIAN_POINT('Ctrl Pts',(1.10902222587865,-28.3634365821474,
54.6875838185676));
#125882=CARTESIAN_POINT('Ctrl Pts',(1.10765621507157,-28.3672430045154,
54.668264863394));
#125883=CARTESIAN_POINT('Ctrl Pts',(1.104239881799,-28.3775137553063,54.6206069001332));
#125884=CARTESIAN_POINT('Ctrl Pts',(1.10217408030968,-28.3843789473843,
54.5923614838859));
#125885=CARTESIAN_POINT('Ctrl Pts',(1.09432056936455,-28.4130189305222,
54.4866581517853));
#125886=CARTESIAN_POINT('Ctrl Pts',(1.0884267795435,-28.4396557592631,54.4106323466519));
#125887=CARTESIAN_POINT('Ctrl Pts',(1.07530638859385,-28.5116588000358,
54.2446965534111));
#125888=CARTESIAN_POINT('Ctrl Pts',(1.06814665844362,-28.5598923465102,
54.156353663732));
#125889=CARTESIAN_POINT('Ctrl Pts',(1.05990691753729,-28.6268670473983,
54.0563595152035));
#125890=CARTESIAN_POINT('Ctrl Pts',(1.05855636733932,-28.6382290561309,
54.0400357163173));
#125891=CARTESIAN_POINT('Ctrl Pts',(1.05641644138395,-28.6568437020813,
54.0142878770965));
#125892=CARTESIAN_POINT('Ctrl Pts',(1.05562002030217,-28.6639093480471,
54.0047316882814));
#125893=CARTESIAN_POINT('Ctrl Pts',(1.05411255135894,-28.6775436475373,
53.9866983789375));
#125894=CARTESIAN_POINT('Ctrl Pts',(1.0534008036682,-28.6840930426992,53.9782075218927));
#125895=CARTESIAN_POINT('Ctrl Pts',(1.05177659261749,-28.6992932435353,
53.9588900335077));
#125896=CARTESIAN_POINT('Ctrl Pts',(1.05086633451863,-28.7079981432164,
53.948106825792));
#125897=CARTESIAN_POINT('Ctrl Pts',(1.04800720552964,-28.7359192230794,
53.9143891314306));
#125898=CARTESIAN_POINT('Ctrl Pts',(1.04607794402249,-28.7556198149369,
53.8918622376811));
#125899=CARTESIAN_POINT('Ctrl Pts',(1.03901442524823,-28.8307620313791,
53.8104726236096));
#125900=CARTESIAN_POINT('Ctrl Pts',(1.03403000485387,-28.8898606397321,
53.7551364483433));
#125901=CARTESIAN_POINT('Ctrl Pts',(1.02299686358755,-29.0301372817023,
53.641757151509));
#125902=CARTESIAN_POINT('Ctrl Pts',(1.01699173984669,-29.1129663323208,
53.586272645239));
#125903=CARTESIAN_POINT('Ctrl Pts',(1.00882317195071,-29.2257573147217,
53.5245508088232));
#125904=CARTESIAN_POINT('Ctrl Pts',(1.00694893069188,-29.2516331498732,
53.5112593010003));
#125905=CARTESIAN_POINT('Ctrl Pts',(1.00438787609396,-29.2867415356805,
53.4943719263102));
#125906=CARTESIAN_POINT('Ctrl Pts',(1.00373437504665,-29.2956790001159,
53.4901703902266));
#125907=CARTESIAN_POINT('Ctrl Pts',(1.00269448035717,-29.3098564742229,
53.4836587780271));
#125908=CARTESIAN_POINT('Ctrl Pts',(1.00231123296883,-29.3150721180615,
53.4812957556926));
#125909=CARTESIAN_POINT('Ctrl Pts',(1.00150802720176,-29.3259806095401,
53.4764211284065));
#125910=CARTESIAN_POINT('Ctrl Pts',(1.00108776034537,-29.3316754693969,
53.4739144736553));
#125911=CARTESIAN_POINT('Ctrl Pts',(1.00003988045341,-29.3458461348936,
53.467771628282));
#125912=CARTESIAN_POINT('Ctrl Pts',(0.999410044857784,-29.35433826898,53.4641738439509));
#125913=CARTESIAN_POINT('Ctrl Pts',(0.996980507169826,-29.3870159065608,
53.45064852419));
#125914=CARTESIAN_POINT('Ctrl Pts',(0.995155025085117,-29.4114026488488,
53.4412208402037));
#125915=CARTESIAN_POINT('Ctrl Pts',(0.99022383204168,-29.4770840403755,
53.4175900217503));
#125916=CARTESIAN_POINT('Ctrl Pts',(0.987082286576581,-29.5187314527544,
53.4044303373608));
#125917=CARTESIAN_POINT('Ctrl Pts',(0.973279874152865,-29.7024637997197,
53.3542230395125));
#125918=CARTESIAN_POINT('Ctrl Pts',(0.962524276868997,-29.8486113982833,
53.334404853455));
#125919=CARTESIAN_POINT('Ctrl Pts',(0.950598892162561,-30.0213236605926,
53.3339359706849));
#125920=CARTESIAN_POINT('Ctrl Pts',(0.948832291167848,-30.0471694992282,
53.3344672875928));
#125921=CARTESIAN_POINT('Ctrl Pts',(0.946186726389482,-30.0862532601435,
53.336181342138));
#125922=CARTESIAN_POINT('Ctrl Pts',(0.945294172911729,-30.0995056080924,
53.336921287858));
#125923=CARTESIAN_POINT('Ctrl Pts',(0.9436931362223,-30.1233915632246,53.3385415057917));
#125924=CARTESIAN_POINT('Ctrl Pts',(0.942982942691258,-30.1340281142516,
53.3393656996426));
#125925=CARTESIAN_POINT('Ctrl Pts',(0.941464033961621,-30.1568606527204,
53.3413557298148));
#125926=CARTESIAN_POINT('Ctrl Pts',(0.940656377603993,-30.1690532350134,
53.3425540441495));
#125927=CARTESIAN_POINT('Ctrl Pts',(0.938435069860581,-30.2027187878852,
53.3462381326349));
#125928=CARTESIAN_POINT('Ctrl Pts',(0.93703032077653,-30.2241587654593,
53.3490075292339));
#125929=CARTESIAN_POINT('Ctrl Pts',(0.928761603677918,-30.3510850959352,
53.367920818445));
#125930=CARTESIAN_POINT('Ctrl Pts',(0.922216310365715,-30.4548798673067,
53.3937524230652));
#125931=CARTESIAN_POINT('Ctrl Pts',(0.909190829915431,-30.6559510039607,
53.464865905101));
#125932=CARTESIAN_POINT('Ctrl Pts',(0.902734071567557,-30.7527479627162,
53.5099420591852));
#125933=CARTESIAN_POINT('Ctrl Pts',(0.89482074879949,-30.8578161669773,
53.5717340019465));
#125934=CARTESIAN_POINT('Ctrl Pts',(0.893813333509112,-30.870958545872,
53.5797100620832));
#125935=CARTESIAN_POINT('Ctrl Pts',(0.892297356381249,-30.8903529844528,
53.591850877824));
#125936=CARTESIAN_POINT('Ctrl Pts',(0.891797223519456,-30.8966907125267,
53.5958781577637));
#125937=CARTESIAN_POINT('Ctrl Pts',(0.890892525057947,-30.9080413722192,
53.6031990684467));
#125938=CARTESIAN_POINT('Ctrl Pts',(0.89048897293095,-30.9130640394406,
53.6064771142445));
#125939=CARTESIAN_POINT('Ctrl Pts',(0.88957877330433,-30.9243015955239,
53.6138981470499));
#125940=CARTESIAN_POINT('Ctrl Pts',(0.88907119092711,-30.9305063269588,
53.6180558056394));
#125941=CARTESIAN_POINT('Ctrl Pts',(0.887523648197904,-30.9492427515387,
53.630794073457));
#125942=CARTESIAN_POINT('Ctrl Pts',(0.886475727312991,-30.9616848630911,
53.6395041880975));
#125943=CARTESIAN_POINT('Ctrl Pts',(0.879750634011209,-31.0400912972663,
53.696005618615));
#125944=CARTESIAN_POINT('Ctrl Pts',(0.873841249761727,-31.1025889396038,
53.748406510031));
#125945=CARTESIAN_POINT('Ctrl Pts',(0.858494524399951,-31.2538123075522,
53.8953467709984));
#125946=CARTESIAN_POINT('Ctrl Pts',(0.849114437939133,-31.3358207167937,
53.9960581539459));
#125947=CARTESIAN_POINT('Ctrl Pts',(0.838771987341453,-31.4165702836705,
54.1228904173036));
#125948=CARTESIAN_POINT('Ctrl Pts',(0.837346648791826,-31.4274597475475,
54.1407262796545));
#125949=CARTESIAN_POINT('Ctrl Pts',(0.835034953584482,-31.4447199387857,
54.1702308652387));
#125950=CARTESIAN_POINT('Ctrl Pts',(0.834141431539081,-31.4512913830487,
54.1817788454352));
#125951=CARTESIAN_POINT('Ctrl Pts',(0.832540049376055,-31.462884502025,
54.2027305733635));
#125952=CARTESIAN_POINT('Ctrl Pts',(0.831830461129028,-31.4679553376095,
54.212106136104));
#125953=CARTESIAN_POINT('Ctrl Pts',(0.83031436203537,-31.4786445855784,
54.2323311618035));
#125954=CARTESIAN_POINT('Ctrl Pts',(0.82950889333664,-31.4842343603653,
54.2431951159927));
#125955=CARTESIAN_POINT('Ctrl Pts',(0.827297705722188,-31.4993268412837,
54.2733384737363));
#125956=CARTESIAN_POINT('Ctrl Pts',(0.825900773112623,-31.508576957018,
54.2927422081236));
#125957=CARTESIAN_POINT('Ctrl Pts',(0.82280112519334,-31.5284310914414,
54.3365527809227));
#125958=CARTESIAN_POINT('Ctrl Pts',(0.821105162298961,-31.5388311954838,
54.3610457919199));
#125959=CARTESIAN_POINT('Ctrl Pts',(0.815601995257463,-31.5709531990043,
54.4420351969047));
#125960=CARTESIAN_POINT('Ctrl Pts',(0.811865118567678,-31.5901849074589,
54.4994688481055));
#125961=CARTESIAN_POINT('Ctrl Pts',(0.802783956080069,-31.6295249209977,
54.6423756857888));
#125962=CARTESIAN_POINT('Ctrl Pts',(0.797488790093301,-31.6460869352314,
54.7286277771464));
#125963=CARTESIAN_POINT('Ctrl Pts',(0.789184423591483,-31.6607855854843,
54.8607385156302));
#125964=CARTESIAN_POINT('Ctrl Pts',(0.786311587025967,-31.6639541013579,
54.905880479385));
#125965=CARTESIAN_POINT('Ctrl Pts',(0.782603682227426,-31.6656165636806,
54.9624847188622));
#125966=CARTESIAN_POINT('Ctrl Pts',(0.781851773580448,-31.6658342456913,
54.9738813914868));
#125967=CARTESIAN_POINT('Ctrl Pts',(0.780649029015884,-31.6659940248568,
54.9919631699322));
#125968=CARTESIAN_POINT('Ctrl Pts',(0.780202289534688,-31.6660128595703,
54.9986474787928));
#125969=CARTESIAN_POINT('Ctrl Pts',(0.77934123350569,-31.6659718388379,
55.011465496239));
#125970=CARTESIAN_POINT('Ctrl Pts',(0.778927263617136,-31.6659183338037,
55.0175990182009));
#125971=CARTESIAN_POINT('Ctrl Pts',(0.777917704064818,-31.6657061974064,
55.0324896424649));
#125972=CARTESIAN_POINT('Ctrl Pts',(0.777320231466912,-31.665512375544,
55.0412459860966));
#125973=CARTESIAN_POINT('Ctrl Pts',(0.775156322922067,-31.6645657689097,
55.0727726170826));
#125974=CARTESIAN_POINT('Ctrl Pts',(0.773570558434099,-31.6634149990333,
55.0955273151611));
#125975=CARTESIAN_POINT('Ctrl Pts',(0.761777916473459,-31.6515198482567,
55.2626932155156));
#125976=CARTESIAN_POINT('Ctrl Pts',(0.751007005008851,-31.6224544700863,
55.4051798530242));
#125977=CARTESIAN_POINT('Ctrl Pts',(0.736115130301,-31.5545905070751,55.6023838077631));
#125978=CARTESIAN_POINT('Ctrl Pts',(0.731648427581999,-31.5304086840699,
55.6614143490946));
#125979=CARTESIAN_POINT('Ctrl Pts',(0.726025326849968,-31.4948935124071,
55.7356586554303));
#125980=CARTESIAN_POINT('Ctrl Pts',(0.724767201104126,-31.4866074373264,
55.7522623520767));
#125981=CARTESIAN_POINT('Ctrl Pts',(0.722737892684079,-31.4726908064105,
55.7790201900131));
#125982=CARTESIAN_POINT('Ctrl Pts',(0.721960903523555,-31.4672286612023,
55.7892596120809));
#125983=CARTESIAN_POINT('Ctrl Pts',(0.720467211776136,-31.4564709513518,
55.8089284877257));
#125984=CARTESIAN_POINT('Ctrl Pts',(0.719750048647606,-31.4511897066254,
55.8183650622773));
#125985=CARTESIAN_POINT('Ctrl Pts',(0.718079753404172,-31.4386194148121,
55.8403213841295));
#125986=CARTESIAN_POINT('Ctrl Pts',(0.717129270570933,-31.4312581356779,
55.85279893306));
#125987=CARTESIAN_POINT('Ctrl Pts',(0.71399260796866,-31.4062828836215,
55.8938980905331));
#125988=CARTESIAN_POINT('Ctrl Pts',(0.711832020490769,-31.387965105435,
55.9220837577085));
#125989=CARTESIAN_POINT('Ctrl Pts',(0.706620482125906,-31.3411915824033,
55.9894987808133));
#125990=CARTESIAN_POINT('Ctrl Pts',(0.703600490750051,-31.3118528933047,
56.0280784000104));
#125991=CARTESIAN_POINT('Ctrl Pts',(0.696505448911896,-31.2383217635587,
56.1164869739304));
#125992=CARTESIAN_POINT('Ctrl Pts',(0.692465420791772,-31.1927438745192,
56.1650519945106));
#125993=CARTESIAN_POINT('Ctrl Pts',(0.683632256201668,-31.087899989496,
56.2641479728702));
#125994=CARTESIAN_POINT('Ctrl Pts',(0.678837433618865,-31.027756542017,
56.313510616572));
#125995=CARTESIAN_POINT('Ctrl Pts',(0.672754215512254,-30.9512069767532,
56.3678533993608));
#125996=CARTESIAN_POINT('Ctrl Pts',(0.671695895796978,-30.937882381046,
56.3770236841965));
#125997=CARTESIAN_POINT('Ctrl Pts',(0.670110755775963,-30.917957443895,
56.3903131322876));
#125998=CARTESIAN_POINT('Ctrl Pts',(0.669593282966531,-30.9114579191173,
56.3945827083055));
#125999=CARTESIAN_POINT('Ctrl Pts',(0.668669726593056,-30.8998724836048,
56.4020776658342));
#126000=CARTESIAN_POINT('Ctrl Pts',(0.66826484204571,-30.8947986298631,
56.405321200796));
#126001=CARTESIAN_POINT('Ctrl Pts',(0.667366701809323,-30.8835558053559,
56.4124227681519));
#126002=CARTESIAN_POINT('Ctrl Pts',(0.666872671499463,-30.8773791657986,
56.4162678883598));
#126003=CARTESIAN_POINT('Ctrl Pts',(0.665412459139005,-30.8591392915425,
56.4274575799269));
#126004=CARTESIAN_POINT('Ctrl Pts',(0.664439590437624,-30.8470079618816,
56.434689145578));
#126005=CARTESIAN_POINT('Ctrl Pts',(0.662166838642417,-30.8186839734351,
56.4510888245021));
#126006=CARTESIAN_POINT('Ctrl Pts',(0.660861378299215,-30.8024269061112,
56.460141508049));
#126007=CARTESIAN_POINT('Ctrl Pts',(0.656239668831929,-30.7448092058579,
56.4909728770553));
#126008=CARTESIAN_POINT('Ctrl Pts',(0.652870583563433,-30.7026886030704,
56.5112806029566));
#126009=CARTESIAN_POINT('Ctrl Pts',(0.64154904114023,-30.5593663034603,
56.5730931427838));
#126010=CARTESIAN_POINT('Ctrl Pts',(0.633549622447796,-30.4549280125623,
56.6064115039828));
#126011=CARTESIAN_POINT('Ctrl Pts',(0.622393051233916,-30.3004469393127,
56.6394051642707));
#126012=CARTESIAN_POINT('Ctrl Pts',(0.619016261141123,-30.2524968739035,
56.6474719432033));
#126013=CARTESIAN_POINT('Ctrl Pts',(0.614543968262986,-30.187361226336,
56.6555185405715));
#126014=CARTESIAN_POINT('Ctrl Pts',(0.613391881250385,-30.1704326578384,
56.6573468598146));
#126015=CARTESIAN_POINT('Ctrl Pts',(0.611564736807413,-30.1433540543122,
56.6598521007722));
#126016=CARTESIAN_POINT('Ctrl Pts',(0.610884507356309,-30.1332210798639,
56.6606960989632));
#126017=CARTESIAN_POINT('Ctrl Pts',(0.609484289612966,-30.1122588079788,
56.6622489941722));
#126018=CARTESIAN_POINT('Ctrl Pts',(0.608764737727573,-30.101429013331,
56.6629449549879));
#126019=CARTESIAN_POINT('Ctrl Pts',(0.60708144742816,-30.0759643992842,
56.6643317096555));
#126020=CARTESIAN_POINT('Ctrl Pts',(0.606120466413455,-30.0613255871529,
56.6649353815292));
#126021=CARTESIAN_POINT('Ctrl Pts',(0.602912778805024,-30.0121466847089,
56.6663138861494));
#126022=CARTESIAN_POINT('Ctrl Pts',(0.600693295279663,-29.9775895644834,
56.6662075340011));
#126023=CARTESIAN_POINT('Ctrl Pts',(0.59530640700282,-29.8927428511392,
56.6633059102952));
#126024=CARTESIAN_POINT('Ctrl Pts',(0.592172932785695,-29.8425285284031,
56.6593052584522));
#126025=CARTESIAN_POINT('Ctrl Pts',(0.582906926889831,-29.6933085474579,
56.6405804570941));
#126026=CARTESIAN_POINT('Ctrl Pts',(0.57689533921652,-29.5953764194341,
56.6192103106182));
#126027=CARTESIAN_POINT('Ctrl Pts',(0.567606146855471,-29.4530995130802,
56.5744424032324));
#126028=CARTESIAN_POINT('Ctrl Pts',(0.564496395484269,-29.4069214705016,
56.5576347153741));
#126029=CARTESIAN_POINT('Ctrl Pts',(0.560520020241607,-29.3507948586255,
56.5343482252573));
#126030=CARTESIAN_POINT('Ctrl Pts',(0.559751716019859,-29.3400790147403,
56.5297699390206));
#126031=CARTESIAN_POINT('Ctrl Pts',(0.558528558300658,-29.3232398187259,
56.5223656344813));
#126032=CARTESIAN_POINT('Ctrl Pts',(0.558078032595549,-29.3170838560514,
56.519614097171));
#126033=CARTESIAN_POINT('Ctrl Pts',(0.557217019932719,-29.3054111737008,
56.514311495));
#126034=CARTESIAN_POINT('Ctrl Pts',(0.556806951378812,-29.2998915039549,
56.5117675186392));
#126035=CARTESIAN_POINT('Ctrl Pts',(0.555815032476529,-29.2866331659693,
56.5055686650774));
#126036=CARTESIAN_POINT('Ctrl Pts',(0.555231426341487,-29.2789086081284,
56.5018842970498));
#126037=CARTESIAN_POINT('Ctrl Pts',(0.55315739431752,-29.2517125119825,
56.4886544570432));
#126038=CARTESIAN_POINT('Ctrl Pts',(0.551649395663401,-29.2324002279826,
56.4787889425007));
#126039=CARTESIAN_POINT('Ctrl Pts',(0.547784117502843,-29.1839256256531,
56.4528207469828));
#126040=CARTESIAN_POINT('Ctrl Pts',(0.54540590785726,-29.1550441329977,
56.4362154506226));
#126041=CARTESIAN_POINT('Ctrl Pts',(0.531573373523371,-28.9915056759951,
56.33554904769));
#126042=CARTESIAN_POINT('Ctrl Pts',(0.519839473796115,-28.8688787605094,
56.2334242836303));
#126043=CARTESIAN_POINT('Ctrl Pts',(0.50676852445426,-28.7426736331756,
56.093420531934));
#126044=CARTESIAN_POINT('Ctrl Pts',(0.5047326476553,-28.7233806477863,56.0708320497424));
#126045=CARTESIAN_POINT('Ctrl Pts',(0.501799048754285,-28.6961343404467,
56.0371479573592));
#126046=CARTESIAN_POINT('Ctrl Pts',(0.500881968650037,-28.6876978821238,
56.0264524900288));
#126047=CARTESIAN_POINT('Ctrl Pts',(0.499256145630107,-28.6728908968879,
56.007199679074));
#126048=CARTESIAN_POINT('Ctrl Pts',(0.498545415866182,-28.6664696865922,
55.9986824707877));
#126049=CARTESIAN_POINT('Ctrl Pts',(0.497057403954751,-28.6531380219633,
55.9806412452735));
#126050=CARTESIAN_POINT('Ctrl Pts',(0.496280857520036,-28.6462457545938,
55.9711044716594));
#126051=CARTESIAN_POINT('Ctrl Pts',(0.494224169513516,-28.628171475085,
55.9455288163754));
#126052=CARTESIAN_POINT('Ctrl Pts',(0.492950927267009,-28.6171695690114,
55.9293644580919));
#126053=CARTESIAN_POINT('Ctrl Pts',(0.485637773665962,-28.5551409659613,
55.8346889052855));
#126054=CARTESIAN_POINT('Ctrl Pts',(0.47984189674057,-28.5105183090986,
55.7521773320803));
#126055=CARTESIAN_POINT('Ctrl Pts',(0.472112722188003,-28.4600025376136,
55.6364195169717));
#126056=CARTESIAN_POINT('Ctrl Pts',(0.470123713197726,-28.447831751358,
55.6061303190444));
#126057=CARTESIAN_POINT('Ctrl Pts',(0.468131487137799,-28.4365623373493,
55.5755160076012));
#126058=CARTESIAN_POINT('Origin',(5.,30.,55.));
#126059=CARTESIAN_POINT('',(1.3202157917438,31.6659997347684,55.0009400806026));
#126060=CARTESIAN_POINT('Ctrl Pts',(0.659214778542432,31.5634376782623,
55.5755159651912));
#126061=CARTESIAN_POINT('Ctrl Pts',(0.659963674773577,31.5594860338117,
55.5862509407588));
#126062=CARTESIAN_POINT('Ctrl Pts',(0.660718146030943,31.5554240663698,
55.5969445627462));
#126063=CARTESIAN_POINT('Ctrl Pts',(0.661924467957585,31.5488090252237,
55.613833438356));
#126064=CARTESIAN_POINT('Ctrl Pts',(0.662372189405329,31.5463280517853,
55.6200568030159));
#126065=CARTESIAN_POINT('Ctrl Pts',(0.66323392355848,31.5415054148437,55.6319451166599));
#126066=CARTESIAN_POINT('Ctrl Pts',(0.663647576898634,31.5391699275969,
55.6376123456943));
#126067=CARTESIAN_POINT('Ctrl Pts',(0.664654577091319,31.5334339350216,
55.6513159872087));
#126068=CARTESIAN_POINT('Ctrl Pts',(0.665249782236512,31.5300014869306,
55.6593387519811));
#126069=CARTESIAN_POINT('Ctrl Pts',(0.667395303766544,31.5174732562376,
55.6879967012015));
#126070=CARTESIAN_POINT('Ctrl Pts',(0.668964528083185,31.5080221693331,
55.7084726944259));
#126071=CARTESIAN_POINT('Ctrl Pts',(0.680707776955766,31.434998241425,55.8585949080955));
#126072=CARTESIAN_POINT('Ctrl Pts',(0.691446166056638,31.3552264309243,
55.9796785122895));
#126073=CARTESIAN_POINT('Ctrl Pts',(0.706348193913444,31.2188515169005,
56.1375777165001));
#126074=CARTESIAN_POINT('Ctrl Pts',(0.710851114015021,31.1740848164214,
56.183726636443));
#126075=CARTESIAN_POINT('Ctrl Pts',(0.716511261941901,31.1130642518199,
56.2397538568652));
#126076=CARTESIAN_POINT('Ctrl Pts',(0.71777194462588,31.0991595200653,56.2520982598632));
#126077=CARTESIAN_POINT('Ctrl Pts',(0.719804369030032,31.0762379635695,
56.2717714879298));
#126078=CARTESIAN_POINT('Ctrl Pts',(0.720581950409677,31.0673463317197,
56.2792430151123));
#126079=CARTESIAN_POINT('Ctrl Pts',(0.722076130964953,31.0500272157867,
56.2934897544291));
#126080=CARTESIAN_POINT('Ctrl Pts',(0.72279319735446,31.0416105013657,56.3002770749091));
#126081=CARTESIAN_POINT('Ctrl Pts',(0.724462303762982,31.0217766686898,
56.3159550940202));
#126082=CARTESIAN_POINT('Ctrl Pts',(0.72541170656721,31.0103084994599,56.3247800299974));
#126083=CARTESIAN_POINT('Ctrl Pts',(0.72854027604579,30.9719152031312,56.3535357151689));
#126084=CARTESIAN_POINT('Ctrl Pts',(0.730694032283207,30.9445030435336,
56.3728045520156));
#126085=CARTESIAN_POINT('Ctrl Pts',(0.735884884584433,30.8762606271322,
56.4177617454544));
#126086=CARTESIAN_POINT('Ctrl Pts',(0.738891356592106,30.8348598001479,
56.4425292630904));
#126087=CARTESIAN_POINT('Ctrl Pts',(0.745995231813121,30.7335959365295,
56.4972869328982));
#126088=CARTESIAN_POINT('Ctrl Pts',(0.750056350595555,30.6728883584316,
56.5255335352461));
#126089=CARTESIAN_POINT('Ctrl Pts',(0.758912647442102,30.5383045961151,
56.5785530396186));
#126090=CARTESIAN_POINT('Ctrl Pts',(0.763709168879551,30.4640645987096,
56.6019496697849));
#126091=CARTESIAN_POINT('Ctrl Pts',(0.769794313488902,30.3727460295175,
56.6238466503994));
#126092=CARTESIAN_POINT('Ctrl Pts',(0.770852462074844,30.3569660635819,
56.6273883152812));
#126093=CARTESIAN_POINT('Ctrl Pts',(0.772437302118265,30.3335281211712,
56.6322914670152));
#126094=CARTESIAN_POINT('Ctrl Pts',(0.772954640244863,30.3259076144078,
56.6338300590287));
#126095=CARTESIAN_POINT('Ctrl Pts',(0.773877471459437,30.3123742586365,
56.6364640180472));
#126096=CARTESIAN_POINT('Ctrl Pts',(0.774281759344064,30.306465840248,56.637580790813));
#126097=CARTESIAN_POINT('Ctrl Pts',(0.775177653612938,30.293419209587,56.6399737029599));
#126098=CARTESIAN_POINT('Ctrl Pts',(0.77567002350507,30.2862787488537,56.6412352213943));
#126099=CARTESIAN_POINT('Ctrl Pts',(0.77712445941937,30.265266708266,56.6448061673337));
#126100=CARTESIAN_POINT('Ctrl Pts',(0.778093178502888,30.2513742527611,
56.6469865534037));
#126101=CARTESIAN_POINT('Ctrl Pts',(0.784689935432296,30.1573501703635,
56.6605261228646));
#126102=CARTESIAN_POINT('Ctrl Pts',(0.790553974769039,30.0765178487816,
56.6662077882946));
#126103=CARTESIAN_POINT('Ctrl Pts',(0.806063510907355,29.8633650116075,
56.6656451293248));
#126104=CARTESIAN_POINT('Ctrl Pts',(0.815656604586156,29.7316125475259,
56.6495526434039));
#126105=CARTESIAN_POINT('Ctrl Pts',(0.826166746061048,29.5831461540704,
56.6131374478684));
#126106=CARTESIAN_POINT('Ctrl Pts',(0.827570139913132,29.5632499976581,
56.6078647504266));
#126107=CARTESIAN_POINT('Ctrl Pts',(0.829854328291138,29.5307598483869,
56.5986068797755));
#126108=CARTESIAN_POINT('Ctrl Pts',(0.830741985896256,29.5181069842943,
56.5948383663475));
#126109=CARTESIAN_POINT('Ctrl Pts',(0.832337806176316,29.4953167834712,
56.5877545672487));
#126110=CARTESIAN_POINT('Ctrl Pts',(0.833047629721722,29.485164066098,56.5844916172385));
#126111=CARTESIAN_POINT('Ctrl Pts',(0.834569600723171,29.4633660279139,
56.5772543759887));
#126112=CARTESIAN_POINT('Ctrl Pts',(0.835380649743124,29.4517319373144,
56.5732480833068));
#126113=CARTESIAN_POINT('Ctrl Pts',(0.837621661865729,29.4195466305778,
56.5617644194604));
#126114=CARTESIAN_POINT('Ctrl Pts',(0.839042451604891,29.3990961879455,
56.5540105845071));
#126115=CARTESIAN_POINT('Ctrl Pts',(0.847871545164079,29.2719069539899,
56.5029000673142));
#126116=CARTESIAN_POINT('Ctrl Pts',(0.854901810203552,29.1697508616464,
56.4489715324176));
#126117=CARTESIAN_POINT('Ctrl Pts',(0.867843281551346,28.9935758290465,
56.3311719757932));
#126118=CARTESIAN_POINT('Ctrl Pts',(0.873738399752646,28.9180269742054,
56.2705266337626));
#126119=CARTESIAN_POINT('Ctrl Pts',(0.881042755825898,28.8366476961067,
56.192653310532));
#126120=CARTESIAN_POINT('Ctrl Pts',(0.882087291892754,28.8252811193462,
56.1814592705049));
#126121=CARTESIAN_POINT('Ctrl Pts',(0.883648396481805,28.8087249421397,
56.1646792765745));
#126122=CARTESIAN_POINT('Ctrl Pts',(0.884155789803154,28.8034097488822,
56.1592177733404));
#126123=CARTESIAN_POINT('Ctrl Pts',(0.885068105851131,28.7939745280309,
56.1493887979365));
#126124=CARTESIAN_POINT('Ctrl Pts',(0.885471934599636,28.7898403750829,
56.1450352516483));
#126125=CARTESIAN_POINT('Ctrl Pts',(0.886375889732285,28.7806806084086,
56.1352843723342));
#126126=CARTESIAN_POINT('Ctrl Pts',(0.88687687662457,28.7756673070899,56.1298760271112));
#126127=CARTESIAN_POINT('Ctrl Pts',(0.888382867171218,28.76078025105,56.1136004676827));
#126128=CARTESIAN_POINT('Ctrl Pts',(0.889395227501982,28.7510143813196,
56.1026361482085));
#126129=CARTESIAN_POINT('Ctrl Pts',(0.891777961222555,28.7285593866664,
56.0767444311353));
#126130=CARTESIAN_POINT('Ctrl Pts',(0.893154679035589,28.7159862886877,
56.0617196057646));
#126131=CARTESIAN_POINT('Ctrl Pts',(0.898143930548396,28.6717555545062,
56.0069290121172));
#126132=CARTESIAN_POINT('Ctrl Pts',(0.901817792886701,28.6416578810171,
55.9659427518692));
#126133=CARTESIAN_POINT('Ctrl Pts',(0.914506057533618,28.5448501336338,
55.8206215257514));
#126134=CARTESIAN_POINT('Ctrl Pts',(0.923540887224526,28.4879032779091,
55.7102487288947));
#126135=CARTESIAN_POINT('Ctrl Pts',(0.934524493244932,28.4316602796097,
55.5630333153845));
#126136=CARTESIAN_POINT('Ctrl Pts',(0.936848123405035,28.4205713274763,
55.5311321359396));
#126137=CARTESIAN_POINT('Ctrl Pts',(0.940052720156528,28.4064332387933,
55.4860881432053));
#126138=CARTESIAN_POINT('Ctrl Pts',(0.940960112133307,28.4025628689944,
55.4732138377933));
#126139=CARTESIAN_POINT('Ctrl Pts',(0.942531789310143,28.396093430618,55.4507096223187));
#126140=CARTESIAN_POINT('Ctrl Pts',(0.943198320871191,28.3934242713645,
55.4411007623922));
#126141=CARTESIAN_POINT('Ctrl Pts',(0.944591957268216,28.3880013610972,
55.4208760517827));
#126142=CARTESIAN_POINT('Ctrl Pts',(0.945318444150124,28.3852658209177,
55.4102557780982));
#126143=CARTESIAN_POINT('Ctrl Pts',(0.947057532354182,28.3789398176874,
55.3846521176276));
#126144=CARTESIAN_POINT('Ctrl Pts',(0.948066805141481,28.3754519024687,
55.3696442495976));
#126145=CARTESIAN_POINT('Ctrl Pts',(0.951654600013756,28.3637209195867,
55.3157904183378));
#126146=CARTESIAN_POINT('Ctrl Pts',(0.954195847185852,28.3566586619238,
55.2766992129396));
#126147=CARTESIAN_POINT('Ctrl Pts',(0.960608477038097,28.3421848769875,
55.1761590171424));
#126148=CARTESIAN_POINT('Ctrl Pts',(0.964424727524717,28.3367868788208,
55.1144811052257));
#126149=CARTESIAN_POINT('Ctrl Pts',(0.973795099258164,28.3319518174995,
54.961540822956));
#126150=CARTESIAN_POINT('Ctrl Pts',(0.97929714832269,28.3365530150519,54.8703621973523));
#126151=CARTESIAN_POINT('Ctrl Pts',(0.987546786681617,28.3539117228408,
54.7400462640853));
#126152=CARTESIAN_POINT('Ctrl Pts',(0.99011849501523,28.360686374524,54.7002787648945));
#126153=CARTESIAN_POINT('Ctrl Pts',(0.993485357352461,28.3711465983728,
54.6499789235106));
#126154=CARTESIAN_POINT('Ctrl Pts',(0.994214910994948,28.3735044579729,
54.6391809407212));
#126155=CARTESIAN_POINT('Ctrl Pts',(0.995390352702229,28.3774444053126,
54.6219615512177));
#126156=CARTESIAN_POINT('Ctrl Pts',(0.995832464198432,28.3789576453801,
54.6155245036074));
#126157=CARTESIAN_POINT('Ctrl Pts',(0.996691663417114,28.3819577276792,
54.6030953252751));
#126158=CARTESIAN_POINT('Ctrl Pts',(0.997108475790868,28.3834396171674,
54.5971021972253));
#126159=CARTESIAN_POINT('Ctrl Pts',(0.998135483652145,28.3871563348902,
54.5824215272881));
#126160=CARTESIAN_POINT('Ctrl Pts',(0.998747715927455,28.389428068324,54.5737436067658));
#126161=CARTESIAN_POINT('Ctrl Pts',(1.00102901243452,28.3981033413843,54.5416641718702));
#126162=CARTESIAN_POINT('Ctrl Pts',(1.00272014057986,28.4049474384177,54.5183862415263));
#126163=CARTESIAN_POINT('Ctrl Pts',(1.00718530026382,28.424137671168,54.4580208052705));
#126164=CARTESIAN_POINT('Ctrl Pts',(1.00998807895293,28.43728477872,54.4212044542003));
#126165=CARTESIAN_POINT('Ctrl Pts',(1.01797729513375,28.4780893895311,54.3184961284334));
#126166=CARTESIAN_POINT('Ctrl Pts',(1.02320480885816,28.5087083946863,54.2538707123977));
#126167=CARTESIAN_POINT('Ctrl Pts',(1.03512347050194,28.5886228123156,54.109910463198));
#126168=CARTESIAN_POINT('Ctrl Pts',(1.04174799528417,28.6406304124562,54.0323407351921));
#126169=CARTESIAN_POINT('Ctrl Pts',(1.04949123279008,28.7112681920914,53.9440071906692));
#126170=CARTESIAN_POINT('Ctrl Pts',(1.0508400584708,28.7239494120389,53.9287178512361));
#126171=CARTESIAN_POINT('Ctrl Pts',(1.05297808378099,28.7446488621043,53.9046504280458));
#126172=CARTESIAN_POINT('Ctrl Pts',(1.05377430308946,28.75249252959,53.8957254471249));
#126173=CARTESIAN_POINT('Ctrl Pts',(1.05528189985961,28.7675989285154,53.8789029086026));
#126174=CARTESIAN_POINT('Ctrl Pts',(1.05599397217408,28.7748437448607,53.8709901466265));
#126175=CARTESIAN_POINT('Ctrl Pts',(1.05761964209106,28.7916327038708,53.8530052342212));
#126176=CARTESIAN_POINT('Ctrl Pts',(1.05853102383887,28.8012273367748,53.8429811426392));
#126177=CARTESIAN_POINT('Ctrl Pts',(1.06139667209143,28.8319616524653,53.8116639289647));
#126178=CARTESIAN_POINT('Ctrl Pts',(1.06333120326394,28.8535525653389,53.7908206680888));
#126179=CARTESIAN_POINT('Ctrl Pts',(1.06788218003509,28.9062255612992,53.7426515877071));
#126180=CARTESIAN_POINT('Ctrl Pts',(1.07047751114992,28.9377860812315,53.7158779265474));
#126181=CARTESIAN_POINT('Ctrl Pts',(1.08276478671506,29.0934265415283,53.5935127062661));
#126182=CARTESIAN_POINT('Ctrl Pts',(1.09195761566225,29.2295508095331,53.5145791717377));
#126183=CARTESIAN_POINT('Ctrl Pts',(1.10317170578295,29.3900128559393,53.449598139637));
#126184=CARTESIAN_POINT('Ctrl Pts',(1.10425507158038,29.4054534543692,53.4436116812001));
#126185=CARTESIAN_POINT('Ctrl Pts',(1.1058632136874,29.4282329461096,53.4351682938226));
#126186=CARTESIAN_POINT('Ctrl Pts',(1.10637800404369,29.4355043527415,53.432530545467));
#126187=CARTESIAN_POINT('Ctrl Pts',(1.10729804200894,29.4484570688819,53.427933681803));
#126188=CARTESIAN_POINT('Ctrl Pts',(1.10770211194395,29.4541309910689,53.4259545316262));
#126189=CARTESIAN_POINT('Ctrl Pts',(1.1085996984854,29.466701181022,53.4216459995717));
#126190=CARTESIAN_POINT('Ctrl Pts',(1.10909400146366,29.4736019768989,53.4193311234645));
#126191=CARTESIAN_POINT('Ctrl Pts',(1.11056001178771,29.4940113049587,53.4126332711549));
#126192=CARTESIAN_POINT('Ctrl Pts',(1.11153852804422,29.5075605748194,53.4083778493662));
#126193=CARTESIAN_POINT('Ctrl Pts',(1.11910413224452,29.6118816777519,53.3770732230114));
#126194=CARTESIAN_POINT('Ctrl Pts',(1.12601146325622,29.7047489583111,53.3576387176011));
#126195=CARTESIAN_POINT('Ctrl Pts',(1.14132830868975,29.9136428125962,53.3322190242885));
#126196=CARTESIAN_POINT('Ctrl Pts',(1.14967533091106,30.0296951607165,53.3302461267074));
#126197=CARTESIAN_POINT('Ctrl Pts',(1.15915999706084,30.1668561083711,53.3422319109193));
#126198=CARTESIAN_POINT('Ctrl Pts',(1.16065619284714,30.1886428967115,53.3445695621347));
#126199=CARTESIAN_POINT('Ctrl Pts',(1.1630586979109,30.2238580689484,53.3490523275096));
#126200=CARTESIAN_POINT('Ctrl Pts',(1.16397313375916,30.2373168109122,53.3509331721888));
#126201=CARTESIAN_POINT('Ctrl Pts',(1.1655980449246,30.2613253048975,53.3545883541528));
#126202=CARTESIAN_POINT('Ctrl Pts',(1.16631045208938,30.2718836795725,53.3563000051061));
#126203=CARTESIAN_POINT('Ctrl Pts',(1.16781813103271,30.2942928872174,53.3601546690648));
#126204=CARTESIAN_POINT('Ctrl Pts',(1.16861250303092,30.3061384919742,53.3623247423918));
#126205=CARTESIAN_POINT('Ctrl Pts',(1.17075643389708,30.338203111707,53.3685589382604));
#126206=CARTESIAN_POINT('Ctrl Pts',(1.17209811365845,30.3583722912001,53.3728704278661));
#126207=CARTESIAN_POINT('Ctrl Pts',(1.17505597317585,30.4030134065257,53.3832835671536));
#126208=CARTESIAN_POINT('Ctrl Pts',(1.1766663398387,30.4274375227992,53.3895686624122));
#126209=CARTESIAN_POINT('Ctrl Pts',(1.18177668028163,30.5051478955028,53.4114586140517));
#126210=CARTESIAN_POINT('Ctrl Pts',(1.18521766952564,30.5578021788056,53.4291736117712));
#126211=CARTESIAN_POINT('Ctrl Pts',(1.19515096346947,30.7083264333205,53.4883417151074));
#126212=CARTESIAN_POINT('Ctrl Pts',(1.20152694237223,30.8032261729406,53.5365583087831));
#126213=CARTESIAN_POINT('Ctrl Pts',(1.21049707279574,30.9233995796738,53.6128461814064));
#126214=CARTESIAN_POINT('Ctrl Pts',(1.21281057002896,30.9532745631696,53.633204596608));
#126215=CARTESIAN_POINT('Ctrl Pts',(1.21588022871239,30.9910653381725,53.6607991207853));
#126216=CARTESIAN_POINT('Ctrl Pts',(1.21658401888085,30.9996085963038,53.6671638739113));
#126217=CARTESIAN_POINT('Ctrl Pts',(1.21772775460492,31.0132854923741,53.6775586602082));
#126218=CARTESIAN_POINT('Ctrl Pts',(1.21816427452302,31.0184576772661,53.6815378116196));
#126219=CARTESIAN_POINT('Ctrl Pts',(1.21900877905731,31.0283689957166,53.6892560705806));
#126220=CARTESIAN_POINT('Ctrl Pts',(1.2194164563968,31.0331114052629,53.6929907193143));
#126221=CARTESIAN_POINT('Ctrl Pts',(1.22038104170437,31.0442355238733,53.7018493335292));
#126222=CARTESIAN_POINT('Ctrl Pts',(1.22093941704082,31.0505999455364,53.706994690768));
#126223=CARTESIAN_POINT('Ctrl Pts',(1.22218434736042,31.0646298189081,53.7185091992837));
#126224=CARTESIAN_POINT('Ctrl Pts',(1.22287231140984,31.0722764984545,53.7249006222609));
#126225=CARTESIAN_POINT('Ctrl Pts',(1.22483234739306,31.0937748572291,53.743200005788));
#126226=CARTESIAN_POINT('Ctrl Pts',(1.22611350427427,31.107488292973,53.7552673839139));
#126227=CARTESIAN_POINT('Ctrl Pts',(1.23061560482753,31.1545949602295,53.7981144612208));
#126228=CARTESIAN_POINT('Ctrl Pts',(1.23388712409717,31.1869244959774,53.8300307286654));
#126229=CARTESIAN_POINT('Ctrl Pts',(1.24794376716423,31.3191713370836,53.9717162195025));
#126230=CARTESIAN_POINT('Ctrl Pts',(1.25880023520702,31.4055088503652,54.0932791123764));
#126231=CARTESIAN_POINT('Ctrl Pts',(1.27048477212937,31.4845138953527,54.2435422931743));
#126232=CARTESIAN_POINT('Ctrl Pts',(1.2719385409479,31.4940650473768,54.2625859544202));
#126233=CARTESIAN_POINT('Ctrl Pts',(1.27428702924811,31.5090307050563,54.2939106096332));
#126234=CARTESIAN_POINT('Ctrl Pts',(1.27518928693818,31.5146664612768,54.3060825514971));
#126235=CARTESIAN_POINT('Ctrl Pts',(1.27680084095772,31.5245243762305,54.3280658723908));
#126236=CARTESIAN_POINT('Ctrl Pts',(1.27751194612753,31.5288002881486,54.3378521814277));
#126237=CARTESIAN_POINT('Ctrl Pts',(1.27902552219088,31.537740727347,54.3588625951354));
#126238=CARTESIAN_POINT('Ctrl Pts',(1.27982700722774,31.5423771441183,54.3700980434219));
#126239=CARTESIAN_POINT('Ctrl Pts',(1.28201229344357,31.5547447610464,54.4010240629602));
#126240=CARTESIAN_POINT('Ctrl Pts',(1.28338767433082,31.5622247230256,54.4208131342422));
#126241=CARTESIAN_POINT('Ctrl Pts',(1.28643158955148,31.5780725691943,54.4652833983786));
#126242=CARTESIAN_POINT('Ctrl Pts',(1.28809375679505,31.5862424285784,54.490029467944));
#126243=CARTESIAN_POINT('Ctrl Pts',(1.29343886300011,31.6108588879297,54.5709181818392));
#126244=CARTESIAN_POINT('Ctrl Pts',(1.29705621264224,31.6249308483184,54.6277392667515));
#126245=CARTESIAN_POINT('Ctrl Pts',(1.30714294227936,31.6560116465503,54.7892559436727));
#126246=CARTESIAN_POINT('Ctrl Pts',(1.31351093898179,31.6660595218301,54.894986156346));
#126247=CARTESIAN_POINT('Ctrl Pts',(1.3202157917438,31.6659997347684,55.0009400806026));
#126248=CARTESIAN_POINT('Ctrl Pts',(1.32021594204516,31.6659997334265,55.00094245575));
#126249=CARTESIAN_POINT('Ctrl Pts',(1.32220988897509,31.6659819085261,55.032451923777));
#126250=CARTESIAN_POINT('Ctrl Pts',(1.32423296675841,31.6650701672133,55.06395268441));
#126251=CARTESIAN_POINT('Ctrl Pts',(1.32682078314898,31.6628108339044,55.1033406294786));
#126252=CARTESIAN_POINT('Ctrl Pts',(1.32734478152174,31.6622989805633,55.1112710577923));
#126253=CARTESIAN_POINT('Ctrl Pts',(1.32826702746228,31.6613039342568,55.1251430018115));
#126254=CARTESIAN_POINT('Ctrl Pts',(1.32866397223534,31.6608455471467,55.1310862261613));
#126255=CARTESIAN_POINT('Ctrl Pts',(1.32945879277765,31.6598681994625,55.1429287635264));
#126256=CARTESIAN_POINT('Ctrl Pts',(1.32985664277534,31.659349673797,55.1488278524614));
#126257=CARTESIAN_POINT('Ctrl Pts',(1.33072932606067,31.6581487459355,55.1617030106065));
#126258=CARTESIAN_POINT('Ctrl Pts',(1.33120480792667,31.6574537805996,55.1686774672297));
#126259=CARTESIAN_POINT('Ctrl Pts',(1.33253752092831,31.655392562013,55.1881190070045));
#126260=CARTESIAN_POINT('Ctrl Pts',(1.33339975384111,31.653929538601,55.2005750558197));
#126261=CARTESIAN_POINT('Ctrl Pts',(1.33796731482122,31.6454975568926,55.2659813370139));
#126262=CARTESIAN_POINT('Ctrl Pts',(1.34177817048429,31.6361266114523,55.3185857050561));
#126263=CARTESIAN_POINT('Ctrl Pts',(1.35078326094407,31.6083821889067,55.4401682876052));
#126264=CARTESIAN_POINT('Ctrl Pts',(1.35600139652401,31.5880703088527,55.5085993456218));
#126265=CARTESIAN_POINT('Ctrl Pts',(1.36116735710803,31.5634376788384,55.575515963626));
#126266=CARTESIAN_POINT('Ctrl Pts',(1.16624544379888,31.5634376782622,55.5755159651914));
#126267=CARTESIAN_POINT('Ctrl Pts',(1.16623403829253,31.5634966974797,55.5753556345072));
#126268=CARTESIAN_POINT('Ctrl Pts',(1.16622263360327,31.5635556920785,55.5751952946246));
#126269=CARTESIAN_POINT('Ctrl Pts',(1.16549978278659,31.5672935887586,55.5650313383302));
#126270=CARTESIAN_POINT('Ctrl Pts',(1.16479155412673,31.5708765010653,55.5549924630923));
#126271=CARTESIAN_POINT('Ctrl Pts',(1.16321387684814,31.5786777090593,55.5324534860398));
#126272=CARTESIAN_POINT('Ctrl Pts',(1.16234616653486,31.5828444033223,55.5199361839881));
#126273=CARTESIAN_POINT('Ctrl Pts',(1.1601383138976,31.5931230899973,55.4877883527716));
#126274=CARTESIAN_POINT('Ctrl Pts',(1.15880512462655,31.5990213017183,55.4680914366092));
#126275=CARTESIAN_POINT('Ctrl Pts',(1.14770618951907,31.6454494232188,55.3019122563605));
#126276=CARTESIAN_POINT('Ctrl Pts',(1.13864990821346,31.6661227755638,55.1506356284136));
#126277=CARTESIAN_POINT('Ctrl Pts',(1.12530414052524,31.6659471960532,54.9342472468964));
#126278=CARTESIAN_POINT('Ctrl Pts',(1.12127414953928,31.6621607415656,54.8699108188114));
#126279=CARTESIAN_POINT('Ctrl Pts',(1.1162752786559,31.6532510523558,54.793932828679));
#126280=CARTESIAN_POINT('Ctrl Pts',(1.11547760114754,31.6517091741316,54.7819185831932));
#126281=CARTESIAN_POINT('Ctrl Pts',(1.11421378868947,31.6490819982911,54.7630773716748));
#126282=CARTESIAN_POINT('Ctrl Pts',(1.1137523699807,31.6480849417241,54.7562382526835));
#126283=CARTESIAN_POINT('Ctrl Pts',(1.11288181022897,31.6461337943836,54.7434142255889));
#126284=CARTESIAN_POINT('Ctrl Pts',(1.11247321311694,31.6451895641239,54.7374280632467));
#126285=CARTESIAN_POINT('Ctrl Pts',(1.11150212154691,31.6428781770869,54.723276606843));
#126286=CARTESIAN_POINT('Ctrl Pts',(1.1109380953463,31.6414827909169,54.7151161974368));
#126287=CARTESIAN_POINT('Ctrl Pts',(1.1090222045819,31.6365634252889,54.6875838585901));
#126288=CARTESIAN_POINT('Ctrl Pts',(1.10765619497171,31.632757006768,54.668264919935));
#126289=CARTESIAN_POINT('Ctrl Pts',(1.10423986519777,31.6224862684322,54.6206070041068));
#126290=CARTESIAN_POINT('Ctrl Pts',(1.10217406604258,31.6156210860061,54.5923616185086));
#126291=CARTESIAN_POINT('Ctrl Pts',(1.09432055537429,31.5869811140024,54.4866582845914));
#126292=CARTESIAN_POINT('Ctrl Pts',(1.08842676319786,31.5603442806905,54.4106324482154));
#126293=CARTESIAN_POINT('Ctrl Pts',(1.07530636567537,31.4883412133279,54.2446965723646));
#126294=CARTESIAN_POINT('Ctrl Pts',(1.0681466313918,31.4401076398284,54.1563536337982));
#126295=CARTESIAN_POINT('Ctrl Pts',(1.0599068869644,31.3731329048861,54.0563594458513));
#126296=CARTESIAN_POINT('Ctrl Pts',(1.05855633702873,31.3617708975396,54.0400356506754));
#126297=CARTESIAN_POINT('Ctrl Pts',(1.05641641155044,31.3431562545548,54.0142878180469));
#126298=CARTESIAN_POINT('Ctrl Pts',(1.05561999068524,31.336090610107,54.0047316321445));
#126299=CARTESIAN_POINT('Ctrl Pts',(1.05411252219701,31.3224563140401,53.9866983288307));
#126300=CARTESIAN_POINT('Ctrl Pts',(1.05340077474465,31.3159069207834,53.9782074749021));
#126301=CARTESIAN_POINT('Ctrl Pts',(1.05177656430949,31.3007067251372,53.9588899944462));
#126302=CARTESIAN_POINT('Ctrl Pts',(1.05086630658539,31.2920018288,53.9481067914974));
#126303=CARTESIAN_POINT('Ctrl Pts',(1.04800717911774,31.2640807632862,53.9143891160484));
#126304=CARTESIAN_POINT('Ctrl Pts',(1.04607791873211,31.2443801830687,53.8918622359251));
#126305=CARTESIAN_POINT('Ctrl Pts',(1.03901434101723,31.169237342049,53.8104719438515));
#126306=CARTESIAN_POINT('Ctrl Pts',(1.03402986482835,31.1101379987447,53.7551351731194));
#126307=CARTESIAN_POINT('Ctrl Pts',(1.02299657396941,30.9698592406278,53.6417545557324));
#126308=CARTESIAN_POINT('Ctrl Pts',(1.0169913574635,30.887028736885,53.586269443464));
#126309=CARTESIAN_POINT('Ctrl Pts',(1.00882279596341,30.7742378446537,53.5245483071496));
#126310=CARTESIAN_POINT('Ctrl Pts',(1.00694867667202,30.7483637088535,53.5112577600136));
#126311=CARTESIAN_POINT('Ctrl Pts',(1.00438776453645,30.7132572841634,53.4943713688402));
#126312=CARTESIAN_POINT('Ctrl Pts',(1.00373427929968,30.7043200378587,53.4901699430492));
#126313=CARTESIAN_POINT('Ctrl Pts',(1.0026944037241,30.6901428265271,53.4836584599552));
#126314=CARTESIAN_POINT('Ctrl Pts',(1.00231115943869,30.6849272256988,53.4812954599143));
#126315=CARTESIAN_POINT('Ctrl Pts',(1.00150795393641,30.6740187393585,53.4764208401987));
#126316=CARTESIAN_POINT('Ctrl Pts',(1.00108768419088,30.6683238412235,53.4739141715872));
#126317=CARTESIAN_POINT('Ctrl Pts',(1.00003978700348,30.6541529439843,53.4677712337712));
#126318=CARTESIAN_POINT('Ctrl Pts',(0.999409936846762,30.6456606152799,
53.4641733736404));
#126319=CARTESIAN_POINT('Ctrl Pts',(0.996980272384737,30.6129812800444,
53.450647383833));
#126320=CARTESIAN_POINT('Ctrl Pts',(0.99515467477545,30.5885930081612,53.441219173195));
#126321=CARTESIAN_POINT('Ctrl Pts',(0.990223071858972,30.5229061866649,
53.4175866802113));
#126322=CARTESIAN_POINT('Ctrl Pts',(0.987081225495934,30.4812548006023,
53.4044260799589));
#126323=CARTESIAN_POINT('Ctrl Pts',(0.973275756936014,30.2974815630265,
53.3542097944964));
#126324=CARTESIAN_POINT('Ctrl Pts',(0.96251745536523,30.1512951460901,53.3343930279766));
#126325=CARTESIAN_POINT('Ctrl Pts',(0.950591734803027,29.9785721445165,
53.333937727724));
#126326=CARTESIAN_POINT('Ctrl Pts',(0.948827029643659,29.9527534430484,
53.3344698921893));
#126327=CARTESIAN_POINT('Ctrl Pts',(0.946183708033942,29.9137023296954,
53.3361836890162));
#126328=CARTESIAN_POINT('Ctrl Pts',(0.945291536352232,29.9004555142163,
53.336923658514));
#126329=CARTESIAN_POINT('Ctrl Pts',(0.94369091073918,29.8765754986089,53.3385439548971));
#126330=CARTESIAN_POINT('Ctrl Pts',(0.94298075034712,29.8659393610362,53.3393683275592));
#126331=CARTESIAN_POINT('Ctrl Pts',(0.941461618673189,29.8431033009809,
53.3413591098246));
#126332=CARTESIAN_POINT('Ctrl Pts',(0.940653709210325,29.8309067927053,
53.3425580922916));
#126333=CARTESIAN_POINT('Ctrl Pts',(0.93843092168224,29.7972184928342,53.3462455734345));
#126334=CARTESIAN_POINT('Ctrl Pts',(0.937024966057036,29.7757597774687,
53.3490183418476));
#126335=CARTESIAN_POINT('Ctrl Pts',(0.933902588934588,29.7278298552886,
53.356163353642));
#126336=CARTESIAN_POINT('Ctrl Pts',(0.932193062671097,29.7013977718548,
53.3607586102609));
#126337=CARTESIAN_POINT('Ctrl Pts',(0.926628040775296,29.6149603799195,
53.3779461628909));
#126338=CARTESIAN_POINT('Ctrl Pts',(0.922844664320479,29.5555363798742,
53.3932121901108));
#126339=CARTESIAN_POINT('Ctrl Pts',(0.913593322738773,29.4115448535048,
53.4388057515699));
#126340=CARTESIAN_POINT('Ctrl Pts',(0.908176262808959,29.328336818378,53.4727561737609));
#126341=CARTESIAN_POINT('Ctrl Pts',(0.899904699423246,29.2104833508854,
53.5323445526535));
#126342=CARTESIAN_POINT('Ctrl Pts',(0.897209163146009,29.1734401492577,
53.5528831405394));
#126343=CARTESIAN_POINT('Ctrl Pts',(0.893701527215476,29.1276350308805,
53.580612463476));
#126344=CARTESIAN_POINT('Ctrl Pts',(0.892961937286515,29.1181062444252,
53.5865131747315));
#126345=CARTESIAN_POINT('Ctrl Pts',(0.891774173536246,29.1030233592756,
53.5960651460512));
#126346=CARTESIAN_POINT('Ctrl Pts',(0.891329915986969,29.0974301284945,
53.5996544028974));
#126347=CARTESIAN_POINT('Ctrl Pts',(0.890470221332444,29.0867027366668,
53.6066292918335));
#126348=CARTESIAN_POINT('Ctrl Pts',(0.890055095152861,29.0815656347868,
53.610010024027));
#126349=CARTESIAN_POINT('Ctrl Pts',(0.88903715500841,29.0690707331154,53.6183324356169));
#126350=CARTESIAN_POINT('Ctrl Pts',(0.888432379421689,29.0617334892426,
53.6233044982939));
#126351=CARTESIAN_POINT('Ctrl Pts',(0.886208436377775,29.0350530367429,
53.6416967862867));
#126352=CARTESIAN_POINT('Ctrl Pts',(0.884568532850984,29.0159561887648,
53.6554674039132));
#126353=CARTESIAN_POINT('Ctrl Pts',(0.880274988250084,28.9672784494778,
53.69216118529));
#126354=CARTESIAN_POINT('Ctrl Pts',(0.877594993253211,28.9381672569238,
53.7156842112387));
#126355=CARTESIAN_POINT('Ctrl Pts',(0.869806054999817,28.8566070072196,
53.7862577004912));
#126356=CARTESIAN_POINT('Ctrl Pts',(0.864651643722582,28.8063166503866,
53.8356813250772));
#126357=CARTESIAN_POINT('Ctrl Pts',(0.852526539317233,28.6946564412618,
53.9602798842364));
#126358=CARTESIAN_POINT('Ctrl Pts',(0.845631044149412,28.6364131696759,
54.0379311614804));
#126359=CARTESIAN_POINT('Ctrl Pts',(0.837635025485726,28.5747386586289,
54.1371084991372));
#126360=CARTESIAN_POINT('Ctrl Pts',(0.836284189287029,28.5645378103655,
54.1541867847296));
#126361=CARTESIAN_POINT('Ctrl Pts',(0.834144343814903,28.5487371450569,
54.1817498965096));
#126362=CARTESIAN_POINT('Ctrl Pts',(0.833348275666138,28.5429396920421,
54.1921185868982));
#126363=CARTESIAN_POINT('Ctrl Pts',(0.831841815384134,28.5321255584706,
54.21195470068));
#126364=CARTESIAN_POINT('Ctrl Pts',(0.831130720372282,28.5270883629943,
54.221410192333));
#126365=CARTESIAN_POINT('Ctrl Pts',(0.829508494149889,28.5157548244046,
54.2431884452231));
#126366=CARTESIAN_POINT('Ctrl Pts',(0.828599559893766,28.5095200439121,
54.2555424858402));
#126367=CARTESIAN_POINT('Ctrl Pts',(0.825746749503835,28.4903271304715,
54.2947805943529));
#126368=CARTESIAN_POINT('Ctrl Pts',(0.823822384930057,28.4779365815331,
54.3219367958556));
#126369=CARTESIAN_POINT('Ctrl Pts',(0.816519047277932,28.4332119272116,
54.4273723233963));
#126370=CARTESIAN_POINT('Ctrl Pts',(0.811307955225365,28.4061327360044,
54.507743464591));
#126371=CARTESIAN_POINT('Ctrl Pts',(0.799647107030315,28.3591662828282,
54.6926375990911));
#126372=CARTESIAN_POINT('Ctrl Pts',(0.793245369348885,28.3429325806394,
54.7976900760107));
#126373=CARTESIAN_POINT('Ctrl Pts',(0.785068161700053,28.335562014142,54.9248006017527));
#126374=CARTESIAN_POINT('Ctrl Pts',(0.783685474318799,28.334737404848,54.9460635019496));
#126375=CARTESIAN_POINT('Ctrl Pts',(0.781704316928369,28.3341484662617,
54.9760952577574));
#126376=CARTESIAN_POINT('Ctrl Pts',(0.781122965769341,28.334045789722,54.984856353958));
#126377=CARTESIAN_POINT('Ctrl Pts',(0.780132315556956,28.3339889628622,
54.9996898057422));
#126378=CARTESIAN_POINT('Ctrl Pts',(0.779724974732296,28.3339988984451,
55.0057619937108));
#126379=CARTESIAN_POINT('Ctrl Pts',(0.778866540186639,28.3340893727542,
55.0184987328981));
#126380=CARTESIAN_POINT('Ctrl Pts',(0.778415105289353,28.3341767077085,
55.025162989298));
#126381=CARTESIAN_POINT('Ctrl Pts',(0.777192885164705,28.3345198133665,
55.0431200885004));
#126382=CARTESIAN_POINT('Ctrl Pts',(0.77641819953582,28.3348504484209,55.0544109132017));
#126383=CARTESIAN_POINT('Ctrl Pts',(0.772236304599404,28.3372384702508,
55.1149211838566));
#126384=CARTESIAN_POINT('Ctrl Pts',(0.768735890934266,28.341363235936,55.1640301718498));
#126385=CARTESIAN_POINT('Ctrl Pts',(0.75384952111547,28.3677864031852,55.3691239121344));
#126386=CARTESIAN_POINT('Ctrl Pts',(0.742214657580388,28.4099837168053,
55.5217660675314));
#126387=CARTESIAN_POINT('Ctrl Pts',(0.729199729424099,28.4850158501175,
55.6937445200622));
#126388=CARTESIAN_POINT('Ctrl Pts',(0.72713997536398,28.4977717882302,55.7209500921857));
#126389=CARTESIAN_POINT('Ctrl Pts',(0.72417509256806,28.5174218994855,55.7600702611463));
#126390=CARTESIAN_POINT('Ctrl Pts',(0.723250262152292,28.5237382485796,
55.7722667200562));
#126391=CARTESIAN_POINT('Ctrl Pts',(0.721611635753326,28.535261719143,55.7938596400568));
#126392=CARTESIAN_POINT('Ctrl Pts',(0.72089582484082,28.5404101869745,55.803286341546));
#126393=CARTESIAN_POINT('Ctrl Pts',(0.719397961123313,28.5514232858508,
55.8229955067832));
#126394=CARTESIAN_POINT('Ctrl Pts',(0.718616642452789,28.5573070822822,
55.8332666189716));
#126395=CARTESIAN_POINT('Ctrl Pts',(0.716548754468793,28.5732465218691,
55.8604164575752));
#126396=CARTESIAN_POINT('Ctrl Pts',(0.715269103039929,28.5834922957881,
55.8771818196099));
#126397=CARTESIAN_POINT('Ctrl Pts',(0.707913424028041,28.6445549642229,
55.9732387813358));
#126398=CARTESIAN_POINT('Ctrl Pts',(0.702083065101889,28.7017278787835,
56.0482927723663));
#126399=CARTESIAN_POINT('Ctrl Pts',(0.690587632322136,28.8277413581298,
56.1874849758101));
#126400=CARTESIAN_POINT('Ctrl Pts',(0.684939420233994,28.8962656891405,
56.2514308033437));
#126401=CARTESIAN_POINT('Ctrl Pts',(0.67672268997073,28.9988126347639,56.3321200353707));
#126402=CARTESIAN_POINT('Ctrl Pts',(0.674360470722042,29.0285854034851,
56.3539841775009));
#126403=CARTESIAN_POINT('Ctrl Pts',(0.671234809158863,29.0679126331245,
56.3808998108574));
#126404=CARTESIAN_POINT('Ctrl Pts',(0.670526040649685,29.0768259980924,
56.3868745056533));
#126405=CARTESIAN_POINT('Ctrl Pts',(0.669375955721784,29.0912686810264,
56.3963546260907));
#126406=CARTESIAN_POINT('Ctrl Pts',(0.668938124725499,29.0967622029471,
56.3999144010123));
#126407=CARTESIAN_POINT('Ctrl Pts',(0.668079047827891,29.1075282332294,
56.4068009852452));
#126408=CARTESIAN_POINT('Ctrl Pts',(0.667657999454671,29.1127986741173,
56.4101307277259));
#126409=CARTESIAN_POINT('Ctrl Pts',(0.666609254673614,29.1259138992273,
56.4183139944637));
#126410=CARTESIAN_POINT('Ctrl Pts',(0.665979347765396,29.133780469857,56.4231320438587));
#126411=CARTESIAN_POINT('Ctrl Pts',(0.663556970511623,29.1640060283959,
56.4413008871406));
#126412=CARTESIAN_POINT('Ctrl Pts',(0.661739036458412,29.1866356999515,
56.4541913568609));
#126413=CARTESIAN_POINT('Ctrl Pts',(0.656835581106417,29.2477549135031,
56.4871335917686));
#126414=CARTESIAN_POINT('Ctrl Pts',(0.65371484967794,29.2867407747695,56.506220368829));
#126415=CARTESIAN_POINT('Ctrl Pts',(0.640076189821123,29.4589623937029,
56.582350519456));
#126416=CARTESIAN_POINT('Ctrl Pts',(0.629462598419139,29.5986092714402,
56.6234086133886));
#126417=CARTESIAN_POINT('Ctrl Pts',(0.617561620180513,29.7686874948643,
56.6500879181067));
#126418=CARTESIAN_POINT('Ctrl Pts',(0.615701457171254,29.7956552060657,
56.653644147925));
#126419=CARTESIAN_POINT('Ctrl Pts',(0.612957121000256,29.835998568582,56.657962130611));
#126420=CARTESIAN_POINT('Ctrl Pts',(0.612057486776425,29.8493147962743,
56.6592253865871));
#126421=CARTESIAN_POINT('Ctrl Pts',(0.610447721933842,29.8733009036232,
56.661209698211));
#126422=CARTESIAN_POINT('Ctrl Pts',(0.609735821961458,29.8839651165113,
56.6619886393708));
#126423=CARTESIAN_POINT('Ctrl Pts',(0.608217440895881,29.9068273772939,
56.6634374293711));
#126424=CARTESIAN_POINT('Ctrl Pts',(0.607411978681493,29.919026839703,56.6640758936066));
#126425=CARTESIAN_POINT('Ctrl Pts',(0.60520759669882,29.9526008428531,56.665462910222));
#126426=CARTESIAN_POINT('Ctrl Pts',(0.603817320110536,29.9739849476055,
56.6659341733854));
#126427=CARTESIAN_POINT('Ctrl Pts',(0.595896665760208,30.0968653934603,
56.6662754507159));
#126428=CARTESIAN_POINT('Ctrl Pts',(0.589651416925288,30.1981760767792,
56.6572828877345));
#126429=CARTESIAN_POINT('Ctrl Pts',(0.576644099756275,30.4076116534788,
56.6192003237016));
#126430=CARTESIAN_POINT('Ctrl Pts',(0.569920155937744,30.5148861087348,
56.5883458173367));
#126431=CARTESIAN_POINT('Ctrl Pts',(0.561662264105647,30.633149300932,56.5410823750858));
#126432=CARTESIAN_POINT('Ctrl Pts',(0.560612884267485,30.6479462416258,
56.5349197196464));
#126433=CARTESIAN_POINT('Ctrl Pts',(0.559045953680191,30.6696561357093,
56.5255080955093));
#126434=CARTESIAN_POINT('Ctrl Pts',(0.558537676427858,30.6766398528819,
56.5224233292216));
#126435=CARTESIAN_POINT('Ctrl Pts',(0.557625806109177,30.6890592359119,
56.5168352517106));
#126436=CARTESIAN_POINT('Ctrl Pts',(0.55722333295034,30.6945029726856,56.5143504978949));
#126437=CARTESIAN_POINT('Ctrl Pts',(0.556325795834287,30.7065577552782,
56.5087695076465));
#126438=CARTESIAN_POINT('Ctrl Pts',(0.555829912306552,30.7131617844598,
56.5056591755241));
#126439=CARTESIAN_POINT('Ctrl Pts',(0.554343599794483,30.7327956957268,
56.4962539464864));
#126440=CARTESIAN_POINT('Ctrl Pts',(0.553345980772109,30.7457638374317,
56.4898327648505));
#126441=CARTESIAN_POINT('Ctrl Pts',(0.546088146329676,30.8387189767206,
56.4422882825654));
#126442=CARTESIAN_POINT('Ctrl Pts',(0.539537884083121,30.915336030933,56.3949199888804));
#126443=CARTESIAN_POINT('Ctrl Pts',(0.524133826461675,31.0856074310675,
56.2695589093804));
#126444=CARTESIAN_POINT('Ctrl Pts',(0.51534630348892,31.1753074655953,56.1870071311232));
#126445=CARTESIAN_POINT('Ctrl Pts',(0.505485110241221,31.2694579066818,
56.0791202099465));
#126446=CARTESIAN_POINT('Ctrl Pts',(0.504008422704584,31.2833609669245,
56.0625481210254));
#126447=CARTESIAN_POINT('Ctrl Pts',(0.501633853707625,31.3053884812245,
56.0352285593731));
#126448=CARTESIAN_POINT('Ctrl Pts',(0.500728035043655,31.3137118554183,
56.0246455175189));
#126449=CARTESIAN_POINT('Ctrl Pts',(0.499116706646434,31.3283712533504,
56.0055340115715));
#126450=CARTESIAN_POINT('Ctrl Pts',(0.498409304206956,31.3347556301056,
55.9970437563527));
#126451=CARTESIAN_POINT('Ctrl Pts',(0.496910589125443,31.3481689769721,
55.9788462723328));
#126452=CARTESIAN_POINT('Ctrl Pts',(0.496120185035914,31.355175316799,55.9691230513945));
#126453=CARTESIAN_POINT('Ctrl Pts',(0.493983313289197,31.3739259121142,
55.9425004312645));
#126454=CARTESIAN_POINT('Ctrl Pts',(0.492644753405512,31.3854631966573,
55.9254573282705));
#126455=CARTESIAN_POINT('Ctrl Pts',(0.484129435350948,31.4574196212838,
55.8147991138387));
#126456=CARTESIAN_POINT('Ctrl Pts',(0.477309236783129,31.5086369027444,
55.7155336274773));
#126457=CARTESIAN_POINT('Ctrl Pts',(0.469715587863468,31.554331224466,55.5998157085011));
#126458=CARTESIAN_POINT('Ctrl Pts',(0.468923766207712,31.5589558739021,
55.5876911645927));
#126459=CARTESIAN_POINT('Ctrl Pts',(0.468131466136093,31.5634376737814,
55.5755159773639));
#126460=CARTESIAN_POINT('Origin',(-1.54592528053767,-30.,125.));
#126461=CARTESIAN_POINT('',(0.904074719503818,-27.9452506257245,124.99839643692));
#126462=CARTESIAN_POINT('Ctrl Pts',(0.452117106605179,-31.2520409112987,
126.629230222815));
#126463=CARTESIAN_POINT('Ctrl Pts',(0.455981894727876,-31.3083783410325,
126.585935686613));
#126464=CARTESIAN_POINT('Ctrl Pts',(0.459846682850573,-31.3625576973326,
126.539646253954));
#126465=CARTESIAN_POINT('Ctrl Pts',(0.463711470973271,-31.4142452973653,
126.490606521313));
#126466=CARTESIAN_POINT('Ctrl Pts',(0.467571428034043,-31.4658682868712,
126.441628089312));
#126467=CARTESIAN_POINT('Ctrl Pts',(0.471431385094814,-31.5150053569671,
126.389906519012));
#126468=CARTESIAN_POINT('Ctrl Pts',(0.475291342155586,-31.5613556938613,
126.335726753399));
#126469=CARTESIAN_POINT('Ctrl Pts',(0.479148671756006,-31.6076744802303,
126.281583867779));
#126470=CARTESIAN_POINT('Ctrl Pts',(0.483006001356426,-31.6512099818744,
126.224986474436));
#126471=CARTESIAN_POINT('Ctrl Pts',(0.486863330956846,-31.6916990980054,
126.166255428415));
#126472=CARTESIAN_POINT('Ctrl Pts',(0.490719324021933,-31.7321741849659,
126.107544732255));
#126473=CARTESIAN_POINT('Ctrl Pts',(0.49457531708702,-31.7696047062383,
126.0467022504));
#126474=CARTESIAN_POINT('Ctrl Pts',(0.498431310152108,-31.8037696906984,
125.984079501574));
#126475=CARTESIAN_POINT('Ctrl Pts',(0.502287255796065,-31.8379342549964,
125.921457522884));
#126476=CARTESIAN_POINT('Ctrl Pts',(0.506143201440022,-31.8688331313069,
125.857055747879));
#126477=CARTESIAN_POINT('Ctrl Pts',(0.509999147083979,-31.896291146279,
125.791250561481));
#126478=CARTESIAN_POINT('Ctrl Pts',(0.513859005452489,-31.9237770235862,
125.725378600913));
#126479=CARTESIAN_POINT('Ctrl Pts',(0.517718863821,-31.9478148798075,125.658100834341));
#126480=CARTESIAN_POINT('Ctrl Pts',(0.521578722189511,-31.9682779451068,
125.589813100318));
#126481=CARTESIAN_POINT('Ctrl Pts',(0.525440585853742,-31.9887516414949,
125.52148988906));
#126482=CARTESIAN_POINT('Ctrl Pts',(0.529302449517972,-32.0056467333534,
125.452156137726));
#126483=CARTESIAN_POINT('Ctrl Pts',(0.533164313182203,-32.0188872512256,
125.382219608784));
#126484=CARTESIAN_POINT('Ctrl Pts',(0.537033128459735,-32.032151602917,
125.312157189405));
#126485=CARTESIAN_POINT('Ctrl Pts',(0.540901943737267,-32.0417481756389,
125.241490307152));
#126486=CARTESIAN_POINT('Ctrl Pts',(0.544770759014798,-32.0476527861995,
125.170633026315));
#126487=CARTESIAN_POINT('Ctrl Pts',(0.547681165584014,-32.0520946672745,
125.11732898339));
#126488=CARTESIAN_POINT('Ctrl Pts',(0.550591572153229,-32.0544482948932,
125.063917320894));
#126489=CARTESIAN_POINT('Ctrl Pts',(0.553501978722444,-32.054722795758,
125.010573319835));
#126490=CARTESIAN_POINT('Ctrl Pts',(0.557370585381146,-32.0550876711967,
124.939666746204));
#126491=CARTESIAN_POINT('Ctrl Pts',(0.561239192039847,-32.0517785733045,
124.86860204487));
#126492=CARTESIAN_POINT('Ctrl Pts',(0.565107798698548,-32.0447760923756,
124.797791457774));
#126493=CARTESIAN_POINT('Ctrl Pts',(0.568970633233783,-32.037784059442,
124.727086523045));
#126494=CARTESIAN_POINT('Ctrl Pts',(0.572833467769018,-32.0271096293515,
124.656635429572));
#126495=CARTESIAN_POINT('Ctrl Pts',(0.576696302304252,-32.0127854036125,
124.586850533699));
#126496=CARTESIAN_POINT('Ctrl Pts',(0.580554596587112,-31.9984780141111,
124.517147660766));
#126497=CARTESIAN_POINT('Ctrl Pts',(0.584412890869972,-31.9805294472387,
124.448109903765));
#126498=CARTESIAN_POINT('Ctrl Pts',(0.588271185152831,-31.9590239119133,
124.380142859159));
#126499=CARTESIAN_POINT('Ctrl Pts',(0.592127043638286,-31.9375319533458,
124.312218723139));
#126500=CARTESIAN_POINT('Ctrl Pts',(0.595982902123741,-31.9124876276894,
124.245364420624));
#126501=CARTESIAN_POINT('Ctrl Pts',(0.599838760609196,-31.8840255135458,
124.179972301194));
#126502=CARTESIAN_POINT('Ctrl Pts',(0.60369347558556,-31.8555718402427,
124.114599574718));
#126503=CARTESIAN_POINT('Ctrl Pts',(0.607548190561925,-31.8237025845142,
124.050688615762));
#126504=CARTESIAN_POINT('Ctrl Pts',(0.611402905538289,-31.7886005409679,
123.988612009489));
#126505=CARTESIAN_POINT('Ctrl Pts',(0.615257767676156,-31.7534971573306,
123.926533033317));
#126506=CARTESIAN_POINT('Ctrl Pts',(0.619112629814023,-31.7151609819453,
123.866288970761));
#126507=CARTESIAN_POINT('Ctrl Pts',(0.62296749195189,-31.6738200106235,
123.808226475149));
#126508=CARTESIAN_POINT('Ctrl Pts',(0.626826387848944,-31.6324357797721,
123.750103222468));
#126509=CARTESIAN_POINT('Ctrl Pts',(0.630685283745995,-31.5880407587821,
123.694166490385));
#126510=CARTESIAN_POINT('Ctrl Pts',(0.634544179643048,-31.5409048822941,
123.640731922606));
#126511=CARTESIAN_POINT('Ctrl Pts',(0.638405258875845,-31.4937423366638,
123.58726712193));
#126512=CARTESIAN_POINT('Ctrl Pts',(0.642266338108641,-31.443836188636,
123.536307651104));
#126513=CARTESIAN_POINT('Ctrl Pts',(0.646127417341438,-31.3914931636325,
123.488132169115));
#126514=CARTESIAN_POINT('Ctrl Pts',(0.649995255646101,-31.3390585087384,
123.439872352793));
#126515=CARTESIAN_POINT('Ctrl Pts',(0.653863093950765,-31.2841788341738,
123.394406565587));
#126516=CARTESIAN_POINT('Ctrl Pts',(0.657730932255428,-31.2271932805672,
123.351972629284));
#126517=CARTESIAN_POINT('Ctrl Pts',(0.660033038023954,-31.1932759444877,
123.326716296973));
#126518=CARTESIAN_POINT('Ctrl Pts',(0.66233514379248,-31.158613154127,123.302533177827));
#126519=CARTESIAN_POINT('Ctrl Pts',(0.664637249561006,-31.1232806678074,
123.279465750463));
#126520=CARTESIAN_POINT('Ctrl Pts',(0.668506416678538,-31.0638970825189,
123.240696145407));
#126521=CARTESIAN_POINT('Ctrl Pts',(0.672375583796069,-31.0023876857733,
123.204928638054));
#126522=CARTESIAN_POINT('Ctrl Pts',(0.6762447509136,-30.9390884475194,123.17240309416));
#126523=CARTESIAN_POINT('Ctrl Pts',(0.680108153533234,-30.8758835159508,
123.13992600861));
#126524=CARTESIAN_POINT('Ctrl Pts',(0.683971556152868,-30.8108944645568,
123.110681519179));
#126525=CARTESIAN_POINT('Ctrl Pts',(0.687834958772501,-30.7444855552332,
123.084865847898));
#126526=CARTESIAN_POINT('Ctrl Pts',(0.691693829694629,-30.6781545422923,
123.059080457906));
#126527=CARTESIAN_POINT('Ctrl Pts',(0.695552700616756,-30.6104074301625,
123.036716072269));
#126528=CARTESIAN_POINT('Ctrl Pts',(0.699411571538884,-30.5416307797413,
123.017921883241));
#126529=CARTESIAN_POINT('Ctrl Pts',(0.703268011629716,-30.4728974540225,
122.999139533298));
#126530=CARTESIAN_POINT('Ctrl Pts',(0.707124451720549,-30.4031363441796,
122.983923045746));
#126531=CARTESIAN_POINT('Ctrl Pts',(0.710980891811382,-30.3327501894497,
122.972372106643));
#126532=CARTESIAN_POINT('Ctrl Pts',(0.714836192489223,-30.2623848308161,
122.960824580347));
#126533=CARTESIAN_POINT('Ctrl Pts',(0.718691493167064,-30.1913952730109,
122.952940531037));
#126534=CARTESIAN_POINT('Ctrl Pts',(0.722546793844905,-30.1201937916367,
122.948768415085));
#126535=CARTESIAN_POINT('Ctrl Pts',(0.726402244915015,-30.0489895327484,
122.944596136382));
#126536=CARTESIAN_POINT('Ctrl Pts',(0.730257695985126,-29.9775738189337,
122.944136104734));
#126537=CARTESIAN_POINT('Ctrl Pts',(0.734113147055236,-29.9063616475896,
122.947384736133));
#126538=CARTESIAN_POINT('Ctrl Pts',(0.737972632756789,-29.8350749545201,
122.950636767143));
#126539=CARTESIAN_POINT('Ctrl Pts',(0.741832118458341,-29.7639927153693,
122.95760518641));
#126540=CARTESIAN_POINT('Ctrl Pts',(0.745691604159893,-29.6935266156856,
122.968234357214));
#126541=CARTESIAN_POINT('Ctrl Pts',(0.749553274580396,-29.6230206276243,
122.978869544816));
#126542=CARTESIAN_POINT('Ctrl Pts',(0.753414945000898,-29.5531319494602,
122.993169511702));
#126543=CARTESIAN_POINT('Ctrl Pts',(0.757276615421401,-29.4842611454871,
123.011027653172));
#126544=CARTESIAN_POINT('Ctrl Pts',(0.761145040678233,-29.4152698726602,
123.028917032115));
#126545=CARTESIAN_POINT('Ctrl Pts',(0.765013465935067,-29.3473004921461,
123.050376865672));
#126546=CARTESIAN_POINT('Ctrl Pts',(0.768881891191899,-29.2807368380768,
123.07525116797));
#126547=CARTESIAN_POINT('Ctrl Pts',(0.771178767594455,-29.2412146872921,
123.090020277927));
#126548=CARTESIAN_POINT('Ctrl Pts',(0.773475643997011,-29.2021877165685,
123.105992201612));
#126549=CARTESIAN_POINT('Ctrl Pts',(0.775772520399567,-29.1637321695312,
123.123126621686));
#126550=CARTESIAN_POINT('Ctrl Pts',(0.779641657361591,-29.0989529858227,
123.151989915313));
#126551=CARTESIAN_POINT('Ctrl Pts',(0.783510794323616,-29.0355430214481,
123.184267382036));
#126552=CARTESIAN_POINT('Ctrl Pts',(0.78737993128564,-28.9738860106988,
123.219806852204));
#126553=CARTESIAN_POINT('Ctrl Pts',(0.79124330480375,-28.912320843874,123.255293382983));
#126554=CARTESIAN_POINT('Ctrl Pts',(0.795106678321859,-28.8525038649618,
123.294032031484));
#126555=CARTESIAN_POINT('Ctrl Pts',(0.798970051839968,-28.7947974852949,
123.335823188165));
#126556=CARTESIAN_POINT('Ctrl Pts',(0.802828895384963,-28.7371587688626,
123.377565342902));
#126557=CARTESIAN_POINT('Ctrl Pts',(0.806687738929957,-28.6816261274668,
123.422352612775));
#126558=CARTESIAN_POINT('Ctrl Pts',(0.810546582474951,-28.628534554461,
123.469941146821));
#126559=CARTESIAN_POINT('Ctrl Pts',(0.81440299627091,-28.5754764109521,
123.517499716398));
#126560=CARTESIAN_POINT('Ctrl Pts',(0.818259410066869,-28.5248566472431,
123.567855727257));
#126561=CARTESIAN_POINT('Ctrl Pts',(0.822115823862828,-28.4769774383036,
123.620724886376));
#126562=CARTESIAN_POINT('Ctrl Pts',(0.82597109937082,-28.4291123617499,
123.673578440238));
#126563=CARTESIAN_POINT('Ctrl Pts',(0.829826374878813,-28.3839865599273,
123.728943309816));
#126564=CARTESIAN_POINT('Ctrl Pts',(0.833681650386806,-28.3418643390767,
123.786499405655));
#126565=CARTESIAN_POINT('Ctrl Pts',(0.837537077455988,-28.299740462289,
123.844057764179));
#126566=CARTESIAN_POINT('Ctrl Pts',(0.841392504525171,-28.2606206860118,
123.903807126687));
#126567=CARTESIAN_POINT('Ctrl Pts',(0.845247931594353,-28.2247270707112,
123.96539689299));
#126568=CARTESIAN_POINT('Ctrl Pts',(0.849107395262291,-28.1887958751061,
124.027051143246));
#126569=CARTESIAN_POINT('Ctrl Pts',(0.852966858930228,-28.1560978283416,
124.090549223239));
#126570=CARTESIAN_POINT('Ctrl Pts',(0.856826322598166,-28.1268094624695,
124.155515084441));
#126571=CARTESIAN_POINT('Ctrl Pts',(0.860687972062339,-28.097504509215,
124.220517738873));
#126572=CARTESIAN_POINT('Ctrl Pts',(0.864549621526512,-28.0716132573966,
124.286989376467));
#126573=CARTESIAN_POINT('Ctrl Pts',(0.868411270990685,-28.0492633864212,
124.354535650138));
#126574=CARTESIAN_POINT('Ctrl Pts',(0.872279677238259,-28.0268744095564,
124.422200110491));
#126575=CARTESIAN_POINT('Ctrl Pts',(0.876148083485833,-28.0080393132444,
124.490942492359));
#126576=CARTESIAN_POINT('Ctrl Pts',(0.880016489733406,-27.9928352155008,
124.560355722923));
#126577=CARTESIAN_POINT('Ctrl Pts',(0.88231359023498,-27.9838068616213,
124.60157403262));
#126578=CARTESIAN_POINT('Ctrl Pts',(0.884610690736553,-27.9760578526443,
124.643028722785));
#126579=CARTESIAN_POINT('Ctrl Pts',(0.886907791238126,-27.969595668015,
124.684633845893));
#126580=CARTESIAN_POINT('Ctrl Pts',(0.892630100646193,-27.9534977132778,
124.788276410603));
#126581=CARTESIAN_POINT('Ctrl Pts',(0.898352410054259,-27.9453327368298,
124.893182202474));
#126582=CARTESIAN_POINT('Ctrl Pts',(0.904074719462325,-27.9452506257251,
124.998396436157));
#126583=CARTESIAN_POINT('Ctrl Pts',(0.904074719503818,-27.9452506257245,
124.99839643692));
#126584=CARTESIAN_POINT('Ctrl Pts',(0.907990067111021,-27.9451944432742,
125.070386654283));
#126585=CARTESIAN_POINT('Ctrl Pts',(0.911905414718225,-27.9489263631045,
125.142516745463));
#126586=CARTESIAN_POINT('Ctrl Pts',(0.915820762325428,-27.9564608111608,
125.214348189119));
#126587=CARTESIAN_POINT('Ctrl Pts',(0.919623075698889,-27.9637777432651,
125.284105892968));
#126588=CARTESIAN_POINT('Ctrl Pts',(0.923425389072348,-27.9746805797795,
125.353581419206));
#126589=CARTESIAN_POINT('Ctrl Pts',(0.927227702445809,-27.9891298100322,
125.422372633582));
#126590=CARTESIAN_POINT('Ctrl Pts',(0.931027545776556,-28.0035696538372,
125.4911191601));
#126591=CARTESIAN_POINT('Ctrl Pts',(0.934827389107304,-28.0215512222172,
125.55918176638));
#126592=CARTESIAN_POINT('Ctrl Pts',(0.93862723243805,-28.0429835185496,
125.626166155131));
#126593=CARTESIAN_POINT('Ctrl Pts',(0.942425966459145,-28.0644095580311,
125.693130988752));
#126594=CARTESIAN_POINT('Ctrl Pts',(0.946224700480239,-28.0892841740311,
125.75901775194));
#126595=CARTESIAN_POINT('Ctrl Pts',(0.950023434501334,-28.1174663973963,
125.823446900272));
#126596=CARTESIAN_POINT('Ctrl Pts',(0.953822418190325,-28.1456504730093,
125.887880283144));
#126597=CARTESIAN_POINT('Ctrl Pts',(0.957621401879316,-28.1771423830415,
125.95085540307));
#126598=CARTESIAN_POINT('Ctrl Pts',(0.961420385568307,-28.2117536492897,
126.012014106459));
#126599=CARTESIAN_POINT('Ctrl Pts',(0.965223301434588,-28.2464007402864,
126.073236112794));
#126600=CARTESIAN_POINT('Ctrl Pts',(0.969026217300869,-28.2841733783799,
126.132637516528));
#126601=CARTESIAN_POINT('Ctrl Pts',(0.972829133167149,-28.3248385009404,
126.189887185648));
#126602=CARTESIAN_POINT('Ctrl Pts',(0.976634453101162,-28.3655293305405,
126.247173045965));
#126603=CARTESIAN_POINT('Ctrl Pts',(0.980439773035174,-28.4091159674221,
126.302304075996));
#126604=CARTESIAN_POINT('Ctrl Pts',(0.984245092969186,-28.4553254313972,
126.354982671333));
#126605=CARTESIAN_POINT('Ctrl Pts',(0.988056543848615,-28.5016093458013,
126.407746139846));
#126606=CARTESIAN_POINT('Ctrl Pts',(0.991867994728043,-28.5505241611592,
126.458048940715));
#126607=CARTESIAN_POINT('Ctrl Pts',(0.995679445607472,-28.6017613924464,
126.505631548171));
#126608=CARTESIAN_POINT('Ctrl Pts',(0.996467317763876,-28.6123527365773,
126.515467438158));
#126609=CARTESIAN_POINT('Ctrl Pts',(0.99725518992028,-28.623043212392,126.525187238548));
#126610=CARTESIAN_POINT('Ctrl Pts',(0.998043062076684,-28.6338299377042,
126.534788885608));
#126611=CARTESIAN_POINT('Ctrl Pts',(1.00191215041398,-28.6868014671125,
126.581940724086));
#126612=CARTESIAN_POINT('Ctrl Pts',(1.00578123875128,-28.7423207029647,
126.626439315564));
#126613=CARTESIAN_POINT('Ctrl Pts',(1.00965032708858,-28.8000910094635,
126.667997595001));
#126614=CARTESIAN_POINT('Ctrl Pts',(1.01351365059778,-28.8577752399007,
126.709493953822));
#126615=CARTESIAN_POINT('Ctrl Pts',(1.01737697410698,-28.9177034921955,
126.748058415354));
#126616=CARTESIAN_POINT('Ctrl Pts',(1.02124029761618,-28.9795446740498,
126.783442875519));
#126617=CARTESIAN_POINT('Ctrl Pts',(1.02509908933243,-29.0413133143655,
126.818785828664));
#126618=CARTESIAN_POINT('Ctrl Pts',(1.02895788104868,-29.1049900074564,
126.850955949871));
#126619=CARTESIAN_POINT('Ctrl Pts',(1.03281667276493,-29.1702146287174,
126.879748334247));
#126620=CARTESIAN_POINT('Ctrl Pts',(1.03667303363584,-29.2353981617367,
126.908522580864));
#126621=CARTESIAN_POINT('Ctrl Pts',(1.04052939450675,-29.3021272449515,
126.933923116469));
#126622=CARTESIAN_POINT('Ctrl Pts',(1.04438575537766,-29.3700184070463,
126.955791592946));
#126623=CARTESIAN_POINT('Ctrl Pts',(1.04824097694197,-29.4378895116695,
126.977653608695));
#126624=CARTESIAN_POINT('Ctrl Pts',(1.05209619850629,-29.506921551454,126.995985488087));
#126625=CARTESIAN_POINT('Ctrl Pts',(1.0559514200706,-29.5767140212836,127.010678130065));
#126626=CARTESIAN_POINT('Ctrl Pts',(1.05980679225408,-29.6465092178263,
127.025371346068));
#126627=CARTESIAN_POINT('Ctrl Pts',(1.06366216443755,-29.7170644275819,
127.03642494446));
#126628=CARTESIAN_POINT('Ctrl Pts',(1.06751753662103,-29.7879687307261,
127.043780884378));
#126629=CARTESIAN_POINT('Ctrl Pts',(1.07137694433534,-29.8589472514783,
127.051144523975));
#126630=CARTESIAN_POINT('Ctrl Pts',(1.07523635204964,-29.9302751108738,
127.054802728585));
#126631=CARTESIAN_POINT('Ctrl Pts',(1.07909575976395,-30.0015369395232,
127.05474942519));
#126632=CARTESIAN_POINT('Ctrl Pts',(1.08295735258731,-30.0728391150027,
127.054696091615));
#126633=CARTESIAN_POINT('Ctrl Pts',(1.08681894541067,-30.1440746999807,
127.050927092529));
#126634=CARTESIAN_POINT('Ctrl Pts',(1.09068053823403,-30.2148317599149,
127.04348840893));
#126635=CARTESIAN_POINT('Ctrl Pts',(1.09454888736175,-30.2857126175292,
127.036036710492));
#126636=CARTESIAN_POINT('Ctrl Pts',(1.09841723648948,-30.3561127985652,
127.024902584658));
#126637=CARTESIAN_POINT('Ctrl Pts',(1.1022855856172,-30.4256295856275,127.010183329535));
#126638=CARTESIAN_POINT('Ctrl Pts',(1.10458316804988,-30.4669186584224,
127.001440917494));
#126639=CARTESIAN_POINT('Ctrl Pts',(1.10688075048256,-30.5078963491774,
126.991434748811));
#126640=CARTESIAN_POINT('Ctrl Pts',(1.10917833291525,-30.5484811992541,
126.980193408878));
#126641=CARTESIAN_POINT('Ctrl Pts',(1.11304631609095,-30.6168058500052,
126.961268597688));
#126642=CARTESIAN_POINT('Ctrl Pts',(1.11691429926665,-30.6842836647767,
126.938766367269));
#126643=CARTESIAN_POINT('Ctrl Pts',(1.12078228244236,-30.7505129247959,
126.912780152609));
#126644=CARTESIAN_POINT('Ctrl Pts',(1.12464523167393,-30.8166559914737,
126.886827757421));
#126645=CARTESIAN_POINT('Ctrl Pts',(1.12850818090551,-30.8815532773588,
126.857400544484));
#126646=CARTESIAN_POINT('Ctrl Pts',(1.13237113013709,-30.9448168729143,
126.824642057817));
#126647=CARTESIAN_POINT('Ctrl Pts',(1.13622985099915,-31.0080112203791,
126.791919428466));
#126648=CARTESIAN_POINT('Ctrl Pts',(1.1400885718612,-31.069574998631,126.755872986999));
#126649=CARTESIAN_POINT('Ctrl Pts',(1.14394729272326,-31.1291407496662,
126.716694128243));
#126650=CARTESIAN_POINT('Ctrl Pts',(1.146668096559,-31.1711408656863,126.689068914345));
#126651=CARTESIAN_POINT('Ctrl Pts',(1.14938890039474,-31.212148009238,126.659887366754));
#126652=CARTESIAN_POINT('Ctrl Pts',(1.15210970423049,-31.2520409112987,
126.629230222815));
#126653=CARTESIAN_POINT('',(0.845925280586436,-27.945250330481,125.00116538046));
#126654=CARTESIAN_POINT('Ctrl Pts',(0.845925280586436,-27.945250330481,
125.00116538046));
#126655=CARTESIAN_POINT('Ctrl Pts',(0.85022219368581,-27.9452954735043,
125.080759654999));
#126656=CARTESIAN_POINT('Ctrl Pts',(0.854519106785184,-27.9499695693127,
125.160186918996));
#126657=CARTESIAN_POINT('Ctrl Pts',(0.858816019884558,-27.9591900445396,
125.23893992591));
#126658=CARTESIAN_POINT('Ctrl Pts',(0.86313050384008,-27.9684482239602,
125.318014968137));
#126659=CARTESIAN_POINT('Ctrl Pts',(0.867444987795601,-27.9822899038121,
125.396409967232));
#126660=CARTESIAN_POINT('Ctrl Pts',(0.871759471751123,-28.0005817423557,
125.473628750709));
#126661=CARTESIAN_POINT('Ctrl Pts',(0.876096088705256,-28.0189674167418,
125.551243661104));
#126662=CARTESIAN_POINT('Ctrl Pts',(0.88043270565939,-28.0418488879396,
125.62767000483));
#126663=CARTESIAN_POINT('Ctrl Pts',(0.884769322613523,-28.0690426460444,
125.702425269836));
#126664=CARTESIAN_POINT('Ctrl Pts',(0.88620693731184,-28.0780575410115,
125.727207091447));
#126665=CARTESIAN_POINT('Ctrl Pts',(0.887644552010157,-28.0875459587084,
125.751805457319));
#126666=CARTESIAN_POINT('Ctrl Pts',(0.889082166708475,-28.0975000961443,
125.776203374335));
#126667=CARTESIAN_POINT('Ctrl Pts',(0.892951333584334,-28.1242904586036,
125.841867430545));
#126668=CARTESIAN_POINT('Ctrl Pts',(0.896820500460194,-28.15453682424,125.906271445725));
#126669=CARTESIAN_POINT('Ctrl Pts',(0.900689667336053,-28.1880992959586,
125.969027038423));
#126670=CARTESIAN_POINT('Ctrl Pts',(0.904553069711517,-28.2216117644367,
126.031689134342));
#126671=CARTESIAN_POINT('Ctrl Pts',(0.90841647208698,-28.2584303049682,
126.092707257843));
#126672=CARTESIAN_POINT('Ctrl Pts',(0.912279874462444,-28.2983669267469,
126.151712831617));
#126673=CARTESIAN_POINT('Ctrl Pts',(0.916138745137886,-28.3382567036019,
126.210649192937));
#126674=CARTESIAN_POINT('Ctrl Pts',(0.919997615813329,-28.3812570258022,
126.267577293327));
#126675=CARTESIAN_POINT('Ctrl Pts',(0.923856486488771,-28.4271348119871,
126.32215455331));
#126676=CARTESIAN_POINT('Ctrl Pts',(0.927712926331499,-28.4729836982081,
126.376697433237));
#126677=CARTESIAN_POINT('Ctrl Pts',(0.931569366174226,-28.521706140386,
126.428892039833));
#126678=CARTESIAN_POINT('Ctrl Pts',(0.935425806016954,-28.5730275921944,
126.478427309631));
#126679=CARTESIAN_POINT('Ctrl Pts',(0.939281106445644,-28.6243338806954,
126.527947943862));
#126680=CARTESIAN_POINT('Ctrl Pts',(0.943136406874334,-28.6782373050151,
126.574810464008));
#126681=CARTESIAN_POINT('Ctrl Pts',(0.946991707303024,-28.7344263364808,
126.618740518028));
#126682=CARTESIAN_POINT('Ctrl Pts',(0.950847158123302,-28.7906175598271,
126.662672285718));
#126683=CARTESIAN_POINT('Ctrl Pts',(0.954702608943581,-28.8490941832946,
126.703671062714));
#126684=CARTESIAN_POINT('Ctrl Pts',(0.958558059763859,-28.9095128396272,
126.741503751234));
#126685=CARTESIAN_POINT('Ctrl Pts',(0.962417545216279,-28.9699947225614,
126.77937603071));
#126686=CARTESIAN_POINT('Ctrl Pts',(0.966277030668698,-29.0324222827182,
126.814075349425));
#126687=CARTESIAN_POINT('Ctrl Pts',(0.970136516121118,-29.0964252698175,
126.845413305868));
#126688=CARTESIAN_POINT('Ctrl Pts',(0.973998186292504,-29.1604644867567,
126.876769001626));
#126689=CARTESIAN_POINT('Ctrl Pts',(0.977859856463891,-29.2260804589129,
126.904759356628));
#126690=CARTESIAN_POINT('Ctrl Pts',(0.981721526635277,-29.292883093083,
126.929244215348));
#126691=CARTESIAN_POINT('Ctrl Pts',(0.985589951645727,-29.3598025785177,
126.953771903018));
#126692=CARTESIAN_POINT('Ctrl Pts',(0.989458376656176,-29.4279124058617,
126.974781708812));
#126693=CARTESIAN_POINT('Ctrl Pts',(0.993326801666625,-29.4968081547775,
126.992183608356));
#126694=CARTESIAN_POINT('Ctrl Pts',(0.99562368029343,-29.5377150284366,
127.002515991954));
#126695=CARTESIAN_POINT('Ctrl Pts',(0.997920558920233,-29.5788987710876,
127.0115774254));
#126696=CARTESIAN_POINT('Ctrl Pts',(1.00021743754704,-29.6202737412824,
127.019357702573));
#126697=CARTESIAN_POINT('Ctrl Pts',(1.00411924001165,-29.6905591097799,
127.032574380325));
#126698=CARTESIAN_POINT('Ctrl Pts',(1.00802104247626,-29.7616741112237,
127.042143266183));
#126699=CARTESIAN_POINT('Ctrl Pts',(1.01192284494087,-29.8332062447118,
127.047969092955));
#126700=CARTESIAN_POINT('Ctrl Pts',(1.01578547045942,-29.9040201433429,
127.053736424171));
#126701=CARTESIAN_POINT('Ctrl Pts',(1.01964809597797,-29.9752423456309,
127.055835443642));
#126702=CARTESIAN_POINT('Ctrl Pts',(1.02351072149651,-30.0464614134387,
127.05422464681));
#126703=CARTESIAN_POINT('Ctrl Pts',(1.02736946478645,-30.117608900737,127.052615468949));
#126704=CARTESIAN_POINT('Ctrl Pts',(1.03122820807639,-30.1887527767806,
127.047303883675));
#126705=CARTESIAN_POINT('Ctrl Pts',(1.03508695136633,-30.2594788442955,
127.03830034388));
#126706=CARTESIAN_POINT('Ctrl Pts',(1.03894310717835,-30.3301574864897,
127.029302841403));
#126707=CARTESIAN_POINT('Ctrl Pts',(1.04279926299038,-30.4004183956563,
127.016618359994));
#126708=CARTESIAN_POINT('Ctrl Pts',(1.0466554188024,-30.4698514739257,127.000309264826));
#126709=CARTESIAN_POINT('Ctrl Pts',(1.05058919196034,-30.5406821127495,
126.983671897477));
#126710=CARTESIAN_POINT('Ctrl Pts',(1.05452296511828,-30.6106507113064,
126.963262454806));
#126711=CARTESIAN_POINT('Ctrl Pts',(1.05845673827622,-30.6793332005368,
126.939201888703));
#126712=CARTESIAN_POINT('Ctrl Pts',(1.06231299626292,-30.7466622983283,
126.915615437102));
#126713=CARTESIAN_POINT('Ctrl Pts',(1.06616925424962,-30.8127550614049,
126.888520672006));
#126714=CARTESIAN_POINT('Ctrl Pts',(1.07002551223631,-30.8772297845218,
126.858081125152));
#126715=CARTESIAN_POINT('Ctrl Pts',(1.07399804297988,-30.9436485305311,
126.826723774033));
#126716=CARTESIAN_POINT('Ctrl Pts',(1.07797057372345,-31.0083495876843,
126.791816908259));
#126717=CARTESIAN_POINT('Ctrl Pts',(1.08194310446701,-31.0709426864352,
126.753590409666));
#126718=CARTESIAN_POINT('Ctrl Pts',(1.08591563521058,-31.1335357851862,
126.715363911072));
#126719=CARTESIAN_POINT('Ctrl Pts',(1.08988816595415,-31.1940204803808,
126.67381812217));
#126720=CARTESIAN_POINT('Ctrl Pts',(1.09386069669771,-31.2520409112987,
126.629230222815));
#126721=CARTESIAN_POINT('Ctrl Pts',(0.393902764517251,-31.2520409112987,
126.629230222815));
#126722=CARTESIAN_POINT('Ctrl Pts',(0.397765020730025,-31.3086816915374,
126.585702565942));
#126723=CARTESIAN_POINT('Ctrl Pts',(0.401627276942799,-31.3630392040398,
126.539226023053));
#126724=CARTESIAN_POINT('Ctrl Pts',(0.405489533155574,-31.4148028017945,
126.490077378707));
#126725=CARTESIAN_POINT('Ctrl Pts',(0.409356059028123,-31.4666236233425,
126.440874401355));
#126726=CARTESIAN_POINT('Ctrl Pts',(0.413222584900672,-31.5158444569778,
126.388993762238));
#126727=CARTESIAN_POINT('Ctrl Pts',(0.417089110773222,-31.5621914994499,
126.33474914555));
#126728=CARTESIAN_POINT('Ctrl Pts',(0.42095811694271,-31.6085682725979,
126.280469732055));
#126729=CARTESIAN_POINT('Ctrl Pts',(0.424827123112198,-31.6520672913701,
126.223823706893));
#126730=CARTESIAN_POINT('Ctrl Pts',(0.428696129281686,-31.6924567108541,
126.165155716797));
#126731=CARTESIAN_POINT('Ctrl Pts',(0.432571643378787,-31.7329140680478,
126.106389043211));
#126732=CARTESIAN_POINT('Ctrl Pts',(0.436447157475887,-31.7702511359751,
126.045594029938));
#126733=CARTESIAN_POINT('Ctrl Pts',(0.440322671572987,-31.8042812499767,
125.983141258153));
#126734=CARTESIAN_POINT('Ctrl Pts',(0.441728808833403,-31.8166282599669,
125.960481769057));
#126735=CARTESIAN_POINT('Ctrl Pts',(0.443134946093818,-31.828540390247,
125.937604245957));
#126736=CARTESIAN_POINT('Ctrl Pts',(0.444541083354234,-31.8400103070147,
125.914526999372));
#126737=CARTESIAN_POINT('Ctrl Pts',(0.44840642658579,-31.8715400633143,
125.851089750817));
#126738=CARTESIAN_POINT('Ctrl Pts',(0.452271769817345,-31.8998482225227,
125.785893454723));
#126739=CARTESIAN_POINT('Ctrl Pts',(0.456137113048901,-31.9247355213386,
125.719298780339));
#126740=CARTESIAN_POINT('Ctrl Pts',(0.459996637425455,-31.9495853550253,
125.652804357015));
#126741=CARTESIAN_POINT('Ctrl Pts',(0.463856161802009,-31.9710243806548,
125.584916185923));
#126742=CARTESIAN_POINT('Ctrl Pts',(0.467715686178562,-31.988899935638,
125.516018031196));
#126743=CARTESIAN_POINT('Ctrl Pts',(0.471570616814023,-32.0067542145096,
125.447201881465));
#126744=CARTESIAN_POINT('Ctrl Pts',(0.475425547449484,-32.0210533254499,
125.377378604707));
#126745=CARTESIAN_POINT('Ctrl Pts',(0.479280478084945,-32.0316938889068,
125.306948699751));
#126746=CARTESIAN_POINT('Ctrl Pts',(0.483132941660506,-32.0423276426672,
125.236563868186));
#126747=CARTESIAN_POINT('Ctrl Pts',(0.486985405236067,-32.0493074212925,
125.165573658832));
#126748=CARTESIAN_POINT('Ctrl Pts',(0.490837868811627,-32.0525808856403,
125.094388931576));
#126749=CARTESIAN_POINT('Ctrl Pts',(0.494689162603668,-32.0558533560152,
125.023225819248));
#126750=CARTESIAN_POINT('Ctrl Pts',(0.498540456395708,-32.0554217238142,
124.951868792349));
#126751=CARTESIAN_POINT('Ctrl Pts',(0.502391750187749,-32.0512856380332,
124.880732260444));
#126752=CARTESIAN_POINT('Ctrl Pts',(0.506243169824716,-32.0471494171013,
124.80959340408));
#126753=CARTESIAN_POINT('Ctrl Pts',(0.510094589461684,-32.0393085327444,
124.73867554294));
#126754=CARTESIAN_POINT('Ctrl Pts',(0.513946009098651,-32.0278146390282,
124.668389758537));
#126755=CARTESIAN_POINT('Ctrl Pts',(0.517801453495946,-32.0163087341131,
124.598030525001));
#126756=CARTESIAN_POINT('Ctrl Pts',(0.52165689789324,-32.0011422781157,
124.528305168249));
#126757=CARTESIAN_POINT('Ctrl Pts',(0.525512342290535,-31.9824182414273,
124.459615434569));
#126758=CARTESIAN_POINT('Ctrl Pts',(0.529369959655217,-31.9636836516829,
124.390886986662));
#126759=CARTESIAN_POINT('Ctrl Pts',(0.5332275770199,-31.9413876423888,124.323195786347));
#126760=CARTESIAN_POINT('Ctrl Pts',(0.537085194384582,-31.9156825106371,
124.256926597879));
#126761=CARTESIAN_POINT('Ctrl Pts',(0.540949591980453,-31.8899321989934,
124.190540933262));
#126762=CARTESIAN_POINT('Ctrl Pts',(0.544813989576324,-31.8607610014774,
124.125582714751));
#126763=CARTESIAN_POINT('Ctrl Pts',(0.548678387172195,-31.8283683107149,
124.062414333048));
#126764=CARTESIAN_POINT('Ctrl Pts',(0.551011042845729,-31.8088152000389,
124.024284176844));
#126765=CARTESIAN_POINT('Ctrl Pts',(0.553343698519263,-31.7880891683627,
123.986805673443));
#126766=CARTESIAN_POINT('Ctrl Pts',(0.555676354192797,-31.7662416108555,
123.950053270598));
#126767=CARTESIAN_POINT('Ctrl Pts',(0.559545932806801,-31.7299992960307,
123.889085716031));
#126768=CARTESIAN_POINT('Ctrl Pts',(0.563415511420805,-31.6905256384392,
123.829877628157));
#126769=CARTESIAN_POINT('Ctrl Pts',(0.56728509003481,-31.6480166895168,
123.772792375523));
#126770=CARTESIAN_POINT('Ctrl Pts',(0.571148902574401,-31.6055710833475,
123.71579218585));
#126771=CARTESIAN_POINT('Ctrl Pts',(0.575012715113993,-31.5600994514413,
123.660908938752));
#126772=CARTESIAN_POINT('Ctrl Pts',(0.578876527653584,-31.5118424650373,
123.608479276687));
#126773=CARTESIAN_POINT('Ctrl Pts',(0.582735804066608,-31.4636421324683,
123.556111167189));
#126774=CARTESIAN_POINT('Ctrl Pts',(0.586595080479631,-31.4126632681155,
123.506191276576));
#126775=CARTESIAN_POINT('Ctrl Pts',(0.590454356892654,-31.3591872739167,
123.459023842844));
#126776=CARTESIAN_POINT('Ctrl Pts',(0.594311199502693,-31.3057450036651,
123.411886154647));
#126777=CARTESIAN_POINT('Ctrl Pts',(0.598168042112731,-31.2498090912909,
123.367497799978));
#126778=CARTESIAN_POINT('Ctrl Pts',(0.602024884722769,-31.1916972663116,
123.326125695291));
#126779=CARTESIAN_POINT('Ctrl Pts',(0.605880584327041,-31.1336026632306,
123.284765851553));
#126780=CARTESIAN_POINT('Ctrl Pts',(0.609736283931313,-31.0733338231633,
123.246420764666));
#126781=CARTESIAN_POINT('Ctrl Pts',(0.613591983535585,-31.0112396003772,
123.211315557979));
#126782=CARTESIAN_POINT('Ctrl Pts',(0.617447829314859,-30.9491430235117,
123.176209020403));
#126783=CARTESIAN_POINT('Ctrl Pts',(0.621303675094133,-30.8852213503721,
123.144342843979));
#126784=CARTESIAN_POINT('Ctrl Pts',(0.625159520873407,-30.8198488004311,
123.115896630508));
#126785=CARTESIAN_POINT('Ctrl Pts',(0.629019392036878,-30.7544080035621,
123.087420720066));
#126786=CARTESIAN_POINT('Ctrl Pts',(0.63287926320035,-30.6875137524757,
123.062372093968));
#126787=CARTESIAN_POINT('Ctrl Pts',(0.636739134363821,-30.6195602206645,
123.040882163965));
#126788=CARTESIAN_POINT('Ctrl Pts',(0.640601185605821,-30.5515683082884,
123.01938009632));
#126789=CARTESIAN_POINT('Ctrl Pts',(0.644463236847821,-30.4825163944218,
123.001440848258));
#126790=CARTESIAN_POINT('Ctrl Pts',(0.648325288089821,-30.4128111208673,
122.987145176376));
#126791=CARTESIAN_POINT('Ctrl Pts',(0.652194082616269,-30.3429841393247,
122.97282454372));
#126792=CARTESIAN_POINT('Ctrl Pts',(0.656062877142717,-30.2725020007958,
122.962160261539));
#126793=CARTESIAN_POINT('Ctrl Pts',(0.659931671669165,-30.2017780807413,
122.955181384907));
#126794=CARTESIAN_POINT('Ctrl Pts',(0.662224989456562,-30.1598548349481,
122.951044493736));
#126795=CARTESIAN_POINT('Ctrl Pts',(0.664518307243959,-30.1178466836125,
122.948201584349));
#126796=CARTESIAN_POINT('Ctrl Pts',(0.666811625031356,-30.0758394270535,
122.946650067864));
#126797=CARTESIAN_POINT('Ctrl Pts',(0.670681339064105,-30.0049569392113,
122.944032059515));
#126798=CARTESIAN_POINT('Ctrl Pts',(0.674551053096854,-29.9338004265351,
122.945083589534));
#126799=CARTESIAN_POINT('Ctrl Pts',(0.678420767129603,-29.8627815495254,
122.949836918841));
#126800=CARTESIAN_POINT('Ctrl Pts',(0.682284730142912,-29.791868218026,
122.954583183933));
#126801=CARTESIAN_POINT('Ctrl Pts',(0.686148693156222,-29.7210925967539,
122.963020295739));
#126802=CARTESIAN_POINT('Ctrl Pts',(0.690012656169532,-29.6508680762893,
122.975128531895));
#126803=CARTESIAN_POINT('Ctrl Pts',(0.693872104829046,-29.5807256006914,
122.98722262173));
#126804=CARTESIAN_POINT('Ctrl Pts',(0.697731553488561,-29.5111334231914,
123.002979234233));
#126805=CARTESIAN_POINT('Ctrl Pts',(0.701591002148075,-29.4424997873939,
123.022326853233));
#126806=CARTESIAN_POINT('Ctrl Pts',(0.705448030375005,-29.3739091948138,
123.041662338476));
#126807=CARTESIAN_POINT('Ctrl Pts',(0.709305058601936,-29.3062764175459,
123.06458423062));
#126808=CARTESIAN_POINT('Ctrl Pts',(0.713162086828866,-29.2399980313748,
123.090970254243));
#126809=CARTESIAN_POINT('Ctrl Pts',(0.717017985171078,-29.1737390609121,
123.117348548296));
#126810=CARTESIAN_POINT('Ctrl Pts',(0.720873883513291,-29.1088341447766,
123.147188779646));
#126811=CARTESIAN_POINT('Ctrl Pts',(0.724729781855503,-29.0456616135279,
123.180319861458));
#126812=CARTESIAN_POINT('Ctrl Pts',(0.728585839258048,-28.982486476338,
123.213452309965));
#126813=CARTESIAN_POINT('Ctrl Pts',(0.732441896660594,-28.9210442949365,
123.249875650967));
#126814=CARTESIAN_POINT('Ctrl Pts',(0.736297954063139,-28.8616888998584,
123.289372804555));
#126815=CARTESIAN_POINT('Ctrl Pts',(0.740158055211578,-28.8022712603399,
123.328911377769));
#126816=CARTESIAN_POINT('Ctrl Pts',(0.744018156360015,-28.7449451806828,
123.371529928666));
#126817=CARTESIAN_POINT('Ctrl Pts',(0.747878257508454,-28.6900348175087,
123.416968483207));
#126818=CARTESIAN_POINT('Ctrl Pts',(0.751740549446914,-28.6350932901056,
123.462432826277));
#126819=CARTESIAN_POINT('Ctrl Pts',(0.755602841385376,-28.5825705661525,
123.510720030277));
#126820=CARTESIAN_POINT('Ctrl Pts',(0.759465133323836,-28.5327549971333,
123.561532181777));
#126821=CARTESIAN_POINT('Ctrl Pts',(0.763334183008087,-28.4828522671855,
123.612433237899));
#126822=CARTESIAN_POINT('Ctrl Pts',(0.767203232692338,-28.4356664705326,
123.665867697753));
#126823=CARTESIAN_POINT('Ctrl Pts',(0.771072282376589,-28.3914461665989,
123.721503958727));
#126824=CARTESIAN_POINT('Ctrl Pts',(0.773363820207697,-28.3652556268962,
123.75445587385));
#126825=CARTESIAN_POINT('Ctrl Pts',(0.775655358038806,-28.3401045395053,
123.788179572696));
#126826=CARTESIAN_POINT('Ctrl Pts',(0.777946895869915,-28.3160371429284,
123.822601741761));
#126827=CARTESIAN_POINT('Ctrl Pts',(0.781859926298845,-28.2749396520329,
123.881381044094));
#126828=CARTESIAN_POINT('Ctrl Pts',(0.785772956727774,-28.236845311038,
123.942426078789));
#126829=CARTESIAN_POINT('Ctrl Pts',(0.789685987156704,-28.2020089815868,
124.005401658856));
#126830=CARTESIAN_POINT('Ctrl Pts',(0.793592843665999,-28.1672276163641,
124.068277877016));
#126831=CARTESIAN_POINT('Ctrl Pts',(0.797499700175295,-28.135694282503,
124.133078184039));
#126832=CARTESIAN_POINT('Ctrl Pts',(0.80140655668459,-28.1076211970859,
124.199437679639));
#126833=CARTESIAN_POINT('Ctrl Pts',(0.805307700426477,-28.0795891612971,
124.265700141636));
#126834=CARTESIAN_POINT('Ctrl Pts',(0.809208844168363,-28.0550074979398,
124.333516828244));
#126835=CARTESIAN_POINT('Ctrl Pts',(0.813109987910249,-28.0340421790454,
124.402499030354));
#126836=CARTESIAN_POINT('Ctrl Pts',(0.81700774558199,-28.0130950573889,
124.471421358081));
#126837=CARTESIAN_POINT('Ctrl Pts',(0.820905503253732,-27.9957581837704,
124.541506743162));
#126838=CARTESIAN_POINT('Ctrl Pts',(0.824803260925473,-27.9821487118791,
124.612348427671));
#126839=CARTESIAN_POINT('Ctrl Pts',(0.82869925686719,-27.9685453912721,
124.683158092765));
#126840=CARTESIAN_POINT('Ctrl Pts',(0.832595252808908,-27.9586662201479,
124.75472291711));
#126841=CARTESIAN_POINT('Ctrl Pts',(0.836491248750625,-27.9525776100896,
124.826624339097));
#126842=CARTESIAN_POINT('Ctrl Pts',(0.839635926012976,-27.9476631507585,
124.884660017326));
#126843=CARTESIAN_POINT('Ctrl Pts',(0.842780603275327,-27.9452172927798,
124.942914654077));
#126844=CARTESIAN_POINT('Ctrl Pts',(0.845925280537678,-27.9452503304805,
125.001165379557));
#126845=CARTESIAN_POINT('Origin',(-1.54592528053767,30.,125.));
#126846=CARTESIAN_POINT('',(0.904074719503814,32.0547493742749,124.998396436228));
#126847=CARTESIAN_POINT('Ctrl Pts',(0.452117107018789,28.7479590808042,
126.629230216746));
#126848=CARTESIAN_POINT('Ctrl Pts',(0.455981895232545,28.6916216498318,
126.585935679157));
#126849=CARTESIAN_POINT('Ctrl Pts',(0.4598466834463,28.6374422924799,126.539646245016));
#126850=CARTESIAN_POINT('Ctrl Pts',(0.463711471660055,28.5857546915823,
126.490606510827));
#126851=CARTESIAN_POINT('Ctrl Pts',(0.46757142881513,28.5341317011676,126.441628077236));
#126852=CARTESIAN_POINT('Ctrl Pts',(0.471431385970206,28.4849946303537,
126.389906505276));
#126853=CARTESIAN_POINT('Ctrl Pts',(0.475291343125281,28.4386442929298,
126.335726737959));
#126854=CARTESIAN_POINT('Ctrl Pts',(0.479148672821944,28.3923255060073,
126.281583850608));
#126855=CARTESIAN_POINT('Ctrl Pts',(0.483006002518608,28.3487900040007,
126.224986455488));
#126856=CARTESIAN_POINT('Ctrl Pts',(0.486863332215272,28.3083008876935,
126.166255407671));
#126857=CARTESIAN_POINT('Ctrl Pts',(0.490719325378409,28.2678258005376,
126.107544709687));
#126858=CARTESIAN_POINT('Ctrl Pts',(0.494575318541546,28.2303952792588,
126.046702225986));
#126859=CARTESIAN_POINT('Ctrl Pts',(0.498431311704683,28.1962302949751,
125.984079475314));
#126860=CARTESIAN_POINT('Ctrl Pts',(0.502287257448356,28.1620657308387,
125.921457494752));
#126861=CARTESIAN_POINT('Ctrl Pts',(0.506143203192031,28.1311668548754,
125.857055717875));
#126862=CARTESIAN_POINT('Ctrl Pts',(0.509999148935705,28.1037088404285,
125.791250529625));
#126863=CARTESIAN_POINT('Ctrl Pts',(0.513859007405818,28.0762229636345,
125.725378567172));
#126864=CARTESIAN_POINT('Ctrl Pts',(0.51771886587593,28.0521851081078,125.658100798736));
#126865=CARTESIAN_POINT('Ctrl Pts',(0.521578724346043,28.0317220436767,
125.589813062887));
#126866=CARTESIAN_POINT('Ctrl Pts',(0.525440588113093,28.011248348151,125.521489849782));
#126867=CARTESIAN_POINT('Ctrl Pts',(0.529302451880144,27.9943532573307,
125.452156096639));
#126868=CARTESIAN_POINT('Ctrl Pts',(0.533164315647195,27.9811127406638,
125.382219565944));
#126869=CARTESIAN_POINT('Ctrl Pts',(0.537033131028333,27.9678483901779,
125.312157144797));
#126870=CARTESIAN_POINT('Ctrl Pts',(0.540901946409472,27.9582518188302,
125.241490260834));
#126871=CARTESIAN_POINT('Ctrl Pts',(0.544770761790611,27.9523472098042,
125.170632978358));
#126872=CARTESIAN_POINT('Ctrl Pts',(0.547681167434558,27.9479053314146,
125.117328952573));
#126873=CARTESIAN_POINT('Ctrl Pts',(0.550591573078505,27.9455517051314,
125.063917307332));
#126874=CARTESIAN_POINT('Ctrl Pts',(0.553501978722452,27.9452772042607,
125.010573323468));
#126875=CARTESIAN_POINT('Ctrl Pts',(0.557370585230107,27.9449123287125,
124.93966675292));
#126876=CARTESIAN_POINT('Ctrl Pts',(0.561239191737762,27.9482214261752,
124.868602054561));
#126877=CARTESIAN_POINT('Ctrl Pts',(0.565107798245418,27.9552239063853,
124.797791470304));
#126878=CARTESIAN_POINT('Ctrl Pts',(0.568970632627215,27.9622159385964,
124.727086538457));
#126879=CARTESIAN_POINT('Ctrl Pts',(0.572833467009012,27.9728903676711,
124.656635447727));
#126880=CARTESIAN_POINT('Ctrl Pts',(0.57669630139081,27.9872145921315,124.586850554434));
#126881=CARTESIAN_POINT('Ctrl Pts',(0.580554595517413,28.0015219803447,
124.51714768413));
#126882=CARTESIAN_POINT('Ctrl Pts',(0.584412889644017,28.0194705456612,
124.448109929595));
#126883=CARTESIAN_POINT('Ctrl Pts',(0.588271183770621,28.0409760791931,
124.380142887266));
#126884=CARTESIAN_POINT('Ctrl Pts',(0.592127042098162,28.0624680359586,
124.312218753553));
#126885=CARTESIAN_POINT('Ctrl Pts',(0.595982900425703,28.0875123595725,
124.245364453157));
#126886=CARTESIAN_POINT('Ctrl Pts',(0.599838758753245,28.1159744714627,
124.179972335637));
#126887=CARTESIAN_POINT('Ctrl Pts',(0.603693473570268,28.1444281425023,
124.114599611096));
#126888=CARTESIAN_POINT('Ctrl Pts',(0.607548188387292,28.1762973957539,
124.050688653865));
#126889=CARTESIAN_POINT('Ctrl Pts',(0.611402903204315,28.2113994366381,
123.988612049092));
#126890=CARTESIAN_POINT('Ctrl Pts',(0.615257765181646,28.2465028176025,
123.926533074439));
#126891=CARTESIAN_POINT('Ctrl Pts',(0.619112627158977,28.2848389901278,
123.866289013174));
#126892=CARTESIAN_POINT('Ctrl Pts',(0.622967489136308,28.3261799584297,
123.808226518613));
#126893=CARTESIAN_POINT('Ctrl Pts',(0.626826384872089,28.3675641862521,
123.750103266992));
#126894=CARTESIAN_POINT('Ctrl Pts',(0.63068528060787,28.411959204052,123.694166535726));
#126895=CARTESIAN_POINT('Ctrl Pts',(0.634544176343651,28.459095077215,123.640731968508));
#126896=CARTESIAN_POINT('Ctrl Pts',(0.638405255414516,28.5062576195114,
123.587267168401));
#126897=CARTESIAN_POINT('Ctrl Pts',(0.64226633448538,28.5561637640696,123.536307697886));
#126898=CARTESIAN_POINT('Ctrl Pts',(0.646127413556245,28.6085067854929,
123.488132215939));
#126899=CARTESIAN_POINT('Ctrl Pts',(0.649995251699682,28.660941436814,123.439872399646));
#126900=CARTESIAN_POINT('Ctrl Pts',(0.653863089843119,28.7158211076959,
123.394406612201));
#126901=CARTESIAN_POINT('Ctrl Pts',(0.657730927986555,28.7728066575346,
123.351972675376));
#126902=CARTESIAN_POINT('Ctrl Pts',(0.660033035178038,28.8067240137499,
123.326716326091));
#126903=CARTESIAN_POINT('Ctrl Pts',(0.662335142369521,28.8413868252004,
123.302533191287));
#126904=CARTESIAN_POINT('Ctrl Pts',(0.664637249561004,28.8767193334179,
123.279465749663));
#126905=CARTESIAN_POINT('Ctrl Pts',(0.668506416735362,28.9361029196769,
123.240696144034));
#126906=CARTESIAN_POINT('Ctrl Pts',(0.672375583909721,28.9976123174276,
123.204928636224));
#126907=CARTESIAN_POINT('Ctrl Pts',(0.676244751084079,29.0609115567066,
123.172403091989));
#126908=CARTESIAN_POINT('Ctrl Pts',(0.680108153761125,29.1241164893097,
123.139926006092));
#126909=CARTESIAN_POINT('Ctrl Pts',(0.683971556438171,29.1891055417586,
123.110681516429));
#126910=CARTESIAN_POINT('Ctrl Pts',(0.687834959115217,29.255514452144,123.08486584503));
#126911=CARTESIAN_POINT('Ctrl Pts',(0.691693830095352,29.3218454661568,
123.059080454915));
#126912=CARTESIAN_POINT('Ctrl Pts',(0.695552701075488,29.3895925793658,
123.03671606927));
#126913=CARTESIAN_POINT('Ctrl Pts',(0.699411572055622,29.4583692308609,
123.017921880343));
#126914=CARTESIAN_POINT('Ctrl Pts',(0.703268012204796,29.5271025576596,
122.9991395305));
#126915=CARTESIAN_POINT('Ctrl Pts',(0.707124452353968,29.5968636685773,
122.98392304316));
#126916=CARTESIAN_POINT('Ctrl Pts',(0.710980892503141,29.6672498243653,
122.972372104375));
#126917=CARTESIAN_POINT('Ctrl Pts',(0.714836193239567,29.7376151840615,
122.960824578398));
#126918=CARTESIAN_POINT('Ctrl Pts',(0.718691493975995,29.8086047429128,
122.952940529514));
#126919=CARTESIAN_POINT('Ctrl Pts',(0.722546794712421,29.8798062253056,
122.948768414092));
#126920=CARTESIAN_POINT('Ctrl Pts',(0.726402245841275,29.9510104852156,
122.94459613592));
#126921=CARTESIAN_POINT('Ctrl Pts',(0.730257696970128,30.0224262000244,
122.944136104907));
#126922=CARTESIAN_POINT('Ctrl Pts',(0.734113148098982,30.0936383723252,
122.947384737042));
#126923=CARTESIAN_POINT('Ctrl Pts',(0.737972633859116,30.1649250663482,
122.950636768788));
#126924=CARTESIAN_POINT('Ctrl Pts',(0.74183211961925,30.2360073064148,122.957605188893));
#126925=CARTESIAN_POINT('Ctrl Pts',(0.745691605379384,30.3064734069668,
122.968234360631));
#126926=CARTESIAN_POINT('Ctrl Pts',(0.749553275858465,30.3769793958963,
122.978869549168));
#126927=CARTESIAN_POINT('Ctrl Pts',(0.753414946337548,30.4468680748809,
122.993169517086));
#126928=CARTESIAN_POINT('Ctrl Pts',(0.757276616816629,30.5157388796174,
123.011027659682));
#126929=CARTESIAN_POINT('Ctrl Pts',(0.761145042131397,30.5847301531956,
123.028917039749));
#126930=CARTESIAN_POINT('Ctrl Pts',(0.765013467446165,30.652699534404,123.050376874523));
#126931=CARTESIAN_POINT('Ctrl Pts',(0.768881892760934,30.7192631891007,
123.075251178126));
#126932=CARTESIAN_POINT('Ctrl Pts',(0.771178768640478,30.7587853306666,
123.090020285274));
#126933=CARTESIAN_POINT('Ctrl Pts',(0.773475644520022,30.7978122923884,
123.105992205597));
#126934=CARTESIAN_POINT('Ctrl Pts',(0.775772520399567,30.8362678306938,
123.123126621786));
#126935=CARTESIAN_POINT('Ctrl Pts',(0.779641657374848,30.9010470146657,
123.15198991554));
#126936=CARTESIAN_POINT('Ctrl Pts',(0.783510794350128,30.9644569792795,
123.184267382412));
#126937=CARTESIAN_POINT('Ctrl Pts',(0.787379931325409,31.0261139902426,
123.219806852747));
#126938=CARTESIAN_POINT('Ctrl Pts',(0.791243304857167,31.0876791572874,
123.255293383696));
#126939=CARTESIAN_POINT('Ctrl Pts',(0.795106678388925,31.147496136394,123.294032032385));
#126940=CARTESIAN_POINT('Ctrl Pts',(0.798970051920683,31.2052025162291,
123.335823189269));
#126941=CARTESIAN_POINT('Ctrl Pts',(0.802828895479853,31.2628412328375,
123.377565344213));
#126942=CARTESIAN_POINT('Ctrl Pts',(0.806687739039024,31.3183738743825,
123.422352614309));
#126943=CARTESIAN_POINT('Ctrl Pts',(0.810546582598194,31.3714654475106,
123.469941148588));
#126944=CARTESIAN_POINT('Ctrl Pts',(0.81440299640865,31.4245235911463,123.517499718403));
#126945=CARTESIAN_POINT('Ctrl Pts',(0.818259410219106,31.4751433549548,
123.567855729509));
#126946=CARTESIAN_POINT('Ctrl Pts',(0.822115824029562,31.5230225639667,
123.620724888882));
#126947=CARTESIAN_POINT('Ctrl Pts',(0.825971099552345,31.5708876405964,
123.673578443003));
#126948=CARTESIAN_POINT('Ctrl Pts',(0.829826375075127,31.6160134424675,
123.728943312848));
#126949=CARTESIAN_POINT('Ctrl Pts',(0.83368165059791,31.6581356633396,123.786499408957));
#126950=CARTESIAN_POINT('Ctrl Pts',(0.837537077682162,31.7002595401519,
123.844057767755));
#126951=CARTESIAN_POINT('Ctrl Pts',(0.841392504766413,31.7393793164261,
123.90380713054));
#126952=CARTESIAN_POINT('Ctrl Pts',(0.845247931850665,31.7752729316972,
123.965396897123));
#126953=CARTESIAN_POINT('Ctrl Pts',(0.849107395533993,31.8112041272755,
124.027051147662));
#126954=CARTESIAN_POINT('Ctrl Pts',(0.852966859217321,31.8439021739859,
124.090549227941));
#126955=CARTESIAN_POINT('Ctrl Pts',(0.856826322900649,31.8731905397776,
124.155515089426));
#126956=CARTESIAN_POINT('Ctrl Pts',(0.86068797238042,31.9024954929531,124.220517744144));
#126957=CARTESIAN_POINT('Ctrl Pts',(0.864549621860191,31.9283867446657,
124.286989382022));
#126958=CARTESIAN_POINT('Ctrl Pts',(0.868411271339961,31.9507366155094,
124.354535655973));
#126959=CARTESIAN_POINT('Ctrl Pts',(0.87227967760329,31.9731255922432,124.422200116608));
#126960=CARTESIAN_POINT('Ctrl Pts',(0.876148083866617,31.991960688398,124.490942498754));
#126961=CARTESIAN_POINT('Ctrl Pts',(0.880016490129945,32.0071647859594,
124.56035572959));
#126962=CARTESIAN_POINT('Ctrl Pts',(0.882313590499338,32.0161931391744,
124.601574036908));
#126963=CARTESIAN_POINT('Ctrl Pts',(0.884610690868732,32.0239421476356,
124.643028724662));
#126964=CARTESIAN_POINT('Ctrl Pts',(0.886907791238125,32.0304043318996,
124.684633845342));
#126965=CARTESIAN_POINT('Ctrl Pts',(0.892630100646191,32.0465022866529,
124.788276409971));
#126966=CARTESIAN_POINT('Ctrl Pts',(0.898352410054257,32.0546672631343,
124.893182201794));
#126967=CARTESIAN_POINT('Ctrl Pts',(0.904074719462323,32.0547493742743,
124.998396435465));
#126968=CARTESIAN_POINT('Ctrl Pts',(0.904074719503815,32.0547493742749,
124.998396436228));
#126969=CARTESIAN_POINT('Ctrl Pts',(0.907990067111018,32.0548055567495,
125.070386653581));
#126970=CARTESIAN_POINT('Ctrl Pts',(0.91190541471822,32.0510736369444,125.142516744769));
#126971=CARTESIAN_POINT('Ctrl Pts',(0.915820762325423,32.0435391889099,
125.214348188444));
#126972=CARTESIAN_POINT('Ctrl Pts',(0.919623075674049,32.0362222568748,
125.284105891857));
#126973=CARTESIAN_POINT('Ctrl Pts',(0.923425389022675,32.0253194204732,
125.353581417674));
#126974=CARTESIAN_POINT('Ctrl Pts',(0.9272277023713,32.0108701903739,125.422372631649));
#126975=CARTESIAN_POINT('Ctrl Pts',(0.931027545677041,31.9964303467229,
125.491119157763));
#126976=CARTESIAN_POINT('Ctrl Pts',(0.934827388982782,31.9784487785375,
125.559181763658));
#126977=CARTESIAN_POINT('Ctrl Pts',(0.938627232288522,31.9570164824372,
125.626166152047));
#126978=CARTESIAN_POINT('Ctrl Pts',(0.942425966284456,31.9355904431887,
125.693130985303));
#126979=CARTESIAN_POINT('Ctrl Pts',(0.946224700280389,31.9107158274593,
125.75901774815));
#126980=CARTESIAN_POINT('Ctrl Pts',(0.950023434276323,31.8825336043991,
125.823446896168));
#126981=CARTESIAN_POINT('Ctrl Pts',(0.953822417940025,31.8543495290922,
125.887880278722));
#126982=CARTESIAN_POINT('Ctrl Pts',(0.957621401603728,31.8228576194006,
125.950855398358));
#126983=CARTESIAN_POINT('Ctrl Pts',(0.96142038526743,31.7882463535246,126.012014101486));
#126984=CARTESIAN_POINT('Ctrl Pts',(0.965223301108344,31.753599262901,126.07323610756));
#126985=CARTESIAN_POINT('Ctrl Pts',(0.969026216949257,31.7158266252122,
126.132637511061));
#126986=CARTESIAN_POINT('Ctrl Pts',(0.97282913279017,31.675161503085,126.189887179981));
#126987=CARTESIAN_POINT('Ctrl Pts',(0.976634452698739,31.634470673919,126.247173040098));
#126988=CARTESIAN_POINT('Ctrl Pts',(0.980439772607308,31.5908840375004,
126.30230406996));
#126989=CARTESIAN_POINT('Ctrl Pts',(0.984245092515878,31.5446745740139,
126.354982665164));
#126990=CARTESIAN_POINT('Ctrl Pts',(0.988056543369924,31.4983906600981,
126.407746133546));
#126991=CARTESIAN_POINT('Ctrl Pts',(0.99186799422397,31.449475845254,126.458048934318));
#126992=CARTESIAN_POINT('Ctrl Pts',(0.995679445078016,31.3982386145035,
126.505631541716));
#126993=CARTESIAN_POINT('Ctrl Pts',(0.996467317410906,31.3876472680404,
126.515467433961));
#126994=CARTESIAN_POINT('Ctrl Pts',(0.997255189743795,31.3769567898488,
126.525187236556));
#126995=CARTESIAN_POINT('Ctrl Pts',(0.998043062076684,31.366170062117,126.534788885767));
#126996=CARTESIAN_POINT('Ctrl Pts',(1.0019121504236,31.3131985325603,126.581940724366));
#126997=CARTESIAN_POINT('Ctrl Pts',(1.00578123877052,31.2576792965509,126.626439315946));
#126998=CARTESIAN_POINT('Ctrl Pts',(1.00965032711744,31.1999089898887,126.667997595467));
#126999=CARTESIAN_POINT('Ctrl Pts',(1.01351365063637,31.1422247592866,126.709493954372));
#127000=CARTESIAN_POINT('Ctrl Pts',(1.01737697415529,31.0822965068207,126.74805841597));
#127001=CARTESIAN_POINT('Ctrl Pts',(1.02124029767421,31.0204553247912,126.783442876182));
#127002=CARTESIAN_POINT('Ctrl Pts',(1.0250990894003,30.9586866842988,126.818785829375));
#127003=CARTESIAN_POINT('Ctrl Pts',(1.02895788112638,30.8950099910271,126.850955950611));
#127004=CARTESIAN_POINT('Ctrl Pts',(1.03281667285247,30.8297853695835,126.879748334997));
#127005=CARTESIAN_POINT('Ctrl Pts',(1.03667303373327,30.7646018363806,126.908522581625));
#127006=CARTESIAN_POINT('Ctrl Pts',(1.04052939461407,30.6978727529803,126.933923117222));
#127007=CARTESIAN_POINT('Ctrl Pts',(1.04438575549487,30.6299815907003,126.955791593672));
#127008=CARTESIAN_POINT('Ctrl Pts',(1.04824097706913,30.562110485891,126.977653609394));
#127009=CARTESIAN_POINT('Ctrl Pts',(1.05209619864339,30.4930784459205,126.995985488741));
#127010=CARTESIAN_POINT('Ctrl Pts',(1.05595142021765,30.423285975907,127.010678130657));
#127011=CARTESIAN_POINT('Ctrl Pts',(1.0598067924111,30.3534907791797,127.025371346597));
#127012=CARTESIAN_POINT('Ctrl Pts',(1.06366216460456,30.2829355692416,127.036424944907));
#127013=CARTESIAN_POINT('Ctrl Pts',(1.06751753679801,30.2120312659187,127.043780884726));
#127014=CARTESIAN_POINT('Ctrl Pts',(1.07137694452228,30.1410527449883,127.051144524223));
#127015=CARTESIAN_POINT('Ctrl Pts',(1.07523635224654,30.0697248854185,127.054802728717));
#127016=CARTESIAN_POINT('Ctrl Pts',(1.07909575997081,29.9984630566003,127.054749425187));
#127017=CARTESIAN_POINT('Ctrl Pts',(1.08295735280413,29.9271608809521,127.054696091478));
#127018=CARTESIAN_POINT('Ctrl Pts',(1.08681894563745,29.855925295811,127.050927092239));
#127019=CARTESIAN_POINT('Ctrl Pts',(1.09068053847077,29.7851682357209,127.043488408471));
#127020=CARTESIAN_POINT('Ctrl Pts',(1.09454888760835,29.7142873779527,127.036036709864));
#127021=CARTESIAN_POINT('Ctrl Pts',(1.09841723674594,29.6438871967701,127.024902583843));
#127022=CARTESIAN_POINT('Ctrl Pts',(1.10228558588353,29.5743704095703,127.010183328518));
#127023=CARTESIAN_POINT('Ctrl Pts',(1.10458316822743,29.5330813383943,127.001440916717));
#127024=CARTESIAN_POINT('Ctrl Pts',(1.10688075057134,29.4921036492357,126.991434748372));
#127025=CARTESIAN_POINT('Ctrl Pts',(1.10917833291525,29.4515188007233,126.980193408872));
#127026=CARTESIAN_POINT('Ctrl Pts',(1.11304631609241,29.3831941499399,126.961268597672));
#127027=CARTESIAN_POINT('Ctrl Pts',(1.11691429926958,29.3157163351387,126.938766367241));
#127028=CARTESIAN_POINT('Ctrl Pts',(1.12078228244674,29.2494870750926,126.912780152565));
#127029=CARTESIAN_POINT('Ctrl Pts',(1.12464523167984,29.1833440083867,126.886827757362));
#127030=CARTESIAN_POINT('Ctrl Pts',(1.12850818091294,29.1184467224764,126.857400544407));
#127031=CARTESIAN_POINT('Ctrl Pts',(1.13237113014605,29.0551831268984,126.82464205772));
#127032=CARTESIAN_POINT('Ctrl Pts',(1.13622985100971,28.9919887794099,126.791919428348));
#127033=CARTESIAN_POINT('Ctrl Pts',(1.14008857187337,28.9304250011371,126.755872986859));
#127034=CARTESIAN_POINT('Ctrl Pts',(1.14394729273703,28.8708592500841,126.716694128079));
#127035=CARTESIAN_POINT('Ctrl Pts',(1.14666809674701,28.8288591313792,126.689068912407));
#127036=CARTESIAN_POINT('Ctrl Pts',(1.14938890075699,28.7878519852708,126.659887362842));
#127037=CARTESIAN_POINT('Ctrl Pts',(1.15210970476697,28.7479590808042,126.629230216746));
#127038=CARTESIAN_POINT('',(0.845925280586436,32.05474966952,125.001165378589));
#127039=CARTESIAN_POINT('Ctrl Pts',(0.845925280586436,32.05474966952,125.001165378589));
#127040=CARTESIAN_POINT('Ctrl Pts',(0.850222193392141,32.054704526572,125.080759648224));
#127041=CARTESIAN_POINT('Ctrl Pts',(0.854519106197847,32.0500304314087,
125.160186907327));
#127042=CARTESIAN_POINT('Ctrl Pts',(0.858816019003553,32.0408099573904,
125.238939909425));
#127043=CARTESIAN_POINT('Ctrl Pts',(0.863130502657197,32.0315517791984,
125.318014946689));
#127044=CARTESIAN_POINT('Ctrl Pts',(0.867444986310841,32.0177101011583,
125.3964099409));
#127045=CARTESIAN_POINT('Ctrl Pts',(0.871759469964486,31.9994182650028,
125.473628719646));
#127046=CARTESIAN_POINT('Ctrl Pts',(0.876096086614631,31.9810325930193,
125.551243625274));
#127047=CARTESIAN_POINT('Ctrl Pts',(0.880432703264777,31.9581511248076,
125.627669964385));
#127048=CARTESIAN_POINT('Ctrl Pts',(0.884769319914922,31.9309573702644,
125.702425225004));
#127049=CARTESIAN_POINT('Ctrl Pts',(0.886206935512773,31.9219424702053,
125.727207062403));
#127050=CARTESIAN_POINT('Ctrl Pts',(0.887644551110624,31.9124540468206,
125.751805443833));
#127051=CARTESIAN_POINT('Ctrl Pts',(0.889082166708474,31.9024999031172,
125.776203376145));
#127052=CARTESIAN_POINT('Ctrl Pts',(0.892951333660256,31.8757095400272,
125.841867433723));
#127053=CARTESIAN_POINT('Ctrl Pts',(0.896820500612038,31.8454631736331,
125.906271450168));
#127054=CARTESIAN_POINT('Ctrl Pts',(0.90068966756382,31.8119007010479,125.96902704402));
#127055=CARTESIAN_POINT('Ctrl Pts',(0.904553070015992,31.7783882316965,
126.031689141106));
#127056=CARTESIAN_POINT('Ctrl Pts',(0.908416472468163,31.7415696901814,
126.092707265663));
#127057=CARTESIAN_POINT('Ctrl Pts',(0.912279874920336,31.7016330673258,
126.151712840375));
#127058=CARTESIAN_POINT('Ctrl Pts',(0.916138745673275,31.6617432893861,
126.210649202644));
#127059=CARTESIAN_POINT('Ctrl Pts',(0.919997616426214,31.6187429660066,
126.267577303863));
#127060=CARTESIAN_POINT('Ctrl Pts',(0.923856487179154,31.5728651785641,
126.32215456455));
#127061=CARTESIAN_POINT('Ctrl Pts',(0.927712927099826,31.5270162910805,
126.376697445188));
#127062=CARTESIAN_POINT('Ctrl Pts',(0.931569367020499,31.4782938475611,
126.428892052369));
#127063=CARTESIAN_POINT('Ctrl Pts',(0.935425806941171,31.4269723943476,
126.47842732262));
#127064=CARTESIAN_POINT('Ctrl Pts',(0.939281107448132,31.3756661044372,
126.52794795731));
#127065=CARTESIAN_POINT('Ctrl Pts',(0.943136407955094,31.3217626786443,
126.574810477783));
#127066=CARTESIAN_POINT('Ctrl Pts',(0.946991708462056,31.2655736456561,
126.618740531994));
#127067=CARTESIAN_POINT('Ctrl Pts',(0.950847159360819,31.2093824207842,
126.662672299878));
#127068=CARTESIAN_POINT('Ctrl Pts',(0.954702610259581,31.1509057957416,
126.703671076931));
#127069=CARTESIAN_POINT('Ctrl Pts',(0.958558061158344,31.0904871377984,
126.74150376537));
#127070=CARTESIAN_POINT('Ctrl Pts',(0.962417546689029,31.0300052532568,
126.77937604476));
#127071=CARTESIAN_POINT('Ctrl Pts',(0.966277032219715,30.9675776914572,
126.814075363251));
#127072=CARTESIAN_POINT('Ctrl Pts',(0.9701365177504,30.9035747026936,126.845413319328));
#127073=CARTESIAN_POINT('Ctrl Pts',(0.973998188000047,30.8395354840899,
126.876769014718));
#127074=CARTESIAN_POINT('Ctrl Pts',(0.977859858249693,30.7739195102478,
126.904759369209));
#127075=CARTESIAN_POINT('Ctrl Pts',(0.98172152849934,30.7071168743834,126.929244227272));
#127076=CARTESIAN_POINT('Ctrl Pts',(0.98558995358719,30.6401973872688,126.953771914278));
#127077=CARTESIAN_POINT('Ctrl Pts',(0.989458378675041,30.5720875582374,
126.974781719263));
#127078=CARTESIAN_POINT('Ctrl Pts',(0.993326803762892,30.50319180764,126.992183617849));
#127079=CARTESIAN_POINT('Ctrl Pts',(0.995623681690939,30.4622849462456,
127.002515997528));
#127080=CARTESIAN_POINT('Ctrl Pts',(0.997920559618986,30.4211012160408,
127.011577427828));
#127081=CARTESIAN_POINT('Ctrl Pts',(1.00021743754703,30.3797262583935,127.019357702634));
#127082=CARTESIAN_POINT('Ctrl Pts',(1.00411924003509,30.3094408894063,127.032574380467));
#127083=CARTESIAN_POINT('Ctrl Pts',(1.00802104252315,30.2383258874802,127.042143266351));
#127084=CARTESIAN_POINT('Ctrl Pts',(1.01192284501121,30.166793753524,127.047969093098));
#127085=CARTESIAN_POINT('Ctrl Pts',(1.01578547054818,30.0959798545174,127.053736424283));
#127086=CARTESIAN_POINT('Ctrl Pts',(1.01964809608515,30.0247576518687,127.055835443684));
#127087=CARTESIAN_POINT('Ctrl Pts',(1.02351072162212,29.9535385837193,127.054224646746));
#127088=CARTESIAN_POINT('Ctrl Pts',(1.02736946493094,29.8823910960708,127.052615468779));
#127089=CARTESIAN_POINT('Ctrl Pts',(1.03122820823977,29.811247219696,127.047303883362));
#127090=CARTESIAN_POINT('Ctrl Pts',(1.0350869515486,29.7405211518721,127.038300343393));
#127091=CARTESIAN_POINT('Ctrl Pts',(1.03894310737994,29.669842509361,127.02930284074));
#127092=CARTESIAN_POINT('Ctrl Pts',(1.04279926321129,29.5995815998998,127.016618359122));
#127093=CARTESIAN_POINT('Ctrl Pts',(1.04665541904263,29.530148521361,127.000309263719));
#127094=CARTESIAN_POINT('Ctrl Pts',(1.05058919222745,29.4593178821334,126.983671896099));
#127095=CARTESIAN_POINT('Ctrl Pts',(1.05452296541227,29.3893492832019,126.963262453114));
#127096=CARTESIAN_POINT('Ctrl Pts',(1.05845673859709,29.3206667936306,126.93920188666));
#127097=CARTESIAN_POINT('Ctrl Pts',(1.06231299660405,29.2533376956111,126.915615434752));
#127098=CARTESIAN_POINT('Ctrl Pts',(1.06616925461102,29.187244932335,126.888520669323));
#127099=CARTESIAN_POINT('Ctrl Pts',(1.07002551261798,29.1227702090487,126.858081122117));
#127100=CARTESIAN_POINT('Ctrl Pts',(1.07399804339173,29.0563514627095,126.826723770561));
#127101=CARTESIAN_POINT('Ctrl Pts',(1.07797057416548,28.9916504052664,126.791816904311));
#127102=CARTESIAN_POINT('Ctrl Pts',(1.08194310493923,28.9290573062697,126.75359040521));
#127103=CARTESIAN_POINT('Ctrl Pts',(1.08591563571297,28.8664642072729,126.715363906109));
#127104=CARTESIAN_POINT('Ctrl Pts',(1.08988816648672,28.8059795118765,126.673818116667));
#127105=CARTESIAN_POINT('Ctrl Pts',(1.09386069726047,28.7479590808042,126.629230216746));
#127106=CARTESIAN_POINT('Ctrl Pts',(0.393902765004298,28.7479590808042,
126.629230216746));
#127107=CARTESIAN_POINT('Ctrl Pts',(0.397765021747291,28.6913182945486,
126.585702554812));
#127108=CARTESIAN_POINT('Ctrl Pts',(0.401627278490284,28.63696077667,126.539226006323));
#127109=CARTESIAN_POINT('Ctrl Pts',(0.405489535233277,28.5851971742094,
126.490077355923));
#127110=CARTESIAN_POINT('Ctrl Pts',(0.409356061646295,28.5333763478207,
126.440874372388));
#127111=CARTESIAN_POINT('Ctrl Pts',(0.413222588059313,28.4841555100294,
126.388993726621));
#127112=CARTESIAN_POINT('Ctrl Pts',(0.417089114472331,28.4378084641117,
126.334749102902));
#127113=CARTESIAN_POINT('Ctrl Pts',(0.420958121188522,28.3914316874453,
126.280469682289));
#127114=CARTESIAN_POINT('Ctrl Pts',(0.424827127904714,28.3479326658746,
126.223823649619));
#127115=CARTESIAN_POINT('Ctrl Pts',(0.428696134620905,28.307543244335,126.165155651707));
#127116=CARTESIAN_POINT('Ctrl Pts',(0.432571649270529,28.267085885031,126.106388970216));
#127117=CARTESIAN_POINT('Ctrl Pts',(0.436447163920152,28.2297488157466,
126.045593948724));
#127118=CARTESIAN_POINT('Ctrl Pts',(0.440322678569775,28.1957187011626,
125.983141168483));
#127119=CARTESIAN_POINT('Ctrl Pts',(0.441728813497928,28.1833717132005,
125.960481717133));
#127120=CARTESIAN_POINT('Ctrl Pts',(0.443134948426081,28.1714596034836,
125.937604232533));
#127121=CARTESIAN_POINT('Ctrl Pts',(0.444541083354233,28.1599897057763,
125.914527025107));
#127122=CARTESIAN_POINT('Ctrl Pts',(0.448406425456853,28.1284599587848,
125.851089797506));
#127123=CARTESIAN_POINT('Ctrl Pts',(0.452271767559472,28.1001518064021,
125.7858935227));
#127124=CARTESIAN_POINT('Ctrl Pts',(0.456137109662091,28.0752645120309,
125.719298869631));
#127125=CARTESIAN_POINT('Ctrl Pts',(0.459996632892445,28.0504146829042,
125.652804467916));
#127126=CARTESIAN_POINT('Ctrl Pts',(0.463856156122799,28.0289756594278,
125.584916318474));
#127127=CARTESIAN_POINT('Ctrl Pts',(0.467715679353152,28.0111001043075,
125.516018185158));
#127128=CARTESIAN_POINT('Ctrl Pts',(0.471570608822083,27.9932458253994,
125.447202057202));
#127129=CARTESIAN_POINT('Ctrl Pts',(0.475425538291014,27.9789467120985,
125.377378801993));
#127130=CARTESIAN_POINT('Ctrl Pts',(0.479280467759945,27.968306144083,125.30694891811));
#127131=CARTESIAN_POINT('Ctrl Pts',(0.483132930157,27.957672385802,125.236564107837));
#127132=CARTESIAN_POINT('Ctrl Pts',(0.486985392554054,27.9506926004373,
125.165573919304));
#127133=CARTESIAN_POINT('Ctrl Pts',(0.490837854951109,27.947419127263,125.094389212171));
#127134=CARTESIAN_POINT('Ctrl Pts',(0.494689147554331,27.9441466480735,
125.023226120157));
#127135=CARTESIAN_POINT('Ctrl Pts',(0.498540440157554,27.9445782693539,
124.951869112878));
#127136=CARTESIAN_POINT('Ctrl Pts',(0.502391732760776,27.948714342242,124.880732599692));
#127137=CARTESIAN_POINT('Ctrl Pts',(0.506243151200269,27.9528505502711,
124.809593762207));
#127138=CARTESIAN_POINT('Ctrl Pts',(0.510094569639761,27.9606914197365,
124.738675919046));
#127139=CARTESIAN_POINT('Ctrl Pts',(0.513945988079253,27.9721852967047,
124.668390151534));
#127140=CARTESIAN_POINT('Ctrl Pts',(0.517801431273902,27.9836911848427,
124.598030934977));
#127141=CARTESIAN_POINT('Ctrl Pts',(0.521656874468552,27.9988576221953,
124.528305594113));
#127142=CARTESIAN_POINT('Ctrl Pts',(0.525512317663202,28.0175816385012,
124.459615875055));
#127143=CARTESIAN_POINT('Ctrl Pts',(0.52936993382045,28.0363162078317,124.390887441852));
#127144=CARTESIAN_POINT('Ctrl Pts',(0.533227549977698,28.0586121949647,
124.32319625497));
#127145=CARTESIAN_POINT('Ctrl Pts',(0.537085166134947,28.0843173029351,
124.2569270785));
#127146=CARTESIAN_POINT('Ctrl Pts',(0.540949562528794,28.1100675908058,
124.190541425772));
#127147=CARTESIAN_POINT('Ctrl Pts',(0.544813958922641,28.1392387629363,
124.125583217714));
#127148=CARTESIAN_POINT('Ctrl Pts',(0.548678355316488,28.1716314268244,
124.062414844868));
#127149=CARTESIAN_POINT('Ctrl Pts',(0.551011021608591,28.1911846163687,
124.024284508575));
#127150=CARTESIAN_POINT('Ctrl Pts',(0.553343687900694,28.2119107377833,
123.986805830846));
#127151=CARTESIAN_POINT('Ctrl Pts',(0.555676354192796,28.233758395163,123.950053260473));
#127152=CARTESIAN_POINT('Ctrl Pts',(0.55954593324945,28.2700007148295,123.889085698557));
#127153=CARTESIAN_POINT('Ctrl Pts',(0.563415512306104,28.3094743779065,
123.829877604035));
#127154=CARTESIAN_POINT('Ctrl Pts',(0.567285091362758,28.3519833328474,
123.77279234549));
#127155=CARTESIAN_POINT('Ctrl Pts',(0.571148904349671,28.3944289450848,
123.715792149837));
#127156=CARTESIAN_POINT('Ctrl Pts',(0.575012717336582,28.4399005835988,
123.6609088975));
#127157=CARTESIAN_POINT('Ctrl Pts',(0.578876530323495,28.4881575770453,
123.608479230965));
#127158=CARTESIAN_POINT('Ctrl Pts',(0.582735807188568,28.5363579167142,
123.556111116932));
#127159=CARTESIAN_POINT('Ctrl Pts',(0.586595084053642,28.587336788608,123.506191222558));
#127160=CARTESIAN_POINT('Ctrl Pts',(0.590454360918715,28.6408127906897,
123.459023785859));
#127161=CARTESIAN_POINT('Ctrl Pts',(0.594311203983475,28.69425506886,123.411886094661));
#127162=CARTESIAN_POINT('Ctrl Pts',(0.598168047048235,28.7501909894982,
123.36749773779));
#127163=CARTESIAN_POINT('Ctrl Pts',(0.602024890112995,28.8083028229929,
123.326125631711));
#127164=CARTESIAN_POINT('Ctrl Pts',(0.60588059017397,28.8663974346187,123.284765786561));
#127165=CARTESIAN_POINT('Ctrl Pts',(0.609736290234945,28.9266662834845,
123.246420699076));
#127166=CARTESIAN_POINT('Ctrl Pts',(0.61359199029592,28.988760515234,123.211315492618));
#127167=CARTESIAN_POINT('Ctrl Pts',(0.61744783653321,29.0508571010842,123.176208955259));
#127168=CARTESIAN_POINT('Ctrl Pts',(0.6213036827705,29.1147787833747,123.14434277988));
#127169=CARTESIAN_POINT('Ctrl Pts',(0.62515952900779,29.1801513425479,123.115896568292));
#127170=CARTESIAN_POINT('Ctrl Pts',(0.629019400628104,29.2455921486309,
123.087420659747));
#127171=CARTESIAN_POINT('Ctrl Pts',(0.632879272248418,29.3124864090116,
123.062372036382));
#127172=CARTESIAN_POINT('Ctrl Pts',(0.636739143868732,29.3804399501159,
123.040882109957));
#127173=CARTESIAN_POINT('Ctrl Pts',(0.640601195567596,29.4484318717861,
123.019380045892));
#127174=CARTESIAN_POINT('Ctrl Pts',(0.644463247266461,29.5174837949454,
123.001440802256));
#127175=CARTESIAN_POINT('Ctrl Pts',(0.648325298965326,29.5871890777104,
122.98714513565));
#127176=CARTESIAN_POINT('Ctrl Pts',(0.652194093943705,29.6570160683762,
122.972824508302));
#127177=CARTESIAN_POINT('Ctrl Pts',(0.656062888922084,29.727498215944,122.962160232273));
#127178=CARTESIAN_POINT('Ctrl Pts',(0.659931683900464,29.7982221448728,
122.955181362644));
#127179=CARTESIAN_POINT('Ctrl Pts',(0.662224997610761,29.8401453164972,
122.951044483462));
#127180=CARTESIAN_POINT('Ctrl Pts',(0.664518311321058,29.8821533932848,
122.948201581459));
#127181=CARTESIAN_POINT('Ctrl Pts',(0.666811625031356,29.9241605753862,
122.946650067774));
#127182=CARTESIAN_POINT('Ctrl Pts',(0.670681339183318,29.9950430657896,
122.944032059414));
#127183=CARTESIAN_POINT('Ctrl Pts',(0.674551053335281,30.0661995809263,
122.945083589692));
#127184=CARTESIAN_POINT('Ctrl Pts',(0.678420767487243,30.1372184602691,
122.949836919496));
#127185=CARTESIAN_POINT('Ctrl Pts',(0.682284730622962,30.20813179416,122.954583185089));
#127186=CARTESIAN_POINT('Ctrl Pts',(0.68614869375868,30.2789074176964,122.963020297639));
#127187=CARTESIAN_POINT('Ctrl Pts',(0.6900126568944,30.349131940276,122.975128534751));
#127188=CARTESIAN_POINT('Ctrl Pts',(0.693872105680565,30.4192744180661,
122.987222625555));
#127189=CARTESIAN_POINT('Ctrl Pts',(0.697731554466732,30.4888665976082,
123.002979239247));
#127190=CARTESIAN_POINT('Ctrl Pts',(0.701591003252898,30.5575002352797,
123.022326859624));
#127191=CARTESIAN_POINT('Ctrl Pts',(0.705448031609014,30.626090829779,123.041662346258));
#127192=CARTESIAN_POINT('Ctrl Pts',(0.70930505996513,30.693723608797,123.064584239985));
#127193=CARTESIAN_POINT('Ctrl Pts',(0.713162088321247,30.7600019965348,
123.090970265354));
#127194=CARTESIAN_POINT('Ctrl Pts',(0.717017986794997,30.8262609686048,
123.11734856117));
#127195=CARTESIAN_POINT('Ctrl Pts',(0.720873885268748,30.8911658861629,
123.147188794448));
#127196=CARTESIAN_POINT('Ctrl Pts',(0.724729783742498,30.9543384186385,
123.180319878327));
#127197=CARTESIAN_POINT('Ctrl Pts',(0.72858584127878,31.0175135570912,123.213452328921));
#127198=CARTESIAN_POINT('Ctrl Pts',(0.732441898815062,31.078955739558,123.249875672151));
#127199=CARTESIAN_POINT('Ctrl Pts',(0.736297956351344,31.1383111354956,
123.289372828081));
#127200=CARTESIAN_POINT('Ctrl Pts',(0.740158057635936,31.1977287759096,
123.328911403662));
#127201=CARTESIAN_POINT('Ctrl Pts',(0.744018158920527,31.2550548562536,
123.371529957045));
#127202=CARTESIAN_POINT('Ctrl Pts',(0.747878260205119,31.3099652199,123.416968514163));
#127203=CARTESIAN_POINT('Ctrl Pts',(0.751740552281313,31.3649067477969,
123.462432859829));
#127204=CARTESIAN_POINT('Ctrl Pts',(0.755602844357507,31.4174294720272,
123.510720066518));
#127205=CARTESIAN_POINT('Ctrl Pts',(0.759465136433701,31.4672450411022,
123.561532220778));
#127206=CARTESIAN_POINT('Ctrl Pts',(0.763334186256716,31.5171477711161,
123.612433279674));
#127207=CARTESIAN_POINT('Ctrl Pts',(0.76720323607973,31.5643335676119,123.665867742371));
#127208=CARTESIAN_POINT('Ctrl Pts',(0.771072285902744,31.608553871162,123.721504006236));
#127209=CARTESIAN_POINT('Ctrl Pts',(0.773363822558468,31.6347443962645,
123.754455904988));
#127210=CARTESIAN_POINT('Ctrl Pts',(0.775655359214192,31.659895470117,123.788179586632));
#127211=CARTESIAN_POINT('Ctrl Pts',(0.777946895869915,31.6839628542883,
123.822601737781));
#127212=CARTESIAN_POINT('Ctrl Pts',(0.781859926094245,31.7250603429308,
123.881381036595));
#127213=CARTESIAN_POINT('Ctrl Pts',(0.785772956318574,31.7631546821155,
123.942426067642));
#127214=CARTESIAN_POINT('Ctrl Pts',(0.789685986542903,31.7979910101894,
124.00540164399));
#127215=CARTESIAN_POINT('Ctrl Pts',(0.793592842844341,31.8327723740052,
124.068277858378));
#127216=CARTESIAN_POINT('Ctrl Pts',(0.797499699145779,31.8643057068968,
124.133078161557));
#127217=CARTESIAN_POINT('Ctrl Pts',(0.801406555447216,31.8923787917684,
124.199437653293));
#127218=CARTESIAN_POINT('Ctrl Pts',(0.805307698977523,31.9204108269836,
124.265700111363));
#127219=CARTESIAN_POINT('Ctrl Pts',(0.80920884250783,31.9449924901972,124.333516794022));
#127220=CARTESIAN_POINT('Ctrl Pts',(0.813109986038136,31.9659578093617,
124.40249899221));
#127221=CARTESIAN_POINT('Ctrl Pts',(0.817007743496307,31.9869049312765,
124.471421315981));
#127222=CARTESIAN_POINT('Ctrl Pts',(0.820905500954478,32.0042418055704,
124.541506697131));
#127223=CARTESIAN_POINT('Ctrl Pts',(0.824803258412648,32.0178512785365,
124.612348377782));
#127224=CARTESIAN_POINT('Ctrl Pts',(0.828699254139108,32.0314546002117,
124.683158038986));
#127225=CARTESIAN_POINT('Ctrl Pts',(0.832595249865569,32.0413337728066,
124.754722859513));
#127226=CARTESIAN_POINT('Ctrl Pts',(0.83649124559203,32.0474223847194,124.826624277795));
#127227=CARTESIAN_POINT('Ctrl Pts',(0.839635923907246,32.0523368474643,
124.88465997567));
#127228=CARTESIAN_POINT('Ctrl Pts',(0.842780602222461,32.0547827071795,
124.942914632312));
#127229=CARTESIAN_POINT('Ctrl Pts',(0.845925280537677,32.0547496695206,
125.001165377686));
#127230=CARTESIAN_POINT('Origin',(-1.54592528053767,30.,55.));
#127231=CARTESIAN_POINT('',(0.904074719503237,32.0547493739418,54.9983960094259));
#127232=CARTESIAN_POINT('Ctrl Pts',(0.452117494115148,28.7479524050421,
56.6292250864936));
#127233=CARTESIAN_POINT('Ctrl Pts',(0.455982334291425,28.6916143219704,
56.5859296805983));
#127234=CARTESIAN_POINT('Ctrl Pts',(0.459847174467703,28.6374344239205,
56.5396393262805));
#127235=CARTESIAN_POINT('Ctrl Pts',(0.46371201464398,28.5857463933444,56.4905986376492));
#127236=CARTESIAN_POINT('Ctrl Pts',(0.467572025665764,28.5341229474532,
56.4416192258239));
#127237=CARTESIAN_POINT('Ctrl Pts',(0.471432036687546,28.4849855344149,
56.3898966386622));
#127238=CARTESIAN_POINT('Ctrl Pts',(0.475292047709329,28.4386349661428,
56.3357158356282));
#127239=CARTESIAN_POINT('Ctrl Pts',(0.479149432414872,28.3923159343738,
56.2815718967177));
#127240=CARTESIAN_POINT('Ctrl Pts',(0.483006817120415,28.3487803004197,
56.2249734280577));
#127241=CARTESIAN_POINT('Ctrl Pts',(0.486864201825958,28.3082911618458,
56.1662412998222));
#127242=CARTESIAN_POINT('Ctrl Pts',(0.490720251061402,28.2678160410684,
56.107529505312));
#127243=CARTESIAN_POINT('Ctrl Pts',(0.494576300296846,28.2303855974567,
56.0466859170156));
#127244=CARTESIAN_POINT('Ctrl Pts',(0.498432349532289,28.1962207978899,
55.9840620674201));
#127245=CARTESIAN_POINT('Ctrl Pts',(0.502288352334105,28.1620564097275,
55.921438971926));
#127246=CARTESIAN_POINT('Ctrl Pts',(0.506144355135921,28.1311578184329,
55.8570360848732));
#127247=CARTESIAN_POINT('Ctrl Pts',(0.510000357937737,28.1037001923878,
55.7912298036284));
#127248=CARTESIAN_POINT('Ctrl Pts',(0.513860274577921,28.0762146968841,
55.7253567290845));
#127249=CARTESIAN_POINT('Ctrl Pts',(0.517720191218106,28.0521773284542,
55.6580778649955));
#127250=CARTESIAN_POINT('Ctrl Pts',(0.52158010785829,28.0317148515083,55.5897890612133));
#127251=CARTESIAN_POINT('Ctrl Pts',(0.525442030519987,28.011241740092,55.5214647673358));
#127252=CARTESIAN_POINT('Ctrl Pts',(0.529303953181685,27.9943473351431,
55.4521299607925));
#127253=CARTESIAN_POINT('Ctrl Pts',(0.533165875843382,27.9811076004398,
55.3821924142338));
#127254=CARTESIAN_POINT('Ctrl Pts',(0.537034750574321,27.967844032128,55.3121289690725));
#127255=CARTESIAN_POINT('Ctrl Pts',(0.540903625305261,27.9582483400407,
55.2414610986422));
#127256=CARTESIAN_POINT('Ctrl Pts',(0.5447725000362,27.9523447016016,55.1706028764146));
#127257=CARTESIAN_POINT('Ctrl Pts',(0.547682326264951,27.9479045056351,
55.1173095733486));
#127258=CARTESIAN_POINT('Ctrl Pts',(0.550592152493701,27.9455517174084,
55.063908723299));
#127259=CARTESIAN_POINT('Ctrl Pts',(0.553501978722452,27.9452772154524,
55.010575498138));
#127260=CARTESIAN_POINT('Ctrl Pts',(0.557370495096533,27.9449122743088,
54.9396707641098));
#127261=CARTESIAN_POINT('Ctrl Pts',(0.561239011470614,27.9482211155754,
54.8686078387497));
#127262=CARTESIAN_POINT('Ctrl Pts',(0.565107527844695,27.9552231671876,
54.7977989453697));
#127263=CARTESIAN_POINT('Ctrl Pts',(0.568970270673785,27.9622147686281,
54.727095730315));
#127264=CARTESIAN_POINT('Ctrl Pts',(0.572833013502874,27.9728885921152,
54.6566462743214));
#127265=CARTESIAN_POINT('Ctrl Pts',(0.576695756331965,27.9872120544266,
54.5868629178416));
#127266=CARTESIAN_POINT('Ctrl Pts',(0.580553957234481,28.00151867479,54.5171616146837));
#127267=CARTESIAN_POINT('Ctrl Pts',(0.584412158136999,28.0194663127297,
54.4481253290154));
#127268=CARTESIAN_POINT('Ctrl Pts',(0.588270359039516,28.0409707773654,
54.380159643647));
#127269=CARTESIAN_POINT('Ctrl Pts',(0.59212612316034,28.0624616601046,54.3122368843837));
#127270=CARTESIAN_POINT('Ctrl Pts',(0.595981887281165,28.0875047664499,
54.2453838461247));
#127271=CARTESIAN_POINT('Ctrl Pts',(0.599837651401989,28.1159655353422,
54.1799928668105));
#127272=CARTESIAN_POINT('Ctrl Pts',(0.603692271167429,28.1444178573397,
54.1146212949386));
#127273=CARTESIAN_POINT('Ctrl Pts',(0.607546890932868,28.176285634357,54.0507113658897));
#127274=CARTESIAN_POINT('Ctrl Pts',(0.611401510698308,28.2113860886913,
53.9886356547846));
#127275=CARTESIAN_POINT('Ctrl Pts',(0.615256276916005,28.2464878766308,
53.9265575851776));
#127276=CARTESIAN_POINT('Ctrl Pts',(0.619111043133703,28.2848223446265,
53.8663142937954));
#127277=CARTESIAN_POINT('Ctrl Pts',(0.622965809351401,28.3261615130957,
53.8082524251093));
#127278=CARTESIAN_POINT('Ctrl Pts',(0.626824608897236,28.3675439356617,
53.750129804991));
#127279=CARTESIAN_POINT('Ctrl Pts',(0.630683408443071,28.4119370521812,
53.694193560574));
#127280=CARTESIAN_POINT('Ctrl Pts',(0.634542207988907,28.4590709436111,
53.6407593275374));
#127281=CARTESIAN_POINT('Ctrl Pts',(0.638403190481053,28.5062314989694,
53.5872948664311));
#127282=CARTESIAN_POINT('Ctrl Pts',(0.6422641729732,28.5561355755575,53.5363355816682));
#127283=CARTESIAN_POINT('Ctrl Pts',(0.646125155465346,28.608476463058,53.4881601246705));
#127284=CARTESIAN_POINT('Ctrl Pts',(0.649992897456676,28.6609089847958,
53.4399003259378));
#127285=CARTESIAN_POINT('Ctrl Pts',(0.653860639448007,28.7157864606461,
53.3944343955679));
#127286=CARTESIAN_POINT('Ctrl Pts',(0.657728381439337,28.77276976465,53.3520001480756));
#127287=CARTESIAN_POINT('Ctrl Pts',(0.660031337479892,28.8066991333775,
53.3267336730088));
#127288=CARTESIAN_POINT('Ctrl Pts',(0.662334293520448,28.841374526437,53.3025411983353));
#127289=CARTESIAN_POINT('Ctrl Pts',(0.664637249561003,28.8767200983988,
53.2794652502321));
#127290=CARTESIAN_POINT('Ctrl Pts',(0.668506451727346,28.9361042816819,
53.2406952924827));
#127291=CARTESIAN_POINT('Ctrl Pts',(0.67237565389369,28.9976142977631,53.2049275043511));
#127292=CARTESIAN_POINT('Ctrl Pts',(0.676244856060033,29.0609141675609,
53.1724017504352));
#127293=CARTESIAN_POINT('Ctrl Pts',(0.680108294091384,29.1241197365239,
53.1399244516861));
#127294=CARTESIAN_POINT('Ctrl Pts',(0.683971732122735,29.1891094378702,
53.1106798202829));
#127295=CARTESIAN_POINT('Ctrl Pts',(0.687835170154086,29.2555190013059,
53.0848640766036));
#127296=CARTESIAN_POINT('Ctrl Pts',(0.691694076853992,29.321850674598,53.0590786115751));
#127297=CARTESIAN_POINT('Ctrl Pts',(0.695552983553898,29.3895984515335,
53.0367142210235));
#127298=CARTESIAN_POINT('Ctrl Pts',(0.699411890253804,29.4583757634714,
53.017920095227));
#127299=CARTESIAN_POINT('Ctrl Pts',(0.703268366328725,29.527109754369,52.9991378073617));
#127300=CARTESIAN_POINT('Ctrl Pts',(0.707124842403646,29.5968715262351,
52.9839214503626));
#127301=CARTESIAN_POINT('Ctrl Pts',(0.710981318478567,29.6672583326809,
52.9723707081101));
#127302=CARTESIAN_POINT('Ctrl Pts',(0.714836655293049,29.7376243458164,
52.9608233781189));
#127303=CARTESIAN_POINT('Ctrl Pts',(0.718691992107531,29.8086145478841,
52.9529395916762));
#127304=CARTESIAN_POINT('Ctrl Pts',(0.722547328922012,29.8798166566084,
52.9487678028874));
#127305=CARTESIAN_POINT('Ctrl Pts',(0.726402816227741,29.9510215446733,
52.9445958512549));
#127306=CARTESIAN_POINT('Ctrl Pts',(0.73025830353347,30.0224378707715,52.9441362111621));
#127307=CARTESIAN_POINT('Ctrl Pts',(0.734113790839199,30.0936506311823,
52.9473852963161));
#127308=CARTESIAN_POINT('Ctrl Pts',(0.737973312677396,30.1649379114063,
52.9506377814398));
#127309=CARTESIAN_POINT('Ctrl Pts',(0.741832834515594,30.236020714471,52.9576067168871));
#127310=CARTESIAN_POINT('Ctrl Pts',(0.74569235635379,30.3064873487565,52.968236463672));
#127311=CARTESIAN_POINT('Ctrl Pts',(0.749554062909574,30.376993871324,52.9788722275221));
#127312=CARTESIAN_POINT('Ctrl Pts',(0.753415769465359,30.446883054666,52.9931728304852));
#127313=CARTESIAN_POINT('Ctrl Pts',(0.757277476021143,30.5157543284872,
53.0110316656249));
#127314=CARTESIAN_POINT('Ctrl Pts',(0.761145937018379,30.5847460638143,
53.0289217373319));
#127315=CARTESIAN_POINT('Ctrl Pts',(0.765014398015613,30.6527158716266,
53.050382320605));
#127316=CARTESIAN_POINT('Ctrl Pts',(0.768882859012849,30.7192799118218,
53.0752574273556));
#127317=CARTESIAN_POINT('Ctrl Pts',(0.771179412808421,30.7587963756735,
53.0900248040629));
#127318=CARTESIAN_POINT('Ctrl Pts',(0.773475966603994,30.7978177932748,
53.1059946535758));
#127319=CARTESIAN_POINT('Ctrl Pts',(0.775772520399566,30.8362679536972,
53.1231266765924));
#127320=CARTESIAN_POINT('Ctrl Pts',(0.779641665029999,30.9010472904688,
53.1519900435167));
#127321=CARTESIAN_POINT('Ctrl Pts',(0.783510809660432,30.9644573937457,
53.1842675964721));
#127322=CARTESIAN_POINT('Ctrl Pts',(0.787379954290865,31.0261145286024,
53.2198071630604));
#127323=CARTESIAN_POINT('Ctrl Pts',(0.791243335712682,31.0876798232813,
53.2552937923833));
#127324=CARTESIAN_POINT('Ctrl Pts',(0.7951067171345,31.1474969150771,53.2940325499976));
#127325=CARTESIAN_POINT('Ctrl Pts',(0.798970098556317,31.2052033923354,
53.3358238237484));
#127326=CARTESIAN_POINT('Ctrl Pts',(0.802828950318409,31.2628422110641,
53.3775660989074));
#127327=CARTESIAN_POINT('Ctrl Pts',(0.8066878020805,31.3183749391514,53.4223534976467));
#127328=CARTESIAN_POINT('Ctrl Pts',(0.810546653842592,31.3714665831634,
53.469942166529));
#127329=CARTESIAN_POINT('Ctrl Pts',(0.814403076044992,31.4245248003102,
53.517500873257));
#127330=CARTESIAN_POINT('Ctrl Pts',(0.818259498247393,31.4751446217494,
53.5678570275087));
#127331=CARTESIAN_POINT('Ctrl Pts',(0.822115920449793,31.5230238726558,
53.6207263339639));
#127332=CARTESIAN_POINT('Ctrl Pts',(0.825971204541594,31.5708889933969,
53.6735800375845));
#127333=CARTESIAN_POINT('Ctrl Pts',(0.829826488633396,31.6160148234011,
53.7289450610951));
#127334=CARTESIAN_POINT('Ctrl Pts',(0.833681772725197,31.6581370567484,
53.786501312923));
#127335=CARTESIAN_POINT('Ctrl Pts',(0.837537208543773,31.7002609478389,
53.8440598299081));
#127336=CARTESIAN_POINT('Ctrl Pts',(0.84139264436235,31.7393807224787,53.9038093531206));
#127337=CARTESIAN_POINT('Ctrl Pts',(0.845248080180926,31.7752743206541,
53.9653992804343));
#127338=CARTESIAN_POINT('Ctrl Pts',(0.84910755279315,31.8112055008452,54.0270536948355));
#127339=CARTESIAN_POINT('Ctrl Pts',(0.852967025405373,31.8439035163674,
54.0905519394591));
#127340=CARTESIAN_POINT('Ctrl Pts',(0.856826498017596,31.8731918357075,
54.1555179639928));
#127341=CARTESIAN_POINT('Ctrl Pts',(0.860688156549584,31.9024967433027,
54.2205207838432));
#127342=CARTESIAN_POINT('Ctrl Pts',(0.864549815081573,31.9283879339482,
54.2869925856471));
#127343=CARTESIAN_POINT('Ctrl Pts',(0.868411473613561,31.9507377288338,
54.3545390206958));
#127344=CARTESIAN_POINT('Ctrl Pts',(0.872279889027977,31.9731266299571,
54.4222036441644));
#127345=CARTESIAN_POINT('Ctrl Pts',(0.876148304442392,31.9919616354081,
54.4909461863541));
#127346=CARTESIAN_POINT('Ctrl Pts',(0.880016719856808,32.007165627798,54.5603595729619));
#127347=CARTESIAN_POINT('Ctrl Pts',(0.88231374365058,32.0161935962395,54.6015765012294));
#127348=CARTESIAN_POINT('Ctrl Pts',(0.884610767444353,32.0239423062121,
54.6430297915521));
#127349=CARTESIAN_POINT('Ctrl Pts',(0.886907791238125,32.0304042790898,
54.6846335053405));
#127350=CARTESIAN_POINT('Ctrl Pts',(0.892630100646191,32.0465022438967,
54.7882760202622));
#127351=CARTESIAN_POINT('Ctrl Pts',(0.898352410054257,32.0546672409534,
54.8931817831011));
#127352=CARTESIAN_POINT('Ctrl Pts',(0.904074719462322,32.0547493739412,
54.9983960086736));
#127353=CARTESIAN_POINT('Ctrl Pts',(0.904074719503237,32.0547493739418,
54.9983960094259));
#127354=CARTESIAN_POINT('Ctrl Pts',(0.907990067110464,32.0548055713655,
55.070386221239));
#127355=CARTESIAN_POINT('Ctrl Pts',(0.911905414717691,32.0510736670533,
55.1425163169785));
#127356=CARTESIAN_POINT('Ctrl Pts',(0.915820762324918,32.0435392324816,
55.2143477730435));
#127357=CARTESIAN_POINT('Ctrl Pts',(0.919623060278423,32.0362223431458,
55.2841052060461));
#127358=CARTESIAN_POINT('Ctrl Pts',(0.923425358231927,32.0253195766014,
55.3535804711167));
#127359=CARTESIAN_POINT('Ctrl Pts',(0.927227656185431,32.0108704414169,
55.4223714364582));
#127360=CARTESIAN_POINT('Ctrl Pts',(0.931027483988993,31.996430693064,55.4911177119828));
#127361=CARTESIAN_POINT('Ctrl Pts',(0.934827311792556,31.9784492454175,
55.5591800794248));
#127362=CARTESIAN_POINT('Ctrl Pts',(0.938627139596119,31.9570170930322,
55.6261642436932));
#127363=CARTESIAN_POINT('Ctrl Pts',(0.942425857996128,31.9355911980109,
55.6931288511622));
#127364=CARTESIAN_POINT('Ctrl Pts',(0.946224576396138,31.9107167498486,
55.7590154025972));
#127365=CARTESIAN_POINT('Ctrl Pts',(0.950023294796147,31.8825347156863,
55.8234443555797));
#127366=CARTESIAN_POINT('Ctrl Pts',(0.953822262783287,31.8543508298802,
55.8878775417366));
#127367=CARTESIAN_POINT('Ctrl Pts',(0.957621230770428,31.8228591311617,
55.9508524814108));
#127368=CARTESIAN_POINT('Ctrl Pts',(0.961420198757568,31.7882480957827,
56.0120110228795));
#127369=CARTESIAN_POINT('Ctrl Pts',(0.96522309887351,31.7536012361879,56.0732328666089));
#127370=CARTESIAN_POINT('Ctrl Pts',(0.969025998989452,31.7158288491463,
56.1326341261334));
#127371=CARTESIAN_POINT('Ctrl Pts',(0.972828899105393,31.6751639953886,
56.1898836712275));
#127372=CARTESIAN_POINT('Ctrl Pts',(0.976634203238837,31.6344734351918,
56.2471694068352));
#127373=CARTESIAN_POINT('Ctrl Pts',(0.98043950737228,31.5908870855503,56.3023003324072));
#127374=CARTESIAN_POINT('Ctrl Pts',(0.984244811505724,31.5446779247817,
56.3549788452932));
#127375=CARTESIAN_POINT('Ctrl Pts',(0.988056246624191,31.4983943132825,
56.4077422321242));
#127376=CARTESIAN_POINT('Ctrl Pts',(0.991867681742658,31.4494798167601,
56.4580449733025));
#127377=CARTESIAN_POINT('Ctrl Pts',(0.995679116861126,31.398242918379,56.5056275448141));
#127378=CARTESIAN_POINT('Ctrl Pts',(0.996467098599645,31.3876501261609,
56.5154648360856));
#127379=CARTESIAN_POINT('Ctrl Pts',(0.997255080338164,31.3769581744616,
56.5251860055168));
#127380=CARTESIAN_POINT('Ctrl Pts',(0.998043062076684,31.3661699466928,
56.5347889885106));
#127381=CARTESIAN_POINT('Ctrl Pts',(1.00191215656167,31.3131983224499,56.5819409042527));
#127382=CARTESIAN_POINT('Ctrl Pts',(1.00578125104665,31.2576789862063,56.626439560984));
#127383=CARTESIAN_POINT('Ctrl Pts',(1.00965034553163,31.1999085753941,56.6679978936425));
#127384=CARTESIAN_POINT('Ctrl Pts',(1.0135136752563,31.1422242396501,56.7094943064311));
#127385=CARTESIAN_POINT('Ctrl Pts',(1.01737700498097,31.0822958780486,56.7480588098205));
#127386=CARTESIAN_POINT('Ctrl Pts',(1.02124033470564,31.020454584405,56.7834432998183));
#127387=CARTESIAN_POINT('Ctrl Pts',(1.02509913270775,30.9586858311878,56.8187862834724));
#127388=CARTESIAN_POINT('Ctrl Pts',(1.02895793070986,30.8950090226413,56.8509564230656));
#127389=CARTESIAN_POINT('Ctrl Pts',(1.03281672871197,30.8297842847801,56.8797488138664));
#127390=CARTESIAN_POINT('Ctrl Pts',(1.03667309590875,30.7646006344909,56.9085230672323));
#127391=CARTESIAN_POINT('Ctrl Pts',(1.04052946310553,30.6978714328268,56.9339235975645));
#127392=CARTESIAN_POINT('Ctrl Pts',(1.04438583030231,30.6299801524122,56.9557920569597));
#127393=CARTESIAN_POINT('Ctrl Pts',(1.04824105822307,30.5621089289329,56.9776540558157));
#127394=CARTESIAN_POINT('Ctrl Pts',(1.05209628614383,30.4930767704008,56.9959859064551));
#127395=CARTESIAN_POINT('Ctrl Pts',(1.05595151406459,30.4232841831565,57.0106785080638));
#127396=CARTESIAN_POINT('Ctrl Pts',(1.05980689262569,30.3534888688156,57.0253716837756));
#127397=CARTESIAN_POINT('Ctrl Pts',(1.06366227118679,30.2829335425852,57.0364252302183));
#127398=CARTESIAN_POINT('Ctrl Pts',(1.06751764974788,30.21202912545,57.0437811067873));
#127399=CARTESIAN_POINT('Ctrl Pts',(1.07137706382818,30.1410504909242,57.0511446829326));
#127400=CARTESIAN_POINT('Ctrl Pts',(1.07523647790847,30.0697225202458,57.0548028127025));
#127401=CARTESIAN_POINT('Ctrl Pts',(1.07909589198877,29.9984605839173,57.0547494233356));
#127402=CARTESIAN_POINT('Ctrl Pts',(1.08295749118116,29.9271583007081,57.0546960037409));
#127403=CARTESIAN_POINT('Ctrl Pts',(1.08681909037356,29.8559226116065,57.050926907492));
#127404=CARTESIAN_POINT('Ctrl Pts',(1.09068068956595,29.7851654522512,57.0434881158435));
#127405=CARTESIAN_POINT('Ctrl Pts',(1.09454904499834,29.7142844964256,57.0360363093119));
#127406=CARTESIAN_POINT('Ctrl Pts',(1.09841740043072,29.6438842218769,57.0249020646029));
#127407=CARTESIAN_POINT('Ctrl Pts',(1.10228575586311,29.5743673470875,57.0101826800753));
#127408=CARTESIAN_POINT('Ctrl Pts',(1.10458328154716,29.5330793092908,57.0014404213566));
#127409=CARTESIAN_POINT('Ctrl Pts',(1.1068808072312,29.4921026391673,56.991434468854));
#127410=CARTESIAN_POINT('Ctrl Pts',(1.10917833291525,29.4515187891883,56.980193405677));
#127411=CARTESIAN_POINT('Ctrl Pts',(1.11304631691874,29.3831941199109,56.9612685889262));
#127412=CARTESIAN_POINT('Ctrl Pts',(1.11691430092223,29.3157162880953,56.9387663512784));
#127413=CARTESIAN_POINT('Ctrl Pts',(1.12078228492572,29.2494870126202,56.912780128053));
#127414=CARTESIAN_POINT('Ctrl Pts',(1.1246452350137,29.1833439299984,56.8868277241122));
#127415=CARTESIAN_POINT('Ctrl Pts',(1.12850818510168,29.1184466297722,56.8574005010361));
#127416=CARTESIAN_POINT('Ctrl Pts',(1.13237113518965,29.0551830215408,56.8246420031653));
#127417=CARTESIAN_POINT('Ctrl Pts',(1.1362298569753,28.9919886602983,56.7919193620438));
#127418=CARTESIAN_POINT('Ctrl Pts',(1.14008857876095,28.9304248699874,56.7558729076272));
#127419=CARTESIAN_POINT('Ctrl Pts',(1.1439473005466,28.8708591086472,56.7166940350497));
#127420=CARTESIAN_POINT('Ctrl Pts',(1.1466682533244,28.8288566962466,56.6890673057614));
#127421=CARTESIAN_POINT('Ctrl Pts',(1.14938920610221,28.7878473654915,56.6598840725942));
#127422=CARTESIAN_POINT('Ctrl Pts',(1.15211015888001,28.7479524050421,56.6292250864936));
#127423=CARTESIAN_POINT('',(0.845925280586868,32.0547496699795,55.0011645681513));
#127424=CARTESIAN_POINT('Ctrl Pts',(0.845925280586868,32.0547496699795,
55.0011645681513));
#127425=CARTESIAN_POINT('Ctrl Pts',(0.850222060205272,32.0547045596875,
55.0807566105182));
#127426=CARTESIAN_POINT('Ctrl Pts',(0.854518839823676,32.0500307559347,
55.1601816477493));
#127427=CARTESIAN_POINT('Ctrl Pts',(0.85881561944208,32.0408108291358,55.2389324636425));
#127428=CARTESIAN_POINT('Ctrl Pts',(0.863129966126428,32.0315532073474,
55.3180052464269));
#127429=CARTESIAN_POINT('Ctrl Pts',(0.867444312810776,32.0177123505107,
55.3963980230681));
#127430=CARTESIAN_POINT('Ctrl Pts',(0.871758659495125,31.9994215971072,
55.4736146529843));
#127431=CARTESIAN_POINT('Ctrl Pts',(0.87609513814191,31.9810370148352,55.5512273928281));
#127432=CARTESIAN_POINT('Ctrl Pts',(0.880431616788695,31.9581569012951,
55.6276516357164));
#127433=CARTESIAN_POINT('Ctrl Pts',(0.88476809543548,31.9309647626119,55.7024049032084));
#127434=CARTESIAN_POINT('Ctrl Pts',(0.886206119193146,31.9219475519594,
55.7271939044633));
#127435=CARTESIAN_POINT('Ctrl Pts',(0.88764414295081,31.9124565475937,55.7517993452135));
#127436=CARTESIAN_POINT('Ctrl Pts',(0.889082166708476,31.9024995598415,
55.7762042175245));
#127437=CARTESIAN_POINT('Ctrl Pts',(0.892951368473773,31.875708907474,55.8418689011044));
#127438=CARTESIAN_POINT('Ctrl Pts',(0.89682057023907,31.8454621937363,55.9062734968565));
#127439=CARTESIAN_POINT('Ctrl Pts',(0.900689772004367,31.811899323857,55.969029619107));
#127440=CARTESIAN_POINT('Ctrl Pts',(0.904553209630516,31.7783864542268,
56.0316922504921));
#127441=CARTESIAN_POINT('Ctrl Pts',(0.908416647256666,31.7415674619314,
56.0927108582529));
#127442=CARTESIAN_POINT('Ctrl Pts',(0.912280084882815,31.7016303455885,
56.1517168616776));
#127443=CARTESIAN_POINT('Ctrl Pts',(0.916138991173326,31.6617400705553,
56.2106536583409));
#127444=CARTESIAN_POINT('Ctrl Pts',(0.919997897463837,31.618739206825,56.2675821391834));
#127445=CARTESIAN_POINT('Ctrl Pts',(0.923856803754348,31.5728608432167,
56.3221597219609));
#127446=CARTESIAN_POINT('Ctrl Pts',(0.927713279417508,31.5270113772277,
56.3767029277012));
#127447=CARTESIAN_POINT('Ctrl Pts',(0.931569755080669,31.4782883190936,
56.4288978022599));
#127448=CARTESIAN_POINT('Ctrl Pts',(0.935426230743829,31.4269662222281,
56.4784332799015));
#127449=CARTESIAN_POINT('Ctrl Pts',(0.9392815671448,31.3756592866988,56.5279541240015));
#127450=CARTESIAN_POINT('Ctrl Pts',(0.94313690354577,31.3217551860451,56.5748167937198));
#127451=CARTESIAN_POINT('Ctrl Pts',(0.946992239946741,31.2655654556863,
56.6187469350931));
#127452=CARTESIAN_POINT('Ctrl Pts',(0.950847726837816,31.2093735320045,
56.662678791246));
#127453=CARTESIAN_POINT('Ctrl Pts',(0.954703213728891,31.1508961855199,
56.7036775943421));
#127454=CARTESIAN_POINT('Ctrl Pts',(0.958558700619966,31.0904767899601,
56.7415102448904));
#127455=CARTESIAN_POINT('Ctrl Pts',(0.962418222044635,31.029994169161,56.779382485017));
#127456=CARTESIAN_POINT('Ctrl Pts',(0.966277743469305,30.9675658550251,
56.8140817004074));
#127457=CARTESIAN_POINT('Ctrl Pts',(0.970137264893974,30.9035621040846,
56.8454194879653));
#127458=CARTESIAN_POINT('Ctrl Pts',(0.973998971036238,30.8395221232323,
56.8767750145661));
#127459=CARTESIAN_POINT('Ctrl Pts',(0.977860677178502,30.7739053772985,
56.9047651348175));
#127460=CARTESIAN_POINT('Ctrl Pts',(0.981722383320766,30.7071019656674,
56.9292496916287));
#127461=CARTESIAN_POINT('Ctrl Pts',(0.985590843908987,30.6401817093007,
56.9537770739707));
#127462=CARTESIAN_POINT('Ctrl Pts',(0.98945930449721,30.5720711075993,56.9747865078759));
#127463=CARTESIAN_POINT('Ctrl Pts',(0.993327765085431,30.5031745870426,
56.9921879674003));
#127464=CARTESIAN_POINT('Ctrl Pts',(0.995624322572632,30.4622733508743,
57.0025185501341));
#127465=CARTESIAN_POINT('Ctrl Pts',(0.997920880059832,30.421095329188,57.0115785376082));
#127466=CARTESIAN_POINT('Ctrl Pts',(1.00021743754703,30.3797261264494,57.019357727445));
#127467=CARTESIAN_POINT('Ctrl Pts',(1.00411925951087,30.3094403771173,57.0325744720444));
#127468=CARTESIAN_POINT('Ctrl Pts',(1.00802108147471,30.2383249941629,57.0421433837288));
#127469=CARTESIAN_POINT('Ctrl Pts',(1.01192290343855,30.1667924843784,57.0479691964614));
#127470=CARTESIAN_POINT('Ctrl Pts',(1.01578553689087,30.0959784216706,57.0537364968038));
#127471=CARTESIAN_POINT('Ctrl Pts',(1.01964817034319,30.0247560628285,57.0558354679589));
#127472=CARTESIAN_POINT('Ctrl Pts',(1.02351080379551,29.9535368477729,57.0542246074821));
#127473=CARTESIAN_POINT('Ctrl Pts',(1.02736955523059,29.8823892093306,57.0526153659496));
#127474=CARTESIAN_POINT('Ctrl Pts',(1.03122830666567,29.8112451914293,57.0473037012904));
#127475=CARTESIAN_POINT('Ctrl Pts',(1.03508705810074,29.7405189927952,57.0383000685375));
#127476=CARTESIAN_POINT('Ctrl Pts',(1.03894322225702,29.66984021582,57.0293024726876));
#127477=CARTESIAN_POINT('Ctrl Pts',(1.04279938641329,29.5995791826385,57.016617883963));
#127478=CARTESIAN_POINT('Ctrl Pts',(1.04665555056957,29.5301459922717,57.0003086696612));
#127479=CARTESIAN_POINT('Ctrl Pts',(1.05058935174537,29.4593148878801,56.9836710982828));
#127480=CARTESIAN_POINT('Ctrl Pts',(1.05452315292117,29.3893458447176,56.9632614018325));
#127481=CARTESIAN_POINT('Ctrl Pts',(1.05845695409698,29.3206629389884,56.9392005363129));
#127482=CARTESIAN_POINT('Ctrl Pts',(1.06231322087807,29.2533337589013,56.9156139053976));
#127483=CARTESIAN_POINT('Ctrl Pts',(1.06616948765916,29.187240928555,56.8885189511515));
#127484=CARTESIAN_POINT('Ctrl Pts',(1.07002575444025,29.1227661537687,56.8580792075491));
#127485=CARTESIAN_POINT('Ctrl Pts',(1.07399832281341,29.056346876856,56.8267214282287));
#127486=CARTESIAN_POINT('Ctrl Pts',(1.07797089118657,28.9916453300971,56.7918140750785));
#127487=CARTESIAN_POINT('Ctrl Pts',(1.08194345955972,28.92905179168,56.7535870373598));
#127488=CARTESIAN_POINT('Ctrl Pts',(1.08591602793288,28.8664582532629,56.715359999641));
#127489=CARTESIAN_POINT('Ctrl Pts',(1.08988859630604,28.8059731683529,56.6738136198787));
#127490=CARTESIAN_POINT('Ctrl Pts',(1.0938611646792,28.7479524050421,56.6292250864936));
#127491=CARTESIAN_POINT('Ctrl Pts',(0.393903217269906,28.7479524050421,
56.6292250864936));
#127492=CARTESIAN_POINT('Ctrl Pts',(0.397765692980319,28.6913092315187,
56.5856952208116));
#127493=CARTESIAN_POINT('Ctrl Pts',(0.401628168690733,28.6369495977553,
56.5392162516049));
#127494=CARTESIAN_POINT('Ctrl Pts',(0.405490644401147,28.5851841620823,
56.4900650010242));
#127495=CARTESIAN_POINT('Ctrl Pts',(0.409357394093613,28.5333614459085,
56.4408593626418));
#127496=CARTESIAN_POINT('Ctrl Pts',(0.413224143786079,28.4841390070372,
56.3889758765177));
#127497=CARTESIAN_POINT('Ctrl Pts',(0.417090893478545,28.4377906583134,
56.3347282626989));
#127498=CARTESIAN_POINT('Ctrl Pts',(0.42096012610705,28.3914125481636,56.2804458151396));
#127499=CARTESIAN_POINT('Ctrl Pts',(0.424829358735555,28.3479124954103,
56.2237966025194));
#127500=CARTESIAN_POINT('Ctrl Pts',(0.42869859136406,28.3075223532751,56.1651253056374));
#127501=CARTESIAN_POINT('Ctrl Pts',(0.432574334358801,28.2670642507347,
56.1063552885007));
#127502=CARTESIAN_POINT('Ctrl Pts',(0.436450077353541,28.2297267531038,
56.0455568097575));
#127503=CARTESIAN_POINT('Ctrl Pts',(0.440325820348281,28.1956965327029,
55.9831004833686));
#127504=CARTESIAN_POINT('Ctrl Pts',(0.441730908016932,28.1833594290529,
55.9604579567208));
#127505=CARTESIAN_POINT('Ctrl Pts',(0.443135995685583,28.171456547217,55.9375977354635));
#127506=CARTESIAN_POINT('Ctrl Pts',(0.444541083354234,28.1599952039845,
55.9145380873096));
#127507=CARTESIAN_POINT('Ctrl Pts',(0.448405941216207,28.1284694397995,
55.8511098298063));
#127508=CARTESIAN_POINT('Ctrl Pts',(0.45227079907818,28.1001642080859,55.7859226688689));
#127509=CARTESIAN_POINT('Ctrl Pts',(0.456135656940153,28.0752788153013,
55.7193371418688));
#127510=CARTESIAN_POINT('Ctrl Pts',(0.459994688596713,28.0504309368096,
55.6528519913822));
#127511=CARTESIAN_POINT('Ctrl Pts',(0.463853720253272,28.0289928339176,
55.5849731111926));
#127512=CARTESIAN_POINT('Ctrl Pts',(0.467712751909832,28.0111172190746,
55.5160841464706));
#127513=CARTESIAN_POINT('Ctrl Pts',(0.471567181193553,27.9932629231145,
55.4472773403647));
#127514=CARTESIAN_POINT('Ctrl Pts',(0.475421610477274,27.9789627980082,
55.377463311472));
#127515=CARTESIAN_POINT('Ctrl Pts',(0.479276039760995,27.9683202772573,
55.3070424509678));
#127516=CARTESIAN_POINT('Ctrl Pts',(0.483127996899415,27.9576845823828,
55.2366667568388));
#127517=CARTESIAN_POINT('Ctrl Pts',(0.486979954037834,27.9507019106231,
55.1656854835747));
#127518=CARTESIAN_POINT('Ctrl Pts',(0.490831911176254,27.9474246574332,
55.0945093941715));
#127519=CARTESIAN_POINT('Ctrl Pts',(0.494682694160181,27.9441484032163,
55.0233550006808));
#127520=CARTESIAN_POINT('Ctrl Pts',(0.498533477144108,27.9445753478264,
54.9520063951509));
#127521=CARTESIAN_POINT('Ctrl Pts',(0.502384260128034,27.9487058992826,
54.8808778993558));
#127522=CARTESIAN_POINT('Ctrl Pts',(0.506235165295295,27.952836581799,54.8097471466906));
#127523=CARTESIAN_POINT('Ctrl Pts',(0.510086070462555,27.9606710740166,
54.7388370036943));
#127524=CARTESIAN_POINT('Ctrl Pts',(0.513936975629815,27.9721577784347,
54.6685584713146));
#127525=CARTESIAN_POINT('Ctrl Pts',(0.517791903410963,27.9836564817401,
54.5982065267401));
#127526=CARTESIAN_POINT('Ctrl Pts',(0.52164683119211,27.9988149342846,54.5284879914766));
#127527=CARTESIAN_POINT('Ctrl Pts',(0.525501758973257,28.0175302211821,
54.4598045366966));
#127528=CARTESIAN_POINT('Ctrl Pts',(0.529358857706701,28.0362560478348,
54.3910824019431));
#127529=CARTESIAN_POINT('Ctrl Pts',(0.533215956440145,28.0585425436682,
54.323396970801));
#127530=CARTESIAN_POINT('Ctrl Pts',(0.537073055173589,28.084237465828,54.2571329357396));
#127531=CARTESIAN_POINT('Ctrl Pts',(0.540936936527285,28.109977571923,54.1907523768821));
#127532=CARTESIAN_POINT('Ctrl Pts',(0.544800817880983,28.1391378711156,
54.1257986487736));
#127533=CARTESIAN_POINT('Ctrl Pts',(0.54866469923468,28.1715190236334,54.0626340727521));
#127534=CARTESIAN_POINT('Ctrl Pts',(0.551001917554052,28.1911060181446,
54.0244265320181));
#127535=CARTESIAN_POINT('Ctrl Pts',(0.553339135873424,28.2118706089704,
53.9868731216588));
#127536=CARTESIAN_POINT('Ctrl Pts',(0.555676354192796,28.2337610839925,
53.9500487372831));
#127537=CARTESIAN_POINT('Ctrl Pts',(0.559546127776258,28.2700055294806,
53.8890779547493));
#127538=CARTESIAN_POINT('Ctrl Pts',(0.56341590135972,28.3094816006687,53.8298669467456));
#127539=CARTESIAN_POINT('Ctrl Pts',(0.567285674943182,28.3519931974908,
53.7727790983758));
#127540=CARTESIAN_POINT('Ctrl Pts',(0.571149684492805,28.3944414732225,
53.7157762824459));
#127541=CARTESIAN_POINT('Ctrl Pts',(0.575013694042429,28.439916011926,53.6608907349997));
#127542=CARTESIAN_POINT('Ctrl Pts',(0.578877703592051,28.4881760962043,
53.6084591107654));
#127543=CARTESIAN_POINT('Ctrl Pts',(0.582737179080315,28.536379551693,53.5560890102407));
#127544=CARTESIAN_POINT('Ctrl Pts',(0.586596654568578,28.5873617328976,
53.5061674688283));
#127545=CARTESIAN_POINT('Ctrl Pts',(0.590456130056842,28.6408411942136,
53.4589987335653));
#127546=CARTESIAN_POINT('Ctrl Pts',(0.594313172906131,28.6942869472648,
53.4118597288976));
#127547=CARTESIAN_POINT('Ctrl Pts',(0.598170215755419,28.7502264941943,
53.3674704083578));
#127548=CARTESIAN_POINT('Ctrl Pts',(0.602027258604707,28.8083420642981,
53.3260976949718));
#127549=CARTESIAN_POINT('Ctrl Pts',(0.605883159311579,28.8664404252962,
53.284737232819));
#127550=CARTESIAN_POINT('Ctrl Pts',(0.609739060018451,28.926713134852,53.2463918858627));
#127551=CARTESIAN_POINT('Ctrl Pts',(0.613594960725322,28.9888112996955,
53.2112867823833));
#127552=CARTESIAN_POINT('Ctrl Pts',(0.617451008170922,29.0509118277238,
53.1761803429571));
#127553=CARTESIAN_POINT('Ctrl Pts',(0.621307055616521,29.1148375251662,
53.1443146288754));
#127554=CARTESIAN_POINT('Ctrl Pts',(0.62516310306212,29.180214135265,53.1158692459172));
#127555=CARTESIAN_POINT('Ctrl Pts',(0.629023175358348,29.2456589839147,
53.0873941723447));
#127556=CARTESIAN_POINT('Ctrl Pts',(0.632883247654576,29.3125573221994,
53.0623467506991));
#127557=CARTESIAN_POINT('Ctrl Pts',(0.636743319950804,29.3805149406725,
53.0408583961923));
#127558=CARTESIAN_POINT('Ctrl Pts',(0.640605572326229,29.4485109400305,
53.0193579055619));
#127559=CARTESIAN_POINT('Ctrl Pts',(0.644467824701654,29.5175669403351,
53.0014206057529));
#127560=CARTESIAN_POINT('Ctrl Pts',(0.648330077077079,29.5872762642552,
52.9871272567664));
#127561=CARTESIAN_POINT('Ctrl Pts',(0.652199070552378,29.657107257468,52.9728089604476));
#127562=CARTESIAN_POINT('Ctrl Pts',(0.656068064027678,29.7275933706668,
52.9621473857586));
#127563=CARTESIAN_POINT('Ctrl Pts',(0.659937057502978,29.7983211930969,
52.9551715912219));
#127564=CARTESIAN_POINT('Ctrl Pts',(0.662228580012437,29.8402117773479,
52.9510399765514));
#127565=CARTESIAN_POINT('Ctrl Pts',(0.664520102521896,29.8821871002605,
52.948200316185));
#127566=CARTESIAN_POINT('Ctrl Pts',(0.666811625031355,29.9241615682704,
52.9466500311022));
#127567=CARTESIAN_POINT('Ctrl Pts',(0.670681389893222,29.9950451492649,
52.9440320167844));
#127568=CARTESIAN_POINT('Ctrl Pts',(0.674551154755091,30.0662027119619,
52.9450836557535));
#127569=CARTESIAN_POINT('Ctrl Pts',(0.678420919616958,30.1372225844074,
52.9498371955309));
#127570=CARTESIAN_POINT('Ctrl Pts',(0.682284934848094,30.208136936736,52.9545836725799));
#127571=CARTESIAN_POINT('Ctrl Pts',(0.68614895007923,30.2789135243227,52.9630211003315));
#127572=CARTESIAN_POINT('Ctrl Pts',(0.690012965310366,30.3491389472087,
52.9751297429114));
#127573=CARTESIAN_POINT('Ctrl Pts',(0.693872468011491,30.4192823584284,
52.9872242446016));
#127574=CARTESIAN_POINT('Ctrl Pts',(0.697731970712618,30.4888754072847,
53.0029813627833));
#127575=CARTESIAN_POINT('Ctrl Pts',(0.701591473413743,30.5575098425005,
53.0223295678968));
#127576=CARTESIAN_POINT('Ctrl Pts',(0.705448556780905,30.6261012541369,
53.0416656445644));
#127577=CARTESIAN_POINT('Ctrl Pts',(0.709305640148067,30.6937347780694,
53.0645882105555));
#127578=CARTESIAN_POINT('Ctrl Pts',(0.713162723515229,30.7600138325188,
53.0909749774086));
#127579=CARTESIAN_POINT('Ctrl Pts',(0.717018678017908,30.826273488873,53.1173540215653));
#127580=CARTESIAN_POINT('Ctrl Pts',(0.720874632520587,30.8911790118523,
53.1471950742087));
#127581=CARTESIAN_POINT('Ctrl Pts',(0.724730587023266,30.9543520663278,
53.1803270359771));
#127582=CARTESIAN_POINT('Ctrl Pts',(0.728586701529236,31.0175277421768,
53.2134603725602));
#127583=CARTESIAN_POINT('Ctrl Pts',(0.732442816035207,31.0789703777892,
53.2498846619025));
#127584=CARTESIAN_POINT('Ctrl Pts',(0.736298930541177,31.1383261392231,
53.2893828121811));
#127585=CARTESIAN_POINT('Ctrl Pts',(0.74015908985444,31.1977441608976,53.3289223933887));
#127586=CARTESIAN_POINT('Ctrl Pts',(0.744019249167702,31.2550705336062,
53.3715420023265));
#127587=CARTESIAN_POINT('Ctrl Pts',(0.747879408480964,31.3099810981801,
53.4169816536404));
#127588=CARTESIAN_POINT('Ctrl Pts',(0.751741759271153,31.3649228363987,
53.4624471018035));
#127589=CARTESIAN_POINT('Ctrl Pts',(0.755604110061343,31.417445678612,53.5107354506283));
#127590=CARTESIAN_POINT('Ctrl Pts',(0.759466460851533,31.4672612714758,
53.5615487760347));
#127591=CARTESIAN_POINT('Ctrl Pts',(0.763335569848735,31.5171640299305,
53.6124510128298));
#127592=CARTESIAN_POINT('Ctrl Pts',(0.767204678845938,31.5643497598586,
53.6658866830124));
#127593=CARTESIAN_POINT('Ctrl Pts',(0.77107378784314,31.6085699004703,53.7215241739474));
#127594=CARTESIAN_POINT('Ctrl Pts',(0.773364823852066,31.6347542066076,
53.7544690962203));
#127595=CARTESIAN_POINT('Ctrl Pts',(0.77565585986099,31.6598995138589,53.7881854473603));
#127596=CARTESIAN_POINT('Ctrl Pts',(0.777946895869916,31.683961613921,53.8225999637589));
#127597=CARTESIAN_POINT('Ctrl Pts',(0.781859836390422,31.7250581161037,
53.8813777198417));
#127598=CARTESIAN_POINT('Ctrl Pts',(0.785772776910929,31.7631516630838,
53.9424211513269));
#127599=CARTESIAN_POINT('Ctrl Pts',(0.789685717431435,31.7979873888736,
54.0053950975631));
#127600=CARTESIAN_POINT('Ctrl Pts',(0.79359248258054,31.8327681371999,54.0682696588216));
#127601=CARTESIAN_POINT('Ctrl Pts',(0.797499247729644,31.8643010465251,
54.1330682768469));
#127602=CARTESIAN_POINT('Ctrl Pts',(0.801406012878749,31.892373893761,54.1994260754236));
#127603=CARTESIAN_POINT('Ctrl Pts',(0.805307063592873,31.9204056787743,
54.2656868122852));
#127604=CARTESIAN_POINT('Ctrl Pts',(0.809208114306997,31.9449872803149,
54.3335017643087));
#127605=CARTESIAN_POINT('Ctrl Pts',(0.813109165021121,31.9659527192365,
54.4024822444255));
#127606=CARTESIAN_POINT('Ctrl Pts',(0.817006828775115,31.986899955599,54.4714028344888));
#127607=CARTESIAN_POINT('Ctrl Pts',(0.820904492529109,32.0042371272175,
54.541486493878));
#127608=CARTESIAN_POINT('Ctrl Pts',(0.824802156283103,32.0178470725133,
54.6123264847203));
#127609=CARTESIAN_POINT('Ctrl Pts',(0.828698057535242,32.0314508634676,
54.6831344421129));
#127610=CARTESIAN_POINT('Ctrl Pts',(0.832593958787382,32.0413306817161,
54.7546975904148));
#127611=CARTESIAN_POINT('Ctrl Pts',(0.836489860039521,32.0474201073761,
54.8265973863746));
#127612=CARTESIAN_POINT('Ctrl Pts',(0.839635000205574,32.0523360680208,
54.8846417056654));
#127613=CARTESIAN_POINT('Ctrl Pts',(0.842780140371627,32.0547826896117,
54.9429050911716));
#127614=CARTESIAN_POINT('Ctrl Pts',(0.84592528053768,32.0547496699801,55.0011645672402));
#127615=CARTESIAN_POINT('Origin',(-1.54592528053767,-30.,55.));
#127616=CARTESIAN_POINT('',(0.904074719503239,-27.9452506260572,54.9983960106767));
#127617=CARTESIAN_POINT('Ctrl Pts',(0.452117492759457,-31.2520475724682,
56.6292251037768));
#127618=CARTESIAN_POINT('Ctrl Pts',(0.455982332793877,-31.3083856538667,
56.5859297004043));
#127619=CARTESIAN_POINT('Ctrl Pts',(0.459847172828296,-31.3625655505572,
56.5396393487449));
#127620=CARTESIAN_POINT('Ctrl Pts',(0.463712012862715,-31.4142535800857,
56.4905986628582));
#127621=CARTESIAN_POINT('Ctrl Pts',(0.46757202373732,-31.4658770248571,
56.4416192538439));
#127622=CARTESIAN_POINT('Ctrl Pts',(0.471432034611924,-31.5150144370937,
56.3898966695869));
#127623=CARTESIAN_POINT('Ctrl Pts',(0.475292045486528,-31.5613650048761,
56.3357158695053));
#127624=CARTESIAN_POINT('Ctrl Pts',(0.479149430041697,-31.607684036116,
56.2815719335914));
#127625=CARTESIAN_POINT('Ctrl Pts',(0.483006814596865,-31.6512196698572,
56.2249734679798));
#127626=CARTESIAN_POINT('Ctrl Pts',(0.486864199152033,-31.6917088085244,
56.1662413428021));
#127627=CARTESIAN_POINT('Ctrl Pts',(0.490720248234121,-31.7321839293632,
56.1075295513949));
#127628=CARTESIAN_POINT('Ctrl Pts',(0.494576297316209,-31.7696143733469,
56.0466859662144));
#127629=CARTESIAN_POINT('Ctrl Pts',(0.498432346398297,-31.8037791735835,
55.9840621197092));
#127630=CARTESIAN_POINT('Ctrl Pts',(0.502288349043991,-31.8379435623911,
55.9214390273503));
#127631=CARTESIAN_POINT('Ctrl Pts',(0.506144351689685,-31.8688421546333,
55.8570361434098));
#127632=CARTESIAN_POINT('Ctrl Pts',(0.510000354335379,-31.8962997819133,
55.7912298652196));
#127633=CARTESIAN_POINT('Ctrl Pts',(0.513860270816316,-31.9237852786321,
55.725356793784));
#127634=CARTESIAN_POINT('Ctrl Pts',(0.517720187297254,-31.9478226485702,
55.658077932748));
#127635=CARTESIAN_POINT('Ctrl Pts',(0.521580103778191,-31.9682851273012,
55.5897891319318));
#127636=CARTESIAN_POINT('Ctrl Pts',(0.525442026278597,-31.9887582404931,
55.5214648410566));
#127637=CARTESIAN_POINT('Ctrl Pts',(0.529303948779003,-32.0056526474982,
55.4521300374299));
#127638=CARTESIAN_POINT('Ctrl Pts',(0.533165871279409,-32.0188923845216,
55.3821924936739));
#127639=CARTESIAN_POINT('Ctrl Pts',(0.537034745847787,-32.0321559551542,
55.3121290513381));
#127640=CARTESIAN_POINT('Ctrl Pts',(0.540903620416166,-32.0417516498287,
55.2414611836194));
#127641=CARTESIAN_POINT('Ctrl Pts',(0.544772494984544,-32.0476552911041,
55.1706029639645));
#127642=CARTESIAN_POINT('Ctrl Pts',(0.54768232289718,-32.0520954919598,
55.1173096297538));
#127643=CARTESIAN_POINT('Ctrl Pts',(0.550592150809814,-32.0544482826237,
55.0639087483478));
#127644=CARTESIAN_POINT('Ctrl Pts',(0.55350197872245,-32.0547227845796,
55.0105754919346));
#127645=CARTESIAN_POINT('Ctrl Pts',(0.557370495353025,-32.0550877255359,
54.9396707526882));
#127646=CARTESIAN_POINT('Ctrl Pts',(0.561239011983601,-32.0517788835405,
54.8686078222902));
#127647=CARTESIAN_POINT('Ctrl Pts',(0.565107528614176,-32.0447768307097,
54.7977989241054));
#127648=CARTESIAN_POINT('Ctrl Pts',(0.568970271703778,-32.0377852280443,
54.7270957041724));
#127649=CARTESIAN_POINT('Ctrl Pts',(0.57283301479338,-32.0271114028356,
54.6566462435337));
#127650=CARTESIAN_POINT('Ctrl Pts',(0.576695757882982,-32.0127879383576,
54.5868628826867));
#127651=CARTESIAN_POINT('Ctrl Pts',(0.580553959050737,-31.9984813158116,
54.5171615750759));
#127652=CARTESIAN_POINT('Ctrl Pts',(0.584412160218493,-31.9805336752359,
54.4481252852337));
#127653=CARTESIAN_POINT('Ctrl Pts',(0.588270361386249,-31.9590292075618,
54.3801595960091));
#127654=CARTESIAN_POINT('Ctrl Pts',(0.59212612577509,-31.9375383217699,
54.3122368328403));
#127655=CARTESIAN_POINT('Ctrl Pts',(0.595981890163931,-31.9124952119648,
54.2453837909946));
#127656=CARTESIAN_POINT('Ctrl Pts',(0.599837654552772,-31.8840344392551,
54.1799928084458));
#127657=CARTESIAN_POINT('Ctrl Pts',(0.603692274588616,-31.8555821134233,
54.1146212332983));
#127658=CARTESIAN_POINT('Ctrl Pts',(0.60754689462446,-31.82371433221,54.0507113013275));
#127659=CARTESIAN_POINT('Ctrl Pts',(0.611401514660303,-31.7886138733661,
53.9886355876825));
#127660=CARTESIAN_POINT('Ctrl Pts',(0.615256281150403,-31.7535120808988,
53.9265575155035));
#127661=CARTESIAN_POINT('Ctrl Pts',(0.619111047640502,-31.7151776080581,
53.8663142219333));
#127662=CARTESIAN_POINT('Ctrl Pts',(0.622965814130601,-31.673838434473,
53.8082523514682));
#127663=CARTESIAN_POINT('Ctrl Pts',(0.62682461395004,-31.6324560067758,
53.7501297295552));
#127664=CARTESIAN_POINT('Ctrl Pts',(0.630683413769478,-31.5880628848521,
53.6941934837545));
#127665=CARTESIAN_POINT('Ctrl Pts',(0.634542213588916,-31.5409289877891,
53.640759249768));
#127666=CARTESIAN_POINT('Ctrl Pts',(0.638403196355759,-31.493768426783,
53.5872947876981));
#127667=CARTESIAN_POINT('Ctrl Pts',(0.642264179122601,-31.4438643443167,
53.5363355024071));
#127668=CARTESIAN_POINT('Ctrl Pts',(0.646125161889444,-31.3915234507503,
53.4881600453382));
#127669=CARTESIAN_POINT('Ctrl Pts',(0.649992904154239,-31.3390909229591,
53.4399002465555));
#127670=CARTESIAN_POINT('Ctrl Pts',(0.653860646419034,-31.2842134408693,
53.3944343165916));
#127671=CARTESIAN_POINT('Ctrl Pts',(0.657728388683829,-31.2272301304811,
53.352000069982));
#127672=CARTESIAN_POINT('Ctrl Pts',(0.660031342309557,-31.1933007959288,
53.3267336237211));
#127673=CARTESIAN_POINT('Ctrl Pts',(0.662334295935285,-31.1586254386636,
53.302541175617));
#127674=CARTESIAN_POINT('Ctrl Pts',(0.664637249561013,-31.1232799038679,
53.279465251712));
#127675=CARTESIAN_POINT('Ctrl Pts',(0.668506451624919,-31.063895722331,
53.240695294991));
#127676=CARTESIAN_POINT('Ctrl Pts',(0.672375653688824,-31.0023857080583,
53.2049275076779));
#127677=CARTESIAN_POINT('Ctrl Pts',(0.676244855752729,-30.9390858401043,
53.1724017543739));
#127678=CARTESIAN_POINT('Ctrl Pts',(0.68010829368058,-30.8758802730024,
53.139924456246));
#127679=CARTESIAN_POINT('Ctrl Pts',(0.683971731608431,-30.8108905735538,
53.110679825256));
#127680=CARTESIAN_POINT('Ctrl Pts',(0.687835169536282,-30.7444810120277,
53.0848640817868));
#127681=CARTESIAN_POINT('Ctrl Pts',(0.691694076131616,-30.6781493406635,
53.0590786169762));
#127682=CARTESIAN_POINT('Ctrl Pts',(0.695552982726951,-30.6104015656689,
53.0367142264377));
#127683=CARTESIAN_POINT('Ctrl Pts',(0.699411889322285,-30.5416242556622,
53.0179201004555));
#127684=CARTESIAN_POINT('Ctrl Pts',(0.70326836529203,-30.4728902667065,
52.9991378124078));
#127685=CARTESIAN_POINT('Ctrl Pts',(0.707124841261774,-30.4031284967729,
52.9839214550263));
#127686=CARTESIAN_POINT('Ctrl Pts',(0.710981317231519,-30.3327416922295,
52.972370712198));
#127687=CARTESIAN_POINT('Ctrl Pts',(0.714836653940378,-30.2623756810045,
52.9608233816326));
#127688=CARTESIAN_POINT('Ctrl Pts',(0.718691990649237,-30.1913854808174,
52.9529395944213));
#127689=CARTESIAN_POINT('Ctrl Pts',(0.722547327358096,-30.1201833739241,
52.9487678046764));
#127690=CARTESIAN_POINT('Ctrl Pts',(0.72640281455791,-30.0489784876957,
52.9445958520879));
#127691=CARTESIAN_POINT('Ctrl Pts',(0.730258301757724,-29.9775621633845,
52.944136210851));
#127692=CARTESIAN_POINT('Ctrl Pts',(0.734113788957539,-29.9063494046929,
52.9473852946793));
#127693=CARTESIAN_POINT('Ctrl Pts',(0.737973310690108,-29.8350621261825,
52.9506377784762));
#127694=CARTESIAN_POINT('Ctrl Pts',(0.741832832422678,-29.7639793247635,
52.9576067124157));
#127695=CARTESIAN_POINT('Ctrl Pts',(0.745692354155247,-29.693512692038,
52.9682364575182));
#127696=CARTESIAN_POINT('Ctrl Pts',(0.749554060605406,-29.6230061710303,
52.9788722196852));
#127697=CARTESIAN_POINT('Ctrl Pts',(0.753415767055565,-29.5531169891623,
52.9931728207905));
#127698=CARTESIAN_POINT('Ctrl Pts',(0.757277473505724,-29.4842457167119,
53.0110316539045));
#127699=CARTESIAN_POINT('Ctrl Pts',(0.761145934398485,-29.4152539827343,
53.0289217235882));
#127700=CARTESIAN_POINT('Ctrl Pts',(0.765014395291245,-29.3472841761686,
53.050382304672));
#127701=CARTESIAN_POINT('Ctrl Pts',(0.768882856184006,-29.2807201370997,
53.0752574090736));
#127702=CARTESIAN_POINT('Ctrl Pts',(0.771179410922525,-29.2412036566243,
53.0900247908485));
#127703=CARTESIAN_POINT('Ctrl Pts',(0.773475965661045,-29.2021822227904,
53.1059946464256));
#127704=CARTESIAN_POINT('Ctrl Pts',(0.775772520399564,-29.1637320466221,
53.1231266764501));
#127705=CARTESIAN_POINT('Ctrl Pts',(0.779641665008882,-29.0989527102737,
53.1519900431726));
#127706=CARTESIAN_POINT('Ctrl Pts',(0.783510809618202,-29.0355426073808,
53.1842675958906));
#127707=CARTESIAN_POINT('Ctrl Pts',(0.787379954227521,-28.973885472867,
53.2198071622134));
#127708=CARTESIAN_POINT('Ctrl Pts',(0.791243335627565,-28.9123201785415,
53.2552937912649));
#127709=CARTESIAN_POINT('Ctrl Pts',(0.79510671702761,-28.8525030870576,
53.2940325485787));
#127710=CARTESIAN_POINT('Ctrl Pts',(0.798970098427655,-28.7947966100688,
53.3358238220073));
#127711=CARTESIAN_POINT('Ctrl Pts',(0.80282895016708,-28.737157791623,53.3775660968344));
#127712=CARTESIAN_POINT('Ctrl Pts',(0.806687801906505,-28.6816250637753,
53.4223534952188));
#127713=CARTESIAN_POINT('Ctrl Pts',(0.81054665364593,-28.6285334199595,
53.4699421637298));
#127714=CARTESIAN_POINT('Ctrl Pts',(0.814403075825124,-28.5754752030164,
53.5175008700799));
#127715=CARTESIAN_POINT('Ctrl Pts',(0.818259498004319,-28.5248553817368,
53.5678570239367));
#127716=CARTESIAN_POINT('Ctrl Pts',(0.822115920183513,-28.4769761309464,
53.6207263299863));
#127717=CARTESIAN_POINT('Ctrl Pts',(0.825971204251606,-28.4291110103275,
53.6735800331944));
#127718=CARTESIAN_POINT('Ctrl Pts',(0.829826488319699,-28.3839851804013,
53.7289450562814));
#127719=CARTESIAN_POINT('Ctrl Pts',(0.833681772387792,-28.3418629470885,
53.7865013076801));
#127720=CARTESIAN_POINT('Ctrl Pts',(0.837537208182194,-28.2997390560378,
53.8440598242291));
#127721=CARTESIAN_POINT('Ctrl Pts',(0.841392643976596,-28.2606192813935,
53.9038093469996));
#127722=CARTESIAN_POINT('Ctrl Pts',(0.845248079770998,-28.224725683171,
53.9653992738707));
#127723=CARTESIAN_POINT('Ctrl Pts',(0.849107552358481,-28.1887945029378,
54.0270536878203));
#127724=CARTESIAN_POINT('Ctrl Pts',(0.852967024945965,-28.1560964873298,
54.0905519319911));
#127725=CARTESIAN_POINT('Ctrl Pts',(0.856826497533448,-28.1268081678616,
54.155517956076));
#127726=CARTESIAN_POINT('Ctrl Pts',(0.860688156040342,-28.0975032601409,
54.2205207754715));
#127727=CARTESIAN_POINT('Ctrl Pts',(0.864549814547237,-28.0716120693271,
54.2869925768243));
#127728=CARTESIAN_POINT('Ctrl Pts',(0.868411473054131,-28.0492622742321,
54.3545390114299));
#127729=CARTESIAN_POINT('Ctrl Pts',(0.87227988844316,-28.0268733729005,
54.4222036344503));
#127730=CARTESIAN_POINT('Ctrl Pts',(0.876148303832189,-28.0080383671996,
54.4909461761997));
#127731=CARTESIAN_POINT('Ctrl Pts',(0.880016719221218,-27.9928343745199,
54.5603595623795));
#127732=CARTESIAN_POINT('Ctrl Pts',(0.882313743226854,-27.9838064050144,
54.6015764944648));
#127733=CARTESIAN_POINT('Ctrl Pts',(0.884610767232489,-27.9760576942167,
54.6430297886563));
#127734=CARTESIAN_POINT('Ctrl Pts',(0.886907791238125,-27.969595720755,
54.6846335063398));
#127735=CARTESIAN_POINT('Ctrl Pts',(0.892630100646191,-27.9534977559779,
54.7882760214057));
#127736=CARTESIAN_POINT('Ctrl Pts',(0.898352410054257,-27.9453327589816,
54.8931817843288));
#127737=CARTESIAN_POINT('Ctrl Pts',(0.904074719462322,-27.9452506260578,
54.9983960099243));
#127738=CARTESIAN_POINT('Ctrl Pts',(0.904074719503241,-27.9452506260572,
54.9983960106767));
#127739=CARTESIAN_POINT('Ctrl Pts',(0.907990067110467,-27.9451944286773,
55.0703862225056));
#127740=CARTESIAN_POINT('Ctrl Pts',(0.911905414717693,-27.9489263330349,
55.1425163182313));
#127741=CARTESIAN_POINT('Ctrl Pts',(0.91582076232492,-27.956460767646,55.2143477742593));
#127742=CARTESIAN_POINT('Ctrl Pts',(0.919623060323791,-27.9637776571072,
55.2841052080584));
#127743=CARTESIAN_POINT('Ctrl Pts',(0.923425358322662,-27.9746804238571,
55.353580473897));
#127744=CARTESIAN_POINT('Ctrl Pts',(0.927227656321533,-27.9891295593209,
55.4223714399708));
#127745=CARTESIAN_POINT('Ctrl Pts',(0.931027484170776,-28.0035693079543,
55.4911177162335));
#127746=CARTESIAN_POINT('Ctrl Pts',(0.934827312020019,-28.0215507559555,
55.5591800843778));
#127747=CARTESIAN_POINT('Ctrl Pts',(0.938627139869262,-28.0429829087638,
55.6261642493064));
#127748=CARTESIAN_POINT('Ctrl Pts',(0.942425858315227,-28.0644088042096,
55.6931288574405));
#127749=CARTESIAN_POINT('Ctrl Pts',(0.946224576761191,-28.0892832528651,
55.7590154094981));
#127750=CARTESIAN_POINT('Ctrl Pts',(0.950023295207156,-28.1174652875836,
55.8234443630551));
#127751=CARTESIAN_POINT('Ctrl Pts',(0.953822263240489,-28.1456491739475,
55.8878775497905));
#127752=CARTESIAN_POINT('Ctrl Pts',(0.957621231273823,-28.1771408732871,
55.9508524899949));
#127753=CARTESIAN_POINT('Ctrl Pts',(0.961420199307156,-28.2117519093447,
56.0120110319398));
#127754=CARTESIAN_POINT('Ctrl Pts',(0.965223099469433,-28.2463987696197,
56.0732328761475));
#127755=CARTESIAN_POINT('Ctrl Pts',(0.96902599963171,-28.2841711573993,
56.1326341360962));
#127756=CARTESIAN_POINT('Ctrl Pts',(0.972828899793987,-28.3248360119472,
56.1898836815551));
#127757=CARTESIAN_POINT('Ctrl Pts',(0.976634203973915,-28.3655265729359,
56.2471694175296));
#127758=CARTESIAN_POINT('Ctrl Pts',(0.980439508153843,-28.4091129234218,
56.302300343409));
#127759=CARTESIAN_POINT('Ctrl Pts',(0.984244812333771,-28.4553220850818,
56.3549788565376));
#127760=CARTESIAN_POINT('Ctrl Pts',(0.988056247498605,-28.5016056974715,
56.407742243609));
#127761=CARTESIAN_POINT('Ctrl Pts',(0.991867682663438,-28.5505201949312,
56.4580449849629));
#127762=CARTESIAN_POINT('Ctrl Pts',(0.995679117828272,-28.601757094291,
56.5056275565804));
#127763=CARTESIAN_POINT('Ctrl Pts',(0.996467099244409,-28.6123498822488,
56.5154648437295));
#127764=CARTESIAN_POINT('Ctrl Pts',(0.997255080660547,-28.623041829606,
56.5251860091331));
#127765=CARTESIAN_POINT('Ctrl Pts',(0.998043062076684,-28.6338300529546,
56.5347889881968));
#127766=CARTESIAN_POINT('Ctrl Pts',(1.00191215654311,-28.6868016769114,
56.5819409037059));
#127767=CARTESIAN_POINT('Ctrl Pts',(1.00578125100953,-28.742321012852,56.6264395602405));
#127768=CARTESIAN_POINT('Ctrl Pts',(1.00965034547595,-28.8000914233495,
56.6679978927386));
#127769=CARTESIAN_POINT('Ctrl Pts',(1.01351367518186,-28.8577757587759,
56.7094943053647));
#127770=CARTESIAN_POINT('Ctrl Pts',(1.01737700488776,-28.9177041200476,
56.748058808628));
#127771=CARTESIAN_POINT('Ctrl Pts',(1.02124033459367,-28.979545413354,56.783443298536));
#127772=CARTESIAN_POINT('Ctrl Pts',(1.02509913257681,-29.0413141662306,
56.8187862820983));
#127773=CARTESIAN_POINT('Ctrl Pts',(1.02895793055994,-29.1049909744289,
56.8509564216362));
#127774=CARTESIAN_POINT('Ctrl Pts',(1.03281672854308,-29.1702157119384,
56.8797488124178));
#127775=CARTESIAN_POINT('Ctrl Pts',(1.03667309572076,-29.235399361874,56.9085230657636));
#127776=CARTESIAN_POINT('Ctrl Pts',(1.04052946289844,-29.3021285631809,
56.9339235961119));
#127777=CARTESIAN_POINT('Ctrl Pts',(1.04438583007612,-29.3700198432387,
56.9557920555588));
#127778=CARTESIAN_POINT('Ctrl Pts',(1.04824105797769,-29.4378910663595,
56.977654054466));
#127779=CARTESIAN_POINT('Ctrl Pts',(1.05209628587926,-29.5069232245335,
56.9959859051922));
#127780=CARTESIAN_POINT('Ctrl Pts',(1.05595151378083,-29.5767158114237,
57.0106785069228));
#127781=CARTESIAN_POINT('Ctrl Pts',(1.05980689232267,-29.6465111254094,
57.0253716827563));
#127782=CARTESIAN_POINT('Ctrl Pts',(1.06366227086452,-29.7170664512887,
57.0364252293559));
#127783=CARTESIAN_POINT('Ctrl Pts',(1.06751764940637,-29.7879708680803,
57.0437811061162));
#127784=CARTESIAN_POINT('Ctrl Pts',(1.07137706346744,-29.858949502263,57.051144682453));
#127785=CARTESIAN_POINT('Ctrl Pts',(1.07523647752851,-29.9302774726059,
57.0548028124487));
#127786=CARTESIAN_POINT('Ctrl Pts',(1.07909589158959,-30.0015394086098,
57.0547494233412));
#127787=CARTESIAN_POINT('Ctrl Pts',(1.08295749076274,-30.072841691494,57.054696004006));
#127788=CARTESIAN_POINT('Ctrl Pts',(1.0868190899359,-30.1440773802816,57.0509269080504));
#127789=CARTESIAN_POINT('Ctrl Pts',(1.09068068910905,-30.214834539337,57.0434881167278));
#127790=CARTESIAN_POINT('Ctrl Pts',(1.0945490445224,-30.2857154948666,57.0360363105224));
#127791=CARTESIAN_POINT('Ctrl Pts',(1.09841739993575,-30.3561157691335,
57.024902066172));
#127792=CARTESIAN_POINT('Ctrl Pts',(1.1022857553491,-30.4256326436585,57.0101826820347));
#127793=CARTESIAN_POINT('Ctrl Pts',(1.10458328120448,-30.4669206845804,
57.0014404228529));
#127794=CARTESIAN_POINT('Ctrl Pts',(1.10688080705986,-30.5078973577857,
56.9914344696973));
#127795=CARTESIAN_POINT('Ctrl Pts',(1.10917833291525,-30.5484812107845,
56.9801934056845));
#127796=CARTESIAN_POINT('Ctrl Pts',(1.1130463169165,-30.6168058800112,56.9612685889488));
#127797=CARTESIAN_POINT('Ctrl Pts',(1.11691430091776,-30.6842837117802,
56.9387663513206));
#127798=CARTESIAN_POINT('Ctrl Pts',(1.12078228491901,-30.750512987213,56.9127801281184));
#127799=CARTESIAN_POINT('Ctrl Pts',(1.12464523500466,-30.8166560697911,
56.8868277242015));
#127800=CARTESIAN_POINT('Ctrl Pts',(1.12850818509031,-30.881553369978,56.857400501153));
#127801=CARTESIAN_POINT('Ctrl Pts',(1.13237113517596,-30.9448169781747,
56.8246420033126));
#127802=CARTESIAN_POINT('Ctrl Pts',(1.13622985695909,-31.0080113393794,
56.7919193622232));
#127803=CARTESIAN_POINT('Ctrl Pts',(1.14008857874222,-31.0695751296572,
56.7558729078419));
#127804=CARTESIAN_POINT('Ctrl Pts',(1.14394730052535,-31.1291408909691,
56.716694035302));
#127805=CARTESIAN_POINT('Ctrl Pts',(1.1466682528,-31.1711432956104,56.6890673111309));
#127806=CARTESIAN_POINT('Ctrl Pts',(1.14938920507465,-31.2121526189746,
56.659884083656));
#127807=CARTESIAN_POINT('Ctrl Pts',(1.15211015734929,-31.2520475724682,
56.6292251037768));
#127808=CARTESIAN_POINT('',(0.845925280586865,-27.9452503300222,55.0011645711683));
#127809=CARTESIAN_POINT('Ctrl Pts',(0.845925280586864,-27.9452503300222,
55.0011645711683));
#127810=CARTESIAN_POINT('Ctrl Pts',(0.850222060722874,-27.945295440436,
55.0807566222002));
#127811=CARTESIAN_POINT('Ctrl Pts',(0.854518840858883,-27.9499692453172,
55.1601816680743));
#127812=CARTESIAN_POINT('Ctrl Pts',(0.858815620994894,-27.9591891742394,
55.2389324924709));
#127813=CARTESIAN_POINT('Ctrl Pts',(0.863129968211751,-27.9684467981871,
55.3180052840278));
#127814=CARTESIAN_POINT('Ctrl Pts',(0.867444315428608,-27.9822876582133,
55.3963980692969));
#127815=CARTESIAN_POINT('Ctrl Pts',(0.871758662645465,-28.0005784158235,
55.4736147075728));
#127816=CARTESIAN_POINT('Ctrl Pts',(0.87609514182901,-28.0189630023301,
55.5512274558463));
#127817=CARTESIAN_POINT('Ctrl Pts',(0.880431621012555,-28.0418431211359,
55.6276517068927));
#127818=CARTESIAN_POINT('Ctrl Pts',(0.8847681001961,-28.0690352661005,55.702404982141));
#127819=CARTESIAN_POINT('Ctrl Pts',(0.886206122366891,-28.0780524677693,
55.7271939555446));
#127820=CARTESIAN_POINT('Ctrl Pts',(0.887644144537682,-28.0875434620998,
55.7517993688499));
#127821=CARTESIAN_POINT('Ctrl Pts',(0.889082166708474,-28.0975004387939,
55.77620421418));
#127822=CARTESIAN_POINT('Ctrl Pts',(0.892951368337054,-28.1242910900254,
55.8418688953053));
#127823=CARTESIAN_POINT('Ctrl Pts',(0.896820569965634,-28.1545378023993,
55.9062734887861));
#127824=CARTESIAN_POINT('Ctrl Pts',(0.900689771594214,-28.1881006707189,
55.969029608965));
#127825=CARTESIAN_POINT('Ctrl Pts',(0.90455320908223,-28.2216135387777,
56.0316922382554));
#127826=CARTESIAN_POINT('Ctrl Pts',(0.908416646570245,-28.2584325293038,
56.0927108441219));
#127827=CARTESIAN_POINT('Ctrl Pts',(0.912280084058261,-28.2983696437099,
56.1517168458662));
#127828=CARTESIAN_POINT('Ctrl Pts',(0.916138990209208,-28.3382599167921,
56.2106536408268));
#127829=CARTESIAN_POINT('Ctrl Pts',(0.919997896360154,-28.3812607784018,
56.2675821201815));
#127830=CARTESIAN_POINT('Ctrl Pts',(0.923856802511101,-28.4271391397493,
56.3221597016969));
#127831=CARTESIAN_POINT('Ctrl Pts',(0.927713278033892,-28.4729886034681,
56.3767029061633));
#127832=CARTESIAN_POINT('Ctrl Pts',(0.931569753556685,-28.5217116591905,
56.4288977796746));
#127833=CARTESIAN_POINT('Ctrl Pts',(0.935426229079476,-28.5730337535307,
56.4784332565041));
#127834=CARTESIAN_POINT('Ctrl Pts',(0.939281565339479,-28.6243406865268,
56.5279540997841));
#127835=CARTESIAN_POINT('Ctrl Pts',(0.943136901599481,-28.6782447845327,
56.5748167689184));
#127836=CARTESIAN_POINT('Ctrl Pts',(0.946992237859484,-28.7344345121555,
56.6187469099513));
#127837=CARTESIAN_POINT('Ctrl Pts',(0.950847724609213,-28.7906264330959,
56.6626787657594));
#127838=CARTESIAN_POINT('Ctrl Pts',(0.954703211358941,-28.8491037767504,
56.703677568755));
#127839=CARTESIAN_POINT('Ctrl Pts',(0.958558698108669,-28.9095231694168,
56.7415102194536));
#127840=CARTESIAN_POINT('Ctrl Pts',(0.962418219392364,-28.9700057873276,
56.7793824597356));
#127841=CARTESIAN_POINT('Ctrl Pts',(0.96627774067606,-29.0324340985123,
56.8140816755319));
#127842=CARTESIAN_POINT('Ctrl Pts',(0.970137261959756,-29.0964378464631,
56.8454194637523));
#127843=CARTESIAN_POINT('Ctrl Pts',(0.97399896796105,-29.1604778243254,
56.8767749910166));
#127844=CARTESIAN_POINT('Ctrl Pts',(0.977860673962344,-29.2260945672309,
56.9047651121883));
#127845=CARTESIAN_POINT('Ctrl Pts',(0.981722379963638,-29.2928979758192,
56.9292496701825));
#127846=CARTESIAN_POINT('Ctrl Pts',(0.985590840412425,-29.3598182291688,
56.9537770537211));
#127847=CARTESIAN_POINT('Ctrl Pts',(0.989459300861211,-29.4279288278397,
56.9747864890832));
#127848=CARTESIAN_POINT('Ctrl Pts',(0.993327761309998,-29.4968253453767,
56.9921879503312));
#127849=CARTESIAN_POINT('Ctrl Pts',(0.995624320055678,-29.5377266036399,
57.0025185401216));
#127850=CARTESIAN_POINT('Ctrl Pts',(0.997920878801357,-29.5789046477481,
57.0115785332614));
#127851=CARTESIAN_POINT('Ctrl Pts',(1.00021743754704,-29.620273873091,57.0193577273585));
#127852=CARTESIAN_POINT('Ctrl Pts',(1.00411925944499,-29.6905596211249,
57.0325744717304));
#127853=CARTESIAN_POINT('Ctrl Pts',(1.00802108134294,-29.7616750027816,
57.0421433833276));
#127854=CARTESIAN_POINT('Ctrl Pts',(1.01192290324089,-29.8332075112887,
57.0479691961085));
#127855=CARTESIAN_POINT('Ctrl Pts',(1.01578553666388,-29.90402157339,57.0537364965524));
#127856=CARTESIAN_POINT('Ctrl Pts',(1.01964817008687,-29.9752439316532,
57.0558354678734));
#127857=CARTESIAN_POINT('Ctrl Pts',(1.02351080350986,-30.0464631461639,
57.0542246076193));
#127858=CARTESIAN_POINT('Ctrl Pts',(1.02736955491481,-30.1176107840465,
57.0526153663095));
#127859=CARTESIAN_POINT('Ctrl Pts',(1.03122830631976,-30.1887548014223,
57.0473037019312));
#127860=CARTESIAN_POINT('Ctrl Pts',(1.03508705772471,-30.2594809995703,
57.0383000695094));
#127861=CARTESIAN_POINT('Ctrl Pts',(1.03894322185011,-30.3301597760455,
57.0293024739922));
#127862=CARTESIAN_POINT('Ctrl Pts',(1.0427993859755,-30.4004208087665,57.0166178856518));
#127863=CARTESIAN_POINT('Ctrl Pts',(1.04665555010089,-30.4698539987165,
57.000308671778));
#127864=CARTESIAN_POINT('Ctrl Pts',(1.05058935118398,-30.5406851015808,
56.9836711010951));
#127865=CARTESIAN_POINT('Ctrl Pts',(1.05452315226706,-30.6106541432883,
56.9632614055032));
#127866=CARTESIAN_POINT('Ctrl Pts',(1.05845695335014,-30.6793370476578,
56.9392005409909));
#127867=CARTESIAN_POINT('Ctrl Pts',(1.06231322009866,-30.7466662274301,
56.9156139107065));
#127868=CARTESIAN_POINT('Ctrl Pts',(1.06616948684717,-30.8127590575158,
56.8885189571279));
#127869=CARTESIAN_POINT('Ctrl Pts',(1.07002575359569,-30.8772338320979,
56.8580792142217));
#127870=CARTESIAN_POINT('Ctrl Pts',(1.07399832184605,-30.9436531073082,
56.8267214363229));
#127871=CARTESIAN_POINT('Ctrl Pts',(1.07797089009642,-31.0083546525018,
56.7918140847842));
#127872=CARTESIAN_POINT('Ctrl Pts',(1.08194345834679,-31.0709481895177,
56.7535870488427));
#127873=CARTESIAN_POINT('Ctrl Pts',(1.08591602659716,-31.1335417265337,
56.7153600129011));
#127874=CARTESIAN_POINT('Ctrl Pts',(1.08988859484753,-31.1940268102068,
56.6738136350815));
#127875=CARTESIAN_POINT('Ctrl Pts',(1.09386116309789,-31.2520475724682,
56.6292251037768));
#127876=CARTESIAN_POINT('Ctrl Pts',(0.393903215690563,-31.2520475724682,
56.6292251037768));
#127877=CARTESIAN_POINT('Ctrl Pts',(0.39776569061235,-31.3086907373524,
56.5856952459777));
#127878=CARTESIAN_POINT('Ctrl Pts',(0.401628165534137,-31.3630503634527,
56.5392162854362));
#127879=CARTESIAN_POINT('Ctrl Pts',(0.405490640455925,-31.4148157924792,
56.490065044168));
#127880=CARTESIAN_POINT('Ctrl Pts',(0.409357389344096,-31.4666385018009,
56.4408594152967));
#127881=CARTESIAN_POINT('Ctrl Pts',(0.413224138232267,-31.5158609348587,
56.3889759393529));
#127882=CARTESIAN_POINT('Ctrl Pts',(0.417090887120438,-31.5622092788417,
56.3347283362546));
#127883=CARTESIAN_POINT('Ctrl Pts',(0.420960118935074,-31.6085873841392,
56.2804458995498));
#127884=CARTESIAN_POINT('Ctrl Pts',(0.424829350749709,-31.6520874331276,
56.2237966983362));
#127885=CARTESIAN_POINT('Ctrl Pts',(0.428698582564345,-31.6924775726151,
56.1651254132904));
#127886=CARTESIAN_POINT('Ctrl Pts',(0.432574324736315,-31.7329356724247,
56.106355408124));
#127887=CARTESIAN_POINT('Ctrl Pts',(0.436450066908286,-31.7702731684576,
56.0455569417902));
#127888=CARTESIAN_POINT('Ctrl Pts',(0.440325809080256,-31.8043033884208,
55.9831006281319));
#127889=CARTESIAN_POINT('Ctrl Pts',(0.441730900504915,-31.81664052751,55.9604580407659));
#127890=CARTESIAN_POINT('Ctrl Pts',(0.443135991929574,-31.8285434424312,
55.9375977575761));
#127891=CARTESIAN_POINT('Ctrl Pts',(0.444541083354233,-31.8400048163345,
55.9145380464287));
#127892=CARTESIAN_POINT('Ctrl Pts',(0.44840594300457,-31.8715305951977,
55.851109755858));
#127893=CARTESIAN_POINT('Ctrl Pts',(0.452270802654908,-31.8998358376757,
55.7859225613206));
#127894=CARTESIAN_POINT('Ctrl Pts',(0.456135662305245,-31.9247212374688,
55.7193370006726));
#127895=CARTESIAN_POINT('Ctrl Pts',(0.459994695776998,-31.9495691231484,
55.6528518160803));
#127896=CARTESIAN_POINT('Ctrl Pts',(0.463853729248751,-31.9710072294324,
55.5849729017156));
#127897=CARTESIAN_POINT('Ctrl Pts',(0.467712762720505,-31.9888828440538,
55.5160839031867));
#127898=CARTESIAN_POINT('Ctrl Pts',(0.471567193850847,-32.0067371399481,
55.4472770627144));
#127899=CARTESIAN_POINT('Ctrl Pts',(0.47542162498119,-32.0210372613224,
55.3774629998046));
#127900=CARTESIAN_POINT('Ctrl Pts',(0.479276056111532,-32.0316797748725,
55.3070421060282));
#127901=CARTESIAN_POINT('Ctrl Pts',(0.483128015115094,-32.0423154626052,
55.2366663782884));
#127902=CARTESIAN_POINT('Ctrl Pts',(0.486979974118655,-32.0492981237219,
55.1656850721509));
#127903=CARTESIAN_POINT('Ctrl Pts',(0.490831933122217,-32.0525753629738,
55.0945089509679));
#127904=CARTESIAN_POINT('Ctrl Pts',(0.494682717987179,-32.0558516032708,
55.0233545254029));
#127905=CARTESIAN_POINT('Ctrl Pts',(0.498533502852141,-32.0554246414167,
54.9520058888896));
#127906=CARTESIAN_POINT('Ctrl Pts',(0.502384287717103,-32.0512940696008,
54.8808773635249));
#127907=CARTESIAN_POINT('Ctrl Pts',(0.506235194778705,-32.0471633667097,
54.8097465810445));
#127908=CARTESIAN_POINT('Ctrl Pts',(0.510086101840306,-32.0393288509765,
54.7388364096479));
#127909=CARTESIAN_POINT('Ctrl Pts',(0.513937008901907,-32.0278421201088,
54.6685578505792));
#127910=CARTESIAN_POINT('Ctrl Pts',(0.517791938585007,-32.0163433903094,
54.5982058791851));
#127911=CARTESIAN_POINT('Ctrl Pts',(0.521646868268107,-32.0011849083202,
54.5284873188182));
#127912=CARTESIAN_POINT('Ctrl Pts',(0.525501797951207,-31.9824695892304,
54.4598038409277));
#127913=CARTESIAN_POINT('Ctrl Pts',(0.529358898593875,-31.9637437303373,
54.3910816829403));
#127914=CARTESIAN_POINT('Ctrl Pts',(0.533215999236543,-31.9414571995012,
54.3233962305621));
#127915=CARTESIAN_POINT('Ctrl Pts',(0.537073099879211,-31.9157622397753,
54.2571321765271));
#127916=CARTESIAN_POINT('Ctrl Pts',(0.540936983133111,-31.8900220961305,
54.1907515988753));
#127917=CARTESIAN_POINT('Ctrl Pts',(0.544800866387012,-31.8608617568373,
54.1257978542333));
#127918=CARTESIAN_POINT('Ctrl Pts',(0.548664749640912,-31.8284805618616,
54.0626332641948));
#127919=CARTESIAN_POINT('Ctrl Pts',(0.551001951158207,-31.8088936921102,
54.0244260084429));
#127920=CARTESIAN_POINT('Ctrl Pts',(0.553339152675502,-31.7881292432781,
53.9868728739325));
#127921=CARTESIAN_POINT('Ctrl Pts',(0.555676354192796,-31.7662389263135,
53.95004875462));
#127922=CARTESIAN_POINT('Ctrl Pts',(0.559546127041688,-31.7299944888457,
53.8890779842155));
#127923=CARTESIAN_POINT('Ctrl Pts',(0.56341589989058,-31.6905184267416,
53.8298669871839));
#127924=CARTESIAN_POINT('Ctrl Pts',(0.567285672739472,-31.6480068398848,
53.7727791485666));
#127925=CARTESIAN_POINT('Ctrl Pts',(0.571149681546897,-31.6055585741993,
53.7157763425034));
#127926=CARTESIAN_POINT('Ctrl Pts',(0.575013690354322,-31.5600840464339,
53.6608908036987));
#127927=CARTESIAN_POINT('Ctrl Pts',(0.578877699161747,-31.5118239738126,
53.6084591868344));
#127928=CARTESIAN_POINT('Ctrl Pts',(0.582737173900105,-31.4636205300742,
53.5560890937875));
#127929=CARTESIAN_POINT('Ctrl Pts',(0.586596648638463,-31.4126383613493,
53.5061675585738));
#127930=CARTESIAN_POINT('Ctrl Pts',(0.590456123376821,-31.3591589130782,
53.4589988281964));
#127931=CARTESIAN_POINT('Ctrl Pts',(0.594313165471867,-31.3057131731303,
53.4118598284699));
#127932=CARTESIAN_POINT('Ctrl Pts',(0.598170207566914,-31.249773639875,
53.3674705115531));
#127933=CARTESIAN_POINT('Ctrl Pts',(0.60202724966196,-31.1916580838614,
53.3260978004472));
#127934=CARTESIAN_POINT('Ctrl Pts',(0.605883149611384,-31.1335597370009,
53.2847373406104));
#127935=CARTESIAN_POINT('Ctrl Pts',(0.609739049560808,-31.0732870420026,
53.2463919946229));
#127936=CARTESIAN_POINT('Ctrl Pts',(0.613594949510231,-31.0111888919898,
53.2112868907462));
#127937=CARTESIAN_POINT('Ctrl Pts',(0.617450996196304,-30.9490883788258,
53.1761804509413));
#127938=CARTESIAN_POINT('Ctrl Pts',(0.621307042882376,-30.885162696523,
53.1443147351114));
#127939=CARTESIAN_POINT('Ctrl Pts',(0.625163089568449,-30.819786101699,
53.1158693490203));
#127940=CARTESIAN_POINT('Ctrl Pts',(0.62902316110723,-30.7543412682912,
53.0873942722905));
#127941=CARTESIAN_POINT('Ctrl Pts',(0.632883232646012,-30.687442945382,
53.0623468461053));
#127942=CARTESIAN_POINT('Ctrl Pts',(0.636743304184793,-30.6194853422827,
53.0408584856635));
#127943=CARTESIAN_POINT('Ctrl Pts',(0.640605555802807,-30.551489358299,
53.019357989092));
#127944=CARTESIAN_POINT('Ctrl Pts',(0.644467807420821,-30.4824333733671,
53.0014206819458));
#127945=CARTESIAN_POINT('Ctrl Pts',(0.648330059038836,-30.4127240646842,
52.9871273242128));
#127946=CARTESIAN_POINT('Ctrl Pts',(0.652199051765006,-30.342893086562,
52.9728090190969));
#127947=CARTESIAN_POINT('Ctrl Pts',(0.656068044491176,-30.2724069883148,
52.9621474342147));
#127948=CARTESIAN_POINT('Ctrl Pts',(0.659937037217347,-30.2016791805648,
52.9551716280757));
#127949=CARTESIAN_POINT('Ctrl Pts',(0.662228566488683,-30.1597884732859,
52.9510399935418));
#127950=CARTESIAN_POINT('Ctrl Pts',(0.664520095760019,-30.1178130267174,
52.9482003209458));
#127951=CARTESIAN_POINT('Ctrl Pts',(0.666811625031356,-30.0758384352019,
52.9466500312304));
#127952=CARTESIAN_POINT('Ctrl Pts',(0.670681389707337,-30.0049548582094,
52.9440320169404));
#127953=CARTESIAN_POINT('Ctrl Pts',(0.674551154383317,-29.933797299356,
52.9450836555165));
#127954=CARTESIAN_POINT('Ctrl Pts',(0.678420919059298,-29.8627774305534,
52.9498371945296));
#127955=CARTESIAN_POINT('Ctrl Pts',(0.682284934099417,-29.7918630819617,
52.9545836708086));
#127956=CARTESIAN_POINT('Ctrl Pts',(0.686148949139536,-29.7210864979116,
52.9630210974097));
#127957=CARTESIAN_POINT('Ctrl Pts',(0.690012964179655,-29.6508610783276,
52.9751297385083));
#127958=CARTESIAN_POINT('Ctrl Pts',(0.693872466683003,-29.5807176705331,
52.9872242386971));
#127959=CARTESIAN_POINT('Ctrl Pts',(0.697731969186351,-29.5111246248659,
53.002981355034));
#127960=CARTESIAN_POINT('Ctrl Pts',(0.701591471689699,-29.4424901925755,
53.0223295580088));
#127961=CARTESIAN_POINT('Ctrl Pts',(0.705448554854998,-29.3738987839373,
53.041665632518));
#127962=CARTESIAN_POINT('Ctrl Pts',(0.709305638020299,-29.3062652627375,
53.0645881960493));
#127963=CARTESIAN_POINT('Ctrl Pts',(0.713162721185598,-29.2399862107333,
53.0909749601892));
#127964=CARTESIAN_POINT('Ctrl Pts',(0.717018675482635,-29.1737265568896,
53.1173540016073));
#127965=CARTESIAN_POINT('Ctrl Pts',(0.720874629779671,-29.1088210361309,
53.1471950512521));
#127966=CARTESIAN_POINT('Ctrl Pts',(0.724730584076708,-29.0456479835695,
53.1803270098078));
#127967=CARTESIAN_POINT('Ctrl Pts',(0.728586698373548,-28.9824723096917,
53.2134603431483));
#127968=CARTESIAN_POINT('Ctrl Pts',(0.732442812670388,-28.9210296757409,
53.249884629028));
#127969=CARTESIAN_POINT('Ctrl Pts',(0.736298926967228,-28.8616739156467,
53.2893827756681));
#127970=CARTESIAN_POINT('Ctrl Pts',(0.74015908606738,-28.8022558953714,
53.3289223531948));
#127971=CARTESIAN_POINT('Ctrl Pts',(0.744019245167533,-28.7449295237354,
53.3715419582693));
#127972=CARTESIAN_POINT('Ctrl Pts',(0.747879404267685,-28.6900189598985,
53.4169816055792));
#127973=CARTESIAN_POINT('Ctrl Pts',(0.751741754842204,-28.635077222452,
53.4624470497072));
#127974=CARTESIAN_POINT('Ctrl Pts',(0.755604105416722,-28.5825543806718,
53.5107353943525));
#127975=CARTESIAN_POINT('Ctrl Pts',(0.759466455991241,-28.5327387878957,
53.5615487154741));
#127976=CARTESIAN_POINT('Ctrl Pts',(0.763335564771012,-28.4828360295466,
53.6124509479586));
#127977=CARTESIAN_POINT('Ctrl Pts',(0.767204673550783,-28.4356502993757,
53.6658866137231));
#127978=CARTESIAN_POINT('Ctrl Pts',(0.771073782330553,-28.3914301581678,
53.7215241001693));
#127979=CARTESIAN_POINT('Ctrl Pts',(0.773364820177007,-28.3652458292049,
53.7544690480591));
#127980=CARTESIAN_POINT('Ctrl Pts',(0.775655858023461,-28.3401005007883,
53.7881854261158));
#127981=CARTESIAN_POINT('Ctrl Pts',(0.777946895869916,-28.316038381332,
53.8225999705482));
#127982=CARTESIAN_POINT('Ctrl Pts',(0.781859836728712,-28.2749418754339,
53.8813777324496));
#127983=CARTESIAN_POINT('Ctrl Pts',(0.785772777587509,-28.2368483254715,
53.9424211699665));
#127984=CARTESIAN_POINT('Ctrl Pts',(0.789685718446306,-28.2020125974159,
54.0053951223482));
#127985=CARTESIAN_POINT('Ctrl Pts',(0.793592483939231,-28.1672318467734,
54.0682696898399));
#127986=CARTESIAN_POINT('Ctrl Pts',(0.797499249432156,-28.1356989358561,
54.1330683142181));
#127987=CARTESIAN_POINT('Ctrl Pts',(0.801406014925082,-28.1076260877293,
54.1994261191761));
#127988=CARTESIAN_POINT('Ctrl Pts',(0.805307065989411,-28.079594301777,
54.2656868625268));
#127989=CARTESIAN_POINT('Ctrl Pts',(0.80920811705374,-28.0550127000085,
54.3335018210736));
#127990=CARTESIAN_POINT('Ctrl Pts',(0.813109168118069,-28.0340472615431,
54.4024823076646));
#127991=CARTESIAN_POINT('Ctrl Pts',(0.817006832225679,-28.0131000256163,
54.4714029042622));
#127992=CARTESIAN_POINT('Ctrl Pts',(0.82090449633329,-27.9957628551231,
54.5414865701392));
#127993=CARTESIAN_POINT('Ctrl Pts',(0.8248021604409,-27.9821529116122,54.6123265673472));
#127994=CARTESIAN_POINT('Ctrl Pts',(0.828698062049659,-27.9685491224309,
54.6831345311603));
#127995=CARTESIAN_POINT('Ctrl Pts',(0.832593963658419,-27.9586693066202,
54.7546976857619));
#127996=CARTESIAN_POINT('Ctrl Pts',(0.836489865267178,-27.9525798840312,
54.8265974878318));
#127997=CARTESIAN_POINT('Ctrl Pts',(0.839635003690678,-27.9476639290393,
54.8846417745827));
#127998=CARTESIAN_POINT('Ctrl Pts',(0.842780142114177,-27.9452173103231,
54.9429051271427));
#127999=CARTESIAN_POINT('Ctrl Pts',(0.845925280537677,-27.9452503300217,
55.0011645702572));
#128000=CARTESIAN_POINT('Origin',(80.,-9.,134.));
#128001=CARTESIAN_POINT('',(78.3340002645784,-8.99906107773531,138.679802703723));
#128002=CARTESIAN_POINT('Ctrl Pts',(78.4365593749993,-8.42449203993574,
139.340802385574));
#128003=CARTESIAN_POINT('Ctrl Pts',(78.4404068256367,-8.41403995056995,
139.340073131));
#128004=CARTESIAN_POINT('Ctrl Pts',(78.4443588637281,-8.40362705661283,
139.339338587103));
#128005=CARTESIAN_POINT('Ctrl Pts',(78.450721004147,-8.38735761703001,139.338177103129));
#128006=CARTESIAN_POINT('Ctrl Pts',(78.4530606904758,-8.38147363376576,
139.337754185242));
#128007=CARTESIAN_POINT('Ctrl Pts',(78.4572880769896,-8.37101637513597,
139.336997211539));
#128008=CARTESIAN_POINT('Ctrl Pts',(78.4591626864472,-8.3664379679219,139.336663938979));
#128009=CARTESIAN_POINT('Ctrl Pts',(78.4637554384923,-8.35536191966457,
139.335853231315));
#128010=CARTESIAN_POINT('Ctrl Pts',(78.4664944016446,-8.34887314395052,
139.335374571223));
#128011=CARTESIAN_POINT('Ctrl Pts',(78.4751941165289,-8.32862235513383,
139.333869501142));
#128012=CARTESIAN_POINT('Ctrl Pts',(78.4812994162062,-8.3149237838157,139.332835100129));
#128013=CARTESIAN_POINT('Ctrl Pts',(78.5143713886673,-8.24333489887553,
139.327350021681));
#128014=CARTESIAN_POINT('Ctrl Pts',(78.5444630974817,-8.1869531698572,139.322756877021));
#128015=CARTESIAN_POINT('Ctrl Pts',(78.6346517897326,-8.03909622286664,
139.310189682049));
#128016=CARTESIAN_POINT('Ctrl Pts',(78.7006497236031,-7.95157005770015,
139.302185330614));
#128017=CARTESIAN_POINT('Ctrl Pts',(78.8088854917817,-7.83409277274342,
139.290895045155));
#128018=CARTESIAN_POINT('Ctrl Pts',(78.8446829265701,-7.79861046733643,
139.287394266339));
#128019=CARTESIAN_POINT('Ctrl Pts',(78.8941308511983,-7.75385574502929,
139.282852431406));
#128020=CARTESIAN_POINT('Ctrl Pts',(78.9063852206201,-7.74308758234494,
139.281749041542));
#128021=CARTESIAN_POINT('Ctrl Pts',(78.9267516322524,-7.72571459899383,
139.279950590039));
#128022=CARTESIAN_POINT('Ctrl Pts',(78.9347709786541,-7.71900332444436,
139.279251179898));
#128023=CARTESIAN_POINT('Ctrl Pts',(78.9505043452793,-7.7060862197635,139.277895611099));
#128024=CARTESIAN_POINT('Ctrl Pts',(78.9582115228496,-7.69987278467009,
139.277239162322));
#128025=CARTESIAN_POINT('Ctrl Pts',(78.9765383417246,-7.68536553366061,
139.275695685906));
#128026=CARTESIAN_POINT('Ctrl Pts',(78.9872042244231,-7.6771310417617,139.274811034834));
#128027=CARTESIAN_POINT('Ctrl Pts',(79.0235620733276,-7.64975882722003,
139.271839678635));
#128028=CARTESIAN_POINT('Ctrl Pts',(79.0497066872027,-7.63123227537913,
139.269776519917));
#128029=CARTESIAN_POINT('Ctrl Pts',(79.1149223844842,-7.58778919564296,
139.264789027379));
#128030=CARTESIAN_POINT('Ctrl Pts',(79.1545301201519,-7.56372603772657,
139.261893507738));
#128031=CARTESIAN_POINT('Ctrl Pts',(79.2558412699803,-7.50782103574636,
139.254738139325));
#128032=CARTESIAN_POINT('Ctrl Pts',(79.3186268530432,-7.47812577495616,
139.25052548465));
#128033=CARTESIAN_POINT('Ctrl Pts',(79.4047570279563,-7.44379104376631,
139.244851496986));
#128034=CARTESIAN_POINT('Ctrl Pts',(79.42661178888,-7.43560668773582,139.243420092094));
#128035=CARTESIAN_POINT('Ctrl Pts',(79.5093040189332,-7.40660504285213,
139.238012131354));
#128036=CARTESIAN_POINT('Ctrl Pts',(79.5711511706588,-7.38885856077627,
139.233984518759));
#128037=CARTESIAN_POINT('Ctrl Pts',(79.645020838286,-7.3722172548364,139.229029798449));
#128038=CARTESIAN_POINT('Ctrl Pts',(79.6562062440389,-7.36981819839152,
139.228275698206));
#128039=CARTESIAN_POINT('Ctrl Pts',(79.6736845488838,-7.3662573140173,139.227090081093));
#128040=CARTESIAN_POINT('Ctrl Pts',(79.6799611875879,-7.36501617966122,
139.226662860076));
#128041=CARTESIAN_POINT('Ctrl Pts',(79.6910965948281,-7.36288085561345,
139.225902100367));
#128042=CARTESIAN_POINT('Ctrl Pts',(79.6959524107364,-7.36197207964264,
139.225569389795));
#128043=CARTESIAN_POINT('Ctrl Pts',(79.7076584209494,-7.35983511981965,
139.224765019745));
#128044=CARTESIAN_POINT('Ctrl Pts',(79.7145122729696,-7.35862826076438,
139.224292190922));
#128045=CARTESIAN_POINT('Ctrl Pts',(79.7357207741475,-7.35503061934712,
139.222823712972));
#128046=CARTESIAN_POINT('Ctrl Pts',(79.7500988928056,-7.35278502519239,
139.221820598745));
#128047=CARTESIAN_POINT('Ctrl Pts',(79.8237555849773,-7.3422677417297,139.216649342557));
#128048=CARTESIAN_POINT('Ctrl Pts',(79.8834144880129,-7.33700729622843,
139.212355050607));
#128049=CARTESIAN_POINT('Ctrl Pts',(80.049545421667,-7.33134203810467,139.20030964474));
#128050=CARTESIAN_POINT('Ctrl Pts',(80.1559845018728,-7.33790895035622,
139.192510301768));
#128051=CARTESIAN_POINT('Ctrl Pts',(80.3168552909091,-7.36343389448626,
139.18094372524));
#128052=CARTESIAN_POINT('Ctrl Pts',(80.3721553983385,-7.37511615084551,
139.177004371144));
#128053=CARTESIAN_POINT('Ctrl Pts',(80.4432516755323,-7.39395672751375,
139.171989438108));
#128054=CARTESIAN_POINT('Ctrl Pts',(80.4596747997823,-7.39857995610281,
139.170834357321));
#128055=CARTESIAN_POINT('Ctrl Pts',(80.4861969677707,-7.4064877830627,139.168973820899));
#128056=CARTESIAN_POINT('Ctrl Pts',(80.4963403561506,-7.40961799027086,
139.168263415141));
#128057=CARTESIAN_POINT('Ctrl Pts',(80.5158196689459,-7.41583374298972,
139.166901131199));
